#128058=CARTESIAN_POINT('Ctrl Pts',(80.5251595237089,-7.41890539737718,
139.166248831528));
#128059=CARTESIAN_POINT('Ctrl Pts',(80.5468327157855,-7.42624642897226,
139.164736927369));
#128060=CARTESIAN_POINT('Ctrl Pts',(80.559144276443,-7.43057844554725,139.163879422684));
#128061=CARTESIAN_POINT('Ctrl Pts',(80.5990935705138,-7.44516501676963,
139.161100159304));
#128062=CARTESIAN_POINT('Ctrl Pts',(80.6265112179921,-7.45600880997235,
139.159197893095));
#128063=CARTESIAN_POINT('Ctrl Pts',(80.6916105920269,-7.48377576698143,
139.154680964787));
#128064=CARTESIAN_POINT('Ctrl Pts',(80.7289794051964,-7.50138379780424,
139.152088145992));
#128065=CARTESIAN_POINT('Ctrl Pts',(80.8623561745392,-7.57040135230035,
139.142761079237));
#128066=CARTESIAN_POINT('Ctrl Pts',(80.9539129070601,-7.62979577890478,
139.136233145291));
#128067=CARTESIAN_POINT('Ctrl Pts',(81.0837382271023,-7.73337446686093,
139.125942516964));
#128068=CARTESIAN_POINT('Ctrl Pts',(81.1265853934548,-7.77132890007261,
139.122340462722));
#128069=CARTESIAN_POINT('Ctrl Pts',(81.1754549745402,-7.81932673492763,
139.117856955963));
#128070=CARTESIAN_POINT('Ctrl Pts',(81.1834378663579,-7.8273284537776,139.117111704332));
#128071=CARTESIAN_POINT('Ctrl Pts',(81.1957887035048,-7.83996297203915,
139.115937137606));
#128072=CARTESIAN_POINT('Ctrl Pts',(81.2002127297484,-7.84454081437404,
139.115511994429));
#128073=CARTESIAN_POINT('Ctrl Pts',(81.2080252573827,-7.85271824908043,
139.114753077978));
#128074=CARTESIAN_POINT('Ctrl Pts',(81.2114241279721,-7.8563077256886,139.114420111112));
#128075=CARTESIAN_POINT('Ctrl Pts',(81.219597008072,-7.86501624100604,139.113612707633));
#128076=CARTESIAN_POINT('Ctrl Pts',(81.224354739907,-7.87015024817455,139.113137074994));
#128077=CARTESIAN_POINT('Ctrl Pts',(81.2390495351768,-7.88620902058621,
139.111650882181));
#128078=CARTESIAN_POINT('Ctrl Pts',(81.2488734714249,-7.89723569545139,
139.110632602807));
#128079=CARTESIAN_POINT('Ctrl Pts',(81.2990284598913,-7.95506090269255,
139.105310447461));
#128080=CARTESIAN_POINT('Ctrl Pts',(81.3368766919029,-8.00394184402509,
139.100872666353));
#128081=CARTESIAN_POINT('Ctrl Pts',(81.4570882857847,-8.17842517040699,
139.085508070088));
#128082=CARTESIAN_POINT('Ctrl Pts',(81.5251785484698,-8.31302113873978,
139.074524324563));
#128083=CARTESIAN_POINT('Ctrl Pts',(81.5811030584779,-8.47454789597075,
139.062769785278));
#128084=CARTESIAN_POINT('Ctrl Pts',(81.587526807376,-8.49428713845587,139.061354270288));
#128085=CARTESIAN_POINT('Ctrl Pts',(81.5972254986323,-8.52609817184272,
139.059105574938));
#128086=CARTESIAN_POINT('Ctrl Pts',(81.6007361444671,-8.53809519726469,
139.058264818814));
#128087=CARTESIAN_POINT('Ctrl Pts',(81.6067534547674,-8.55955129749134,
139.056773805271));
#128088=CARTESIAN_POINT('Ctrl Pts',(81.6093123974102,-8.56899496695653,
139.056121879899));
#128089=CARTESIAN_POINT('Ctrl Pts',(81.614512959671,-8.58887972317174,139.054758002613));
#128090=CARTESIAN_POINT('Ctrl Pts',(81.6171368357983,-8.59932501643513,
139.054046649405));
#128091=CARTESIAN_POINT('Ctrl Pts',(81.6238244612891,-8.62708396658456,
139.052169138659));
#128092=CARTESIAN_POINT('Ctrl Pts',(81.6277126660476,-8.64443880207056,
139.051008621214));
#128093=CARTESIAN_POINT('Ctrl Pts',(81.646684389425,-8.73596411027016,139.044952676544));
#128094=CARTESIAN_POINT('Ctrl Pts',(81.6569794717248,-8.81104083498744,
139.040211539027));
#128095=CARTESIAN_POINT('Ctrl Pts',(81.6692157845001,-8.99033709402061,
139.029131904));
#128096=CARTESIAN_POINT('Ctrl Pts',(81.6665639372429,-9.09453784548305,
139.022889697919));
#128097=CARTESIAN_POINT('Ctrl Pts',(81.6485596052606,-9.24510491714907,
139.013428296461));
#128098=CARTESIAN_POINT('Ctrl Pts',(81.6408782397394,-9.29213504358959,
139.010406203584));
#128099=CARTESIAN_POINT('Ctrl Pts',(81.6289718448549,-9.34946549794788,
139.006569086307));
#128100=CARTESIAN_POINT('Ctrl Pts',(81.6266447414103,-9.36014202085136,
139.005847883685));
#128101=CARTESIAN_POINT('Ctrl Pts',(81.622828921443,-9.37685667925658,139.004707275751));
#128102=CARTESIAN_POINT('Ctrl Pts',(81.6214110816232,-9.38291091157659,
139.004291750468));
#128103=CARTESIAN_POINT('Ctrl Pts',(81.6186685003208,-9.39433343660984,
139.003503021156));
#128104=CARTESIAN_POINT('Ctrl Pts',(81.6173508844832,-9.39970324732988,
139.003130217162));
#128105=CARTESIAN_POINT('Ctrl Pts',(81.6141616867702,-9.41242650897211,
139.002242202601));
#128106=CARTESIAN_POINT('Ctrl Pts',(81.6122665676593,-9.4197738504856,139.001725684514));
#128107=CARTESIAN_POINT('Ctrl Pts',(81.6056823884638,-9.44459813193324,
138.99996853776));
#128108=CARTESIAN_POINT('Ctrl Pts',(81.6007589903592,-9.46201084391851,
138.998715814736));
#128109=CARTESIAN_POINT('Ctrl Pts',(81.5879289415297,-9.50471762477543,
138.995599043641));
#128110=CARTESIAN_POINT('Ctrl Pts',(81.5797006411595,-9.52990936294555,
138.993721808239));
#128111=CARTESIAN_POINT('Ctrl Pts',(81.5407094005852,-9.64029176324238,
138.985353711912));
#128112=CARTESIAN_POINT('Ctrl Pts',(81.5036303681489,-9.72308662970838,
138.978706454975));
#128113=CARTESIAN_POINT('Ctrl Pts',(81.4133986209474,-9.887256275759,138.965137209152));
#128114=CARTESIAN_POINT('Ctrl Pts',(81.3594846578721,-9.96784638168643,
138.958256394555));
#128115=CARTESIAN_POINT('Ctrl Pts',(81.2871068676301,-10.0579530477069,
138.950352436821));
#128116=CARTESIAN_POINT('Ctrl Pts',(81.2750981212901,-10.0723961819373,
138.949077814952));
#128117=CARTESIAN_POINT('Ctrl Pts',(81.255614451474,-10.0950394144237,138.947066337866));
#128118=CARTESIAN_POINT('Ctrl Pts',(81.2482977415181,-10.1033728874261,
138.946323108888));
#128119=CARTESIAN_POINT('Ctrl Pts',(81.234469922968,-10.1188086629687,138.944940642752));
#128120=CARTESIAN_POINT('Ctrl Pts',(81.2279793960653,-10.1259286942567,
138.944300586777));
#128121=CARTESIAN_POINT('Ctrl Pts',(81.213184158602,-10.1418787674245,138.94286109795));
#128122=CARTESIAN_POINT('Ctrl Pts',(81.2048440499005,-10.1506753454214,
138.942063215308));
#128123=CARTESIAN_POINT('Ctrl Pts',(81.1794611121129,-10.1768689610236,
138.939674376835));
#128124=CARTESIAN_POINT('Ctrl Pts',(81.1621316509018,-10.1939845856308,
138.938095900388));
#128125=CARTESIAN_POINT('Ctrl Pts',(81.1211872542965,-10.23268741861,138.934478500816));
#128126=CARTESIAN_POINT('Ctrl Pts',(81.097313156499,-10.2539869040337,138.93245113995));
#128127=CARTESIAN_POINT('Ctrl Pts',(81.0072187051488,-10.329820797807,138.925062898522));
#128128=CARTESIAN_POINT('Ctrl Pts',(80.9374294033046,-10.3799058304871,
138.919846998417));
#128129=CARTESIAN_POINT('Ctrl Pts',(80.7867978735428,-10.4712843910356,
138.909083028692));
#128130=CARTESIAN_POINT('Ctrl Pts',(80.7058266837974,-10.5117979899266,
138.903548120027));
#128131=CARTESIAN_POINT('Ctrl Pts',(80.6073565927027,-10.5514259613815,
138.896661246888));
#128132=CARTESIAN_POINT('Ctrl Pts',(80.5926490493154,-10.5571035946484,
138.89562856959));
#128133=CARTESIAN_POINT('Ctrl Pts',(80.5711965936094,-10.5650370547405,
138.894113377604));
#128134=CARTESIAN_POINT('Ctrl Pts',(80.5645138102336,-10.5674599467685,
138.893640126414));
#128135=CARTESIAN_POINT('Ctrl Pts',(80.5526467059649,-10.5716767200934,
138.892797194074));
#128136=CARTESIAN_POINT('Ctrl Pts',(80.5474687308649,-10.5734878714346,
138.892428530702));
#128137=CARTESIAN_POINT('Ctrl Pts',(80.5362057212862,-10.5773651187782,
138.891624647997));
#128138=CARTESIAN_POINT('Ctrl Pts',(80.5301177430218,-10.5794215613716,
138.891188912372));
#128139=CARTESIAN_POINT('Ctrl Pts',(80.5127235205137,-10.5851852152572,
138.889940802131));
#128140=CARTESIAN_POINT('Ctrl Pts',(80.5013895207989,-10.5888065028011,
138.889123758127));
#128141=CARTESIAN_POINT('Ctrl Pts',(80.4754563525984,-10.5967872066983,
138.887247212396));
#128142=CARTESIAN_POINT('Ctrl Pts',(80.4608343613467,-10.6010683250892,
138.886184082174));
#128143=CARTESIAN_POINT('Ctrl Pts',(80.3060670505471,-10.6440864178984,
138.874892248395));
#128144=CARTESIAN_POINT('Ctrl Pts',(80.1614840342172,-10.664519051482,138.864075581864));
#128145=CARTESIAN_POINT('Ctrl Pts',(79.9507120684992,-10.666553286255,138.849022903426));
#128146=CARTESIAN_POINT('Ctrl Pts',(79.8853587767227,-10.6633365494475,
138.844443159493));
#128147=CARTESIAN_POINT('Ctrl Pts',(79.8028201934209,-10.6543842482472,
138.838777170037));
#128148=CARTESIAN_POINT('Ctrl Pts',(79.7853152806429,-10.6522038705261,
138.837582081662));
#128149=CARTESIAN_POINT('Ctrl Pts',(79.7572137075095,-10.6482494159339,
138.835673439323));
#128150=CARTESIAN_POINT('Ctrl Pts',(79.746594227845,-10.6466501889977,138.834954450985));
#128151=CARTESIAN_POINT('Ctrl Pts',(79.7263216489237,-10.6433965010427,
138.833586008472));
#128152=CARTESIAN_POINT('Ctrl Pts',(79.7166662623906,-10.6417593915083,
138.832936037184));
#128153=CARTESIAN_POINT('Ctrl Pts',(79.6944492618709,-10.6377905728283,
138.831444293622));
#128154=CARTESIAN_POINT('Ctrl Pts',(79.6818988072796,-10.6353992969059,
138.830604443108));
#128155=CARTESIAN_POINT('Ctrl Pts',(79.6420374199767,-10.6273281405852,
138.827945004566));
#128156=CARTESIAN_POINT('Ctrl Pts',(79.614840198836,-10.6211064611918,138.82614258319));
#128157=CARTESIAN_POINT('Ctrl Pts',(79.5156892451251,-10.5957881311155,
138.819599937934));
#128158=CARTESIAN_POINT('Ctrl Pts',(79.4448791678645,-10.5725581631489,
138.814987170475));
#128159=CARTESIAN_POINT('Ctrl Pts',(79.2563727472063,-10.496389367791,138.802521098322));
#128160=CARTESIAN_POINT('Ctrl Pts',(79.1429144477376,-10.4344187789382,
138.794823601157));
#128161=CARTESIAN_POINT('Ctrl Pts',(79.0263614493235,-10.3519535891143,
138.785554713314));
#128162=CARTESIAN_POINT('Ctrl Pts',(79.0150776629315,-10.3437553698324,
138.784641540473));
#128163=CARTESIAN_POINT('Ctrl Pts',(78.9983272179701,-10.3312610367618,
138.783259831104));
#128164=CARTESIAN_POINT('Ctrl Pts',(78.9927820373413,-10.3270705639592,
138.782798048324));
#128165=CARTESIAN_POINT('Ctrl Pts',(78.9828227851343,-10.3194460161396,
138.781960421194));
#128166=CARTESIAN_POINT('Ctrl Pts',(78.9783994072971,-10.3160241273241,
138.781585413341));
#128167=CARTESIAN_POINT('Ctrl Pts',(78.9694186609889,-10.3090041325214,
138.780817760678));
#128168=CARTESIAN_POINT('Ctrl Pts',(78.9648627588378,-10.3054043835621,
138.780425014286));
#128169=CARTESIAN_POINT('Ctrl Pts',(78.9535305410094,-10.2963538487905,
138.779439982242));
#128170=CARTESIAN_POINT('Ctrl Pts',(78.9467780071182,-10.2908737565632,
138.778845701987));
#128171=CARTESIAN_POINT('Ctrl Pts',(78.9317431800531,-10.2784755846167,
138.777506569767));
#128172=CARTESIAN_POINT('Ctrl Pts',(78.9234846425289,-10.2715294431498,
138.776759968635));
#128173=CARTESIAN_POINT('Ctrl Pts',(78.8991134467303,-10.2506235570128,
138.774525111573));
#128174=CARTESIAN_POINT('Ctrl Pts',(78.8832011607647,-10.2364346921585,
138.773024144763));
#128175=CARTESIAN_POINT('Ctrl Pts',(78.8231402598813,-10.1807734479365,
138.767209270554));
#128176=CARTESIAN_POINT('Ctrl Pts',(78.7809950559529,-10.1372118943443,
138.762810883504));
#128177=CARTESIAN_POINT('Ctrl Pts',(78.6562619125777,-9.99336781705434,
138.748954119857));
#128178=CARTESIAN_POINT('Ctrl Pts',(78.5829465834908,-9.88565436811021,
138.739549489168));
#128179=CARTESIAN_POINT('Ctrl Pts',(78.5134952003582,-9.7525099803891,138.729229690625));
#128180=CARTESIAN_POINT('Ctrl Pts',(78.5044393173238,-9.73434739552867,
138.72784644108));
#128181=CARTESIAN_POINT('Ctrl Pts',(78.4903442080147,-9.70473518234833,
138.725629613013));
#128182=CARTESIAN_POINT('Ctrl Pts',(78.4850983435307,-9.69338681378128,
138.724788985808));
#128183=CARTESIAN_POINT('Ctrl Pts',(78.4759856550359,-9.67307616041793,
138.723299962849));
#128184=CARTESIAN_POINT('Ctrl Pts',(78.4720689647162,-9.66413703387003,
138.722649884185));
#128185=CARTESIAN_POINT('Ctrl Pts',(78.46395169687,-9.64515891166399,138.721280601481));
#128186=CARTESIAN_POINT('Ctrl Pts',(78.4597704593522,-9.63511210225471,
138.720562078149));
#128187=CARTESIAN_POINT('Ctrl Pts',(78.448820388865,-9.60805665503589,138.718643617584));
#128188=CARTESIAN_POINT('Ctrl Pts',(78.4422328186799,-9.59097591628757,
138.717449777295));
#128189=CARTESIAN_POINT('Ctrl Pts',(78.4060847467122,-9.49244119123581,
138.710655162977));
#128190=CARTESIAN_POINT('Ctrl Pts',(78.3826313546794,-9.40888344053641,
138.705261407724));
#128191=CARTESIAN_POINT('Ctrl Pts',(78.3445816311609,-9.21688870063967,
138.693247528272));
#128192=CARTESIAN_POINT('Ctrl Pts',(78.3339388140977,-9.10809724434987,
138.686703611574));
#128193=CARTESIAN_POINT('Ctrl Pts',(78.3340002645784,-8.99906107773531,
138.679802703723));
#128194=CARTESIAN_POINT('Ctrl Pts',(78.3340002659352,-8.9990586732761,138.679802551545));
#128195=CARTESIAN_POINT('Ctrl Pts',(78.3340122908892,-8.97777640250722,
138.678455593874));
#128196=CARTESIAN_POINT('Ctrl Pts',(78.3344321193602,-8.95649709999227,
138.677095246544));
#128197=CARTESIAN_POINT('Ctrl Pts',(78.3358009540242,-8.92131348367504,
138.67481502874));
#128198=CARTESIAN_POINT('Ctrl Pts',(78.3365170051759,-8.90740232859391,
138.673905425437));
#128199=CARTESIAN_POINT('Ctrl Pts',(78.3378248684508,-8.88698456957304,
138.672556420238));
#128200=CARTESIAN_POINT('Ctrl Pts',(78.3382806792744,-8.88046945513672,
138.672123874439));
#128201=CARTESIAN_POINT('Ctrl Pts',(78.3391689393945,-8.86876230860699,
138.671342591399));
#128202=CARTESIAN_POINT('Ctrl Pts',(78.3395874622305,-8.86356926269507,
138.67099460244));
#128203=CARTESIAN_POINT('Ctrl Pts',(78.3404626590702,-8.85331094236375,
138.6703042116));
#128204=CARTESIAN_POINT('Ctrl Pts',(78.3409181710623,-8.84824576329396,
138.669961869966));
#128205=CARTESIAN_POINT('Ctrl Pts',(78.3420395514555,-8.83638530291543,
138.669156852411));
#128206=CARTESIAN_POINT('Ctrl Pts',(78.3427239995179,-8.82959204207361,
138.668693172819));
#128207=CARTESIAN_POINT('Ctrl Pts',(78.3449257623353,-8.80900852954848,
138.667280747579));
#128208=CARTESIAN_POINT('Ctrl Pts',(78.3465735514021,-8.79523325050894,
138.666325306197));
#128209=CARTESIAN_POINT('Ctrl Pts',(78.3545977592447,-8.73458488322595,
138.66207839854));
#128210=CARTESIAN_POINT('Ctrl Pts',(78.3627964138434,-8.68797865093281,
138.658708642598));
#128211=CARTESIAN_POINT('Ctrl Pts',(78.3892162346329,-8.56797690308466,
138.649852340649));
#128212=CARTESIAN_POINT('Ctrl Pts',(78.4104657701459,-8.49537864982559,
138.644319845945));
#128213=CARTESIAN_POINT('Ctrl Pts',(78.436559345854,-8.42449211911253,138.638847691527));
#128214=CARTESIAN_POINT('Ctrl Pts',(78.4365593750041,-8.42449203992252,
138.833737849951));
#128215=CARTESIAN_POINT('Ctrl Pts',(78.4357654627803,-8.42664880352886,
138.833891290677));
#128216=CARTESIAN_POINT('Ctrl Pts',(78.4349760076973,-8.42880722551953,
138.834044583115));
#128217=CARTESIAN_POINT('Ctrl Pts',(78.4308396898992,-8.44018914343849,
138.834851539479));
#128218=CARTESIAN_POINT('Ctrl Pts',(78.4275698389047,-8.44944058502104,
138.835502628057));
#128219=CARTESIAN_POINT('Ctrl Pts',(78.4201791056846,-8.47095437667124,
138.83700585588));
#128220=CARTESIAN_POINT('Ctrl Pts',(78.4161188918261,-8.48323701707355,
138.837855968269));
#128221=CARTESIAN_POINT('Ctrl Pts',(78.4034747020729,-8.52303690839969,
138.840585659804));
#128222=CARTESIAN_POINT('Ctrl Pts',(78.3954613590095,-8.55073089736053,
138.842446720717));
#128223=CARTESIAN_POINT('Ctrl Pts',(78.3649421910079,-8.66747049985526,
138.850153225424));
#128224=CARTESIAN_POINT('Ctrl Pts',(78.3490992446991,-8.75809293572287,
138.855791524017));
#128225=CARTESIAN_POINT('Ctrl Pts',(78.3307435608108,-8.96054648702028,
138.868210307207));
#128226=CARTESIAN_POINT('Ctrl Pts',(78.3318429385482,-9.07223950797057,
138.874946240725));
#128227=CARTESIAN_POINT('Ctrl Pts',(78.345676015335,-9.19743340964611,138.883137059902));
#128228=CARTESIAN_POINT('Ctrl Pts',(78.3474637306941,-9.21187647540124,
138.884091970012));
#128229=CARTESIAN_POINT('Ctrl Pts',(78.3503854186024,-9.23318692748227,
138.885518151753));
#128230=CARTESIAN_POINT('Ctrl Pts',(78.3513736460147,-9.24007405299294,
138.885981735949));
#128231=CARTESIAN_POINT('Ctrl Pts',(78.3532149466878,-9.25235856789412,
138.886813725034));
#128232=CARTESIAN_POINT('Ctrl Pts',(78.3540514732453,-9.25775822795488,
138.887181205429));
#128233=CARTESIAN_POINT('Ctrl Pts',(78.3559612207556,-9.2696968667602,138.887997699576));
#128234=CARTESIAN_POINT('Ctrl Pts',(78.3570468824366,-9.27623351948151,
138.888447373386));
#128235=CARTESIAN_POINT('Ctrl Pts',(78.3603559833217,-9.29544738024032,
138.889776537574));
#128236=CARTESIAN_POINT('Ctrl Pts',(78.362687311603,-9.30810516225522,138.890661655817));
#128237=CARTESIAN_POINT('Ctrl Pts',(78.3684118462298,-9.33728406070953,
138.89272206758));
#128238=CARTESIAN_POINT('Ctrl Pts',(78.3719097151171,-9.35378300890375,
138.893902022913));
#128239=CARTESIAN_POINT('Ctrl Pts',(78.3848745738333,-9.4106655989781,138.898015580042));
#128240=CARTESIAN_POINT('Ctrl Pts',(78.3955983074982,-9.45074510014426,
138.900993480983));
#128241=CARTESIAN_POINT('Ctrl Pts',(78.4451145988264,-9.61151751358259,
138.913166572));
#128242=CARTESIAN_POINT('Ctrl Pts',(78.4961331980123,-9.72802109726034,
138.922476660456));
#128243=CARTESIAN_POINT('Ctrl Pts',(78.5817385502336,-9.875203573505,138.93444442158));
#128244=CARTESIAN_POINT('Ctrl Pts',(78.6050656555788,-9.91192412359391,
138.93745427323));
#128245=CARTESIAN_POINT('Ctrl Pts',(78.6386422790772,-9.96046994167867,
138.941468598723));
#128246=CARTESIAN_POINT('Ctrl Pts',(78.6476581072446,-9.97312321248951,
138.942518391084));
#128247=CARTESIAN_POINT('Ctrl Pts',(78.6623297722622,-9.9931163850955,138.944183255617));
#128248=CARTESIAN_POINT('Ctrl Pts',(78.6678719369064,-10.0005381662012,
138.944802656392));
#128249=CARTESIAN_POINT('Ctrl Pts',(78.6794382270635,-10.0157606670721,
138.946076128631));
#128250=CARTESIAN_POINT('Ctrl Pts',(78.6854702666044,-10.0235549404123,
138.94672985669));
#128251=CARTESIAN_POINT('Ctrl Pts',(78.699755812662,-10.0416793497508,138.948254268952));
#128252=CARTESIAN_POINT('Ctrl Pts',(78.7080639106748,-10.0519657657019,
138.949122740492));
#128253=CARTESIAN_POINT('Ctrl Pts',(78.7359439856612,-10.085656079992,138.951979430824));
#128254=CARTESIAN_POINT('Ctrl Pts',(78.7560370060276,-10.1086221124858,
138.953946565433));
#128255=CARTESIAN_POINT('Ctrl Pts',(78.8777093875024,-10.2402157882939,
138.965372180505));
#128256=CARTESIAN_POINT('Ctrl Pts',(78.9928255613813,-10.3353914340398,
138.974203251278));
#128257=CARTESIAN_POINT('Ctrl Pts',(79.1676650222503,-10.4443185494194,
138.986966430809));
#128258=CARTESIAN_POINT('Ctrl Pts',(79.2178108548987,-10.472078889972,138.990573127886));
#128259=CARTESIAN_POINT('Ctrl Pts',(79.2794407214493,-10.5021578317847,
138.995061827805));
#128260=CARTESIAN_POINT('Ctrl Pts',(79.2896510534084,-10.5070130000715,
138.995807276204));
#128261=CARTESIAN_POINT('Ctrl Pts',(79.3056866175785,-10.5144389909557,
138.996982042738));
#128262=CARTESIAN_POINT('Ctrl Pts',(79.311478740144,-10.5170810794716,138.997407186286));
#128263=CARTESIAN_POINT('Ctrl Pts',(79.3217950848453,-10.5217156538283,
138.998166097348));
#128264=CARTESIAN_POINT('Ctrl Pts',(79.3263132329559,-10.523721291979,138.998499058561));
#128265=CARTESIAN_POINT('Ctrl Pts',(79.3372499262112,-10.5285180166273,
138.999306413092));
#128266=CARTESIAN_POINT('Ctrl Pts',(79.343677146171,-10.5312887691616,138.999782001796));
#128267=CARTESIAN_POINT('Ctrl Pts',(79.363714522277,-10.5397774914202,139.001267754765));
#128268=CARTESIAN_POINT('Ctrl Pts',(79.3773829243795,-10.5453549339939,
139.002285627907));
#128269=CARTESIAN_POINT('Ctrl Pts',(79.4485795306223,-10.5733091368075,
139.007603595204));
#128270=CARTESIAN_POINT('Ctrl Pts',(79.5072399477876,-10.5926557040071,
139.012037311236));
#128271=CARTESIAN_POINT('Ctrl Pts',(79.7118081413373,-10.6477389056236,
139.027398716744));
#128272=CARTESIAN_POINT('Ctrl Pts',(79.8614335449113,-10.6670079403707,
139.038383640353));
#128273=CARTESIAN_POINT('Ctrl Pts',(80.0323665402619,-10.6658146426545,
139.050137982387));
#128274=CARTESIAN_POINT('Ctrl Pts',(80.0530991329156,-10.6652827284884,
139.051552181808));
#128275=CARTESIAN_POINT('Ctrl Pts',(80.0862990603242,-10.6638102580642,
139.053799212641));
#128276=CARTESIAN_POINT('Ctrl Pts',(80.0987745577488,-10.6631162629689,
139.054639599674));
#128277=CARTESIAN_POINT('Ctrl Pts',(80.1210027308491,-10.6616287341169,
139.056130199461));
#128278=CARTESIAN_POINT('Ctrl Pts',(80.1307583240794,-10.660889514271,139.056782076316));
#128279=CARTESIAN_POINT('Ctrl Pts',(80.1512408935126,-10.6591558798163,
139.058146094951));
#128280=CARTESIAN_POINT('Ctrl Pts',(80.1619659080164,-10.658143267402,139.058857636047));
#128281=CARTESIAN_POINT('Ctrl Pts',(80.190381465752,-10.6551820510527,139.06073620679));
#128282=CARTESIAN_POINT('Ctrl Pts',(80.2080522030789,-10.653053854273,139.06189758614));
#128283=CARTESIAN_POINT('Ctrl Pts',(80.3009130684846,-10.640357347065,139.067969907922));
#128284=CARTESIAN_POINT('Ctrl Pts',(80.3753541586966,-10.6249406998734,
139.072725524982));
#128285=CARTESIAN_POINT('Ctrl Pts',(80.5500972025953,-10.5760962469182,
139.083910609427));
#128286=CARTESIAN_POINT('Ctrl Pts',(80.648769083236,-10.5381101484378,139.090239133787));
#128287=CARTESIAN_POINT('Ctrl Pts',(80.7844210682072,-10.4704974628363,
139.099708393852));
#128288=CARTESIAN_POINT('Ctrl Pts',(80.8247861040395,-10.4482424687139,
139.102635401686));
#128289=CARTESIAN_POINT('Ctrl Pts',(80.8734287501862,-10.4187302157357,
139.106364745582));
#128290=CARTESIAN_POINT('Ctrl Pts',(80.8826293490558,-10.4130246366018,
139.10707941089));
#128291=CARTESIAN_POINT('Ctrl Pts',(80.8970066692135,-10.4039136087939,
139.108211930331));
#128292=CARTESIAN_POINT('Ctrl Pts',(80.9022213035857,-10.4005681353655,
139.108625994407));
#128293=CARTESIAN_POINT('Ctrl Pts',(80.9120557258954,-10.3941811023156,
139.109413403265));
#128294=CARTESIAN_POINT('Ctrl Pts',(80.9166791767232,-10.3911455266973,
139.109786363018));
#128295=CARTESIAN_POINT('Ctrl Pts',(80.9276385213664,-10.3838716993669,
139.110676941632));
#128296=CARTESIAN_POINT('Ctrl Pts',(80.9339605435542,-10.3796129181916,
139.111195893278));
#128297=CARTESIAN_POINT('Ctrl Pts',(80.955388482954,-10.3649633710228,139.112972057691));
#128298=CARTESIAN_POINT('Ctrl Pts',(80.9703513945365,-10.3543671067065,
139.114241727563));
#128299=CARTESIAN_POINT('Ctrl Pts',(81.0068974031942,-10.32756989012,139.117410391055));
#128300=CARTESIAN_POINT('Ctrl Pts',(81.0282671182901,-10.3110876264722,
139.119323123501));
#128301=CARTESIAN_POINT('Ctrl Pts',(81.1223055716679,-10.2348431425141,
139.127982044712));
#128302=CARTESIAN_POINT('Ctrl Pts',(81.1902335271836,-10.1695090043202,
139.134893419425));
#128303=CARTESIAN_POINT('Ctrl Pts',(81.3135590047839,-10.0289559907336,
139.148420685002));
#128304=CARTESIAN_POINT('Ctrl Pts',(81.3688940057096,-9.9541080016211,139.155014791111));
#128305=CARTESIAN_POINT('Ctrl Pts',(81.4275744848557,-9.8590344266445,139.162653017737));
#128306=CARTESIAN_POINT('Ctrl Pts',(81.4371724637305,-9.84287864824879,
139.163927794711));
#128307=CARTESIAN_POINT('Ctrl Pts',(81.451942601725,-9.81703073625185,139.165931753165));
#128308=CARTESIAN_POINT('Ctrl Pts',(81.4572955243766,-9.80744430601168,
139.166667391658));
#128309=CARTESIAN_POINT('Ctrl Pts',(81.4667474109426,-9.79011691281913,
139.167983746783));
#128310=CARTESIAN_POINT('Ctrl Pts',(81.4708807948246,-9.7823952938621,139.168565672047));
#128311=CARTESIAN_POINT('Ctrl Pts',(81.480454589229,-9.76416634305832,139.169928705837));
#128312=CARTESIAN_POINT('Ctrl Pts',(81.4858443843175,-9.75363284715538,
139.170708010123));
#128313=CARTESIAN_POINT('Ctrl Pts',(81.5013392258646,-9.72253813808178,
139.172984966399));
#128314=CARTESIAN_POINT('Ctrl Pts',(81.511133180982,-9.701824354067,139.174471836469));
#128315=CARTESIAN_POINT('Ctrl Pts',(81.5545678892191,-9.60483365950251,
139.181307329184));
#128316=CARTESIAN_POINT('Ctrl Pts',(81.5828824965542,-9.52629880540434,
139.186476374112));
#128317=CARTESIAN_POINT('Ctrl Pts',(81.6283618491473,-9.36260144581922,
139.196889616307));
#128318=CARTESIAN_POINT('Ctrl Pts',(81.6449922152124,-9.27756328726469,
139.202114256777));
#128319=CARTESIAN_POINT('Ctrl Pts',(81.6605055395375,-9.14358313068467,
139.210524640583));
#128320=CARTESIAN_POINT('Ctrl Pts',(81.6639730348982,-9.09532865618125,
139.21359091935));
#128321=CARTESIAN_POINT('Ctrl Pts',(81.6656425916159,-9.0361679198286,139.217469048152));
#128322=CARTESIAN_POINT('Ctrl Pts',(81.6658425518073,-9.02533651086294,
139.218183950568));
#128323=CARTESIAN_POINT('Ctrl Pts',(81.6659913384069,-9.00824713174338,
139.21932067823));
#128324=CARTESIAN_POINT('Ctrl Pts',(81.6660105618148,-9.00198985817584,
139.219738748212));
#128325=CARTESIAN_POINT('Ctrl Pts',(81.6659804065235,-8.99021679746421,
139.220529091812));
#128326=CARTESIAN_POINT('Ctrl Pts',(81.665938884974,-8.98470118065836,139.220900933308));
#128327=CARTESIAN_POINT('Ctrl Pts',(81.665776247815,-8.97168436904526,139.221782089728));
#128328=CARTESIAN_POINT('Ctrl Pts',(81.6656318524333,-8.96418367016243,
139.222292656523));
#128329=CARTESIAN_POINT('Ctrl Pts',(81.6649796485914,-8.93910716416467,
139.224008449677));
#128330=CARTESIAN_POINT('Ctrl Pts',(81.6642442727935,-8.92153913792775,
139.225225038674));
#128331=CARTESIAN_POINT('Ctrl Pts',(81.6617623174051,-8.87854430881846,
139.228232910677));
#128332=CARTESIAN_POINT('Ctrl Pts',(81.6597100664976,-8.85314007145961,
139.230036297735));
#128333=CARTESIAN_POINT('Ctrl Pts',(81.6484208755317,-8.74450804695441,
139.237834262732));
#128334=CARTESIAN_POINT('Ctrl Pts',(81.6334992484543,-8.66199558686887,
139.243968580014));
#128335=CARTESIAN_POINT('Ctrl Pts',(81.5880354831232,-8.48705516877,139.257090678194));
#128336=CARTESIAN_POINT('Ctrl Pts',(81.5554728734917,-8.39545161228709,
139.264029326413));
#128337=CARTESIAN_POINT('Ctrl Pts',(81.5052710113702,-8.28566429093416,
139.272340679899));
#128338=CARTESIAN_POINT('Ctrl Pts',(81.4949692404908,-8.26434832108724,
139.273955102075));
#128339=CARTESIAN_POINT('Ctrl Pts',(81.478699577489,-8.23243823474725,139.276374176812));
#128340=CARTESIAN_POINT('Ctrl Pts',(81.4730646652475,-8.2216787234766,139.277190258056));
#128341=CARTESIAN_POINT('Ctrl Pts',(81.4627059432925,-8.20241493857962,
139.278652437866));
#128342=CARTESIAN_POINT('Ctrl Pts',(81.4580244058265,-8.19388868905047,
139.279299990825));
#128343=CARTESIAN_POINT('Ctrl Pts',(81.4478369629443,-8.17571393194336,
139.280681405892));
#128344=CARTESIAN_POINT('Ctrl Pts',(81.442308662733,-8.16607846609383,139.281414429577));
#128345=CARTESIAN_POINT('Ctrl Pts',(81.4268821689816,-8.13980345713761,
139.283415691732));
#128346=CARTESIAN_POINT('Ctrl Pts',(81.4167894605229,-8.12327969583428,
139.284676868815));
#128347=CARTESIAN_POINT('Ctrl Pts',(81.3465725830168,-8.0127012163698,139.293143772132));
#128348=CARTESIAN_POINT('Ctrl Pts',(81.2774132635477,-7.92471572678365,
139.299989343676));
#128349=CARTESIAN_POINT('Ctrl Pts',(81.1262955392844,-7.76780996550157,
139.313294437602));
#128350=CARTESIAN_POINT('Ctrl Pts',(81.0454917251394,-7.69854900069521,
139.319734685963));
#128351=CARTESIAN_POINT('Ctrl Pts',(80.9465992895673,-7.62896997803671,
139.327592255134));
#128352=CARTESIAN_POINT('Ctrl Pts',(80.9344250221196,-7.62064385393388,
139.328559383554));
#128353=CARTESIAN_POINT('Ctrl Pts',(80.9162291843967,-7.60855093843947,
139.330007170816));
#128354=CARTESIAN_POINT('Ctrl Pts',(80.9102911040183,-7.60465899844532,
139.330480003006));
#128355=CARTESIAN_POINT('Ctrl Pts',(80.8997246339761,-7.59782967077172,
139.331322355417));
#128356=CARTESIAN_POINT('Ctrl Pts',(80.8951063650861,-7.59487700086125,
139.331690863198));
#128357=CARTESIAN_POINT('Ctrl Pts',(80.8849473958799,-7.58845231815264,
139.332502299767));
#128358=CARTESIAN_POINT('Ctrl Pts',(80.8794008690894,-7.58499015572465,
139.332945819337));
#128359=CARTESIAN_POINT('Ctrl Pts',(80.8632818028448,-7.57505995086257,
139.334235864697));
#128360=CARTESIAN_POINT('Ctrl Pts',(80.8526575485988,-7.56867729113766,
139.335087517461));
#128361=CARTESIAN_POINT('Ctrl Pts',(80.8281114789083,-7.55430118142076,
139.337056565091));
#128362=CARTESIAN_POINT('Ctrl Pts',(80.814143503225,-7.54638931972059,139.338178072111));
#128363=CARTESIAN_POINT('Ctrl Pts',(80.766367502663,-7.52023222950363,139.342012187541));
#128364=CARTESIAN_POINT('Ctrl Pts',(80.7320450405205,-7.50295574849416,
139.344763249164));
#128365=CARTESIAN_POINT('Ctrl Pts',(80.6328625112713,-7.45725809061481,
139.35264864543));
#128366=CARTESIAN_POINT('Ctrl Pts',(80.5667439989889,-7.431762503023,139.357826474518));
#128367=CARTESIAN_POINT('Ctrl Pts',(80.4070366551528,-7.3816026603498,139.369947844441));
#128368=CARTESIAN_POINT('Ctrl Pts',(80.3125131974446,-7.36072270970312,
139.376816046572));
#128369=CARTESIAN_POINT('Ctrl Pts',(80.1980779205702,-7.34571048063891,
139.384708637636));
#128370=CARTESIAN_POINT('Ctrl Pts',(80.1794171779391,-7.34358272082952,
139.385983097254));
#128371=CARTESIAN_POINT('Ctrl Pts',(80.1496787973133,-7.34070032995489,
139.387994920842));
#128372=CARTESIAN_POINT('Ctrl Pts',(80.1386231842156,-7.33974015272477,
139.388738641321));
#128373=CARTESIAN_POINT('Ctrl Pts',(80.1179405065252,-7.33815190540202,
139.390122410837));
#128374=CARTESIAN_POINT('Ctrl Pts',(80.1083160440931,-7.33749685898879,
139.390763275428));
#128375=CARTESIAN_POINT('Ctrl Pts',(80.0865629160185,-7.33620603602546,
139.39220511338));
#128376=CARTESIAN_POINT('Ctrl Pts',(80.0744318096969,-7.33561921072226,
139.393004528911));
#128377=CARTESIAN_POINT('Ctrl Pts',(80.0378816720721,-7.33425157098279,
139.395399930388));
#128378=CARTESIAN_POINT('Ctrl Pts',(80.0134501600528,-7.33387514206634,
139.39698335957));
#128379=CARTESIAN_POINT('Ctrl Pts',(79.9569122344079,-7.33424783383181,
139.400613212122));
#128380=CARTESIAN_POINT('Ctrl Pts',(79.9248178057395,-7.33538753403498,
139.402647977563));
#128381=CARTESIAN_POINT('Ctrl Pts',(79.8066594070181,-7.3430081095544,139.41007559726));
#128382=CARTESIAN_POINT('Ctrl Pts',(79.7211041821049,-7.35524441251809,
139.415321710573));
#128383=CARTESIAN_POINT('Ctrl Pts',(79.549169724019,-7.39364246086482,139.426085428576));
#128384=CARTESIAN_POINT('Ctrl Pts',(79.4632007283571,-7.42029278227903,
139.431589757663));
#128385=CARTESIAN_POINT('Ctrl Pts',(79.3652150567596,-7.45959374814087,
139.438440030539));
#128386=CARTESIAN_POINT('Ctrl Pts',(79.3507024823065,-7.46565452569573,
139.439470267458));
#128387=CARTESIAN_POINT('Ctrl Pts',(79.3297659706607,-7.47474829581623,
139.440982438017));
#128388=CARTESIAN_POINT('Ctrl Pts',(79.3232717054569,-7.47761856751154,
139.441455156496));
#128389=CARTESIAN_POINT('Ctrl Pts',(79.31180577059,-7.48277403096381,139.442296607062));
#128390=CARTESIAN_POINT('Ctrl Pts',(79.3068267075362,-7.48504233585205,
139.44266431683));
#128391=CARTESIAN_POINT('Ctrl Pts',(79.2960636870118,-7.49000980008923,
139.443464321018));
#128392=CARTESIAN_POINT('Ctrl Pts',(79.2902841397156,-7.49271763402121,
139.443897114828));
#128393=CARTESIAN_POINT('Ctrl Pts',(79.2738498905341,-7.50053288548231,
139.445136638163));
#128394=CARTESIAN_POINT('Ctrl Pts',(79.2632340257019,-7.5057204116621,139.445948006113));
#128395=CARTESIAN_POINT('Ctrl Pts',(79.1670791002145,-7.55398098386478,
139.453388948551));
#128396=CARTESIAN_POINT('Ctrl Pts',(79.0853565530412,-7.60423795889812,
139.46036873848));
#128397=CARTESIAN_POINT('Ctrl Pts',(78.9109705802748,-7.73340036811098,
139.47617715688));
#128398=CARTESIAN_POINT('Ctrl Pts',(78.8216819984057,-7.81600815811391,
139.484937470301));
#128399=CARTESIAN_POINT('Ctrl Pts',(78.7283665603689,-7.92345651350948,
139.494728244193));
#128400=CARTESIAN_POINT('Ctrl Pts',(78.7148900055743,-7.93958033989662,
139.496161656021));
#128401=CARTESIAN_POINT('Ctrl Pts',(78.6938650444635,-7.96572506198106,
139.498430543781));
#128402=CARTESIAN_POINT('Ctrl Pts',(78.6861189059643,-7.97558326096429,
139.499273907597));
#128403=CARTESIAN_POINT('Ctrl Pts',(78.6725513831199,-7.99325717798711,
139.500764844494));
#128404=CARTESIAN_POINT('Ctrl Pts',(78.6666859840328,-8.00103819796508,
139.501414142837));
#128405=CARTESIAN_POINT('Ctrl Pts',(78.6545511924222,-8.01743346206989,
139.502767757607));
#128406=CARTESIAN_POINT('Ctrl Pts',(78.6482954684241,-8.02605730993669,
139.503471521148));
#128407=CARTESIAN_POINT('Ctrl Pts',(78.6320287865222,-8.04894044397087,
139.50531786036));
#128408=CARTESIAN_POINT('Ctrl Pts',(78.6221578606527,-8.06329802149247,
139.506455058233));
#128409=CARTESIAN_POINT('Ctrl Pts',(78.5734443906988,-8.13659001803001,
139.512158771233));
#128410=CARTESIAN_POINT('Ctrl Pts',(78.5381473041907,-8.19779915812948,
139.516592024258));
#128411=CARTESIAN_POINT('Ctrl Pts',(78.4805144020893,-8.31425847162602,
139.524620536356));
#128412=CARTESIAN_POINT('Ctrl Pts',(78.457055835973,-8.36881079569985,139.528231549375));
#128413=CARTESIAN_POINT('Ctrl Pts',(78.4365593777415,-8.42449203248626,
139.531855306428));
#128414=CARTESIAN_POINT('Origin',(80.,-9.,141.545925280538));
#128415=CARTESIAN_POINT('',(77.9452506264311,-9.00160446819347,139.095925280496));
#128416=CARTESIAN_POINT('Ctrl Pts',(81.2520391107129,-7.37076839346111,
139.547882946156));
#128417=CARTESIAN_POINT('Ctrl Pts',(81.308376492207,-7.41406279355911,139.544018177529));
#128418=CARTESIAN_POINT('Ctrl Pts',(81.3625557941979,-7.46035206945108,
139.540153408901));
#128419=CARTESIAN_POINT('Ctrl Pts',(81.4142433388808,-7.50939162053498,
139.536288640274));
#128420=CARTESIAN_POINT('Ctrl Pts',(81.4658662946457,-7.55836989164198,
139.532428701074));
#128421=CARTESIAN_POINT('Ctrl Pts',(81.515003327894,-7.61009127859361,139.528568761873));
#128422=CARTESIAN_POINT('Ctrl Pts',(81.5613536305889,-7.66427083480709,
139.524708822673));
#128423=CARTESIAN_POINT('Ctrl Pts',(81.6076723958972,-7.71841352650165,
139.520851509828));
#128424=CARTESIAN_POINT('Ctrl Pts',(81.6512078775579,-7.7750107012777,139.516994196984));
#128425=CARTESIAN_POINT('Ctrl Pts',(81.6916969813358,-7.83374150127879,
139.51313688414));
#128426=CARTESIAN_POINT('Ctrl Pts',(81.7321720676574,-7.89245196849052,
139.509280906709));
#128427=CARTESIAN_POINT('Ctrl Pts',(81.7696025941656,-7.95329419518399,
139.505424929279));
#128428=CARTESIAN_POINT('Ctrl Pts',(81.8037675969863,-8.01591666076381,
139.501568951848));
#128429=CARTESIAN_POINT('Ctrl Pts',(81.8379321897393,-8.07853837471322,
139.497713020699));
#128430=CARTESIAN_POINT('Ctrl Pts',(81.8688311057131,-8.14293985793319,
139.493857089551));
#128431=CARTESIAN_POINT('Ctrl Pts',(81.896289179377,-8.20874472470788,139.490001158402));
#128432=CARTESIAN_POINT('Ctrl Pts',(81.9237751180498,-8.27461637159319,
139.486141314176));
#128433=CARTESIAN_POINT('Ctrl Pts',(81.9478130540654,-8.34189379684482,
139.48228146995));
#128434=CARTESIAN_POINT('Ctrl Pts',(81.9682762259155,-8.41018116256268,
139.478421625724));
#128435=CARTESIAN_POINT('Ctrl Pts',(81.9887500346486,-8.47850402447474,
139.474559775128));
#128436=CARTESIAN_POINT('Ctrl Pts',(82.0056452636483,-8.54783740001086,
139.470697924531));
#128437=CARTESIAN_POINT('Ctrl Pts',(82.0188859519888,-8.61777352870029,
139.466836073934));
#128438=CARTESIAN_POINT('Ctrl Pts',(82.0321504672958,-8.68783550929022,
139.462967273836));
#128439=CARTESIAN_POINT('Ctrl Pts',(82.0417472410663,-8.7585019275549,139.459098473738));
#128440=CARTESIAN_POINT('Ctrl Pts',(82.0476520986989,-8.82935872365122,
139.45522967364));
#128441=CARTESIAN_POINT('Ctrl Pts',(82.052086736227,-8.88257325084868,139.452324146162));
#128442=CARTESIAN_POINT('Ctrl Pts',(82.0544401302615,-8.93589502683532,
139.449418618684));
#128443=CARTESIAN_POINT('Ctrl Pts',(82.0547213515201,-8.98914964943005,
139.446513091206));
#128444=CARTESIAN_POINT('Ctrl Pts',(82.0550957922083,-9.06005715348447,
139.442644437343));
#128445=CARTESIAN_POINT('Ctrl Pts',(82.0517961792383,-9.1311232476299,139.438775783481));
#128446=CARTESIAN_POINT('Ctrl Pts',(82.0448030571631,-9.20193568262351,
139.434907129618));
#128447=CARTESIAN_POINT('Ctrl Pts',(82.0378203675282,-9.27264247860433,
139.431044247069));
#128448=CARTESIAN_POINT('Ctrl Pts',(82.0271551533183,-9.34309588696136,
139.427181364519));
#128449=CARTESIAN_POINT('Ctrl Pts',(82.0128399703195,-9.41288353852396,
139.42331848197));
#128450=CARTESIAN_POINT('Ctrl Pts',(81.998541609247,-9.48258918186285,139.419460138736));
#128451=CARTESIAN_POINT('Ctrl Pts',(81.9806018961423,-9.55163014870729,
139.415601795502));
#128452=CARTESIAN_POINT('Ctrl Pts',(81.9591049949775,-9.61960082404249,
139.411743452268));
#128453=CARTESIAN_POINT('Ctrl Pts',(81.9376216617892,-9.68752859903064,
139.407887544264));
#128454=CARTESIAN_POINT('Ctrl Pts',(81.9125857410267,-9.75438696053742,
139.404031636261));
#128455=CARTESIAN_POINT('Ctrl Pts',(81.8841317678587,-9.81978353474901,
139.400175728257));
#128456=CARTESIAN_POINT('Ctrl Pts',(81.8556862293651,-9.8851607233089,139.396320963269));
#128457=CARTESIAN_POINT('Ctrl Pts',(81.8238248437278,-9.9490765395105,139.392466198281));
#128458=CARTESIAN_POINT('Ctrl Pts',(81.7887303644301,-10.0111583683408,
139.388611433293));
#128459=CARTESIAN_POINT('Ctrl Pts',(81.7536345415136,-10.0732425740212,
139.384756520722));
#128460=CARTESIAN_POINT('Ctrl Pts',(81.7153056202243,-10.133492231011,139.380901608151));
#128461=CARTESIAN_POINT('Ctrl Pts',(81.6739715583618,-10.1915606506997,
139.37704669558));
#128462=CARTESIAN_POINT('Ctrl Pts',(81.6325942438482,-10.2496898341503,
139.373187749165));
#128463=CARTESIAN_POINT('Ctrl Pts',(81.5882057937322,-10.3056328272753,
139.369328802749));
#128464=CARTESIAN_POINT('Ctrl Pts',(81.5410761084176,-10.3590739459516,
139.365469856334));
#128465=CARTESIAN_POINT('Ctrl Pts',(81.4939197547027,-10.4125453043619,
139.361608726328));
#128466=CARTESIAN_POINT('Ctrl Pts',(81.444019418087,-10.4635116227775,139.357747596322));
#128467=CARTESIAN_POINT('Ctrl Pts',(81.3916817944375,-10.5116941970952,
139.353886466316));
#128468=CARTESIAN_POINT('Ctrl Pts',(81.339252561045,-10.559961108319,139.350018577938));
#128469=CARTESIAN_POINT('Ctrl Pts',(81.2843778974373,-10.6054342371213,
139.34615068956));
#128470=CARTESIAN_POINT('Ctrl Pts',(81.2273969197782,-10.6478757124914,
139.342282801182));
#128471=CARTESIAN_POINT('Ctrl Pts',(81.1934998810702,-10.6731234423926,
139.339981858526));
#128472=CARTESIAN_POINT('Ctrl Pts',(81.1588580068394,-10.6972991413891,
139.337680915871));
#128473=CARTESIAN_POINT('Ctrl Pts',(81.1235469328426,-10.7203603843962,
139.335379973215));
#128474=CARTESIAN_POINT('Ctrl Pts',(81.064169403796,-10.7591391433384,139.331510810544));
#128475=CARTESIAN_POINT('Ctrl Pts',(81.0026656025668,-10.7949161392637,
139.327641647873));
#128476=CARTESIAN_POINT('Ctrl Pts',(80.9393714614606,-10.8274514548664,
139.323772485202));
#128477=CARTESIAN_POINT('Ctrl Pts',(80.8761716184376,-10.8599382980854,
139.319909086961));
#128478=CARTESIAN_POINT('Ctrl Pts',(80.8111871586046,-10.8891928273149,
139.31604568872));
#128479=CARTESIAN_POINT('Ctrl Pts',(80.7447823129528,-10.9150187646111,
139.312182290478));
#128480=CARTESIAN_POINT('Ctrl Pts',(80.6784553574967,-10.9408144091283,
139.308323423847));
#128481=CARTESIAN_POINT('Ctrl Pts',(80.610711776106,-10.9631892747637,139.304464557215));
#128482=CARTESIAN_POINT('Ctrl Pts',(80.5419381060237,-10.9819941099154,
139.300605690584));
#128483=CARTESIAN_POINT('Ctrl Pts',(80.4732077575516,-11.0007870996075,
139.296749254713));
#128484=CARTESIAN_POINT('Ctrl Pts',(80.4034490751883,-11.016014392627,139.292892818841));
#128485=CARTESIAN_POINT('Ctrl Pts',(80.3330647821262,-11.0275762410837,
139.28903638297));
#128486=CARTESIAN_POINT('Ctrl Pts',(80.2627012832298,-11.0391346737358,
139.285181086435));
#128487=CARTESIAN_POINT('Ctrl Pts',(80.1917130196465,-11.0470297330092,
139.2813257899));
#128488=CARTESIAN_POINT('Ctrl Pts',(80.1205122587922,-11.0512128992332,
139.277470493365));
#128489=CARTESIAN_POINT('Ctrl Pts',(80.0493087189167,-11.0553962287295,
139.273615046355));
#128490=CARTESIAN_POINT('Ctrl Pts',(79.9778931503567,-11.0558673512484,
139.269759599345));
#128491=CARTESIAN_POINT('Ctrl Pts',(79.9066805502896,-11.0526297870794,
139.265904152335));
#128492=CARTESIAN_POINT('Ctrl Pts',(79.8353934290479,-11.0493888349274,
139.262044670751));
#128493=CARTESIAN_POINT('Ctrl Pts',(79.764310186547,-11.0424314708572,139.258185189168));
#128494=CARTESIAN_POINT('Ctrl Pts',(79.6938425160225,-11.0318132683651,
139.254325707585));
#128495=CARTESIAN_POINT('Ctrl Pts',(79.6233349545345,-11.0211890550269,
139.250464041192));
#128496=CARTESIAN_POINT('Ctrl Pts',(79.5534441348589,-11.0068999751735,
139.246602374799));
#128497=CARTESIAN_POINT('Ctrl Pts',(79.4845706367511,-10.989052571955,139.242740708406));
#128498=CARTESIAN_POINT('Ctrl Pts',(79.4155766714858,-10.9711739517083,
139.238872287543));
#128499=CARTESIAN_POINT('Ctrl Pts',(79.3476040438129,-10.949724728142,139.23500386668));
#128500=CARTESIAN_POINT('Ctrl Pts',(79.2810366107104,-10.92486082805,139.231135445818));
#128501=CARTESIAN_POINT('Ctrl Pts',(79.2415238646542,-10.9101022452939,
139.228839248953));
#128502=CARTESIAN_POINT('Ctrl Pts',(79.2025058194015,-10.8941414848041,
139.226543052088));
#128503=CARTESIAN_POINT('Ctrl Pts',(79.1640586576305,-10.8770188157335,
139.224246855223));
#128504=CARTESIAN_POINT('Ctrl Pts',(79.0992743299609,-10.8481667353053,
139.220377712139));
#128505=CARTESIAN_POINT('Ctrl Pts',(79.035858637873,-10.8159002327603,139.216508569054));
#128506=CARTESIAN_POINT('Ctrl Pts',(78.9741953427939,-10.7803714128671,
139.21263942597));
#128507=CARTESIAN_POINT('Ctrl Pts',(78.912623899062,-10.7448955153804,139.208776046217));
#128508=CARTESIAN_POINT('Ctrl Pts',(78.8528000884208,-10.7061671869215,
139.204912666463));
#128509=CARTESIAN_POINT('Ctrl Pts',(78.7950863573877,-10.664385975772,139.20104928671));
#128510=CARTESIAN_POINT('Ctrl Pts',(78.7374402965986,-10.6226537537402,
139.19719043683));
#128511=CARTESIAN_POINT('Ctrl Pts',(78.6818997925833,-10.5778760426978,
139.193331586949));
#128512=CARTESIAN_POINT('Ctrl Pts',(78.6287998814073,-10.5302966370189,
139.189472737069));
#128513=CARTESIAN_POINT('Ctrl Pts',(78.5757334039231,-10.4827471891149,
139.185616316865));
#128514=CARTESIAN_POINT('Ctrl Pts',(78.5251048314328,-10.4323998698312,
139.181759896661));
#128515=CARTESIAN_POINT('Ctrl Pts',(78.4772163885171,-10.3795389211976,
139.177903476456));
#128516=CARTESIAN_POINT('Ctrl Pts',(78.4293420799125,-10.3266935745141,
139.174048194478));
#128517=CARTESIAN_POINT('Ctrl Pts',(78.3842066212449,-10.2713364311666,
139.170192912499));
#128518=CARTESIAN_POINT('Ctrl Pts',(78.342074374492,-10.2137875360968,139.16633763052));
#128519=CARTESIAN_POINT('Ctrl Pts',(78.2999404708373,-10.1562363778468,
139.162482196928));
#128520=CARTESIAN_POINT('Ctrl Pts',(78.2608102987546,-10.0964936900018,
139.158626763336));
#128521=CARTESIAN_POINT('Ctrl Pts',(78.2249059796854,-10.0349100354831,
139.154771329743));
#128522=CARTESIAN_POINT('Ctrl Pts',(78.1889640708374,-9.97326190638249,
139.150911859731));
#128523=CARTESIAN_POINT('Ctrl Pts',(78.1562550019824,-9.90976938362367,
139.147052389719));
#128524=CARTESIAN_POINT('Ctrl Pts',(78.1269553705043,-9.84480848623664,
139.143192919707));
#128525=CARTESIAN_POINT('Ctrl Pts',(78.0976391450011,-9.77981079784868,
139.139331263861));
#128526=CARTESIAN_POINT('Ctrl Pts',(78.0717363772824,-9.71334353215134,
139.135469608015));
#128527=CARTESIAN_POINT('Ctrl Pts',(78.0493748152645,-9.64580101515523,
139.131607952168));
#128528=CARTESIAN_POINT('Ctrl Pts',(78.026974130229,-9.57814032810112,139.127739540102));
#128529=CARTESIAN_POINT('Ctrl Pts',(78.0081271490154,-9.50940110245736,
139.123871128036));
#128530=CARTESIAN_POINT('Ctrl Pts',(77.9929110603408,-9.4399903985291,139.12000271597));
#128531=CARTESIAN_POINT('Ctrl Pts',(77.9838786451825,-9.39878754359592,
139.117706389724));
#128532=CARTESIAN_POINT('Ctrl Pts',(77.9761246711039,-9.35734824655245,
139.115410063478));
#128533=CARTESIAN_POINT('Ctrl Pts',(77.9696566259696,-9.31575836652541,
139.113113737232));
#128534=CARTESIAN_POINT('Ctrl Pts',(77.9535184264028,-9.21198887050296,
139.107384251667));
#128535=CARTESIAN_POINT('Ctrl Pts',(77.9453328874797,-9.10695137253559,
139.101654766102));
#128536=CARTESIAN_POINT('Ctrl Pts',(77.9452506264317,-9.00160446896122,
139.095925280538));
#128537=CARTESIAN_POINT('Ctrl Pts',(77.9452506264311,-9.00160446819347,
139.095925280496));
#128538=CARTESIAN_POINT('Ctrl Pts',(77.9451944260495,-8.9296318985583,139.092010919611));
#128539=CARTESIAN_POINT('Ctrl Pts',(77.9489244684886,-8.85751959834465,
139.088096558725));
#128540=CARTESIAN_POINT('Ctrl Pts',(77.9564551529281,-8.78570576184602,
139.084182197839));
#128541=CARTESIAN_POINT('Ctrl Pts',(77.9637702774153,-8.71594754025189,
139.080379882473));
#128542=CARTESIAN_POINT('Ctrl Pts',(77.9746713407522,-8.64647146490485,
139.076577567106));
#128543=CARTESIAN_POINT('Ctrl Pts',(77.989118824301,-8.57767967167147,139.072775251739));
#128544=CARTESIAN_POINT('Ctrl Pts',(78.0035569312041,-8.50893252540201,
139.068975404136));
#128545=CARTESIAN_POINT('Ctrl Pts',(78.0215367933465,-8.44086927047645,
139.065175556532));
#128546=CARTESIAN_POINT('Ctrl Pts',(78.04296740632,-8.37388420418094,139.061375708928));
#128547=CARTESIAN_POINT('Ctrl Pts',(78.0643917757445,-8.3069186531715,139.057576968364));
#128548=CARTESIAN_POINT('Ctrl Pts',(78.0892647486508,-8.24103114499242,
139.053778227799));
#128549=CARTESIAN_POINT('Ctrl Pts',(78.1174453485376,-8.17660122251894,
139.049979487235));
#128550=CARTESIAN_POINT('Ctrl Pts',(78.1456278173538,-8.11216702707126,
139.046180494739));
#128551=CARTESIAN_POINT('Ctrl Pts',(78.1771181441239,-8.04919106713867,
139.042381502244));
#128552=CARTESIAN_POINT('Ctrl Pts',(78.2117278439726,-7.98803149333731,
139.038582509748));
#128553=CARTESIAN_POINT('Ctrl Pts',(78.2463733781589,-7.92680859587732,
139.034779583835));
#128554=CARTESIAN_POINT('Ctrl Pts',(78.284144478339,-7.86740627170997,139.030976657923));
#128555=CARTESIAN_POINT('Ctrl Pts',(78.3248080762865,-7.81015564831994,
139.02717373201));
#128556=CARTESIAN_POINT('Ctrl Pts',(78.3654974020029,-7.75286880258645,
139.023368399995));
#128557=CARTESIAN_POINT('Ctrl Pts',(78.4090825513877,-7.69773675553732,
139.019563067979));
#128558=CARTESIAN_POINT('Ctrl Pts',(78.4552905398303,-7.64505710594054,
139.015757735964));
#128559=CARTESIAN_POINT('Ctrl Pts',(78.5015729500498,-7.59229261142271,
139.011946275147));
#128560=CARTESIAN_POINT('Ctrl Pts',(78.5504862702189,-7.5419887443633,139.00813481433));
#128561=CARTESIAN_POINT('Ctrl Pts',(78.6017220132516,-7.49440502316367,
139.004323353514));
#128562=CARTESIAN_POINT('Ctrl Pts',(78.6122194521588,-7.48465582901318,
139.003542442089));
#128563=CARTESIAN_POINT('Ctrl Pts',(78.622814278579,-7.47502067954326,139.002761530665));
#128564=CARTESIAN_POINT('Ctrl Pts',(78.6335036862727,-7.46550158453334,
139.001980619241));
#128565=CARTESIAN_POINT('Ctrl Pts',(78.6864653129501,-7.41833837674232,
138.99811152373));
#128566=CARTESIAN_POINT('Ctrl Pts',(78.741975216377,-7.37382789140775,138.994242428218));
#128567=CARTESIAN_POINT('Ctrl Pts',(78.7997368192305,-7.33225725623249,
138.990373332707));
#128568=CARTESIAN_POINT('Ctrl Pts',(78.8574123619349,-7.29074855796495,
138.986510001838));
#128569=CARTESIAN_POINT('Ctrl Pts',(78.9173325537051,-7.25217129684877,
138.982646670968));
#128570=CARTESIAN_POINT('Ctrl Pts',(78.9791663526586,-7.21677364674147,
138.978783340098));
#128571=CARTESIAN_POINT('Ctrl Pts',(79.0409276221684,-7.18141751716047,
138.974924540816));
#128572=CARTESIAN_POINT('Ctrl Pts',(79.1045976207614,-7.14923383050781,
138.971065741533));
#128573=CARTESIAN_POINT('Ctrl Pts',(79.1698162652816,-7.12042756747473,
138.967206942251));
#128574=CARTESIAN_POINT('Ctrl Pts',(79.234993827726,-7.09163944988286,138.963350573676));
#128575=CARTESIAN_POINT('Ctrl Pts',(79.3017176573821,-7.06622473082228,
138.959494205102));
#128576=CARTESIAN_POINT('Ctrl Pts',(79.3696043147107,-7.04434183905555,
138.955637836527));
#128577=CARTESIAN_POINT('Ctrl Pts',(79.437470918147,-7.02246541155104,138.951782607134));
#128578=CARTESIAN_POINT('Ctrl Pts',(79.5064992052078,-7.00411888903381,
138.94792737774));
#128579=CARTESIAN_POINT('Ctrl Pts',(79.5762886922953,-6.98941145675622,
138.944072148347));
#128580=CARTESIAN_POINT('Ctrl Pts',(79.6460809080327,-6.9747034494431,138.940216768221));
#128581=CARTESIAN_POINT('Ctrl Pts',(79.7166339070914,-6.9636349128697,138.936361388094));
#128582=CARTESIAN_POINT('Ctrl Pts',(79.7875367805005,-6.95626397427165,
138.932506007968));
#128583=CARTESIAN_POINT('Ctrl Pts',(79.8585138681322,-6.94888532049294,
138.928646592405));
#128584=CARTESIAN_POINT('Ctrl Pts',(79.929841076995,-6.94521204097988,138.924787176843));
#128585=CARTESIAN_POINT('Ctrl Pts',(80.0011030377304,-6.94525029606821,
138.92092776128));
#128586=CARTESIAN_POINT('Ctrl Pts',(80.0724053469192,-6.94528857281654,
138.91706616052));
#128587=CARTESIAN_POINT('Ctrl Pts',(80.1436418491016,-6.94904254196509,
138.91320455976));
#128588=CARTESIAN_POINT('Ctrl Pts',(80.2144005988324,-6.95646630913011,
138.909342959));
#128589=CARTESIAN_POINT('Ctrl Pts',(80.2852831397793,-6.96390306404816,
138.905474602435));
#128590=CARTESIAN_POINT('Ctrl Pts',(80.3556857795533,-6.97502235938342,
138.901606245871));
#128591=CARTESIAN_POINT('Ctrl Pts',(80.425205779222,-6.98972698177183,138.897737889307));
#128592=CARTESIAN_POINT('Ctrl Pts',(80.4664825477539,-6.99845769663903,
138.895441093288));
#128593=CARTESIAN_POINT('Ctrl Pts',(80.5074484142674,-7.00845136765168,
138.893144297268));
#128594=CARTESIAN_POINT('Ctrl Pts',(80.5480219975304,-7.01967945707702,
138.890847501249));
#128595=CARTESIAN_POINT('Ctrl Pts',(80.6163512059742,-7.03858847129437,
138.886979510272));
#128596=CARTESIAN_POINT('Ctrl Pts',(80.6838343956939,-7.06107511666485,
138.883111519295));
#128597=CARTESIAN_POINT('Ctrl Pts',(80.7500698253181,-7.08704604873845,
138.879243528319));
#128598=CARTESIAN_POINT('Ctrl Pts',(80.8162190584746,-7.11298318315084,
138.87538057101));
#128599=CARTESIAN_POINT('Ctrl Pts',(80.8811233032238,-7.1423954376098,138.871517613701));
#128600=CARTESIAN_POINT('Ctrl Pts',(80.9443946161016,-7.17513935557307,
138.867654656392));
#128601=CARTESIAN_POINT('Ctrl Pts',(81.0075967034356,-7.20784744820844,
138.86379592557));
#128602=CARTESIAN_POINT('Ctrl Pts',(81.0691689767197,-7.24387974524783,
138.859937194747));
#128603=CARTESIAN_POINT('Ctrl Pts',(81.1287439327008,-7.28304493451599,
138.856078463924));
#128604=CARTESIAN_POINT('Ctrl Pts',(81.1708819766027,-7.31074691830482,
138.853349139728));
#128605=CARTESIAN_POINT('Ctrl Pts',(81.21202117558,-7.34001523367997,138.850619815533));
#128606=CARTESIAN_POINT('Ctrl Pts',(81.2520391107129,-7.37076839346111,
138.847890491337));
#128607=CARTESIAN_POINT('',(77.9452503313529,-8.99883308321583,139.154074719413));
#128608=CARTESIAN_POINT('Ctrl Pts',(77.9452503313529,-8.99883308321583,
139.154074719413));
#128609=CARTESIAN_POINT('Ctrl Pts',(77.9452955388054,-8.91923015076267,
139.149777319356));
#128610=CARTESIAN_POINT('Ctrl Pts',(77.9499707048544,-8.83979433416053,
139.145479919299));
#128611=CARTESIAN_POINT('Ctrl Pts',(77.9591932155917,-8.761032991371,139.141182519242));
#128612=CARTESIAN_POINT('Ctrl Pts',(77.9684534931109,-8.68194911575514,
139.136867521052));
#128613=CARTESIAN_POINT('Ctrl Pts',(77.9822982979791,-8.60354550943924,
139.132552522862));
#128614=CARTESIAN_POINT('Ctrl Pts',(78.0005942479508,-8.52631846017337,
139.128237524672));
#128615=CARTESIAN_POINT('Ctrl Pts',(78.0189841118794,-8.44869500089355,
139.123900377397));
#128616=CARTESIAN_POINT('Ctrl Pts',(78.0418707971446,-8.37226046029615,
139.119563230122));
#128617=CARTESIAN_POINT('Ctrl Pts',(78.069070752716,-8.29749747012325,139.115226082847));
#128618=CARTESIAN_POINT('Ctrl Pts',(78.0780409913188,-8.2728414790961,139.113795740587));
#128619=CARTESIAN_POINT('Ctrl Pts',(78.0874799658388,-8.2483670990492,139.112365398327));
#128620=CARTESIAN_POINT('Ctrl Pts',(78.0973799938381,-8.22409106549,139.110935056068));
#128621=CARTESIAN_POINT('Ctrl Pts',(78.1241601719728,-8.15842291756506,
139.107065893222));
#128622=CARTESIAN_POINT('Ctrl Pts',(78.1543965425552,-8.09401427390062,
139.103196730376));
#128623=CARTESIAN_POINT('Ctrl Pts',(78.1879492686742,-8.03125353698621,
139.09932756753));
#128624=CARTESIAN_POINT('Ctrl Pts',(78.2214520066495,-7.96858630343507,
139.095464169112));
#128625=CARTESIAN_POINT('Ctrl Pts',(78.2582610655738,-7.90756252818727,
139.091600770694));
#128626=CARTESIAN_POINT('Ctrl Pts',(78.2981885117691,-7.84855081700258,
139.087737372276));
#128627=CARTESIAN_POINT('Ctrl Pts',(78.3380691247073,-7.78960832413534,
139.083878505466));
#128628=CARTESIAN_POINT('Ctrl Pts',(78.3810605885034,-7.73267360779941,
139.080019638656));
#128629=CARTESIAN_POINT('Ctrl Pts',(78.4269298749198,-7.67808928286357,
139.076160771846));
#128630=CARTESIAN_POINT('Ctrl Pts',(78.4727702675689,-7.62353934143152,
139.072304335796));
#128631=CARTESIAN_POINT('Ctrl Pts',(78.5214845745239,-7.57133722501943,
139.068447899745));
#128632=CARTESIAN_POINT('Ctrl Pts',(78.5727982977411,-7.52179403885339,
139.064591463694));
#128633=CARTESIAN_POINT('Ctrl Pts',(78.6240968609664,-7.47226548959643,
139.060736166979));
#128634=CARTESIAN_POINT('Ctrl Pts',(78.6779929665586,-7.42539464827194,
139.056880870264));
#128635=CARTESIAN_POINT('Ctrl Pts',(78.7341751285011,-7.3814559143493,139.053025573549));
#128636=CARTESIAN_POINT('Ctrl Pts',(78.7903594832843,-7.33751546545815,
139.049170126358));
#128637=CARTESIAN_POINT('Ctrl Pts',(78.8488296875721,-7.29650764869656,
139.045314679167));
#128638=CARTESIAN_POINT('Ctrl Pts',(78.9092424104538,-7.25866561414891,
139.041459231976));
#128639=CARTESIAN_POINT('Ctrl Pts',(78.969718352854,-7.22078397941294,139.037599750212));
#128640=CARTESIAN_POINT('Ctrl Pts',(79.0321404592024,-7.18607499850772,
139.033740268449));
#128641=CARTESIAN_POINT('Ctrl Pts',(79.0961385087842,-7.15472712933909,
139.029880786685));
#128642=CARTESIAN_POINT('Ctrl Pts',(79.1601727869471,-7.12336151449182,
139.026019120112));
#128643=CARTESIAN_POINT('Ctrl Pts',(79.2257843373035,-7.09536098981289,
139.022157453539));
#128644=CARTESIAN_POINT('Ctrl Pts',(79.2925830888667,-7.0708657702631,139.018295786966));
#128645=CARTESIAN_POINT('Ctrl Pts',(79.3594986785926,-7.04632770595379,
139.014427365925));
#128646=CARTESIAN_POINT('Ctrl Pts',(79.4276051510998,-7.02530733110495,
139.010558944884));
#128647=CARTESIAN_POINT('Ctrl Pts',(79.4964981007915,-7.0078947316988,139.006690523843));
#128648=CARTESIAN_POINT('Ctrl Pts',(79.5373911841844,-6.99755906044666,
139.004394328587));
#128649=CARTESIAN_POINT('Ctrl Pts',(79.5785611680086,-6.98849353941898,
139.002098133332));
#128650=CARTESIAN_POINT('Ctrl Pts',(79.6199224887927,-6.98070837966023,
138.999801938076));
#128651=CARTESIAN_POINT('Ctrl Pts',(79.6902200529322,-6.96747674785778,
138.995899332206));
#128652=CARTESIAN_POINT('Ctrl Pts',(79.7613482220587,-6.95789427115864,
138.991996726337));
#128653=CARTESIAN_POINT('Ctrl Pts',(79.8328942558139,-6.95205634043317,
138.988094120467));
#128654=CARTESIAN_POINT('Ctrl Pts',(79.9037074294676,-6.94627820878081,
138.984231489758));
#128655=CARTESIAN_POINT('Ctrl Pts',(79.9749294567065,-6.94416834348739,
138.980368859048));
#128656=CARTESIAN_POINT('Ctrl Pts',(80.0461489039904,-6.94576830879268,
138.976506228338));
#128657=CARTESIAN_POINT('Ctrl Pts',(80.1172967808345,-6.94736666624752,
138.972647479296));
#128658=CARTESIAN_POINT('Ctrl Pts',(80.1884415998422,-6.95266744653637,
138.968788730253));
#128659=CARTESIAN_POINT('Ctrl Pts',(80.2591691608483,-6.9616602568352,138.964929981211));
#128660=CARTESIAN_POINT('Ctrl Pts',(80.3298493056808,-6.97064703830099,
138.961073819096));
#128661=CARTESIAN_POINT('Ctrl Pts',(80.4001122671532,-6.98332087521417,
138.957217656981));
#128662=CARTESIAN_POINT('Ctrl Pts',(80.4695479369975,-6.99961946186196,
138.953361494867));
#128663=CARTESIAN_POINT('Ctrl Pts',(80.5404063424309,-7.01625200624832,
138.949426320062));
#128664=CARTESIAN_POINT('Ctrl Pts',(80.6104026566569,-7.0366594470523,138.945491145257));
#128665=CARTESIAN_POINT('Ctrl Pts',(80.6791123432621,-7.06072075560815,
138.941555970452));
#128666=CARTESIAN_POINT('Ctrl Pts',(80.7464442673682,-7.08429958825344,
138.937699703536));
#128667=CARTESIAN_POINT('Ctrl Pts',(80.8125402343916,-7.11138688392842,
138.933843436619));
#128668=CARTESIAN_POINT('Ctrl Pts',(80.877018521144,-7.1418191487182,138.929987169702));
#128669=CARTESIAN_POINT('Ctrl Pts',(80.9434758638943,-7.17318548231151,
138.926012540953));
#128670=CARTESIAN_POINT('Ctrl Pts',(81.0082140902805,-7.20810526770631,
138.922037912204));
#128671=CARTESIAN_POINT('Ctrl Pts',(81.0708422988144,-7.24634828612698,
138.918063283455));
#128672=CARTESIAN_POINT('Ctrl Pts',(81.1334705073483,-7.28459130454764,
138.914088654706));
#128673=CARTESIAN_POINT('Ctrl Pts',(81.1939882517061,-7.32615721258586,
138.910114025957));
#128674=CARTESIAN_POINT('Ctrl Pts',(81.2520391107129,-7.37076839346111,
138.906139397208));
#128675=CARTESIAN_POINT('Ctrl Pts',(81.2520391107129,-7.37076839346111,
139.606097362913));
#128676=CARTESIAN_POINT('Ctrl Pts',(81.3086788835608,-7.4142951766041,139.60223519659));
#128677=CARTESIAN_POINT('Ctrl Pts',(81.3630354864183,-7.46077074580535,
139.598373030266));
#128678=CARTESIAN_POINT('Ctrl Pts',(81.4147982803809,-7.50991832830168,
139.594510863943));
#128679=CARTESIAN_POINT('Ctrl Pts',(81.466618276899,-7.55912022330893,139.590644429577));
#128680=CARTESIAN_POINT('Ctrl Pts',(81.5158383936151,-7.61099968960752,
139.586777995211));
#128681=CARTESIAN_POINT('Ctrl Pts',(81.5621848353351,-7.66524305480394,
139.582911560846));
#128682=CARTESIAN_POINT('Ctrl Pts',(81.6085610024906,-7.71952121032284,
139.579042646647));
#128683=CARTESIAN_POINT('Ctrl Pts',(81.652059532174,-7.7761658982234,139.575173732448));
#128684=CARTESIAN_POINT('Ctrl Pts',(81.6924485874334,-7.83483248354808,
139.571304818249));
#128685=CARTESIAN_POINT('Ctrl Pts',(81.7329055584333,-7.89359771897892,
139.567429398323));
#128686=CARTESIAN_POINT('Ctrl Pts',(81.7702423687397,-7.95439122419767,
139.563553978397));
#128687=CARTESIAN_POINT('Ctrl Pts',(81.8042723619686,-8.0168424305656,139.559678558471));
#128688=CARTESIAN_POINT('Ctrl Pts',(81.8165980230159,-8.03946225292367,
139.558274881659));
#128689=CARTESIAN_POINT('Ctrl Pts',(81.8284903220569,-8.06229934988405,
139.556871204846));
#128690=CARTESIAN_POINT('Ctrl Pts',(81.8399419628445,-8.0853355063938,139.555467528034));
#128691=CARTESIAN_POINT('Ctrl Pts',(81.8714784322706,-8.14877436715937,
139.551601967482));
#128692=CARTESIAN_POINT('Ctrl Pts',(81.8997929599867,-8.21397258847203,
139.547736406931));
#128693=CARTESIAN_POINT('Ctrl Pts',(81.9246862746981,-8.28056945680009,
139.543870846379));
#128694=CARTESIAN_POINT('Ctrl Pts',(81.949542139255,-8.34706613505579,139.540011101278));
#128695=CARTESIAN_POINT('Ctrl Pts',(81.9709868376719,-8.41495683172817,
139.536151356177));
#128696=CARTESIAN_POINT('Ctrl Pts',(81.9888677006433,-8.48385774069773,
139.532291611075));
#128697=CARTESIAN_POINT('Ctrl Pts',(82.0067273008979,-8.55267671735107,
139.528436455723));
#128698=CARTESIAN_POINT('Ctrl Pts',(82.0210313614891,-8.62250305142058,
139.524581300371));
#128699=CARTESIAN_POINT('Ctrl Pts',(82.0316764967262,-8.69293620345219,
139.520726145018));
#128700=CARTESIAN_POINT('Ctrl Pts',(82.0423148262782,-8.76332432591449,
139.516873454357));
#128701=CARTESIAN_POINT('Ctrl Pts',(82.0492987985764,-8.8343180165325,139.513020763696));
#128702=CARTESIAN_POINT('Ctrl Pts',(82.0525760686228,-8.90550637578659,
139.509168073035));
#128703=CARTESIAN_POINT('Ctrl Pts',(82.0558523453396,-8.97667315808627,
139.505316550112));
#128704=CARTESIAN_POINT('Ctrl Pts',(82.0554241276904,-9.04803400587314,
139.501465027188));
#128705=CARTESIAN_POINT('Ctrl Pts',(82.0512910588627,-9.11917447012652,
139.497613504265));
#128706=CARTESIAN_POINT('Ctrl Pts',(82.0471578531392,-9.19031729069972,
139.493761853771));
#128707=CARTESIAN_POINT('Ctrl Pts',(82.0393195830591,-9.2612392273806,139.489910203277));
#128708=CARTESIAN_POINT('Ctrl Pts',(82.0278278969249,-9.33152915852604,
139.486058552784));
#128709=CARTESIAN_POINT('Ctrl Pts',(82.0163242000214,-9.4018925546219,139.482202876659));
#128710=CARTESIAN_POINT('Ctrl Pts',(82.0011595432771,-9.47162214513738,
139.478347200534));
#128711=CARTESIAN_POINT('Ctrl Pts',(81.9824368915262,-9.54031614228697,
139.47449152441));
#128712=CARTESIAN_POINT('Ctrl Pts',(81.9637036833706,-9.60904887121698,
139.470633674337));
#128713=CARTESIAN_POINT('Ctrl Pts',(81.9414086392753,-9.67674438189115,
139.466775824264));
#128714=CARTESIAN_POINT('Ctrl Pts',(81.9157040514693,-9.74301786632893,
139.462917974191));
#128715=CARTESIAN_POINT('Ctrl Pts',(81.8899542975128,-9.80940780150311,
139.459053345397));
#128716=CARTESIAN_POINT('Ctrl Pts',(81.8607832382982,-9.87437027759518,
139.455188716602));
#128717=CARTESIAN_POINT('Ctrl Pts',(81.8283902625532,-9.93754285784748,
139.451324087808));
#128718=CARTESIAN_POINT('Ctrl Pts',(81.808861309546,-9.97562810079643,139.448994195219));
#128719=CARTESIAN_POINT('Ctrl Pts',(81.7881621998911,-10.0130632909878,
139.446664302631));
#128720=CARTESIAN_POINT('Ctrl Pts',(81.7663441333031,-10.0497742448953,
139.444334410042));
#128721=CARTESIAN_POINT('Ctrl Pts',(81.7301084811426,-10.1107441457301,
139.440464902308));
#128722=CARTESIAN_POINT('Ctrl Pts',(81.6906414186229,-10.169955001328,139.436595394573));
#128723=CARTESIAN_POINT('Ctrl Pts',(81.6481389450854,-10.2270434304428,
139.432725886839));
#128724=CARTESIAN_POINT('Ctrl Pts',(81.605699812798,-10.2840467809218,139.428862145815));
#128725=CARTESIAN_POINT('Ctrl Pts',(81.5602345365568,-10.3389335971282,
139.424998404791));
#128726=CARTESIAN_POINT('Ctrl Pts',(81.5119837389329,-10.3913672181356,
139.421134663766));
#128727=CARTESIAN_POINT('Ctrl Pts',(81.4637895967741,-10.4437392722606,
139.417275459497));
#128728=CARTESIAN_POINT('Ctrl Pts',(81.4128167573264,-10.4936634972701,
139.413416255228));
#128729=CARTESIAN_POINT('Ctrl Pts',(81.3593465778319,-10.5408356316742,
139.409557050959));
#128730=CARTESIAN_POINT('Ctrl Pts',(81.3059101238675,-10.5879780129475,
139.405700280826));
#128731=CARTESIAN_POINT('Ctrl Pts',(81.249979818307,-10.6323714269904,139.401843510694));
#128732=CARTESIAN_POINT('Ctrl Pts',(81.1918733503977,-10.6737489295327,
139.397986740561));
#128733=CARTESIAN_POINT('Ctrl Pts',(81.1337841065074,-10.7151141668846,
139.394131113659));
#128734=CARTESIAN_POINT('Ctrl Pts',(81.0735203762951,-10.7534649859936,
139.390275486756));
#128735=CARTESIAN_POINT('Ctrl Pts',(81.0114309784969,-10.7885762321569,
139.386419859854));
#128736=CARTESIAN_POINT('Ctrl Pts',(80.949339228629,-10.8236888084041,139.382564086893));
#128737=CARTESIAN_POINT('Ctrl Pts',(80.885422097698,-10.8555613309118,139.378708313932));
#128738=CARTESIAN_POINT('Ctrl Pts',(80.8200537745665,-10.8840141637788,
139.374852540971));
#128739=CARTESIAN_POINT('Ctrl Pts',(80.7546172056999,-10.9124967019282,
139.370992742511));
#128740=CARTESIAN_POINT('Ctrl Pts',(80.6877268664157,-10.9375522292262,
139.367132944052));
#128741=CARTESIAN_POINT('Ctrl Pts',(80.6197769045767,-10.9590492977598,
139.363273145593));
#128742=CARTESIAN_POINT('Ctrl Pts',(80.5517885619752,-10.9805585086679,
139.35941116697));
#128743=CARTESIAN_POINT('Ctrl Pts',(80.4827398756082,-10.9985051373091,
139.355549188348));
#128744=CARTESIAN_POINT('Ctrl Pts',(80.4130374665832,-11.0128083897129,
139.351687209725));
#128745=CARTESIAN_POINT('Ctrl Pts',(80.3432133455862,-11.0271366179687,
139.347818487448));
#128746=CARTESIAN_POINT('Ctrl Pts',(80.2727337032124,-11.0378086954034,
139.34394976517));
#128747=CARTESIAN_POINT('Ctrl Pts',(80.2020118990309,-11.0447955289344,
139.340081042892));
#128748=CARTESIAN_POINT('Ctrl Pts',(80.1600903586339,-11.0489370921694,
139.337787792611));
#128749=CARTESIAN_POINT('Ctrl Pts',(80.1180837809894,-11.0517847582771,
139.335494542331));
#128750=CARTESIAN_POINT('Ctrl Pts',(80.0760779610836,-11.0533411081302,
139.333201292051));
#128751=CARTESIAN_POINT('Ctrl Pts',(80.0051960423676,-11.055967340972,139.329331590654));
#128752=CARTESIAN_POINT('Ctrl Pts',(79.9340396619645,-11.054924095133,139.325461889257));
#128753=CARTESIAN_POINT('Ctrl Pts',(79.8630204738569,-11.0501790585014,
139.32159218786));
#128754=CARTESIAN_POINT('Ctrl Pts',(79.7921068390491,-11.0454410742493,
139.317728237864));
#128755=CARTESIAN_POINT('Ctrl Pts',(79.7213304723844,-11.0370122524541,
139.313864287867));
#128756=CARTESIAN_POINT('Ctrl Pts',(79.6511047644822,-11.0249122640581,
139.31000033787));
#128757=CARTESIAN_POINT('Ctrl Pts',(79.5809611129923,-11.0128264140976,
139.30614090277));
#128758=CARTESIAN_POINT('Ctrl Pts',(79.5113673184356,-10.997078000316,139.302281467671));
#128759=CARTESIAN_POINT('Ctrl Pts',(79.4427316308838,-10.9777384880925,
139.298422032572));
#128760=CARTESIAN_POINT('Ctrl Pts',(79.374138993588,-10.9584111061614,139.29456501822));
#128761=CARTESIAN_POINT('Ctrl Pts',(79.3065037373071,-10.9354972260411,
139.290708003868));
#128762=CARTESIAN_POINT('Ctrl Pts',(79.2402224506115,-10.9091190737995,
139.286850989516));
#128763=CARTESIAN_POINT('Ctrl Pts',(79.1739605856351,-10.8827486508749,
139.282995105345));
#128764=CARTESIAN_POINT('Ctrl Pts',(79.1090523535346,-10.8529161505769,
139.279139221174));
#128765=CARTESIAN_POINT('Ctrl Pts',(79.0458761036871,-10.8197926126305,
139.275283337003));
#128766=CARTESIAN_POINT('Ctrl Pts',(78.9826972522886,-10.7866677106816,
139.27142729405));
#128767=CARTESIAN_POINT('Ctrl Pts',(78.9212509537941,-10.7502517294585,
139.267571251097));
#128768=CARTESIAN_POINT('Ctrl Pts',(78.8618910631971,-10.7107617047588,
139.263715208144));
#128769=CARTESIAN_POINT('Ctrl Pts',(78.802468931596,-10.6712302733322,139.259855121989));
#128770=CARTESIAN_POINT('Ctrl Pts',(78.7451379801005,-10.6286186336461,
139.255995035834));
#128771=CARTESIAN_POINT('Ctrl Pts',(78.6902223949398,-10.5831867191783,
139.25213494968));
#128772=CARTESIAN_POINT('Ctrl Pts',(78.6352756453157,-10.5377290222076,
139.248272672935));
#128773=CARTESIAN_POINT('Ctrl Pts',(78.5827473484004,-10.4894481931033,
139.244410396191));
#128774=CARTESIAN_POINT('Ctrl Pts',(78.5329258898893,-10.4386421090539,
139.240548119447));
#128775=CARTESIAN_POINT('Ctrl Pts',(78.4830172689758,-10.3877471400044,
139.236679085668));
#128776=CARTESIAN_POINT('Ctrl Pts',(78.4358252628058,-10.334318459567,139.232810051889));
#128777=CARTESIAN_POINT('Ctrl Pts',(78.3915984689724,-10.2786876387484,
139.22894101811));
#128778=CARTESIAN_POINT('Ctrl Pts',(78.3654107199297,-10.2457472908652,
139.226650070093));
#128779=CARTESIAN_POINT('Ctrl Pts',(78.3402617982504,-10.2120354314329,
139.224359122076));
#128780=CARTESIAN_POINT('Ctrl Pts',(78.3161959180139,-10.1776253122225,
139.222068174059));
#128781=CARTESIAN_POINT('Ctrl Pts',(78.2750915169463,-10.1188530035883,
139.218155246495));
#128782=CARTESIAN_POINT('Ctrl Pts',(78.2369898127519,-10.0578146704116,
139.214242318932));
#128783=CARTESIAN_POINT('Ctrl Pts',(78.2021456985161,-9.99484545188481,
139.210329391368));
#128784=CARTESIAN_POINT('Ctrl Pts',(78.1673565385612,-9.93197554505502,
139.206422635065));
#128785=CARTESIAN_POINT('Ctrl Pts',(78.1358149939178,-9.86718120799267,
139.202515878762));
#128786=CARTESIAN_POINT('Ctrl Pts',(78.1077333167647,-9.80082729849671,
139.198609122459));
#128787=CARTESIAN_POINT('Ctrl Pts',(78.0796926665112,-9.73457033104502,
139.194708073868));
#128788=CARTESIAN_POINT('Ctrl Pts',(78.0551020175886,-9.66675875233996,
139.190807025276));
#128789=CARTESIAN_POINT('Ctrl Pts',(78.0341273801337,-9.59778123503494,
139.186905976684));
#128790=CARTESIAN_POINT('Ctrl Pts',(78.0131709343877,-9.52886354326538,
139.183008311547));
#128791=CARTESIAN_POINT('Ctrl Pts',(77.9958244089983,-9.45878237028468,
139.17911064641));
#128792=CARTESIAN_POINT('Ctrl Pts',(77.9822049975602,-9.38794444270915,
139.175212981273));
#128793=CARTESIAN_POINT('Ctrl Pts',(77.9685917193691,-9.31713841566859,
139.171317071377));
#128794=CARTESIAN_POINT('Ctrl Pts',(77.9587023155159,-9.24557677214363,
139.167421161481));
#128795=CARTESIAN_POINT('Ctrl Pts',(77.9526032387532,-9.17367804851513,
139.163525251585));
#128796=CARTESIAN_POINT('Ctrl Pts',(77.9476716119619,-9.11554176240162,
139.16037507421));
#128797=CARTESIAN_POINT('Ctrl Pts',(77.9452171923888,-9.05718542585664,
139.157224896836));
#128798=CARTESIAN_POINT('Ctrl Pts',(77.9452503313524,-8.99883308411473,
139.154074719462));
#128799=CARTESIAN_POINT('Origin',(80.,9.,134.));
#128800=CARTESIAN_POINT('',(78.3340002645793,9.00093892397456,138.679802731044));
#128801=CARTESIAN_POINT('Ctrl Pts',(78.4365593737638,9.57550795670799,139.340802412607));
#128802=CARTESIAN_POINT('Ctrl Pts',(78.4404068226713,9.58596004144325,139.340073158341));
#128803=CARTESIAN_POINT('Ctrl Pts',(78.4443588589399,9.59637293080484,139.339338614757));
#128804=CARTESIAN_POINT('Ctrl Pts',(78.4507209975141,9.61264236620036,139.338177131073));
#128805=CARTESIAN_POINT('Ctrl Pts',(78.4530606839165,9.61852634983335,139.337754213156));
#128806=CARTESIAN_POINT('Ctrl Pts',(78.4572880712981,9.62898361092206,139.336997239269));
#128807=CARTESIAN_POINT('Ctrl Pts',(78.4591626815642,9.63356202021996,139.336663966555));
#128808=CARTESIAN_POINT('Ctrl Pts',(78.4637554368413,9.64463807647073,139.335853258296));
#128809=CARTESIAN_POINT('Ctrl Pts',(78.466494402472,9.65112685806699,139.335374597762));
#128810=CARTESIAN_POINT('Ctrl Pts',(78.4751941310678,9.67137767851389,139.333869525295));
#128811=CARTESIAN_POINT('Ctrl Pts',(78.4812994425996,9.68507627530903,139.332835122305));
#128812=CARTESIAN_POINT('Ctrl Pts',(78.5143715333345,9.75666540579144,139.327350024636));
#128813=CARTESIAN_POINT('Ctrl Pts',(78.5444633730473,9.81304734265798,139.322756861721));
#128814=CARTESIAN_POINT('Ctrl Pts',(78.6346526201113,9.96090503443917,139.310189598706));
#128815=CARTESIAN_POINT('Ctrl Pts',(78.7006510636092,10.0484316740427,139.302185198289));
#128816=CARTESIAN_POINT('Ctrl Pts',(78.8088869487155,10.165908680851,139.290894928653));
#128817=CARTESIAN_POINT('Ctrl Pts',(78.8446838450898,10.2013903821324,139.287394207462));
#128818=CARTESIAN_POINT('Ctrl Pts',(78.8941311229802,10.2461444950879,139.282852433657));
#128819=CARTESIAN_POINT('Ctrl Pts',(78.9063854330165,10.2569126013951,139.281749049446));
#128820=CARTESIAN_POINT('Ctrl Pts',(78.9267517724024,10.2742855189152,139.27995060464));
#128821=CARTESIAN_POINT('Ctrl Pts',(78.934771107336,10.2809967824331,139.279251195608));
#128822=CARTESIAN_POINT('Ctrl Pts',(78.9505044712475,10.2939138824925,139.277895627228));
#128823=CARTESIAN_POINT('Ctrl Pts',(78.9582116578861,10.3001273236168,139.277239177777));
#128824=CARTESIAN_POINT('Ctrl Pts',(78.9765385304608,10.3146346138431,139.275695697084));
#128825=CARTESIAN_POINT('Ctrl Pts',(78.9872044584987,10.3228691380142,139.274811042446));
#128826=CARTESIAN_POINT('Ctrl Pts',(79.0235626270761,10.3502415812307,139.271839660943));
#128827=CARTESIAN_POINT('Ctrl Pts',(79.0497075258949,10.3687683147958,139.269776481048));
#128828=CARTESIAN_POINT('Ctrl Pts',(79.114924104198,10.4122119044117,139.264788925647));
#128829=CARTESIAN_POINT('Ctrl Pts',(79.1545324549174,10.4362753585315,139.261893365329));
#128830=CARTESIAN_POINT('Ctrl Pts',(79.2558435354716,10.4921800527771,139.254738013854));
#128831=CARTESIAN_POINT('Ctrl Pts',(79.3186283502537,10.5218748548831,139.250525413001));
#128832=CARTESIAN_POINT('Ctrl Pts',(79.4047577048759,10.5562092149828,139.244851480178));
#128833=CARTESIAN_POINT('Ctrl Pts',(79.4266124587449,10.5643935576172,139.243420075882));
#128834=CARTESIAN_POINT('Ctrl Pts',(79.5093044828733,10.593395091149,139.238012128862));
#128835=CARTESIAN_POINT('Ctrl Pts',(79.5711514267309,10.6111414986151,139.23398452943));
#128836=CARTESIAN_POINT('Ctrl Pts',(79.6450208759008,10.6277827533342,139.229029823763));
#128837=CARTESIAN_POINT('Ctrl Pts',(79.6562062772238,10.6301818085748,139.228275723817));
#128838=CARTESIAN_POINT('Ctrl Pts',(79.6736845772325,10.6337426916433,139.227090107031));
#128839=CARTESIAN_POINT('Ctrl Pts',(79.6799612155504,10.6349838258107,139.226662886039));
#128840=CARTESIAN_POINT('Ctrl Pts',(79.6910966237643,10.6371191498506,139.225902126262));
#128841=CARTESIAN_POINT('Ctrl Pts',(79.695952441036,10.6380279259856,139.225569415596));
#128842=CARTESIAN_POINT('Ctrl Pts',(79.7076584566262,10.6401648865566,139.224765045173));
#128843=CARTESIAN_POINT('Ctrl Pts',(79.7145123126687,10.6413717461578,139.22429221607));
#128844=CARTESIAN_POINT('Ctrl Pts',(79.7357208331176,10.6449693902631,139.222823736774));
#128845=CARTESIAN_POINT('Ctrl Pts',(79.750098967077,10.6472149862114,139.221820621464));
#128846=CARTESIAN_POINT('Ctrl Pts',(79.8237557947681,10.6577322849405,139.21664935566));
#128847=CARTESIAN_POINT('Ctrl Pts',(79.883414819369,10.6629927313519,139.212355054702));
#128848=CARTESIAN_POINT('Ctrl Pts',(80.0495460003891,10.6686579526859,139.20030963045));
#128849=CARTESIAN_POINT('Ctrl Pts',(80.1559852038318,10.662090991782,139.1925102786));
#128850=CARTESIAN_POINT('Ctrl Pts',(80.3168558794727,10.6365659837214,139.180943711137));
#128851=CARTESIAN_POINT('Ctrl Pts',(80.3721557607356,10.6248837582514,139.177004373364));
#128852=CARTESIAN_POINT('Ctrl Pts',(80.4432517991695,10.6060432381723,139.171989457209));
#128853=CARTESIAN_POINT('Ctrl Pts',(80.4596749057441,10.6014200132898,139.17083437767));
#128854=CARTESIAN_POINT('Ctrl Pts',(80.4861970543714,10.593512190503,139.168973842607));
#128855=CARTESIAN_POINT('Ctrl Pts',(80.4963404409305,10.5903819832587,139.168263436977));
#128856=CARTESIAN_POINT('Ctrl Pts',(80.5158197563398,10.5841662285839,139.166901152849));
#128857=CARTESIAN_POINT('Ctrl Pts',(80.5251596155036,10.5810945721632,139.16624885287));
#128858=CARTESIAN_POINT('Ctrl Pts',(80.5468328269296,10.5737535325418,139.164736947359));
#128859=CARTESIAN_POINT('Ctrl Pts',(80.5591444024363,10.5694215096984,139.163879441639));
#128860=CARTESIAN_POINT('Ctrl Pts',(80.5990937860606,10.5548349017069,139.161100172025));
#128861=CARTESIAN_POINT('Ctrl Pts',(80.6265115068149,10.543991074371,139.159197900738));
#128862=CARTESIAN_POINT('Ctrl Pts',(80.6916110878453,10.5162240109812,139.154680958014));
#128863=CARTESIAN_POINT('Ctrl Pts',(80.7289800316512,10.4986159016409,139.152088130076));
#128864=CARTESIAN_POINT('Ctrl Pts',(80.8623365761505,10.4296087269023,139.142762476515));
#128865=CARTESIAN_POINT('Ctrl Pts',(80.9538751682516,10.3702286761206,139.136235854507));
#128866=CARTESIAN_POINT('Ctrl Pts',(81.0837028540863,10.2666567248658,139.12594551084));
#128867=CARTESIAN_POINT('Ctrl Pts',(81.1265662505306,10.2286896072184,139.122342222886));
#128868=CARTESIAN_POINT('Ctrl Pts',(81.1754514646162,10.180676770483,139.117857309997));
#128869=CARTESIAN_POINT('Ctrl Pts',(81.1834351897454,10.1726742584859,139.117111984074));
#128870=CARTESIAN_POINT('Ctrl Pts',(81.1957870321312,10.1600387522657,139.115937325167));
#128871=CARTESIAN_POINT('Ctrl Pts',(81.2002112447982,10.155460729518,139.115512165151));
#128872=CARTESIAN_POINT('Ctrl Pts',(81.208023934129,10.1472831440658,139.114753234609));
#128873=CARTESIAN_POINT('Ctrl Pts',(81.2114227823699,10.1436936994349,139.114420270673));
#128874=CARTESIAN_POINT('Ctrl Pts',(81.2195953961233,10.1349854888543,139.113612895331));
#128875=CARTESIAN_POINT('Ctrl Pts',(81.2243528870579,10.1298517573838,139.113137288134));
#128876=CARTESIAN_POINT('Ctrl Pts',(81.2390461532584,10.1137947158913,139.111651255061));
#128877=CARTESIAN_POINT('Ctrl Pts',(81.2488688365197,10.1027695275106,139.110633112279));
#128878=CARTESIAN_POINT('Ctrl Pts',(81.2990113950014,10.0449592768906,139.105312326445));
#128879=CARTESIAN_POINT('Ctrl Pts',(81.3368499205332,9.99609300183868,139.100875849382));
#128880=CARTESIAN_POINT('Ctrl Pts',(81.4570768493695,9.82160117787799,139.08551020595));
#128881=CARTESIAN_POINT('Ctrl Pts',(81.5251832678669,9.68697564742368,139.074523934561));
#128882=CARTESIAN_POINT('Ctrl Pts',(81.5811126946868,9.52542283135678,139.062767708023));
#128883=CARTESIAN_POINT('Ctrl Pts',(81.5875339559354,9.50569013338958,139.061352680344));
#128884=CARTESIAN_POINT('Ctrl Pts',(81.5972297090175,9.47388758510644,139.059104602231));
#128885=CARTESIAN_POINT('Ctrl Pts',(81.6007396985286,9.46189243229859,139.058263982643));
#128886=CARTESIAN_POINT('Ctrl Pts',(81.6067562634227,9.44043845065898,139.056773123634));
#128887=CARTESIAN_POINT('Ctrl Pts',(81.6093150786288,9.43099501572934,139.056121217502));
#128888=CARTESIAN_POINT('Ctrl Pts',(81.6145157169252,9.41110947581618,139.054757292526));
#128889=CARTESIAN_POINT('Ctrl Pts',(81.6171397726104,9.40066315819406,139.054045873163));
#128890=CARTESIAN_POINT('Ctrl Pts',(81.6238285502723,9.37289845794113,139.052167984069));
#128891=CARTESIAN_POINT('Ctrl Pts',(81.6277175965278,9.35553886739058,139.051007158595));
#128892=CARTESIAN_POINT('Ctrl Pts',(81.6467065083611,9.26392297529577,139.044945286787));
#128893=CARTESIAN_POINT('Ctrl Pts',(81.657006347636,9.18875841022886,139.040198916405));
#128894=CARTESIAN_POINT('Ctrl Pts',(81.6692599293877,9.00874863605022,139.029075772722));
#128895=CARTESIAN_POINT('Ctrl Pts',(81.6665149103011,8.90392049647273,139.022797288656));
#128896=CARTESIAN_POINT('Ctrl Pts',(81.6483191537308,8.75340945376733,139.013332909244));
#128897=CARTESIAN_POINT('Ctrl Pts',(81.6407112838855,8.70703492592829,139.010351004561));
#128898=CARTESIAN_POINT('Ctrl Pts',(81.62893935155,8.65038416620291,139.006558974952));
#128899=CARTESIAN_POINT('Ctrl Pts',(81.6266188276171,8.63974201409532,139.005840034976));
#128900=CARTESIAN_POINT('Ctrl Pts',(81.6228116393935,8.62306903299932,139.004702212132));
#128901=CARTESIAN_POINT('Ctrl Pts',(81.621395263543,8.61702223687432,139.004287178101));
#128902=CARTESIAN_POINT('Ctrl Pts',(81.618653519927,8.60560504589117,139.003498785897));
#128903=CARTESIAN_POINT('Ctrl Pts',(81.6173351739051,8.60023315677666,139.003125821843));
#128904=CARTESIAN_POINT('Ctrl Pts',(81.6141412395193,8.58749319333404,139.002236603353));
#128905=CARTESIAN_POINT('Ctrl Pts',(81.6122419339988,8.58013127374146,139.001719031333));
#128906=CARTESIAN_POINT('Ctrl Pts',(81.60562856751,8.55520378179635,138.999954458945));
#128907=CARTESIAN_POINT('Ctrl Pts',(81.6006774725734,8.53770319712688,138.998695230358));
#128908=CARTESIAN_POINT('Ctrl Pts',(81.5877579298106,8.49473497060424,138.995558735837));
#128909=CARTESIAN_POINT('Ctrl Pts',(81.5794623250883,8.46937150563186,138.993668081348));
#128910=CARTESIAN_POINT('Ctrl Pts',(81.5399122156118,8.35760812529544,138.985191840629));
#128911=CARTESIAN_POINT('Ctrl Pts',(81.5021515070241,8.2736822746639,138.978446679774));
#128912=CARTESIAN_POINT('Ctrl Pts',(81.411496417037,8.1098735246819,138.964892067466));
#128913=CARTESIAN_POINT('Ctrl Pts',(81.358244601958,8.03055456833383,138.958116998613));
#128914=CARTESIAN_POINT('Ctrl Pts',(81.2866515207404,7.94149122292979,138.950303546905));
#128915=CARTESIAN_POINT('Ctrl Pts',(81.2745642685879,7.92696740813512,138.949021584936));
#128916=CARTESIAN_POINT('Ctrl Pts',(81.2550477401424,7.90431193354309,138.947008570631));
#128917=CARTESIAN_POINT('Ctrl Pts',(81.2477807341328,7.89604328952335,138.946270974457));
#128918=CARTESIAN_POINT('Ctrl Pts',(81.2345818487011,7.8813220025922,138.944952264514));
#128919=CARTESIAN_POINT('Ctrl Pts',(81.2286800528808,7.87484306174711,138.944369928145));
#128920=CARTESIAN_POINT('Ctrl Pts',(81.2147005736506,7.85973767516507,138.943007385054));
#128921=CARTESIAN_POINT('Ctrl Pts',(81.2065816141077,7.85114993423826,138.94222896933));
#128922=CARTESIAN_POINT('Ctrl Pts',(81.1825296049206,7.8262454305747,138.939959626976));
#128923=CARTESIAN_POINT('Ctrl Pts',(81.1663517042526,7.81016814669137,138.938479352931));
#128924=CARTESIAN_POINT('Ctrl Pts',(81.0901643650076,7.73750236615975,138.931706266261));
#128925=CARTESIAN_POINT('Ctrl Pts',(81.0263323756214,7.68508449802901,138.926588875406));
#128926=CARTESIAN_POINT('Ctrl Pts',(80.9119012339443,7.60454613930618,138.918009272305));
#128927=CARTESIAN_POINT('Ctrl Pts',(80.8632511251667,7.5739380242485,138.914520117631));
#128928=CARTESIAN_POINT('Ctrl Pts',(80.7458212019398,7.50827224107048,138.906263423895));
#128929=CARTESIAN_POINT('Ctrl Pts',(80.67600185028,7.47536255512107,138.901477853062));
#128930=CARTESIAN_POINT('Ctrl Pts',(80.5933465041269,7.44319856504702,138.895676617026));
#128931=CARTESIAN_POINT('Ctrl Pts',(80.5824838966771,7.43910177352648,138.894911563568));
#128932=CARTESIAN_POINT('Ctrl Pts',(80.5655353298124,7.43291123424384,138.893712449777));
#128933=CARTESIAN_POINT('Ctrl Pts',(80.5594783073788,7.43073857209131,138.893282845821));
#128934=CARTESIAN_POINT('Ctrl Pts',(80.5482850922439,7.42679659036717,138.892486715536));
#128935=CARTESIAN_POINT('Ctrl Pts',(80.5431526463564,7.42501723497488,138.892120780624));
#128936=CARTESIAN_POINT('Ctrl Pts',(80.5312107586048,7.42094244348017,138.891267338891));
#128937=CARTESIAN_POINT('Ctrl Pts',(80.524395107462,7.41866594188989,138.890778764549));
#128938=CARTESIAN_POINT('Ctrl Pts',(80.5025736348129,7.41153391817042,138.889210249206));
#128939=CARTESIAN_POINT('Ctrl Pts',(80.4875140137342,7.40684752994001,138.888121364217));
#128940=CARTESIAN_POINT('Ctrl Pts',(80.4039927024236,7.38215167014042,138.882055582529));
#128941=CARTESIAN_POINT('Ctrl Pts',(80.3343728683518,7.36634272133175,138.876903749626));
#128942=CARTESIAN_POINT('Ctrl Pts',(80.1347254798889,7.3343057734282,138.862204453047));
#128943=CARTESIAN_POINT('Ctrl Pts',(80.0034697195409,7.32886632828541,138.852669560682));
#128944=CARTESIAN_POINT('Ctrl Pts',(79.8447127407914,7.34101175452654,138.841651452545));
#128945=CARTESIAN_POINT('Ctrl Pts',(79.8165667005079,7.34388752631555,138.839715470578));
#128946=CARTESIAN_POINT('Ctrl Pts',(79.7759022594195,7.34909186850973,138.836942130089));
#128947=CARTESIAN_POINT('Ctrl Pts',(79.7633171035397,7.3508491039305,138.836087104017));
#128948=CARTESIAN_POINT('Ctrl Pts',(79.7410500895531,7.35421834822134,138.83457978855));
#128949=CARTESIAN_POINT('Ctrl Pts',(79.7313601919956,7.35577222925397,138.833925701665));
#128950=CARTESIAN_POINT('Ctrl Pts',(79.7111656646915,7.35919393370254,138.832566155215));
#128951=CARTESIAN_POINT('Ctrl Pts',(79.7006640824533,7.36107723249207,138.83186121731));
#128952=CARTESIAN_POINT('Ctrl Pts',(79.6731713115377,7.36628071382591,138.830020649792));
#128953=CARTESIAN_POINT('Ctrl Pts',(79.6562122350053,7.36976513750182,138.82889025843));
#128954=CARTESIAN_POINT('Ctrl Pts',(79.5729583094963,7.38822754385139,138.823361087912));
#128955=CARTESIAN_POINT('Ctrl Pts',(79.5075645725196,7.40698900395815,138.819084530675));
#128956=CARTESIAN_POINT('Ctrl Pts',(79.3768020250966,7.45333046446893,138.81049777654));
#128957=CARTESIAN_POINT('Ctrl Pts',(79.3116826741024,7.48119062532437,138.806202147965));
#128958=CARTESIAN_POINT('Ctrl Pts',(79.175671963896,7.54992972835588,138.796878436688));
#128959=CARTESIAN_POINT('Ctrl Pts',(79.1056257332216,7.5920540089126,138.791851628775));
#128960=CARTESIAN_POINT('Ctrl Pts',(79.0260641671065,7.64824035246158,138.785532306932));
#128961=CARTESIAN_POINT('Ctrl Pts',(79.0133012696898,7.65752812970628,138.784498397428));
#128962=CARTESIAN_POINT('Ctrl Pts',(78.9949825298433,7.6712613265876,138.782981736006));
#128963=CARTESIAN_POINT('Ctrl Pts',(78.9893197284526,7.67556353053581,138.782508273499));
#128964=CARTESIAN_POINT('Ctrl Pts',(78.9795158616251,7.68311131662061,138.78168015851));
#128965=CARTESIAN_POINT('Ctrl Pts',(78.975362355064,7.68634046394217,138.781326647072));
#128966=CARTESIAN_POINT('Ctrl Pts',(78.9664098434199,7.69336889268544,138.780558786581));
#128967=CARTESIAN_POINT('Ctrl Pts',(78.9616165386678,7.69717489792751,138.780143986943));
#128968=CARTESIAN_POINT('Ctrl Pts',(78.9487827224328,7.70748108793751,138.779023702781));
#128969=CARTESIAN_POINT('Ctrl Pts',(78.9407817255431,7.71402972962652,138.778314965539));
#128970=CARTESIAN_POINT('Ctrl Pts',(78.9226228123415,7.72917683922673,138.77668365365));
#128971=CARTESIAN_POINT('Ctrl Pts',(78.9125060396484,7.73782332005442,138.775758184024));
#128972=CARTESIAN_POINT('Ctrl Pts',(78.8806777361102,7.76569268247144,138.772796060345));
#128973=CARTESIAN_POINT('Ctrl Pts',(78.8593648579604,7.78536089185063,138.770736390998));
#128974=CARTESIAN_POINT('Ctrl Pts',(78.7593527734994,7.88260952872156,138.760738120544));
#128975=CARTESIAN_POINT('Ctrl Pts',(78.687988437749,7.96733632513103,138.752595624068));
#128976=CARTESIAN_POINT('Ctrl Pts',(78.5836293190767,8.11968798760006,138.739342731608));
#128977=CARTESIAN_POINT('Ctrl Pts',(78.5458489314751,8.18360391158375,138.734124780613));
#128978=CARTESIAN_POINT('Ctrl Pts',(78.5042636115694,8.26606597521267,138.727816668625));
#128979=CARTESIAN_POINT('Ctrl Pts',(78.4963436930611,8.28243170883749,138.726584144183));
#128980=CARTESIAN_POINT('Ctrl Pts',(78.484125129964,8.30877123608531,138.724630503009));
#128981=CARTESIAN_POINT('Ctrl Pts',(78.4796535544265,8.31866269678607,138.723903483568));
#128982=CARTESIAN_POINT('Ctrl Pts',(78.4713436667529,8.3375340274822,138.722528747547));
#128983=CARTESIAN_POINT('Ctrl Pts',(78.4674870295011,8.34650527767667,138.721880428125));
#128984=CARTESIAN_POINT('Ctrl Pts',(78.4588544455196,8.36708303553032,138.720404943349));
#128985=CARTESIAN_POINT('Ctrl Pts',(78.4541302886478,8.37871073252396,138.719579554884));
#128986=CARTESIAN_POINT('Ctrl Pts',(78.4397898314646,8.41518384045414,138.717015504033));
#128987=CARTESIAN_POINT('Ctrl Pts',(78.4306374736656,8.44020798626491,138.715292267821));
#128988=CARTESIAN_POINT('Ctrl Pts',(78.3843189260331,8.57693133839935,138.70604944903));
#128989=CARTESIAN_POINT('Ctrl Pts',(78.358470220905,8.69211092607303,138.698908399452));
#128990=CARTESIAN_POINT('Ctrl Pts',(78.3376286856976,8.87276265300322,138.687793230822));
#128991=CARTESIAN_POINT('Ctrl Pts',(78.3339641330686,8.93682820906066,138.683860303415));
#128992=CARTESIAN_POINT('Ctrl Pts',(78.3340002645793,9.00093892397456,138.679802731044));
#128993=CARTESIAN_POINT('Ctrl Pts',(78.3340002659362,9.00094132848483,138.679802578862));
#128994=CARTESIAN_POINT('Ctrl Pts',(78.3340122909079,9.02222359066603,138.678455621731));
#128995=CARTESIAN_POINT('Ctrl Pts',(78.3344321190674,9.04350288459769,138.677095274952));
#128996=CARTESIAN_POINT('Ctrl Pts',(78.335800952913,9.07868649292419,138.674815057685));
#128997=CARTESIAN_POINT('Ctrl Pts',(78.3365170039007,9.09259764858293,138.673905454353));
#128998=CARTESIAN_POINT('Ctrl Pts',(78.3378248671248,9.11301541109249,138.672556448937));
#128999=CARTESIAN_POINT('Ctrl Pts',(78.3382806780811,9.11953052843225,138.672123902949));
#129000=CARTESIAN_POINT('Ctrl Pts',(78.3391689384659,9.13123767971605,138.671342619596));
#129001=CARTESIAN_POINT('Ctrl Pts',(78.3395874614174,9.13643072747922,138.670994630515));
#129002=CARTESIAN_POINT('Ctrl Pts',(78.3404626584501,9.14668905065455,138.670304239487));
#129003=CARTESIAN_POINT('Ctrl Pts',(78.3409181705115,9.15175423071767,138.669961897786));
#129004=CARTESIAN_POINT('Ctrl Pts',(78.3420395510613,9.16361469313387,138.669156880096));
#129005=CARTESIAN_POINT('Ctrl Pts',(78.3427239992148,9.17040795502056,138.668693200433));
#129006=CARTESIAN_POINT('Ctrl Pts',(78.3449257620241,9.19099146768943,138.667280775185));
#129007=CARTESIAN_POINT('Ctrl Pts',(78.346573550956,9.20476674582777,138.666325333866));
#129008=CARTESIAN_POINT('Ctrl Pts',(78.3545977611215,9.26541513195532,138.662078424901));
#129009=CARTESIAN_POINT('Ctrl Pts',(78.3627964198778,9.31202138374526,138.658708667515));
#129010=CARTESIAN_POINT('Ctrl Pts',(78.3852576384601,9.41404270652216,138.651179346744));
#129011=CARTESIAN_POINT('Ctrl Pts',(78.4004150068948,9.4692034413495,138.647007138059));
#129012=CARTESIAN_POINT('Ctrl Pts',(78.4241525990979,9.54092402435479,138.641512903841));
#129013=CARTESIAN_POINT('Ctrl Pts',(78.4302142694855,9.55827066911257,138.640178362243));
#129014=CARTESIAN_POINT('Ctrl Pts',(78.4365593294404,9.57550783629781,138.638847722432));
#129015=CARTESIAN_POINT('Ctrl Pts',(78.4365593737687,9.57550795672114,138.833737829798));
#129016=CARTESIAN_POINT('Ctrl Pts',(78.4357692491731,9.57336148267508,138.833890538484));
#129017=CARTESIAN_POINT('Ctrl Pts',(78.434983539282,9.57121336600505,138.834043100294));
#129018=CARTESIAN_POINT('Ctrl Pts',(78.4308510841927,9.55984277640087,138.834849266783));
#129019=CARTESIAN_POINT('Ctrl Pts',(78.4275813760033,9.55059234665785,138.835500295248));
#129020=CARTESIAN_POINT('Ctrl Pts',(78.4201928105344,9.52908637313912,138.837003003153));
#129021=CARTESIAN_POINT('Ctrl Pts',(78.4161344814598,9.51681058518315,138.837852660339));
#129022=CARTESIAN_POINT('Ctrl Pts',(78.4035034946116,9.47705698110891,138.840579250395));
#129023=CARTESIAN_POINT('Ctrl Pts',(78.3954995880927,9.44940298378392,138.842437725573));
#129024=CARTESIAN_POINT('Ctrl Pts',(78.3648350198884,9.332159038107,138.850178097835));
#129025=CARTESIAN_POINT('Ctrl Pts',(78.3489306474362,9.24097008691327,138.855849713538));
#129026=CARTESIAN_POINT('Ctrl Pts',(78.3307615371578,9.03852853225636,138.868266132359));
#129027=CARTESIAN_POINT('Ctrl Pts',(78.3318966575602,8.92743470978668,138.874968455501));
#129028=CARTESIAN_POINT('Ctrl Pts',(78.3456509678574,8.80277234630258,138.883123457903));
#129029=CARTESIAN_POINT('Ctrl Pts',(78.3474441632568,8.78827225429018,138.884082046146));
#129030=CARTESIAN_POINT('Ctrl Pts',(78.3503739193868,8.7668941091527,138.885512684605));
#129031=CARTESIAN_POINT('Ctrl Pts',(78.3513633794776,8.7599961431404,138.88597697809));
#129032=CARTESIAN_POINT('Ctrl Pts',(78.3532059284696,8.74770027724662,138.886809706563));
#129033=CARTESIAN_POINT('Ctrl Pts',(78.3540423403343,8.74230008741915,138.887177209765));
#129034=CARTESIAN_POINT('Ctrl Pts',(78.3559503006038,8.73036993477362,138.88799309534));
#129035=CARTESIAN_POINT('Ctrl Pts',(78.3570341766908,8.72384228091856,138.888442131348));
#129036=CARTESIAN_POINT('Ctrl Pts',(78.36033309306,8.70468164012298,138.889767550045));
#129037=CARTESIAN_POINT('Ctrl Pts',(78.362655106246,8.6920679081068,138.890649514557));
#129038=CARTESIAN_POINT('Ctrl Pts',(78.3683523979806,8.66300746293163,138.892701332986));
#129039=CARTESIAN_POINT('Ctrl Pts',(78.3718310932534,8.64658263923721,138.893875797502));
#129040=CARTESIAN_POINT('Ctrl Pts',(78.3846990049891,8.59005486258268,138.897962887116));
#129041=CARTESIAN_POINT('Ctrl Pts',(78.395326260614,8.55025109615191,138.9009192615));
#129042=CARTESIAN_POINT('Ctrl Pts',(78.4439959631655,8.39178014556828,138.912913224673));
#129043=CARTESIAN_POINT('Ctrl Pts',(78.4938274719577,8.27713667223757,138.922065989366));
#129044=CARTESIAN_POINT('Ctrl Pts',(78.5786993296101,8.12963487475271,138.93404814134));
#129045=CARTESIAN_POINT('Ctrl Pts',(78.6030292165121,8.09109716641648,138.937205119208));
#129046=CARTESIAN_POINT('Ctrl Pts',(78.6378754586152,8.0406138443944,138.941378731347));
#129047=CARTESIAN_POINT('Ctrl Pts',(78.6470248568391,8.02775345021318,138.942445514144));
#129048=CARTESIAN_POINT('Ctrl Pts',(78.6624702455775,8.0066837810718,138.944199786827));
#129049=CARTESIAN_POINT('Ctrl Pts',(78.6686622455977,7.99839990675778,138.944891219221));
#129050=CARTESIAN_POINT('Ctrl Pts',(78.6809650325927,7.98225649055595,138.946242297613));
#129051=CARTESIAN_POINT('Ctrl Pts',(78.6870699120153,7.97439301501973,138.946902135934));
#129052=CARTESIAN_POINT('Ctrl Pts',(78.7018142601135,7.95574876994713,138.948471082713));
#129053=CARTESIAN_POINT('Ctrl Pts',(78.7105181515312,7.94501970247346,138.949377584196));
#129054=CARTESIAN_POINT('Ctrl Pts',(78.7412614358887,7.9080722199774,138.95251355375));
#129055=CARTESIAN_POINT('Ctrl Pts',(78.7639759108039,7.88242505387744,138.954715645285));
#129056=CARTESIAN_POINT('Ctrl Pts',(78.822383092881,7.82043786565147,138.960124168288));
#129057=CARTESIAN_POINT('Ctrl Pts',(78.8589819740554,7.78499923645947,138.963294508447));
#129058=CARTESIAN_POINT('Ctrl Pts',(78.9772810613102,7.68051834483437,138.97302113719));
#129059=CARTESIAN_POINT('Ctrl Pts',(79.0640340870432,7.61762839794364,138.979431576538));
#129060=CARTESIAN_POINT('Ctrl Pts',(79.1942384289264,7.54114785047247,138.988881566925));
#129061=CARTESIAN_POINT('Ctrl Pts',(79.2331371563621,7.52033046286871,138.99168777954));
#129062=CARTESIAN_POINT('Ctrl Pts',(79.2824431925521,7.49641002125102,138.995280964287));
#129063=CARTESIAN_POINT('Ctrl Pts',(79.2921190555448,7.49183053013492,138.995987785118));
#129064=CARTESIAN_POINT('Ctrl Pts',(79.3074397010656,7.4847593276703,138.997110660218));
#129065=CARTESIAN_POINT('Ctrl Pts',(79.3130555430832,7.48220509528942,138.997523031445));
#129066=CARTESIAN_POINT('Ctrl Pts',(79.3237446737536,7.47741487222536,138.998309647952));
#129067=CARTESIAN_POINT('Ctrl Pts',(79.3288151011754,7.47517293917561,138.998683531523));
#129068=CARTESIAN_POINT('Ctrl Pts',(79.3409428793794,7.46988274621522,138.999579483106));
#129069=CARTESIAN_POINT('Ctrl Pts',(79.3480102592148,7.46685797439554,139.000102924389));
#129070=CARTESIAN_POINT('Ctrl Pts',(79.3723453572463,7.45664147219591,139.001909224417));
#129071=CARTESIAN_POINT('Ctrl Pts',(79.3897124140637,7.44969200302547,139.003205072442));
#129072=CARTESIAN_POINT('Ctrl Pts',(79.4331066815716,7.43316979192352,139.006453323264));
#129073=CARTESIAN_POINT('Ctrl Pts',(79.4592623958316,7.42395190272819,139.008420277806));
#129074=CARTESIAN_POINT('Ctrl Pts',(79.5681683902661,7.38860089929623,139.016615754553));
#129075=CARTESIAN_POINT('Ctrl Pts',(79.6526673643786,7.3682998958565,139.022979473595));
#129076=CARTESIAN_POINT('Ctrl Pts',(79.8357847192328,7.33918073794056,139.036415851139));
#129077=CARTESIAN_POINT('Ctrl Pts',(79.9344052656145,7.33236972653376,139.043434880908));
#129078=CARTESIAN_POINT('Ctrl Pts',(80.0519278264193,7.33470258459134,139.051471897582));
#129079=CARTESIAN_POINT('Ctrl Pts',(80.0707844850185,7.33539746834601,139.052752046667));
#129080=CARTESIAN_POINT('Ctrl Pts',(80.1006114830504,7.33700440126782,139.054762843428));
#129081=CARTESIAN_POINT('Ctrl Pts',(80.1115910922268,7.33770505923055,139.055500010075));
#129082=CARTESIAN_POINT('Ctrl Pts',(80.1313030568346,7.33915915625824,139.056818279471));
#129083=CARTESIAN_POINT('Ctrl Pts',(80.1400378425088,7.3398728335882,139.057400600822));
#129084=CARTESIAN_POINT('Ctrl Pts',(80.1605431207748,7.34171121201776,139.058763525863));
#129085=CARTESIAN_POINT('Ctrl Pts',(80.1723081792958,7.34289236880078,139.059542334698));
#129086=CARTESIAN_POINT('Ctrl Pts',(80.2067588999614,7.34672193281049,139.061814275838));
#129087=CARTESIAN_POINT('Ctrl Pts',(80.2294044232828,7.34971175169727,139.063296717616));
#129088=CARTESIAN_POINT('Ctrl Pts',(80.3337770024127,7.36568181396698,139.070089013551));
#129089=CARTESIAN_POINT('Ctrl Pts',(80.4145305097773,7.38427422003881,139.075222228073));
#129090=CARTESIAN_POINT('Ctrl Pts',(80.5482693859694,7.42575862916321,139.083806765298));
#129091=CARTESIAN_POINT('Ctrl Pts',(80.6020514041023,7.44553248866636,139.08728534675));
#129092=CARTESIAN_POINT('Ctrl Pts',(80.7254998019522,7.49829003881839,139.095524342095));
#129093=CARTESIAN_POINT('Ctrl Pts',(80.7941004190273,7.53341070020239,139.100302985286));
#129094=CARTESIAN_POINT('Ctrl Pts',(80.8699589936861,7.57913333599058,139.106096369263));
#129095=CARTESIAN_POINT('Ctrl Pts',(80.8798368561949,7.58522870556923,139.106861271032));
#129096=CARTESIAN_POINT('Ctrl Pts',(80.8950892173173,7.59486204170529,139.108060126745));
#129097=CARTESIAN_POINT('Ctrl Pts',(80.9005084941648,7.59832891259672,139.108489625891));
#129098=CARTESIAN_POINT('Ctrl Pts',(80.9105067571738,7.60480701003788,139.109288869155));
#129099=CARTESIAN_POINT('Ctrl Pts',(80.9150911278067,7.60780954652006,139.109658049459));
#129100=CARTESIAN_POINT('Ctrl Pts',(80.9256711350002,7.61481376335306,139.110516319469));
#129101=CARTESIAN_POINT('Ctrl Pts',(80.9316556693983,7.61883177374747,139.111006466169));
#129102=CARTESIAN_POINT('Ctrl Pts',(80.9507727503427,7.63184774057316,139.112586764383));
#129103=CARTESIAN_POINT('Ctrl Pts',(80.9638020164294,7.64099482908725,139.113686056936));
#129104=CARTESIAN_POINT('Ctrl Pts',(81.0357393633405,7.69305264070969,139.119871973738));
#129105=CARTESIAN_POINT('Ctrl Pts',(81.0919083323157,7.73960262617889,139.125140816355));
#129106=CARTESIAN_POINT('Ctrl Pts',(81.2435074045345,7.88299978946355,139.140315999192));
#129107=CARTESIAN_POINT('Ctrl Pts',(81.330409862682,7.98805958431232,139.150195079913));
#129108=CARTESIAN_POINT('Ctrl Pts',(81.4163593328022,8.12247881739747,139.161179912788));
#129109=CARTESIAN_POINT('Ctrl Pts',(81.4286942594245,8.14270775185891,139.162795588655));
#129110=CARTESIAN_POINT('Ctrl Pts',(81.4466923350692,8.17369213335468,139.165215588268));
#129111=CARTESIAN_POINT('Ctrl Pts',(81.4526757449046,8.1842570278951,139.166031378889));
#129112=CARTESIAN_POINT('Ctrl Pts',(81.4632388376915,8.20339312542098,139.167492574988));
#129113=CARTESIAN_POINT('Ctrl Pts',(81.4678599824138,8.2119406826567,139.168139439171));
#129114=CARTESIAN_POINT('Ctrl Pts',(81.4775943503616,8.23032870636824,139.169518874926));
#129115=CARTESIAN_POINT('Ctrl Pts',(81.4826846575776,8.24018082371478,139.170250613835));
#129116=CARTESIAN_POINT('Ctrl Pts',(81.496366277121,8.2673222644671,139.172246988692));
#129117=CARTESIAN_POINT('Ctrl Pts',(81.504756206573,8.28471159065525,139.173504602973));
#129118=CARTESIAN_POINT('Ctrl Pts',(81.560933364796,8.40651220572631,139.182174775952));
#129119=CARTESIAN_POINT('Ctrl Pts',(81.5981184416421,8.51547690452788,139.189202974856));
#129120=CARTESIAN_POINT('Ctrl Pts',(81.6467966474662,8.72762500633572,139.202493444823));
#129121=CARTESIAN_POINT('Ctrl Pts',(81.6604614833694,8.82973781925677,139.208740482576));
#129122=CARTESIAN_POINT('Ctrl Pts',(81.6651844740251,8.94611256066371,139.216305709975));
#129123=CARTESIAN_POINT('Ctrl Pts',(81.6655708385299,8.95978878752331,139.217201853024));
#129124=CARTESIAN_POINT('Ctrl Pts',(81.6658983279396,8.98034968508746,139.218561852008));
#129125=CARTESIAN_POINT('Ctrl Pts',(81.6659652912678,8.98723214651758,139.219019235916));
#129126=CARTESIAN_POINT('Ctrl Pts',(81.6660092905257,8.99968724595585,139.219851157759));
#129127=CARTESIAN_POINT('Ctrl Pts',(81.6660010165673,9.00525981466055,139.220224893772));
#129128=CARTESIAN_POINT('Ctrl Pts',(81.6659260856385,9.01678399480822,139.221001118786));
#129129=CARTESIAN_POINT('Ctrl Pts',(81.6658554929286,9.02273541648955,139.221403804207));
#129130=CARTESIAN_POINT('Ctrl Pts',(81.6655858267819,9.03839440896083,139.222467890329));
#129131=CARTESIAN_POINT('Ctrl Pts',(81.6653337777657,9.04810066860475,139.223132085162));
#129132=CARTESIAN_POINT('Ctrl Pts',(81.6637555761683,9.09355957250443,139.226262758297));
#129133=CARTESIAN_POINT('Ctrl Pts',(81.6613628834445,9.12926309794042,139.228779261488));
#129134=CARTESIAN_POINT('Ctrl Pts',(81.6503915938091,9.23959063454353,139.236681672161));
#129135=CARTESIAN_POINT('Ctrl Pts',(81.6379157083485,9.31373126292154,139.242168142917));
#129136=CARTESIAN_POINT('Ctrl Pts',(81.5953222533608,9.49218671842658,139.255513048377));
#129137=CARTESIAN_POINT('Ctrl Pts',(81.5599330956303,9.5949092957262,139.263299512595));
#129138=CARTESIAN_POINT('Ctrl Pts',(81.5050176944035,9.71486425501044,139.272380687931));
#129139=CARTESIAN_POINT('Ctrl Pts',(81.4947754805915,9.73604043644773,139.2739845395));
#129140=CARTESIAN_POINT('Ctrl Pts',(81.4785835593894,9.76778473759124,139.276391065084));
#129141=CARTESIAN_POINT('Ctrl Pts',(81.4729616380445,9.77851574914366,139.277204991305));
#129142=CARTESIAN_POINT('Ctrl Pts',(81.4626167011207,9.79774867279879,139.278664839818));
#129143=CARTESIAN_POINT('Ctrl Pts',(81.4579353892392,9.80627226606789,139.27931219662));
#129144=CARTESIAN_POINT('Ctrl Pts',(81.4477364844404,9.82446282526617,139.280694826209));
#129145=CARTESIAN_POINT('Ctrl Pts',(81.4421960800286,9.83411651193372,139.281429245587));
#129146=CARTESIAN_POINT('Ctrl Pts',(81.4267025032489,9.86049682182268,139.283438563704));
#129147=CARTESIAN_POINT('Ctrl Pts',(81.4165521173167,9.87710601612858,139.284706303334));
#129148=CARTESIAN_POINT('Ctrl Pts',(81.3469557760927,9.98662650915673,139.293092718759));
#129149=CARTESIAN_POINT('Ctrl Pts',(81.2786983865789,10.0736183654656,139.299861126766));
#129150=CARTESIAN_POINT('Ctrl Pts',(81.1279686121786,10.2307657788421,139.313161309424));
#129151=CARTESIAN_POINT('Ctrl Pts',(81.0462876306508,10.3009124991158,139.319671439941));
#129152=CARTESIAN_POINT('Ctrl Pts',(80.9474605814812,10.3704213160674,139.327523795779));
#129153=CARTESIAN_POINT('Ctrl Pts',(80.9363900032069,10.3780093873317,139.32840326883));
#129154=CARTESIAN_POINT('Ctrl Pts',(80.919554744259,10.3892521854819,139.329742461064));
#129155=CARTESIAN_POINT('Ctrl Pts',(80.9138569989904,10.3930067996752,139.330195998075));
#129156=CARTESIAN_POINT('Ctrl Pts',(80.9034714638576,10.3997593636885,139.331023534536));
#129157=CARTESIAN_POINT('Ctrl Pts',(80.8987913456885,10.4027690751538,139.331396768845));
#129158=CARTESIAN_POINT('Ctrl Pts',(80.8890336025733,10.4089752489483,139.332175763998));
#129159=CARTESIAN_POINT('Ctrl Pts',(80.8839536958779,10.4121677872447,139.332581750743));
#129160=CARTESIAN_POINT('Ctrl Pts',(80.8704576236274,10.4205482294225,139.333661289074));
#129161=CARTESIAN_POINT('Ctrl Pts',(80.862012483487,10.4256886802755,139.334337758768));
#129162=CARTESIAN_POINT('Ctrl Pts',(80.8211143979894,10.4500866147024,139.337616475561));
#129163=CARTESIAN_POINT('Ctrl Pts',(80.7880616347628,10.4683114143862,139.340274218421));
#129164=CARTESIAN_POINT('Ctrl Pts',(80.6803365676113,10.5230241602307,139.348897684124));
#129165=CARTESIAN_POINT('Ctrl Pts',(80.6035426474527,10.5550549722217,139.354981446099));
#129166=CARTESIAN_POINT('Ctrl Pts',(80.4244444872526,10.6144834426629,139.368676281499));
#129167=CARTESIAN_POINT('Ctrl Pts',(80.3212556839463,10.6381428675606,139.376213547164));
#129168=CARTESIAN_POINT('Ctrl Pts',(80.1976987827919,10.6543370055795,139.384734680179));
#129169=CARTESIAN_POINT('Ctrl Pts',(80.1788515345371,10.6564805814864,139.3860216645));
#129170=CARTESIAN_POINT('Ctrl Pts',(80.1489907367143,10.6593611573852,139.388041254577));
#129171=CARTESIAN_POINT('Ctrl Pts',(80.1379999067815,10.6603113340909,139.388780455287));
#129172=CARTESIAN_POINT('Ctrl Pts',(80.1182528024387,10.6618210611349,139.390101387859));
#129173=CARTESIAN_POINT('Ctrl Pts',(80.1095001019975,10.6624207341126,139.390684350556));
#129174=CARTESIAN_POINT('Ctrl Pts',(80.0889468035803,10.6636658695073,139.39204755524));
#129175=CARTESIAN_POINT('Ctrl Pts',(80.077143163462,10.664254969525,139.392826012649));
#129176=CARTESIAN_POINT('Ctrl Pts',(80.042587680798,10.6656111434507,139.39509277293));
#129177=CARTESIAN_POINT('Ctrl Pts',(80.0198246263635,10.6660375916688,139.396570485389));
#129178=CARTESIAN_POINT('Ctrl Pts',(79.9150083711597,10.6658525623273,139.403314013684));
#129179=CARTESIAN_POINT('Ctrl Pts',(79.8330756485913,10.6596466130065,139.408406458951));
#129180=CARTESIAN_POINT('Ctrl Pts',(79.623794575424,10.6281324774774,139.421384618289));
#129181=CARTESIAN_POINT('Ctrl Pts',(79.4983715315212,10.5939588600333,139.429121433734));
#129182=CARTESIAN_POINT('Ctrl Pts',(79.3639637242141,10.5398860845557,139.438528689698));
#129183=CARTESIAN_POINT('Ctrl Pts',(79.3498131381566,10.5339648957099,139.439534061743));
#129184=CARTESIAN_POINT('Ctrl Pts',(79.3292996749242,10.5250463921841,139.441016304928));
#129185=CARTESIAN_POINT('Ctrl Pts',(79.3228703531876,10.5222026347784,139.441484463366));
#129186=CARTESIAN_POINT('Ctrl Pts',(79.3114761846957,10.5170764035241,139.442320883757));
#129187=CARTESIAN_POINT('Ctrl Pts',(79.3065042822255,10.514810069531,139.442688168378));
#129188=CARTESIAN_POINT('Ctrl Pts',(79.2957037759191,10.5098225733702,139.443491175486));
#129189=CARTESIAN_POINT('Ctrl Pts',(79.289879855386,10.5070921508022,139.443927432893));
#129190=CARTESIAN_POINT('Ctrl Pts',(79.2731889810486,10.4991487614854,139.445186779839));
#129191=CARTESIAN_POINT('Ctrl Pts',(79.2623628622817,10.4938516319351,139.446014734336));
#129192=CARTESIAN_POINT('Ctrl Pts',(79.2377359605263,10.4814689287182,139.447922095803));
#129193=CARTESIAN_POINT('Ctrl Pts',(79.2239749092783,10.4743071839206,139.44900534099));
#129194=CARTESIAN_POINT('Ctrl Pts',(79.1781252738224,10.4496256410324,139.452668738487));
#129195=CARTESIAN_POINT('Ctrl Pts',(79.1465151992474,10.4312427889872,139.45528456391));
#129196=CARTESIAN_POINT('Ctrl Pts',(79.0542519521836,10.3734433281636,139.463142569012));
#129197=CARTESIAN_POINT('Ctrl Pts',(78.9955318730438,10.3311009278282,139.4684391669));
#129198=CARTESIAN_POINT('Ctrl Pts',(78.8627301698412,10.2215330967392,139.480926723629));
#129199=CARTESIAN_POINT('Ctrl Pts',(78.7915685120538,10.1511843896484,139.488036808255));
#129200=CARTESIAN_POINT('Ctrl Pts',(78.7151245231262,10.0606588081365,139.49613812222));
#129201=CARTESIAN_POINT('Ctrl Pts',(78.7033602644596,10.0462444951057,139.49740047211));
#129202=CARTESIAN_POINT('Ctrl Pts',(78.685021072553,10.0229895724865,139.499394449581));
#129203=CARTESIAN_POINT('Ctrl Pts',(78.6782884051204,10.0142759561069,139.500132349261));
#129204=CARTESIAN_POINT('Ctrl Pts',(78.6658601359839,9.99785701058727,139.501505879796));
#129205=CARTESIAN_POINT('Ctrl Pts',(78.6601436945794,9.9901681058014,139.502142314505));
#129206=CARTESIAN_POINT('Ctrl Pts',(78.6473754008669,9.9726810427655,139.503574805987));
#129207=CARTESIAN_POINT('Ctrl Pts',(78.6403630241468,9.96285462240757,139.504369310828));
#129208=CARTESIAN_POINT('Ctrl Pts',(78.6195548004498,9.93301545462512,139.506751514334));
#129209=CARTESIAN_POINT('Ctrl Pts',(78.606089124474,9.91277563334462,139.508326707875));
#129210=CARTESIAN_POINT('Ctrl Pts',(78.5759582657796,9.86526416330425,139.511938231557));
#129211=CARTESIAN_POINT('Ctrl Pts',(78.5596250305868,9.8377929747174,139.513962951576));
#129212=CARTESIAN_POINT('Ctrl Pts',(78.5023852446224,9.73489233014485,139.521348469257));
#129213=CARTESIAN_POINT('Ctrl Pts',(78.4665321901734,9.65680612437858,139.526563553791));
#129214=CARTESIAN_POINT('Ctrl Pts',(78.4367543527153,9.57603743440659,139.531820828887));
#129215=CARTESIAN_POINT('Ctrl Pts',(78.4366568293464,9.57577270720414,139.531838058773));
#129216=CARTESIAN_POINT('Ctrl Pts',(78.4365593737676,9.57550795671827,139.531855288841));
#129217=CARTESIAN_POINT('Origin',(80.,9.,141.545925280538));
#129218=CARTESIAN_POINT('',(77.9452506264307,8.99839553228233,139.095925280496));
#129219=CARTESIAN_POINT('Ctrl Pts',(81.252039109102,10.6292316077768,139.54788294617));
#129220=CARTESIAN_POINT('Ctrl Pts',(81.308376489574,10.585937208553,139.54401817761));
#129221=CARTESIAN_POINT('Ctrl Pts',(81.3625557906715,10.539647933612,139.54015340905));
#129222=CARTESIAN_POINT('Ctrl Pts',(81.4142433345909,10.4906083835351,139.53628864049));
#129223=CARTESIAN_POINT('Ctrl Pts',(81.4658662895611,10.4416301134644,139.532428701359));
#129224=CARTESIAN_POINT('Ctrl Pts',(81.5150033221473,10.3899087276083,139.528568762228));
#129225=CARTESIAN_POINT('Ctrl Pts',(81.5613536243118,10.3357291725303,139.524708823097));
#129226=CARTESIAN_POINT('Ctrl Pts',(81.6076723890728,10.2815864819905,139.520851510324));
#129227=CARTESIAN_POINT('Ctrl Pts',(81.6512078703199,10.2249893084108,139.51699419755));
#129228=CARTESIAN_POINT('Ctrl Pts',(81.6916969738153,10.1662585096298,139.513136884777));
#129229=CARTESIAN_POINT('Ctrl Pts',(81.7321720598409,10.1075480436577,139.509280907419));
#129230=CARTESIAN_POINT('Ctrl Pts',(81.7696025861863,10.0467058182288,139.505424930061));
#129231=CARTESIAN_POINT('Ctrl Pts',(81.803767588974,9.98408335392235,139.501568952702));
#129232=CARTESIAN_POINT('Ctrl Pts',(81.8379321816834,9.92146164126539,139.497713021627));
#129233=CARTESIAN_POINT('Ctrl Pts',(81.8688310977455,9.85706015934763,139.493857090552));
#129234=CARTESIAN_POINT('Ctrl Pts',(81.8962891716252,9.79125529386987,139.490001159476));
#129235=CARTESIAN_POINT('Ctrl Pts',(81.9237751105049,9.72538364830441,139.486141315325));
#129236=CARTESIAN_POINT('Ctrl Pts',(81.9478130468575,9.65810622436826,139.482281471174));
#129237=CARTESIAN_POINT('Ctrl Pts',(81.96827621917,9.58981885994765,139.478421627023));
#129238=CARTESIAN_POINT('Ctrl Pts',(81.9887500283614,9.52149599934791,139.474559776502));
#129239=CARTESIAN_POINT('Ctrl Pts',(82.0056452579464,9.45216262510631,139.470697925981));
#129240=CARTESIAN_POINT('Ctrl Pts',(82.0188859469942,9.38222649768085,139.46683607546));
#129241=CARTESIAN_POINT('Ctrl Pts',(82.0321504630082,9.31216451836531,139.462967275438));
#129242=CARTESIAN_POINT('Ctrl Pts',(82.0417472376092,9.2414981013445,139.459098475416));
#129243=CARTESIAN_POINT('Ctrl Pts',(82.0476520961904,9.17064130644974,139.455229675394));
#129244=CARTESIAN_POINT('Ctrl Pts',(82.0520867354107,9.11742676839861,139.452324147332));
#129245=CARTESIAN_POINT('Ctrl Pts',(82.0544401302839,9.06410498148714,139.449418619269));
#129246=CARTESIAN_POINT('Ctrl Pts',(82.0547213515336,9.0108503480071,139.446513091207));
#129247=CARTESIAN_POINT('Ctrl Pts',(82.055095792145,8.93994284176746,139.442644437237));
#129248=CARTESIAN_POINT('Ctrl Pts',(82.0517961788713,8.86887674551251,139.438775783267));
#129249=CARTESIAN_POINT('Ctrl Pts',(82.0448030562872,8.7980643085072,139.434907129298));
#129250=CARTESIAN_POINT('Ctrl Pts',(82.0378203661409,8.72735751048363,139.43104424664));
#129251=CARTESIAN_POINT('Ctrl Pts',(82.0271551512116,8.65690410018162,139.427181363982));
#129252=CARTESIAN_POINT('Ctrl Pts',(82.0128399673072,8.58711644679066,139.423318481324));
#129253=CARTESIAN_POINT('Ctrl Pts',(81.9985416053222,8.517410801587,139.41946013798));
#129254=CARTESIAN_POINT('Ctrl Pts',(81.9806018911152,8.44836983299485,139.415601794635));
#129255=CARTESIAN_POINT('Ctrl Pts',(81.9591049886799,8.3803991560452,139.41174345129));
#129256=CARTESIAN_POINT('Ctrl Pts',(81.9376216542149,8.31247137942159,139.407887543175));
#129257=CARTESIAN_POINT('Ctrl Pts',(81.9125857320053,8.24561301641311,139.404031635059));
#129258=CARTESIAN_POINT('Ctrl Pts',(81.8841317572407,8.18021644084738,139.400175726944));
#129259=CARTESIAN_POINT('Ctrl Pts',(81.8556862171433,8.11483925091596,139.396320961843));
#129260=CARTESIAN_POINT('Ctrl Pts',(81.8238248297509,8.05092343349106,139.392466196742));
#129261=CARTESIAN_POINT('Ctrl Pts',(81.7887303485671,7.98884160359757,139.388611431641));
#129262=CARTESIAN_POINT('Ctrl Pts',(81.7536345237565,7.9267573968403,139.384756518956));
#129263=CARTESIAN_POINT('Ctrl Pts',(81.7153056004407,7.86650773893452,139.380901606272));
#129264=CARTESIAN_POINT('Ctrl Pts',(81.6739715364385,7.80843931850121,139.377046693587));
#129265=CARTESIAN_POINT('Ctrl Pts',(81.6325942197785,7.750310134299,139.373187747058));
#129266=CARTESIAN_POINT('Ctrl Pts',(81.588205767402,7.69436714059467,139.369328800528));
#129267=CARTESIAN_POINT('Ctrl Pts',(81.5410760797314,7.64092602152064,139.365469853998));
#129268=CARTESIAN_POINT('Ctrl Pts',(81.4939197236542,7.58745466270674,139.361608723878));
#129269=CARTESIAN_POINT('Ctrl Pts',(81.4440193845799,7.53648834406992,139.357747593757));
#129270=CARTESIAN_POINT('Ctrl Pts',(81.3916817583935,7.48830576972232,139.353886463636));
#129271=CARTESIAN_POINT('Ctrl Pts',(81.3392525224691,7.44003885847724,139.350018575144));
#129272=CARTESIAN_POINT('Ctrl Pts',(81.2843778562518,7.39456572984455,139.346150686652));
#129273=CARTESIAN_POINT('Ctrl Pts',(81.2273968759229,7.35212425484364,139.34228279816));
#129274=CARTESIAN_POINT('Ctrl Pts',(81.1934998514691,7.32687653696197,139.339981856512));
#129275=CARTESIAN_POINT('Ctrl Pts',(81.1588579921675,7.3027008490532,139.337680914863));
#129276=CARTESIAN_POINT('Ctrl Pts',(81.1235469336721,7.27963961614549,139.335379973215));
#129277=CARTESIAN_POINT('Ctrl Pts',(81.0641694052924,7.24086085759806,139.331510810583));
#129278=CARTESIAN_POINT('Ctrl Pts',(81.0026656047539,7.20508386198724,139.327641647951));
#129279=CARTESIAN_POINT('Ctrl Pts',(80.9393714643523,7.17254854662003,139.323772485319));
#129280=CARTESIAN_POINT('Ctrl Pts',(80.8761716220403,7.14006170364008,139.319909087117));
#129281=CARTESIAN_POINT('Ctrl Pts',(80.8111871629325,7.11080717457016,139.316045688916));
#129282=CARTESIAN_POINT('Ctrl Pts',(80.7447823180106,7.08498123735595,139.312182290714));
#129283=CARTESIAN_POINT('Ctrl Pts',(80.6784553632913,7.05918559292363,139.308323424122));
#129284=CARTESIAN_POINT('Ctrl Pts',(80.6107117826425,7.03681072729491,139.30446455753));
#129285=CARTESIAN_POINT('Ctrl Pts',(80.5419381132986,7.01800589207375,139.300605690939));
#129286=CARTESIAN_POINT('Ctrl Pts',(80.4732077655688,6.99921290231356,139.296749255107));
#129287=CARTESIAN_POINT('Ctrl Pts',(80.4034490839446,6.98398560914946,139.292892819276));
#129288=CARTESIAN_POINT('Ctrl Pts',(80.3330647916101,6.97242376047416,139.289036383445));
#129289=CARTESIAN_POINT('Ctrl Pts',(80.2627012934443,6.96086532760408,139.285181086951));
#129290=CARTESIAN_POINT('Ctrl Pts',(80.1917130305803,6.95297026803838,139.281325790456));
#129291=CARTESIAN_POINT('Ctrl Pts',(80.1205122704267,6.94878710145032,139.277470493961));
#129292=CARTESIAN_POINT('Ctrl Pts',(80.0493087312538,6.94460377159011,139.273615046991));
#129293=CARTESIAN_POINT('Ctrl Pts',(79.9778931633775,6.94413264863522,139.269759600021));
#129294=CARTESIAN_POINT('Ctrl Pts',(79.9066805639685,6.94737021229868,139.265904153051));
#129295=CARTESIAN_POINT('Ctrl Pts',(79.8353934433826,6.95061116394483,139.262044671508));
#129296=CARTESIAN_POINT('Ctrl Pts',(79.7643102015117,6.95756852743989,139.258185189965));
#129297=CARTESIAN_POINT('Ctrl Pts',(79.6938425315846,6.96818672928996,139.254325708422));
#129298=CARTESIAN_POINT('Ctrl Pts',(79.6233349706938,6.9788109419859,139.250464042069));
#129299=CARTESIAN_POINT('Ctrl Pts',(79.5534441515828,6.99310002113018,139.246602375717));
#129300=CARTESIAN_POINT('Ctrl Pts',(79.4845706540003,7.01094742357516,139.242740709364));
#129301=CARTESIAN_POINT('Ctrl Pts',(79.415576689252,7.02882604304938,139.238872288541));
#129302=CARTESIAN_POINT('Ctrl Pts',(79.347604062057,7.05027526577957,139.235003867718));
#129303=CARTESIAN_POINT('Ctrl Pts',(79.2810366293864,7.07513916497426,139.231135446895));
#129304=CARTESIAN_POINT('Ctrl Pts',(79.2415238770009,7.08989774965758,139.228839249671));
#129305=CARTESIAN_POINT('Ctrl Pts',(79.2025058255676,7.105858512454,139.226543052447));
#129306=CARTESIAN_POINT('Ctrl Pts',(79.1640586578012,7.1229811841905,139.224246855223));
#129307=CARTESIAN_POINT('Ctrl Pts',(79.099274330323,7.15183326452633,139.220377712148));
#129308=CARTESIAN_POINT('Ctrl Pts',(79.035858638409,7.18409976696277,139.216508569073));
#129309=CARTESIAN_POINT('Ctrl Pts',(78.9741953434853,7.21962858673456,139.212639425999));
#129310=CARTESIAN_POINT('Ctrl Pts',(78.9126238999133,7.25510448409725,139.208776046255));
#129311=CARTESIAN_POINT('Ctrl Pts',(78.8528000894136,7.29383281241874,139.204912666512));
#129312=CARTESIAN_POINT('Ctrl Pts',(78.7950863585028,7.33561402342066,139.201049286769));
#129313=CARTESIAN_POINT('Ctrl Pts',(78.7374402978417,7.37734624530099,139.197190436899));
#129314=CARTESIAN_POINT('Ctrl Pts',(78.6818997939348,7.42212395618128,139.193331587029));
#129315=CARTESIAN_POINT('Ctrl Pts',(78.6287998828478,7.46970336169033,139.189472737159));
#129316=CARTESIAN_POINT('Ctrl Pts',(78.5757334054558,7.51725280942168,139.185616316965));
#129317=CARTESIAN_POINT('Ctrl Pts',(78.5251048330378,7.56760012852479,139.181759896771));
#129318=CARTESIAN_POINT('Ctrl Pts',(78.4772163901747,7.62046107697261,139.177903476578));
#129319=CARTESIAN_POINT('Ctrl Pts',(78.4293420816255,7.67330642346745,139.17404819461));
#129320=CARTESIAN_POINT('Ctrl Pts',(78.3842066229932,7.72866356662089,139.170192912642));
#129321=CARTESIAN_POINT('Ctrl Pts',(78.342074376256,7.78621246149379,139.166337630674));
#129322=CARTESIAN_POINT('Ctrl Pts',(78.2999404726191,7.84376361954402,139.162482197093));
#129323=CARTESIAN_POINT('Ctrl Pts',(78.2608103005342,7.90350630718624,139.158626763511));
#129324=CARTESIAN_POINT('Ctrl Pts',(78.2249059814435,7.96508996150155,139.15477132993));
#129325=CARTESIAN_POINT('Ctrl Pts',(78.1889640725758,8.02673809039502,139.150911859929));
#129326=CARTESIAN_POINT('Ctrl Pts',(78.1562550036814,8.0902306129459,139.147052389928));
#129327=CARTESIAN_POINT('Ctrl Pts',(78.1269553721447,8.15519151012636,139.143192919928));
#129328=CARTESIAN_POINT('Ctrl Pts',(78.0976391465839,8.22018919830535,139.139331264092));
#129329=CARTESIAN_POINT('Ctrl Pts',(78.0717363787881,8.28665646379498,139.135469608257));
#129330=CARTESIAN_POINT('Ctrl Pts',(78.0493748166742,8.35419898058668,139.131607952422));
#129331=CARTESIAN_POINT('Ctrl Pts',(78.0269741315431,8.42185966743443,139.127739540368));
#129332=CARTESIAN_POINT('Ctrl Pts',(78.0081271502149,8.49059889287508,139.123871128313));
#129333=CARTESIAN_POINT('Ctrl Pts',(77.9929110614074,8.56000959660532,139.120002716258));
#129334=CARTESIAN_POINT('Ctrl Pts',(77.9838786457656,8.60121245326676,139.117706389916));
#129335=CARTESIAN_POINT('Ctrl Pts',(77.9761246713115,8.64265175206147,139.115410063574));
#129336=CARTESIAN_POINT('Ctrl Pts',(77.969656625911,8.68424163385155,139.113113737232));
#129337=CARTESIAN_POINT('Ctrl Pts',(77.9535184263551,8.78801112993064,139.107384251667));
#129338=CARTESIAN_POINT('Ctrl Pts',(77.945332887455,8.89304862793086,139.101654766102));
#129339=CARTESIAN_POINT('Ctrl Pts',(77.9452506264313,8.99839553151457,139.095925280538));
#129340=CARTESIAN_POINT('Ctrl Pts',(77.9452506264307,8.99839553228234,139.095925280496));
#129341=CARTESIAN_POINT('Ctrl Pts',(77.9451944260658,9.07036810192396,139.092010919611));
#129342=CARTESIAN_POINT('Ctrl Pts',(77.9489244685222,9.14248040213294,139.088096558725));
#129343=CARTESIAN_POINT('Ctrl Pts',(77.9564551529768,9.21429423861822,139.084182197839));
#129344=CARTESIAN_POINT('Ctrl Pts',(77.9637702775113,9.28405246051092,139.080379882456));
#129345=CARTESIAN_POINT('Ctrl Pts',(77.9746713409255,9.35352853614584,139.076577567072));
#129346=CARTESIAN_POINT('Ctrl Pts',(77.9891188245793,9.42232032965372,139.072775251688));
#129347=CARTESIAN_POINT('Ctrl Pts',(78.0035569315878,9.49106747619983,139.068975404067));
#129348=CARTESIAN_POINT('Ctrl Pts',(78.0215367938635,9.55913073138864,139.065175556447));
#129349=CARTESIAN_POINT('Ctrl Pts',(78.0429674069959,9.62611579793157,139.061375708826));
#129350=CARTESIAN_POINT('Ctrl Pts',(78.0643917765798,9.69308134919031,139.057576968244));
#129351=CARTESIAN_POINT('Ctrl Pts',(78.0892647496713,9.7589688576028,139.053778227663));
#129352=CARTESIAN_POINT('Ctrl Pts',(78.1174453497669,9.82339878029161,139.049979487081));
#129353=CARTESIAN_POINT('Ctrl Pts',(78.1456278187924,9.88783297595597,139.046180494568));
#129354=CARTESIAN_POINT('Ctrl Pts',(78.1771181457956,9.95080893608708,139.042381502055));
#129355=CARTESIAN_POINT('Ctrl Pts',(78.2117278458989,10.0119685100668,139.038582509542));
#129356=CARTESIAN_POINT('Ctrl Pts',(78.2463733803406,10.0731914077059,139.034779583612));
#129357=CARTESIAN_POINT('Ctrl Pts',(78.2841444807975,10.1325937320322,139.030976657682));
#129358=CARTESIAN_POINT('Ctrl Pts',(78.3248080790415,10.1898443555589,139.027173731752));
#129359=CARTESIAN_POINT('Ctrl Pts',(78.3654974050552,10.2471312014299,139.023368399719));
#129360=CARTESIAN_POINT('Ctrl Pts',(78.4090825547568,10.3022632485942,139.019563067687));
#129361=CARTESIAN_POINT('Ctrl Pts',(78.4552905435339,10.3549428982818,139.015757735654));
#129362=CARTESIAN_POINT('Ctrl Pts',(78.5015729540876,10.4077073928896,139.01194627482));
#129363=CARTESIAN_POINT('Ctrl Pts',(78.5504862746083,10.4580112600147,139.008134813986));
#129364=CARTESIAN_POINT('Ctrl Pts',(78.6017220180081,10.5055949812539,139.004323353152));
#129365=CARTESIAN_POINT('Ctrl Pts',(78.6122194553207,10.5153441738616,139.003542441848));
#129366=CARTESIAN_POINT('Ctrl Pts',(78.6228142801158,10.5249793218239,139.002761530544));
#129367=CARTESIAN_POINT('Ctrl Pts',(78.6335036861555,10.5344984153623,139.001980619241));
#129368=CARTESIAN_POINT('Ctrl Pts',(78.6864653127342,10.5816616230727,138.998111523736));
#129369=CARTESIAN_POINT('Ctrl Pts',(78.7419752160566,10.6261721083391,138.994242428231));
#129370=CARTESIAN_POINT('Ctrl Pts',(78.7997368188016,10.6677427434588,138.990373332726));
#129371=CARTESIAN_POINT('Ctrl Pts',(78.8574123613961,10.7092514416698,138.986510001863));
#129372=CARTESIAN_POINT('Ctrl Pts',(78.9173325530523,10.7478287027422,138.982646671));
#129373=CARTESIAN_POINT('Ctrl Pts',(78.9791663518893,10.7832263528181,138.978783340137));
#129374=CARTESIAN_POINT('Ctrl Pts',(79.0409276212815,10.8185824823672,138.974924540861));
#129375=CARTESIAN_POINT('Ctrl Pts',(79.1045976197542,10.8507661690005,138.971065741585));
#129376=CARTESIAN_POINT('Ctrl Pts',(79.1698162641529,10.8795724320267,138.967206942309));
#129377=CARTESIAN_POINT('Ctrl Pts',(79.2349938264751,10.9083605496114,138.963350573741));
#129378=CARTESIAN_POINT('Ctrl Pts',(79.3017176560076,10.9337752686773,138.959494205173));
#129379=CARTESIAN_POINT('Ctrl Pts',(79.3696043132128,10.9556581604616,138.955637836605));
#129380=CARTESIAN_POINT('Ctrl Pts',(79.4374709165253,10.9775345879836,138.951782607218));
#129381=CARTESIAN_POINT('Ctrl Pts',(79.5064992034623,10.9958811105306,138.947927377831));
#129382=CARTESIAN_POINT('Ctrl Pts',(79.5762886904272,11.0105885428501,138.944072148445));
#129383=CARTESIAN_POINT('Ctrl Pts',(79.6460809060418,11.0252965502051,138.940216768325));
#129384=CARTESIAN_POINT('Ctrl Pts',(79.7166339049791,11.0363650868325,138.936361388205));
#129385=CARTESIAN_POINT('Ctrl Pts',(79.7875367782694,11.0437360254964,138.932506008086));
#129386=CARTESIAN_POINT('Ctrl Pts',(79.8585138657824,11.0511146793411,138.92864659253));
#129387=CARTESIAN_POINT('Ctrl Pts',(79.9298410745291,11.054787958932,138.924787176974));
#129388=CARTESIAN_POINT('Ctrl Pts',(80.0011030351522,11.0547497039332,138.920927761417));
#129389=CARTESIAN_POINT('Ctrl Pts',(80.0724053442286,11.0547114272744,138.917066160664));
#129390=CARTESIAN_POINT('Ctrl Pts',(80.1436418463023,11.050957458227,138.91320455991));
#129391=CARTESIAN_POINT('Ctrl Pts',(80.2144005959293,11.0435336911745,138.909342959157));
#129392=CARTESIAN_POINT('Ctrl Pts',(80.2852831367737,11.036096936369,138.905474602599));
#129393=CARTESIAN_POINT('Ctrl Pts',(80.35568577645,11.0249776411575,138.901606246042));
#129394=CARTESIAN_POINT('Ctrl Pts',(80.4252057760271,11.010273018904,138.897737889484));
#129395=CARTESIAN_POINT('Ctrl Pts',(80.4664825456352,11.0015423038777,138.895441093406));
#129396=CARTESIAN_POINT('Ctrl Pts',(80.5074484132099,10.9915486326406,138.893144297327));
#129397=CARTESIAN_POINT('Ctrl Pts',(80.5480219975128,10.9803205429278,138.890847501249));
#129398=CARTESIAN_POINT('Ctrl Pts',(80.6163512059331,10.9614115287177,138.886979510273));
#129399=CARTESIAN_POINT('Ctrl Pts',(80.683834395631,10.9389248833565,138.883111519298));
#129400=CARTESIAN_POINT('Ctrl Pts',(80.7500698252355,10.912953951294,138.879243528322));
#129401=CARTESIAN_POINT('Ctrl Pts',(80.8162190583714,10.8870168168929,138.875380571014));
#129402=CARTESIAN_POINT('Ctrl Pts',(80.8811233031021,10.8576045624471,138.871517613707));
#129403=CARTESIAN_POINT('Ctrl Pts',(80.9443946159635,10.8248606444984,138.867654656399));
#129404=CARTESIAN_POINT('Ctrl Pts',(81.0075967032803,10.792152551878,138.863795925577));
#129405=CARTESIAN_POINT('Ctrl Pts',(81.0691689765495,10.756120254855,138.859937194756));
#129406=CARTESIAN_POINT('Ctrl Pts',(81.1287439325178,10.7169550656043,138.856078463934));
#129407=CARTESIAN_POINT('Ctrl Pts',(81.1708819759179,10.6892530821518,138.853349139771));
#129408=CARTESIAN_POINT('Ctrl Pts',(81.2120211744178,10.6599847671502,138.850619815608));
#129409=CARTESIAN_POINT('Ctrl Pts',(81.252039109102,10.6292316077768,138.847890491445));
#129410=CARTESIAN_POINT('',(77.9452503313537,9.00116691815225,139.154074719413));
#129411=CARTESIAN_POINT('Ctrl Pts',(77.9452503313537,9.00116691815225,139.154074719413));
#129412=CARTESIAN_POINT('Ctrl Pts',(77.9452955388611,9.08076985405426,139.14977731915));
#129413=CARTESIAN_POINT('Ctrl Pts',(77.9499707053658,9.16020567409785,139.145479918886));
#129414=CARTESIAN_POINT('Ctrl Pts',(77.9591932169553,9.23896702027448,139.141182518622));
#129415=CARTESIAN_POINT('Ctrl Pts',(77.9684534953407,9.31805089938046,139.13686752022));
#129416=CARTESIAN_POINT('Ctrl Pts',(77.9822983014852,9.39645450913027,139.132552521817));
#129417=CARTESIAN_POINT('Ctrl Pts',(78.0005942531386,9.47368156172441,139.128237523415));
#129418=CARTESIAN_POINT('Ctrl Pts',(78.0189841187588,9.55130502435452,139.123900375926));
#129419=CARTESIAN_POINT('Ctrl Pts',(78.0418708061259,9.62773956819543,139.119563228437));
#129420=CARTESIAN_POINT('Ctrl Pts',(78.0690707642039,9.70250256145301,139.115226080948));
#129421=CARTESIAN_POINT('Ctrl Pts',(78.0780409992218,9.72715854137151,139.113795739321));
#129422=CARTESIAN_POINT('Ctrl Pts',(78.0874799697398,9.75163291047114,139.112365397694));
#129423=CARTESIAN_POINT('Ctrl Pts',(78.0973799933312,9.7759089332671,139.110935056068));
#129424=CARTESIAN_POINT('Ctrl Pts',(78.124160171027,9.84157708023847,139.107065893275));
#129425=CARTESIAN_POINT('Ctrl Pts',(78.1543965410821,9.90598572302029,139.103196730482));
#129426=CARTESIAN_POINT('Ctrl Pts',(78.1879492665976,9.96874645912945,139.099327567689));
#129427=CARTESIAN_POINT('Ctrl Pts',(78.2214520039649,10.0314136918665,139.095464169324));
#129428=CARTESIAN_POINT('Ctrl Pts',(78.2582610622044,10.0924374663779,139.09160077096));
#129429=CARTESIAN_POINT('Ctrl Pts',(78.2981885076497,10.151449176909,139.087737372595));
#129430=CARTESIAN_POINT('Ctrl Pts',(78.3380691198323,10.2103916691139,139.083878505839));
#129431=CARTESIAN_POINT('Ctrl Pts',(78.381060582807,10.2673263848709,139.080019639083));
#129432=CARTESIAN_POINT('Ctrl Pts',(78.4269298683473,10.3219107093152,139.076160772327));
#129433=CARTESIAN_POINT('Ctrl Pts',(78.4727702601167,10.3764606502512,139.072304336331));
#129434=CARTESIAN_POINT('Ctrl Pts',(78.5214845661371,10.428662766255,139.068447900334));
#129435=CARTESIAN_POINT('Ctrl Pts',(78.5727982883753,10.4782059521039,139.064591464338));
#129436=CARTESIAN_POINT('Ctrl Pts',(78.6240968506186,10.5277345010408,139.060736167677));
#129437=CARTESIAN_POINT('Ctrl Pts',(78.6779929551842,10.5746053421367,139.056880871016));
#129438=CARTESIAN_POINT('Ctrl Pts',(78.7341751160657,10.6185440759253,139.053025574356));
#129439=CARTESIAN_POINT('Ctrl Pts',(78.7903594697857,10.6624845246806,139.049170127219));
#129440=CARTESIAN_POINT('Ctrl Pts',(78.8488296729757,10.703492341401,139.045314680083));
#129441=CARTESIAN_POINT('Ctrl Pts',(78.9092423947348,10.7413343760048,139.041459232947));
#129442=CARTESIAN_POINT('Ctrl Pts',(78.9697183360146,10.7792160107991,139.037599751238));
#129443=CARTESIAN_POINT('Ctrl Pts',(79.0321404412179,10.8139249918597,139.033740269529));
#129444=CARTESIAN_POINT('Ctrl Pts',(79.0961384896395,10.8452728612833,139.029880787819));
#129445=CARTESIAN_POINT('Ctrl Pts',(79.1601727666421,10.876638476386,139.026019121301));
#129446=CARTESIAN_POINT('Ctrl Pts',(79.225784315823,10.90463900142,139.022157454782));
#129447=CARTESIAN_POINT('Ctrl Pts',(79.292583066205,10.9291342214268,139.018295788264));
#129448=CARTESIAN_POINT('Ctrl Pts',(79.3594986547597,10.9536722861984,139.014427367277));
#129449=CARTESIAN_POINT('Ctrl Pts',(79.4276051260904,10.9746926616106,139.010558946289));
#129450=CARTESIAN_POINT('Ctrl Pts',(79.4964980746094,10.9921052616837,139.006690525302));
#129451=CARTESIAN_POINT('Ctrl Pts',(79.537391166539,11.0024409356653,139.00439432956));
#129452=CARTESIAN_POINT('Ctrl Pts',(79.5785611590264,11.0115064588851,139.002098133818));
#129453=CARTESIAN_POINT('Ctrl Pts',(79.6199224885441,11.019291620293,138.999801938076));
#129454=CARTESIAN_POINT('Ctrl Pts',(79.6902200525406,11.0325232520775,138.995899332212));
#129455=CARTESIAN_POINT('Ctrl Pts',(79.7613482215346,11.0421057287759,138.991996726347));
#129456=CARTESIAN_POINT('Ctrl Pts',(79.8328942551689,11.0479436595142,138.988094120483));
#129457=CARTESIAN_POINT('Ctrl Pts',(79.9037074285486,11.0537217911667,138.984231489787));
#129458=CARTESIAN_POINT('Ctrl Pts',(79.9749294555231,11.0558316564894,138.980368859091));
#129459=CARTESIAN_POINT('Ctrl Pts',(80.0461489025551,11.0542316912396,138.976506228395));
#129460=CARTESIAN_POINT('Ctrl Pts',(80.1172967791412,11.0526333338403,138.972647479366));
#129461=CARTESIAN_POINT('Ctrl Pts',(80.1884415979034,11.0473325536336,138.968788730337));
#129462=CARTESIAN_POINT('Ctrl Pts',(80.2591691586792,11.0383397434406,138.964929981309));
#129463=CARTESIAN_POINT('Ctrl Pts',(80.3298493032757,11.0293529620813,138.961073819208));
#129464=CARTESIAN_POINT('Ctrl Pts',(80.4001122645271,11.0166791252986,138.957217657108));
#129465=CARTESIAN_POINT('Ctrl Pts',(80.4695479341675,11.0003805388023,138.953361495008));
#129466=CARTESIAN_POINT('Ctrl Pts',(80.5404063396775,10.9837479945037,138.949426320201));
#129467=CARTESIAN_POINT('Ctrl Pts',(80.610402653991,10.963340553779,138.945491145395));
#129468=CARTESIAN_POINT('Ctrl Pts',(80.6791123406911,10.9392792452922,138.941555970589));
#129469=CARTESIAN_POINT('Ctrl Pts',(80.7464442646084,10.9157004128132,138.937699703687));
#129470=CARTESIAN_POINT('Ctrl Pts',(80.8125402314606,10.8886131173241,138.933843436786));
#129471=CARTESIAN_POINT('Ctrl Pts',(80.8770185180608,10.858180852737,138.929987169884));
#129472=CARTESIAN_POINT('Ctrl Pts',(80.9434758610669,10.8268145191578,138.926012541126));
#129473=CARTESIAN_POINT('Ctrl Pts',(81.0082140877077,10.7918947337507,138.922037912367));
#129474=CARTESIAN_POINT('Ctrl Pts',(81.0708422964889,10.7536517152931,138.918063283609));
#129475=CARTESIAN_POINT('Ctrl Pts',(81.1334705052701,10.7154086968354,138.91408865485));
#129476=CARTESIAN_POINT('Ctrl Pts',(81.1939882498678,10.6738427887355,138.910114026092));
#129477=CARTESIAN_POINT('Ctrl Pts',(81.252039109102,10.6292316077768,138.906139397334));
#129478=CARTESIAN_POINT('Ctrl Pts',(81.252039109102,10.6292316077768,139.606097362941));
#129479=CARTESIAN_POINT('Ctrl Pts',(81.3086788770668,10.5857048284755,139.602235197034));
#129480=CARTESIAN_POINT('Ctrl Pts',(81.3630354755369,10.5392292635521,139.598373031127));
#129481=CARTESIAN_POINT('Ctrl Pts',(81.4147982656329,10.4900816857012,139.59451086522));
#129482=CARTESIAN_POINT('Ctrl Pts',(81.4666182581804,10.4408797954392,139.590644431278));
#129483=CARTESIAN_POINT('Ctrl Pts',(81.5158383714577,10.3890003342646,139.586777997337));
#129484=CARTESIAN_POINT('Ctrl Pts',(81.5621848102927,10.3347569745054,139.582911563396));
#129485=CARTESIAN_POINT('Ctrl Pts',(81.6085609745073,10.2804788244905,139.579042649626));
#129486=CARTESIAN_POINT('Ctrl Pts',(81.6520595018109,10.2238341424132,139.575173735856));
#129487=CARTESIAN_POINT('Ctrl Pts',(81.6924485552715,10.1651675631683,139.571304822086));
#129488=CARTESIAN_POINT('Ctrl Pts',(81.7329055244302,10.1064023338847,139.567429402594));
#129489=CARTESIAN_POINT('Ctrl Pts',(81.7702423334845,10.0456088350746,139.563553983102));
#129490=CARTESIAN_POINT('Ctrl Pts',(81.8042723260695,9.98315763531587,139.559678563609));
#129491=CARTESIAN_POINT('Ctrl Pts',(81.8165980033016,9.96053778522156,139.558274885084));
#129492=CARTESIAN_POINT('Ctrl Pts',(81.8284903174524,9.93770065997237,139.556871206559));
#129493=CARTESIAN_POINT('Ctrl Pts',(81.8399419722473,9.91466447469142,139.555467528034));
#129494=CARTESIAN_POINT('Ctrl Pts',(81.8714784485882,9.85122559838008,139.551601966646));
#129495=CARTESIAN_POINT('Ctrl Pts',(81.8997929813764,9.78602736127449,139.547736405259));
#129496=CARTESIAN_POINT('Ctrl Pts',(81.9246862993926,9.71943047713488,139.543870843871));
#129497=CARTESIAN_POINT('Ctrl Pts',(81.9495421673408,9.65293378284705,139.540011097921));
#129498=CARTESIAN_POINT('Ctrl Pts',(81.9709868673624,9.58504307011365,139.536151351971));
#129499=CARTESIAN_POINT('Ctrl Pts',(81.988867730239,9.51614214526027,139.532291606022));
#129500=CARTESIAN_POINT('Ctrl Pts',(82.0067273304742,9.44732315245196,139.528436449805));
#129501=CARTESIAN_POINT('Ctrl Pts',(82.021031389321,9.37749680239563,139.524581293589));
#129502=CARTESIAN_POINT('Ctrl Pts',(82.0316765211828,9.30706363473175,139.520726137372));
#129503=CARTESIAN_POINT('Ctrl Pts',(82.0423148473879,9.23667549647311,139.516873445838));
#129504=CARTESIAN_POINT('Ctrl Pts',(82.0492988146928,9.16568179040966,139.513020754304));
#129505=CARTESIAN_POINT('Ctrl Pts',(82.0525760781977,9.0944934162287,139.50916806277));
#129506=CARTESIAN_POINT('Ctrl Pts',(82.0558523483818,9.02332661885882,139.505316538966));
#129507=CARTESIAN_POINT('Ctrl Pts',(82.0554241226374,8.95196575651897,139.501465015162));
#129508=CARTESIAN_POINT('Ctrl Pts',(82.0512910442517,8.88082527838157,139.497613491358));
#129509=CARTESIAN_POINT('Ctrl Pts',(82.0471578289629,8.80968244380407,139.493761839977));
#129510=CARTESIAN_POINT('Ctrl Pts',(82.0393195478422,8.73876049378837,139.489910188596));
#129511=CARTESIAN_POINT('Ctrl Pts',(82.027827849291,8.66847055011675,139.486058537215));
#129512=CARTESIAN_POINT('Ctrl Pts',(82.0163241399483,8.59810714142592,139.482202860199));
#129513=CARTESIAN_POINT('Ctrl Pts',(82.0011594693797,8.5283775391265,139.478347183183));
#129514=CARTESIAN_POINT('Ctrl Pts',(81.9824368025165,8.45968353113359,139.474491506167));
#129515=CARTESIAN_POINT('Ctrl Pts',(81.9637035792248,8.3909507912984,139.470633655199));
#129516=CARTESIAN_POINT('Ctrl Pts',(81.9414085186979,8.32325527066213,139.466775804232));
#129517=CARTESIAN_POINT('Ctrl Pts',(81.9157039132598,8.25698177732901,139.462917953264));
#129518=CARTESIAN_POINT('Ctrl Pts',(81.8899541416765,8.19059183333773,139.459053323579));
#129519=CARTESIAN_POINT('Ctrl Pts',(81.8607830636398,8.12562934949478,139.455188693893));
#129520=CARTESIAN_POINT('Ctrl Pts',(81.8283900679697,8.06245676267714,139.451324064208));
#129521=CARTESIAN_POINT('Ctrl Pts',(81.8088611733903,8.02437165314194,139.448994179486));
#129522=CARTESIAN_POINT('Ctrl Pts',(81.7881621302068,7.98693659210319,139.446664294764));
#129523=CARTESIAN_POINT('Ctrl Pts',(81.7663441375903,7.95022576231819,139.444334410042));
#129524=CARTESIAN_POINT('Ctrl Pts',(81.7301084889346,7.88925586681367,139.440464902628));
#129525=CARTESIAN_POINT('Ctrl Pts',(81.6906414303863,7.83004501603826,139.436595395214));
#129526=CARTESIAN_POINT('Ctrl Pts',(81.6481389612067,7.77295659121104,139.432725887799));
#129527=CARTESIAN_POINT('Ctrl Pts',(81.6056998333134,7.71595324507047,139.428862147099));
#129528=CARTESIAN_POINT('Ctrl Pts',(81.5602345618575,7.66106643266508,139.424998406399));
#129529=CARTESIAN_POINT('Ctrl Pts',(81.5119837693341,7.60863281490103,139.421134665698));
#129530=CARTESIAN_POINT('Ctrl Pts',(81.4637896323175,7.55626076406748,139.417275461756));
#129531=CARTESIAN_POINT('Ctrl Pts',(81.4128167983318,7.50633654178831,139.413416257814));
#129532=CARTESIAN_POINT('Ctrl Pts',(81.3593466245471,7.45916440953868,139.409557053872));
#129533=CARTESIAN_POINT('Ctrl Pts',(81.3059101763189,7.41202203044485,139.405700284068));
#129534=CARTESIAN_POINT('Ctrl Pts',(81.2499798767448,7.36762861800326,139.401843514265));
#129535=CARTESIAN_POINT('Ctrl Pts',(81.1918734150042,7.32625111647348,139.397986744461));
#129536=CARTESIAN_POINT('Ctrl Pts',(81.133784177304,7.2848858801503,139.394131117889));
#129537=CARTESIAN_POINT('Ctrl Pts',(81.0735204534658,7.24653506147924,139.390275491317));
#129538=CARTESIAN_POINT('Ctrl Pts',(81.0114310621613,7.21142381515487,139.386419864745));
#129539=CARTESIAN_POINT('Ctrl Pts',(80.9493393188025,7.17631123875524,139.382564092116));
#129540=CARTESIAN_POINT('Ctrl Pts',(80.8854221945011,7.14443871549472,139.378708319486));
#129541=CARTESIAN_POINT('Ctrl Pts',(80.8200538780584,7.11598588126802,139.374852546856));
#129542=CARTESIAN_POINT('Ctrl Pts',(80.7546173158675,7.08750334174889,139.370992748728));
#129543=CARTESIAN_POINT('Ctrl Pts',(80.6877269833174,7.06244781247504,139.367132950599));
#129544=CARTESIAN_POINT('Ctrl Pts',(80.6197770282117,7.04095074135409,139.363273152471));
#129545=CARTESIAN_POINT('Ctrl Pts',(80.5517886923445,7.01944152785635,139.359411174179));
#129546=CARTESIAN_POINT('Ctrl Pts',(80.482740012711,7.00149489601355,139.355549195887));
#129547=CARTESIAN_POINT('Ctrl Pts',(80.41303761036,6.98719163979078,139.351687217595));
#129548=CARTESIAN_POINT('Ctrl Pts',(80.3432134959739,6.97286340769394,139.347818495644));
#129549=CARTESIAN_POINT('Ctrl Pts',(80.2727338601499,6.96219132580645,139.343949773694));
#129550=CARTESIAN_POINT('Ctrl Pts',(80.2020120623991,6.95520448720532,139.340081051743));
#129551=CARTESIAN_POINT('Ctrl Pts',(80.1600904683361,6.9510629152864,139.337787798512));
#129552=CARTESIAN_POINT('Ctrl Pts',(80.1180838367506,6.94821524382756,139.335494545281));
#129553=CARTESIAN_POINT('Ctrl Pts',(80.0760779629691,6.94665889193966,139.333201292051));
#129554=CARTESIAN_POINT('Ctrl Pts',(80.0051960461625,6.94403265910342,139.329331590743));
#129555=CARTESIAN_POINT('Ctrl Pts',(79.934039667594,6.94507590474726,139.325461889435));
#129556=CARTESIAN_POINT('Ctrl Pts',(79.8630204812265,6.94982094100623,139.321592188127));
#129557=CARTESIAN_POINT('Ctrl Pts',(79.7921068482023,6.95455892488306,139.317728238222));
#129558=CARTESIAN_POINT('Ctrl Pts',(79.7213304832265,6.96298774612134,139.313864288316));
#129559=CARTESIAN_POINT('Ctrl Pts',(79.6511047769023,6.97508773380188,139.310000338411));
#129560=CARTESIAN_POINT('Ctrl Pts',(79.5809611270469,6.98717358303777,139.306140903406));
#129561=CARTESIAN_POINT('Ctrl Pts',(79.5113673340132,7.00292199593063,139.302281468401));
#129562=CARTESIAN_POINT('Ctrl Pts',(79.4427316478592,7.02226150712429,139.298422033396));
#129563=CARTESIAN_POINT('Ctrl Pts',(79.3741390119948,7.04158888801658,139.29456501914));
#129564=CARTESIAN_POINT('Ctrl Pts',(79.3065037570193,7.06450276695379,139.290708004885));
#129565=CARTESIAN_POINT('Ctrl Pts',(79.2402224714927,7.09088091789029,139.286850990629));
#129566=CARTESIAN_POINT('Ctrl Pts',(79.1739606077154,7.11725133949825,139.282995106556));
#129567=CARTESIAN_POINT('Ctrl Pts',(79.1090523766764,7.14708383835458,139.279139222483));
#129568=CARTESIAN_POINT('Ctrl Pts',(79.0458761277446,7.18020737475601,139.275283338411));
#129569=CARTESIAN_POINT('Ctrl Pts',(78.9826972772882,7.21333227514625,139.271427295557));
#129570=CARTESIAN_POINT('Ctrl Pts',(78.9212509795886,7.24974825470462,139.267571252703));
#129571=CARTESIAN_POINT('Ctrl Pts',(78.8618910896333,7.28923827765412,139.26371520985));
#129572=CARTESIAN_POINT('Ctrl Pts',(78.8024689587002,7.32876970731177,139.259855123796));
#129573=CARTESIAN_POINT('Ctrl Pts',(78.7451380077172,7.37138134514055,139.255995037743));
#129574=CARTESIAN_POINT('Ctrl Pts',(78.6902224229091,7.41681325768247,139.25213495169));
#129575=CARTESIAN_POINT('Ctrl Pts',(78.6352756736537,7.46227095271314,139.248272675048));
#129576=CARTESIAN_POINT('Ctrl Pts',(78.5827473769454,7.51055177980714,139.244410398407));
#129577=CARTESIAN_POINT('Ctrl Pts',(78.5329259184762,7.5613578617943,139.240548121765));
#129578=CARTESIAN_POINT('Ctrl Pts',(78.4830172976119,7.61225282877056,139.23667908809));
#129579=CARTESIAN_POINT('Ctrl Pts',(78.4358252913247,7.665681507082,139.232810054414));
#129580=CARTESIAN_POINT('Ctrl Pts',(78.391598497205,7.72131232573913,139.228941020738));
#129581=CARTESIAN_POINT('Ctrl Pts',(78.3654107372799,7.75425268581786,139.226650071845));
#129582=CARTESIAN_POINT('Ctrl Pts',(78.3402618055092,7.78796455806452,139.224359122952));
#129583=CARTESIAN_POINT('Ctrl Pts',(78.3161959160251,7.82237469062124,139.222068174059));
#129584=CARTESIAN_POINT('Ctrl Pts',(78.2750915133202,7.88114700180774,139.218155246347));
#129585=CARTESIAN_POINT('Ctrl Pts',(78.2369898078095,7.94218533763197,139.214242318635));
#129586=CARTESIAN_POINT('Ctrl Pts',(78.2021456925714,8.0051545588583,139.210329390922));
#129587=CARTESIAN_POINT('Ctrl Pts',(78.1673565315928,8.06802446842476,139.206422634469));
#129588=CARTESIAN_POINT('Ctrl Pts',(78.1358149862431,8.1328188082781,139.202515878015));
#129589=CARTESIAN_POINT('Ctrl Pts',(78.1077333086913,8.19917272057976,139.198609121561));
#129590=CARTESIAN_POINT('Ctrl Pts',(78.0796926580191,8.26542969088187,139.194708072816));
#129591=CARTESIAN_POINT('Ctrl Pts',(78.0551020089896,8.33324127245433,139.190807024071));
#129592=CARTESIAN_POINT('Ctrl Pts',(78.0341273717282,8.40221879260742,139.186905975326));
#129593=CARTESIAN_POINT('Ctrl Pts',(78.0131709261672,8.47113648725012,139.183008310034));
#129594=CARTESIAN_POINT('Ctrl Pts',(77.9958244012656,8.54121766308561,139.179110644742));
#129595=CARTESIAN_POINT('Ctrl Pts',(77.9822049906054,8.61205559346455,139.17521297945));
#129596=CARTESIAN_POINT('Ctrl Pts',(77.9685917131875,8.6828616233298,139.171317069398));
#129597=CARTESIAN_POINT('Ctrl Pts',(77.9587023103997,8.75442326962861,139.167421159346));
#129598=CARTESIAN_POINT('Ctrl Pts',(77.9526032349813,8.82632199594982,139.163525249293));
#129599=CARTESIAN_POINT('Ctrl Pts',(77.9476716106702,8.88445826781668,139.160375072683));
#129600=CARTESIAN_POINT('Ctrl Pts',(77.9452171923589,8.94281458993765,139.157224896072));
#129601=CARTESIAN_POINT('Ctrl Pts',(77.9452503313532,9.00116691725337,139.154074719462));
#129602=CARTESIAN_POINT('Origin',(80.,9.,129.));
#129603=CARTESIAN_POINT('Ctrl Pts',(79.2300979593294,7.52256748114465,129.));
#129604=CARTESIAN_POINT('Ctrl Pts',(79.281830748178,7.48750058327585,129.));
#129605=CARTESIAN_POINT('Ctrl Pts',(79.3355405243692,7.45568942276443,129.));
#129606=CARTESIAN_POINT('Ctrl Pts',(79.3908959010939,7.42706960794827,129.));
#129607=CARTESIAN_POINT('Ctrl Pts',(79.4259930678064,7.40892368480008,129.));
#129608=CARTESIAN_POINT('Ctrl Pts',(79.4617526563836,7.39206132563758,129.));
#129609=CARTESIAN_POINT('Ctrl Pts',(79.4980977986663,7.37647332647928,129.));
#129610=CARTESIAN_POINT('Ctrl Pts',(79.5226963251973,7.36592331107759,129.));
#129611=CARTESIAN_POINT('Ctrl Pts',(79.5475631896663,7.35595715019795,129.));
#129612=CARTESIAN_POINT('Ctrl Pts',(79.5726757725026,7.34657353461922,129.));
#129613=CARTESIAN_POINT('Ctrl Pts',(79.5862857126981,7.34148801841897,129.));
#129614=CARTESIAN_POINT('Ctrl Pts',(79.599968045098,7.33657368647343,129.));
#129615=CARTESIAN_POINT('Ctrl Pts',(79.6137049524654,7.33183503949085,129.));
#129616=CARTESIAN_POINT('Ctrl Pts',(79.6760826347754,7.31031740031977,129.));
#129617=CARTESIAN_POINT('Ctrl Pts',(79.7396533189192,7.29239195390877,129.));
#129618=CARTESIAN_POINT('Ctrl Pts',(79.8040665846156,7.2780116608573,129.));
#129619=CARTESIAN_POINT('Ctrl Pts',(79.850512417162,7.26764260603894,129.));
#129620=CARTESIAN_POINT('Ctrl Pts',(79.8973972321369,7.25911760209265,129.));
#129621=CARTESIAN_POINT('Ctrl Pts',(79.9445987750863,7.25243304107414,129.));
#129622=CARTESIAN_POINT('Ctrl Pts',(79.9573802290497,7.25062296446254,129.));
#129623=CARTESIAN_POINT('Ctrl Pts',(79.9701849395111,7.24894790625536,129.));
#129624=CARTESIAN_POINT('Ctrl Pts',(79.9830105439016,7.24740795082224,129.));
#129625=CARTESIAN_POINT('Ctrl Pts',(79.9965305707581,7.2457846168896,129.));
#129626=CARTESIAN_POINT('Ctrl Pts',(80.010066274218,7.24431236541112,129.));
#129627=CARTESIAN_POINT('Ctrl Pts',(80.0236082610051,7.24299136914067,129.));
#129628=CARTESIAN_POINT('Ctrl Pts',(80.0912918487103,7.23638895781539,129.));
#129629=CARTESIAN_POINT('Ctrl Pts',(80.1591802213322,7.23355533205344,129.));
#129630=CARTESIAN_POINT('Ctrl Pts',(80.2269161369356,7.23444184514064,129.));
#129631=CARTESIAN_POINT('Ctrl Pts',(80.2955027350948,7.23533949177806,129.));
#129632=CARTESIAN_POINT('Ctrl Pts',(80.3639340445116,7.24005098621149,129.));
#129633=CARTESIAN_POINT('Ctrl Pts',(80.4318607174046,7.24857423381045,129.));
#129634=CARTESIAN_POINT('Ctrl Pts',(80.4737684724859,7.25383270088474,129.));
#129635=CARTESIAN_POINT('Ctrl Pts',(80.515484509682,7.26054302178907,129.));
#129636=CARTESIAN_POINT('Ctrl Pts',(80.5569281451476,7.26871452189268,129.));
#129637=CARTESIAN_POINT('Ctrl Pts',(80.59098326124,7.27542921720238,129.));
#129638=CARTESIAN_POINT('Ctrl Pts',(80.6248544845506,7.28313067078347,129.));
#129639=CARTESIAN_POINT('Ctrl Pts',(80.6584967044525,7.29182802522507,129.));
#129640=CARTESIAN_POINT('Ctrl Pts',(80.6723040435688,7.29539756738195,129.));
#129641=CARTESIAN_POINT('Ctrl Pts',(80.6860753217099,7.29913575892529,129.));
#129642=CARTESIAN_POINT('Ctrl Pts',(80.6997840581602,7.30303636166769,129.));
#129643=CARTESIAN_POINT('Ctrl Pts',(80.7675838280963,7.32232770697194,129.));
#129644=CARTESIAN_POINT('Ctrl Pts',(80.8339731467169,7.34561685223654,129.));
#129645=CARTESIAN_POINT('Ctrl Pts',(80.898588998481,7.37288464964485,129.));
#129646=CARTESIAN_POINT('Ctrl Pts',(80.9057659256999,7.37591330270869,129.));
#129647=CARTESIAN_POINT('Ctrl Pts',(80.9129209821764,7.37899109153126,129.));
#129648=CARTESIAN_POINT('Ctrl Pts',(80.9200536746534,7.3821180294085,129.));
#129649=CARTESIAN_POINT('Ctrl Pts',(80.984149627247,7.41021738495922,129.));
#129650=CARTESIAN_POINT('Ctrl Pts',(81.0464406059207,7.44228062654433,129.));
#129651=CARTESIAN_POINT('Ctrl Pts',(81.1067678836995,7.477962347096,129.));
#129652=CARTESIAN_POINT('Ctrl Pts',(81.1670951614783,7.51364406764767,129.));
#129653=CARTESIAN_POINT('Ctrl Pts',(81.2254594571749,7.55294494292302,129.));
#129654=CARTESIAN_POINT('Ctrl Pts',(81.2816840111194,7.59557425376097,129.));
#129655=CARTESIAN_POINT('Ctrl Pts',(81.2922356478337,7.60357447732499,129.));
#129656=CARTESIAN_POINT('Ctrl Pts',(81.3027118541411,7.61169206594889,129.));
#129657=CARTESIAN_POINT('Ctrl Pts',(81.313111358469,7.61992528231288,129.));
#129658=CARTESIAN_POINT('Ctrl Pts',(81.3222610024349,7.62716899278696,129.));
#129659=CARTESIAN_POINT('Ctrl Pts',(81.3313442109961,7.63449663645984,129.));
#129660=CARTESIAN_POINT('Ctrl Pts',(81.340358501486,7.64190506046335,129.));
#129661=CARTESIAN_POINT('Ctrl Pts',(81.3958400493656,7.68750275132147,129.));
#129662=CARTESIAN_POINT('Ctrl Pts',(81.4487348274871,7.73617414202039,129.));
#129663=CARTESIAN_POINT('Ctrl Pts',(81.4988881430576,7.78755864017411,129.));
#129664=CARTESIAN_POINT('Ctrl Pts',(81.5490414586282,7.83894313832784,129.));
#129665=CARTESIAN_POINT('Ctrl Pts',(81.596453992352,7.89304144632724,129.));
#129666=CARTESIAN_POINT('Ctrl Pts',(81.6409514014518,7.94954263372726,129.));
#129667=CARTESIAN_POINT('Ctrl Pts',(81.6861833091593,8.00697646067449,129.));
#129668=CARTESIAN_POINT('Ctrl Pts',(81.7284038904358,8.06689379464521,129.));
#129669=CARTESIAN_POINT('Ctrl Pts',(81.7673981934856,8.12900933410927,129.));
#129670=CARTESIAN_POINT('Ctrl Pts',(81.7770296357955,8.14435163255051,129.));
#129671=CARTESIAN_POINT('Ctrl Pts',(81.786464068092,8.15982820433461,129.));
#129672=CARTESIAN_POINT('Ctrl Pts',(81.7956978659394,8.17543505634213,129.));
#129673=CARTESIAN_POINT('Ctrl Pts',(81.8029371409721,8.18767079032106,129.));
#129674=CARTESIAN_POINT('Ctrl Pts',(81.8100538149155,8.19998811837099,129.));
#129675=CARTESIAN_POINT('Ctrl Pts',(81.8170357172675,8.21236610903634,129.));
#129676=CARTESIAN_POINT('Ctrl Pts',(81.854021820935,8.27793758552841,129.));
#129677=CARTESIAN_POINT('Ctrl Pts',(81.8872984696483,8.34532395025826,129.));
#129678=CARTESIAN_POINT('Ctrl Pts',(81.9166855007576,8.41417988544907,129.));
#129679=CARTESIAN_POINT('Ctrl Pts',(81.9459284893018,8.48269831851237,129.));
#129680=CARTESIAN_POINT('Ctrl Pts',(81.9713206084984,8.55267279654377,129.));
#129681=CARTESIAN_POINT('Ctrl Pts',(81.9926494449667,8.62379991350796,129.));
#129682=CARTESIAN_POINT('Ctrl Pts',(82.0137867709559,8.69428838390283,129.));
#129683=CARTESIAN_POINT('Ctrl Pts',(82.0309341246297,8.76590972191823,129.));
#129684=CARTESIAN_POINT('Ctrl Pts',(82.0438402050009,8.83839240103824,129.));
#129685=CARTESIAN_POINT('Ctrl Pts',(82.0465861966793,8.85381434387207,129.));
#129686=CARTESIAN_POINT('Ctrl Pts',(82.0491400035047,8.8692753399892,129.));
#129687=CARTESIAN_POINT('Ctrl Pts',(82.0514988962123,8.88477285886849,129.));
#129688=CARTESIAN_POINT('Ctrl Pts',(82.053488432599,8.89784377032416,129.));
#129689=CARTESIAN_POINT('Ctrl Pts',(82.0553393131761,8.9109406630385,129.));
#129690=CARTESIAN_POINT('Ctrl Pts',(82.0570523367261,8.92406189548185,129.));
#129691=CARTESIAN_POINT('Ctrl Pts',(81.8174278887596,9.95862058795901,129.));
#129692=CARTESIAN_POINT('Ctrl Pts',(81.7762160018567,10.0216592895785,129.));
#129693=CARTESIAN_POINT('Ctrl Pts',(81.7313405655059,10.0821005916704,129.));
#129694=CARTESIAN_POINT('Ctrl Pts',(81.6831396740662,10.1397906903828,129.));
#129695=CARTESIAN_POINT('Ctrl Pts',(81.6370503035558,10.1949535775186,129.));
#129696=CARTESIAN_POINT('Ctrl Pts',(81.5879193937338,10.2476011126225,129.));
#129697=CARTESIAN_POINT('Ctrl Pts',(81.5360172152856,10.2975621775029,129.));
#129698=CARTESIAN_POINT('Ctrl Pts',(81.5243247634357,10.3088173379403,129.));
#129699=CARTESIAN_POINT('Ctrl Pts',(81.5124900085598,10.3199374555242,129.));
#129700=CARTESIAN_POINT('Ctrl Pts',(81.5005210105629,10.3309156511376,129.));
#129701=CARTESIAN_POINT('Ctrl Pts',(81.4455937863517,10.381295959669,129.));
#129702=CARTESIAN_POINT('Ctrl Pts',(81.3879517403589,10.4285914676262,129.));
#129703=CARTESIAN_POINT('Ctrl Pts',(81.32791149294,10.4726299004967,129.));
#129704=CARTESIAN_POINT('Ctrl Pts',(81.2857591326134,10.5035478925167,129.));
#129705=CARTESIAN_POINT('Ctrl Pts',(81.2424240158456,10.5328595775406,129.));
#129706=CARTESIAN_POINT('Ctrl Pts',(81.198010382721,10.5604909361764,129.));
#129707=CARTESIAN_POINT('Ctrl Pts',(81.1811383966962,10.5709876207291,129.));
#129708=CARTESIAN_POINT('Ctrl Pts',(81.1641107403089,10.5812416863955,129.));
#129709=CARTESIAN_POINT('Ctrl Pts',(81.1469330529734,10.5912485887382,129.));
#129710=CARTESIAN_POINT('Ctrl Pts',(81.1305340848948,10.6008018463378,129.));
#129711=CARTESIAN_POINT('Ctrl Pts',(81.1139930505993,10.6101325847749,129.));
#129712=CARTESIAN_POINT('Ctrl Pts',(81.0973444947477,10.6192209212688,129.));
#129713=CARTESIAN_POINT('Ctrl Pts',(81.0336769966004,10.6539765872885,129.));
#129714=CARTESIAN_POINT('Ctrl Pts',(80.968373580833,10.6852316531886,129.));
#129715=CARTESIAN_POINT('Ctrl Pts',(80.9017255995023,10.7128251457784,129.));
#129716=CARTESIAN_POINT('Ctrl Pts',(80.8366062693887,10.7397857485914,129.));
#129717=CARTESIAN_POINT('Ctrl Pts',(80.7702024261762,10.7632509566609,129.));
#129718=CARTESIAN_POINT('Ctrl Pts',(80.7027772959504,10.783022803573,129.));
#129719=CARTESIAN_POINT('Ctrl Pts',(80.6364369119638,10.8024765578613,129.));
#129720=CARTESIAN_POINT('Ctrl Pts',(80.5691070645839,10.8183549948411,129.));
#129721=CARTESIAN_POINT('Ctrl Pts',(80.501042459281,10.8304204386017,129.));
#129722=CARTESIAN_POINT('Ctrl Pts',(80.4789907160657,10.8343294316298,129.));
#129723=CARTESIAN_POINT('Ctrl Pts',(80.4568619287533,10.8378377953482,129.));
#129724=CARTESIAN_POINT('Ctrl Pts',(80.4346650539684,10.8409362728209,129.));
#129725=CARTESIAN_POINT('Ctrl Pts',(80.4221749866782,10.8426797701603,129.));
#129726=CARTESIAN_POINT('Ctrl Pts',(80.4096620712929,10.8442935310645,129.));
#129727=CARTESIAN_POINT('Ctrl Pts',(80.3971456250734,10.8457740253543,129.));
#129728=CARTESIAN_POINT('Ctrl Pts',(80.3293080731436,10.8537981167383,129.));
#129729=CARTESIAN_POINT('Ctrl Pts',(80.2612484637432,10.8579293246703,129.));
#129730=CARTESIAN_POINT('Ctrl Pts',(80.1932129649845,10.8579897571609,129.));
#129731=CARTESIAN_POINT('Ctrl Pts',(80.183419062696,10.8579984565887,129.));
#129732=CARTESIAN_POINT('Ctrl Pts',(80.173625666279,10.8579227116332,129.));
#129733=CARTESIAN_POINT('Ctrl Pts',(80.1638335195185,10.8577619017594,129.));
#129734=CARTESIAN_POINT('Ctrl Pts',(80.094125774739,10.8566171381119,129.));
#129735=CARTESIAN_POINT('Ctrl Pts',(80.0244798679339,10.8511657002129,129.));
#129736=CARTESIAN_POINT('Ctrl Pts',(79.9552253060309,10.8415831053598,129.));
#129737=CARTESIAN_POINT('Ctrl Pts',(79.8912776929718,10.8327348208435,129.));
#129738=CARTESIAN_POINT('Ctrl Pts',(79.8276632746924,10.8203632855842,129.));
#129739=CARTESIAN_POINT('Ctrl Pts',(79.7646616788188,10.8045727994338,129.));
#129740=CARTESIAN_POINT('Ctrl Pts',(79.7507943070261,10.8010971328383,129.));
#129741=CARTESIAN_POINT('Ctrl Pts',(79.7369567233517,10.7974557117189,129.));
#129742=CARTESIAN_POINT('Ctrl Pts',(79.7231520870758,10.7936494709069,129.));
#129743=CARTESIAN_POINT('Ctrl Pts',(79.7120934934718,10.7906003742514,129.));
#129744=CARTESIAN_POINT('Ctrl Pts',(79.7010565962289,10.7874455711953,129.));
#129745=CARTESIAN_POINT('Ctrl Pts',(79.6900560633263,10.7841896646439,129.));
#129746=CARTESIAN_POINT('Ctrl Pts',(79.6245012361557,10.7647869326896,129.));
#129747=CARTESIAN_POINT('Ctrl Pts',(79.5601138344761,10.7417646897258,129.));
#129748=CARTESIAN_POINT('Ctrl Pts',(79.4971959262021,10.715304780306,129.));
#129749=CARTESIAN_POINT('Ctrl Pts',(79.4345683059016,10.6889669504927,129.));
#129750=CARTESIAN_POINT('Ctrl Pts',(79.3733957590305,10.6592224003991,129.));
#129751=CARTESIAN_POINT('Ctrl Pts',(79.3140059902934,10.6262089191606,129.));
#129752=CARTESIAN_POINT('Ctrl Pts',(79.2558864207415,10.5939015140336,129.));
#129753=CARTESIAN_POINT('Ctrl Pts',(79.1994735144971,10.558462809005,129.));
#129754=CARTESIAN_POINT('Ctrl Pts',(79.1451143324441,10.5199925315035,129.));
#129755=CARTESIAN_POINT('Ctrl Pts',(79.1336097299013,10.5118506641014,129.));
#129756=CARTESIAN_POINT('Ctrl Pts',(79.1221972825761,10.5035729216371,129.));
#129757=CARTESIAN_POINT('Ctrl Pts',(79.1108805595173,10.4951601203912,129.));
#129758=CARTESIAN_POINT('Ctrl Pts',(79.1002618280376,10.4872662029598,129.));
#129759=CARTESIAN_POINT('Ctrl Pts',(79.0897261684286,10.479252279507,129.));
#129760=CARTESIAN_POINT('Ctrl Pts',(79.0792930565818,10.4711322469418,129.));
#129761=CARTESIAN_POINT('Ctrl Pts',(79.0277338571515,10.4310040105575,129.));
#129762=CARTESIAN_POINT('Ctrl Pts',(78.978581104871,10.3882180036356,129.));
#129763=CARTESIAN_POINT('Ctrl Pts',(78.9321255592781,10.3429060921625,129.));
#129764=CARTESIAN_POINT('Ctrl Pts',(78.8871753821825,10.2990624903005,129.));
#129765=CARTESIAN_POINT('Ctrl Pts',(78.8447499809854,10.2528533437791,129.));
#129766=CARTESIAN_POINT('Ctrl Pts',(78.8051532326766,10.2043735161521,129.));
#129767=CARTESIAN_POINT('Ctrl Pts',(78.7657598821795,10.1561427163183,129.));
#129768=CARTESIAN_POINT('Ctrl Pts',(78.7291656220547,10.1056639886396,129.));
#129769=CARTESIAN_POINT('Ctrl Pts',(78.6957182918309,10.0530146622108,129.));
#129770=CARTESIAN_POINT('Ctrl Pts',(78.6902769744426,10.0444495033935,129.));
#129771=CARTESIAN_POINT('Ctrl Pts',(78.6849190588097,10.0358268728766,129.));
#129772=CARTESIAN_POINT('Ctrl Pts',(78.6796461810995,10.0271470773945,129.));
#129773=CARTESIAN_POINT('Ctrl Pts',(78.6739912646832,10.017838399921,129.));
#129774=CARTESIAN_POINT('Ctrl Pts',(78.6684341558143,10.0084639727813,129.));
#129775=CARTESIAN_POINT('Ctrl Pts',(78.6629752590626,9.99902545690085,129.));
#129776=CARTESIAN_POINT('Ctrl Pts',(81.2663555529872,10.0778216258784,139.998270369527));
#129777=CARTESIAN_POINT('Ctrl Pts',(81.624882726317,9.65660459345759,139.961212857736));
#129778=CARTESIAN_POINT('Ctrl Pts',(81.8817055576156,8.43521511269861,139.887110973282));
#129779=CARTESIAN_POINT('Ctrl Pts',(80.5443606420769,7.1101993889356,139.775964716164));
#129780=CARTESIAN_POINT('Ctrl Pts',(78.7083082983556,7.51894549756411,139.664831598172));
#129781=CARTESIAN_POINT('Ctrl Pts',(78.0547700623159,9.28127667726292,139.553698480181));
#129782=CARTESIAN_POINT('Ctrl Pts',(79.181430819152,10.7871147142069,139.442565362189));
#129783=CARTESIAN_POINT('Ctrl Pts',(81.0573526210883,10.6568543838274,139.331432244198));
#129784=CARTESIAN_POINT('Ctrl Pts',(81.9655073494158,9.01040090821446,139.220299126206));
#129785=CARTESIAN_POINT('Ctrl Pts',(81.0747701558528,7.35431801012218,139.109166008215));
#129786=CARTESIAN_POINT('Ctrl Pts',(79.2003523271827,7.20448187233449,138.998032890223));
#129787=CARTESIAN_POINT('Ctrl Pts',(78.0578077691287,8.69794827804849,138.886899772231));
#129788=CARTESIAN_POINT('Ctrl Pts',(78.6928319084955,10.4678771753584,138.77576665424));
#129789=CARTESIAN_POINT('Ctrl Pts',(80.5242287499213,10.8943408158948,138.664633536248));
#129790=CARTESIAN_POINT('Ctrl Pts',(81.8758303096953,9.58703225682554,138.553500418257));
#129791=CARTESIAN_POINT('Ctrl Pts',(81.5105983807109,7.74244716724272,138.442367300265));
#129792=CARTESIAN_POINT('Ctrl Pts',(79.7628072385,7.04882466216988,138.331234182274));
#129793=CARTESIAN_POINT('Ctrl Pts',(78.2321043054277,8.14099426435935,138.220101064282));
#129794=CARTESIAN_POINT('Ctrl Pts',(78.3194490673689,10.0193599016733,138.108967946291));
#129795=CARTESIAN_POINT('Ctrl Pts',(79.9449002025574,10.9647671494451,137.997834828299));
#129796=CARTESIAN_POINT('Ctrl Pts',(81.6207808342945,10.1119422115685,137.886701710307));
#129797=CARTESIAN_POINT('Ctrl Pts',(81.8132590564869,8.24142397550868,137.775568592316));
#129798=CARTESIAN_POINT('Ctrl Pts',(80.3461712193815,7.06518438436528,137.664435474324));
#129799=CARTESIAN_POINT('Ctrl Pts',(78.5622538579237,7.65976419334241,137.553302356333));
#129800=CARTESIAN_POINT('Ctrl Pts',(78.0942183544438,9.48098056613988,137.442169238341));
#129801=CARTESIAN_POINT('Ctrl Pts',(79.3704292240006,10.8619845924221,137.33103612035));
#129802=CARTESIAN_POINT('Ctrl Pts',(81.222848047324,10.5388270332939,137.219903002358));
#129803=CARTESIAN_POINT('Ctrl Pts',(81.9560682069516,8.80727440537282,137.108769884366));
#129804=CARTESIAN_POINT('Ctrl Pts',(80.8990177534605,7.25211182739711,136.997636766375));
#129805=CARTESIAN_POINT('Ctrl Pts',(79.0191508670193,7.2966853011286,136.886503648383));
#129806=CARTESIAN_POINT('Ctrl Pts',(78.0369957129224,8.90019942911323,136.775370530392));
#129807=CARTESIAN_POINT('Ctrl Pts',(78.8514593454574,10.5950549676696,136.6642374124));
#129808=CARTESIAN_POINT('Ctrl Pts',(80.7171125911482,10.8300534190709,136.553104294409));
#129809=CARTESIAN_POINT('Ctrl Pts',(81.9264361681442,9.39011495113394,136.441971176417));
#129810=CARTESIAN_POINT('Ctrl Pts',(81.3726095402657,7.59312792514629,136.330838058426));
#129811=CARTESIAN_POINT('Ctrl Pts',(79.562516635751,7.08376559600911,136.219704940434));
#129812=CARTESIAN_POINT('Ctrl Pts',(78.1528257253745,8.32821641565602,136.108571822443));
#129813=CARTESIAN_POINT('Ctrl Pts',(78.4337414152061,10.1875100128385,135.997438704451));
#129814=CARTESIAN_POINT('Ctrl Pts',(80.1481586091783,10.9599477063327,135.886305586459));
#129815=CARTESIAN_POINT('Ctrl Pts',(81.7269752125645,9.93856411620112,135.775172468468));
#129816=CARTESIAN_POINT('Ctrl Pts',(81.7251961283297,8.05816970539868,135.664039350476));
#129817=CARTESIAN_POINT('Ctrl Pts',(80.1444496443897,7.0397754502945,135.552906232485));
#129818=CARTESIAN_POINT('Ctrl Pts',(78.4314971604217,7.81545585676727,135.441773114493));
#129819=CARTESIAN_POINT('Ctrl Pts',(78.1541002109059,9.67527768632976,135.330639996501));
#129820=CARTESIAN_POINT('Ctrl Pts',(79.5661434022768,10.9170587986925,135.21950687851));
#129821=CARTESIAN_POINT('Ctrl Pts',(81.3752692283133,10.4042722437928,135.108373760518));
#129822=CARTESIAN_POINT('Ctrl Pts',(81.9256945265281,8.60624045975704,134.997240642527));
#129823=CARTESIAN_POINT('Ctrl Pts',(80.7136483994663,7.16859290517607,134.886107524535));
#129824=CARTESIAN_POINT('Ctrl Pts',(78.8484431682858,7.40712120725877,134.774974406544));
#129825=CARTESIAN_POINT('Ctrl Pts',(78.0371880743253,9.10351487555662,134.663841288552));
#129826=CARTESIAN_POINT('Ctrl Pts',(79.0223757102669,10.7051676554393,134.552708170561));
#129827=CARTESIAN_POINT('Ctrl Pts',(80.9023235750891,10.7461838823189,134.441575052569));
#129828=CARTESIAN_POINT('Ctrl Pts',(81.9564293888803,9.18902389097254,134.330441934578));
#129829=CARTESIAN_POINT('Ctrl Pts',(81.2199340216575,7.45886179470017,134.219308816586));
#129830=CARTESIAN_POINT('Ctrl Pts',(79.3669070216788,7.13921004252689,134.108175698594));
#129831=CARTESIAN_POINT('Ctrl Pts',(78.0933116337564,8.52262649941205,133.997042580603));
#129832=CARTESIAN_POINT('Ctrl Pts',(78.5647924851429,10.3429539732731,133.885909462611));
#129833=CARTESIAN_POINT('Ctrl Pts',(80.3498317433441,10.9341571126414,133.77477634462));
#129834=CARTESIAN_POINT('Ctrl Pts',(81.8146912207933,9.75514353483809,133.663643226628));
#129835=CARTESIAN_POINT('Ctrl Pts',(81.6186738674224,7.88499287179108,133.552510108637));
#129836=CARTESIAN_POINT('Ctrl Pts',(79.9411824802037,7.03534061873377,133.441376990645));
#129837=CARTESIAN_POINT('Ctrl Pts',(78.3175232021377,7.98382195965104,133.330243872653));
#129838=CARTESIAN_POINT('Ctrl Pts',(78.2337329111168,9.86234943947361,133.219110754662));
#129839=CARTESIAN_POINT('Ctrl Pts',(79.766499779437,10.9516207705468,133.10797763667));
#129840=CARTESIAN_POINT('Ctrl Pts',(81.5129752400956,10.2546919573705,132.996844518679));
#129841=CARTESIAN_POINT('Ctrl Pts',(81.8747162108936,8.40941968061457,132.885711400687));
#129842=CARTESIAN_POINT('Ctrl Pts',(80.5206431173708,7.10466975717507,132.774578282696));
#129843=CARTESIAN_POINT('Ctrl Pts',(78.6900569505169,7.53460067144032,132.663445164704));
#129844=CARTESIAN_POINT('Ctrl Pts',(78.0583822214058,9.30572272875902,132.552312046712));
#129845=CARTESIAN_POINT('Ctrl Pts',(79.2037525045956,10.7970353115879,132.441178928721));
#129846=CARTESIAN_POINT('Ctrl Pts',(81.0778798355747,10.6436304466314,132.330045810729));
#129847=CARTESIAN_POINT('Ctrl Pts',(81.9654891161006,8.98591030425289,132.218912692738));
#129848=CARTESIAN_POINT('Ctrl Pts',(81.0542053966701,7.34108560598915,132.107779574746));
#129849=CARTESIAN_POINT('Ctrl Pts',(79.1780714050938,7.21456465535435,131.996646456755));
#129850=CARTESIAN_POINT('Ctrl Pts',(78.0541988143562,8.72214440619798,131.885513338763));
#129851=CARTESIAN_POINT('Ctrl Pts',(78.7112000547364,10.4840285327618,131.774380220772));
#129852=CARTESIAN_POINT('Ctrl Pts',(80.5477617316354,10.887671335383,131.66324710278));
#129853=CARTESIAN_POINT('Ctrl Pts',(81.8829903121689,9.56364303377056,131.552113984788));
#129854=CARTESIAN_POINT('Ctrl Pts',(81.4948320449856,7.72374644302386,131.440980866797));
#129855=CARTESIAN_POINT('Ctrl Pts',(79.7385446547136,7.05192734017315,131.329847748805));
#129856=CARTESIAN_POINT('Ctrl Pts',(78.2215514862109,8.16306101160042,131.218714630814));
#129857=CARTESIAN_POINT('Ctrl Pts',(78.3322643986637,10.0401941855574,131.107581512822));
#129858=CARTESIAN_POINT('Ctrl Pts',(79.9693545706299,10.9653007018072,130.996448394831));
#129859=CARTESIAN_POINT('Ctrl Pts',(81.634492654468,10.0916866570469,130.885315276839));
#129860=CARTESIAN_POINT('Ctrl Pts',(81.8036787100972,8.2189180260953,130.774182158847));
#129861=CARTESIAN_POINT('Ctrl Pts',(80.3220670546241,7.06102633885022,130.663049040856));
#129862=CARTESIAN_POINT('Ctrl Pts',(78.5456868797065,7.67775970833857,130.551915922864));
#129863=CARTESIAN_POINT('Ctrl Pts',(78.1003514663068,9.50465934401503,130.440782804873));
#129864=CARTESIAN_POINT('Ctrl Pts',(79.3936488482192,10.8696750722296,130.329649686881));
#129865=CARTESIAN_POINT('Ctrl Pts',(81.2419033084764,10.5234902013865,130.21851656889));
#129866=CARTESIAN_POINT('Ctrl Pts',(81.9535176740369,8.78294791815207,130.107383450898));
#129867=CARTESIAN_POINT('Ctrl Pts',(80.8771984457467,7.24105863992984,129.996250332907));
#129868=CARTESIAN_POINT('Ctrl Pts',(78.9980272102543,7.30902500521152,129.885117214915));
#129869=CARTESIAN_POINT('Ctrl Pts',(78.0359120840056,8.92463153403525,129.773984096924));
#129870=CARTESIAN_POINT('Ctrl Pts',(78.8713846676021,10.6092319693557,129.662850978932));
#129871=CARTESIAN_POINT('Ctrl Pts',(80.7398571755473,10.8209719051349,129.551717860941));
#129872=CARTESIAN_POINT('Ctrl Pts',(81.9310876541967,9.36614407866247,129.440584742949));
#129873=CARTESIAN_POINT('Ctrl Pts',(81.3551062875205,7.57608937952851,129.329451624957));
#129874=CARTESIAN_POINT('Ctrl Pts',(79.5384782449276,7.08949384998904,129.218318506966));
#129875=CARTESIAN_POINT('Ctrl Pts',(78.1450715048774,8.35097752792031,129.107185388974));
#129876=CARTESIAN_POINT('Ctrl Pts',(78.4476865286044,10.2074757739787,128.996052270983));
#129877=CARTESIAN_POINT('Ctrl Pts',(80.1745002968193,10.9567650420694,128.884919152991));
#129878=CARTESIAN_POINT('Ctrl Pts',(81.2128991468495,10.264901734376,128.810830407663));
#129879=CARTESIAN_POINT('Ctrl Pts',(81.4708680456716,9.7758241190599,128.773786035));
#129880=CARTESIAN_POINT('Ctrl Pts',(81.3664711693111,10.1630321152291,140.074173738579));
#129881=CARTESIAN_POINT('Ctrl Pts',(81.7533428062807,9.70851448037676,140.037116226789));
#129882=CARTESIAN_POINT('Ctrl Pts',(82.0304695530007,8.39056431383793,139.963014342335));
#129883=CARTESIAN_POINT('Ctrl Pts',(80.5873967396842,6.96079541430976,139.851868085216));
#129884=CARTESIAN_POINT('Ctrl Pts',(78.6061896552104,7.40185619829842,139.740734967225));
#129885=CARTESIAN_POINT('Ctrl Pts',(77.9009839525276,9.30351386636456,139.629601849233));
#129886=CARTESIAN_POINT('Ctrl Pts',(79.116716325777,10.9284005407918,139.518468731242));
#129887=CARTESIAN_POINT('Ctrl Pts',(81.140944870581,10.7878420810855,139.40733561325));
#129888=CARTESIAN_POINT('Ctrl Pts',(82.1208965520861,9.01122318386506,139.296202495259));
#129889=CARTESIAN_POINT('Ctrl Pts',(81.1597394018957,7.22421358068219,139.185069377267));
#129890=CARTESIAN_POINT('Ctrl Pts',(79.1371337315701,7.06253168816407,139.073936259276));
#129891=CARTESIAN_POINT('Ctrl Pts',(77.9042618145551,8.67406865416758,138.962803141284));
#129892=CARTESIAN_POINT('Ctrl Pts',(78.5894897319551,10.5839247006777,138.851670023292));
#129893=CARTESIAN_POINT('Ctrl Pts',(80.5656732591424,11.0441037303175,138.740536905301));
#129894=CARTESIAN_POINT('Ctrl Pts',(82.0241298193638,9.63344188961423,138.629403787309));
#129895=CARTESIAN_POINT('Ctrl Pts',(81.6300233617486,7.64302747692412,138.518270669318));
#129896=CARTESIAN_POINT('Ctrl Pts',(79.7440552383615,6.89456852056587,138.407137551326));
#129897=CARTESIAN_POINT('Ctrl Pts',(78.0923378972964,8.0730829353124,138.296004433335));
#129898=CARTESIAN_POINT('Ctrl Pts',(78.186587966877,10.0999485203839,138.184871315343));
#129899=CARTESIAN_POINT('Ctrl Pts',(79.9405441193332,11.1200978333399,138.073738197351));
#129900=CARTESIAN_POINT('Ctrl Pts',(81.7489166266227,10.1998502083116,137.96260507936));
#129901=CARTESIAN_POINT('Ctrl Pts',(81.9566118041151,8.18145242483221,137.851471961368));
#129902=CARTESIAN_POINT('Ctrl Pts',(80.3735388452432,6.91222161069935,137.740338843377));
#129903=CARTESIAN_POINT('Ctrl Pts',(78.4485884337135,7.5538077473141,137.629205725385));
#129904=CARTESIAN_POINT('Ctrl Pts',(77.9435509501959,9.5190059577491,137.518072607394));
#129905=CARTESIAN_POINT('Ctrl Pts',(79.3206565783088,11.0091894865106,137.406939489402));
#129906=CARTESIAN_POINT('Ctrl Pts',(81.3195240445505,10.660483716909,137.295806371411));
#129907=CARTESIAN_POINT('Ctrl Pts',(82.1107111693078,8.79203789328744,137.184673253419));
#129908=CARTESIAN_POINT('Ctrl Pts',(80.9700923551089,7.11392717518595,137.073540135427));
#129909=CARTESIAN_POINT('Ctrl Pts',(78.9416068350628,7.16202454138493,136.962407017436));
#129910=CARTESIAN_POINT('Ctrl Pts',(77.8818043975107,8.89230938935288,136.851273899444));
#129911=CARTESIAN_POINT('Ctrl Pts',(78.760657946726,10.7211569228289,136.740140781453));
#129912=CARTESIAN_POINT('Ctrl Pts',(80.7738061231242,10.974733896464,136.629007663461));
#129913=CARTESIAN_POINT('Ctrl Pts',(82.0787364789275,9.42095668328237,136.51787454547));
#129914=CARTESIAN_POINT('Ctrl Pts',(81.4811253909457,7.48190334486909,136.406741427478));
#129915=CARTESIAN_POINT('Ctrl Pts',(79.5279300486431,6.93227181693272,136.295608309486));
#129916=CARTESIAN_POINT('Ctrl Pts',(78.0067917063145,8.27510650712824,136.184475191495));
#129917=CARTESIAN_POINT('Ctrl Pts',(78.3099160462811,10.2813922535296,136.073342073503));
#129918=CARTESIAN_POINT('Ctrl Pts',(80.1598717417471,11.1148973743932,135.962208955512));
#129919=CARTESIAN_POINT('Ctrl Pts',(81.863506526676,10.0127651766626,135.85107583752));
#129920=CARTESIAN_POINT('Ctrl Pts',(81.8615867914887,7.98371042720149,135.739942719529));
#129921=CARTESIAN_POINT('Ctrl Pts',(80.155869553389,6.8848038955334,135.628809601537));
#129922=CARTESIAN_POINT('Ctrl Pts',(78.3074943650616,7.72180809198056,135.517676483546));
#129923=CARTESIAN_POINT('Ctrl Pts',(78.0081669502028,9.72866383179037,135.406543365554));
#129924=CARTESIAN_POINT('Ctrl Pts',(79.531843540303,11.0686177528167,135.295410247562));
#129925=CARTESIAN_POINT('Ctrl Pts',(81.4839953487769,10.5152912864638,135.184277129571));
#129926=CARTESIAN_POINT('Ctrl Pts',(82.0779362045621,8.57511059345543,135.073144011579));
#129927=CARTESIAN_POINT('Ctrl Pts',(80.7700680591604,7.0238054088007,134.962010893588));
#129928=CARTESIAN_POINT('Ctrl Pts',(78.7574033164313,7.28119129627272,134.850877775596));
#129929=CARTESIAN_POINT('Ctrl Pts',(77.8820119666334,9.11169856104729,134.739744657605));
#129930=CARTESIAN_POINT('Ctrl Pts',(78.9450866281691,10.8399749063389,134.628611539613));
#129931=CARTESIAN_POINT('Ctrl Pts',(80.9736595285902,10.8842337966425,134.517478421622));
#129932=CARTESIAN_POINT('Ctrl Pts',(82.1111009055799,9.2039677535394,134.40634530363));
#129933=CARTESIAN_POINT('Ctrl Pts',(81.316379641661,7.33702239430447,134.295212185638));
#129934=CARTESIAN_POINT('Ctrl Pts',(79.3168559174961,6.99209959396283,134.184079067647));
#129935=CARTESIAN_POINT('Ctrl Pts',(77.9425725459279,8.4848862754163,134.072945949655));
#129936=CARTESIAN_POINT('Ctrl Pts',(78.4513277598819,10.4491253122873,133.961812831664));
#129937=CARTESIAN_POINT('Ctrl Pts',(80.3774887631374,11.0870678263366,133.850679713672));
#129938=CARTESIAN_POINT('Ctrl Pts',(81.9581571925566,9.81484371953338,133.739546595681));
#129939=CARTESIAN_POINT('Ctrl Pts',(81.746643087032,7.79684256867697,133.628413477689));
#129940=CARTESIAN_POINT('Ctrl Pts',(79.9365324810536,6.88001845478242,133.517280359698));
#129941=CARTESIAN_POINT('Ctrl Pts',(78.1845098464722,7.90348489273153,133.406147241706));
#129942=CARTESIAN_POINT('Ctrl Pts',(78.0940952573956,9.93052511526679,133.295014123714));
#129943=CARTESIAN_POINT('Ctrl Pts',(79.7480397044302,11.1059121271983,133.183881005723));
#129944=CARTESIAN_POINT('Ctrl Pts',(81.6325881310308,10.3538854724243,133.072747887731));
#129945=CARTESIAN_POINT('Ctrl Pts',(82.0229276420695,8.36272954487466,132.96161476974));
#129946=CARTESIAN_POINT('Ctrl Pts',(80.5618041534298,6.95482862057646,132.850481651748));
#129947=CARTESIAN_POINT('Ctrl Pts',(78.5864953911754,7.41874903988775,132.739348533757));
#129948=CARTESIAN_POINT('Ctrl Pts',(77.9048816819162,9.32989257532517,132.628215415765));
#129949=CARTESIAN_POINT('Ctrl Pts',(79.1408027204212,10.9391054413796,132.517082297773));
#129950=CARTESIAN_POINT('Ctrl Pts',(81.163094926871,10.7735726850374,132.405949179782));
#129951=CARTESIAN_POINT('Ctrl Pts',(82.1208768772803,8.98479640020736,132.29481606179));
#129952=CARTESIAN_POINT('Ctrl Pts',(81.1375488326983,7.20993504831756,132.183682943799));
#129953=CARTESIAN_POINT('Ctrl Pts',(79.1130913229525,7.07341159647303,132.072549825807));
#129954=CARTESIAN_POINT('Ctrl Pts',(77.9003675428109,8.70017768132606,131.961416707816));
#129955=CARTESIAN_POINT('Ctrl Pts',(78.6093100282476,10.6013529531025,131.850283589824));
#129956=CARTESIAN_POINT('Ctrl Pts',(80.5910667127933,11.0369069735992,131.739150471833));
#129957=CARTESIAN_POINT('Ctrl Pts',(82.0318558777597,9.60820355990355,131.628017353841));
#129958=CARTESIAN_POINT('Ctrl Pts',(81.6130105700699,7.62284830968311,131.51688423585));
#129959=CARTESIAN_POINT('Ctrl Pts',(79.7178745017121,6.8979164902803,131.405751117858));
#129960=CARTESIAN_POINT('Ctrl Pts',(78.0809507926393,8.09689423683374,131.294617999866));
#129961=CARTESIAN_POINT('Ctrl Pts',(78.200416453433,10.1224299223834,131.183484881875));
#129962=CARTESIAN_POINT('Ctrl Pts',(79.9669318023625,11.1206735673178,131.072351763883));
#129963=CARTESIAN_POINT('Ctrl Pts',(81.763712476731,10.1779932888968,130.961218645892));
#129964=CARTESIAN_POINT('Ctrl Pts',(81.9462740541028,8.15716719866583,130.8500855279));
#129965=CARTESIAN_POINT('Ctrl Pts',(80.3475290519243,6.90773483816252,130.738952409908));
#129966=CARTESIAN_POINT('Ctrl Pts',(78.4307117022989,7.57322595285769,130.627819291917));
#129967=CARTESIAN_POINT('Ctrl Pts',(77.9501689339994,9.54455673392297,130.516686173925));
#129968=CARTESIAN_POINT('Ctrl Pts',(79.3457119010278,11.0174879607505,130.405553055934));
#129969=CARTESIAN_POINT('Ctrl Pts',(81.3400857777279,10.6439343847877,130.294419937942));
#129970=CARTESIAN_POINT('Ctrl Pts',(82.107958996203,8.76578820112213,130.183286819951));
#129971=CARTESIAN_POINT('Ctrl Pts',(80.9465480552043,7.1020001441342,130.072153701959));
#129972=CARTESIAN_POINT('Ctrl Pts',(78.9188131829234,7.17533979856319,129.961020583968));
#129973=CARTESIAN_POINT('Ctrl Pts',(77.8806350989911,8.91867304915029,129.849887465976));
#129974=CARTESIAN_POINT('Ctrl Pts',(78.7821585262321,10.7364547307989,129.738754347984));
#129975=CARTESIAN_POINT('Ctrl Pts',(80.7983488502959,10.9649344156327,129.627621229993));
#129976=CARTESIAN_POINT('Ctrl Pts',(82.0837557024546,9.39509072007935,129.516488112001));
#129977=CARTESIAN_POINT('Ctrl Pts',(81.4622383649526,7.46351776484872,129.40535499401));
#129978=CARTESIAN_POINT('Ctrl Pts',(79.501991229218,6.93845293557322,129.294221876018));
#129979=CARTESIAN_POINT('Ctrl Pts',(77.9984244521695,8.29966706882612,129.183088758027));
#129980=CARTESIAN_POINT('Ctrl Pts',(78.3249636333244,10.3029364690596,129.071955640035));
#129981=CARTESIAN_POINT('Ctrl Pts',(80.1882959521733,11.11146309486,128.960822522044));
#129982=CARTESIAN_POINT('Ctrl Pts',(81.3087886032814,10.3649024146173,128.886733776716));
#129983=CARTESIAN_POINT('Ctrl Pts',(81.5871520234028,9.83715927067298,128.849689404052));
#129984=CARTESIAN_POINT('Ctrl Pts',(81.4665867856348,10.2482426045797,140.150077107631));
#129985=CARTESIAN_POINT('Ctrl Pts',(81.8818028862442,9.76042436729594,140.113019595841));
#129986=CARTESIAN_POINT('Ctrl Pts',(82.1792335483859,8.34591351497726,140.038917711386));
#129987=CARTESIAN_POINT('Ctrl Pts',(80.6304328372915,6.81139143968391,139.927771454269));
#129988=CARTESIAN_POINT('Ctrl Pts',(78.5040710120652,7.28476689903274,139.816638336277));
#129989=CARTESIAN_POINT('Ctrl Pts',(77.7471978427393,9.32575105546619,139.705505218286));
#129990=CARTESIAN_POINT('Ctrl Pts',(79.052001832402,11.0696863673767,139.594372100294));
#129991=CARTESIAN_POINT('Ctrl Pts',(81.2245371200737,10.9188297783435,139.483238982303));
#129992=CARTESIAN_POINT('Ctrl Pts',(82.2762857547564,9.01204545951565,139.372105864311));
#129993=CARTESIAN_POINT('Ctrl Pts',(81.2447086479385,7.09410915124218,139.260972746319));
#129994=CARTESIAN_POINT('Ctrl Pts',(79.0739151359574,6.92058150399365,139.149839628328));
#129995=CARTESIAN_POINT('Ctrl Pts',(77.7507158599816,8.65018903028666,139.038706510336));
#129996=CARTESIAN_POINT('Ctrl Pts',(78.4861475554145,10.6999722259972,138.927573392345));
#129997=CARTESIAN_POINT('Ctrl Pts',(80.6071177683635,11.1938666447401,138.816440274353));
#129998=CARTESIAN_POINT('Ctrl Pts',(82.1724293290323,9.67985152240289,138.705307156362));
#129999=CARTESIAN_POINT('Ctrl Pts',(81.7494483427865,7.54360778660553,138.59417403837));
#130000=CARTESIAN_POINT('Ctrl Pts',(79.7253032382228,6.74031237896183,138.483040920378));
#130001=CARTESIAN_POINT('Ctrl Pts',(77.952571489165,8.00517160626547,138.371907802387));
#130002=CARTESIAN_POINT('Ctrl Pts',(78.0537268663851,10.1805371390946,138.260774684395));
#130003=CARTESIAN_POINT('Ctrl Pts',(79.936188036109,11.2754285172347,138.149641566404));
#130004=CARTESIAN_POINT('Ctrl Pts',(81.8770524189507,10.2877582050546,138.038508448412));
#130005=CARTESIAN_POINT('Ctrl Pts',(82.0999645517432,8.12148087415575,137.927375330421));
#130006=CARTESIAN_POINT('Ctrl Pts',(80.4009064711046,6.75925883703344,137.816242212429));
#130007=CARTESIAN_POINT('Ctrl Pts',(78.3349230095036,7.44785130128577,137.705109094438));
#130008=CARTESIAN_POINT('Ctrl Pts',(77.792883545948,9.55703134935834,137.593975976446));
#130009=CARTESIAN_POINT('Ctrl Pts',(79.2708839326172,11.1563943805989,137.482842858454));
#130010=CARTESIAN_POINT('Ctrl Pts',(81.4162000417767,10.782140400524,137.371709740463));
#130011=CARTESIAN_POINT('Ctrl Pts',(82.265354131664,8.77680138120206,137.260576622471));
#130012=CARTESIAN_POINT('Ctrl Pts',(81.0411669567573,6.9757425229748,137.14944350448));
#130013=CARTESIAN_POINT('Ctrl Pts',(78.8640628031065,7.02736378164124,137.038310386488));
#130014=CARTESIAN_POINT('Ctrl Pts',(77.7266130820991,8.88441934959255,136.927177268497));
#130015=CARTESIAN_POINT('Ctrl Pts',(78.6698565479946,10.8472588779883,136.816044150505));
#130016=CARTESIAN_POINT('Ctrl Pts',(80.8304996551003,11.1194143738573,136.704911032514));
#130017=CARTESIAN_POINT('Ctrl Pts',(82.2310367897109,9.45179841543078,136.593777914522));
#130018=CARTESIAN_POINT('Ctrl Pts',(81.5896412416254,7.37067876459188,136.482644796531));
#130019=CARTESIAN_POINT('Ctrl Pts',(79.493343461535,6.78077803785633,136.371511678539));
#130020=CARTESIAN_POINT('Ctrl Pts',(77.8607576872547,8.22199659860045,136.260378560547));
#130021=CARTESIAN_POINT('Ctrl Pts',(78.1860906773558,10.3752744942207,136.149245442556));
#130022=CARTESIAN_POINT('Ctrl Pts',(80.1715848743162,11.2698470424537,136.038112324564));
#130023=CARTESIAN_POINT('Ctrl Pts',(82.0000378407876,10.086966237124,135.926979206573));
#130024=CARTESIAN_POINT('Ctrl Pts',(81.9979774546478,7.90925114900429,135.815846088581));
#130025=CARTESIAN_POINT('Ctrl Pts',(80.1672894623882,6.7298323407723,135.70471297059));
#130026=CARTESIAN_POINT('Ctrl Pts',(78.1834915697017,7.62816032719385,135.593579852598));
#130027=CARTESIAN_POINT('Ctrl Pts',(77.8622336894994,9.78204997725095,135.482446734607));
#130028=CARTESIAN_POINT('Ctrl Pts',(79.4975436783292,11.2201767069408,135.371313616615));
#130029=CARTESIAN_POINT('Ctrl Pts',(81.5927214692403,10.6263103291348,135.260180498623));
#130030=CARTESIAN_POINT('Ctrl Pts',(82.2301778825965,8.54398072715382,135.149047380632));
#130031=CARTESIAN_POINT('Ctrl Pts',(80.8264877188542,6.87901791242533,135.03791426264));
#130032=CARTESIAN_POINT('Ctrl Pts',(78.666363464577,7.15526138528666,134.926781144649));
#130033=CARTESIAN_POINT('Ctrl Pts',(77.7268358589415,9.11988224653797,134.815648026657));
#130034=CARTESIAN_POINT('Ctrl Pts',(78.8677975460713,10.9747821572384,134.704514908666));
#130035=CARTESIAN_POINT('Ctrl Pts',(81.0449954820912,11.022283710966,134.593381790674));
#130036=CARTESIAN_POINT('Ctrl Pts',(82.2657724222796,9.21891161610627,134.482248672683));
#130037=CARTESIAN_POINT('Ctrl Pts',(81.4128252616645,7.21518299390877,134.371115554691));
#130038=CARTESIAN_POINT('Ctrl Pts',(79.2668048133133,6.84498914539877,134.259982436699));
#130039=CARTESIAN_POINT('Ctrl Pts',(77.7918334580994,8.44714605142053,134.148849318708));
#130040=CARTESIAN_POINT('Ctrl Pts',(78.3378630346208,10.5552966513015,134.037716200716));
#130041=CARTESIAN_POINT('Ctrl Pts',(80.405145782931,11.2399785400318,133.926583082725));
#130042=CARTESIAN_POINT('Ctrl Pts',(82.1016231643198,9.87454390422866,133.815449964733));
#130043=CARTESIAN_POINT('Ctrl Pts',(81.8746123066417,7.70869226556286,133.704316846742));
#130044=CARTESIAN_POINT('Ctrl Pts',(79.9318824819036,6.72469629083107,133.59318372875));
#130045=CARTESIAN_POINT('Ctrl Pts',(78.0514964908067,7.82314782581201,133.482050610758));
#130046=CARTESIAN_POINT('Ctrl Pts',(77.9544576036744,9.99870079106,133.370917492767));
#130047=CARTESIAN_POINT('Ctrl Pts',(79.7295796294233,11.2602034838498,133.259784374775));
#130048=CARTESIAN_POINT('Ctrl Pts',(81.7522010219662,10.453078987478,133.148651256784));
#130049=CARTESIAN_POINT('Ctrl Pts',(82.1711390732453,8.31603940913473,133.037518138792));
#130050=CARTESIAN_POINT('Ctrl Pts',(80.6029651894892,6.80498748397788,132.926385020801));
#130051=CARTESIAN_POINT('Ctrl Pts',(78.482933831834,7.30289740833519,132.815251902809));
#130052=CARTESIAN_POINT('Ctrl Pts',(77.7513811424265,9.35406242189131,132.704118784817));
#130053=CARTESIAN_POINT('Ctrl Pts',(79.0778529362468,11.0811755711711,132.592985666826));
#130054=CARTESIAN_POINT('Ctrl Pts',(81.2483100181675,10.9035149234434,132.481852548834));
#130055=CARTESIAN_POINT('Ctrl Pts',(82.2762646384599,8.98368249616185,132.370719430843));
#130056=CARTESIAN_POINT('Ctrl Pts',(81.2208922687267,7.07878449064595,132.259586312851));
#130057=CARTESIAN_POINT('Ctrl Pts',(79.0481112408112,6.93225853759174,132.14845319486));
#130058=CARTESIAN_POINT('Ctrl Pts',(77.7465362712657,8.67821095645413,132.037320076868));
#130059=CARTESIAN_POINT('Ctrl Pts',(78.5074200017588,10.7186773734432,131.926186958876));
#130060=CARTESIAN_POINT('Ctrl Pts',(80.634371693951,11.1861426118154,131.815053840885));
#130061=CARTESIAN_POINT('Ctrl Pts',(82.1807214433505,9.65276408603656,131.703920722893));
#130062=CARTESIAN_POINT('Ctrl Pts',(81.7311890951541,7.52195017634236,131.592787604902));
#130063=CARTESIAN_POINT('Ctrl Pts',(79.6972043487107,6.74390564038746,131.48165448691));
#130064=CARTESIAN_POINT('Ctrl Pts',(77.9403500990677,8.03072746206706,131.370521368919));
#130065=CARTESIAN_POINT('Ctrl Pts',(78.0685685082022,10.2046656592093,131.259388250927));
#130066=CARTESIAN_POINT('Ctrl Pts',(79.9645090340951,11.2760464328285,131.148255132935));
#130067=CARTESIAN_POINT('Ctrl Pts',(81.892932298994,10.2642999207466,131.037122014944));
#130068=CARTESIAN_POINT('Ctrl Pts',(82.0888693981082,8.09541637123634,130.925988896952));
#130069=CARTESIAN_POINT('Ctrl Pts',(80.3729910492246,6.75444333747484,130.814855778961));
#130070=CARTESIAN_POINT('Ctrl Pts',(78.3157365248911,7.46869219737679,130.703722660969));
#130071=CARTESIAN_POINT('Ctrl Pts',(77.7999864016918,9.58445412383093,130.592589542978));
#130072=CARTESIAN_POINT('Ctrl Pts',(79.2977749538362,11.1653008492713,130.481456424986));
#130073=CARTESIAN_POINT('Ctrl Pts',(81.4382682469794,10.7643785681889,130.370323306995));
#130074=CARTESIAN_POINT('Ctrl Pts',(82.2624003183689,8.74862848409216,130.259190189003));
#130075=CARTESIAN_POINT('Ctrl Pts',(81.0158976646619,6.96294164833859,130.148057071012));
#130076=CARTESIAN_POINT('Ctrl Pts',(78.8395991555924,7.04165459191484,130.03692395302));
#130077=CARTESIAN_POINT('Ctrl Pts',(77.725358113977,8.91271456426536,129.925790835029));
#130078=CARTESIAN_POINT('Ctrl Pts',(78.6929323848621,10.8636774922421,129.814657717037));
#130079=CARTESIAN_POINT('Ctrl Pts',(80.8568405250446,11.1088969261305,129.703524599046));
#130080=CARTESIAN_POINT('Ctrl Pts',(82.2364237507125,9.42403736149622,129.592391481054));
#130081=CARTESIAN_POINT('Ctrl Pts',(81.5693704423849,7.35094615016893,129.481258363063));
#130082=CARTESIAN_POINT('Ctrl Pts',(79.4655042135082,6.7874120211574,129.370125245071));
#130083=CARTESIAN_POINT('Ctrl Pts',(77.8517773994617,8.24835660973194,129.258992127079));
#130084=CARTESIAN_POINT('Ctrl Pts',(78.2022407380443,10.3983971641407,129.147859009088));
#130085=CARTESIAN_POINT('Ctrl Pts',(80.2020916075274,11.2661611476506,129.036725891096));
#130086=CARTESIAN_POINT('Ctrl Pts',(81.4046780597132,10.4649030948587,128.962637145768));
#130087=CARTESIAN_POINT('Ctrl Pts',(81.7034360011341,9.89849442228607,128.925592773105));
#130088=CARTESIAN_POINT('Ctrl Pts',(81.5667024019587,10.3334530939303,140.225980476683));
#130089=CARTESIAN_POINT('Ctrl Pts',(82.0102629662079,9.81233425421511,140.188922964893));
#130090=CARTESIAN_POINT('Ctrl Pts',(82.327997543771,8.30126271611657,140.114821080439));
#130091=CARTESIAN_POINT('Ctrl Pts',(80.6734689348986,6.66198746505808,140.00367482332));
#130092=CARTESIAN_POINT('Ctrl Pts',(78.4019523689201,7.16767759976703,139.892541705329));
#130093=CARTESIAN_POINT('Ctrl Pts',(77.5934117329509,9.34798824456784,139.781408587337));
#130094=CARTESIAN_POINT('Ctrl Pts',(78.9872873390269,11.2109721939615,139.670275469346));
#130095=CARTESIAN_POINT('Ctrl Pts',(81.3081293695664,11.0498174756014,139.559142351354));
#130096=CARTESIAN_POINT('Ctrl Pts',(82.4316749574265,9.01286773516624,139.448009233363));
#130097=CARTESIAN_POINT('Ctrl Pts',(81.3296778939815,6.96400472180219,139.336876115371));
#130098=CARTESIAN_POINT('Ctrl Pts',(79.010696540345,6.77863131982322,139.225742997379));
#130099=CARTESIAN_POINT('Ctrl Pts',(77.5971699054081,8.62630940640575,139.114609879388));
#130100=CARTESIAN_POINT('Ctrl Pts',(78.3828053788741,10.8160197513165,139.003476761396));
#130101=CARTESIAN_POINT('Ctrl Pts',(80.6485622775848,11.3436295591627,138.892343643405));
#130102=CARTESIAN_POINT('Ctrl Pts',(82.3207288387009,9.72626115519157,138.781210525413));
#130103=CARTESIAN_POINT('Ctrl Pts',(81.8688733238243,7.44418809628693,138.670077407422));
#130104=CARTESIAN_POINT('Ctrl Pts',(79.7065512380843,6.58605623735781,138.55894428943));
#130105=CARTESIAN_POINT('Ctrl Pts',(77.8128050810336,7.93726027721854,138.447811171439));
#130106=CARTESIAN_POINT('Ctrl Pts',(77.9208657658932,10.2611257578052,138.336678053447));
#130107=CARTESIAN_POINT('Ctrl Pts',(79.9318319528847,11.4307592011295,138.225544935455));
#130108=CARTESIAN_POINT('Ctrl Pts',(82.0051882112789,10.3756662017978,138.114411817464));
#130109=CARTESIAN_POINT('Ctrl Pts',(82.2433172993713,8.06150932347929,138.003278699472));
#130110=CARTESIAN_POINT('Ctrl Pts',(80.4282740969664,6.60629606336752,137.892145581481));
#130111=CARTESIAN_POINT('Ctrl Pts',(78.2212575852933,7.34189485525748,137.781012463489));
#130112=CARTESIAN_POINT('Ctrl Pts',(77.6422161417002,9.59505674096755,137.669879345498));
#130113=CARTESIAN_POINT('Ctrl Pts',(79.2211112869253,11.3035992746874,137.558746227506));
#130114=CARTESIAN_POINT('Ctrl Pts',(81.5128760390032,10.9037970841391,137.447613109514));
#130115=CARTESIAN_POINT('Ctrl Pts',(82.4199970940205,8.7615648691167,137.336479991523));
#130116=CARTESIAN_POINT('Ctrl Pts',(81.1122415584055,6.83755787076364,137.225346873531));
#130117=CARTESIAN_POINT('Ctrl Pts',(78.78651877115,6.89270302189758,137.11421375554));
#130118=CARTESIAN_POINT('Ctrl Pts',(77.5714217666873,8.87652930983221,137.003080637548));
#130119=CARTESIAN_POINT('Ctrl Pts',(78.5790551492632,10.9733608331476,136.891947519557));
#130120=CARTESIAN_POINT('Ctrl Pts',(80.8871931870763,11.2640948512505,136.780814401565));
#130121=CARTESIAN_POINT('Ctrl Pts',(82.3833371004942,9.48264014757921,136.669681283574));
#130122=CARTESIAN_POINT('Ctrl Pts',(81.6981570923054,7.25945418431468,136.558548165582));
#130123=CARTESIAN_POINT('Ctrl Pts',(79.4587568744269,6.62928425877995,136.44741504759));
#130124=CARTESIAN_POINT('Ctrl Pts',(77.7147236681948,8.16888669007266,136.336281929599));
#130125=CARTESIAN_POINT('Ctrl Pts',(78.0622653084306,10.4691567349117,136.225148811607));
#130126=CARTESIAN_POINT('Ctrl Pts',(80.1832980068851,11.4247967105141,136.114015693616));
#130127=CARTESIAN_POINT('Ctrl Pts',(82.136569154899,10.1611672975854,136.002882575624));
#130128=CARTESIAN_POINT('Ctrl Pts',(82.134368117807,7.83479187080711,135.891749457633));
#130129=CARTESIAN_POINT('Ctrl Pts',(80.1787093713873,6.57486078601119,135.780616339641));
#130130=CARTESIAN_POINT('Ctrl Pts',(78.0594887743418,7.53451256240715,135.66948322165));
#130131=CARTESIAN_POINT('Ctrl Pts',(77.7163004287961,9.83543612271155,135.558350103658));
#130132=CARTESIAN_POINT('Ctrl Pts',(79.4632438163555,11.371735661065,135.447216985666));
#130133=CARTESIAN_POINT('Ctrl Pts',(81.7014475897037,10.7373293718058,135.336083867675));
#130134=CARTESIAN_POINT('Ctrl Pts',(82.3824195606306,8.51285086085221,135.224950749683));
#130135=CARTESIAN_POINT('Ctrl Pts',(80.8829073785483,6.73423041604996,135.113817631692));
#130136=CARTESIAN_POINT('Ctrl Pts',(78.5753236127225,7.0293314743006,135.0026845137));
#130137=CARTESIAN_POINT('Ctrl Pts',(77.5716597512496,9.12806593202865,134.891551395709));
#130138=CARTESIAN_POINT('Ctrl Pts',(78.7905084639736,11.1095894081381,134.780418277717));
#130139=CARTESIAN_POINT('Ctrl Pts',(81.1163314355921,11.1603336252896,134.669285159726));
#130140=CARTESIAN_POINT('Ctrl Pts',(82.4204439389795,9.23385547867315,134.558152041734));
#130141=CARTESIAN_POINT('Ctrl Pts',(81.5092708816678,7.09334359351305,134.447018923742));
#130142=CARTESIAN_POINT('Ctrl Pts',(79.2167537091307,6.69787869683471,134.335885805751));
#130143=CARTESIAN_POINT('Ctrl Pts',(77.6410943702708,8.40940582742477,134.224752687759));
#130144=CARTESIAN_POINT('Ctrl Pts',(78.2243983093599,10.6614679903157,134.113619569768));
#130145=CARTESIAN_POINT('Ctrl Pts',(80.4328028027243,11.3928892537269,134.002486451776));
#130146=CARTESIAN_POINT('Ctrl Pts',(82.2450891360831,9.93424408892397,133.891353333785));
#130147=CARTESIAN_POINT('Ctrl Pts',(82.0025815262513,7.62054196244875,133.780220215793));
#130148=CARTESIAN_POINT('Ctrl Pts',(79.9272324827536,6.56937412687972,133.669087097802));
#130149=CARTESIAN_POINT('Ctrl Pts',(77.9184831351412,7.74281075889249,133.55795397981));
#130150=CARTESIAN_POINT('Ctrl Pts',(77.8148199499532,10.0668764668532,133.446820861818));
#130151=CARTESIAN_POINT('Ctrl Pts',(79.7111195544165,11.4144948405014,133.335687743827));
#130152=CARTESIAN_POINT('Ctrl Pts',(81.8718139129015,10.5522725025318,133.224554625835));
#130153=CARTESIAN_POINT('Ctrl Pts',(82.3193505044213,8.26934927339481,133.113421507844));
#130154=CARTESIAN_POINT('Ctrl Pts',(80.6441262255484,6.65514634737931,133.002288389852));
#130155=CARTESIAN_POINT('Ctrl Pts',(78.3793722724926,7.18704577678262,132.891155271861));
#130156=CARTESIAN_POINT('Ctrl Pts',(77.597880602937,9.37823226845748,132.780022153869));
#130157=CARTESIAN_POINT('Ctrl Pts',(79.0149031520722,11.2232457009628,132.668889035877));
#130158=CARTESIAN_POINT('Ctrl Pts',(81.333525109464,11.0334571618495,132.557755917886));
#130159=CARTESIAN_POINT('Ctrl Pts',(82.4316523996396,8.98256859211635,132.446622799894));
#130160=CARTESIAN_POINT('Ctrl Pts',(81.3042357047549,6.94763393297434,132.335489681903));
#130161=CARTESIAN_POINT('Ctrl Pts',(78.98313115867,6.79110547871043,132.224356563911));
#130162=CARTESIAN_POINT('Ctrl Pts',(77.5927049997205,8.65624423158219,132.11322344592));
#130163=CARTESIAN_POINT('Ctrl Pts',(78.40552997527,10.836001793784,132.002090327928));
#130164=CARTESIAN_POINT('Ctrl Pts',(80.6776766751088,11.3353782500316,131.890957209937));
#130165=CARTESIAN_POINT('Ctrl Pts',(82.3295870089414,9.69732461216955,131.779824091945));
#130166=CARTESIAN_POINT('Ctrl Pts',(81.8493676202382,7.42105204300162,131.668690973954));
#130167=CARTESIAN_POINT('Ctrl Pts',(79.6765341957092,6.58989479049461,131.557557855962));
#130168=CARTESIAN_POINT('Ctrl Pts',(77.7997494054962,7.96456068730038,131.44642473797));
#130169=CARTESIAN_POINT('Ctrl Pts',(77.9367205629714,10.2869013960352,131.335291619979));
#130170=CARTESIAN_POINT('Ctrl Pts',(79.9620862658279,11.4314192983393,131.224158501987));
#130171=CARTESIAN_POINT('Ctrl Pts',(82.022152121257,10.3506065525964,131.113025383996));
#130172=CARTESIAN_POINT('Ctrl Pts',(82.2314647421138,8.03366554380687,131.001892266004));
#130173=CARTESIAN_POINT('Ctrl Pts',(80.3984530465246,6.60115183678714,130.890759148013));
#130174=CARTESIAN_POINT('Ctrl Pts',(78.2007613474834,7.36415844189591,130.779626030021));
#130175=CARTESIAN_POINT('Ctrl Pts',(77.6498038693843,9.62435151373887,130.668492912029));
#130176=CARTESIAN_POINT('Ctrl Pts',(79.2498380066448,11.3131137377922,130.557359794038));
#130177=CARTESIAN_POINT('Ctrl Pts',(81.5364507162309,10.8848227515901,130.446226676046));
#130178=CARTESIAN_POINT('Ctrl Pts',(82.416841640535,8.73146876706222,130.335093558055));
#130179=CARTESIAN_POINT('Ctrl Pts',(81.0852472741196,6.82388315254297,130.223960440063));
#130180=CARTESIAN_POINT('Ctrl Pts',(78.7603851282614,6.90796938526652,130.112827322072));
#130181=CARTESIAN_POINT('Ctrl Pts',(77.5700811289627,8.90675607938041,130.00169420408));
#130182=CARTESIAN_POINT('Ctrl Pts',(78.6037062434921,10.9909002536853,129.890561086088));
#130183=CARTESIAN_POINT('Ctrl Pts',(80.9153321997933,11.2528594366284,129.779427968097));
#130184=CARTESIAN_POINT('Ctrl Pts',(82.3890917989704,9.45298400291311,129.668294850105));
#130185=CARTESIAN_POINT('Ctrl Pts',(81.6765025198171,7.23837453548914,129.557161732114));
#130186=CARTESIAN_POINT('Ctrl Pts',(79.4290171977985,6.63637110674158,129.446028614122));
#130187=CARTESIAN_POINT('Ctrl Pts',(77.7051303467539,8.19704615063774,129.334895496131));
#130188=CARTESIAN_POINT('Ctrl Pts',(78.0795178427644,10.4938578592218,129.223762378139));
#130189=CARTESIAN_POINT('Ctrl Pts',(80.2158872628815,11.4208592004411,129.112629260147));
#130190=CARTESIAN_POINT('Ctrl Pts',(81.5005675161451,10.5649037751,129.03854051482));
#130191=CARTESIAN_POINT('Ctrl Pts',(81.8197199788653,9.95982957389915,129.001496142156));
#130192=CARTESIAN_POINT('Ctrl Pts',(81.2690708798525,10.0793586530483,140.));
#130193=CARTESIAN_POINT('Ctrl Pts',(81.3143922493461,10.037078625412,140.));
#130194=CARTESIAN_POINT('Ctrl Pts',(81.3569831621752,9.99222888973338,140.));
#130195=CARTESIAN_POINT('Ctrl Pts',(81.3968454123345,9.94515461985499,140.));
#130196=CARTESIAN_POINT('Ctrl Pts',(81.4393469149689,9.89496359458048,140.));
#130197=CARTESIAN_POINT('Ctrl Pts',(81.4787471926403,9.84224348169698,140.));
#130198=CARTESIAN_POINT('Ctrl Pts',(81.5150195594611,9.78735790922335,140.));
#130199=CARTESIAN_POINT('Ctrl Pts',(81.5467578804294,9.73933303330892,140.));
#130200=CARTESIAN_POINT('Ctrl Pts',(81.5761011504664,9.68964900085175,140.));
#130201=CARTESIAN_POINT('Ctrl Pts',(81.6030085858433,9.63852184375101,140.));
#130202=CARTESIAN_POINT('Ctrl Pts',(81.6165037566978,9.61287949951723,140.));
#130203=CARTESIAN_POINT('Ctrl Pts',(81.6293858497916,9.58687379163623,140.));
#130204=CARTESIAN_POINT('Ctrl Pts',(81.6416473796641,9.56053013392403,140.));
#130205=CARTESIAN_POINT('Ctrl Pts',(81.6472597696334,9.54847202357099,140.));
#130206=CARTESIAN_POINT('Ctrl Pts',(81.6527427313326,9.53634140530439,140.));
#130207=CARTESIAN_POINT('Ctrl Pts',(81.6580870166726,9.5241607216166,140.));
#130208=CARTESIAN_POINT('Ctrl Pts',(81.6852360971005,9.46228259571773,140.));
#130209=CARTESIAN_POINT('Ctrl Pts',(81.7088626185403,9.39900435672435,140.));
#130210=CARTESIAN_POINT('Ctrl Pts',(81.7289426467891,9.33469347024794,140.));
#130211=CARTESIAN_POINT('Ctrl Pts',(81.7490226750378,9.27038258377154,140.));
#130212=CARTESIAN_POINT('Ctrl Pts',(81.7655566446948,9.20503811827903,140.));
#130213=CARTESIAN_POINT('Ctrl Pts',(81.7784823019253,9.13899201824649,140.));
#130214=CARTESIAN_POINT('Ctrl Pts',(81.7914980138043,9.07248576688647,140.));
#130215=CARTESIAN_POINT('Ctrl Pts',(81.800855473018,9.00526711378445,140.));
#130216=CARTESIAN_POINT('Ctrl Pts',(81.8064450545183,8.93765313125535,140.));
#130217=CARTESIAN_POINT('Ctrl Pts',(81.8076966254415,8.92251359092883,140.));
#130218=CARTESIAN_POINT('Ctrl Pts',(81.8087590894417,8.90735417722168,140.));
#130219=CARTESIAN_POINT('Ctrl Pts',(81.8096308609416,8.8921783781706,140.));
#130220=CARTESIAN_POINT('Ctrl Pts',(81.8102881062911,8.8807370505378,140.));
#130221=CARTESIAN_POINT('Ctrl Pts',(81.8108368598249,8.86928658800379,140.));
#130222=CARTESIAN_POINT('Ctrl Pts',(81.8112761266604,8.85784267362559,140.));
#130223=CARTESIAN_POINT('Ctrl Pts',(81.8139681483841,8.78770929767787,140.));
#130224=CARTESIAN_POINT('Ctrl Pts',(81.8125602359496,8.71769045278861,140.));
#130225=CARTESIAN_POINT('Ctrl Pts',(81.8069981196216,8.64814732532177,140.));
#130226=CARTESIAN_POINT('Ctrl Pts',(81.8020258450083,8.58597898743637,140.));
#130227=CARTESIAN_POINT('Ctrl Pts',(81.793733374456,8.52418985638038,140.));
#130228=CARTESIAN_POINT('Ctrl Pts',(81.7820488148449,8.46302583141971,140.));
#130229=CARTESIAN_POINT('Ctrl Pts',(81.769316661712,8.39637807078986,140.));
#130230=CARTESIAN_POINT('Ctrl Pts',(81.7525579964158,8.33047169570494,140.));
#130231=CARTESIAN_POINT('Ctrl Pts',(81.7320178331077,8.26552006538765,140.));
#130232=CARTESIAN_POINT('Ctrl Pts',(81.7240897912002,8.2404501942579,140.));
#130233=CARTESIAN_POINT('Ctrl Pts',(81.7155978327267,8.2155226071289,140.));
#130234=CARTESIAN_POINT('Ctrl Pts',(81.7065540378326,8.19074989375515,140.));
#130235=CARTESIAN_POINT('Ctrl Pts',(81.7025873788784,8.17988444330244,140.));
#130236=CARTESIAN_POINT('Ctrl Pts',(81.6985146637445,8.16904935856075,140.));
#130237=CARTESIAN_POINT('Ctrl Pts',(81.6943419939996,8.15825823120868,140.));
#130238=CARTESIAN_POINT('Ctrl Pts',(81.6688285338256,8.09227673380644,140.));
#130239=CARTESIAN_POINT('Ctrl Pts',(81.6395390164229,8.0278166187107,140.));
#130240=CARTESIAN_POINT('Ctrl Pts',(81.6067965122877,7.96510411531983,140.));
#130241=CARTESIAN_POINT('Ctrl Pts',(81.5740540081525,7.90239161192896,140.));
#130242=CARTESIAN_POINT('Ctrl Pts',(81.5378580152312,7.84142593331998,140.));
#130243=CARTESIAN_POINT('Ctrl Pts',(81.4984773919093,7.78243697400106,140.));
#130244=CARTESIAN_POINT('Ctrl Pts',(81.4582451906682,7.72217242046859,140.));
#130245=CARTESIAN_POINT('Ctrl Pts',(81.4146887664041,7.66397006974518,140.));
#130246=CARTESIAN_POINT('Ctrl Pts',(81.3680445980429,7.60809196964191,140.));
#130247=CARTESIAN_POINT('Ctrl Pts',(81.3573469119398,7.59527651176268,140.));
#130248=CARTESIAN_POINT('Ctrl Pts',(81.3464866201888,7.58258341222455,140.));
#130249=CARTESIAN_POINT('Ctrl Pts',(81.3354662478833,7.57001603639548,140.));
#130250=CARTESIAN_POINT('Ctrl Pts',(81.3227850921236,7.55555474180744,140.));
#130251=CARTESIAN_POINT('Ctrl Pts',(81.3098875424283,7.54125535227706,140.));
#130252=CARTESIAN_POINT('Ctrl Pts',(81.2968012384801,7.52714834847591,140.));
#130253=CARTESIAN_POINT('Ctrl Pts',(81.2459376695597,7.47231754499339,140.));
#130254=CARTESIAN_POINT('Ctrl Pts',(81.1921776208598,7.42033184651139,140.));
#130255=CARTESIAN_POINT('Ctrl Pts',(81.1358057253517,7.37145486543547,140.));
#130256=CARTESIAN_POINT('Ctrl Pts',(81.0936523414515,7.33490597651479,140.));
#130257=CARTESIAN_POINT('Ctrl Pts',(81.050037349269,7.30009557097858,140.));
#130258=CARTESIAN_POINT('Ctrl Pts',(81.005063375939,7.26714361886256,140.));
#130259=CARTESIAN_POINT('Ctrl Pts',(80.9910000906874,7.25683959927322,140.));
#130260=CARTESIAN_POINT('Ctrl Pts',(80.9768038313551,7.24671737660939,140.));
#130261=CARTESIAN_POINT('Ctrl Pts',(80.9624774943437,7.23678084594061,140.));
#130262=CARTESIAN_POINT('Ctrl Pts',(80.9486909780282,7.22721872674186,140.));
#130263=CARTESIAN_POINT('Ctrl Pts',(80.9347910474626,7.21783351877335,140.));
#130264=CARTESIAN_POINT('Ctrl Pts',(80.9207856469263,7.20863142672219,140.));
#130265=CARTESIAN_POINT('Ctrl Pts',(80.8578389195166,7.16727298228203,140.));
#130266=CARTESIAN_POINT('Ctrl Pts',(80.7927341061665,7.12958962170196,140.));
#130267=CARTESIAN_POINT('Ctrl Pts',(80.7257321762408,7.09586020443097,140.));
#130268=CARTESIAN_POINT('Ctrl Pts',(80.6745101548169,7.07007454518227,140.));
#130269=CARTESIAN_POINT('Ctrl Pts',(80.6221784116493,7.04660013039904,140.));
#130270=CARTESIAN_POINT('Ctrl Pts',(80.5688396787843,7.02557680443979,140.));
#130271=CARTESIAN_POINT('Ctrl Pts',(80.5565366069901,7.02072757996939,140.));
#130272=CARTESIAN_POINT('Ctrl Pts',(80.5441799163443,7.0160088282093,140.));
#130273=CARTESIAN_POINT('Ctrl Pts',(80.5317714801634,7.01141998135025,140.));
#130274=CARTESIAN_POINT('Ctrl Pts',(79.4691328668544,7.01221613569387,139.998440578768));
#130275=CARTESIAN_POINT('Ctrl Pts',(78.8081758252084,7.18873450679631,139.961396206104));
#130276=CARTESIAN_POINT('Ctrl Pts',(77.687752744404,8.25079161293192,139.887307460776));
#130277=CARTESIAN_POINT('Ctrl Pts',(78.116148705963,10.5399996648632,139.776174342785));
#130278=CARTESIAN_POINT('Ctrl Pts',(80.2721800561424,11.416134581678,139.665041224793));
#130279=CARTESIAN_POINT('Ctrl Pts',(82.177427932532,10.0826818014991,139.553908106802));
#130280=CARTESIAN_POINT('Ctrl Pts',(82.090625956823,7.75746322787376,139.44277498881));
#130281=CARTESIAN_POINT('Ctrl Pts',(80.0900009572206,6.56988012499553,139.331641870819));
#130282=CARTESIAN_POINT('Ctrl Pts',(78.00719905694,7.60623453967738,139.220508752827));
#130283=CARTESIAN_POINT('Ctrl Pts',(77.7481914138751,9.91831763289069,139.109375634835));
#130284=CARTESIAN_POINT('Ctrl Pts',(79.5501743653611,11.3898715478751,138.998242516844));
#130285=CARTESIAN_POINT('Ctrl Pts',(81.7638325852258,10.6741447881572,138.887109398852));
#130286=CARTESIAN_POINT('Ctrl Pts',(82.3631729758628,8.426163172343,138.775976280861));
#130287=CARTESIAN_POINT('Ctrl Pts',(80.7996389804333,6.70338530479118,138.664843162869));
#130288=CARTESIAN_POINT('Ctrl Pts',(78.5042465888265,7.08255681422626,138.553710044878));
#130289=CARTESIAN_POINT('Ctrl Pts',(77.5778252847861,9.21664915934671,138.442576926886));
#130290=CARTESIAN_POINT('Ctrl Pts',(78.8682742548729,11.1524550005147,138.331443808895));
#130291=CARTESIAN_POINT('Ctrl Pts',(81.1945228587917,11.1182496311054,138.220310690903));
#130292=CARTESIAN_POINT('Ctrl Pts',(82.4274972791361,9.14533866655995,138.109177572911));
#130293=CARTESIAN_POINT('Ctrl Pts',(81.4387305695618,7.03940811177544,137.99804445492));
#130294=CARTESIAN_POINT('Ctrl Pts',(79.1331810513629,6.72788838316243,137.886911336928));
#130295=CARTESIAN_POINT('Ctrl Pts',(77.62097833476,8.49589465433908,137.775778218937));
#130296=CARTESIAN_POINT('Ctrl Pts',(78.2861498922971,10.7252779701539,137.664645100945));
#130297=CARTESIAN_POINT('Ctrl Pts',(80.519904520617,11.3756189858562,137.553511982953));
#130298=CARTESIAN_POINT('Ctrl Pts',(82.2778220705136,9.85170000007408,137.442378864962));
#130299=CARTESIAN_POINT('Ctrl Pts',(81.9509872062522,7.54827165270313,137.331245746971));
#130300=CARTESIAN_POINT('Ctrl Pts',(79.8385320612198,6.5735222277288,137.220112628979));
#130301=CARTESIAN_POINT('Ctrl Pts',(77.8738587288312,7.81958076542601,137.108979510988));
#130302=CARTESIAN_POINT('Ctrl Pts',(77.8551135720406,10.1460054473293,136.997846392996));
#130303=CARTESIAN_POINT('Ctrl Pts',(79.7994528959673,11.4235608375628,136.886713275004));
#130304=CARTESIAN_POINT('Ctrl Pts',(81.9273408229903,10.4829779588041,136.775580157013));
#130305=CARTESIAN_POINT('Ctrl Pts',(82.2912505694032,8.18511528271877,136.664447039021));
#130306=CARTESIAN_POINT('Ctrl Pts',(80.5581176119615,6.63306717343212,136.55331392103));
#130307=CARTESIAN_POINT('Ctrl Pts',(78.3141734487542,7.24732914859208,136.442180803038));
#130308=CARTESIAN_POINT('Ctrl Pts',(77.6131640987352,9.46570447141138,136.331047685047));
#130309=CARTESIAN_POINT('Ctrl Pts',(79.0966809104985,11.2578487320464,136.219914567055));
#130310=CARTESIAN_POINT('Ctrl Pts',(81.406950907267,10.9835209650521,136.108781449063));
#130311=CARTESIAN_POINT('Ctrl Pts',(82.4295240566564,8.89379674021785,135.997648331072));
#130312=CARTESIAN_POINT('Ctrl Pts',(81.228501164259,6.90127391885572,135.88651521308));
#130313=CARTESIAN_POINT('Ctrl Pts',(78.903105652997,6.82958781201049,135.775382095089));
#130314=CARTESIAN_POINT('Ctrl Pts',(77.5816310214531,8.74434836620449,135.664248977097));
#130315=CARTESIAN_POINT('Ctrl Pts',(78.4735428651507,10.8930913579985,135.553115859106));
#130316=CARTESIAN_POINT('Ctrl Pts',(80.7625283594298,11.3092026276025,135.441982741114));
#130317=CARTESIAN_POINT('Ctrl Pts',(82.3536178863351,9.61184076309495,135.330849623122));
#130318=CARTESIAN_POINT('Ctrl Pts',(81.7905836861691,7.35449815038521,135.219716505131));
#130319=CARTESIAN_POINT('Ctrl Pts',(79.5887368197341,6.60318359676461,135.108583387139));
#130320=CARTESIAN_POINT('Ctrl Pts',(77.7632942030395,8.04552975315939,134.997450269148));
#130321=CARTESIAN_POINT('Ctrl Pts',(77.9849727676055,10.3614446470455,134.886317151156));
#130322=CARTESIAN_POINT('Ctrl Pts',(80.050883565958,11.4313118140165,134.775184033165));
#130323=CARTESIAN_POINT('Ctrl Pts',(82.070223721988,10.2759467132991,134.664050915173));
#130324=CARTESIAN_POINT('Ctrl Pts',(82.1948136444431,7.95278495979708,134.552917797182));
#130325=CARTESIAN_POINT('Ctrl Pts',(80.3106237324807,6.58807562907116,134.44178467919));
#130326=CARTESIAN_POINT('Ctrl Pts',(78.1421387545208,7.43085441503748,134.330651561199));
#130327=CARTESIAN_POINT('Ctrl Pts',(77.6740415131297,9.70977700132987,134.219518443207));
#130328=CARTESIAN_POINT('Ctrl Pts',(79.3347530277562,11.3390837394547,134.108385325215));
#130329=CARTESIAN_POINT('Ctrl Pts',(81.6043247552459,10.8275689737917,133.997252207224));
#130330=CARTESIAN_POINT('Ctrl Pts',(82.4055553211276,8.64339115090071,133.886119089232));
#130331=CARTESIAN_POINT('Ctrl Pts',(81.0051269753784,6.78559578269294,133.774985971241));
#130332=CARTESIAN_POINT('Ctrl Pts',(78.6847668603508,6.95451031226528,133.663852853249));
#130333=CARTESIAN_POINT('Ctrl Pts',(77.5681598818021,8.995537513742,133.552719735258));
#130334=CARTESIAN_POINT('Ctrl Pts',(78.6772686957224,11.0406489582838,133.441586617266));
#130335=CARTESIAN_POINT('Ctrl Pts',(80.9969932615145,11.218078157044,133.330453499275));
#130336=CARTESIAN_POINT('Ctrl Pts',(82.4042303530961,9.36543492377197,133.219320381283));
#130337=CARTESIAN_POINT('Ctrl Pts',(81.6110211959397,7.17833126488543,133.108187263291));
#130338=CARTESIAN_POINT('Ctrl Pts',(79.3433420310828,6.65849053255848,132.9970541453));
#130339=CARTESIAN_POINT('Ctrl Pts',(77.6766620851849,8.2816914257486,132.885921027308));
#130340=CARTESIAN_POINT('Ctrl Pts',(78.1363924446149,10.5623165984436,132.774787909317));
#130341=CARTESIAN_POINT('Ctrl Pts',(80.3017697896119,11.4130481280609,132.663654791325));
#130342=CARTESIAN_POINT('Ctrl Pts',(82.1909555456132,10.0552630342281,132.552521673334));
#130343=CARTESIAN_POINT('Ctrl Pts',(82.0748925510988,7.73165967672142,132.441388555342));
#130344=CARTESIAN_POINT('Ctrl Pts',(80.0598062268449,6.56889130446804,132.33025543735));
#130345=CARTESIAN_POINT('Ctrl Pts',(77.9899828898302,7.63116929787119,132.219122319359));
#130346=CARTESIAN_POINT('Ctrl Pts',(77.7598063255501,9.94625502651435,132.107989201367));
#130347=CARTESIAN_POINT('Ctrl Pts',(79.5799431852807,11.3952909106561,131.996856083376));
#130348=CARTESIAN_POINT('Ctrl Pts',(81.7845325751376,10.6520622756351,131.885722965384));
#130349=CARTESIAN_POINT('Ctrl Pts',(82.3558475136698,8.39680122141269,131.774589847393));
#130350=CARTESIAN_POINT('Ctrl Pts',(80.7709980825209,6.69361143103145,131.663456729401));
#130351=CARTESIAN_POINT('Ctrl Pts',(78.4805008598881,7.10131923752851,131.55232361141));
#130352=CARTESIAN_POINT('Ctrl Pts',(77.580709057541,9.24677440920892,131.441190493418));
#130353=CARTESIAN_POINT('Ctrl Pts',(78.8951475473763,11.1663719285885,131.330057375426));
#130354=CARTESIAN_POINT('Ctrl Pts',(81.2207904898933,11.1032205914513,131.218924257435));
#130355=CARTESIAN_POINT('Ctrl Pts',(82.429117923205,9.11511898686653,131.107791139443));
#130356=CARTESIAN_POINT('Ctrl Pts',(81.4142210302046,7.02165595486222,130.996658021452));
#130357=CARTESIAN_POINT('Ctrl Pts',(79.104973374576,6.73885125901313,130.88552490346));
#130358=CARTESIAN_POINT('Ctrl Pts',(77.6148893401839,8.52553889053475,130.774391785469));
#130359=CARTESIAN_POINT('Ctrl Pts',(78.307752406047,10.7464720006261,130.663258667477));
#130360=CARTESIAN_POINT('Ctrl Pts',(80.5494271837866,11.3689652022709,130.552125549485));
#130361=CARTESIAN_POINT('Ctrl Pts',(82.288244357474,9.82328819493091,130.440992431494));
#130362=CARTESIAN_POINT('Ctrl Pts',(81.9327706811323,7.52410545653742,130.329859313502));
#130363=CARTESIAN_POINT('Ctrl Pts',(79.8083482832819,6.57571943513415,130.218726195511));
#130364=CARTESIAN_POINT('Ctrl Pts',(77.8593349635166,7.84613052780885,130.107593077519));
#130365=CARTESIAN_POINT('Ctrl Pts',(77.8695386886888,10.1726081270525,129.996459959528));
#130366=CARTESIAN_POINT('Ctrl Pts',(79.8296323383495,11.4258691267836,129.885326841536));
#130367=CARTESIAN_POINT('Ctrl Pts',(81.9456370655975,10.4588781737672,129.774193723544));
#130368=CARTESIAN_POINT('Ctrl Pts',(82.280951121822,8.15666663573472,129.663060605553));
#130369=CARTESIAN_POINT('Ctrl Pts',(80.5285815452698,6.62630260836619,129.551927487561));
#130370=CARTESIAN_POINT('Ctrl Pts',(78.2925711520252,7.2684488144164,129.44079436957));
#130371=CARTESIAN_POINT('Ctrl Pts',(77.6189849879312,9.49536050885278,129.329661251578));
#130372=CARTESIAN_POINT('Ctrl Pts',(79.1251739340349,11.2689362351057,129.218528133587));
#130373=CARTESIAN_POINT('Ctrl Pts',(81.4308590042111,10.9658155584414,129.107395015595));
#130374=CARTESIAN_POINT('Ctrl Pts',(82.429384248427,8.86366644097112,128.996261897604));
#130375=CARTESIAN_POINT('Ctrl Pts',(81.1993093722144,6.88573951185316,128.885115641378));
#130376=CARTESIAN_POINT('Ctrl Pts',(79.6553399314687,6.85926310844778,128.811013757815));
#130377=CARTESIAN_POINT('Ctrl Pts',(79.0485528000777,7.17575966835091,128.773956246917));
#130378=CARTESIAN_POINT('Ctrl Pts',(79.5030640075578,7.13926821666982,140.074365000815));
#130379=CARTESIAN_POINT('Ctrl Pts',(78.8843529912895,7.30450416075302,140.037320628152));
#130380=CARTESIAN_POINT('Ctrl Pts',(77.835543372364,8.29867835070604,139.963231882824));
#130381=CARTESIAN_POINT('Ctrl Pts',(78.2365577863739,10.4415683587053,139.852098764832));
#130382=CARTESIAN_POINT('Ctrl Pts',(80.2547832741512,11.2617038450006,139.740965646841));
#130383=CARTESIAN_POINT('Ctrl Pts',(82.0382544766191,10.0134806280791,139.629832528849));
#130384=CARTESIAN_POINT('Ctrl Pts',(81.9570005747449,7.83688176296831,139.518699410858));
#130385=CARTESIAN_POINT('Ctrl Pts',(80.0842484158553,6.7252047519253,139.407566292866));
#130386=CARTESIAN_POINT('Ctrl Pts',(78.1345718117616,7.69531907512722,139.296433174875));
#130387=CARTESIAN_POINT('Ctrl Pts',(77.8921190168525,9.85962203305674,139.185300056883));
#130388=CARTESIAN_POINT('Ctrl Pts',(79.5789256214626,11.2371194509922,139.074166938891));
#130389=CARTESIAN_POINT('Ctrl Pts',(81.6510946741933,10.5671394024057,138.9630338209));
#130390=CARTESIAN_POINT('Ctrl Pts',(82.212127356829,8.46284078322597,138.851900702908));
#130391=CARTESIAN_POINT('Ctrl Pts',(80.7485288983373,6.85017675504178,138.740767584917));
#130392=CARTESIAN_POINT('Ctrl Pts',(78.5998498316785,7.20511296898747,138.629634466925));
#130393=CARTESIAN_POINT('Ctrl Pts',(77.7326420853354,9.20280171494848,138.518501348934));
#130394=CARTESIAN_POINT('Ctrl Pts',(78.9406101428909,11.0148777256745,138.407368230942));
#130395=CARTESIAN_POINT('Ctrl Pts',(81.118173202419,10.9828586419285,138.296235112951));
#130396=CARTESIAN_POINT('Ctrl Pts',(82.2723402792148,9.13604913545734,138.185101994959));
#130397=CARTESIAN_POINT('Ctrl Pts',(81.3467720241138,7.16472217826751,138.073968876967));
#130398=CARTESIAN_POINT('Ctrl Pts',(79.188585038301,6.87311368371572,137.962835758976));
#130399=CARTESIAN_POINT('Ctrl Pts',(77.7730369457001,8.52811527668511,137.851702640984));
#130400=CARTESIAN_POINT('Ctrl Pts',(78.3956931009801,10.6150043331122,137.740569522993));
#130401=CARTESIAN_POINT('Ctrl Pts',(80.4866740711505,11.2237778620907,137.629436405001));
#130402=CARTESIAN_POINT('Ctrl Pts',(82.1322317780535,9.79726236260266,137.51830328701));
#130403=CARTESIAN_POINT('Ctrl Pts',(81.8262870369014,7.64106096991607,137.407170169018));
#130404=CARTESIAN_POINT('Ctrl Pts',(79.848852518087,6.72861406439414,137.296037051027));
#130405=CARTESIAN_POINT('Ctrl Pts',(78.0097541235979,7.89502896825616,137.184903933035));
#130406=CARTESIAN_POINT('Ctrl Pts',(77.9922070906181,10.0727568514897,137.073770815043));
#130407=CARTESIAN_POINT('Ctrl Pts',(79.8122711542087,11.2686554409985,136.962637697052));
#130408=CARTESIAN_POINT('Ctrl Pts',(81.8041520464296,10.3881912774696,136.85150457906));
#130409=CARTESIAN_POINT('Ctrl Pts',(82.1448019750125,8.23719981813793,136.740371461069));
#130410=CARTESIAN_POINT('Ctrl Pts',(80.5224447174872,6.78435310876227,136.629238343077));
#130411=CARTESIAN_POINT('Ctrl Pts',(78.4219254912908,7.35935364126247,136.518105225086));
#130412=CARTESIAN_POINT('Ctrl Pts',(77.7657221678739,9.43593829648909,136.406972107094));
#130413=CARTESIAN_POINT('Ctrl Pts',(79.1544178567368,11.1135350644055,136.295838989103));
#130414=CARTESIAN_POINT('Ctrl Pts',(81.3170236049032,10.8567413534482,136.184705871111));
#130415=CARTESIAN_POINT('Ctrl Pts',(82.2742375123182,8.90058487518767,136.073572753119));
#130416=CARTESIAN_POINT('Ctrl Pts',(81.1499797353433,7.03541703209655,135.962439635128));
#130417=CARTESIAN_POINT('Ctrl Pts',(78.9732152418211,6.9683128464628,135.851306517136));
#130418=CARTESIAN_POINT('Ctrl Pts',(77.7362045728382,8.76068871017342,135.740173399145));
#130419=CARTESIAN_POINT('Ctrl Pts',(78.5711085809138,10.7720916855339,135.629040281153));
#130420=CARTESIAN_POINT('Ctrl Pts',(80.7137902563551,11.1616066014447,135.517907163162));
#130421=CARTESIAN_POINT('Ctrl Pts',(82.2031829946697,9.57273407570653,135.40677404517));
#130422=CARTESIAN_POINT('Ctrl Pts',(81.6761359398247,7.45967278128821,135.295640927178));
#130423=CARTESIAN_POINT('Ctrl Pts',(79.6150233007846,6.75637958412346,135.184507809187));
#130424=CARTESIAN_POINT('Ctrl Pts',(77.9062564894017,8.10653609960796,135.073374691195));
#130425=CARTESIAN_POINT('Ctrl Pts',(78.1137661478597,10.2744259431277,134.962241573204));
#130426=CARTESIAN_POINT('Ctrl Pts',(80.0476312692378,11.2759110025806,134.851108455212));
#130427=CARTESIAN_POINT('Ctrl Pts',(81.9379023782607,10.1943927334876,134.739975337221));
#130428=CARTESIAN_POINT('Ctrl Pts',(82.0545289556053,8.01971922386687,134.628842219229));
#130429=CARTESIAN_POINT('Ctrl Pts',(80.2907697673081,6.7422372640385,134.517709101238));
#130430=CARTESIAN_POINT('Ctrl Pts',(78.2608866433841,7.53114862483747,134.406575983246));
#130431=CARTESIAN_POINT('Ctrl Pts',(77.8227085142696,9.66441057761191,134.295442865254));
#130432=CARTESIAN_POINT('Ctrl Pts',(79.3772732502533,11.1895778188105,134.184309747263));
#130433=CARTESIAN_POINT('Ctrl Pts',(81.5017820178913,10.7107572592905,134.073176629271));
#130434=CARTESIAN_POINT('Ctrl Pts',(82.2518007731909,8.66618432131833,133.96204351128));
#130435=CARTESIAN_POINT('Ctrl Pts',(80.9408828308515,6.92713263133267,133.850910393288));
#130436=CARTESIAN_POINT('Ctrl Pts',(78.7688318889294,7.08525074441597,133.739777275297));
#130437=CARTESIAN_POINT('Ctrl Pts',(77.7235944605638,8.99582274000608,133.628644157305));
#130438=CARTESIAN_POINT('Ctrl Pts',(78.7618129803392,10.910217928358,133.517511039313));
#130439=CARTESIAN_POINT('Ctrl Pts',(80.9332689950743,11.0763064832317,133.406377921322));
#130440=CARTESIAN_POINT('Ctrl Pts',(82.2505604924078,9.34207762202491,133.29524480333));
#130441=CARTESIAN_POINT('Ctrl Pts',(81.5080504458918,7.29476585709696,133.184111685339));
#130442=CARTESIAN_POINT('Ctrl Pts',(79.3853132750087,6.80815149711572,133.072978567347));
#130443=CARTESIAN_POINT('Ctrl Pts',(77.8251615886712,8.32760315729057,132.961845449356));
#130444=CARTESIAN_POINT('Ctrl Pts',(78.2555076171877,10.462458873195,132.850712331364));
#130445=CARTESIAN_POINT('Ctrl Pts',(80.2824817370051,11.2588146665309,132.739579213373));
#130446=CARTESIAN_POINT('Ctrl Pts',(82.0509174527428,9.98781437097895,132.628446095381));
#130447=CARTESIAN_POINT('Ctrl Pts',(81.9422727924055,7.81272748311218,132.51731297739));
#130448=CARTESIAN_POINT('Ctrl Pts',(80.0559836253476,6.72427913329213,132.406179859398));
#130449=CARTESIAN_POINT('Ctrl Pts',(78.1184560408754,7.71866009218345,132.295046741406));
#130450=CARTESIAN_POINT('Ctrl Pts',(77.902991544647,9.88577376775608,132.183913623415));
#130451=CARTESIAN_POINT('Ctrl Pts',(79.6067917241972,11.242192427362,132.072780505423));
#130452=CARTESIAN_POINT('Ctrl Pts',(81.6704715943076,10.5464683256135,131.961647387432));
#130453=CARTESIAN_POINT('Ctrl Pts',(82.2052701121483,8.43535554386083,131.85051426944));
#130454=CARTESIAN_POINT('Ctrl Pts',(80.7217186248435,6.84102759256112,131.739381151449));
#130455=CARTESIAN_POINT('Ctrl Pts',(78.577621845353,7.22267616486489,131.628248033457));
#130456=CARTESIAN_POINT('Ctrl Pts',(77.7353415375832,9.2310014658902,131.517114915466));
#130457=CARTESIAN_POINT('Ctrl Pts',(78.9657657900324,11.0279051331599,131.405981797474));
#130458=CARTESIAN_POINT('Ctrl Pts',(81.1427618998832,10.968790205083,131.294848679482));
#130459=CARTESIAN_POINT('Ctrl Pts',(82.2738573374737,9.10776099030368,131.183715561491));
#130460=CARTESIAN_POINT('Ctrl Pts',(81.3238290474173,7.14810467614153,131.072582443499));
#130461=CARTESIAN_POINT('Ctrl Pts',(79.1621802959776,6.88337585149887,130.961449325508));
#130462=CARTESIAN_POINT('Ctrl Pts',(77.76733713802,8.55586475864455,130.850316207516));
#130463=CARTESIAN_POINT('Ctrl Pts',(78.4159148588162,10.63484371647,130.739183089525));
#130464=CARTESIAN_POINT('Ctrl Pts',(80.5143097505996,11.217549364708,130.628049971533));
#130465=CARTESIAN_POINT('Ctrl Pts',(82.1419879094673,9.7706665390823,130.516916853541));
#130466=CARTESIAN_POINT('Ctrl Pts',(81.8092348473344,7.6184393911342,130.40578373555));
#130467=CARTESIAN_POINT('Ctrl Pts',(79.8205979799762,6.73067083410996,130.294650617558));
#130468=CARTESIAN_POINT('Ctrl Pts',(77.9961586657518,7.91988176417262,130.183517499567));
#130469=CARTESIAN_POINT('Ctrl Pts',(78.00571020507,10.0976591824581,130.072384381575));
#130470=CARTESIAN_POINT('Ctrl Pts',(79.8405216338773,11.270816192575,129.961251263584));
#130471=CARTESIAN_POINT('Ctrl Pts',(81.8212788582255,10.3656318650533,129.850118145592));
#130472=CARTESIAN_POINT('Ctrl Pts',(82.1351608315215,8.21056950757627,129.738985027601));
#130473=CARTESIAN_POINT('Ctrl Pts',(80.4947964912215,6.77802091065733,129.627851909609));
#130474=CARTESIAN_POINT('Ctrl Pts',(78.4017039366046,7.37912341309647,129.516718791617));
#130475=CARTESIAN_POINT('Ctrl Pts',(77.7711710065171,9.46369882540057,129.405585673626));
#130476=CARTESIAN_POINT('Ctrl Pts',(79.1810897074592,11.1239138936689,129.294452555634));
#130477=CARTESIAN_POINT('Ctrl Pts',(81.3394035812484,10.8401676135116,129.183319437643));
#130478=CARTESIAN_POINT('Ctrl Pts',(82.2741066401341,8.87238039760016,129.072186319651));
#130479=CARTESIAN_POINT('Ctrl Pts',(81.1226537789126,7.02087552918776,128.961040063426));
#130480=CARTESIAN_POINT('Ctrl Pts',(79.6773693782926,6.99609140340361,128.886938179863));
#130481=CARTESIAN_POINT('Ctrl Pts',(79.1093659241097,7.2923586278747,128.849880668964));
#130482=CARTESIAN_POINT('Ctrl Pts',(79.5369951482613,7.26632029764578,140.150289422863));
#130483=CARTESIAN_POINT('Ctrl Pts',(78.9605301573707,7.42027381470975,140.113245050199));
#130484=CARTESIAN_POINT('Ctrl Pts',(77.9833340003239,8.34656508848017,140.039156304871));
#130485=CARTESIAN_POINT('Ctrl Pts',(78.3569668667848,10.3431370525474,139.92802318688));
#130486=CARTESIAN_POINT('Ctrl Pts',(80.2373864921598,11.1072731083233,139.816890068888));
#130487=CARTESIAN_POINT('Ctrl Pts',(81.8990810207062,9.94427945465913,139.705756950897));
#130488=CARTESIAN_POINT('Ctrl Pts',(81.8233751926667,7.91630029806288,139.594623832905));
#130489=CARTESIAN_POINT('Ctrl Pts',(80.07849587449,6.88052937885506,139.483490714914));
#130490=CARTESIAN_POINT('Ctrl Pts',(78.2619445665833,7.78440361057707,139.372357596922));
#130491=CARTESIAN_POINT('Ctrl Pts',(78.0360466198298,9.80092643322281,139.26122447893));
#130492=CARTESIAN_POINT('Ctrl Pts',(79.6076768775642,11.0843673541092,139.150091360939));
#130493=CARTESIAN_POINT('Ctrl Pts',(81.5383567631607,10.4601340166544,139.038958242947));
#130494=CARTESIAN_POINT('Ctrl Pts',(82.0610817377952,8.49951839410893,138.927825124956));
#130495=CARTESIAN_POINT('Ctrl Pts',(80.6974188162415,6.99696820529239,138.816692006964));
#130496=CARTESIAN_POINT('Ctrl Pts',(78.6954530745305,7.32766912374867,138.705558888973));
#130497=CARTESIAN_POINT('Ctrl Pts',(77.8874588858846,9.18895427055025,138.594425770981));
#130498=CARTESIAN_POINT('Ctrl Pts',(79.012946030909,10.8773004508344,138.48329265299));
#130499=CARTESIAN_POINT('Ctrl Pts',(81.0418235460464,10.8474676527515,138.372159534998));
#130500=CARTESIAN_POINT('Ctrl Pts',(82.1171832792935,9.12675960435475,138.261026417006));
#130501=CARTESIAN_POINT('Ctrl Pts',(81.254813478666,7.29003624475958,138.149893299015));
#130502=CARTESIAN_POINT('Ctrl Pts',(79.243989025239,7.01833898426903,138.038760181023));
#130503=CARTESIAN_POINT('Ctrl Pts',(77.9250955566404,8.56033589903112,137.927627063032));
#130504=CARTESIAN_POINT('Ctrl Pts',(78.5052363096632,10.5047306960704,137.81649394504));
#130505=CARTESIAN_POINT('Ctrl Pts',(80.4534436216841,11.0719367383254,137.705360827049));
#130506=CARTESIAN_POINT('Ctrl Pts',(81.9866414855934,9.74282472513125,137.594227709057));
#130507=CARTESIAN_POINT('Ctrl Pts',(81.7015868675506,7.73385028712899,137.483094591066));
#130508=CARTESIAN_POINT('Ctrl Pts',(79.8591729749542,6.88370590105949,137.371961473074));
#130509=CARTESIAN_POINT('Ctrl Pts',(78.1456495183648,7.97047717108632,137.260828355082));
#130510=CARTESIAN_POINT('Ctrl Pts',(78.1293006091955,9.99950825565009,137.149695237091));
#130511=CARTESIAN_POINT('Ctrl Pts',(79.8250894124504,11.1137500444344,137.038562119099));
#130512=CARTESIAN_POINT('Ctrl Pts',(81.680963269869,10.2934045961353,136.927429001108));
#130513=CARTESIAN_POINT('Ctrl Pts',(81.9983533806219,8.28928435355709,136.816295883116));
#130514=CARTESIAN_POINT('Ctrl Pts',(80.486771823013,6.93563904409244,136.705162765125));
#130515=CARTESIAN_POINT('Ctrl Pts',(78.5296775338274,7.47137813393286,136.594029647133));
#130516=CARTESIAN_POINT('Ctrl Pts',(77.9182802370128,9.40617212156682,136.482896529142));
#130517=CARTESIAN_POINT('Ctrl Pts',(79.2121548029749,10.9692213967646,136.37176341115));
#130518=CARTESIAN_POINT('Ctrl Pts',(81.2270963025394,10.7299617418442,136.260630293158));
#130519=CARTESIAN_POINT('Ctrl Pts',(82.11895096798,8.9073730101575,136.149497175167));
#130520=CARTESIAN_POINT('Ctrl Pts',(81.0714583064278,7.16956014533737,136.038364057175));
#130521=CARTESIAN_POINT('Ctrl Pts',(79.0433248306451,7.10703788091514,135.927230939184));
#130522=CARTESIAN_POINT('Ctrl Pts',(77.8907781242235,8.77702905414233,135.816097821192));
#130523=CARTESIAN_POINT('Ctrl Pts',(78.6686742966767,10.6510920130694,135.704964703201));
#130524=CARTESIAN_POINT('Ctrl Pts',(80.6650521532805,11.0140105752869,135.593831585209));
#130525=CARTESIAN_POINT('Ctrl Pts',(82.0527481030041,9.53362738831814,135.482698467217));
#130526=CARTESIAN_POINT('Ctrl Pts',(81.5616881934805,7.56484741219121,135.371565349226));
#130527=CARTESIAN_POINT('Ctrl Pts',(79.6413097818351,6.90957557148231,135.260432231234));
#130528=CARTESIAN_POINT('Ctrl Pts',(78.0492187757636,8.16754244605654,135.149299113243));
#130529=CARTESIAN_POINT('Ctrl Pts',(78.2425595281141,10.1874072392099,135.038165995251));
#130530=CARTESIAN_POINT('Ctrl Pts',(80.0443789725174,11.1205101911448,134.92703287726));
#130531=CARTESIAN_POINT('Ctrl Pts',(81.8055810345334,10.1128387536762,134.815899759268));
#130532=CARTESIAN_POINT('Ctrl Pts',(81.9142442667676,8.08665348793663,134.704766641277));
#130533=CARTESIAN_POINT('Ctrl Pts',(80.2709158021357,6.89639889900585,134.593633523285));
#130534=CARTESIAN_POINT('Ctrl Pts',(78.3796345322474,7.63144283463743,134.482500405293));
#130535=CARTESIAN_POINT('Ctrl Pts',(77.9713755154094,9.61904415389396,134.371367287302));
#130536=CARTESIAN_POINT('Ctrl Pts',(79.4197934727505,11.0400718981662,134.26023416931));
#130537=CARTESIAN_POINT('Ctrl Pts',(81.3992392805367,10.5939455447894,134.149101051319));
#130538=CARTESIAN_POINT('Ctrl Pts',(82.0980462252544,8.68897749173593,134.037967933327));
#130539=CARTESIAN_POINT('Ctrl Pts',(80.8766386863244,7.06866947997241,133.926834815336));
#130540=CARTESIAN_POINT('Ctrl Pts',(78.852896917508,7.21599117656667,133.815701697344));
#130541=CARTESIAN_POINT('Ctrl Pts',(77.8790290393256,8.99610796627015,133.704568579353));
#130542=CARTESIAN_POINT('Ctrl Pts',(78.8463572649559,10.7797868984321,133.593435461361));
#130543=CARTESIAN_POINT('Ctrl Pts',(80.8695447286342,10.9345348094194,133.482302343369));
#130544=CARTESIAN_POINT('Ctrl Pts',(82.0968906317194,9.31872032027786,133.371169225378));
#130545=CARTESIAN_POINT('Ctrl Pts',(81.4050796958441,7.41120044930849,133.260036107386));
#130546=CARTESIAN_POINT('Ctrl Pts',(79.4272845189342,6.95781246167295,133.148902989395));
#130547=CARTESIAN_POINT('Ctrl Pts',(77.9736610921575,8.37351488883257,133.037769871403));
#130548=CARTESIAN_POINT('Ctrl Pts',(78.3746227897605,10.3626011479463,132.926636753412));
#130549=CARTESIAN_POINT('Ctrl Pts',(80.2631936843982,11.104581205001,132.81550363542));
#130550=CARTESIAN_POINT('Ctrl Pts',(81.9108793598724,9.92036570772979,132.704370517429));
#130551=CARTESIAN_POINT('Ctrl Pts',(81.8096530337122,7.89379528950295,132.593237399437));
#130552=CARTESIAN_POINT('Ctrl Pts',(80.0521610238504,6.87966696211622,132.482104281445));
#130553=CARTESIAN_POINT('Ctrl Pts',(78.2469291919207,7.80615088649572,132.370971163454));
#130554=CARTESIAN_POINT('Ctrl Pts',(78.0461767637439,9.8252925089978,132.259838045462));
#130555=CARTESIAN_POINT('Ctrl Pts',(79.6336402631136,11.089093944068,132.148704927471));
#130556=CARTESIAN_POINT('Ctrl Pts',(81.5564106134778,10.4408743755918,132.037571809479));
#130557=CARTESIAN_POINT('Ctrl Pts',(82.0546927106265,8.47390986630898,131.926438691488));
#130558=CARTESIAN_POINT('Ctrl Pts',(80.6724391671662,6.98844375409079,131.815305573496));
#130559=CARTESIAN_POINT('Ctrl Pts',(78.6747428308176,7.34403309220127,131.704172455504));
#130560=CARTESIAN_POINT('Ctrl Pts',(77.8899740176255,9.21522852257146,131.593039337513));
#130561=CARTESIAN_POINT('Ctrl Pts',(79.0363840326883,10.8894383377314,131.481906219521));
#130562=CARTESIAN_POINT('Ctrl Pts',(81.0647333098732,10.8343598187147,131.37077310153));
#130563=CARTESIAN_POINT('Ctrl Pts',(82.1185967517424,9.10040299374085,131.259639983538));
#130564=CARTESIAN_POINT('Ctrl Pts',(81.2334370646298,7.27455339742084,131.148506865547));
#130565=CARTESIAN_POINT('Ctrl Pts',(79.2193872173793,7.0279004439846,131.037373747555));
#130566=CARTESIAN_POINT('Ctrl Pts',(77.9197849358561,8.58619062675434,130.926240629564));
#130567=CARTESIAN_POINT('Ctrl Pts',(78.5240773115852,10.5232154323138,130.815107511572));
#130568=CARTESIAN_POINT('Ctrl Pts',(80.4791923174128,11.0661335271449,130.70397439358));
#130569=CARTESIAN_POINT('Ctrl Pts',(81.9957314614605,9.71804488323371,130.592841275589));
#130570=CARTESIAN_POINT('Ctrl Pts',(81.6856990135364,7.71277332573098,130.481708157597));
#130571=CARTESIAN_POINT('Ctrl Pts',(79.8328476766705,6.88562223308578,130.370575039606));
#130572=CARTESIAN_POINT('Ctrl Pts',(78.132982367987,7.99363300053637,130.259441921614));
#130573=CARTESIAN_POINT('Ctrl Pts',(78.1418817214514,10.0227102378639,130.148308803623));
#130574=CARTESIAN_POINT('Ctrl Pts',(79.8514109294049,11.1157632583664,130.037175685631));
#130575=CARTESIAN_POINT('Ctrl Pts',(81.6969206508535,10.2723855563395,129.926042567639));
#130576=CARTESIAN_POINT('Ctrl Pts',(81.9893705412209,8.26447237941779,129.814909449648));
#130577=CARTESIAN_POINT('Ctrl Pts',(80.4610114371731,6.9297392129485,129.703776331656));
#130578=CARTESIAN_POINT('Ctrl Pts',(78.5108367211839,7.48979801177652,129.592643213665));
#130579=CARTESIAN_POINT('Ctrl Pts',(77.9233570251033,9.43203714194838,129.481510095673));
#130580=CARTESIAN_POINT('Ctrl Pts',(79.2370054808835,10.9788915522322,129.370376977682));
#130581=CARTESIAN_POINT('Ctrl Pts',(81.247948158286,10.7145196685817,129.25924385969));
#130582=CARTESIAN_POINT('Ctrl Pts',(82.1188290318412,8.88109435422919,129.148110741698));
#130583=CARTESIAN_POINT('Ctrl Pts',(81.045998185611,7.15601154652237,129.036964485473));
#130584=CARTESIAN_POINT('Ctrl Pts',(79.6993988251165,7.13291969835944,128.96286260191));
#130585=CARTESIAN_POINT('Ctrl Pts',(79.1701790481417,7.4089575873985,128.925805091013));
#130586=CARTESIAN_POINT('Ctrl Pts',(79.5709262889649,7.39337237862174,140.22621384491));
#130587=CARTESIAN_POINT('Ctrl Pts',(79.0367073234519,7.53604346866648,140.189169472247));
#130588=CARTESIAN_POINT('Ctrl Pts',(78.1311246282838,8.39445182625427,140.115080726919));
#130589=CARTESIAN_POINT('Ctrl Pts',(78.4773759471957,10.2447057463896,140.003947608927));
#130590=CARTESIAN_POINT('Ctrl Pts',(80.2199897101685,10.9528423716459,139.892814490936));
#130591=CARTESIAN_POINT('Ctrl Pts',(81.7599075647934,9.87507828123918,139.781681372944));
#130592=CARTESIAN_POINT('Ctrl Pts',(81.6897498105885,7.99571883315742,139.670548254953));
#130593=CARTESIAN_POINT('Ctrl Pts',(80.0727433331246,7.03585400578483,139.559415136961));
#130594=CARTESIAN_POINT('Ctrl Pts',(78.3893173214049,7.87348814602691,139.44828201897));
#130595=CARTESIAN_POINT('Ctrl Pts',(78.1799742228073,9.74223083338886,139.337148900978));
#130596=CARTESIAN_POINT('Ctrl Pts',(79.6364281336657,10.9316152572264,139.226015782987));
#130597=CARTESIAN_POINT('Ctrl Pts',(81.4256188521281,10.353128630903,139.114882664995));
#130598=CARTESIAN_POINT('Ctrl Pts',(81.9100361187613,8.53619600499189,139.003749547003));
#130599=CARTESIAN_POINT('Ctrl Pts',(80.6463087341457,7.143759655543,138.892616429012));
#130600=CARTESIAN_POINT('Ctrl Pts',(78.7910563173825,7.45022527850987,138.78148331102));
#130601=CARTESIAN_POINT('Ctrl Pts',(78.0422756864338,9.17510682615201,138.670350193029));
#130602=CARTESIAN_POINT('Ctrl Pts',(79.085281918927,10.7397231759942,138.559217075037));
#130603=CARTESIAN_POINT('Ctrl Pts',(80.9654738896738,10.7120766635745,138.448083957046));
#130604=CARTESIAN_POINT('Ctrl Pts',(81.9620262793723,9.11747007325214,138.336950839054));
#130605=CARTESIAN_POINT('Ctrl Pts',(81.1628549332179,7.41535031125165,138.225817721063));
#130606=CARTESIAN_POINT('Ctrl Pts',(79.2993930121772,7.16356428482233,138.114684603071));
#130607=CARTESIAN_POINT('Ctrl Pts',(78.0771541675805,8.59255652137716,138.003551485079));
#130608=CARTESIAN_POINT('Ctrl Pts',(78.6147795183462,10.3944570590286,137.892418367088));
#130609=CARTESIAN_POINT('Ctrl Pts',(80.4202131722175,10.92009561456,137.781285249096));
#130610=CARTESIAN_POINT('Ctrl Pts',(81.8410511931334,9.68838708765981,137.670152131105));
#130611=CARTESIAN_POINT('Ctrl Pts',(81.5768866981997,7.82663960434193,137.559019013113));
#130612=CARTESIAN_POINT('Ctrl Pts',(79.8694934318215,7.03879773772482,137.447885895122));
#130613=CARTESIAN_POINT('Ctrl Pts',(78.2815449131314,8.04592537391647,137.33675277713));
#130614=CARTESIAN_POINT('Ctrl Pts',(78.2663941277731,9.92625965981055,137.225619659138));
#130615=CARTESIAN_POINT('Ctrl Pts',(79.837907670692,10.9588446478703,137.114486541147));
#130616=CARTESIAN_POINT('Ctrl Pts',(81.5577744933084,10.198617914801,137.003353423155));
#130617=CARTESIAN_POINT('Ctrl Pts',(81.8519047862312,8.34136888897625,136.892220305164));
#130618=CARTESIAN_POINT('Ctrl Pts',(80.4510989285387,7.0869249794226,136.781087187172));
#130619=CARTESIAN_POINT('Ctrl Pts',(78.6374295763639,7.58340262660325,136.66995406918));
#130620=CARTESIAN_POINT('Ctrl Pts',(78.0708383061516,9.37640594664453,136.558820951189));
#130621=CARTESIAN_POINT('Ctrl Pts',(79.269891749213,10.8249077291237,136.447687833197));
#130622=CARTESIAN_POINT('Ctrl Pts',(81.1371690001757,10.6031821302402,136.336554715206));
#130623=CARTESIAN_POINT('Ctrl Pts',(81.9636644236418,8.91416114512732,136.225421597214));
#130624=CARTESIAN_POINT('Ctrl Pts',(80.9929368775125,7.30370325857819,136.114288479223));
#130625=CARTESIAN_POINT('Ctrl Pts',(79.113434419469,7.24576291536748,136.003155361231));
#130626=CARTESIAN_POINT('Ctrl Pts',(78.0453516756087,8.79336939811123,135.89202224324));
#130627=CARTESIAN_POINT('Ctrl Pts',(78.7662400124398,10.5300923406048,135.780889125248));
#130628=CARTESIAN_POINT('Ctrl Pts',(80.6163140502057,10.8664145491293,135.669756007257));
#130629=CARTESIAN_POINT('Ctrl Pts',(81.9023132113388,9.49452070092974,135.558622889265));
#130630=CARTESIAN_POINT('Ctrl Pts',(81.4472404471363,7.67002204309423,135.447489771273));
#130631=CARTESIAN_POINT('Ctrl Pts',(79.6675962628857,7.06277155884116,135.336356653282));
#130632=CARTESIAN_POINT('Ctrl Pts',(78.1921810621257,8.2285487925051,135.22522353529));
#130633=CARTESIAN_POINT('Ctrl Pts',(78.3713529083684,10.100388535292,135.114090417299));
#130634=CARTESIAN_POINT('Ctrl Pts',(80.0411266757971,10.965109379709,135.002957299307));
#130635=CARTESIAN_POINT('Ctrl Pts',(81.6732596908063,10.0312847738648,134.891824181316));
#130636=CARTESIAN_POINT('Ctrl Pts',(81.7739595779298,8.15358775200641,134.780691063324));
#130637=CARTESIAN_POINT('Ctrl Pts',(80.2510618369633,7.05056053397319,134.669557945332));
#130638=CARTESIAN_POINT('Ctrl Pts',(78.4983824211106,7.73173704443741,134.558424827341));
#130639=CARTESIAN_POINT('Ctrl Pts',(78.1200425165492,9.573677730176,134.447291709349));
#130640=CARTESIAN_POINT('Ctrl Pts',(79.4623136952477,10.890565977522,134.336158591358));
#130641=CARTESIAN_POINT('Ctrl Pts',(81.2966965431822,10.4771338302882,134.225025473366));
#130642=CARTESIAN_POINT('Ctrl Pts',(81.9442916773176,8.71177066215355,134.113892355375));
#130643=CARTESIAN_POINT('Ctrl Pts',(80.8123945417976,7.21020632861215,134.002759237383));
#130644=CARTESIAN_POINT('Ctrl Pts',(78.9369619460865,7.34673160871737,133.891626119392));
#130645=CARTESIAN_POINT('Ctrl Pts',(78.0344636180874,8.99639319253423,133.7804930014));
#130646=CARTESIAN_POINT('Ctrl Pts',(78.9309015495727,10.6493558685063,133.669359883408));
#130647=CARTESIAN_POINT('Ctrl Pts',(80.8058204621942,10.7927631356071,133.558226765417));
#130648=CARTESIAN_POINT('Ctrl Pts',(81.9432207710311,9.29536301853081,133.447093647425));
#130649=CARTESIAN_POINT('Ctrl Pts',(81.3021089457963,7.52763504152003,133.335960529434));
#130650=CARTESIAN_POINT('Ctrl Pts',(79.4692557628599,7.10747342623018,133.224827411442));
#130651=CARTESIAN_POINT('Ctrl Pts',(78.1221605956438,8.41942662037456,133.113694293451));
#130652=CARTESIAN_POINT('Ctrl Pts',(78.4937379623332,10.2627434226976,133.002561175459));
#130653=CARTESIAN_POINT('Ctrl Pts',(80.2439056317912,10.9503477434711,132.891428057468));
#130654=CARTESIAN_POINT('Ctrl Pts',(81.770841267002,9.85291704448063,132.780294939476));
#130655=CARTESIAN_POINT('Ctrl Pts',(81.6770332750191,7.97486309589373,132.669161821485));
#130656=CARTESIAN_POINT('Ctrl Pts',(80.048338422353,7.0350547909403,132.558028703493));
#130657=CARTESIAN_POINT('Ctrl Pts',(78.375402342966,7.89364168080799,132.446895585501));
#130658=CARTESIAN_POINT('Ctrl Pts',(78.1893619828409,9.76481125023954,132.33576246751));
#130659=CARTESIAN_POINT('Ctrl Pts',(79.66048880203,10.935995460774,132.224629349518));
#130660=CARTESIAN_POINT('Ctrl Pts',(81.4423496326477,10.3352804255702,132.113496231527));
#130661=CARTESIAN_POINT('Ctrl Pts',(81.904115309105,8.51246418875713,132.002363113535));
#130662=CARTESIAN_POINT('Ctrl Pts',(80.6231597094889,7.13585991562045,131.891229995544));
#130663=CARTESIAN_POINT('Ctrl Pts',(78.7718638162824,7.46539001953766,131.780096877552));
#130664=CARTESIAN_POINT('Ctrl Pts',(78.0446064976679,9.1994555792527,131.668963759561));
#130665=CARTESIAN_POINT('Ctrl Pts',(79.1070022753443,10.7509715423028,131.557830641569));
#130666=CARTESIAN_POINT('Ctrl Pts',(80.9867047198631,10.6999294323463,131.446697523577));
#130667=CARTESIAN_POINT('Ctrl Pts',(81.9633361660112,9.093044997178,131.335564405586));
#130668=CARTESIAN_POINT('Ctrl Pts',(81.1430450818425,7.40100211870016,131.224431287594));
#130669=CARTESIAN_POINT('Ctrl Pts',(79.2765941387811,7.17242503647032,131.113298169603));
#130670=CARTESIAN_POINT('Ctrl Pts',(78.0722327336921,8.61651649486414,131.002165051611));
#130671=CARTESIAN_POINT('Ctrl Pts',(78.6322397643545,10.4115871481576,130.89103193362));
#130672=CARTESIAN_POINT('Ctrl Pts',(80.4440748842258,10.9147176895819,130.779898815628));
#130673=CARTESIAN_POINT('Ctrl Pts',(81.8494750134538,9.66542322738512,130.668765697637));
#130674=CARTESIAN_POINT('Ctrl Pts',(81.5621631797384,7.80710726032776,130.557632579645));
#130675=CARTESIAN_POINT('Ctrl Pts',(79.8450973733649,7.04057363206159,130.446499461653));
#130676=CARTESIAN_POINT('Ctrl Pts',(78.269806070222,8.06738423690015,130.335366343662));
#130677=CARTESIAN_POINT('Ctrl Pts',(78.2780532378328,9.94776129326954,130.22423322567));
#130678=CARTESIAN_POINT('Ctrl Pts',(79.8623002249327,10.9607103241578,130.113100107679));
#130679=CARTESIAN_POINT('Ctrl Pts',(81.5725624434815,10.1791392476256,130.001966989687));
#130680=CARTESIAN_POINT('Ctrl Pts',(81.8435802509203,8.31837525125933,129.890833871696));
#130681=CARTESIAN_POINT('Ctrl Pts',(80.4272263831248,7.08145751523965,129.779700753704));
#130682=CARTESIAN_POINT('Ctrl Pts',(78.6199695057632,7.60047261045659,129.668567635712));
#130683=CARTESIAN_POINT('Ctrl Pts',(78.0755430436893,9.40037545849617,129.557434517721));
#130684=CARTESIAN_POINT('Ctrl Pts',(79.2929212543077,10.8338692107953,129.446301399729));
#130685=CARTESIAN_POINT('Ctrl Pts',(81.1564927353234,10.5888717236517,129.335168281738));
#130686=CARTESIAN_POINT('Ctrl Pts',(81.9635514235481,8.88980831085824,129.224035163746));
#130687=CARTESIAN_POINT('Ctrl Pts',(80.9693425923095,7.29114756385696,129.112888907521));
#130688=CARTESIAN_POINT('Ctrl Pts',(79.7214282719405,7.26974799331527,129.038787023958));
#130689=CARTESIAN_POINT('Ctrl Pts',(79.2309921721737,7.5255565469223,129.00172951306));
#130690=CARTESIAN_POINT('',(78.7297156500765,10.0802549060841,140.000878868843));
#130691=CARTESIAN_POINT('Ctrl Pts',(78.7308621553943,10.0792799133634,140.000878868843));
#130692=CARTESIAN_POINT('Ctrl Pts',(78.736370574171,10.0857573272824,140.000585912562));
#130693=CARTESIAN_POINT('Ctrl Pts',(78.7419285829586,10.092192569647,140.000292956281));
#130694=CARTESIAN_POINT('Ctrl Pts',(78.7475355302757,10.0985848861505,140.));
#130695=CARTESIAN_POINT('Ctrl Pts',(79.4698297828112,7.01482567432834,140.));
#130696=CARTESIAN_POINT('Ctrl Pts',(79.4008201088926,7.04037739808265,140.));
#130697=CARTESIAN_POINT('Ctrl Pts',(79.333531264625,7.06986024816562,140.));
#130698=CARTESIAN_POINT('Ctrl Pts',(79.2681550277024,7.10297535276265,140.));
#130699=CARTESIAN_POINT('Ctrl Pts',(79.2013067432528,7.13683609537928,140.));
#130700=CARTESIAN_POINT('Ctrl Pts',(79.1364574168441,7.17449523887906,140.));
#130701=CARTESIAN_POINT('Ctrl Pts',(79.0738433838076,7.21567796853842,140.));
#130702=CARTESIAN_POINT('Ctrl Pts',(79.0212317769186,7.25028186607351,140.));
#130703=CARTESIAN_POINT('Ctrl Pts',(78.9701986946478,7.28737455147851,140.));
#130704=CARTESIAN_POINT('Ctrl Pts',(78.9209066494717,7.32681062951119,140.));
#130705=CARTESIAN_POINT('Ctrl Pts',(78.8988725699372,7.34443898469096,140.));
#130706=CARTESIAN_POINT('Ctrl Pts',(78.8771866812342,7.36253576994061,140.));
#130707=CARTESIAN_POINT('Ctrl Pts',(78.8558650479428,7.38108871910383,140.));
#130708=CARTESIAN_POINT('Ctrl Pts',(78.8441549123335,7.39127825513441,140.));
#130709=CARTESIAN_POINT('Ctrl Pts',(78.8325546668865,7.40160539314329,140.));
#130710=CARTESIAN_POINT('Ctrl Pts',(78.8210671070671,7.41206814268509,140.));
#130711=CARTESIAN_POINT('Ctrl Pts',(78.8104708100333,7.42171913938738,140.));
#130712=CARTESIAN_POINT('Ctrl Pts',(78.7999689523207,7.43148704191031,140.));
#130713=CARTESIAN_POINT('Ctrl Pts',(78.7895796274579,7.44135481790265,140.));
#130714=CARTESIAN_POINT('Ctrl Pts',(78.7364949706948,7.4917746005629,140.));
#130715=CARTESIAN_POINT('Ctrl Pts',(78.6862504774249,7.54488334682044,140.));
#130716=CARTESIAN_POINT('Ctrl Pts',(78.6390647471674,7.60042107429915,140.));
#130717=CARTESIAN_POINT('Ctrl Pts',(78.592610468946,7.65509788082504,140.));
#130718=CARTESIAN_POINT('Ctrl Pts',(78.5491204205517,7.71212983833611,140.));
#130719=CARTESIAN_POINT('Ctrl Pts',(78.5088467574884,7.77129247852492,140.));
#130720=CARTESIAN_POINT('Ctrl Pts',(78.474800950115,7.82130630141469,140.));
#130721=CARTESIAN_POINT('Ctrl Pts',(78.4430542558921,7.87284343154723,140.));
#130722=CARTESIAN_POINT('Ctrl Pts',(78.4137873790238,7.92577492972471,140.));
#130723=CARTESIAN_POINT('Ctrl Pts',(78.4016823401401,7.94766786508959,140.));
#130724=CARTESIAN_POINT('Ctrl Pts',(78.3900018581821,7.96979937807893,140.));
#130725=CARTESIAN_POINT('Ctrl Pts',(78.3787601693597,7.992160428703,140.));
#130726=CARTESIAN_POINT('Ctrl Pts',(78.3735606798431,8.00250282922102,140.));
#130727=CARTESIAN_POINT('Ctrl Pts',(78.3684550708377,8.01289433315706,140.));
#130728=CARTESIAN_POINT('Ctrl Pts',(78.3634448160861,8.02333404404232,140.));
#130729=CARTESIAN_POINT('Ctrl Pts',(78.3582119146326,8.03423767688612,140.));
#130730=CARTESIAN_POINT('Ctrl Pts',(78.3530866368273,8.04518644941609,140.));
#130731=CARTESIAN_POINT('Ctrl Pts',(78.3480720486465,8.05617503558337,140.));
#130732=CARTESIAN_POINT('Ctrl Pts',(78.3195311610532,8.11871736035694,140.));
#130733=CARTESIAN_POINT('Ctrl Pts',(78.2945512775789,8.18259159922865,140.));
#130734=CARTESIAN_POINT('Ctrl Pts',(78.2733558100535,8.24759283259564,140.));
#130735=CARTESIAN_POINT('Ctrl Pts',(78.2541541352166,8.30647959909913,140.));
#130736=CARTESIAN_POINT('Ctrl Pts',(78.2380587088044,8.36629190489806,140.));
#130737=CARTESIAN_POINT('Ctrl Pts',(78.2252723327201,8.42688219532759,140.));
#130738=CARTESIAN_POINT('Ctrl Pts',(78.2101393236097,8.49859238209378,140.));
#130739=CARTESIAN_POINT('Ctrl Pts',(78.1996408096421,8.5713938352022,140.));
#130740=CARTESIAN_POINT('Ctrl Pts',(78.1937017441597,8.64486393524295,140.));
#130741=CARTESIAN_POINT('Ctrl Pts',(78.1923945903257,8.66103427773769,140.));
#130742=CARTESIAN_POINT('Ctrl Pts',(78.1913085266392,8.67723692864844,140.));
#130743=CARTESIAN_POINT('Ctrl Pts',(78.1904431222916,8.69346721770384,140.));
#130744=CARTESIAN_POINT('Ctrl Pts',(78.1895475165414,8.71026392117007,140.));
#130745=CARTESIAN_POINT('Ctrl Pts',(78.1888882301811,8.72709641868181,140.));
#130746=CARTESIAN_POINT('Ctrl Pts',(78.1884653473802,8.74392526443646,140.));
#130747=CARTESIAN_POINT('Ctrl Pts',(78.1867426630314,8.81248040340845,140.));
#130748=CARTESIAN_POINT('Ctrl Pts',(78.1889312907711,8.88106164831567,140.));
#130749=CARTESIAN_POINT('Ctrl Pts',(78.1949107281129,8.94933109926134,140.));
#130750=CARTESIAN_POINT('Ctrl Pts',(78.2008889807299,9.01758702376556,140.));
#130751=CARTESIAN_POINT('Ctrl Pts',(78.2106569943201,9.08553234841923,140.));
#130752=CARTESIAN_POINT('Ctrl Pts',(78.2241439421755,9.15281433200293,140.));
#130753=CARTESIAN_POINT('Ctrl Pts',(78.2339020360718,9.20149427948872,140.));
#130754=CARTESIAN_POINT('Ctrl Pts',(78.2456079790146,9.24982671336545,140.));
#130755=CARTESIAN_POINT('Ctrl Pts',(78.2592491471692,9.29766838566998,140.));
#130756=CARTESIAN_POINT('Ctrl Pts',(78.2670120870047,9.32489420823299,140.));
#130757=CARTESIAN_POINT('Ctrl Pts',(78.2754019651411,9.3519609244368,140.));
#130758=CARTESIAN_POINT('Ctrl Pts',(78.284417996475,9.37884052478954,140.));
#130759=CARTESIAN_POINT('Ctrl Pts',(78.2903710440095,9.39658841548341,140.));
#130760=CARTESIAN_POINT('Ctrl Pts',(78.2965990797181,9.41425955524979,140.));
#130761=CARTESIAN_POINT('Ctrl Pts',(78.3030899812727,9.4318142879203,140.));
#130762=CARTESIAN_POINT('Ctrl Pts',(78.3040429931651,9.43439172171164,140.));
#130763=CARTESIAN_POINT('Ctrl Pts',(78.3050017082472,9.43696676507744,140.));
#130764=CARTESIAN_POINT('Ctrl Pts',(78.3059661198725,9.43953939093159,140.));
#130765=CARTESIAN_POINT('Ctrl Pts',(78.329146503839,9.50137445547726,140.));
#130766=CARTESIAN_POINT('Ctrl Pts',(78.3556159827812,9.56181902474221,140.));
#130767=CARTESIAN_POINT('Ctrl Pts',(78.38532430616,9.62053681691923,140.));
#130768=CARTESIAN_POINT('Ctrl Pts',(78.4060956394296,9.66159086142438,140.));
#130769=CARTESIAN_POINT('Ctrl Pts',(78.4284511313581,9.70180023814684,140.));
#130770=CARTESIAN_POINT('Ctrl Pts',(78.4523839013391,9.74103877789827,140.));
#130771=CARTESIAN_POINT('Ctrl Pts',(78.4600963609368,9.75368360140783,140.));
#130772=CARTESIAN_POINT('Ctrl Pts',(78.4679737809338,9.76622922088728,140.));
#130773=CARTESIAN_POINT('Ctrl Pts',(78.4760125858817,9.77866574969129,140.));
#130774=CARTESIAN_POINT('Ctrl Pts',(78.5102589136736,9.8316469384092,140.));
#130775=CARTESIAN_POINT('Ctrl Pts',(78.5473615905134,9.88254471555941,140.));
#130776=CARTESIAN_POINT('Ctrl Pts',(78.5872864455964,9.93104413524139,140.));
#130777=CARTESIAN_POINT('Ctrl Pts',(78.6240638497462,9.97572013356295,140.));
#130778=CARTESIAN_POINT('Ctrl Pts',(78.6632365895196,10.018361106523,140.));
#130779=CARTESIAN_POINT('Ctrl Pts',(78.7047993791355,10.0586880242349,140.));
#130780=CARTESIAN_POINT('Ctrl Pts',(78.7126175960375,10.0662737660143,140.));
#130781=CARTESIAN_POINT('Ctrl Pts',(78.7205204353165,10.0737775242579,140.));
#130782=CARTESIAN_POINT('Ctrl Pts',(78.7285063046483,10.0811986317636,140.));
#130783=CARTESIAN_POINT('Origin',(80.,-9.,129.));
#130784=CARTESIAN_POINT('Ctrl Pts',(79.2300979593296,-10.4774325188555,
129.));
#130785=CARTESIAN_POINT('Ctrl Pts',(79.2818307626562,-10.5124994265382,
129.));
#130786=CARTESIAN_POINT('Ctrl Pts',(79.3355405524417,-10.5443105979769,
129.));
#130787=CARTESIAN_POINT('Ctrl Pts',(79.3908959420258,-10.5729304242413,
129.));
#130788=CARTESIAN_POINT('Ctrl Pts',(79.4259931310383,-10.5910763619622,
129.));
#130789=CARTESIAN_POINT('Ctrl Pts',(79.4617527421542,-10.607938734873,129.));
#130790=CARTESIAN_POINT('Ctrl Pts',(79.4980979071617,-10.6235267468153,
129.));
#130791=CARTESIAN_POINT('Ctrl Pts',(79.5226967495725,-10.63407689975,129.));
#130792=CARTESIAN_POINT('Ctrl Pts',(79.5475639365611,-10.6440431834583,
129.));
#130793=CARTESIAN_POINT('Ctrl Pts',(79.572676847719,-10.6534269071554,129.));
#130794=CARTESIAN_POINT('Ctrl Pts',(79.5862865628442,-10.6585123313631,
129.));
#130795=CARTESIAN_POINT('Ctrl Pts',(79.5999686671651,-10.6634265769751,
129.));
#130796=CARTESIAN_POINT('Ctrl Pts',(79.6137053445211,-10.6681651435862,
129.));
#130797=CARTESIAN_POINT('Ctrl Pts',(79.6760830398119,-10.6896827825697,
129.));
#130798=CARTESIAN_POINT('Ctrl Pts',(79.7396537355289,-10.7076082288804,
129.));
#130799=CARTESIAN_POINT('Ctrl Pts',(79.8040670116738,-10.7219885211612,
129.));
#130800=CARTESIAN_POINT('Ctrl Pts',(79.850512820343,-10.7323575684114,129.));
#130801=CARTESIAN_POINT('Ctrl Pts',(79.8973976102623,-10.7408825669339,
129.));
#130802=CARTESIAN_POINT('Ctrl Pts',(79.9445991273204,-10.7475671243797,
129.));
#130803=CARTESIAN_POINT('Ctrl Pts',(79.9573807540249,-10.7493772254798,
129.));
#130804=CARTESIAN_POINT('Ctrl Pts',(79.97018563782,-10.7510523045138,129.));
#130805=CARTESIAN_POINT('Ctrl Pts',(79.9830114160439,-10.7525922771026,
129.));
#130806=CARTESIAN_POINT('Ctrl Pts',(79.996531159052,-10.7542155730365,129.));
#130807=CARTESIAN_POINT('Ctrl Pts',(80.0100665770587,-10.7556877927573,
129.));
#130808=CARTESIAN_POINT('Ctrl Pts',(80.0236082784729,-10.7570087636515,
129.));
#130809=CARTESIAN_POINT('Ctrl Pts',(80.091484178783,-10.7636299470602,129.));
#130810=CARTESIAN_POINT('Ctrl Pts',(80.1595660163247,-10.7664609181679,
129.));
#130811=CARTESIAN_POINT('Ctrl Pts',(80.2274935340178,-10.7655506742358,
129.));
#130812=CARTESIAN_POINT('Ctrl Pts',(80.296076466387,-10.7646316476003,129.));
#130813=CARTESIAN_POINT('Ctrl Pts',(80.3645031228694,-10.7598991585355,
129.));
#130814=CARTESIAN_POINT('Ctrl Pts',(80.4324242364423,-10.7513551603384,
129.));
#130815=CARTESIAN_POINT('Ctrl Pts',(80.4996588750007,-10.7428975158681,
129.));
#130816=CARTESIAN_POINT('Ctrl Pts',(80.5663992262361,-10.730705158574,129.));
#130817=CARTESIAN_POINT('Ctrl Pts',(80.6323115272082,-10.7147296965981,
129.));
#130818=CARTESIAN_POINT('Ctrl Pts',(80.6410547490952,-10.7126105624344,
129.));
#130819=CARTESIAN_POINT('Ctrl Pts',(80.6497833941471,-10.7104247863846,
129.));
#130820=CARTESIAN_POINT('Ctrl Pts',(80.6584966740677,-10.7081721860126,
129.));
#130821=CARTESIAN_POINT('Ctrl Pts',(80.6723039786817,-10.7046026530936,
129.));
#130822=CARTESIAN_POINT('Ctrl Pts',(80.6860752224786,-10.7008644715111,
129.));
#130823=CARTESIAN_POINT('Ctrl Pts',(80.6997839249182,-10.6969638794083,
129.));
#130824=CARTESIAN_POINT('Ctrl Pts',(80.767583687095,-10.6776725410715,129.));
#130825=CARTESIAN_POINT('Ctrl Pts',(80.8339729993893,-10.654383400419,129.));
#130826=CARTESIAN_POINT('Ctrl Pts',(80.8985888467434,-10.6271156045297,
129.));
#130827=CARTESIAN_POINT('Ctrl Pts',(80.9057657592136,-10.6240869576517,
129.));
#130828=CARTESIAN_POINT('Ctrl Pts',(80.9129208010519,-10.6210091751721,
129.));
#130829=CARTESIAN_POINT('Ctrl Pts',(80.9200534790049,-10.617882243794,129.));
#130830=CARTESIAN_POINT('Ctrl Pts',(80.9841494242166,-10.5897828926648,
129.));
#130831=CARTESIAN_POINT('Ctrl Pts',(81.0464403977837,-10.5577196528645,
129.));
#130832=CARTESIAN_POINT('Ctrl Pts',(81.1067676723926,-10.5220379319953,
129.));
#130833=CARTESIAN_POINT('Ctrl Pts',(81.1670949470016,-10.4863562111261,
129.));
#130834=CARTESIAN_POINT('Ctrl Pts',(81.2254592414653,-10.4470553334301,
129.));
#130835=CARTESIAN_POINT('Ctrl Pts',(81.2816837958061,-10.4044260185767,
129.));
#130836=CARTESIAN_POINT('Ctrl Pts',(81.2922353885737,-10.3964258276358,
129.));
#130837=CARTESIAN_POINT('Ctrl Pts',(81.3027115516211,-10.3883082725581,
129.));
#130838=CARTESIAN_POINT('Ctrl Pts',(81.31311101339,-10.380075090645,129.));
#130839=CARTESIAN_POINT('Ctrl Pts',(81.3222607011055,-10.3728313462008,
129.));
#130840=CARTESIAN_POINT('Ctrl Pts',(81.3313439530095,-10.3655036675837,
129.));
#130841=CARTESIAN_POINT('Ctrl Pts',(81.3403582861554,-10.3580952079013,
129.));
#130842=CARTESIAN_POINT('Ctrl Pts',(81.3951033706617,-10.3131027780881,
129.));
#130843=CARTESIAN_POINT('Ctrl Pts',(81.4473298717614,-10.2651175909719,
129.));
#130844=CARTESIAN_POINT('Ctrl Pts',(81.496889274164,-10.2144864134273,129.));
#130845=CARTESIAN_POINT('Ctrl Pts',(81.5478632629694,-10.1624100575344,
129.));
#130846=CARTESIAN_POINT('Ctrl Pts',(81.5960165224352,-10.1075340205125,
129.));
#130847=CARTESIAN_POINT('Ctrl Pts',(81.641166947533,-10.0501836096891,129.));
#130848=CARTESIAN_POINT('Ctrl Pts',(81.6863173726308,-9.99283319886575,
129.));
#130849=CARTESIAN_POINT('Ctrl Pts',(81.7284657192251,-9.93300764353711,
129.));
#130850=CARTESIAN_POINT('Ctrl Pts',(81.7673980299202,-9.87099085777822,
129.));
#130851=CARTESIAN_POINT('Ctrl Pts',(81.7770294648137,-9.85564857206042,
129.));
#130852=CARTESIAN_POINT('Ctrl Pts',(81.7864638901199,-9.84017201327144,
129.));
#130853=CARTESIAN_POINT('Ctrl Pts',(81.7956976814099,-9.82456517452716,
129.));
#130854=CARTESIAN_POINT('Ctrl Pts',(81.8029369736993,-9.81232941309025,
129.));
#130855=CARTESIAN_POINT('Ctrl Pts',(81.8100536644344,-9.80001205719501,
129.));
#130856=CARTESIAN_POINT('Ctrl Pts',(81.8170355830307,-9.78763403843294,
129.));
#130857=CARTESIAN_POINT('Ctrl Pts',(81.8540216960544,-9.72206254907344,
129.));
#130858=CARTESIAN_POINT('Ctrl Pts',(81.8872983542923,-9.6546761717898,129.));
#130859=CARTESIAN_POINT('Ctrl Pts',(81.9166853947369,-9.58582022495588,
129.));
#130860=CARTESIAN_POINT('Ctrl Pts',(81.9459283936586,-9.51730177775739,
129.));
#130861=CARTESIAN_POINT('Ctrl Pts',(81.9713205227596,-9.4473272863831,129.));
#130862=CARTESIAN_POINT('Ctrl Pts',(81.9926493682963,-9.37620015748104,
129.));
#130863=CARTESIAN_POINT('Ctrl Pts',(82.0137867027778,-9.30571167690551,
129.));
#130864=CARTESIAN_POINT('Ctrl Pts',(82.0309340643105,-9.23409033014075,
129.));
#130865=CARTESIAN_POINT('Ctrl Pts',(82.0438401515687,-9.1616076442864,129.));
#130866=CARTESIAN_POINT('Ctrl Pts',(82.0465861480475,-9.14618568128984,
129.));
#130867=CARTESIAN_POINT('Ctrl Pts',(82.0491399591624,-9.13072466500652,
129.));
#130868=CARTESIAN_POINT('Ctrl Pts',(82.0514988556353,-9.11522712597233,
129.));
#130869=CARTESIAN_POINT('Ctrl Pts',(82.0534883930455,-9.10215621165814,
129.));
#130870=CARTESIAN_POINT('Ctrl Pts',(82.0553392745732,-9.08905931614965,
129.));
#130871=CARTESIAN_POINT('Ctrl Pts',(82.0570522990024,-9.07593808097501,
129.));
#130872=CARTESIAN_POINT('Ctrl Pts',(81.8174278887595,-8.04137941204075,
129.));
#130873=CARTESIAN_POINT('Ctrl Pts',(81.7762159990727,-7.97834070616292,
129.));
#130874=CARTESIAN_POINT('Ctrl Pts',(81.7313405623381,-7.91789939904031,
129.));
#130875=CARTESIAN_POINT('Ctrl Pts',(81.6831396723547,-7.86020929481065,
129.));
#130876=CARTESIAN_POINT('Ctrl Pts',(81.6370503049079,-7.80504640439929,
129.));
#130877=CARTESIAN_POINT('Ctrl Pts',(81.5879194000536,-7.75239886539245,
129.));
#130878=CARTESIAN_POINT('Ctrl Pts',(81.5360172279659,-7.70243779621757,
129.));
#130879=CARTESIAN_POINT('Ctrl Pts',(81.5243247771145,-7.69118263439461,
129.));
#130880=CARTESIAN_POINT('Ctrl Pts',(81.5124900232915,-7.68006251540966,
129.));
#130881=CARTESIAN_POINT('Ctrl Pts',(81.5005210264171,-7.66908431840279,
129.));
#130882=CARTESIAN_POINT('Ctrl Pts',(81.4455928567033,-7.61870313151859,
129.));
#130883=CARTESIAN_POINT('Ctrl Pts',(81.3879497724495,-7.57140685173894,
129.));
#130884=CARTESIAN_POINT('Ctrl Pts',(81.3279084097019,-7.52736776321866,
129.));
#130885=CARTESIAN_POINT('Ctrl Pts',(81.2857570428461,-7.49645061391918,
129.));
#130886=CARTESIAN_POINT('Ctrl Pts',(81.2424229811911,-7.46713969363308,
129.));
#130887=CARTESIAN_POINT('Ctrl Pts',(81.1980104568253,-7.43950901649432,
129.));
#130888=CARTESIAN_POINT('Ctrl Pts',(81.1811384663816,-7.42901232603832,
129.));
#130889=CARTESIAN_POINT('Ctrl Pts',(81.1641108054664,-7.41875825468291,
129.));
#130890=CARTESIAN_POINT('Ctrl Pts',(81.14693311349,-7.40875134687659,129.));
#130891=CARTESIAN_POINT('Ctrl Pts',(81.1305341636591,-7.39919809727218,
129.));
#130892=CARTESIAN_POINT('Ctrl Pts',(81.1139931479043,-7.38986736642136,
129.));
#130893=CARTESIAN_POINT('Ctrl Pts',(81.0973446108032,-7.38077903707112,
129.));
#130894=CARTESIAN_POINT('Ctrl Pts',(81.0336771270485,-7.34602336708333,
129.));
#130895=CARTESIAN_POINT('Ctrl Pts',(80.9683737258037,-7.31476829705795,
129.));
#130896=CARTESIAN_POINT('Ctrl Pts',(80.9017257585264,-7.28717480040604,
129.));
#130897=CARTESIAN_POINT('Ctrl Pts',(80.8366064434856,-7.2602141941796,129.));
#130898=CARTESIAN_POINT('Ctrl Pts',(80.770202614952,-7.2367489826126,129.));
#130899=CARTESIAN_POINT('Ctrl Pts',(80.7027774984244,-7.2169771323118,129.));
#130900=CARTESIAN_POINT('Ctrl Pts',(80.6364371264415,-7.19752337425697,
129.));
#130901=CARTESIAN_POINT('Ctrl Pts',(80.5691072900731,-7.18164493377435,
129.));
#130902=CARTESIAN_POINT('Ctrl Pts',(80.5010426942184,-7.16957948697683,
129.));
#130903=CARTESIAN_POINT('Ctrl Pts',(80.4789909407811,-7.16567049061024,
129.));
#130904=CARTESIAN_POINT('Ctrl Pts',(80.4568621429895,-7.1621621240849,129.));
#130905=CARTESIAN_POINT('Ctrl Pts',(80.434665257464,-7.15906364436086,129.));
#130906=CARTESIAN_POINT('Ctrl Pts',(80.4221751971582,-7.15732014757321,
129.));
#130907=CARTESIAN_POINT('Ctrl Pts',(80.4096622887256,-7.15570638712659,
129.));
#130908=CARTESIAN_POINT('Ctrl Pts',(80.3971458493996,-7.15422589319744,
129.));
#130909=CARTESIAN_POINT('Ctrl Pts',(80.3293083065445,-7.14620180042234,
129.));
#130910=CARTESIAN_POINT('Ctrl Pts',(80.2612487043902,-7.14207059151351,
129.));
#130911=CARTESIAN_POINT('Ctrl Pts',(80.1932132104911,-7.14201015864512,
129.));
#130912=CARTESIAN_POINT('Ctrl Pts',(80.1834193046227,-7.14200145915915,
129.));
#130913=CARTESIAN_POINT('Ctrl Pts',(80.1736259045768,-7.14207720414265,
129.));
#130914=CARTESIAN_POINT('Ctrl Pts',(80.1638337541376,-7.14223801413209,
129.));
#130915=CARTESIAN_POINT('Ctrl Pts',(80.0941260097053,-7.14338277816691,
129.));
#130916=CARTESIAN_POINT('Ctrl Pts',(80.0244801006768,-7.14883421760917,
129.));
#130917=CARTESIAN_POINT('Ctrl Pts',(79.9552255344744,-7.15841681494381,
129.));
#130918=CARTESIAN_POINT('Ctrl Pts',(79.8912779185903,-7.16726510159306,
129.));
#130919=CARTESIAN_POINT('Ctrl Pts',(79.8276634957026,-7.17963663965979,
129.));
#130920=CARTESIAN_POINT('Ctrl Pts',(79.7646618938049,-7.19542712913009,
129.));
#130921=CARTESIAN_POINT('Ctrl Pts',(79.7507945251221,-7.19890279534443,
129.));
#130922=CARTESIAN_POINT('Ctrl Pts',(79.73695694447,-7.20254421600149,129.));
#130923=CARTESIAN_POINT('Ctrl Pts',(79.7231523111297,-7.20635045626908,
129.));
#130924=CARTESIAN_POINT('Ctrl Pts',(79.7120937153582,-7.20939955373447,
129.));
#130925=CARTESIAN_POINT('Ctrl Pts',(79.7010568159009,-7.21255435763673,
129.));
#130926=CARTESIAN_POINT('Ctrl Pts',(79.6900562807526,-7.21581026506554,
129.));
#130927=CARTESIAN_POINT('Ctrl Pts',(79.6245241542564,-7.2352062794056,129.));
#130928=CARTESIAN_POINT('Ctrl Pts',(79.5601586446492,-7.25821930074134,
129.));
#130929=CARTESIAN_POINT('Ctrl Pts',(79.497261502229,-7.28466766521021,129.));
#130930=CARTESIAN_POINT('Ctrl Pts',(79.4350282189579,-7.31083687568166,
129.));
#130931=CARTESIAN_POINT('Ctrl Pts',(79.3742316278236,-7.34037002111481,
129.));
#130932=CARTESIAN_POINT('Ctrl Pts',(79.3151931372451,-7.37313178272857,
129.));
#130933=CARTESIAN_POINT('Ctrl Pts',(79.2566545492536,-7.40561613736218,
129.));
#130934=CARTESIAN_POINT('Ctrl Pts',(79.1998436436882,-7.44127530985043,
129.));
#130935=CARTESIAN_POINT('Ctrl Pts',(79.1451144630058,-7.48000743341435,
129.));
#130936=CARTESIAN_POINT('Ctrl Pts',(79.1336098695569,-7.48814929356024,
129.));
#130937=CARTESIAN_POINT('Ctrl Pts',(79.1221974311397,-7.49642702849065,
129.));
#130938=CARTESIAN_POINT('Ctrl Pts',(79.1108807167964,-7.50483982192541,
129.));
#130939=CARTESIAN_POINT('Ctrl Pts',(79.1002619712711,-7.51273374854853,
129.));
#130940=CARTESIAN_POINT('Ctrl Pts',(79.0897262977731,-7.52074768146701,
129.));
#130941=CARTESIAN_POINT('Ctrl Pts',(79.0792931722657,-7.52886772372503,
129.));
#130942=CARTESIAN_POINT('Ctrl Pts',(79.0276936912682,-7.56902730638227,
129.));
#130943=CARTESIAN_POINT('Ctrl Pts',(78.9785044128779,-7.61184880861672,
129.));
#130944=CARTESIAN_POINT('Ctrl Pts',(78.9320167948803,-7.65720006725642,
129.));
#130945=CARTESIAN_POINT('Ctrl Pts',(78.8870712692266,-7.70104692898903,
129.));
#130946=CARTESIAN_POINT('Ctrl Pts',(78.8446506824178,-7.74725918924175,
129.));
#130947=CARTESIAN_POINT('Ctrl Pts',(78.8050589359191,-7.7957420041302,129.));
#130948=CARTESIAN_POINT('Ctrl Pts',(78.7657015104581,-7.84393787680228,
129.));
#130949=CARTESIAN_POINT('Ctrl Pts',(78.7291389707237,-7.8943780226341,129.));
#130950=CARTESIAN_POINT('Ctrl Pts',(78.6957183447143,-7.94698530266433,
129.));
#130951=CARTESIAN_POINT('Ctrl Pts',(78.6902770143314,-7.95555048008235,
129.));
#130952=CARTESIAN_POINT('Ctrl Pts',(78.6849190860989,-7.9641731294301,129.));
#130953=CARTESIAN_POINT('Ctrl Pts',(78.6796461961968,-7.97285294397019,
129.));
#130954=CARTESIAN_POINT('Ctrl Pts',(78.6739912788964,-7.98216162181429,
129.));
#130955=CARTESIAN_POINT('Ctrl Pts',(78.6684341691904,-7.99153604930243,
129.));
#130956=CARTESIAN_POINT('Ctrl Pts',(78.6629752716474,-8.00097456550985,
129.));
#130957=CARTESIAN_POINT('Ctrl Pts',(81.2663555976867,-7.92217834879833,
139.998270398006));
#130958=CARTESIAN_POINT('Ctrl Pts',(81.6248827770132,-8.34339539386142,
139.961212886432));
#130959=CARTESIAN_POINT('Ctrl Pts',(81.8817058969813,-9.56478460164107,
139.887111002195));
#130960=CARTESIAN_POINT('Ctrl Pts',(80.5443605470635,-10.8898007373938,
139.775964745293));
#130961=CARTESIAN_POINT('Ctrl Pts',(78.7083083354406,-10.4810544455385,
139.664831627301));
#130962=CARTESIAN_POINT('Ctrl Pts',(78.0547700220628,-8.71872336189441,
139.55369850931));
#130963=CARTESIAN_POINT('Ctrl Pts',(79.1814308219956,-7.21288524523363,
139.442565391318));
#130964=CARTESIAN_POINT('Ctrl Pts',(81.0573526260259,-7.34314561460427,
139.331432273327));
#130965=CARTESIAN_POINT('Ctrl Pts',(81.9655073696431,-8.98959908412584,
139.220299155335));
#130966=CARTESIAN_POINT('Ctrl Pts',(81.0747701647197,-10.6456820091187,
139.109166037344));
#130967=CARTESIAN_POINT('Ctrl Pts',(79.2003523202965,-10.7955181419101,
138.998032919352));
#130968=CARTESIAN_POINT('Ctrl Pts',(78.0578077510972,-9.30205172592216,
138.886899801361));
#130969=CARTESIAN_POINT('Ctrl Pts',(78.6928318965889,-7.53212281053173,
138.775766683369));
#130970=CARTESIAN_POINT('Ctrl Pts',(80.524228754692,-7.10565916705379,138.664633565377));
#130971=CARTESIAN_POINT('Ctrl Pts',(81.8758303269309,-8.41296773760928,
138.553500447386));
#130972=CARTESIAN_POINT('Ctrl Pts',(81.5105983945688,-10.2575528443921,
138.442367329394));
#130973=CARTESIAN_POINT('Ctrl Pts',(79.7628072363265,-10.9511753556914,
138.331234211403));
#130974=CARTESIAN_POINT('Ctrl Pts',(78.2321042891996,-9.85900574355044,
138.220101093411));
#130975=CARTESIAN_POINT('Ctrl Pts',(78.3194490519439,-7.98064008895766,
138.10896797542));
#130976=CARTESIAN_POINT('Ctrl Pts',(79.9449002020512,-7.0352328325274,137.997834857428));
#130977=CARTESIAN_POINT('Ctrl Pts',(81.6207808491711,-7.88805777822167,
137.886701739436));
#130978=CARTESIAN_POINT('Ctrl Pts',(81.8132590731305,-9.75857603145555,
137.775568621445));
#130979=CARTESIAN_POINT('Ctrl Pts',(80.3461712225592,-10.9348156333929,
137.664435503453));
#130980=CARTESIAN_POINT('Ctrl Pts',(78.5622538447273,-10.3402358189599,
137.553302385462));
#130981=CARTESIAN_POINT('Ctrl Pts',(78.094218336951,-8.51901942944539,137.44216926747));
#130982=CARTESIAN_POINT('Ctrl Pts',(79.3704292182216,-7.13801539048741,
137.331036149478));
#130983=CARTESIAN_POINT('Ctrl Pts',(81.222848058548,-7.46117295258134,137.219903031487));
#130984=CARTESIAN_POINT('Ctrl Pts',(81.9560682249059,-9.1927255963959,137.108769913495));
#130985=CARTESIAN_POINT('Ctrl Pts',(80.8990177617125,-10.7478881886462,
136.997636795504));
#130986=CARTESIAN_POINT('Ctrl Pts',(79.0191508580167,-10.7033147145058,
136.886503677512));
#130987=CARTESIAN_POINT('Ctrl Pts',(78.0369956949045,-9.0998005718031,136.775370559521));
#130988=CARTESIAN_POINT('Ctrl Pts',(78.8514593349149,-7.40494501768999,
136.664237441529));
#130989=CARTESIAN_POINT('Ctrl Pts',(80.7171125977301,-7.16994656413151,
136.553104323538));
#130990=CARTESIAN_POINT('Ctrl Pts',(81.9264361858263,-8.60988504528501,
136.441971205546));
#130991=CARTESIAN_POINT('Ctrl Pts',(81.3726095528648,-10.4068720877668,
136.330838087554));
#130992=CARTESIAN_POINT('Ctrl Pts',(79.5625166317358,-10.9162344215796,
136.219704969563));
#130993=CARTESIAN_POINT('Ctrl Pts',(78.15282570842,-9.67178359051037,136.108571851571));
#130994=CARTESIAN_POINT('Ctrl Pts',(78.4337414008296,-7.81248997626183,
135.99743873358));
#130995=CARTESIAN_POINT('Ctrl Pts',(80.148158610538,-7.04005227567747,135.886305615588));
#130996=CARTESIAN_POINT('Ctrl Pts',(81.7269752284157,-8.06143587518381,
135.775172497597));
#130997=CARTESIAN_POINT('Ctrl Pts',(81.7251961441649,-9.9418303032459,135.664039379605));
#130998=CARTESIAN_POINT('Ctrl Pts',(80.1444496457157,-10.9602245676979,
135.552906261614));
#130999=CARTESIAN_POINT('Ctrl Pts',(78.4314971460249,-10.1845441541056,
135.441773143622));
#131000=CARTESIAN_POINT('Ctrl Pts',(78.1541001939629,-8.32472230747231,
135.330640025631));
#131001=CARTESIAN_POINT('Ctrl Pts',(79.5661433982943,-7.08294118371136,
135.219506907639));
#131002=CARTESIAN_POINT('Ctrl Pts',(81.3752692409363,-7.59572774331752,
135.108373789647));
#131003=CARTESIAN_POINT('Ctrl Pts',(81.9256945442036,-9.39375954385691,
134.997240671656));
#131004=CARTESIAN_POINT('Ctrl Pts',(80.713648406017,-10.8314071116339,134.886107553664));
#131005=CARTESIAN_POINT('Ctrl Pts',(78.8484431577161,-10.592878807362,134.774974435673));
#131006=CARTESIAN_POINT('Ctrl Pts',(78.0371880563092,-8.89648512349353,
134.663841317681));
#131007=CARTESIAN_POINT('Ctrl Pts',(79.0223757012933,-7.29483232890963,
134.55270819969));
#131008=CARTESIAN_POINT('Ctrl Pts',(80.9023235833712,-7.25381610165316,
134.441575081698));
#131009=CARTESIAN_POINT('Ctrl Pts',(81.9564294068378,-8.81097610729224,
134.330441963706));
#131010=CARTESIAN_POINT('Ctrl Pts',(81.2199340328551,-10.5411382194453,
134.219308845715));
#131011=CARTESIAN_POINT('Ctrl Pts',(79.3669070158681,-10.8607899745529,
134.108175727723));
#131012=CARTESIAN_POINT('Ctrl Pts',(78.0933116162554,-9.4773735049699,133.997042609732));
#131013=CARTESIAN_POINT('Ctrl Pts',(78.5647924719695,-7.6570460144004,133.88590949174));
#131014=CARTESIAN_POINT('Ctrl Pts',(80.3498317465547,-7.06584286960547,
133.774776373749));
#131015=CARTESIAN_POINT('Ctrl Pts',(81.8146912374499,-8.24485645823041,
133.663643255757));
#131016=CARTESIAN_POINT('Ctrl Pts',(81.6186738822797,-10.1150071384431,
133.552510137766));
#131017=CARTESIAN_POINT('Ctrl Pts',(79.9411824796641,-10.9646593992994,
133.441377019774));
#131018=CARTESIAN_POINT('Ctrl Pts',(78.3175231866948,-10.0161780496764,
133.330243901783));
#131019=CARTESIAN_POINT('Ctrl Pts',(78.2337328949045,-8.13765055261137,
133.219110783791));
#131020=CARTESIAN_POINT('Ctrl Pts',(79.7664997772935,-7.04837921153991,
133.107977665799));
#131021=CARTESIAN_POINT('Ctrl Pts',(81.5129752539825,-7.74530803111284,
132.996844547808));
#131022=CARTESIAN_POINT('Ctrl Pts',(81.8747162281011,-9.59058032480595,
132.885711429816));
#131023=CARTESIAN_POINT('Ctrl Pts',(80.5206431221497,-10.8953302602216,
132.774578311825));
#131024=CARTESIAN_POINT('Ctrl Pts',(78.6900569384936,-10.4653993420104,
132.663445193833));
#131025=CARTESIAN_POINT('Ctrl Pts',(78.0583822035841,-8.69427726843509,
132.552312075842));
#131026=CARTESIAN_POINT('Ctrl Pts',(79.2037524972869,-7.20296467191772,
132.44117895785));
#131027=CARTESIAN_POINT('Ctrl Pts',(81.077879845468,-7.35636953828203,132.330045839859));
#131028=CARTESIAN_POINT('Ctrl Pts',(81.9654891341413,-9.01408969587618,
132.218912721867));
#131029=CARTESIAN_POINT('Ctrl Pts',(81.0542054063466,-10.6589144092374,
132.107779603875));
#131030=CARTESIAN_POINT('Ctrl Pts',(79.1780713975498,-10.7854353610338,
131.996646485884));
#131031=CARTESIAN_POINT('Ctrl Pts',(78.0541987964962,-9.27785559635263,
131.885513367892));
#131032=CARTESIAN_POINT('Ctrl Pts',(78.7112000429067,-7.51597145361696,
131.774380249901));
#131033=CARTESIAN_POINT('Ctrl Pts',(80.5477617366628,-7.11232864729046,
131.663247131909));
#131034=CARTESIAN_POINT('Ctrl Pts',(81.8829903294524,-8.43635696105569,
131.552114013917));
#131035=CARTESIAN_POINT('Ctrl Pts',(81.4948320587062,-10.2762535686903,
131.440980895926));
#131036=CARTESIAN_POINT('Ctrl Pts',(79.7385446523142,-10.9480726777078,
131.329847777934));
#131037=CARTESIAN_POINT('Ctrl Pts',(78.2215514698866,-9.83693899608168,
131.218714659943));
#131038=CARTESIAN_POINT('Ctrl Pts',(78.3322643833567,-7.95980580489549,
131.107581541951));
#131039=CARTESIAN_POINT('Ctrl Pts',(79.9693545703466,-7.03469928015326,
130.99644842396));
#131040=CARTESIAN_POINT('Ctrl Pts',(81.6344926694737,-7.90831333293382,
130.885315305968));
#131041=CARTESIAN_POINT('Ctrl Pts',(81.8036787266466,-9.78108198107158,
130.774182187977));
#131042=CARTESIAN_POINT('Ctrl Pts',(80.3220670575926,-10.9389736789513,
130.663049069985));
#131043=CARTESIAN_POINT('Ctrl Pts',(78.5456868663343,-10.3222403037902,
130.551915951993));
#131044=CARTESIAN_POINT('Ctrl Pts',(78.1003514489162,-8.49534065136783,
130.440782834002));
#131045=CARTESIAN_POINT('Ctrl Pts',(79.3936488425649,-7.13032491058225,
130.32964971601));
#131046=CARTESIAN_POINT('Ctrl Pts',(81.2419033200459,-7.47650978467848,
130.218516598019));
#131047=CARTESIAN_POINT('Ctrl Pts',(81.9535176916404,-9.21705208375298,
130.107383480027));
#131048=CARTESIAN_POINT('Ctrl Pts',(80.8771984544237,-10.7589413763661,
129.996250362036));
#131049=CARTESIAN_POINT('Ctrl Pts',(78.9980271998695,-10.6909750100548,
129.885117244044));
#131050=CARTESIAN_POINT('Ctrl Pts',(78.035912068222,-9.0753684670664,129.773984126053));
#131051=CARTESIAN_POINT('Ctrl Pts',(78.8713846530321,-7.39076801526417,
129.662851008061));
#131052=CARTESIAN_POINT('Ctrl Pts',(80.7398571901727,-7.17902807893094,
129.551717890069));
#131053=CARTESIAN_POINT('Ctrl Pts',(81.9310876574871,-8.63385591733535,
129.440584772078));
#131054=CARTESIAN_POINT('Ctrl Pts',(81.3551063262338,-10.4239106328993,
129.329451654086));
#131055=CARTESIAN_POINT('Ctrl Pts',(79.538478193619,-10.910506172836,129.218318536095));
#131056=CARTESIAN_POINT('Ctrl Pts',(78.1450715714801,-9.64902245878714,
129.107185418103));
#131057=CARTESIAN_POINT('Ctrl Pts',(78.4476863760178,-7.79252426730275,
128.996052300112));
#131058=CARTESIAN_POINT('Ctrl Pts',(80.1745006914082,-7.04323474754915,
128.88491918212));
#131059=CARTESIAN_POINT('Ctrl Pts',(81.2128991836478,-7.73509822724767,
128.810830436792));
#131060=CARTESIAN_POINT('Ctrl Pts',(81.4708680902966,-8.22417585740202,
128.773786064129));
#131061=CARTESIAN_POINT('Ctrl Pts',(81.3664711939768,-7.83696787750457,
140.074173751493));
#131062=CARTESIAN_POINT('Ctrl Pts',(81.7533428307448,-8.29148551815949,
140.03711623992));
#131063=CARTESIAN_POINT('Ctrl Pts',(82.0304698841766,-9.60943536740704,
139.963014355682));
#131064=CARTESIAN_POINT('Ctrl Pts',(80.5873966270283,-11.0392046868368,
139.85186809878));
#131065=CARTESIAN_POINT('Ctrl Pts',(78.6061897192665,-10.5981437127428,
139.740734980789));
#131066=CARTESIAN_POINT('Ctrl Pts',(77.900983945294,-8.69648618112318,139.629601862797));
#131067=CARTESIAN_POINT('Ctrl Pts',(79.1167163440794,-7.07159944870142,
139.518468744806));
#131068=CARTESIAN_POINT('Ctrl Pts',(81.1409448562311,-7.21215794805729,
139.407335626814));
#131069=CARTESIAN_POINT('Ctrl Pts',(82.1208965373333,-8.98877680806325,
139.296202508823));
#131070=CARTESIAN_POINT('Ctrl Pts',(81.1597393914615,-10.7757864094529,
139.185069390831));
#131071=CARTESIAN_POINT('Ctrl Pts',(79.1371337390217,-10.9374682937912,
139.073936272839));
#131072=CARTESIAN_POINT('Ctrl Pts',(77.9042618312433,-9.32593134449562,
138.962803154848));
#131073=CARTESIAN_POINT('Ctrl Pts',(78.5894897434344,-7.41607531141488,
138.851670036856));
#131074=CARTESIAN_POINT('Ctrl Pts',(80.565673254534,-6.95589628653788,138.740536918865));
#131075=CARTESIAN_POINT('Ctrl Pts',(82.0241298030518,-8.36655811530563,
138.629403800873));
#131076=CARTESIAN_POINT('Ctrl Pts',(81.630023348589,-10.3569725122268,138.518270682882));
#131077=CARTESIAN_POINT('Ctrl Pts',(79.7440552404305,-11.105431462395,138.40713756489));
#131078=CARTESIAN_POINT('Ctrl Pts',(78.0923379126866,-9.92691705723613,
138.296004446898));
#131079=CARTESIAN_POINT('Ctrl Pts',(78.1865879815086,-7.90005148847718,
138.184871328907));
#131080=CARTESIAN_POINT('Ctrl Pts',(79.9405441198124,-6.87990218377285,
138.073738210915));
#131081=CARTESIAN_POINT('Ctrl Pts',(81.7489166125117,-7.80014980136526,
137.962605092924));
#131082=CARTESIAN_POINT('Ctrl Pts',(81.9566117883287,-9.81854756856506,
137.851471974932));
#131083=CARTESIAN_POINT('Ctrl Pts',(80.3735388422295,-11.0877783724548,
137.740338856941));
#131084=CARTESIAN_POINT('Ctrl Pts',(78.4485884462312,-10.4461922410183,
137.629205738949));
#131085=CARTESIAN_POINT('Ctrl Pts',(77.9435509667878,-8.48099404643846,
137.518072620958));
#131086=CARTESIAN_POINT('Ctrl Pts',(79.3206565837898,-6.99081052970044,
137.406939502966));
#131087=CARTESIAN_POINT('Ctrl Pts',(81.3195240339037,-7.33951629648805,
137.295806384974));
#131088=CARTESIAN_POINT('Ctrl Pts',(82.1107111522781,-9.20796210503437,
137.184673266983));
#131089=CARTESIAN_POINT('Ctrl Pts',(80.970092347282,-10.8860728095965,137.073540148991));
#131090=CARTESIAN_POINT('Ctrl Pts',(78.9416068436026,-10.8379754437858,
136.962407031));
#131091=CARTESIAN_POINT('Ctrl Pts',(77.8818044146011,-9.10769060977854,
136.851273913008));
#131092=CARTESIAN_POINT('Ctrl Pts',(78.7606579567252,-7.2788430910581,136.740140795017));
#131093=CARTESIAN_POINT('Ctrl Pts',(80.7738061168806,-7.02526611946862,
136.629007677025));
#131094=CARTESIAN_POINT('Ctrl Pts',(82.0787364621556,-8.57904332011374,
136.517874559034));
#131095=CARTESIAN_POINT('Ctrl Pts',(81.4811253789957,-10.5180966428822,
136.406741441042));
#131096=CARTESIAN_POINT('Ctrl Pts',(79.5279300524522,-11.0677281663842,
136.29560832305));
#131097=CARTESIAN_POINT('Ctrl Pts',(78.0067917223965,-9.72489348702338,
136.184475205059));
#131098=CARTESIAN_POINT('Ctrl Pts',(78.309916059917,-7.71860775680932,136.073342087067));
#131099=CARTESIAN_POINT('Ctrl Pts',(80.159871740457,-6.88510264267047,135.962208969076));
#131100=CARTESIAN_POINT('Ctrl Pts',(81.8635065116406,-7.98723483150851,
135.851075851084));
#131101=CARTESIAN_POINT('Ctrl Pts',(81.861586776469,-10.0162895645985,135.739942733093));
#131102=CARTESIAN_POINT('Ctrl Pts',(80.1558695521316,-11.1151960874005,
135.628809615101));
#131103=CARTESIAN_POINT('Ctrl Pts',(78.3074943787175,-10.2781918977068,
135.51767649711));
#131104=CARTESIAN_POINT('Ctrl Pts',(78.0081669662734,-8.27133617408902,
135.406543379118));
#131105=CARTESIAN_POINT('Ctrl Pts',(79.5318435440799,-6.93138226387365,
135.295410261126));
#131106=CARTESIAN_POINT('Ctrl Pts',(81.4839953368033,-7.48470872576181,
135.184277143135));
#131107=CARTESIAN_POINT('Ctrl Pts',(82.0779361877968,-9.42488940311613,
135.073144025143));
#131108=CARTESIAN_POINT('Ctrl Pts',(80.7700680529474,-10.9761945752546,
134.962010907152));
#131109=CARTESIAN_POINT('Ctrl Pts',(78.7574033264573,-10.7188086898595,
134.85087778916));
#131110=CARTESIAN_POINT('Ctrl Pts',(77.8820119837219,-8.88830143985422,
134.739744671169));
#131111=CARTESIAN_POINT('Ctrl Pts',(78.9450866366803,-7.1600251085068,134.628611553177));
#131112=CARTESIAN_POINT('Ctrl Pts',(80.9736595207341,-7.11576621855994,
134.517478435185));
#131113=CARTESIAN_POINT('Ctrl Pts',(82.1111008885469,-8.79603224810603,
134.406345317194));
#131114=CARTESIAN_POINT('Ctrl Pts',(81.3163796310402,-10.6629775922779,
134.295212199202));
#131115=CARTESIAN_POINT('Ctrl Pts',(79.3168559230081,-11.0079003898369,
134.184079081211));
#131116=CARTESIAN_POINT('Ctrl Pts',(77.942572562528,-9.5151137204279,134.072945963219));
#131117=CARTESIAN_POINT('Ctrl Pts',(78.4513277723769,-7.55087469940482,
133.961812845228));
#131118=CARTESIAN_POINT('Ctrl Pts',(80.3774887600915,-6.9129321905025,133.850679727236));
#131119=CARTESIAN_POINT('Ctrl Pts',(81.9581571767575,-8.18515628704078,
133.739546609245));
#131120=CARTESIAN_POINT('Ctrl Pts',(81.7466430729396,-10.2031574216154,
133.628413491253));
#131121=CARTESIAN_POINT('Ctrl Pts',(79.9365324815659,-11.1199815281129,
133.517280373261));
#131122=CARTESIAN_POINT('Ctrl Pts',(78.1845098611203,-10.0965150984217,
133.40614725527));
#131123=CARTESIAN_POINT('Ctrl Pts',(78.0940952727729,-8.06947489224123,
133.295014137278));
#131124=CARTESIAN_POINT('Ctrl Pts',(79.7480397064628,-6.89408788979295,
133.183881019287));
#131125=CARTESIAN_POINT('Ctrl Pts',(81.6325881178585,-7.6461145384991,133.072747901295));
#131126=CARTESIAN_POINT('Ctrl Pts',(82.0229276257478,-9.63727044998339,
132.961614783304));
#131127=CARTESIAN_POINT('Ctrl Pts',(80.5618041488974,-11.0451713629224,
132.850481665312));
#131128=CARTESIAN_POINT('Ctrl Pts',(78.5864954025802,-10.5812509473544,
132.739348547321));
#131129=CARTESIAN_POINT('Ctrl Pts',(77.9048816988202,-8.67010742733677,
132.628215429329));
#131130=CARTESIAN_POINT('Ctrl Pts',(79.1408027273532,-7.06089457426592,
132.517082311337));
#131131=CARTESIAN_POINT('Ctrl Pts',(81.1630949174867,-7.22642732927219,
132.405949193346));
#131132=CARTESIAN_POINT('Ctrl Pts',(82.1208768601684,-9.01520359966968,
132.294816075354));
#131133=CARTESIAN_POINT('Ctrl Pts',(81.1375488235206,-10.7900649372395,
132.183682957363));
#131134=CARTESIAN_POINT('Ctrl Pts',(79.1130913301086,-10.9265883879828,
132.072549839371));
#131135=CARTESIAN_POINT('Ctrl Pts',(77.9003675597515,-9.29982231625516,
131.96141672138));
#131136=CARTESIAN_POINT('Ctrl Pts',(78.609310039468,-7.39864705981793,131.850283603388));
#131137=CARTESIAN_POINT('Ctrl Pts',(80.591066708024,-6.96309304283512,131.739150485397));
#131138=CARTESIAN_POINT('Ctrl Pts',(82.0318558613661,-8.39179644500338,
131.628017367405));
#131139=CARTESIAN_POINT('Ctrl Pts',(81.6130105570556,-10.3771516792053,
131.516884249414));
#131140=CARTESIAN_POINT('Ctrl Pts',(79.7178745039888,-11.1020834927595,
131.405751131422));
#131141=CARTESIAN_POINT('Ctrl Pts',(78.0809508081225,-9.90310575587979,
131.29461801343));
#131142=CARTESIAN_POINT('Ctrl Pts',(78.2004164679532,-7.87757008667339,
131.183484895439));
#131143=CARTESIAN_POINT('Ctrl Pts',(79.9669318026273,-6.87932644979174,
131.072351777447));
#131144=CARTESIAN_POINT('Ctrl Pts',(81.7637124625041,-7.82200672060876,
130.961218659456));
#131145=CARTESIAN_POINT('Ctrl Pts',(81.946274038393,-9.84283279453126,130.850085541464));
#131146=CARTESIAN_POINT('Ctrl Pts',(80.3475290491337,-11.092265144961,130.738952423472));
#131147=CARTESIAN_POINT('Ctrl Pts',(78.430711714935,-10.4267740356223,130.627819305481));
#131148=CARTESIAN_POINT('Ctrl Pts',(77.9501689505874,-8.45544327048684,
130.516686187489));
#131149=CARTESIAN_POINT('Ctrl Pts',(79.3457119062108,-6.98251205549822,
130.405553069498));
#131150=CARTESIAN_POINT('Ctrl Pts',(81.3400857670997,-7.35606562852865,
130.294419951506));
#131151=CARTESIAN_POINT('Ctrl Pts',(82.1079589788419,-9.23421179689408,
130.183286833515));
#131152=CARTESIAN_POINT('Ctrl Pts',(80.9465480482423,-10.8979998407152,
130.072153715523));
#131153=CARTESIAN_POINT('Ctrl Pts',(78.9188131903647,-10.8246601864401,
129.961020597532));
#131154=CARTESIAN_POINT('Ctrl Pts',(77.8806351185129,-9.08132695063578,
129.84988747954));
#131155=CARTESIAN_POINT('Ctrl Pts',(78.7821585315143,-7.26354528255374,
129.738754361548));
#131156=CARTESIAN_POINT('Ctrl Pts',(80.7983488523086,-7.03506560106271,
129.627621243557));
#131157=CARTESIAN_POINT('Ctrl Pts',(82.0837556700664,-8.6049092824162,129.516488125565));
#131158=CARTESIAN_POINT('Ctrl Pts',(81.4622383815074,-10.5364822220618,
129.405355007574));
#131159=CARTESIAN_POINT('Ctrl Pts',(79.5019911824421,-11.0615470535008,
129.294221889582));
#131160=CARTESIAN_POINT('Ctrl Pts',(77.9984245585591,-9.70033290475177,
129.183088771591));
#131161=CARTESIAN_POINT('Ctrl Pts',(78.3249634975641,-7.69706359795712,
129.071955653599));
#131162=CARTESIAN_POINT('Ctrl Pts',(80.1882963747102,-6.88853671454275,
128.960822535608));
#131163=CARTESIAN_POINT('Ctrl Pts',(81.3087886204161,-7.63509756751294,
128.88673379028));
#131164=CARTESIAN_POINT('Ctrl Pts',(81.5871520441821,-8.16284071836659,
128.849689417616));
#131165=CARTESIAN_POINT('Ctrl Pts',(81.4665867902668,-7.7517574062108,140.150077104981));
#131166=CARTESIAN_POINT('Ctrl Pts',(81.8818028844763,-8.23957564245756,
140.113019593406));
#131167=CARTESIAN_POINT('Ctrl Pts',(82.1792338713718,-9.65408613317302,
140.038917709168));
#131168=CARTESIAN_POINT('Ctrl Pts',(80.6304327069932,-11.1886086362797,
139.927771452267));
#131169=CARTESIAN_POINT('Ctrl Pts',(78.5040711030923,-10.715232979947,139.816638334275));
#131170=CARTESIAN_POINT('Ctrl Pts',(77.7471978685252,-8.67424900035197,
139.705505216284));
#131171=CARTESIAN_POINT('Ctrl Pts',(79.0520018661632,-6.93031365216921,
139.594372098292));
#131172=CARTESIAN_POINT('Ctrl Pts',(81.2245370864363,-7.0811702815103,139.483238980301));
#131173=CARTESIAN_POINT('Ctrl Pts',(82.2762857050234,-8.98795453200066,
139.372105862309));
#131174=CARTESIAN_POINT('Ctrl Pts',(81.2447086182033,-10.9058908097869,
139.260972744318));
#131175=CARTESIAN_POINT('Ctrl Pts',(79.0739151577466,-11.0794184456721,
139.149839626326));
#131176=CARTESIAN_POINT('Ctrl Pts',(77.7507159113895,-9.3498109630691,139.038706508334));
#131177=CARTESIAN_POINT('Ctrl Pts',(78.4861475902798,-7.30002781229801,
138.927573390343));
#131178=CARTESIAN_POINT('Ctrl Pts',(80.607117754376,-6.80613340602198,138.816440272351));
#131179=CARTESIAN_POINT('Ctrl Pts',(82.1724292791728,-8.32014849300197,
138.70530715436));
#131180=CARTESIAN_POINT('Ctrl Pts',(81.7494483026092,-10.4563921800615,
138.594174036368));
#131181=CARTESIAN_POINT('Ctrl Pts',(79.7253032445344,-11.2596875690987,
138.483040918377));
#131182=CARTESIAN_POINT('Ctrl Pts',(77.9525715361738,-9.99482837092183,
138.371907800385));
#131183=CARTESIAN_POINT('Ctrl Pts',(78.0537269110733,-7.81946288799671,
138.260774682393));
#131184=CARTESIAN_POINT('Ctrl Pts',(79.9361880375736,-6.72457153501829,
138.149641564402));
#131185=CARTESIAN_POINT('Ctrl Pts',(81.8770523758524,-7.71224182450884,
138.03850844641));
#131186=CARTESIAN_POINT('Ctrl Pts',(82.0999645035268,-9.8785191056746,137.927375328419));
#131187=CARTESIAN_POINT('Ctrl Pts',(80.4009064619,-11.2407411115166,137.816242210427));
#131188=CARTESIAN_POINT('Ctrl Pts',(78.3349230477351,-10.5521486630767,
137.705109092436));
#131189=CARTESIAN_POINT('Ctrl Pts',(77.7928835966247,-8.44296866343152,
137.593975974444));
#131190=CARTESIAN_POINT('Ctrl Pts',(79.2708839493578,-6.8436056689135,137.482842856453));
#131191=CARTESIAN_POINT('Ctrl Pts',(81.4162000092596,-7.21785964039476,
137.371709738461));
#131192=CARTESIAN_POINT('Ctrl Pts',(82.2653540796503,-9.22319861367285,
137.260576620469));
#131193=CARTESIAN_POINT('Ctrl Pts',(81.0411669328516,-11.0242574305468,
137.149443502478));
#131194=CARTESIAN_POINT('Ctrl Pts',(78.8640628291885,-10.9726361730659,
137.038310384486));
#131195=CARTESIAN_POINT('Ctrl Pts',(77.7266131342975,-9.11558064775398,
136.927177266495));
#131196=CARTESIAN_POINT('Ctrl Pts',(78.6698565785353,-7.15274116442619,
136.816044148503));
#131197=CARTESIAN_POINT('Ctrl Pts',(80.8304996360312,-6.88058567480575,
136.704911030512));
#131198=CARTESIAN_POINT('Ctrl Pts',(82.2310367384848,-8.54820159494246,
136.59377791252));
#131199=CARTESIAN_POINT('Ctrl Pts',(81.5896412051266,-10.6293211979976,
136.482644794529));
#131200=CARTESIAN_POINT('Ctrl Pts',(79.4933434731685,-11.219221911189,136.371511676537));
#131201=CARTESIAN_POINT('Ctrl Pts',(77.8607577363731,-9.77800338353641,
136.260378558545));
#131202=CARTESIAN_POINT('Ctrl Pts',(78.1860907190042,-7.62472553735678,
136.149245440554));
#131203=CARTESIAN_POINT('Ctrl Pts',(80.1715848703761,-6.73015300966351,
136.038112322562));
#131204=CARTESIAN_POINT('Ctrl Pts',(82.0000377948652,-7.91303378783318,
135.926979204571));
#131205=CARTESIAN_POINT('Ctrl Pts',(81.9979774087732,-10.0907488259511,
135.815846086579));
#131206=CARTESIAN_POINT('Ctrl Pts',(80.1672894585474,-11.2701676071032,
135.704712968588));
#131207=CARTESIAN_POINT('Ctrl Pts',(78.1834916114102,-10.3718396413081,
135.593579850596));
#131208=CARTESIAN_POINT('Ctrl Pts',(77.8622337385839,-8.21795004070572,
135.482446732605));
#131209=CARTESIAN_POINT('Ctrl Pts',(79.4975436898657,-6.77982334403592,
135.371313614613));
#131210=CARTESIAN_POINT('Ctrl Pts',(81.5927214326702,-7.37368970820611,
135.260180496621));
#131211=CARTESIAN_POINT('Ctrl Pts',(82.2301778313902,-9.45601926237537,
135.14904737863));
#131212=CARTESIAN_POINT('Ctrl Pts',(80.8264876998778,-11.1209820388755,
135.037914260638));
#131213=CARTESIAN_POINT('Ctrl Pts',(78.6663634951985,-10.8447385723571,
134.926781142647));
#131214=CARTESIAN_POINT('Ctrl Pts',(77.7268359111347,-8.88011775621491,
134.815648024655));
#131215=CARTESIAN_POINT('Ctrl Pts',(78.8677975720673,-7.02521788810393,
134.704514906664));
#131216=CARTESIAN_POINT('Ctrl Pts',(81.044995458097,-6.97771633546675,134.593381788672));
#131217=CARTESIAN_POINT('Ctrl Pts',(82.2657723702561,-8.7810883889198,134.482248670681));
#131218=CARTESIAN_POINT('Ctrl Pts',(81.4128252292252,-10.7848169651105,
134.371115552689));
#131219=CARTESIAN_POINT('Ctrl Pts',(79.2668048301483,-11.1550108051209,
134.259982434697));
#131220=CARTESIAN_POINT('Ctrl Pts',(77.7918335088003,-9.5528539358859,134.148849316706));
#131221=CARTESIAN_POINT('Ctrl Pts',(78.3378630727844,-7.44470338440925,
134.037716198714));
#131222=CARTESIAN_POINT('Ctrl Pts',(80.4051457736282,-6.76002151139955,
133.926583080723));
#131223=CARTESIAN_POINT('Ctrl Pts',(82.1016231160651,-8.12545611585114,
133.815449962731));
#131224=CARTESIAN_POINT('Ctrl Pts',(81.8746122635996,-10.2913077047877,
133.70431684474));
#131225=CARTESIAN_POINT('Ctrl Pts',(79.9318824834679,-11.2753036569265,
133.593183726748));
#131226=CARTESIAN_POINT('Ctrl Pts',(78.0514965355458,-10.176852147167,133.482050608757));
#131227=CARTESIAN_POINT('Ctrl Pts',(77.9544576506411,-8.00129923187109,
133.370917490765));
#131228=CARTESIAN_POINT('Ctrl Pts',(79.7295796356322,-6.73979656804598,
133.259784372773));
#131229=CARTESIAN_POINT('Ctrl Pts',(81.7522009817343,-7.54692104588537,
133.148651254782));
#131230=CARTESIAN_POINT('Ctrl Pts',(82.1711390233947,-9.6839605751608,133.03751813679));
#131231=CARTESIAN_POINT('Ctrl Pts',(80.6029651756449,-11.1950124656231,
132.926385018798));
#131232=CARTESIAN_POINT('Ctrl Pts',(78.482933866667,-10.6971025526985,132.815251900807));
#131233=CARTESIAN_POINT('Ctrl Pts',(77.7513811940564,-8.64593758623847,
132.704118782815));
#131234=CARTESIAN_POINT('Ctrl Pts',(79.0778529574195,-6.91882447661411,
132.592985664824));
#131235=CARTESIAN_POINT('Ctrl Pts',(81.2483099895054,-7.09648512026235,
132.481852546832));
#131236=CARTESIAN_POINT('Ctrl Pts',(82.2762645861953,-9.01631750346318,
132.370719428841));
#131237=CARTESIAN_POINT('Ctrl Pts',(81.2208922406947,-10.9212154652415,
132.259586310849));
#131238=CARTESIAN_POINT('Ctrl Pts',(79.0481112626675,-11.0677414149317,
132.148453192858));
#131239=CARTESIAN_POINT('Ctrl Pts',(77.7465363230069,-9.32178903615767,
132.037320074866));
#131240=CARTESIAN_POINT('Ctrl Pts',(78.5074200360291,-7.2813226660189,131.926186956875));
#131241=CARTESIAN_POINT('Ctrl Pts',(80.6343716793853,-6.81385743837979,
131.815053838883));
#131242=CARTESIAN_POINT('Ctrl Pts',(82.1807213932797,-8.34723592895108,
131.703920720891));
#131243=CARTESIAN_POINT('Ctrl Pts',(81.7311890554049,-10.4780497897204,
131.5927876029));
#131244=CARTESIAN_POINT('Ctrl Pts',(79.6972043556635,-11.2560943078113,
131.481654484908));
#131245=CARTESIAN_POINT('Ctrl Pts',(77.9403501463584,-9.96927251567788,
131.370521366917));
#131246=CARTESIAN_POINT('Ctrl Pts',(78.0685685525499,-7.79533436845129,
131.259388248925));
#131247=CARTESIAN_POINT('Ctrl Pts',(79.9645090349079,-6.72395361943023,
131.148255130934));
#131248=CARTESIAN_POINT('Ctrl Pts',(81.8929322555346,-7.73570010828368,
131.037122012942));
#131249=CARTESIAN_POINT('Ctrl Pts',(82.0888693501395,-9.90458360799097,
130.92598889495));
#131250=CARTESIAN_POINT('Ctrl Pts',(80.3729910406748,-11.2455566109706,
130.814855776959));
#131251=CARTESIAN_POINT('Ctrl Pts',(78.3157365635357,-10.5313077674544,
130.703722658967));
#131252=CARTESIAN_POINT('Ctrl Pts',(77.7999864522586,-8.41554588960587,
130.592589540976));
#131253=CARTESIAN_POINT('Ctrl Pts',(79.2977749698569,-6.8346992004142,130.481456422984));
#131254=CARTESIAN_POINT('Ctrl Pts',(81.4382682141534,-7.23562147237883,
130.370323304993));
#131255=CARTESIAN_POINT('Ctrl Pts',(82.2624002660436,-9.25137151003518,
130.259190187001));
#131256=CARTESIAN_POINT('Ctrl Pts',(81.0158976420608,-11.0370583050643,
130.14805706901));
#131257=CARTESIAN_POINT('Ctrl Pts',(78.8395991808601,-10.9583453628253,
130.036923951018));
#131258=CARTESIAN_POINT('Ctrl Pts',(77.7253581688036,-9.08728543420517,
129.925790833026));
#131259=CARTESIAN_POINT('Ctrl Pts',(78.6929324099967,-7.13632254984329,
129.814657715035));
#131260=CARTESIAN_POINT('Ctrl Pts',(80.8568405144443,-6.89110312319448,
129.703524597043));
#131261=CARTESIAN_POINT('Ctrl Pts',(82.2364236826459,-8.57596264749706,
129.592391479052));
#131262=CARTESIAN_POINT('Ctrl Pts',(81.5693704367807,-10.6490538112244,
129.48125836106));
#131263=CARTESIAN_POINT('Ctrl Pts',(79.4655041712653,-11.2125879341655,
129.370125243069));
#131264=CARTESIAN_POINT('Ctrl Pts',(77.8517775456378,-9.75164335071642,
129.258992125077));
#131265=CARTESIAN_POINT('Ctrl Pts',(78.2022406191104,-7.60160292861149,
129.147859007086));
#131266=CARTESIAN_POINT('Ctrl Pts',(80.2020920580122,-6.73383868153635,
129.036725889094));
#131267=CARTESIAN_POINT('Ctrl Pts',(81.4046780571844,-7.5350969077782,128.962637143766));
#131268=CARTESIAN_POINT('Ctrl Pts',(81.7034359980675,-8.10150557933116,
128.925592771103));
#131269=CARTESIAN_POINT('Ctrl Pts',(81.566702386557,-7.66654693491703,140.225980458467));
#131270=CARTESIAN_POINT('Ctrl Pts',(82.010262938208,-8.18766576675564,140.188922946894));
#131271=CARTESIAN_POINT('Ctrl Pts',(82.327997858567,-9.69873689893897,140.114821062656));
#131272=CARTESIAN_POINT('Ctrl Pts',(80.6734687869581,-11.3380125857227,
140.003674805754));
#131273=CARTESIAN_POINT('Ctrl Pts',(78.401952486918,-10.8323222471513,139.892541687763));
#131274=CARTESIAN_POINT('Ctrl Pts',(77.5934117917565,-8.65201181958074,
139.781408569771));
#131275=CARTESIAN_POINT('Ctrl Pts',(78.9872873882469,-6.78902785563699,
139.67027545178));
#131276=CARTESIAN_POINT('Ctrl Pts',(81.3081293166415,-6.95018261496333,
139.559142333788));
#131277=CARTESIAN_POINT('Ctrl Pts',(82.4316748727135,-8.98713225593806,
139.448009215796));
#131278=CARTESIAN_POINT('Ctrl Pts',(81.3296778449453,-11.035995210121,139.336876097805));
#131279=CARTESIAN_POINT('Ctrl Pts',(79.0106965764716,-11.2213685975531,
139.225742979813));
#131280=CARTESIAN_POINT('Ctrl Pts',(77.5971699915357,-9.37369058164258,
139.114609861822));
#131281=CARTESIAN_POINT('Ctrl Pts',(78.3828054371252,-7.18398031318115,
139.00347674383));
#131282=CARTESIAN_POINT('Ctrl Pts',(80.6485622542183,-6.65637052550606,
138.892343625839));
#131283=CARTESIAN_POINT('Ctrl Pts',(82.3207287552936,-8.27373887069834,
138.781210507847));
#131284=CARTESIAN_POINT('Ctrl Pts',(81.8688732566295,-10.5558118478961,
138.670077389856));
#131285=CARTESIAN_POINT('Ctrl Pts',(79.7065512486383,-11.4139436758023,
138.558944271864));
#131286=CARTESIAN_POINT('Ctrl Pts',(77.8128051596609,-10.0627396846075,
138.447811153873));
#131287=CARTESIAN_POINT('Ctrl Pts',(77.9208658406379,-7.73887428751625,
138.336678035881));
#131288=CARTESIAN_POINT('Ctrl Pts',(79.9318319553347,-6.56924088626373,
138.225544917889));
#131289=CARTESIAN_POINT('Ctrl Pts',(82.0051881391931,-7.62433384765245,
138.114411799898));
#131290=CARTESIAN_POINT('Ctrl Pts',(82.243317218725,-9.93849064278411,138.003278681906));
#131291=CARTESIAN_POINT('Ctrl Pts',(80.4282740815705,-11.3937038505785,
137.892145563915));
#131292=CARTESIAN_POINT('Ctrl Pts',(78.221257649239,-10.658105085135,137.781012445923));
#131293=CARTESIAN_POINT('Ctrl Pts',(77.6422162264616,-8.40494328042461,
137.669879327932));
#131294=CARTESIAN_POINT('Ctrl Pts',(79.2211113149259,-6.69640080812653,
137.55874620994));
#131295=CARTESIAN_POINT('Ctrl Pts',(81.5128759846153,-7.09620298430149,
137.447613091949));
#131296=CARTESIAN_POINT('Ctrl Pts',(82.4199970070225,-9.23843512231133,
137.336479973957));
#131297=CARTESIAN_POINT('Ctrl Pts',(81.1122415184211,-11.162442051497,137.225346855965));
#131298=CARTESIAN_POINT('Ctrl Pts',(78.7865188147747,-11.107296902346,137.114213737974));
#131299=CARTESIAN_POINT('Ctrl Pts',(77.5714218539939,-9.12347068572941,
137.003080619982));
#131300=CARTESIAN_POINT('Ctrl Pts',(78.5790552003455,-7.02663923779428,
136.891947501991));
#131301=CARTESIAN_POINT('Ctrl Pts',(80.8871931551817,-6.73590523014286,
136.780814383999));
#131302=CARTESIAN_POINT('Ctrl Pts',(82.3833370148139,-8.51735986977119,
136.669681266007));
#131303=CARTESIAN_POINT('Ctrl Pts',(81.6981570312575,-10.740545753113,136.558548148016));
#131304=CARTESIAN_POINT('Ctrl Pts',(79.4587568938848,-11.3707156559936,
136.447415030024));
#131305=CARTESIAN_POINT('Ctrl Pts',(77.7147237503498,-9.83111328004943,
136.336281912033));
#131306=CARTESIAN_POINT('Ctrl Pts',(78.0622653780914,-7.53084331790425,
136.225148794041));
#131307=CARTESIAN_POINT('Ctrl Pts',(80.1832980002954,-6.57520337665653,
136.11401567605));
#131308=CARTESIAN_POINT('Ctrl Pts',(82.13656907809,-7.83883274415787,136.002882558058));
#131309=CARTESIAN_POINT('Ctrl Pts',(82.1343680410774,-10.1652080873037,
135.891749440067));
#131310=CARTESIAN_POINT('Ctrl Pts',(80.1787093649632,-11.4251391268058,
135.780616322075));
#131311=CARTESIAN_POINT('Ctrl Pts',(78.0594888441027,-10.4654873849093,
135.669483204083));
#131312=CARTESIAN_POINT('Ctrl Pts',(77.7163005108943,-8.16456390732242,
135.558350086092));
#131313=CARTESIAN_POINT('Ctrl Pts',(79.4632438356514,-6.62826442419822,
135.4472169681));
#131314=CARTESIAN_POINT('Ctrl Pts',(81.7014475285372,-7.2626706906504,135.336083850109));
#131315=CARTESIAN_POINT('Ctrl Pts',(82.3824194749835,-9.48714912163461,
135.224950732117));
#131316=CARTESIAN_POINT('Ctrl Pts',(80.8829073468083,-11.2657695024962,
135.113817614126));
#131317=CARTESIAN_POINT('Ctrl Pts',(78.5753236639396,-10.9706684548548,
135.002684496134));
#131318=CARTESIAN_POINT('Ctrl Pts',(77.5716598385475,-8.8719340725756,134.891551378143));
#131319=CARTESIAN_POINT('Ctrl Pts',(78.7905085074542,-6.89041066770108,
134.780418260151));
#131320=CARTESIAN_POINT('Ctrl Pts',(81.11633139546,-6.83966645237353,134.66928514216));
#131321=CARTESIAN_POINT('Ctrl Pts',(82.4204438519653,-8.76614452973359,
134.558152024168));
#131322=CARTESIAN_POINT('Ctrl Pts',(81.5092708274104,-10.906656337943,134.447018906177));
#131323=CARTESIAN_POINT('Ctrl Pts',(79.2167537372884,-11.3021212204049,
134.335885788185));
#131324=CARTESIAN_POINT('Ctrl Pts',(77.6410944550728,-9.59059415134389,
134.224752670193));
#131325=CARTESIAN_POINT('Ctrl Pts',(78.224398373192,-7.33853206941367,134.113619552202));
#131326=CARTESIAN_POINT('Ctrl Pts',(80.432802787165,-6.60711083229659,134.00248643421));
#131327=CARTESIAN_POINT('Ctrl Pts',(82.2450890553728,-8.06575594466151,
133.891353316218));
#131328=CARTESIAN_POINT('Ctrl Pts',(82.0025814542595,-10.37945798796,133.780220198227));
#131329=CARTESIAN_POINT('Ctrl Pts',(79.9272324853697,-11.4306257857401,
133.669087080235));
#131330=CARTESIAN_POINT('Ctrl Pts',(77.9184832099714,-10.2571891959123,
133.557953962244));
#131331=CARTESIAN_POINT('Ctrl Pts',(77.8148200285094,-7.93312357150095,
133.446820844252));
#131332=CARTESIAN_POINT('Ctrl Pts',(79.7111195648015,-6.58550524629902,
133.335687726261));
#131333=CARTESIAN_POINT('Ctrl Pts',(81.8718138456102,-7.44772755327165,
133.224554608269));
#131334=CARTESIAN_POINT('Ctrl Pts',(82.3193504210416,-9.73065070033822,
133.113421490278));
#131335=CARTESIAN_POINT('Ctrl Pts',(80.6441262023926,-11.3448535683239,
133.002288372286));
#131336=CARTESIAN_POINT('Ctrl Pts',(78.3793723307539,-10.8129541580425,
132.891155254295));
#131337=CARTESIAN_POINT('Ctrl Pts',(77.5978806892923,-8.62176774514015,
132.780022136303));
#131338=CARTESIAN_POINT('Ctrl Pts',(79.014903187486,-6.77675437896232,132.668889018312));
#131339=CARTESIAN_POINT('Ctrl Pts',(81.3335250615239,-6.9665429112525,132.55775590032));
#131340=CARTESIAN_POINT('Ctrl Pts',(82.4316523122226,-9.01743140725671,
132.446622782328));
#131341=CARTESIAN_POINT('Ctrl Pts',(81.3042356578685,-11.0523659932435,
132.335489664337));
#131342=CARTESIAN_POINT('Ctrl Pts',(78.9831311952265,-11.2088944418807,
132.224356546345));
#131343=CARTESIAN_POINT('Ctrl Pts',(77.5927050862621,-9.34375575606019,
132.113223428354));
#131344=CARTESIAN_POINT('Ctrl Pts',(78.4055300325905,-7.16399827221987,
132.002090310362));
#131345=CARTESIAN_POINT('Ctrl Pts',(80.6776766507465,-6.66462183392446,
131.890957192371));
#131346=CARTESIAN_POINT('Ctrl Pts',(82.3295869251935,-8.30267541289877,
131.779824074379));
#131347=CARTESIAN_POINT('Ctrl Pts',(81.8493675537542,-10.5789479002354,
131.668690956388));
#131348=CARTESIAN_POINT('Ctrl Pts',(79.6765342073382,-11.4101051228631,
131.557557838396));
#131349=CARTESIAN_POINT('Ctrl Pts',(77.7997494845942,-10.035439275476,131.446424720404));
#131350=CARTESIAN_POINT('Ctrl Pts',(77.9367206371466,-7.71309865022921,
131.335291602413));
#131351=CARTESIAN_POINT('Ctrl Pts',(79.9620862671886,-6.56858078906871,
131.224158484421));
#131352=CARTESIAN_POINT('Ctrl Pts',(82.0221520485652,-7.6493934959586,131.11302536643));
#131353=CARTESIAN_POINT('Ctrl Pts',(82.2314646618857,-9.96633442145068,
131.001892248438));
#131354=CARTESIAN_POINT('Ctrl Pts',(80.3984530322158,-11.3988480769803,
130.890759130447));
#131355=CARTESIAN_POINT('Ctrl Pts',(78.2007614121363,-10.6358414992865,
130.779626012455));
#131356=CARTESIAN_POINT('Ctrl Pts',(77.6498039539297,-8.3756485087249,130.668492894463));
#131357=CARTESIAN_POINT('Ctrl Pts',(79.249838033503,-6.68688634533016,130.557359776472));
#131358=CARTESIAN_POINT('Ctrl Pts',(81.536450661207,-7.11517731622901,130.44622665848));
#131359=CARTESIAN_POINT('Ctrl Pts',(82.4168415532452,-9.26853122317627,
130.335093540489));
#131360=CARTESIAN_POINT('Ctrl Pts',(81.0852472358793,-11.1761167694134,
130.223960422497));
#131361=CARTESIAN_POINT('Ctrl Pts',(78.7603851713554,-11.0920305392106,
130.112827304506));
#131362=CARTESIAN_POINT('Ctrl Pts',(77.5700812190944,-9.09324391777456,
130.001694186514));
#131363=CARTESIAN_POINT('Ctrl Pts',(78.6037062884789,-7.00909981713288,
129.890561068523));
#131364=CARTESIAN_POINT('Ctrl Pts',(80.9153321765801,-6.74714064532625,
129.779427950531));
#131365=CARTESIAN_POINT('Ctrl Pts',(82.3890916952254,-8.54701601257792,
129.668294832539));
#131366=CARTESIAN_POINT('Ctrl Pts',(81.6765024920544,-10.7616254003869,
129.557161714548));
#131367=CARTESIAN_POINT('Ctrl Pts',(79.4290171600884,-11.3636288148302,
129.446028596556));
#131368=CARTESIAN_POINT('Ctrl Pts',(77.7051305327169,-9.80295379668104,
129.334895478565));
#131369=CARTESIAN_POINT('Ctrl Pts',(78.0795177406565,-7.50614225926586,
129.223762360573));
#131370=CARTESIAN_POINT('Ctrl Pts',(80.2158877413142,-6.57914064852994,
129.112629242582));
#131371=CARTESIAN_POINT('Ctrl Pts',(81.5005674939528,-7.43509624804347,
129.038540497254));
#131372=CARTESIAN_POINT('Ctrl Pts',(81.8197199519531,-8.04017044029572,
129.00149612459));
#131373=CARTESIAN_POINT('Ctrl Pts',(81.2690708798523,-7.92064134695145,
140.));
#131374=CARTESIAN_POINT('Ctrl Pts',(81.3143922592526,-7.96292138382976,
140.));
#131375=CARTESIAN_POINT('Ctrl Pts',(81.3569831825551,-8.00777112798572,
140.));
#131376=CARTESIAN_POINT('Ctrl Pts',(81.3968454433617,-8.05484540576437,
140.));
#131377=CARTESIAN_POINT('Ctrl Pts',(81.4393469469686,-8.10503642720478,
140.));
#131378=CARTESIAN_POINT('Ctrl Pts',(81.4787472273247,-8.15775653436478,
140.));
#131379=CARTESIAN_POINT('Ctrl Pts',(81.5150195980997,-8.21264209971973,
140.));
#131380=CARTESIAN_POINT('Ctrl Pts',(81.5467579225278,-8.26066696940532,
140.));
#131381=CARTESIAN_POINT('Ctrl Pts',(81.5761011969975,-8.31035099456426,
140.));
#131382=CARTESIAN_POINT('Ctrl Pts',(81.6030086375,-8.36147814360778,140.));
#131383=CARTESIAN_POINT('Ctrl Pts',(81.6165038148102,-8.38712049118233,
140.));
#131384=CARTESIAN_POINT('Ctrl Pts',(81.6293859141812,-8.41312620242211,
140.));
#131385=CARTESIAN_POINT('Ctrl Pts',(81.6416474501114,-8.4394698635273,140.));
#131386=CARTESIAN_POINT('Ctrl Pts',(81.6472598357352,-8.45152796013997,
140.));
#131387=CARTESIAN_POINT('Ctrl Pts',(81.6527427933622,-8.46365856446902,
140.));
#131388=CARTESIAN_POINT('Ctrl Pts',(81.6580870749244,-8.47583923409168,
140.));
#131389=CARTESIAN_POINT('Ctrl Pts',(81.6849965902534,-8.53717131626459,
140.));
#131390=CARTESIAN_POINT('Ctrl Pts',(81.7084453900242,-8.59987896898128,
140.));
#131391=CARTESIAN_POINT('Ctrl Pts',(81.7284103210218,-8.66360419268533,
140.));
#131392=CARTESIAN_POINT('Ctrl Pts',(81.7487859790682,-8.72864039878482,
140.));
#131393=CARTESIAN_POINT('Ctrl Pts',(81.7655335305298,-8.79473730760459,
140.));
#131394=CARTESIAN_POINT('Ctrl Pts',(81.7785886627868,-8.86155122472489,
140.));
#131395=CARTESIAN_POINT('Ctrl Pts',(81.7894440925633,-8.91710744362078,
140.));
#131396=CARTESIAN_POINT('Ctrl Pts',(81.7977459929751,-8.97316035289416,
140.));
#131397=CARTESIAN_POINT('Ctrl Pts',(81.8034327980193,-9.02952452320688,
140.));
#131398=CARTESIAN_POINT('Ctrl Pts',(81.806059918276,-9.05556294942861,140.));
#131399=CARTESIAN_POINT('Ctrl Pts',(81.8081286078971,-9.08166791525863,
140.));
#131400=CARTESIAN_POINT('Ctrl Pts',(81.8096310008458,-9.10782153849097,
140.));
#131401=CARTESIAN_POINT('Ctrl Pts',(81.8102882463636,-9.11926285393143,
140.));
#131402=CARTESIAN_POINT('Ctrl Pts',(81.8108370002414,-9.13071330424245,
140.));
#131403=CARTESIAN_POINT('Ctrl Pts',(81.8112762675986,-9.14215720643866,
140.));
#131404=CARTESIAN_POINT('Ctrl Pts',(81.813968295031,-9.21229057315298,140.));
#131405=CARTESIAN_POINT('Ctrl Pts',(81.8125603873038,-9.28230940983736,
140.));
#131406=CARTESIAN_POINT('Ctrl Pts',(81.8069982742316,-9.35185253060966,
140.));
#131407=CARTESIAN_POINT('Ctrl Pts',(81.8020260032913,-9.41402085297565,
140.));
#131408=CARTESIAN_POINT('Ctrl Pts',(81.7937335362703,-9.47580996983483,
140.));
#131409=CARTESIAN_POINT('Ctrl Pts',(81.7820489797618,-9.53697398237741,
140.));
#131410=CARTESIAN_POINT('Ctrl Pts',(81.7693168290942,-9.6036217342678,140.));
#131411=CARTESIAN_POINT('Ctrl Pts',(81.7525581651765,-9.6695281026167,140.));
#131412=CARTESIAN_POINT('Ctrl Pts',(81.7320180024232,-9.73447972793787,
140.));
#131413=CARTESIAN_POINT('Ctrl Pts',(81.7240899589877,-9.75954960264804,
140.));
#131414=CARTESIAN_POINT('Ctrl Pts',(81.7155979986156,-9.78447719355442,
140.));
#131415=CARTESIAN_POINT('Ctrl Pts',(81.7065542014754,-9.80924991088,140.));
#131416=CARTESIAN_POINT('Ctrl Pts',(81.702587541701,-9.82011536261413,140.));
#131417=CARTESIAN_POINT('Ctrl Pts',(81.6985148256868,-9.83095044867854,
140.));
#131418=CARTESIAN_POINT('Ctrl Pts',(81.6943421550071,-9.84174157738441,
140.));
#131419=CARTESIAN_POINT('Ctrl Pts',(81.6692401550965,-9.90665897264566,
140.));
#131420=CARTESIAN_POINT('Ctrl Pts',(81.6404827620673,-9.97010366580973,
140.));
#131421=CARTESIAN_POINT('Ctrl Pts',(81.6083781064462,-10.0318601884806,
140.));
#131422=CARTESIAN_POINT('Ctrl Pts',(81.575580286364,-10.0949500824628,140.));
#131423=CARTESIAN_POINT('Ctrl Pts',(81.5392887976022,-10.1562789155961,
140.));
#131424=CARTESIAN_POINT('Ctrl Pts',(81.499777343564,-10.21561337491,140.));
#131425=CARTESIAN_POINT('Ctrl Pts',(81.4596177776799,-10.2759211055673,
140.));
#131426=CARTESIAN_POINT('Ctrl Pts',(81.416131326886,-10.3341694205845,140.));
#131427=CARTESIAN_POINT('Ctrl Pts',(81.3695549575856,-10.3900965447165,
140.));
#131428=CARTESIAN_POINT('Ctrl Pts',(81.3583695251126,-10.4035275845288,
140.));
#131429=CARTESIAN_POINT('Ctrl Pts',(81.3470056786722,-10.4168246423396,
140.));
#131430=CARTESIAN_POINT('Ctrl Pts',(81.3354663202672,-10.4299838569706,
140.));
#131431=CARTESIAN_POINT('Ctrl Pts',(81.3227851686387,-10.444445145908,140.));
#131432=CARTESIAN_POINT('Ctrl Pts',(81.3098876232902,-10.4587445299804,
140.));
#131433=CARTESIAN_POINT('Ctrl Pts',(81.2968013238845,-10.4728515285403,
140.));
#131434=CARTESIAN_POINT('Ctrl Pts',(81.2459377457121,-10.527682340658,140.));
#131435=CARTESIAN_POINT('Ctrl Pts',(81.1921776876492,-10.5796680480248,
140.));
#131436=CARTESIAN_POINT('Ctrl Pts',(81.1358057830487,-10.6285450378629,
140.));
#131437=CARTESIAN_POINT('Ctrl Pts',(81.0936523916007,-10.6650939339847,
140.));
#131438=CARTESIAN_POINT('Ctrl Pts',(81.0500373919693,-10.6999043465923,
140.));
#131439=CARTESIAN_POINT('Ctrl Pts',(81.0050634114518,-10.7328563054907,
140.));
#131440=CARTESIAN_POINT('Ctrl Pts',(80.9910001257159,-10.7431603259091,
140.));
#131441=CARTESIAN_POINT('Ctrl Pts',(80.9768038659581,-10.7532825494193,
140.));
#131442=CARTESIAN_POINT('Ctrl Pts',(80.9624775285841,-10.7632190809483,
140.));
#131443=CARTESIAN_POINT('Ctrl Pts',(80.948691008792,-10.7727812031442,140.));
#131444=CARTESIAN_POINT('Ctrl Pts',(80.9347910747477,-10.782166414048,140.));
#131445=CARTESIAN_POINT('Ctrl Pts',(80.9207856707492,-10.7913685089582,
140.));
#131446=CARTESIAN_POINT('Ctrl Pts',(80.8578389347226,-10.8327269616862,
140.));
#131447=CARTESIAN_POINT('Ctrl Pts',(80.7927341134844,-10.8704103298825,
140.));
#131448=CARTESIAN_POINT('Ctrl Pts',(80.7257321767826,-10.9041397537238,
140.));
#131449=CARTESIAN_POINT('Ctrl Pts',(80.6745101487068,-10.9299254187363,
140.));
#131450=CARTESIAN_POINT('Ctrl Pts',(80.6221783994731,-10.9533998385397,
140.));
#131451=CARTESIAN_POINT('Ctrl Pts',(80.56883966131,-10.9744231685942,140.));
#131452=CARTESIAN_POINT('Ctrl Pts',(80.5565365876157,-10.9792723942765,
140.));
#131453=CARTESIAN_POINT('Ctrl Pts',(80.5441798951046,-10.9839911471849,
140.));
#131454=CARTESIAN_POINT('Ctrl Pts',(80.5317714570928,-10.98857999513,140.));
#131455=CARTESIAN_POINT('Ctrl Pts',(79.4691328777287,-10.9877838235895,
139.9984406031));
#131456=CARTESIAN_POINT('Ctrl Pts',(78.8081758496214,-10.811265456103,139.961396230436));
#131457=CARTESIAN_POINT('Ctrl Pts',(77.6877526904063,-9.74920906242341,
139.887307485108));
#131458=CARTESIAN_POINT('Ctrl Pts',(78.1161488323421,-7.46000016524759,
139.776174367117));
#131459=CARTESIAN_POINT('Ctrl Pts',(80.2721800425073,-6.58386568048153,
139.665041249125));
#131460=CARTESIAN_POINT('Ctrl Pts',(82.1774278168464,-7.91731817278388,
139.553908131134));
#131461=CARTESIAN_POINT('Ctrl Pts',(82.0906258630199,-10.2425367543248,
139.442775013142));
#131462=CARTESIAN_POINT('Ctrl Pts',(80.0900009463851,-11.4301197324817,
139.331641895151));
#131463=CARTESIAN_POINT('Ctrl Pts',(78.0071991588717,-10.3937654044698,
139.220508777159));
#131464=CARTESIAN_POINT('Ctrl Pts',(77.7481915217547,-8.0816824054986,139.109375659168));
#131465=CARTESIAN_POINT('Ctrl Pts',(79.550174388928,-6.61012857285443,138.998242541176));
#131466=CARTESIAN_POINT('Ctrl Pts',(81.763832497857,-7.32585529210686,138.887109423184));
#131467=CARTESIAN_POINT('Ctrl Pts',(82.3631728604374,-9.57383680047761,
138.775976305193));
#131468=CARTESIAN_POINT('Ctrl Pts',(80.7996389409501,-11.2966145820648,
138.664843187201));
#131469=CARTESIAN_POINT('Ctrl Pts',(78.5042466623318,-10.9174430919909,
138.55371006921));
#131470=CARTESIAN_POINT('Ctrl Pts',(77.5778254035081,-8.78335085114467,
138.442576951218));
#131471=CARTESIAN_POINT('Ctrl Pts',(78.8682743104211,-6.84754510512543,
138.331443833227));
#131472=CARTESIAN_POINT('Ctrl Pts',(81.1945228001823,-6.88175047275135,
138.220310715235));
#131473=CARTESIAN_POINT('Ctrl Pts',(82.4274971600873,-8.85466134058638,
138.109177597244));
#131474=CARTESIAN_POINT('Ctrl Pts',(81.4387304989914,-10.9605917920548,
137.998044479252));
#131475=CARTESIAN_POINT('Ctrl Pts',(79.1331810938808,-11.2721115054034,
137.88691136126));
#131476=CARTESIAN_POINT('Ctrl Pts',(77.6209784514413,-9.50410532093426,
137.775778243269));
#131477=CARTESIAN_POINT('Ctrl Pts',(78.286149976356,-7.27472211446641,137.664645125277));
#131478=CARTESIAN_POINT('Ctrl Pts',(80.5199044951167,-6.62438113065896,
137.553512007286));
#131479=CARTESIAN_POINT('Ctrl Pts',(82.2778219587944,-8.1483000416988,137.442378889294));
#131480=CARTESIAN_POINT('Ctrl Pts',(81.9509871105632,-10.4517282760942,
137.331245771303));
#131481=CARTESIAN_POINT('Ctrl Pts',(79.8385320691397,-11.4264776532609,
137.220112653311));
#131482=CARTESIAN_POINT('Ctrl Pts',(77.8738588331112,-10.1804191766788,
137.10897953532));
#131483=CARTESIAN_POINT('Ctrl Pts',(77.8551136772396,-7.85399460887872,
136.997846417328));
#131484=CARTESIAN_POINT('Ctrl Pts',(79.799452905803,-6.57643928130455,136.886713299336));
#131485=CARTESIAN_POINT('Ctrl Pts',(81.9273407284608,-7.51702211393059,
136.775580181345));
#131486=CARTESIAN_POINT('Ctrl Pts',(82.2912504570253,-9.81488467731359,
136.664447063353));
#131487=CARTESIAN_POINT('Ctrl Pts',(80.5581175845882,-11.366932710478,136.553313945362));
#131488=CARTESIAN_POINT('Ctrl Pts',(78.3141735314383,-10.7526707654457,
136.44218082737));
#131489=CARTESIAN_POINT('Ctrl Pts',(77.6131642158011,-8.5342955514302,136.331047709378));
#131490=CARTESIAN_POINT('Ctrl Pts',(79.0966809548029,-6.74215137869336,
136.219914591387));
#131491=CARTESIAN_POINT('Ctrl Pts',(81.4069508382607,-7.01647913223252,
136.108781473395));
#131492=CARTESIAN_POINT('Ctrl Pts',(82.4295239374967,-9.10620325457287,
135.997648355404));
#131493=CARTESIAN_POINT('Ctrl Pts',(81.2285011040056,-11.0987259782088,
135.886515237412));
#131494=CARTESIAN_POINT('Ctrl Pts',(78.9031057067962,-11.1704120815385,
135.775382119421));
#131495=CARTESIAN_POINT('Ctrl Pts',(77.5816311400657,-9.25565162125707,
135.664249001429));
#131496=CARTESIAN_POINT('Ctrl Pts',(78.4735429400179,-7.10690873485139,
135.553115883438));
#131497=CARTESIAN_POINT('Ctrl Pts',(80.76252832203,-6.69079748565583,135.441982765446));
#131498=CARTESIAN_POINT('Ctrl Pts',(82.3536177708982,-8.38815926691335,
135.330849647455));
#131499=CARTESIAN_POINT('Ctrl Pts',(81.7905835983475,-10.6455017689083,
135.219716529463));
#131500=CARTESIAN_POINT('Ctrl Pts',(79.5887368399055,-11.3968162856799,
135.108583411471));
#131501=CARTESIAN_POINT('Ctrl Pts',(77.7632943127424,-9.95447020002752,
134.99745029348));
#131502=CARTESIAN_POINT('Ctrl Pts',(77.9849728664353,-7.63855541972894,
134.886317175488));
#131503=CARTESIAN_POINT('Ctrl Pts',(80.0508835634619,-6.56868830523093,
134.775184057497));
#131504=CARTESIAN_POINT('Ctrl Pts',(82.0702236204505,-7.72405334928139,
134.664050939505));
#131505=CARTESIAN_POINT('Ctrl Pts',(82.1948135367953,-10.0472149888403,
134.552917821514));
#131506=CARTESIAN_POINT('Ctrl Pts',(80.3106237172459,-11.4119242526323,
134.441784703522));
#131507=CARTESIAN_POINT('Ctrl Pts',(78.1421388456428,-10.5691455080017,
134.33065158553));
#131508=CARTESIAN_POINT('Ctrl Pts',(77.6740416272099,-8.2902230334826,134.219518467539));
#131509=CARTESIAN_POINT('Ctrl Pts',(79.3347530603838,-6.6609163752694,134.108385349547));
#131510=CARTESIAN_POINT('Ctrl Pts',(81.6043246765592,-7.17243111584399,
133.997252231556));
#131511=CARTESIAN_POINT('Ctrl Pts',(82.4055552031433,-9.35660883160848,
133.886119113564));
#131512=CARTESIAN_POINT('Ctrl Pts',(81.0051269260808,-11.2144041086981,
133.774985995573));
#131513=CARTESIAN_POINT('Ctrl Pts',(78.6847669248588,-11.0454895874108,
133.663852877581));
#131514=CARTESIAN_POINT('Ctrl Pts',(77.5681600010754,-9.00446248603955,
133.55271975959));
#131515=CARTESIAN_POINT('Ctrl Pts',(78.6772687605974,-6.95935114180318,
133.441586641598));
#131516=CARTESIAN_POINT('Ctrl Pts',(80.996993212615,-6.78192195174491,133.330453523606));
#131517=CARTESIAN_POINT('Ctrl Pts',(82.4042302351769,-8.63456509415099,
133.219320405615));
#131518=CARTESIAN_POINT('Ctrl Pts',(81.611021116925,-10.8216686457678,133.108187287623));
#131519=CARTESIAN_POINT('Ctrl Pts',(79.3433420632901,-11.3415093525987,
132.997054169632));
#131520=CARTESIAN_POINT('Ctrl Pts',(77.6766621991367,-9.71830853902125,
132.88592105164));
#131521=CARTESIAN_POINT('Ctrl Pts',(78.1363925360183,-7.43768347818297,
132.774787933649));
#131522=CARTESIAN_POINT('Ctrl Pts',(80.3017697748106,-6.58695199029069,
132.663654815657));
#131523=CARTESIAN_POINT('Ctrl Pts',(82.1909554381543,-7.94473701752852,
132.552521697666));
#131524=CARTESIAN_POINT('Ctrl Pts',(82.0748924493326,-10.2683402610705,
132.441388579674));
#131525=CARTESIAN_POINT('Ctrl Pts',(80.0598062239121,-11.4311085762945,
132.330255461682));
#131526=CARTESIAN_POINT('Ctrl Pts',(77.9899829884147,-10.3688306349928,
132.219122343691));
#131527=CARTESIAN_POINT('Ctrl Pts',(77.7598064354237,-8.05374501989655,
132.107989225699));
#131528=CARTESIAN_POINT('Ctrl Pts',(79.5799432058827,-6.60470920682474,
131.996856107708));
#131529=CARTESIAN_POINT('Ctrl Pts',(81.7845324876121,-7.34793780539253,
131.885722989716));
#131530=CARTESIAN_POINT('Ctrl Pts',(82.3558473981236,-9.6031987490021,131.774589871725));
#131531=CARTESIAN_POINT('Ctrl Pts',(80.7709980447065,-11.3063884558481,
131.663456753733));
#131532=CARTESIAN_POINT('Ctrl Pts',(78.4805009344145,-10.8986806693481,
131.552323635741));
#131533=CARTESIAN_POINT('Ctrl Pts',(77.580709176199,-8.75322560289489,131.44119051775));
#131534=CARTESIAN_POINT('Ctrl Pts',(78.8951476015647,-6.83362817766481,
131.330057399758));
#131535=CARTESIAN_POINT('Ctrl Pts',(81.2207904300182,-6.89677951170404,
131.218924281767));
#131536=CARTESIAN_POINT('Ctrl Pts',(82.4291178040635,-8.8848810187796,131.107791163775));
#131537=CARTESIAN_POINT('Ctrl Pts',(81.4142209608452,-10.9783439481059,
130.996658045784));
#131538=CARTESIAN_POINT('Ctrl Pts',(79.1049734184687,-11.2611486300869,
130.885524927792));
#131539=CARTESIAN_POINT('Ctrl Pts',(77.6148894571761,-9.47446108619213,
130.774391809801));
#131540=CARTESIAN_POINT('Ctrl Pts',(78.3077524890248,-7.25352808503831,
130.663258691809));
#131541=CARTESIAN_POINT('Ctrl Pts',(80.5494271568789,-6.63103491390683,
130.552125573817));
#131542=CARTESIAN_POINT('Ctrl Pts',(82.2882442451662,-8.17671184547162,
130.440992455826));
#131543=CARTESIAN_POINT('Ctrl Pts',(81.9327705864848,-10.4758944710274,
130.329859337834));
#131544=CARTESIAN_POINT('Ctrl Pts',(79.8083482924002,-11.4242804460588,
130.218726219843));
#131545=CARTESIAN_POINT('Ctrl Pts',(77.8593350690433,-10.1538694154057,
130.107593101851));
#131546=CARTESIAN_POINT('Ctrl Pts',(77.8695387921742,-7.82739193084829,
129.99645998386));
#131547=CARTESIAN_POINT('Ctrl Pts',(79.8296323485855,-6.57413099141478,
129.885326865868));
#131548=CARTESIAN_POINT('Ctrl Pts',(81.9456369666873,-7.54112189936117,
129.774193747877));
#131549=CARTESIAN_POINT('Ctrl Pts',(82.2809510163317,-9.84333331972787,
129.663060629885));
#131550=CARTESIAN_POINT('Ctrl Pts',(80.5285815078084,-11.3736972816056,
129.551927511894));
#131551=CARTESIAN_POINT('Ctrl Pts',(78.2925712562624,-10.731551087784,129.440794393902));
#131552=CARTESIAN_POINT('Ctrl Pts',(77.6189850691365,-8.50463954136352,
129.32966127591));
#131553=CARTESIAN_POINT('Ctrl Pts',(79.1251740367243,-6.73106382404891,
129.218528157919));
#131554=CARTESIAN_POINT('Ctrl Pts',(81.4308588372317,-7.03418464412087,
129.107395039927));
#131555=CARTESIAN_POINT('Ctrl Pts',(82.4293842699421,-9.13633334838347,
128.996261921936));
#131556=CARTESIAN_POINT('Ctrl Pts',(81.1993089591602,-11.1142610176031,
128.885115666002));
#131557=CARTESIAN_POINT('Ctrl Pts',(79.65533995085,-11.1407368472887,128.811013782731));
#131558=CARTESIAN_POINT('Ctrl Pts',(79.0485528339274,-10.8242403017729,
128.773956272126));
#131559=CARTESIAN_POINT('Ctrl Pts',(79.5030640089439,-10.8607317781412,
140.074365003916));
#131560=CARTESIAN_POINT('Ctrl Pts',(78.884352994401,-10.6954958345189,140.037320631253));
#131561=CARTESIAN_POINT('Ctrl Pts',(77.835543283518,-9.70132229389272,139.963231885925));
#131562=CARTESIAN_POINT('Ctrl Pts',(78.2365578734717,-7.55843145675596,
139.852098767933));
#131563=CARTESIAN_POINT('Ctrl Pts',(80.2547832658959,-6.73829636038229,
139.740965649942));
#131564=CARTESIAN_POINT('Ctrl Pts',(82.0382544043942,-7.9865193299143,139.62983253195));
#131565=CARTESIAN_POINT('Ctrl Pts',(81.9570005215658,-10.1631182409492,
139.518699413959));
#131566=CARTESIAN_POINT('Ctrl Pts',(80.0842484072031,-11.2747951549134,
139.407566295967));
#131567=CARTESIAN_POINT('Ctrl Pts',(78.1345718741699,-10.3046808956759,
139.296433177976));
#131568=CARTESIAN_POINT('Ctrl Pts',(77.8921190805384,-8.14037798766803,
139.185300059984));
#131569=CARTESIAN_POINT('Ctrl Pts',(79.5789256360724,-6.76288062243545,
139.074166941992));
#131570=CARTESIAN_POINT('Ctrl Pts',(81.6510946216244,-7.4328606449979,138.963033824001));
#131571=CARTESIAN_POINT('Ctrl Pts',(82.2121272879242,-9.53715920083675,
138.851900706009));
#131572=CARTESIAN_POINT('Ctrl Pts',(80.7485288746228,-11.1498231770866,
138.740767588018));
#131573=CARTESIAN_POINT('Ctrl Pts',(78.5998498757103,-10.794886974984,138.629634470026));
#131574=CARTESIAN_POINT('Ctrl Pts',(77.7326421563487,-8.79719829128381,
138.518501352035));
#131575=CARTESIAN_POINT('Ctrl Pts',(78.9406101761429,-6.98512233756069,
138.407368234043));
#131576=CARTESIAN_POINT('Ctrl Pts',(81.1181731673415,-7.01714142020401,
138.296235116052));
#131577=CARTESIAN_POINT('Ctrl Pts',(82.2723402079837,-8.86395086882484,
138.18510199806));
#131578=CARTESIAN_POINT('Ctrl Pts',(81.3467719818848,-10.8352777641842,
138.073968880068));
#131579=CARTESIAN_POINT('Ctrl Pts',(79.1885850637436,-11.1268862496072,
137.962835762077));
#131580=CARTESIAN_POINT('Ctrl Pts',(77.7730370155179,-9.47188470851856,
137.851702644085));
#131581=CARTESIAN_POINT('Ctrl Pts',(78.3956931512785,-7.38499571752248,
137.740569526094));
#131582=CARTESIAN_POINT('Ctrl Pts',(80.4866740558917,-6.77622220762796,
137.629436408102));
#131583=CARTESIAN_POINT('Ctrl Pts',(82.1322317112042,-8.20273766239288,
137.518303290111));
#131584=CARTESIAN_POINT('Ctrl Pts',(81.8262869796441,-10.3589389874783,
137.407170172119));
#131585=CARTESIAN_POINT('Ctrl Pts',(79.8488525228262,-11.271385864394,137.296037054127));
#131586=CARTESIAN_POINT('Ctrl Pts',(78.0097541859958,-10.1049709971013,
137.184903936136));
#131587=CARTESIAN_POINT('Ctrl Pts',(77.9922071535657,-7.9272431821435,137.073770818144));
#131588=CARTESIAN_POINT('Ctrl Pts',(79.812271160094,-6.73134463012783,136.962637700153));
#131589=CARTESIAN_POINT('Ctrl Pts',(81.8041519898661,-7.61180876605229,
136.851504582161));
#131590=CARTESIAN_POINT('Ctrl Pts',(82.1448019077693,-9.76280015794658,
136.74037146417));
#131591=CARTESIAN_POINT('Ctrl Pts',(80.522444701108,-11.2156468217732,136.629238346178));
#131592=CARTESIAN_POINT('Ctrl Pts',(78.4219255407664,-10.6406463073006,
136.518105228187));
#131593=CARTESIAN_POINT('Ctrl Pts',(77.7657222379225,-8.56406171717871,
136.406972110195));
#131594=CARTESIAN_POINT('Ctrl Pts',(79.1544178832468,-6.88646500185769,
136.295838992204));
#131595=CARTESIAN_POINT('Ctrl Pts',(81.317023563612,-7.14325870476379,136.184705874212));
#131596=CARTESIAN_POINT('Ctrl Pts',(82.2742374410167,-9.09941512169513,
136.07357275622));
#131597=CARTESIAN_POINT('Ctrl Pts',(81.1499796992898,-10.9645829063101,
135.962439638229));
#131598=CARTESIAN_POINT('Ctrl Pts',(78.9732152740129,-11.0316870898403,
135.851306520237));
#131599=CARTESIAN_POINT('Ctrl Pts',(77.7362046438123,-9.23931128232413,
135.740173402246));
#131600=CARTESIAN_POINT('Ctrl Pts',(78.5711086257117,-7.22790837002455,
135.629040284254));
#131601=CARTESIAN_POINT('Ctrl Pts',(80.7137902339762,-6.8383934663254,135.517907166263));
#131602=CARTESIAN_POINT('Ctrl Pts',(82.2031829255959,-8.42726594224934,
135.406774048271));
#131603=CARTESIAN_POINT('Ctrl Pts',(81.6761358872752,-10.5403271704196,
135.29564093028));
#131604=CARTESIAN_POINT('Ctrl Pts',(79.6150233128547,-11.2436203455352,
135.184507812288));
#131605=CARTESIAN_POINT('Ctrl Pts',(77.9062565550443,-9.89346387238071,
135.073374694296));
#131606=CARTESIAN_POINT('Ctrl Pts',(78.1137662069962,-7.72557409682812,
134.962241576305));
#131607=CARTESIAN_POINT('Ctrl Pts',(80.0476312677441,-6.72408906877321,
134.851108458313));
#131608=CARTESIAN_POINT('Ctrl Pts',(81.9379023175039,-7.80560730395839,
134.739975340322));
#131609=CARTESIAN_POINT('Ctrl Pts',(82.0545288911924,-9.98028074539927,
134.62884222233));
#131610=CARTESIAN_POINT('Ctrl Pts',(80.2907697581922,-11.2577626651766,
134.517709104338));
#131611=CARTESIAN_POINT('Ctrl Pts',(78.2608866979087,-10.4688513291117,
134.406575986347));
#131612=CARTESIAN_POINT('Ctrl Pts',(77.8227085825314,-8.33558944321889,
134.295442868355));
#131613=CARTESIAN_POINT('Ctrl Pts',(79.3772732697765,-6.81042224983678,
134.184309750364));
#131614=CARTESIAN_POINT('Ctrl Pts',(81.5017819708075,-7.28924279434453,
134.073176632372));
#131615=CARTESIAN_POINT('Ctrl Pts',(82.251800702593,-9.3338156682156,133.962043514381));
#131616=CARTESIAN_POINT('Ctrl Pts',(80.9408828013534,-11.0728673036791,
133.850910396389));
#131617=CARTESIAN_POINT('Ctrl Pts',(78.768831927529,-10.9147491955534,133.739777278398));
#131618=CARTESIAN_POINT('Ctrl Pts',(77.7235945319332,-9.00417725986336,
133.628644160406));
#131619=CARTESIAN_POINT('Ctrl Pts',(78.7618130191583,-7.08978213153095,
133.517511042414));
#131620=CARTESIAN_POINT('Ctrl Pts',(80.9332689658142,-6.92369358186409,
133.406377924423));
#131621=CARTESIAN_POINT('Ctrl Pts',(82.2505604218487,-8.65792238869949,
133.295244806431));
#131622=CARTESIAN_POINT('Ctrl Pts',(81.508050398612,-10.7052340894407,133.18411168844));
#131623=CARTESIAN_POINT('Ctrl Pts',(79.3853132942805,-11.1918484341661,
133.072978570448));
#131624=CARTESIAN_POINT('Ctrl Pts',(77.8251616568562,-9.67239682162895,
132.961845452457));
#131625=CARTESIAN_POINT('Ctrl Pts',(78.2555076718805,-7.53754117265604,
132.850712334465));
#131626=CARTESIAN_POINT('Ctrl Pts',(80.2824817281482,-6.74118540428684,
132.739579216473));
#131627=CARTESIAN_POINT('Ctrl Pts',(82.0509173884428,-8.01218565999045,
132.628446098482));
#131628=CARTESIAN_POINT('Ctrl Pts',(81.9422727315119,-10.1872724796644,
132.51731298049));
#131629=CARTESIAN_POINT('Ctrl Pts',(80.0559836235928,-11.27572079536,132.406179862499));
#131630=CARTESIAN_POINT('Ctrl Pts',(78.1184560998653,-10.2813398676446,
132.295046744507));
#131631=CARTESIAN_POINT('Ctrl Pts',(77.9029916103919,-8.11422626001485,
132.183913626516));
#131632=CARTESIAN_POINT('Ctrl Pts',(79.6067917365245,-6.75780764293479,
132.072780508524));
#131633=CARTESIAN_POINT('Ctrl Pts',(81.6704715419352,-7.45353172287077,
131.961647390533));
#131634=CARTESIAN_POINT('Ctrl Pts',(82.2052700430089,-9.56464443843619,
131.850514272541));
#131635=CARTESIAN_POINT('Ctrl Pts',(80.7217186022169,-11.1589723397512,
131.73938115455));
#131636=CARTESIAN_POINT('Ctrl Pts',(78.5776218899472,-10.7773237794131,
131.628248036558));
#131637=CARTESIAN_POINT('Ctrl Pts',(77.7353416085845,-8.76899854135246,
131.517114918566));
#131638=CARTESIAN_POINT('Ctrl Pts',(78.9657658224566,-6.97209493041876,
131.405981800575));
#131639=CARTESIAN_POINT('Ctrl Pts',(81.142761864056,-7.03120985664177,131.294848682583));
#131640=CARTESIAN_POINT('Ctrl Pts',(82.2738572661827,-8.89223901307474,
131.183715564592));
#131641=CARTESIAN_POINT('Ctrl Pts',(81.3238290059157,-10.8518952657974,
131.0725824466));
#131642=CARTESIAN_POINT('Ctrl Pts',(79.16218032224,-11.1166240821426,130.961449328609));
#131643=CARTESIAN_POINT('Ctrl Pts',(77.767337208028,-9.44413522742874,130.850316210617));
#131644=CARTESIAN_POINT('Ctrl Pts',(78.4159149084603,-7.36515633479095,
130.739183092626));
#131645=CARTESIAN_POINT('Ctrl Pts',(80.5143097345124,-6.78245070480519,
130.628049974634));
#131646=CARTESIAN_POINT('Ctrl Pts',(82.1419878422397,-8.22933348510106,
130.516916856643));
#131647=CARTESIAN_POINT('Ctrl Pts',(81.8092347907504,-10.3815605655068,
130.405783738651));
#131648=CARTESIAN_POINT('Ctrl Pts',(79.8205979853371,-11.269329094832,130.294650620659));
#131649=CARTESIAN_POINT('Ctrl Pts',(77.9961587290761,-10.0801182017839,
130.183517502668));
#131650=CARTESIAN_POINT('Ctrl Pts',(78.0057102666526,-7.90234085231897,
130.072384384676));
#131651=CARTESIAN_POINT('Ctrl Pts',(79.840521640637,-6.72918387788704,129.961251266685));
#131652=CARTESIAN_POINT('Ctrl Pts',(81.8212787978642,-7.63436817923641,
129.850118148693));
#131653=CARTESIAN_POINT('Ctrl Pts',(82.1351607705549,-9.78943046470178,
129.738985030701));
#131654=CARTESIAN_POINT('Ctrl Pts',(80.4947964649098,-11.2219790256644,
129.62785191271));
#131655=CARTESIAN_POINT('Ctrl Pts',(78.4017040058978,-10.6208765240359,
129.516718794718));
#131656=CARTESIAN_POINT('Ctrl Pts',(77.7711710430936,-8.53630121340103,
129.405585676727));
#131657=CARTESIAN_POINT('Ctrl Pts',(79.1810897890947,-6.87608612412261,
129.294452558735));
#131658=CARTESIAN_POINT('Ctrl Pts',(81.3394034486423,-7.15983254354241,
129.183319440744));
#131659=CARTESIAN_POINT('Ctrl Pts',(82.2741067005136,-9.12761940747632,
129.072186322752));
#131660=CARTESIAN_POINT('Ctrl Pts',(81.1226534121246,-10.9791250014477,
128.961040066819));
#131661=CARTESIAN_POINT('Ctrl Pts',(79.6773693907263,-11.0039085906207,
128.886938183549));
#131662=CARTESIAN_POINT('Ctrl Pts',(79.1093659400363,-10.7076413743751,
128.849880672942));
#131663=CARTESIAN_POINT('Ctrl Pts',(79.5369951401592,-10.7336797326929,
140.150289404733));
#131664=CARTESIAN_POINT('Ctrl Pts',(78.9605301391807,-10.5797262129349,
140.113245032069));
#131665=CARTESIAN_POINT('Ctrl Pts',(77.9833338766298,-9.653435525362,140.039156286741));
#131666=CARTESIAN_POINT('Ctrl Pts',(78.3569669146011,-7.65686274826432,
139.92802316875));
#131667=CARTESIAN_POINT('Ctrl Pts',(80.2373864892844,-6.89272704028306,
139.816890050758));
#131668=CARTESIAN_POINT('Ctrl Pts',(81.8990809919417,-8.05572048704471,
139.705756932767));
#131669=CARTESIAN_POINT('Ctrl Pts',(81.8233751801121,-10.0836997275735,
139.594623814775));
#131670=CARTESIAN_POINT('Ctrl Pts',(80.0784958680211,-11.1194705773451,
139.483490696784));
#131671=CARTESIAN_POINT('Ctrl Pts',(78.2619445894682,-10.2155963868819,
139.372357578792));
#131672=CARTESIAN_POINT('Ctrl Pts',(78.036046639322,-8.19907356983747,139.261224460801));
#131673=CARTESIAN_POINT('Ctrl Pts',(79.6076768832169,-6.91563267201647,
139.150091342809));
#131674=CARTESIAN_POINT('Ctrl Pts',(81.5383567453918,-7.53986599788894,
139.038958224817));
#131675=CARTESIAN_POINT('Ctrl Pts',(82.061081715411,-9.50048160119588,138.927825106826));
#131676=CARTESIAN_POINT('Ctrl Pts',(80.6974188082955,-11.0030317721083,
138.816691988834));
#131677=CARTESIAN_POINT('Ctrl Pts',(78.6954530890887,-10.6723308579772,
138.705558870843));
#131678=CARTESIAN_POINT('Ctrl Pts',(77.8874589091894,-8.81104573142295,
138.594425752851));
#131679=CARTESIAN_POINT('Ctrl Pts',(79.0129460418649,-7.12269956999594,
138.48329263486));
#131680=CARTESIAN_POINT('Ctrl Pts',(81.0418235345008,-7.15253236765667,
138.372159516868));
#131681=CARTESIAN_POINT('Ctrl Pts',(82.11718325588,-8.87324039706331,138.261026398876));
#131682=CARTESIAN_POINT('Ctrl Pts',(81.2548134647783,-10.7099637363138,
138.149893280885));
#131683=CARTESIAN_POINT('Ctrl Pts',(79.2439890336062,-10.9816609938111,
138.038760162893));
#131684=CARTESIAN_POINT('Ctrl Pts',(77.9250955795947,-9.43966409610286,
137.927627044902));
#131685=CARTESIAN_POINT('Ctrl Pts',(78.505236326201,-7.49526932057854,137.81649392691));
#131686=CARTESIAN_POINT('Ctrl Pts',(80.4534436166667,-6.92806328459693,
137.705360808919));
#131687=CARTESIAN_POINT('Ctrl Pts',(81.9866414636141,-8.25717528308697,
137.594227690927));
#131688=CARTESIAN_POINT('Ctrl Pts',(81.7015868487251,-10.2661496988625,
137.483094572936));
#131689=CARTESIAN_POINT('Ctrl Pts',(79.8591729765127,-11.116294075527,137.371961454944));
#131690=CARTESIAN_POINT('Ctrl Pts',(78.1456495388805,-10.0295228175239,
137.260828336952));
#131691=CARTESIAN_POINT('Ctrl Pts',(78.1293006298919,-8.00049175540828,
137.149695218961));
#131692=CARTESIAN_POINT('Ctrl Pts',(79.8250894143851,-6.88624997895113,
137.038562100969));
#131693=CARTESIAN_POINT('Ctrl Pts',(81.6809632512715,-7.70659541817398,
136.927428982978));
#131694=CARTESIAN_POINT('Ctrl Pts',(81.9983533585131,-9.71071563857958,
136.816295864986));
#131695=CARTESIAN_POINT('Ctrl Pts',(80.4867718176279,-11.0643609330684,
136.705162746995));
#131696=CARTESIAN_POINT('Ctrl Pts',(78.5296775500945,-10.5286218491554,
136.594029629003));
#131697=CARTESIAN_POINT('Ctrl Pts',(77.9182802600438,-8.59382788292722,
136.482896511012));
#131698=CARTESIAN_POINT('Ctrl Pts',(79.2121548116908,-7.03077862502201,
136.37176339302));
#131699=CARTESIAN_POINT('Ctrl Pts',(81.2270962889633,-7.27003827729506,
136.260630275028));
#131700=CARTESIAN_POINT('Ctrl Pts',(82.1189509445369,-9.09262698881739,
136.149497157037));
#131701=CARTESIAN_POINT('Ctrl Pts',(81.071458294574,-10.8304398344114,136.038364039045));
#131702=CARTESIAN_POINT('Ctrl Pts',(79.0433248412296,-10.8929620981422,
135.927230921054));
#131703=CARTESIAN_POINT('Ctrl Pts',(77.8907781475588,-9.22297094339117,
135.816097803062));
#131704=CARTESIAN_POINT('Ctrl Pts',(78.6686743114057,-7.34890800519772,
135.704964685071));
#131705=CARTESIAN_POINT('Ctrl Pts',(80.6650521459222,-6.98598944699497,
135.593831567079));
#131706=CARTESIAN_POINT('Ctrl Pts',(82.0527480802936,-8.46637261758534,
135.482698449088));
#131707=CARTESIAN_POINT('Ctrl Pts',(81.5616881762029,-10.4351525719307,
135.371565331096));
#131708=CARTESIAN_POINT('Ctrl Pts',(79.6413097858039,-11.0904244053903,
135.260432213105));
#131709=CARTESIAN_POINT('Ctrl Pts',(78.0492187973462,-9.83245754473388,
135.149299095113));
#131710=CARTESIAN_POINT('Ctrl Pts',(78.2425595475572,-7.81259277392733,
135.038165977121));
#131711=CARTESIAN_POINT('Ctrl Pts',(80.0443789720261,-6.87948983231548,
134.92703285913));
#131712=CARTESIAN_POINT('Ctrl Pts',(81.8055810145572,-7.8871612586354,134.815899741138));
#131713=CARTESIAN_POINT('Ctrl Pts',(81.9142442455895,-9.91334650195824,
134.704766623147));
#131714=CARTESIAN_POINT('Ctrl Pts',(80.2709157991388,-11.1036010777208,
134.593633505155));
#131715=CARTESIAN_POINT('Ctrl Pts',(78.3796345501745,-10.3685571502218,
134.482500387163));
#131716=CARTESIAN_POINT('Ctrl Pts',(77.971375537853,-8.38095585295519,134.371367269172));
#131717=CARTESIAN_POINT('Ctrl Pts',(79.4197934791693,-6.95992812440418,
134.26023415118));
#131718=CARTESIAN_POINT('Ctrl Pts',(81.3992392650559,-7.40605447284507,
134.149101033189));
#131719=CARTESIAN_POINT('Ctrl Pts',(82.0980462020426,-9.31102250482272,
134.037967915197));
#131720=CARTESIAN_POINT('Ctrl Pts',(80.876638676626,-10.9313304986601,133.926834797206));
#131721=CARTESIAN_POINT('Ctrl Pts',(78.8528969301993,-10.7840088036961,
133.815701679214));
#131722=CARTESIAN_POINT('Ctrl Pts',(77.879029062791,-9.00389203368715,133.704568561223));
#131723=CARTESIAN_POINT('Ctrl Pts',(78.846357277719,-7.22021312125874,133.593435443231));
#131724=CARTESIAN_POINT('Ctrl Pts',(80.8695447190136,-7.06546521198324,
133.482302325239));
#131725=CARTESIAN_POINT('Ctrl Pts',(82.0968906085204,-8.68127968324799,
133.371169207248));
#131726=CARTESIAN_POINT('Ctrl Pts',(81.4050796802991,-10.5887995331135,
133.260036089256));
#131727=CARTESIAN_POINT('Ctrl Pts',(79.4272845252708,-11.0421875157334,
133.148902971265));
#131728=CARTESIAN_POINT('Ctrl Pts',(77.973661114576,-9.62648510423664,133.037769853273));
#131729=CARTESIAN_POINT('Ctrl Pts',(78.3746228077427,-7.63739886712913,
132.926636735282));
#131730=CARTESIAN_POINT('Ctrl Pts',(80.2631936814858,-6.89541881828299,
132.81550361729));
#131731=CARTESIAN_POINT('Ctrl Pts',(81.9108793387313,-8.07963430245237,
132.704370499299));
#131732=CARTESIAN_POINT('Ctrl Pts',(81.8096530136912,-10.1062046982582,
132.593237381307));
#131733=CARTESIAN_POINT('Ctrl Pts',(80.0521610232735,-11.1203330144254,
132.482104263315));
#131734=CARTESIAN_POINT('Ctrl Pts',(78.246929211316,-10.1938491002965,132.370971145324));
#131735=CARTESIAN_POINT('Ctrl Pts',(78.04617678536,-8.17470750013315,132.259838027332));
#131736=CARTESIAN_POINT('Ctrl Pts',(79.6336402671663,-6.91090607904484,
132.148704909341));
#131737=CARTESIAN_POINT('Ctrl Pts',(81.5564105962581,-7.55912564034901,
132.037571791349));
#131738=CARTESIAN_POINT('Ctrl Pts',(82.0546926878945,-9.52609012787027,
131.926438673358));
#131739=CARTESIAN_POINT('Ctrl Pts',(80.6724391597271,-11.0115562236542,
131.815305555366));
#131740=CARTESIAN_POINT('Ctrl Pts',(78.6747428454798,-10.6559668894782,
131.704172437375));
#131741=CARTESIAN_POINT('Ctrl Pts',(77.8899740409698,-8.78477147981007,
131.593039319383));
#131742=CARTESIAN_POINT('Ctrl Pts',(79.0363840433487,-7.1105616831727,131.481906201391));
#131743=CARTESIAN_POINT('Ctrl Pts',(81.0647332980937,-7.16564020157951,
131.3707730834));
#131744=CARTESIAN_POINT('Ctrl Pts',(82.118596728302,-8.8995970073699,131.259639965408));
#131745=CARTESIAN_POINT('Ctrl Pts',(81.2334370509863,-10.7254465834888,
131.148506847417));
#131746=CARTESIAN_POINT('Ctrl Pts',(79.2193872260113,-10.9720995341984,
131.037373729425));
#131747=CARTESIAN_POINT('Ctrl Pts',(77.9197849588799,-9.41380936866533,
130.926240611434));
#131748=CARTESIAN_POINT('Ctrl Pts',(78.5240773278958,-7.47678458454359,
130.815107493442));
#131749=CARTESIAN_POINT('Ctrl Pts',(80.4791923121458,-6.93386649570354,
130.70397437545));
#131750=CARTESIAN_POINT('Ctrl Pts',(81.9957314393132,-8.28195512473053,
130.592841257459));
#131751=CARTESIAN_POINT('Ctrl Pts',(81.6856989950159,-10.2872266599862,
130.481708139467));
#131752=CARTESIAN_POINT('Ctrl Pts',(79.8328476782742,-11.1143777436051,
130.370575021476));
#131753=CARTESIAN_POINT('Ctrl Pts',(78.1329823891089,-10.0063669881622,
130.259441903484));
#131754=CARTESIAN_POINT('Ctrl Pts',(78.141881741131,-7.97728977378966,130.148308785492));
#131755=CARTESIAN_POINT('Ctrl Pts',(79.8514109326885,-6.88423676435929,
130.037175667501));
#131756=CARTESIAN_POINT('Ctrl Pts',(81.6969206290413,-7.72761445911164,
129.926042549509));
#131757=CARTESIAN_POINT('Ctrl Pts',(81.9893705247781,-9.7355276096757,129.814909431518));
#131758=CARTESIAN_POINT('Ctrl Pts',(80.4610114220111,-11.0702607697232,
129.703776313526));
#131759=CARTESIAN_POINT('Ctrl Pts',(78.5108367555332,-10.5102019602878,
129.592643195535));
#131760=CARTESIAN_POINT('Ctrl Pts',(77.9233570170507,-8.56796288543854,
129.481510077543));
#131761=CARTESIAN_POINT('Ctrl Pts',(79.2370055414648,-7.02110842419632,
129.370376959552));
#131762=CARTESIAN_POINT('Ctrl Pts',(81.247948060053,-7.28548044296393,129.25924384156));
#131763=CARTESIAN_POINT('Ctrl Pts',(82.1188291310851,-9.11890546656919,
129.148110723569));
#131764=CARTESIAN_POINT('Ctrl Pts',(81.045997865089,-10.8439889852923,129.036964467635));
#131765=CARTESIAN_POINT('Ctrl Pts',(79.6993988306026,-10.8670803339528,
128.962862584365));
#131766=CARTESIAN_POINT('Ctrl Pts',(79.1701790461452,-10.5910424469771,
128.92580507376));
#131767=CARTESIAN_POINT('Ctrl Pts',(79.5709262713745,-10.6066276872446,
140.22621380555));
#131768=CARTESIAN_POINT('Ctrl Pts',(79.0367072839604,-10.4639565913509,
140.189169432887));
#131769=CARTESIAN_POINT('Ctrl Pts',(78.1311244697415,-9.6055487568313,140.115080687559));
#131770=CARTESIAN_POINT('Ctrl Pts',(78.4773759557306,-7.75529403977268,
140.003947569567));
#131771=CARTESIAN_POINT('Ctrl Pts',(80.2199897126731,-7.04715772018383,
139.892814451576));
#131772=CARTESIAN_POINT('Ctrl Pts',(81.7599075794896,-8.12492164417513,
139.781681333584));
#131773=CARTESIAN_POINT('Ctrl Pts',(81.689749838658,-10.0042812141978,139.670548215593));
#131774=CARTESIAN_POINT('Ctrl Pts',(80.0727433288392,-10.9641459997769,
139.559415097601));
#131775=CARTESIAN_POINT('Ctrl Pts',(78.3893173047664,-10.126511878088,139.44828197961));
#131776=CARTESIAN_POINT('Ctrl Pts',(78.1799741981056,-8.25776915200689,
139.337148861618));
#131777=CARTESIAN_POINT('Ctrl Pts',(79.6364281303614,-7.0683847215975,139.226015743626));
#131778=CARTESIAN_POINT('Ctrl Pts',(81.4256188691593,-7.64687135077996,
139.114882625635));
#131779=CARTESIAN_POINT('Ctrl Pts',(81.9100361428979,-9.46380400155503,
139.003749507643));
#131780=CARTESIAN_POINT('Ctrl Pts',(80.6463087419684,-10.8562403671301,
138.892616389652));
#131781=CARTESIAN_POINT('Ctrl Pts',(78.7910563024672,-10.5497747409704,
138.78148327166));
#131782=CARTESIAN_POINT('Ctrl Pts',(78.04227566203,-8.82489317156209,138.670350153669));
#131783=CARTESIAN_POINT('Ctrl Pts',(79.0852819075869,-7.26027680243122,
138.559217035677));
#131784=CARTESIAN_POINT('Ctrl Pts',(80.9654739016601,-7.28792331510932,
138.448083917685));
#131785=CARTESIAN_POINT('Ctrl Pts',(81.9620263037764,-8.88252992530179,
138.336950799694));
#131786=CARTESIAN_POINT('Ctrl Pts',(81.1628549476717,-10.5846497084434,
138.225817681702));
#131787=CARTESIAN_POINT('Ctrl Pts',(79.2993930034689,-10.836435738015,138.114684563711));
#131788=CARTESIAN_POINT('Ctrl Pts',(78.0771541436715,-9.40744348368716,
138.003551445719));
#131789=CARTESIAN_POINT('Ctrl Pts',(78.6147795011235,-7.6055429236346,137.892418327728));
#131790=CARTESIAN_POINT('Ctrl Pts',(80.4202131774415,-7.07990436156593,
137.781285209736));
#131791=CARTESIAN_POINT('Ctrl Pts',(81.8410512160243,-8.31161290378106,
137.670152091745));
#131792=CARTESIAN_POINT('Ctrl Pts',(81.5768867178061,-10.1733604102468,
137.559018973753));
#131793=CARTESIAN_POINT('Ctrl Pts',(79.8694934301991,-10.9612022866599,
137.447885855761));
#131794=CARTESIAN_POINT('Ctrl Pts',(78.281544891765,-9.9540746379463,137.33675273777));
#131795=CARTESIAN_POINT('Ctrl Pts',(78.266394106218,-8.07374032867307,137.225619619778));
#131796=CARTESIAN_POINT('Ctrl Pts',(79.8379076686761,-7.04115532777441,
137.114486501787));
#131797=CARTESIAN_POINT('Ctrl Pts',(81.5577745126769,-7.80138207029568,
137.003353383795));
#131798=CARTESIAN_POINT('Ctrl Pts',(81.851904809257,-9.65863111921257,136.892220265804));
#131799=CARTESIAN_POINT('Ctrl Pts',(80.4510989341479,-10.9130750443636,
136.781087147812));
#131800=CARTESIAN_POINT('Ctrl Pts',(78.6374295594225,-10.4165973910102,
136.669954029821));
#131801=CARTESIAN_POINT('Ctrl Pts',(78.0708382821652,-8.62359404867573,
136.558820911829));
#131802=CARTESIAN_POINT('Ctrl Pts',(79.2698917401348,-7.17509224818634,
136.447687793838));
#131803=CARTESIAN_POINT('Ctrl Pts',(81.1371690143145,-7.39681784982634,
136.336554675846));
#131804=CARTESIAN_POINT('Ctrl Pts',(81.9636644480571,-9.08583885593964,
136.225421557854));
#131805=CARTESIAN_POINT('Ctrl Pts',(80.9929368898583,-10.6962967625126,
136.114288439863));
#131806=CARTESIAN_POINT('Ctrl Pts',(79.1134344084462,-10.7542371064441,
136.003155321871));
#131807=CARTESIAN_POINT('Ctrl Pts',(78.0453516513057,-9.20663060445822,
135.89202220388));
#131808=CARTESIAN_POINT('Ctrl Pts',(78.7662399970995,-7.46990764037088,
135.780889085888));
#131809=CARTESIAN_POINT('Ctrl Pts',(80.6163140578685,-7.13358542766454,
135.669755967897));
#131810=CARTESIAN_POINT('Ctrl Pts',(81.9023132349912,-8.50547929292133,
135.558622849905));
#131811=CARTESIAN_POINT('Ctrl Pts',(81.4472404651308,-10.3299779734419,
135.447489731913));
#131812=CARTESIAN_POINT('Ctrl Pts',(79.6675962587529,-10.9372284652455,
135.336356613922));
#131813=CARTESIAN_POINT('Ctrl Pts',(78.1921810396483,-9.77145121708706,
135.22522349593));
#131814=CARTESIAN_POINT('Ctrl Pts',(78.3713528881184,-7.89961145102653,
135.114090377939));
#131815=CARTESIAN_POINT('Ctrl Pts',(80.0411266763082,-7.03489059585776,
135.002957259947));
#131816=CARTESIAN_POINT('Ctrl Pts',(81.6732597116106,-7.96871521331242,
134.891824141956));
#131817=CARTESIAN_POINT('Ctrl Pts',(81.7739595999865,-9.8464122585172,134.780691023964));
#131818=CARTESIAN_POINT('Ctrl Pts',(80.2510618400852,-10.9494394902652,
134.669557905973));
#131819=CARTESIAN_POINT('Ctrl Pts',(78.4983824024403,-10.2682629713319,
134.558424787981));
#131820=CARTESIAN_POINT('Ctrl Pts',(78.1200424931747,-8.42632226269147,
134.44729166999));
#131821=CARTESIAN_POINT('Ctrl Pts',(79.462313688562,-7.10943399897156,134.336158551998));
#131822=CARTESIAN_POINT('Ctrl Pts',(81.2966965593045,-7.5228661513456,134.225025434006));
#131823=CARTESIAN_POINT('Ctrl Pts',(81.9442917014921,-9.28822934142986,
134.113892316015));
#131824=CARTESIAN_POINT('Ctrl Pts',(80.8123945518987,-10.7897936936412,
134.002759198023));
#131825=CARTESIAN_POINT('Ctrl Pts',(78.9369619328696,-10.6532684118388,
133.891626080032));
#131826=CARTESIAN_POINT('Ctrl Pts',(78.0344635936487,-9.00360680751095,
133.78049296204));
#131827=CARTESIAN_POINT('Ctrl Pts',(78.9309015362798,-7.35064411098652,
133.669359844049));
#131828=CARTESIAN_POINT('Ctrl Pts',(80.805820472213,-7.20723684210242,133.558226726057));
#131829=CARTESIAN_POINT('Ctrl Pts',(81.9432207951922,-8.70463697779649,
133.447093608065));
#131830=CARTESIAN_POINT('Ctrl Pts',(81.3021089619863,-10.4723649767864,
133.335960490074));
#131831=CARTESIAN_POINT('Ctrl Pts',(79.4692557562613,-10.8925265973008,
133.224827372082));
#131832=CARTESIAN_POINT('Ctrl Pts',(78.1221605722958,-9.58057338684435,
133.113694254091));
#131833=CARTESIAN_POINT('Ctrl Pts',(78.4937379436049,-7.73725656160221,
133.002561136099));
#131834=CARTESIAN_POINT('Ctrl Pts',(80.2439056348234,-7.04965223227914,
132.891428018108));
#131835=CARTESIAN_POINT('Ctrl Pts',(81.7708412890197,-8.14708294491428,
132.780294900116));
#131836=CARTESIAN_POINT('Ctrl Pts',(81.6770332958706,-10.0251369168521,
132.669161782124));
#131837=CARTESIAN_POINT('Ctrl Pts',(80.0483384229543,-10.9649452334909,
132.558028664133));
#131838=CARTESIAN_POINT('Ctrl Pts',(78.3754023227666,-10.1063583329482,
132.446895546141));
#131839=CARTESIAN_POINT('Ctrl Pts',(78.1893619603281,-8.23518874025145,
132.33576242815));
#131840=CARTESIAN_POINT('Ctrl Pts',(79.6604887978082,-7.0640045151549,132.224629310158));
#131841=CARTESIAN_POINT('Ctrl Pts',(81.4423496505812,-7.66471955782726,
132.113496192167));
#131842=CARTESIAN_POINT('Ctrl Pts',(81.9041153327798,-9.48753581730435,
132.002363074175));
#131843=CARTESIAN_POINT('Ctrl Pts',(80.6231597172374,-10.8641401075573,
131.891229956184));
#131844=CARTESIAN_POINT('Ctrl Pts',(78.7718638010126,-10.5346099995432,
131.780096838192));
#131845=CARTESIAN_POINT('Ctrl Pts',(78.0446064733555,-8.80054441826766,
131.668963720201));
#131846=CARTESIAN_POINT('Ctrl Pts',(79.1070022642405,-7.24902843592665,
131.557830602209));
#131847=CARTESIAN_POINT('Ctrl Pts',(80.9867047321316,-7.30007054651723,
131.446697484217));
#131848=CARTESIAN_POINT('Ctrl Pts',(81.9633361904213,-8.90695500166506,
131.335564366226));
#131849=CARTESIAN_POINT('Ctrl Pts',(81.1430450960569,-10.5989979011803,
131.224431248234));
#131850=CARTESIAN_POINT('Ctrl Pts',(79.2765941297824,-10.8275749862541,
131.113298130243));
#131851=CARTESIAN_POINT('Ctrl Pts',(78.0722327097319,-9.38348350990194,
131.002165012251));
#131852=CARTESIAN_POINT('Ctrl Pts',(78.6322397473312,-7.58841283429622,
130.89103189426));
#131853=CARTESIAN_POINT('Ctrl Pts',(80.4440748897793,-7.08528228660189,
130.779898776268));
#131854=CARTESIAN_POINT('Ctrl Pts',(81.8494750363867,-8.33457676435999,
130.668765658276));
#131855=CARTESIAN_POINT('Ctrl Pts',(81.5621631992815,-10.1928927544656,
130.557632540285));
#131856=CARTESIAN_POINT('Ctrl Pts',(79.8450973712113,-10.9594263923782,
130.446499422293));
#131857=CARTESIAN_POINT('Ctrl Pts',(78.2698060491417,-9.93261577454027,
130.335366304302));
#131858=CARTESIAN_POINT('Ctrl Pts',(78.2780532156094,-8.05223869526036,
130.22423318631));
#131859=CARTESIAN_POINT('Ctrl Pts',(79.8623002247402,-7.03928965083155,
130.113100068319));
#131860=CARTESIAN_POINT('Ctrl Pts',(81.5725624602183,-7.82086073898689,
130.001966950327));
#131861=CARTESIAN_POINT('Ctrl Pts',(81.8435802790012,-9.68162475464961,
129.890833832335));
#131862=CARTESIAN_POINT('Ctrl Pts',(80.4272263791125,-10.9185425137821,
129.779700714344));
#131863=CARTESIAN_POINT('Ctrl Pts',(78.6199695051686,-10.3995273965398,
129.668567596352));
#131864=CARTESIAN_POINT('Ctrl Pts',(78.0755429910078,-8.59962455747607,
129.557434478361));
#131865=CARTESIAN_POINT('Ctrl Pts',(79.2929212938352,-7.16613072427,129.446301360369));
#131866=CARTESIAN_POINT('Ctrl Pts',(81.1564926714636,-7.41112834238548,
129.335168242378));
#131867=CARTESIAN_POINT('Ctrl Pts',(81.9635515616568,-9.11019152566204,
129.224035124386));
#131868=CARTESIAN_POINT('Ctrl Pts',(80.9693423180533,-10.7088529691368,
129.112888868452));
#131869=CARTESIAN_POINT('Ctrl Pts',(79.7214282704788,-10.7302520772847,
129.038786985182));
#131870=CARTESIAN_POINT('Ctrl Pts',(79.230992152254,-10.4744435195791,129.001729474576));
#131871=CARTESIAN_POINT('',(78.7297156613008,-7.9197450866006,140.000878852949));
#131872=CARTESIAN_POINT('Ctrl Pts',(78.7308621637076,-7.92072007686099,
140.000878852949));
#131873=CARTESIAN_POINT('Ctrl Pts',(78.7363705291969,-7.91424272570425,
140.000585901966));
#131874=CARTESIAN_POINT('Ctrl Pts',(78.7419284837365,-7.9078075452857,140.000292950983));
#131875=CARTESIAN_POINT('Ctrl Pts',(78.7475353758638,-7.90141528989,140.));
#131876=CARTESIAN_POINT('Ctrl Pts',(79.4698297828115,-10.9851743256717,
140.));
#131877=CARTESIAN_POINT('Ctrl Pts',(79.4008200957994,-10.9596225970694,
140.));
#131878=CARTESIAN_POINT('Ctrl Pts',(79.333531238509,-10.9301397446099,140.));
#131879=CARTESIAN_POINT('Ctrl Pts',(79.2681549888845,-10.8970246394104,
140.));
#131880=CARTESIAN_POINT('Ctrl Pts',(79.2013067023064,-10.8631639016782,
140.));
#131881=CARTESIAN_POINT('Ctrl Pts',(79.1364573734554,-10.8255047661518,
140.));
#131882=CARTESIAN_POINT('Ctrl Pts',(79.0738433378323,-10.7843220466833,
140.));
#131883=CARTESIAN_POINT('Ctrl Pts',(79.0212317311646,-10.7497181592862,
140.));
#131884=CARTESIAN_POINT('Ctrl Pts',(78.9701986488695,-10.7126254858123,
140.));
#131885=CARTESIAN_POINT('Ctrl Pts',(78.9209066035052,-10.6731894209709,
140.));
#131886=CARTESIAN_POINT('Ctrl Pts',(78.8988725316228,-10.6555610778773,
140.));
#131887=CARTESIAN_POINT('Ctrl Pts',(78.8771866502947,-10.6374643052944,
140.));
#131888=CARTESIAN_POINT('Ctrl Pts',(78.8558650240912,-10.6189113693179,
140.));
#131889=CARTESIAN_POINT('Ctrl Pts',(78.8441548842812,-10.6087218334872,
140.));
#131890=CARTESIAN_POINT('Ctrl Pts',(78.8325546346987,-10.5983946956447,
140.));
#131891=CARTESIAN_POINT('Ctrl Pts',(78.8210670708132,-10.58793194623,140.));
#131892=CARTESIAN_POINT('Ctrl Pts',(78.8104707785347,-10.5782809573921,
140.));
#131893=CARTESIAN_POINT('Ctrl Pts',(78.7999689254918,-10.5685130628946,
140.));
#131894=CARTESIAN_POINT('Ctrl Pts',(78.7895796051904,-10.5586452950551,
140.));
#131895=CARTESIAN_POINT('Ctrl Pts',(78.7365483625556,-10.5082762646108,
140.));
#131896=CARTESIAN_POINT('Ctrl Pts',(78.6863515775254,-10.4552236751168,
140.));
#131897=CARTESIAN_POINT('Ctrl Pts',(78.6392071691807,-10.3997467391998,
140.));
#131898=CARTESIAN_POINT('Ctrl Pts',(78.5923344111128,-10.3445894663248,
140.));
#131899=CARTESIAN_POINT('Ctrl Pts',(78.5484784305652,-10.2870348269277,
140.));
#131900=CARTESIAN_POINT('Ctrl Pts',(78.5078983274109,-10.2273132639917,
140.));
#131901=CARTESIAN_POINT('Ctrl Pts',(78.4742112341867,-10.177736114065,140.));
#131902=CARTESIAN_POINT('Ctrl Pts',(78.4427822939888,-10.1266650192556,
140.));
#131903=CARTESIAN_POINT('Ctrl Pts',(78.4137873452838,-10.0742253403816,
140.));
#131904=CARTESIAN_POINT('Ctrl Pts',(78.4016823044879,-10.0523324079764,
140.));
#131905=CARTESIAN_POINT('Ctrl Pts',(78.3900018207447,-10.0302008977002,
140.));
#131906=CARTESIAN_POINT('Ctrl Pts',(78.3787601302745,-10.0078398495078,
140.));
#131907=CARTESIAN_POINT('Ctrl Pts',(78.3735606382605,-9.99749744666275,
140.));
#131908=CARTESIAN_POINT('Ctrl Pts',(78.3684550268498,-9.98710594030671,
140.));
#131909=CARTESIAN_POINT('Ctrl Pts',(78.3634447697875,-9.97666622690583,
140.));
#131910=CARTESIAN_POINT('Ctrl Pts',(78.3582118701569,-9.96576260026162,
140.));
#131911=CARTESIAN_POINT('Ctrl Pts',(78.3530865941153,-9.95481383392318,
140.));
#131912=CARTESIAN_POINT('Ctrl Pts',(78.3480720076244,-9.94382525390416,
140.));
#131913=CARTESIAN_POINT('Ctrl Pts',(78.3195311208759,-9.88128294489856,
140.));
#131914=CARTESIAN_POINT('Ctrl Pts',(78.2945512381878,-9.81740871987298,
140.));
#131915=CARTESIAN_POINT('Ctrl Pts',(78.2733557714692,-9.75240749763881,
140.));
#131916=CARTESIAN_POINT('Ctrl Pts',(78.2541540953671,-9.69352073509912,
140.));
#131917=CARTESIAN_POINT('Ctrl Pts',(78.2380586683517,-9.63370843084546,
140.));
#131918=CARTESIAN_POINT('Ctrl Pts',(78.2252722924462,-9.57311813897071,
140.));
#131919=CARTESIAN_POINT('Ctrl Pts',(78.2101392841633,-9.50140795341181,
140.));
#131920=CARTESIAN_POINT('Ctrl Pts',(78.1996407717424,-9.42860649740764,
140.));
#131921=CARTESIAN_POINT('Ctrl Pts',(78.1937017083734,-9.35513639115956,
140.));
#131922=CARTESIAN_POINT('Ctrl Pts',(78.1923945550754,-9.33896604817427,
140.));
#131923=CARTESIAN_POINT('Ctrl Pts',(78.1913084919283,-9.32276339661601,
140.));
#131924=CARTESIAN_POINT('Ctrl Pts',(78.1904430881221,-9.30653310676373,
140.));
#131925=CARTESIAN_POINT('Ctrl Pts',(78.1895474828392,-9.28973640072695,
140.));
#131926=CARTESIAN_POINT('Ctrl Pts',(78.1888881969976,-9.27290390047659,
140.));
#131927=CARTESIAN_POINT('Ctrl Pts',(78.1884653147637,-9.25607505183301,
140.));
#131928=CARTESIAN_POINT('Ctrl Pts',(78.1867405462831,-9.18743686990091,
140.));
#131929=CARTESIAN_POINT('Ctrl Pts',(78.1889365602746,-9.11877251451354,
140.));
#131930=CARTESIAN_POINT('Ctrl Pts',(78.194932447553,-9.05042112078302,140.));
#131931=CARTESIAN_POINT('Ctrl Pts',(78.2009126413601,-8.98224862812093,
140.));
#131932=CARTESIAN_POINT('Ctrl Pts',(78.2106733153825,-8.91438639908554,
140.));
#131933=CARTESIAN_POINT('Ctrl Pts',(78.2241439281836,-8.84718590809215,
140.));
#131934=CARTESIAN_POINT('Ctrl Pts',(78.233903850027,-8.79849684326436,140.));
#131935=CARTESIAN_POINT('Ctrl Pts',(78.2456123494515,-8.7501554211586,140.));
#131936=CARTESIAN_POINT('Ctrl Pts',(78.259256796517,-8.70230497136332,140.));
#131937=CARTESIAN_POINT('Ctrl Pts',(78.26949384472,-8.66640411303307,140.));
#131938=CARTESIAN_POINT('Ctrl Pts',(78.2808209031763,-8.63077978202661,
140.));
#131939=CARTESIAN_POINT('Ctrl Pts',(78.2932365554045,-8.59549668869302,
140.));
#131940=CARTESIAN_POINT('Ctrl Pts',(78.2973629100911,-8.58377031662187,
140.));
#131941=CARTESIAN_POINT('Ctrl Pts',(78.3016063044215,-8.57209085321481,
140.));
#131942=CARTESIAN_POINT('Ctrl Pts',(78.3059661153362,-8.56046079440967,
140.));
#131943=CARTESIAN_POINT('Ctrl Pts',(78.3291465008772,-8.49862571664103,
140.));
#131944=CARTESIAN_POINT('Ctrl Pts',(78.3556159809548,-8.43818113391062,
140.));
#131945=CARTESIAN_POINT('Ctrl Pts',(78.3853243049125,-8.37946332859205,
140.));
#131946=CARTESIAN_POINT('Ctrl Pts',(78.406095636309,-8.3384092794008,140.));
#131947=CARTESIAN_POINT('Ctrl Pts',(78.428451125745,-8.29819989796544,140.));
#131948=CARTESIAN_POINT('Ctrl Pts',(78.4523838925721,-8.25896135362974,
140.));
#131949=CARTESIAN_POINT('Ctrl Pts',(78.4600963530419,-8.24631652554664,
140.));
#131950=CARTESIAN_POINT('Ctrl Pts',(78.4679737739132,-8.23377090157036,
140.));
#131951=CARTESIAN_POINT('Ctrl Pts',(78.4760125797683,-8.22133436830632,
140.));
#131952=CARTESIAN_POINT('Ctrl Pts',(78.5102589047579,-8.16835317090255,
140.));
#131953=CARTESIAN_POINT('Ctrl Pts',(78.5473615778501,-8.11745538563355,
140.));
#131954=CARTESIAN_POINT('Ctrl Pts',(78.5872864281299,-8.06895595885705,
140.));
#131955=CARTESIAN_POINT('Ctrl Pts',(78.6240638473892,-8.02427993027098,
140.));
#131956=CARTESIAN_POINT('Ctrl Pts',(78.663236603919,-7.98163893007374,140.));
#131957=CARTESIAN_POINT('Ctrl Pts',(78.7047994118345,-7.9413119889715,140.));
#131958=CARTESIAN_POINT('Ctrl Pts',(78.7126176289588,-7.93372624591629,
140.));
#131959=CARTESIAN_POINT('Ctrl Pts',(78.7205204684454,-7.9262224864657,140.));
#131960=CARTESIAN_POINT('Ctrl Pts',(78.7285063379699,-7.91880137781994,
140.));
#131961=CARTESIAN_POINT('Origin',(80.,-9.,128.));
#131962=CARTESIAN_POINT('Origin',(80.,9.,128.));
#131963=CARTESIAN_POINT('Origin',(70.,4.,140.));
#131964=CARTESIAN_POINT('',(90.,4.,111.633307652784));
#131965=CARTESIAN_POINT('',(70.,4.,111.633307652784));
#131966=CARTESIAN_POINT('',(60.,4.,111.633307652784));
#131967=CARTESIAN_POINT('',(90.,4.,140.));
#131968=CARTESIAN_POINT('',(90.,4.,140.));
#131969=CARTESIAN_POINT('',(70.,4.,140.));
#131970=CARTESIAN_POINT('',(65.,4.,140.));
#131971=CARTESIAN_POINT('',(70.,4.,140.));
#131972=CARTESIAN_POINT('Origin',(70.,-4.,140.));
#131973=CARTESIAN_POINT('',(70.,-4.,111.633307652784));
#131974=CARTESIAN_POINT('Origin',(70.,0.,90.));
#131975=CARTESIAN_POINT('',(70.,-4.,140.));
#131976=CARTESIAN_POINT('',(70.,-2.,140.));
#131977=CARTESIAN_POINT('',(70.,-4.,140.));
#131978=CARTESIAN_POINT('Origin',(90.,-4.,140.));
#131979=CARTESIAN_POINT('',(90.,-4.,111.633307652784));
#131980=CARTESIAN_POINT('',(60.,-4.,111.633307652784));
#131981=CARTESIAN_POINT('',(90.,-4.,140.));
#131982=CARTESIAN_POINT('',(75.,-4.,140.));
#131983=CARTESIAN_POINT('',(90.,-4.,140.));
#131984=CARTESIAN_POINT('Origin',(90.,4.,140.));
#131985=CARTESIAN_POINT('Origin',(90.,0.,90.));
#131986=CARTESIAN_POINT('',(90.,2.,140.));
#131987=CARTESIAN_POINT('Origin',(130.,-35.,35.));
#131988=CARTESIAN_POINT('',(125.5,-35.,40.));
#131989=CARTESIAN_POINT('Origin',(130.,-35.,40.));
#131990=CARTESIAN_POINT('',(125.5,-35.,30.));
#131991=CARTESIAN_POINT('',(125.5,-35.,35.));
#131992=CARTESIAN_POINT('Origin',(130.,-35.,30.));
#131993=CARTESIAN_POINT('Origin',(-10.,-35.,35.));
#131994=CARTESIAN_POINT('',(-14.5,-35.,40.));
#131995=CARTESIAN_POINT('Origin',(-10.,-35.,40.));
#131996=CARTESIAN_POINT('',(-14.5,-35.,30.));
#131997=CARTESIAN_POINT('',(-14.5,-35.,35.));
#131998=CARTESIAN_POINT('Origin',(-10.,-35.,30.));
#131999=CARTESIAN_POINT('Origin',(-10.,35.,35.));
#132000=CARTESIAN_POINT('',(-14.5,35.,40.));
#132001=CARTESIAN_POINT('Origin',(-10.,35.,40.));
#132002=CARTESIAN_POINT('',(-14.5,35.,30.));
#132003=CARTESIAN_POINT('',(-14.5,35.,35.));
#132004=CARTESIAN_POINT('Origin',(-10.,35.,30.));
#132005=CARTESIAN_POINT('Origin',(130.,35.,35.));
#132006=CARTESIAN_POINT('',(125.5,35.,40.));
#132007=CARTESIAN_POINT('Origin',(130.,35.,40.));
#132008=CARTESIAN_POINT('',(125.5,35.,30.));
#132009=CARTESIAN_POINT('',(125.5,35.,35.));
#132010=CARTESIAN_POINT('Origin',(130.,35.,30.));
#132011=CARTESIAN_POINT('Ctrl Pts',(0.00170278829429053,-31.2663976828551,
56.0778454928015));
#132012=CARTESIAN_POINT('Ctrl Pts',(0.0387608137938565,-31.624937451848,
55.6566083896577));
#132013=CARTESIAN_POINT('Ctrl Pts',(0.112863929572942,-31.8820300337866,
54.4354445242093));
#132014=CARTESIAN_POINT('Ctrl Pts',(0.224012135631548,-30.544181885415,
53.1100227718196));
#132015=CARTESIAN_POINT('Ctrl Pts',(0.335147406470108,-28.7082554303748,
53.5190716991923));
#132016=CARTESIAN_POINT('Ctrl Pts',(0.446282677308667,-28.0547317584378,
55.2813852137159));
#132017=CARTESIAN_POINT('Ctrl Pts',(0.557417948147225,-29.1816019930474,
56.787252268337));
#132018=CARTESIAN_POINT('Ctrl Pts',(0.668553218985785,-31.0575569454888,
56.6567445709802));
#132019=CARTESIAN_POINT('Ctrl Pts',(0.779688489824345,-31.9655456415866,
55.0101441815013));
#132020=CARTESIAN_POINT('Ctrl Pts',(0.890823760662904,-31.074532934791,
53.3541184147092));
#132021=CARTESIAN_POINT('Ctrl Pts',(1.00195903150147,-29.2000268959159,
53.204592662045));
#132022=CARTESIAN_POINT('Ctrl Pts',(1.11309430234002,-28.0577155228313,
54.6983168732093));
#132023=CARTESIAN_POINT('Ctrl Pts',(1.22422957317858,-28.6931214980771,
56.4681812061873));
#132024=CARTESIAN_POINT('Ctrl Pts',(1.33536484401714,-30.5246770131522,
56.894251534457));
#132025=CARTESIAN_POINT('Ctrl Pts',(1.4465001148557,-31.8760102052004,55.5865713892929));
#132026=CARTESIAN_POINT('Ctrl Pts',(1.55763538569426,-31.5102842230428,
53.7420166588749));
#132027=CARTESIAN_POINT('Ctrl Pts',(1.66877065653282,-29.7622375781494,
53.0488598107174));
#132028=CARTESIAN_POINT('Ctrl Pts',(1.77990592737138,-28.2318082099653,
54.1415260230505));
#132029=CARTESIAN_POINT('Ctrl Pts',(1.89104119820994,-28.3197549605855,
56.019929579839));
#132030=CARTESIAN_POINT('Ctrl Pts',(2.0021764690485,-29.9455826694406,56.9648201745416));
#132031=CARTESIAN_POINT('Ctrl Pts',(2.11331173988706,-31.621217024128,56.1113662898202));
#132032=CARTESIAN_POINT('Ctrl Pts',(2.22444701072562,-31.8129971096645,
54.240710110029));
#132033=CARTESIAN_POINT('Ctrl Pts',(2.33558228156418,-30.3453920134525,
53.0650105959154));
#132034=CARTESIAN_POINT('Ctrl Pts',(2.44671755240274,-28.5616593378144,
53.6603523633191));
#132035=CARTESIAN_POINT('Ctrl Pts',(2.5578528232413,-28.0943993507182,55.4818358784335));
#132036=CARTESIAN_POINT('Ctrl Pts',(2.66898809407986,-29.3712819556072,
56.8623085852841));
#132037=CARTESIAN_POINT('Ctrl Pts',(2.78012336491841,-31.2236124749314,
56.5382627081225));
#132038=CARTESIAN_POINT('Ctrl Pts',(2.89125863575698,-31.9560049662107,
54.8062883077869));
#132039=CARTESIAN_POINT('Ctrl Pts',(3.00239390659553,-30.8981212142627,
53.2516127626239));
#132040=CARTESIAN_POINT('Ctrl Pts',(3.1135291774341,-29.0182124157641,53.297186802082));
#132041=CARTESIAN_POINT('Ctrl Pts',(3.22466444827265,-28.0369061353021,
54.901297791946));
#132042=CARTESIAN_POINT('Ctrl Pts',(3.33579971911122,-28.8523643671384,
56.5957481322741));
#132043=CARTESIAN_POINT('Ctrl Pts',(3.44693498994977,-30.7182211638377,
56.8296551607653));
#132044=CARTESIAN_POINT('Ctrl Pts',(3.55807026078833,-31.9267103621918,
55.3889303635752));
#132045=CARTESIAN_POINT('Ctrl Pts',(3.66920553162689,-31.3717358431385,
53.5922285611165));
#132046=CARTESIAN_POINT('Ctrl Pts',(3.78034080246546,-29.5612501498527,
53.0840202985193));
#132047=CARTESIAN_POINT('Ctrl Pts',(3.891476073304,-28.1523398344416,54.3294542818737));
#132048=CARTESIAN_POINT('Ctrl Pts',(4.00261134414257,-28.434540818372,56.1886198711722));
#132049=CARTESIAN_POINT('Ctrl Pts',(4.11374661498113,-30.1495624908996,
56.9598751768429));
#132050=CARTESIAN_POINT('Ctrl Pts',(4.22488188581969,-31.7276938288123,
55.9373119445377));
#132051=CARTESIAN_POINT('Ctrl Pts',(4.33601715665825,-31.724515675851,54.0568534942901));
#132052=CARTESIAN_POINT('Ctrl Pts',(4.44715242749681,-30.1429369058903,
53.0396304714612));
#132053=CARTESIAN_POINT('Ctrl Pts',(4.55828769833536,-28.430532012625,53.8166784527888));
#132054=CARTESIAN_POINT('Ctrl Pts',(4.66942296917392,-28.1546169549256,
55.6767873110815));
#132055=CARTESIAN_POINT('Ctrl Pts',(4.78055824001249,-29.5677290123371,
56.9174518092285));
#132056=CARTESIAN_POINT('Ctrl Pts',(4.89169351085105,-31.3764865273067,
56.4031266826741));
#132057=CARTESIAN_POINT('Ctrl Pts',(5.0028287816896,-31.9253847006554,54.6045592307673));
#132058=CARTESIAN_POINT('Ctrl Pts',(5.11396405252817,-30.7120324972562,
53.1679275750288));
#132059=CARTESIAN_POINT('Ctrl Pts',(5.22509932336672,-28.8469770076932,
53.4081401987923));
#132060=CARTESIAN_POINT('Ctrl Pts',(5.33623459420528,-28.037250981328,55.105337254526));
#132061=CARTESIAN_POINT('Ctrl Pts',(5.44736986504384,-29.023973839406,56.7061220886341));
#132062=CARTESIAN_POINT('Ctrl Pts',(5.5585051358824,-30.9040259467696,56.7453414379588));
#132063=CARTESIAN_POINT('Ctrl Pts',(5.66964040672096,-31.9566485722524,
55.1870989369065));
#132064=CARTESIAN_POINT('Ctrl Pts',(5.78077567755952,-31.2184058800449,
53.4576100496434));
#132065=CARTESIAN_POINT('Ctrl Pts',(5.89191094839808,-29.3649906093859,
53.1398272334751));
#132066=CARTESIAN_POINT('Ctrl Pts',(6.00304621923664,-28.0927815451889,
54.524608147822));
#132067=CARTESIAN_POINT('Ctrl Pts',(6.1141814900752,-28.5661958046776,56.3445018322654));
#132068=CARTESIAN_POINT('Ctrl Pts',(6.22531676091376,-30.3519306526335,
56.9338108654224));
#132069=CARTESIAN_POINT('Ctrl Pts',(6.33645203175232,-31.8155532884263,
55.7531572905929));
#132070=CARTESIAN_POINT('Ctrl Pts',(6.44758730259087,-31.6174511450385,
53.8831600647792));
#132071=CARTESIAN_POINT('Ctrl Pts',(6.55872257342944,-29.9389415336019,
53.0353749693217));
#132072=CARTESIAN_POINT('Ctrl Pts',(6.66985784426799,-28.3163170163911,
53.9857558192458));
#132073=CARTESIAN_POINT('Ctrl Pts',(6.78099311510656,-28.2347201032599,
55.8644457956774));
#132074=CARTESIAN_POINT('Ctrl Pts',(6.89212838594511,-29.7688341501512,
56.9519328875076));
#132075=CARTESIAN_POINT('Ctrl Pts',(7.00326365678368,-31.514527787253,56.2528707950653));
#132076=CARTESIAN_POINT('Ctrl Pts',(7.11439892762223,-31.8740168062734,
54.4070913583285));
#132077=CARTESIAN_POINT('Ctrl Pts',(7.22553419846079,-30.518271035144,53.1039844986238));
#132078=CARTESIAN_POINT('Ctrl Pts',(7.33666946929935,-28.6881663857952,
53.5362472147991));
#132079=CARTESIAN_POINT('Ctrl Pts',(7.44780474013791,-28.0587460878319,
55.3082416203242));
#132080=CARTESIAN_POINT('Ctrl Pts',(7.55894001097647,-29.2061008092653,
56.7981111537161));
#132081=CARTESIAN_POINT('Ctrl Pts',(7.67007528181502,-31.080089094353,56.6422202034286));
#132082=CARTESIAN_POINT('Ctrl Pts',(7.78121055265359,-31.9655022600037,
54.9832513618084));
#132083=CARTESIAN_POINT('Ctrl Pts',(7.89234582349214,-31.051946573859,53.3396120806803));
#132084=CARTESIAN_POINT('Ctrl Pts',(8.00348109433071,-29.1755738291021,
53.2156790800412));
#132085=CARTESIAN_POINT('Ctrl Pts',(8.11461636516927,-28.0537751214917,
54.7248847664219));
#132086=CARTESIAN_POINT('Ctrl Pts',(8.22575163600783,-28.7133012426661,
56.485895646412));
#132087=CARTESIAN_POINT('Ctrl Pts',(8.33688690684639,-30.5505064407611,
56.8869081585993));
#132088=CARTESIAN_POINT('Ctrl Pts',(8.44802217768495,-31.8838486975197,
55.5608866733121));
#132089=CARTESIAN_POINT('Ctrl Pts',(8.55915744852351,-31.4929571214681,
53.7215016460962));
#132090=CARTESIAN_POINT('Ctrl Pts',(8.67029271936206,-29.7356043259867,
53.0522896908207));
#132091=CARTESIAN_POINT('Ctrl Pts',(8.78142799020063,-28.2202446973277,
54.1657630148673));
#132092=CARTESIAN_POINT('Ctrl Pts',(8.89256326103917,-28.3338464376506,
56.0427881618974));
#132093=CARTESIAN_POINT('Ctrl Pts',(9.00369853187775,-29.9724286669489,
56.9653822260781));
#132094=CARTESIAN_POINT('Ctrl Pts',(9.11483380271629,-31.6362519689162,
56.0891102760781));
#132095=CARTESIAN_POINT('Ctrl Pts',(9.22596907355487,-31.8024484231335,
54.2160203074161));
#132096=CARTESIAN_POINT('Ctrl Pts',(9.33710434439342,-30.3189374419903,
53.0604572371698));
#132097=CARTESIAN_POINT('Ctrl Pts',(9.44823961523198,-28.5434667432019,
53.6801577952576));
#132098=CARTESIAN_POINT('Ctrl Pts',(9.55937488607055,-28.1012096376717,
55.5077641444152));
#132099=CARTESIAN_POINT('Ctrl Pts',(9.67051015690909,-29.3966839478976,
56.8708435823807));
#132100=CARTESIAN_POINT('Ctrl Pts',(9.78164542774768,-31.244709241904,56.5211656955268));
#132101=CARTESIAN_POINT('Ctrl Pts',(9.8927806985862,-31.9527868925014,54.7800545118344));
#132102=CARTESIAN_POINT('Ctrl Pts',(10.0039159694248,-30.874933117478,53.2385687957247));
#132103=CARTESIAN_POINT('Ctrl Pts',(10.1150512402633,-28.9933745151999,
53.3126786820222));
#132104=CARTESIAN_POINT('Ctrl Pts',(10.1891414208223,-28.358348784767,54.3865918892037));
#132105=CARTESIAN_POINT('Ctrl Pts',(10.2261865111019,-28.338128692637,54.9391906103726));
#132106=CARTESIAN_POINT('Ctrl Pts',(-0.074183729153435,-31.3664915399073,
56.1630365146595));
#132107=CARTESIAN_POINT('Ctrl Pts',(-0.0371257036538689,-31.7533696649088,
55.7085055679165));
#132108=CARTESIAN_POINT('Ctrl Pts',(0.0369774121252169,-32.0307823946921,
54.3908230471987));
#132109=CARTESIAN_POINT('Ctrl Pts',(0.148125618183823,-30.5871930694899,
52.9606422785743));
#132110=CARTESIAN_POINT('Ctrl Pts',(0.259260889022382,-28.6061581997412,
53.4020217174587));
#132111=CARTESIAN_POINT('Ctrl Pts',(0.370396159860942,-27.9009811602368,
55.3036254086718));
#132112=CARTESIAN_POINT('Ctrl Pts',(0.481531430699501,-29.1169172465188,
56.9285135604929));
#132113=CARTESIAN_POINT('Ctrl Pts',(0.592666701538061,-31.1411443960659,
56.7876907630847));
#132114=CARTESIAN_POINT('Ctrl Pts',(0.70380197237662,-32.1208989300063,
55.010945959858));
#132115=CARTESIAN_POINT('Ctrl Pts',(0.81493724321518,-31.1594621378598,
53.2240308139867));
#132116=CARTESIAN_POINT('Ctrl Pts',(0.926072514053739,-29.1367984214722,
53.0626868074554));
#132117=CARTESIAN_POINT('Ctrl Pts',(1.0372077848923,-27.9042007561473,54.674472366719));
#132118=CARTESIAN_POINT('Ctrl Pts',(1.14834305573085,-28.5898281079144,
56.5842236798656));
#132119=CARTESIAN_POINT('Ctrl Pts',(1.25947832656941,-30.5661465662507,
57.0439698613918));
#132120=CARTESIAN_POINT('Ctrl Pts',(1.37061359740797,-32.0242867693873,
55.6329329655858));
#132121=CARTESIAN_POINT('Ctrl Pts',(1.48174886824653,-31.6296544455062,
53.6425878566706));
#132122=CARTESIAN_POINT('Ctrl Pts',(1.59288413908509,-29.7434452523364,
52.8946451040428));
#132123=CARTESIAN_POINT('Ctrl Pts',(1.70401940992365,-28.0920534246646,
54.0736737419738));
#132124=CARTESIAN_POINT('Ctrl Pts',(1.81515468076221,-28.1869513325744,
56.1005430292712));
#132125=CARTESIAN_POINT('Ctrl Pts',(1.92628995160077,-29.9412816188465,
57.1201161233154));
#132126=CARTESIAN_POINT('Ctrl Pts',(2.03742522243933,-31.7493551810914,
56.1992067368236));
#132127=CARTESIAN_POINT('Ctrl Pts',(2.14856049327789,-31.9562932290335,
54.1806971656458));
#132128=CARTESIAN_POINT('Ctrl Pts',(2.25969576411645,-30.3726911938675,
52.912072419044));
#132129=CARTESIAN_POINT('Ctrl Pts',(2.37083103495501,-28.4479754085223,
53.5544689580811));
#132130=CARTESIAN_POINT('Ctrl Pts',(2.48196630579357,-27.9437840096051,
55.5199193432025));
#132131=CARTESIAN_POINT('Ctrl Pts',(2.59310157663213,-29.3215891814387,
57.0095021974063));
#132132=CARTESIAN_POINT('Ctrl Pts',(2.70423684747069,-31.3203246640101,
56.659844301093));
#132133=CARTESIAN_POINT('Ctrl Pts',(2.81537211830925,-32.1106041763419,
54.7909776745694));
#132134=CARTESIAN_POINT('Ctrl Pts',(2.92650738914781,-30.9691071436062,
53.1134232945136));
#132135=CARTESIAN_POINT('Ctrl Pts',(3.03764265998637,-28.9406136429279,
53.1625994263101));
#132136=CARTESIAN_POINT('Ctrl Pts',(3.14877793082492,-27.8817466310379,
54.8934965421195));
#132137=CARTESIAN_POINT('Ctrl Pts',(3.25991320166349,-28.7616572547211,
56.721873272588));
#132138=CARTESIAN_POINT('Ctrl Pts',(3.37104847250204,-30.7749881079645,
56.9742679033468));
#132139=CARTESIAN_POINT('Ctrl Pts',(3.4821837433406,-32.0789941780779,55.4196707390054));
#132140=CARTESIAN_POINT('Ctrl Pts',(3.59331901417916,-31.4801554440706,
53.4809607697478));
#132141=CARTESIAN_POINT('Ctrl Pts',(3.70445428501772,-29.5265721293723,
52.9325846152807));
#132142=CARTESIAN_POINT('Ctrl Pts',(3.81558955585628,-28.0063040077843,
54.2764555215586));
#132143=CARTESIAN_POINT('Ctrl Pts',(3.92672482669484,-28.310809663721,56.282566306076));
#132144=CARTESIAN_POINT('Ctrl Pts',(4.0378600975334,-30.1613836484926,57.1147802816508));
#132145=CARTESIAN_POINT('Ctrl Pts',(4.14899536837196,-31.8642477261168,
56.0113954406308));
#132146=CARTESIAN_POINT('Ctrl Pts',(4.26013063921052,-31.8608183775063,
53.9823088446907));
#132147=CARTESIAN_POINT('Ctrl Pts',(4.37126591004908,-30.1542343888369,
52.8846862939603));
#132148=CARTESIAN_POINT('Ctrl Pts',(4.48240118088764,-28.3064840089819,
53.7231507881405));
#132149=CARTESIAN_POINT('Ctrl Pts',(4.5935364517262,-28.0087611078872,55.730279395983));
#132150=CARTESIAN_POINT('Ctrl Pts',(4.70467172256476,-29.5335630698115,
57.0690038452879));
#132151=CARTESIAN_POINT('Ctrl Pts',(4.81580699340331,-31.4852816140033,
56.5140273606391));
#132152=CARTESIAN_POINT('Ctrl Pts',(4.92694226424188,-32.077563738573,54.5733042842651));
#132153=CARTESIAN_POINT('Ctrl Pts',(5.03807753508044,-30.7683103000047,
53.0231237761138));
#132154=CARTESIAN_POINT('Ctrl Pts',(5.149212805919,-28.7558440878116,53.2823223853626));
#132155=CARTESIAN_POINT('Ctrl Pts',(5.26034807675755,-27.8821187330902,
55.1136629268163));
#132156=CARTESIAN_POINT('Ctrl Pts',(5.37148334759611,-28.9468304394138,
56.8409709933388));
#132157=CARTESIAN_POINT('Ctrl Pts',(5.48261861843467,-30.9754785758391,
56.8832901714124));
#132158=CARTESIAN_POINT('Ctrl Pts',(5.59375388927323,-32.1112986518792,
55.2018869095149));
#132159=CARTESIAN_POINT('Ctrl Pts',(5.70488916011179,-31.3147065489737,
53.3357022466681));
#132160=CARTESIAN_POINT('Ctrl Pts',(5.81602443095035,-29.31480057822,52.9928024327307));
#132161=CARTESIAN_POINT('Ctrl Pts',(5.92715970178891,-27.9420383355576,
54.4870340076132));
#132162=CARTESIAN_POINT('Ctrl Pts',(6.03829497262747,-28.4528704297891,
56.4507689046292));
#132163=CARTESIAN_POINT('Ctrl Pts',(6.14943024346604,-30.3797466356488,
57.08665589266));
#132164=CARTESIAN_POINT('Ctrl Pts',(6.26056551430458,-31.9590514436921,
55.8126855250512));
#132165=CARTESIAN_POINT('Ctrl Pts',(6.37170078514316,-31.7452916535078,
53.7948869904205));
#132166=CARTESIAN_POINT('Ctrl Pts',(6.4828360559817,-29.9341155792511,52.8800944443774));
#132167=CARTESIAN_POINT('Ctrl Pts',(6.59397132682027,-28.1832416592862,
53.9055917338097));
#132168=CARTESIAN_POINT('Ctrl Pts',(6.70510659765882,-28.0951954689103,
55.9327700788575));
#132169=CARTESIAN_POINT('Ctrl Pts',(6.81624186849739,-29.7505632058472,
57.106210247663));
#132170=CARTESIAN_POINT('Ctrl Pts',(6.92737713933594,-31.6342334136067,
56.3518955105745));
#132171=CARTESIAN_POINT('Ctrl Pts',(7.03851241017451,-32.0221358156968,
54.3602288966959));
#132172=CARTESIAN_POINT('Ctrl Pts',(7.14964768101306,-30.5592342709492,
52.9541267508301));
#132173=CARTESIAN_POINT('Ctrl Pts',(7.26078295185163,-28.5844813522277,
53.4205547557672));
#132174=CARTESIAN_POINT('Ctrl Pts',(7.37191822269018,-27.9053127752024,
55.332604498668));
#132175=CARTESIAN_POINT('Ctrl Pts',(7.48305349352875,-29.1433524063054,
56.9402307131726));
#132176=CARTESIAN_POINT('Ctrl Pts',(7.59418876436729,-31.1654574465519,
56.7720184149349));
#132177=CARTESIAN_POINT('Ctrl Pts',(7.70532403520587,-32.1208521196191,
54.9819275787506));
#132178=CARTESIAN_POINT('Ctrl Pts',(7.81645930604441,-31.1350905904786,
53.2083779246979));
#132179=CARTESIAN_POINT('Ctrl Pts',(7.92759457688299,-29.1104126270428,
53.0746494765322));
#132180=CARTESIAN_POINT('Ctrl Pts',(8.03872984772154,-27.8999489123803,
54.7031401397257));
#132181=CARTESIAN_POINT('Ctrl Pts',(8.1498651185601,-28.6116028242076,56.6033382384509));
#132182=CARTESIAN_POINT('Ctrl Pts',(8.26100038939866,-30.5940175066244,
57.0360460779548));
#132183=CARTESIAN_POINT('Ctrl Pts',(8.37213566023721,-32.0327448024245,
55.6052181745942));
#132184=CARTESIAN_POINT('Ctrl Pts',(8.48327093107578,-31.6109578401403,
53.6204513731766));
#132185=CARTESIAN_POINT('Ctrl Pts',(8.59440620191433,-29.7147069545225,
52.8983460758682));
#132186=CARTESIAN_POINT('Ctrl Pts',(8.7055414727529,-28.0795759522207,54.0998263832167));
#132187=CARTESIAN_POINT('Ctrl Pts',(8.81667674359147,-28.2021565753311,
56.1252083136601));
#132188=CARTESIAN_POINT('Ctrl Pts',(8.92781201443001,-29.9702494770258,
57.120722598422));
#132189=CARTESIAN_POINT('Ctrl Pts',(9.03894728526858,-31.7655784616092,
56.1751916466963));
#132190=CARTESIAN_POINT('Ctrl Pts',(9.15008255610713,-31.944910792776,54.154055924234));
#132191=CARTESIAN_POINT('Ctrl Pts',(9.26121782694571,-30.3441456993643,
52.90715917079));
#132192=CARTESIAN_POINT('Ctrl Pts',(9.37235309778425,-28.428344903063,53.5758397767066));
#132193=CARTESIAN_POINT('Ctrl Pts',(9.48348836862282,-27.9511325697238,
55.547896933961));
#132194=CARTESIAN_POINT('Ctrl Pts',(9.59462363946135,-29.3489989027542,
57.0187117857399));
#132195=CARTESIAN_POINT('Ctrl Pts',(9.70575891029995,-31.3430888825314,
56.6413959705362));
#132196=CARTESIAN_POINT('Ctrl Pts',(9.81689418113849,-32.1071317517173,
54.7626704052856));
#132197=CARTESIAN_POINT('Ctrl Pts',(9.92802945197706,-30.9440863002237,
53.0993483552936));
#132198=CARTESIAN_POINT('Ctrl Pts',(10.0391647228156,-28.9138125981616,
53.1793157573348));
#132199=CARTESIAN_POINT('Ctrl Pts',(10.1132549033747,-28.2285955450921,
54.3381091853991));
#132200=CARTESIAN_POINT('Ctrl Pts',(10.1502999936542,-28.2067772922589,
54.9343843426139));
#132201=CARTESIAN_POINT('Ctrl Pts',(-0.15007024660116,-31.4665853969597,
56.2482275365175));
#132202=CARTESIAN_POINT('Ctrl Pts',(-0.113012221101594,-31.8818018779696,
55.7604027461753));
#132203=CARTESIAN_POINT('Ctrl Pts',(-0.0389091053225084,-32.1795347555977,
54.3462015701881));
#132204=CARTESIAN_POINT('Ctrl Pts',(0.072239100736097,-30.6302042535647,
52.8112617853291));
#132205=CARTESIAN_POINT('Ctrl Pts',(0.183374371574657,-28.5040609691078,
53.284971735725));
#132206=CARTESIAN_POINT('Ctrl Pts',(0.294509642413217,-27.7472305620358,
55.3258656036276));
#132207=CARTESIAN_POINT('Ctrl Pts',(0.405644913251776,-29.0522324999903,
57.0697748526486));
#132208=CARTESIAN_POINT('Ctrl Pts',(0.516780184090336,-31.2247318466428,
56.9186369551892));
#132209=CARTESIAN_POINT('Ctrl Pts',(0.627915454928895,-32.2762522184261,
55.0117477382148));
#132210=CARTESIAN_POINT('Ctrl Pts',(0.739050725767455,-31.2443913409285,
53.0939432132643));
#132211=CARTESIAN_POINT('Ctrl Pts',(0.850185996606014,-29.0735699470287,
52.9207809528658));
#132212=CARTESIAN_POINT('Ctrl Pts',(0.961321267444574,-27.7506859894634,
54.6506278602288));
#132213=CARTESIAN_POINT('Ctrl Pts',(1.07245653828313,-28.4865347177518,
56.7002661535439));
#132214=CARTESIAN_POINT('Ctrl Pts',(1.1835918091217,-30.6076161193494,57.1936881883264));
#132215=CARTESIAN_POINT('Ctrl Pts',(1.29472707996025,-32.1725633335742,
55.6792945418786));
#132216=CARTESIAN_POINT('Ctrl Pts',(1.40586235079882,-31.7490246679696,
53.5431590544662));
#132217=CARTESIAN_POINT('Ctrl Pts',(1.51699762163737,-29.7246529265234,
52.7404303973681));
#132218=CARTESIAN_POINT('Ctrl Pts',(1.62813289247593,-27.9522986393639,
54.0058214608971));
#132219=CARTESIAN_POINT('Ctrl Pts',(1.73926816331449,-28.0541477045633,
56.1811564787034));
#132220=CARTESIAN_POINT('Ctrl Pts',(1.85040343415305,-29.9369805682525,
57.2754120720893));
#132221=CARTESIAN_POINT('Ctrl Pts',(1.96153870499161,-31.8774933380549,
56.2870471838269));
#132222=CARTESIAN_POINT('Ctrl Pts',(2.07267397583017,-32.0995893484024,
54.1206842212628));
#132223=CARTESIAN_POINT('Ctrl Pts',(2.18380924666873,-30.3999903742827,
52.7591342421725));
#132224=CARTESIAN_POINT('Ctrl Pts',(2.29494451750729,-28.3342914792303,
53.448585552843));
#132225=CARTESIAN_POINT('Ctrl Pts',(2.40607978834585,-27.7931686684921,
55.5580028079716));
#132226=CARTESIAN_POINT('Ctrl Pts',(2.51721505918441,-29.2718964072702,
57.1566958095285));
#132227=CARTESIAN_POINT('Ctrl Pts',(2.62835033002297,-31.4170368530889,
56.7814258940635));
#132228=CARTESIAN_POINT('Ctrl Pts',(2.73948560086153,-32.2652033864732,
54.7756670413518));
#132229=CARTESIAN_POINT('Ctrl Pts',(2.85062087170008,-31.0400930729498,
52.9752338264031));
#132230=CARTESIAN_POINT('Ctrl Pts',(2.96175614253865,-28.8630148700916,
53.0280120505382));
#132231=CARTESIAN_POINT('Ctrl Pts',(3.0728914133772,-27.7265871267736,54.885695292293));
#132232=CARTESIAN_POINT('Ctrl Pts',(3.18402668421577,-28.6709501423038,
56.8479984129019));
#132233=CARTESIAN_POINT('Ctrl Pts',(3.29516195505432,-30.8317550520915,
57.1188806459284));
#132234=CARTESIAN_POINT('Ctrl Pts',(3.40629722589288,-32.2312779939638,
55.4504111144357));
#132235=CARTESIAN_POINT('Ctrl Pts',(3.51743249673144,-31.5885750450029,
53.3696929783789));
#132236=CARTESIAN_POINT('Ctrl Pts',(3.62856776757001,-29.4918941088918,
52.781148932042));
#132237=CARTESIAN_POINT('Ctrl Pts',(3.73970303840856,-27.860268181127,54.2234567612437));
#132238=CARTESIAN_POINT('Ctrl Pts',(3.85083830924712,-28.18707850907,56.3765127409798));
#132239=CARTESIAN_POINT('Ctrl Pts',(3.96197358008568,-30.1732048060856,
57.2696853864588));
#132240=CARTESIAN_POINT('Ctrl Pts',(4.07310885092424,-32.0008016234211,
56.0854789367237));
#132241=CARTESIAN_POINT('Ctrl Pts',(4.1842441217628,-31.9971210791615,53.9077641950914));
#132242=CARTESIAN_POINT('Ctrl Pts',(4.29537939260136,-30.1655318717835,
52.7297421164591));
#132243=CARTESIAN_POINT('Ctrl Pts',(4.40651466343992,-28.1824360053388,
53.6296231234923));
#132244=CARTESIAN_POINT('Ctrl Pts',(4.51764993427848,-27.8629052608487,
55.7837714808843));
#132245=CARTESIAN_POINT('Ctrl Pts',(4.62878520511703,-29.4993971272859,
57.2205558813473));
#132246=CARTESIAN_POINT('Ctrl Pts',(4.7399204759556,-31.5940767006999,56.624928038604));
#132247=CARTESIAN_POINT('Ctrl Pts',(4.85105574679415,-32.2297427764907,
54.5420493377628));
#132248=CARTESIAN_POINT('Ctrl Pts',(4.96219101763272,-30.8245881027533,
52.8783199771989));
#132249=CARTESIAN_POINT('Ctrl Pts',(5.07332628847127,-28.6647111679299,
53.1565045719328));
#132250=CARTESIAN_POINT('Ctrl Pts',(5.18446155930983,-27.7269864848525,
55.1219885991068));
#132251=CARTESIAN_POINT('Ctrl Pts',(5.2955968301484,-28.8696870394214,56.9758198980433));
#132252=CARTESIAN_POINT('Ctrl Pts',(5.40673210098694,-31.0469312049086,
57.0212389048661));
#132253=CARTESIAN_POINT('Ctrl Pts',(5.51786737182552,-32.2659487315058,
55.2166748821232));
#132254=CARTESIAN_POINT('Ctrl Pts',(5.62900264266406,-31.4110072179026,
53.2137944436928));
#132255=CARTESIAN_POINT('Ctrl Pts',(5.74013791350264,-29.264610547054,52.8457776319862));
#132256=CARTESIAN_POINT('Ctrl Pts',(5.85127318434119,-27.7912951259262,
54.4494598674044));
#132257=CARTESIAN_POINT('Ctrl Pts',(5.96240845517975,-28.3395450549005,
56.5570359769931));
#132258=CARTESIAN_POINT('Ctrl Pts',(6.07354372601831,-30.4075626186642,
57.2395009198977));
#132259=CARTESIAN_POINT('Ctrl Pts',(6.18467899685687,-32.1025495989578,
55.8722137595095));
#132260=CARTESIAN_POINT('Ctrl Pts',(6.29581426769543,-31.873132161977,53.7066139160619));
#132261=CARTESIAN_POINT('Ctrl Pts',(6.40694953853399,-29.9292896249002,
52.724813919433));
#132262=CARTESIAN_POINT('Ctrl Pts',(6.51808480937254,-28.0501663021814,
53.8254276483735));
#132263=CARTESIAN_POINT('Ctrl Pts',(6.62922008021111,-27.9556708345606,
56.0010943620377));
#132264=CARTESIAN_POINT('Ctrl Pts',(6.74035535104966,-29.7322922615432,
57.2604876078183));
#132265=CARTESIAN_POINT('Ctrl Pts',(6.85149062188823,-31.7539390399603,
56.4509202260838));
#132266=CARTESIAN_POINT('Ctrl Pts',(6.96262589272678,-32.1702548251203,
54.3133664350632));
#132267=CARTESIAN_POINT('Ctrl Pts',(7.07376116356534,-30.6001975067545,
52.8042690030366));
#132268=CARTESIAN_POINT('Ctrl Pts',(7.18489643440391,-28.4807963186602,
53.3048622967354));
#132269=CARTESIAN_POINT('Ctrl Pts',(7.29603170524246,-27.7518794625729,
55.3569673770119));
#132270=CARTESIAN_POINT('Ctrl Pts',(7.40716697608102,-29.0806040033454,
57.0823502726293));
#132271=CARTESIAN_POINT('Ctrl Pts',(7.51830224691958,-31.2508257987508,
56.9018166264413));
#132272=CARTESIAN_POINT('Ctrl Pts',(7.62943751775815,-32.2762019792346,
54.9806037956928));
#132273=CARTESIAN_POINT('Ctrl Pts',(7.7405727885967,-31.2182346070983,53.0771437687153));
#132274=CARTESIAN_POINT('Ctrl Pts',(7.85170805943526,-29.0452514249833,
52.9336198730232));
#132275=CARTESIAN_POINT('Ctrl Pts',(7.96284333027382,-27.746122703269,54.6813955130294));
#132276=CARTESIAN_POINT('Ctrl Pts',(8.07397860111238,-28.509904405749,56.7207808304898));
#132277=CARTESIAN_POINT('Ctrl Pts',(8.18511387195094,-30.6375285724877,
57.1851839973102));
#132278=CARTESIAN_POINT('Ctrl Pts',(8.29624914278949,-32.1816409073294,
55.6495496758762));
#132279=CARTESIAN_POINT('Ctrl Pts',(8.40738441362806,-31.7289585588121,
53.519401100257));
#132280=CARTESIAN_POINT('Ctrl Pts',(8.51851968446662,-29.6938095830584,
52.7444024609157));
#132281=CARTESIAN_POINT('Ctrl Pts',(8.62965495530518,-27.9389072071136,
54.0338897515661));
#132282=CARTESIAN_POINT('Ctrl Pts',(8.74079022614373,-28.0704667130116,
56.2076284654227));
#132283=CARTESIAN_POINT('Ctrl Pts',(8.85192549698231,-29.9680702871027,
57.2760629707658));
#132284=CARTESIAN_POINT('Ctrl Pts',(8.96306076782084,-31.8949049543022,
56.2612730173147));
#132285=CARTESIAN_POINT('Ctrl Pts',(9.07419603865942,-32.0873731624184,
54.0920915410519));
#132286=CARTESIAN_POINT('Ctrl Pts',(9.18533130949797,-30.3693539567383,
52.7538611044103));
#132287=CARTESIAN_POINT('Ctrl Pts',(9.29646658033654,-28.3132230629242,
53.4715217581555));
#132288=CARTESIAN_POINT('Ctrl Pts',(9.40760185117508,-27.8010555017756,
55.5880297235069));
#132289=CARTESIAN_POINT('Ctrl Pts',(9.51873712201365,-29.3013138576107,
57.1665799890989));
#132290=CARTESIAN_POINT('Ctrl Pts',(9.62987239285222,-31.441468523159,56.7616262455456));
#132291=CARTESIAN_POINT('Ctrl Pts',(9.74100766369077,-32.2614766109332,
54.7452862987369));
#132292=CARTESIAN_POINT('Ctrl Pts',(9.85214293452933,-31.0132394829693,
52.9601279148623));
#132293=CARTESIAN_POINT('Ctrl Pts',(9.96327820536789,-28.8342506811234,
53.0459528326475));
#132294=CARTESIAN_POINT('Ctrl Pts',(10.037368385927,-28.0988423054172,54.2896264815944));
#132295=CARTESIAN_POINT('Ctrl Pts',(10.0744134762065,-28.075425891881,54.9295780748552));
#132296=CARTESIAN_POINT('Ctrl Pts',(-0.225956764048886,-31.5666792540119,
56.3334185583754));
#132297=CARTESIAN_POINT('Ctrl Pts',(-0.188898738549319,-32.0102340910304,
55.8122999244342));
#132298=CARTESIAN_POINT('Ctrl Pts',(-0.114795622770234,-32.3282871165031,
54.3015800931774));
#132299=CARTESIAN_POINT('Ctrl Pts',(-0.00364741671162839,-30.6732154376395,
52.6618812920838));
#132300=CARTESIAN_POINT('Ctrl Pts',(0.107487854126931,-28.4019637384743,
53.1679217539914));
#132301=CARTESIAN_POINT('Ctrl Pts',(0.218623124965491,-27.5934799638349,
55.3481057985834));
#132302=CARTESIAN_POINT('Ctrl Pts',(0.32975839580405,-28.9875477534618,
57.2110361448045));
#132303=CARTESIAN_POINT('Ctrl Pts',(0.44089366664261,-31.3083192972198,
57.0495831472937));
#132304=CARTESIAN_POINT('Ctrl Pts',(0.552028937481168,-32.4316055068458,
55.0125495165716));
#132305=CARTESIAN_POINT('Ctrl Pts',(0.66316420831973,-31.3293205439973,
52.9638556125418));
#132306=CARTESIAN_POINT('Ctrl Pts',(0.774299479158287,-29.010341472585,
52.7788750982762));
#132307=CARTESIAN_POINT('Ctrl Pts',(0.885434749996847,-27.5971712227794,
54.6267833537386));
#132308=CARTESIAN_POINT('Ctrl Pts',(0.996570020835408,-28.3832413275893,
56.8163086272222));
#132309=CARTESIAN_POINT('Ctrl Pts',(1.10770529167397,-30.649085672448,57.3434065152611));
#132310=CARTESIAN_POINT('Ctrl Pts',(1.21884056251252,-32.320839897761,55.7256561181716));
#132311=CARTESIAN_POINT('Ctrl Pts',(1.32997583335109,-31.868394890433,53.4437302522617));
#132312=CARTESIAN_POINT('Ctrl Pts',(1.44111110418964,-29.7058606007103,
52.5862156906935));
#132313=CARTESIAN_POINT('Ctrl Pts',(1.5522463750282,-27.8125438540631,53.9379691798205));
#132314=CARTESIAN_POINT('Ctrl Pts',(1.66338164586676,-27.9213440765523,
56.2617699281355));
#132315=CARTESIAN_POINT('Ctrl Pts',(1.77451691670532,-29.9326795176583,
57.4307080208631));
#132316=CARTESIAN_POINT('Ctrl Pts',(1.88565218754388,-32.0056314950183,
56.3748876308303));
#132317=CARTESIAN_POINT('Ctrl Pts',(1.99678745838244,-32.2428854677713,
54.0606712768798));
#132318=CARTESIAN_POINT('Ctrl Pts',(2.107922729221,-30.4272895546977,52.606196065301));
#132319=CARTESIAN_POINT('Ctrl Pts',(2.21905800005956,-28.2206075499382,
53.3427021476049));
#132320=CARTESIAN_POINT('Ctrl Pts',(2.33019327089812,-27.6425533273791,
55.5960862727407));
#132321=CARTESIAN_POINT('Ctrl Pts',(2.44132854173668,-29.2222036331016,
57.3038894216507));
#132322=CARTESIAN_POINT('Ctrl Pts',(2.55246381257524,-31.5137490421676,
56.903007487034));
#132323=CARTESIAN_POINT('Ctrl Pts',(2.6635990834138,-32.4198025966044,54.7603564081343));
#132324=CARTESIAN_POINT('Ctrl Pts',(2.77473435425236,-31.1110790022934,
52.8370443582928));
#132325=CARTESIAN_POINT('Ctrl Pts',(2.88586962509092,-28.7854160972553,
52.8934246747662));
#132326=CARTESIAN_POINT('Ctrl Pts',(2.99700489592947,-27.5714276225093,
54.8778940424664));
#132327=CARTESIAN_POINT('Ctrl Pts',(3.10814016676804,-28.5802430298865,
56.9741235532158));
#132328=CARTESIAN_POINT('Ctrl Pts',(3.2192754376066,-30.8885219962184,57.2634933885099));
#132329=CARTESIAN_POINT('Ctrl Pts',(3.33041070844515,-32.3835618098499,
55.481151489866));
#132330=CARTESIAN_POINT('Ctrl Pts',(3.44154597928371,-31.6969946459351,
53.2584251870102));
#132331=CARTESIAN_POINT('Ctrl Pts',(3.55268125012228,-29.4572160884115,
52.6297132488032));
#132332=CARTESIAN_POINT('Ctrl Pts',(3.66381652096083,-27.7142323544697,
54.1704580009286));
#132333=CARTESIAN_POINT('Ctrl Pts',(3.7749517917994,-28.063347354419,56.4704591758836));
#132334=CARTESIAN_POINT('Ctrl Pts',(3.88608706263795,-30.1850259636787,
57.4245904912667));
#132335=CARTESIAN_POINT('Ctrl Pts',(3.99722233347652,-32.1373555207256,
56.1595624328168));
#132336=CARTESIAN_POINT('Ctrl Pts',(4.10835760431506,-32.1334237808167,
53.833219545492));
#132337=CARTESIAN_POINT('Ctrl Pts',(4.21949287515364,-30.1768293547301,
52.5747979389581));
#132338=CARTESIAN_POINT('Ctrl Pts',(4.33062814599218,-28.0583880016956,
53.536095458844));
#132339=CARTESIAN_POINT('Ctrl Pts',(4.44176341683075,-27.7170494138102,
55.8372635657857));
#132340=CARTESIAN_POINT('Ctrl Pts',(4.5528986876693,-29.4652311847602,57.3721079174066));
#132341=CARTESIAN_POINT('Ctrl Pts',(4.66403395850787,-31.7028717873966,
56.735828716569));
#132342=CARTESIAN_POINT('Ctrl Pts',(4.77516922934643,-32.3819218144083,
54.5107943912606));
#132343=CARTESIAN_POINT('Ctrl Pts',(4.88630450018498,-30.8808659055018,
52.7335161782839));
#132344=CARTESIAN_POINT('Ctrl Pts',(4.99743977102355,-28.5735782480482,
53.0306867585031));
#132345=CARTESIAN_POINT('Ctrl Pts',(5.1085750418621,-27.5718542366147,55.1303142713972));
#132346=CARTESIAN_POINT('Ctrl Pts',(5.21971031270067,-28.7925436394291,
57.110668802748));
#132347=CARTESIAN_POINT('Ctrl Pts',(5.33084558353922,-31.1183838339782,
57.1591876383197));
#132348=CARTESIAN_POINT('Ctrl Pts',(5.44198085437779,-32.4205988111325,
55.2314628547315));
#132349=CARTESIAN_POINT('Ctrl Pts',(5.55311612521634,-31.5073078868314,
53.0918866407176));
#132350=CARTESIAN_POINT('Ctrl Pts',(5.66425139605491,-29.214420515888,52.6987528312416));
#132351=CARTESIAN_POINT('Ctrl Pts',(5.77538666689346,-27.6405519162949,
54.4118857271955));
#132352=CARTESIAN_POINT('Ctrl Pts',(5.88652193773202,-28.2262196800119,
56.6633030493568));
#132353=CARTESIAN_POINT('Ctrl Pts',(5.99765720857058,-30.4353786016796,
57.3923459471355));
#132354=CARTESIAN_POINT('Ctrl Pts',(6.10879247940914,-32.2460477542236,
55.9317419939679));
#132355=CARTESIAN_POINT('Ctrl Pts',(6.2199277502477,-32.0009726704464,53.6183408417034));
#132356=CARTESIAN_POINT('Ctrl Pts',(6.33106302108626,-29.9244636705494,
52.5695333944887));
#132357=CARTESIAN_POINT('Ctrl Pts',(6.44219829192482,-27.9170909450764,
53.7452635629374));
#132358=CARTESIAN_POINT('Ctrl Pts',(6.55333356276338,-27.816146200211,56.0694186452177));
#132359=CARTESIAN_POINT('Ctrl Pts',(6.66446883360194,-29.7140213172392,
57.4147649679738));
#132360=CARTESIAN_POINT('Ctrl Pts',(6.77560410444049,-31.873644666314,56.549944941593));
#132361=CARTESIAN_POINT('Ctrl Pts',(6.88673937527906,-32.3183738345439,
54.2665039734305));
#132362=CARTESIAN_POINT('Ctrl Pts',(6.99787464611762,-30.6411607425598,
52.6544112552431));
#132363=CARTESIAN_POINT('Ctrl Pts',(7.10900991695617,-28.3771112850928,
53.1891698377035));
#132364=CARTESIAN_POINT('Ctrl Pts',(7.22014518779474,-27.5984461499434,
55.3813302553558));
#132365=CARTESIAN_POINT('Ctrl Pts',(7.33128045863329,-29.0178556003855,
57.2244698320859));
#132366=CARTESIAN_POINT('Ctrl Pts',(7.44241572947186,-31.3361941509497,
57.0316148379476));
#132367=CARTESIAN_POINT('Ctrl Pts',(7.55355100031041,-32.4315518388499,
54.979280012635));
#132368=CARTESIAN_POINT('Ctrl Pts',(7.66468627114897,-31.3013786237181,
52.9459096127328));
#132369=CARTESIAN_POINT('Ctrl Pts',(7.77582154198753,-28.980090222924,52.7925902695143));
#132370=CARTESIAN_POINT('Ctrl Pts',(7.88695681282609,-27.5922964941576,
54.6596508863331));
#132371=CARTESIAN_POINT('Ctrl Pts',(7.99809208366465,-28.4082059872904,
56.8382234225286));
#132372=CARTESIAN_POINT('Ctrl Pts',(8.1092273545032,-30.6810396383511,57.3343219166659));
#132373=CARTESIAN_POINT('Ctrl Pts',(8.22036262534177,-32.3305370122343,
55.6938811771581));
#132374=CARTESIAN_POINT('Ctrl Pts',(8.33149789618033,-31.8469592774841,
53.4183508273375));
#132375=CARTESIAN_POINT('Ctrl Pts',(8.44263316701889,-29.6729122115943,
52.5904588459632));
#132376=CARTESIAN_POINT('Ctrl Pts',(8.55376843785744,-27.7982384620065,
53.9679531199155));
#132377=CARTESIAN_POINT('Ctrl Pts',(8.66490370869601,-27.938776850692,56.2900486171853));
#132378=CARTESIAN_POINT('Ctrl Pts',(8.77603897953457,-29.9658910971795,
57.4314033431097));
#132379=CARTESIAN_POINT('Ctrl Pts',(8.88717425037312,-32.0242314469952,
56.3473543879329));
#132380=CARTESIAN_POINT('Ctrl Pts',(8.99830952121169,-32.2298355320608,
54.0301271578697));
#132381=CARTESIAN_POINT('Ctrl Pts',(9.10944479205024,-30.3945622141122,
52.6005630380306));
#132382=CARTESIAN_POINT('Ctrl Pts',(9.22058006288882,-28.1981012227853,
53.3672037396045));
#132383=CARTESIAN_POINT('Ctrl Pts',(9.33171533372735,-27.6509784338276,
55.6281625130527));
#132384=CARTESIAN_POINT('Ctrl Pts',(9.44285060456594,-29.2536288124672,
57.3144481924582));
#132385=CARTESIAN_POINT('Ctrl Pts',(9.55398587540448,-31.5398481637865,
56.8818565205549));
#132386=CARTESIAN_POINT('Ctrl Pts',(9.66512114624305,-32.415821470149,54.7279021921883));
#132387=CARTESIAN_POINT('Ctrl Pts',(9.7762564170816,-31.082392665715,52.8209074744312));
#132388=CARTESIAN_POINT('Ctrl Pts',(9.88739168792017,-28.7546887640851,
52.9125899079599));
#132389=CARTESIAN_POINT('Ctrl Pts',(9.9614818684792,-27.9690890657423,54.2411437777897));
#132390=CARTESIAN_POINT('Ctrl Pts',(9.99852695875872,-27.944074491503,54.9247718070965));
#132391=CARTESIAN_POINT('',(10.0008699698353,-30.7705894968619,53.5212323702993));
#132392=CARTESIAN_POINT('Ctrl Pts',(10.,-27.9466241674713,54.9248651020699));
#132393=CARTESIAN_POINT('Ctrl Pts',(9.99999999999999,-27.9564039519262,
54.8501832546246));
#132394=CARTESIAN_POINT('Ctrl Pts',(9.99999999999998,-27.9706090922962,
54.7762523429086));
#132395=CARTESIAN_POINT('Ctrl Pts',(9.99999999999999,-27.9890023094346,
54.7033576472274));
#132396=CARTESIAN_POINT('Ctrl Pts',(10.,-28.0065895417162,54.633657173656));
#132397=CARTESIAN_POINT('Ctrl Pts',(10.,-28.0280067648394,54.5649035539299));
#132398=CARTESIAN_POINT('Ctrl Pts',(9.99999999999999,-28.0530852461662,
54.4973682348888));
#132399=CARTESIAN_POINT('Ctrl Pts',(9.99999999999999,-28.0587349917983,
54.4821537022067));
#132400=CARTESIAN_POINT('Ctrl Pts',(9.99999999999999,-28.0645714906859,
54.4669991037866));
#132401=CARTESIAN_POINT('Ctrl Pts',(10.,-28.0705904602987,54.451914165365));
#132402=CARTESIAN_POINT('Ctrl Pts',(10.,-28.0982103307347,54.3826923431025));
#132403=CARTESIAN_POINT('Ctrl Pts',(10.,-28.1296130964609,54.3150720673866));
#132404=CARTESIAN_POINT('Ctrl Pts',(10.,-28.1645888762895,54.249345890764));
#132405=CARTESIAN_POINT('Ctrl Pts',(10.,-28.1891445313107,54.2032011206712));
#132406=CARTESIAN_POINT('Ctrl Pts',(10.,-28.2154623661137,54.1579904820105));
#132407=CARTESIAN_POINT('Ctrl Pts',(10.,-28.2434807977927,54.113825883058));
#132408=CARTESIAN_POINT('Ctrl Pts',(10.,-28.2541311786634,54.0970380126577));
#132409=CARTESIAN_POINT('Ctrl Pts',(10.,-28.2650273632795,54.0804013902968));
#132410=CARTESIAN_POINT('Ctrl Pts',(10.,-28.2761662488052,54.0639225691025));
#132411=CARTESIAN_POINT('Ctrl Pts',(10.,-28.2867799276645,54.0482207364789));
#132412=CARTESIAN_POINT('Ctrl Pts',(10.,-28.2976175556647,54.032657412247));
#132413=CARTESIAN_POINT('Ctrl Pts',(10.,-28.3086567111279,54.0172654083652));
#132414=CARTESIAN_POINT('Ctrl Pts',(9.99999999999999,-28.3509657809783,
53.9582734529077));
#132415=CARTESIAN_POINT('Ctrl Pts',(10.,-28.3962731815781,53.9017302005496));
#132416=CARTESIAN_POINT('Ctrl Pts',(10.,-28.444386329927,53.8479078339097));
#132417=CARTESIAN_POINT('Ctrl Pts',(10.,-28.4913495953192,53.7953717980173));
#132418=CARTESIAN_POINT('Ctrl Pts',(10.,-28.5409868702555,53.74542762759));
#132419=CARTESIAN_POINT('Ctrl Pts',(10.,-28.5931475035754,53.6983678482907));
#132420=CARTESIAN_POINT('Ctrl Pts',(10.,-28.644420195856,53.6521091771583));
#132421=CARTESIAN_POINT('Ctrl Pts',(10.,-28.6981316928852,53.6086370584655));
#132422=CARTESIAN_POINT('Ctrl Pts',(10.,-28.7541565899177,53.5682751474532));
#132423=CARTESIAN_POINT('Ctrl Pts',(10.,-28.7723276241148,53.5551842235227));
#132424=CARTESIAN_POINT('Ctrl Pts',(10.,-28.7907421194074,53.5424208732304));
#132425=CARTESIAN_POINT('Ctrl Pts',(9.99999999999999,-28.8093960417122,
53.5299973248125));
#132426=CARTESIAN_POINT('Ctrl Pts',(9.99999999999998,-28.8198979217188,
53.5230030523689));
#132427=CARTESIAN_POINT('Ctrl Pts',(9.99999999999998,-28.8304768374501,
53.5161158780251));
#132428=CARTESIAN_POINT('Ctrl Pts',(9.99999999999999,-28.8411168980571,
53.5093473810421));
#132429=CARTESIAN_POINT('Ctrl Pts',(10.,-28.8987469337441,53.4726869956283));
#132430=CARTESIAN_POINT('Ctrl Pts',(10.,-28.9582678505386,53.439437211614));
#132431=CARTESIAN_POINT('Ctrl Pts',(10.,-29.0195356012334,53.4098650402476));
#132432=CARTESIAN_POINT('Ctrl Pts',(10.,-29.0283680962592,53.4056018503388));
#132433=CARTESIAN_POINT('Ctrl Pts',(9.99999999999997,-29.037236928022,53.4014151736005));
#132434=CARTESIAN_POINT('Ctrl Pts',(9.99999999999997,-29.0461416956092,
53.3973058954662));
#132435=CARTESIAN_POINT('Ctrl Pts',(9.99999999999997,-29.1094439341424,
53.3680938467391));
#132436=CARTESIAN_POINT('Ctrl Pts',(9.99999999999997,-29.1745617485033,
53.3427887894062));
#132437=CARTESIAN_POINT('Ctrl Pts',(9.99999999999996,-29.2411215698538,
53.3213755702336));
#132438=CARTESIAN_POINT('Ctrl Pts',(9.99999999999996,-29.3025810355913,
53.3016032063154));
#132439=CARTESIAN_POINT('Ctrl Pts',(9.99999999999997,-29.3652708265432,
53.2851497565554));
#132440=CARTESIAN_POINT('Ctrl Pts',(9.99999999999996,-29.4288933318821,
53.2720425880717));
#132441=CARTESIAN_POINT('Ctrl Pts',(9.99999999999995,-29.4429446720262,
53.2691478060805));
#132442=CARTESIAN_POINT('Ctrl Pts',(9.99999999999999,-29.4570414665537,
53.266416387187));
#132443=CARTESIAN_POINT('Ctrl Pts',(9.99999999999999,-29.4711804257353,
53.2638488655497));
#132444=CARTESIAN_POINT('Ctrl Pts',(9.99999999999998,-29.4823151499984,
53.2618268888891));
#132445=CARTESIAN_POINT('Ctrl Pts',(9.99999999999999,-29.4934754862078,
53.2599067415914));
#132446=CARTESIAN_POINT('Ctrl Pts',(9.99999999999998,-29.5046466791603,
53.2580905770623));
#132447=CARTESIAN_POINT('Ctrl Pts',(9.99999999999998,-29.5721359464321,
53.2471184621026));
#132448=CARTESIAN_POINT('Ctrl Pts',(9.99999999999995,-29.6401457101856,
53.2399139604603));
#132449=CARTESIAN_POINT('Ctrl Pts',(9.99999999999996,-29.7083244050125,
53.2364442314095));
#132450=CARTESIAN_POINT('Ctrl Pts',(9.99999999999996,-29.7757601728194,
53.2330123111708));
#132451=CARTESIAN_POINT('Ctrl Pts',(9.99999999999997,-29.8433622859179,
53.23323450567));
#132452=CARTESIAN_POINT('Ctrl Pts',(9.99999999999997,-29.91078197846,53.2371283063634));
#132453=CARTESIAN_POINT('Ctrl Pts',(9.99999999999997,-29.977606070675,53.2409877083688));
#132454=CARTESIAN_POINT('Ctrl Pts',(9.99999999999998,-30.044251924723,53.2484543816368));
#132455=CARTESIAN_POINT('Ctrl Pts',(9.99999999999999,-30.1103563112186,
53.2595900434352));
#132456=CARTESIAN_POINT('Ctrl Pts',(9.99999999999999,-30.1294385130765,
53.2628045494237));
#132457=CARTESIAN_POINT('Ctrl Pts',(9.99999999999997,-30.1484753926267,
53.26632506233));
#132458=CARTESIAN_POINT('Ctrl Pts',(9.99999999999998,-30.1674576666939,
53.2701537231559));
#132459=CARTESIAN_POINT('Ctrl Pts',(9.99999999999998,-30.1780436988077,
53.2722888902235));
#132460=CARTESIAN_POINT('Ctrl Pts',(9.99999999999996,-30.1886032905924,
53.2745179938254));
#132461=CARTESIAN_POINT('Ctrl Pts',(9.99999999999996,-30.1991346915138,
53.2768408806036));
#132462=CARTESIAN_POINT('Ctrl Pts',(9.99999999999999,-30.2629071303035,
53.2909070201399));
#132463=CARTESIAN_POINT('Ctrl Pts',(9.99999999999999,-30.3256519182632,
53.3084091752865));
#132464=CARTESIAN_POINT('Ctrl Pts',(9.99999999999999,-30.3870487756711,
53.3293566078869));
#132465=CARTESIAN_POINT('Ctrl Pts',(9.99999999999999,-30.4475549976041,
53.3500001727101));
#132466=CARTESIAN_POINT('Ctrl Pts',(9.99999999999998,-30.5067529547149,
53.3739900996769));
#132467=CARTESIAN_POINT('Ctrl Pts',(9.99999999999999,-30.5643079758142,
53.4013774025353));
#132468=CARTESIAN_POINT('Ctrl Pts',(10.,-30.6218629969135,53.4287647053938));
#132469=CARTESIAN_POINT('Ctrl Pts',(9.99999999999999,-30.6777759450102,
53.4595495876129));
#132470=CARTESIAN_POINT('Ctrl Pts',(10.,-30.7316710181693,53.4938218163979));
#132471=CARTESIAN_POINT('Ctrl Pts',(10.,-30.7357940686267,53.4964436910942));
#132472=CARTESIAN_POINT('Ctrl Pts',(10.,-30.7399052858608,53.4990859932845));
#132473=CARTESIAN_POINT('Ctrl Pts',(10.,-30.7440044894661,53.5017487719653));
#132474=CARTESIAN_POINT('Ctrl Pts',(10.,-30.753120839882,53.5076706109057));
#132475=CARTESIAN_POINT('Ctrl Pts',(9.99999999999998,-30.762177774796,53.5136937234875));
#132476=CARTESIAN_POINT('Ctrl Pts',(9.99999999999999,-30.7711742170104,
53.5198167964781));
#132477=CARTESIAN_POINT('Ctrl Pts',(-2.78423117894278E-16,-31.2690708798524,
56.0793586530485));
#132478=CARTESIAN_POINT('Ctrl Pts',(-2.57282377653238E-14,-31.3146241118499,
56.0368623223042));
#132479=CARTESIAN_POINT('Ctrl Pts',(-2.2197106541116E-14,-31.3574205812789,
55.9917717560589));
#132480=CARTESIAN_POINT('Ctrl Pts',(-2.5278390491934E-14,-31.3974616756518,
55.9444369337232));
#132481=CARTESIAN_POINT('Ctrl Pts',(-2.84724648645398E-14,-31.4389684745802,
55.8953694198661));
#132482=CARTESIAN_POINT('Ctrl Pts',(-7.29811795260109E-15,-31.4775150387688,
55.8438898979911));
#132483=CARTESIAN_POINT('Ctrl Pts',(-8.77076189453874E-15,-31.5130762861459,
55.7903375833125));
#132484=CARTESIAN_POINT('Ctrl Pts',(-1.01167848752535E-14,-31.5455799041824,
55.7413898070204));
#132485=CARTESIAN_POINT('Ctrl Pts',(-3.36001753813602E-15,-31.5755894343036,
55.6907093117701));
#132486=CARTESIAN_POINT('Ctrl Pts',(-6.01602101468757E-15,-31.6030614619887,
55.6385258325769));
#132487=CARTESIAN_POINT('Ctrl Pts',(-7.67020104658086E-15,-31.6165640542223,
55.6128774804074));
#132488=CARTESIAN_POINT('Ctrl Pts',(-1.92883565851348E-14,-31.6294532670974,
55.5868656683753));
#132489=CARTESIAN_POINT('Ctrl Pts',(-6.94583279781114E-15,-31.6417215732041,
55.5605158025313));
#132490=CARTESIAN_POINT('Ctrl Pts',(-1.26737980692756E-15,-31.6473278423374,
55.5484746586063));
#132491=CARTESIAN_POINT('Ctrl Pts',(-1.47443749393244E-14,-31.6528050246646,
55.5363612489351));
#132492=CARTESIAN_POINT('Ctrl Pts',(-1.35724764760425E-14,-31.6581439011687,
55.524197929143));
#132493=CARTESIAN_POINT('Ctrl Pts',(-6.89730998572226E-15,-31.6850933570533,
55.4628002081252));
#132494=CARTESIAN_POINT('Ctrl Pts',(-6.57763955012823E-15,-31.7085741592776,
55.4000241140312));
#132495=CARTESIAN_POINT('Ctrl Pts',(-5.54417622922188E-15,-31.7285626394371,
55.3362284938232));
#132496=CARTESIAN_POINT('Ctrl Pts',(-4.49070260999537E-15,-31.7489381439281,
55.2711976392667));
#132497=CARTESIAN_POINT('Ctrl Pts',(-3.16205974643209E-14,-31.7656853518822,
55.2051065542478));
#132498=CARTESIAN_POINT('Ctrl Pts',(-2.57155408078802E-14,-31.7787394756354,
55.1382984849778));
#132499=CARTESIAN_POINT('Ctrl Pts',(-2.08116559556361E-14,-31.7895803402464,
55.0828173781973));
#132500=CARTESIAN_POINT('Ctrl Pts',(-1.68020975472041E-14,-31.7978736664125,
55.0268408524174));
#132501=CARTESIAN_POINT('Ctrl Pts',(-1.25038868148408E-14,-31.8035578588702,
54.9705533929035));
#132502=CARTESIAN_POINT('Ctrl Pts',(-1.02026785998301E-14,-31.8061882803694,
54.9445057626131));
#132503=CARTESIAN_POINT('Ctrl Pts',(-9.94370814337888E-15,-31.808259630761,
54.9183914347958));
#132504=CARTESIAN_POINT('Ctrl Pts',(-2.18020046460765E-14,-31.8097640080344,
54.8922282921563));
#132505=CARTESIAN_POINT('Ctrl Pts',(-2.8149256454812E-14,-31.8105739898639,
54.8781416195417));
#132506=CARTESIAN_POINT('Ctrl Pts',(-2.39741397133629E-14,-31.8112192935178,
54.8640433553622));
#132507=CARTESIAN_POINT('Ctrl Pts',(-1.78329573330416E-14,-31.811698521278,
54.8499553064024));
#132508=CARTESIAN_POINT('Ctrl Pts',(1.15714359936816E-14,-31.8139930959514,
54.7825007826369));
#132509=CARTESIAN_POINT('Ctrl Pts',(-9.17816564628055E-15,-31.812490761091,
54.7151643158931));
#132510=CARTESIAN_POINT('Ctrl Pts',(-6.80011602582908E-16,-31.8071420452598,
54.6482666402681));
#132511=CARTESIAN_POINT('Ctrl Pts',(7.39918467707698E-15,-31.8021719907044,
54.5861049723127));
#132512=CARTESIAN_POINT('Ctrl Pts',(1.51061130160261E-14,-31.7938807595678,
54.5243213359004));
#132513=CARTESIAN_POINT('Ctrl Pts',(1.60982338570648E-14,-31.7821961531115,
54.4631612860264));
#132514=CARTESIAN_POINT('Ctrl Pts',(1.69344470150937E-14,-31.7694646642199,
54.3965216008566));
#132515=CARTESIAN_POINT('Ctrl Pts',(1.19364270054881E-14,-31.7527055889607,
54.3306214152988));
#132516=CARTESIAN_POINT('Ctrl Pts',(4.9960036108132E-16,-31.7321642059902,
54.2656743472661));
#132517=CARTESIAN_POINT('Ctrl Pts',(-4.13176169865794E-15,-31.7242361536314,
54.240607692472));
#132518=CARTESIAN_POINT('Ctrl Pts',(-1.3612586526406E-14,-31.7157441295239,
54.2156830625258));
#132519=CARTESIAN_POINT('Ctrl Pts',(-1.49880108324396E-15,-31.7067002269016,
54.1909130590085));
#132520=CARTESIAN_POINT('Ctrl Pts',(3.98752837147791E-15,-31.702733264022,
54.1800480941163));
#132521=CARTESIAN_POINT('Ctrl Pts',(-1.32089167663491E-14,-31.6986602242431,
54.1692134541154));
#132522=CARTESIAN_POINT('Ctrl Pts',(-1.05193631583234E-14,-31.6944872093316,
54.1584227272008));
#132523=CARTESIAN_POINT('Ctrl Pts',(4.54181674810102E-15,-31.6694832150762,
54.0937665302998));
#132524=CARTESIAN_POINT('Ctrl Pts',(-2.05732350039661E-14,-31.640852147275,
54.0305697527002));
#132525=CARTESIAN_POINT('Ctrl Pts',(-4.52415882534751E-15,-31.6088988590651,
53.9690455844801));
#132526=CARTESIAN_POINT('Ctrl Pts',(1.20570199622642E-14,-31.5758861685673,
53.9054815997583));
#132527=CARTESIAN_POINT('Ctrl Pts',(-1.76645667684946E-14,-31.5393271021827,
53.8437021556787));
#132528=CARTESIAN_POINT('Ctrl Pts',(-8.93729534823251E-15,-31.4995017172175,
53.7839459944069));
#132529=CARTESIAN_POINT('Ctrl Pts',(-2.19864240011066E-15,-31.4687510467178,
53.7378060254599));
#132530=CARTESIAN_POINT('Ctrl Pts',(-1.86107330608832E-14,-31.4360517893389,
53.6928722834116));
#132531=CARTESIAN_POINT('Ctrl Pts',(-1.52100554373646E-14,-31.4015126326392,
53.6492609538454));
#132532=CARTESIAN_POINT('Ctrl Pts',(-1.30940809355439E-14,-31.3802217602078,
53.6223777481425));
#132533=CARTESIAN_POINT('Ctrl Pts',(-5.96119017066866E-15,-31.3582314248551,
53.595997163054));
#132534=CARTESIAN_POINT('Ctrl Pts',(-1.52655665885959E-14,-31.3355641610242,
53.570148108709));
#132535=CARTESIAN_POINT('Ctrl Pts',(-2.03883579394625E-14,-31.3228721183306,
53.555674491435));
#132536=CARTESIAN_POINT('Ctrl Pts',(1.45111025983856E-14,-31.3099633641148,
53.5413629717455));
#132537=CARTESIAN_POINT('Ctrl Pts',(1.47937218031302E-14,-31.2968655882308,
53.5272440845563));
#132538=CARTESIAN_POINT('Ctrl Pts',(1.63603910997093E-14,-31.2460184014874,
53.4724328173702));
#132539=CARTESIAN_POINT('Ctrl Pts',(-5.80558094253327E-15,-31.1922776399754,
53.4204635517656));
#132540=CARTESIAN_POINT('Ctrl Pts',(-2.99760216648792E-15,-31.1359279003417,
53.3715998536437));
#132541=CARTESIAN_POINT('Ctrl Pts',(-8.95100641520165E-16,-31.0937354826062,
53.335012682582));
#132542=CARTESIAN_POINT('Ctrl Pts',(-2.28577618870274E-15,-31.0500792097546,
53.3001668168172));
#132543=CARTESIAN_POINT('Ctrl Pts',(-1.52655665885959E-15,-31.0050621224658,
53.2671826644093));
#132544=CARTESIAN_POINT('Ctrl Pts',(-1.22529459397018E-15,-30.9910114153834,
53.2568876699582));
#132545=CARTESIAN_POINT('Ctrl Pts',(5.50416399254457E-15,-30.9768280471771,
53.2467741178013));
#132546=CARTESIAN_POINT('Ctrl Pts',(1.66533453693773E-15,-30.962514910112,
53.2368458953558));
#132547=CARTESIAN_POINT('Ctrl Pts',(-2.32875220709882E-15,-30.9487200109087,
53.2272771455227));
#132548=CARTESIAN_POINT('Ctrl Pts',(2.32032892379646E-14,-30.9348115999123,
53.2178854875332));
#132549=CARTESIAN_POINT('Ctrl Pts',(1.97897254139434E-14,-30.9207976678547,
53.2086771606816));
#132550=CARTESIAN_POINT('Ctrl Pts',(4.17236467677409E-15,-30.8578426129519,
53.1673104179198));
#132551=CARTESIAN_POINT('Ctrl Pts',(1.73679733454129E-14,-30.7927302716737,
53.129619436727));
#132552=CARTESIAN_POINT('Ctrl Pts',(1.97064586870965E-15,-30.7257220056234,
53.0958834398336));
#132553=CARTESIAN_POINT('Ctrl Pts',(-9.63241745287261E-15,-30.6744687584743,
53.070079468346));
#132554=CARTESIAN_POINT('Ctrl Pts',(-1.67306283423615E-14,-30.622105344157,
53.0465897299349));
#132555=CARTESIAN_POINT('Ctrl Pts',(-1.8623991238087E-14,-30.5687348286521,
53.0255544534855));
#132556=CARTESIAN_POINT('Ctrl Pts',(-1.893565290737E-14,-30.556454937019,
53.0207144980752));
#132557=CARTESIAN_POINT('Ctrl Pts',(-1.99912525927446E-14,-30.5441216860115,
53.0160045481786));
#132558=CARTESIAN_POINT('Ctrl Pts',(5.27355936696949E-16,-30.5317369366261,
53.0114240379353));
#132559=CARTESIAN_POINT('Ctrl Pts',(10.,-30.7922981853442,53.5344558739157));
#132560=CARTESIAN_POINT('Ctrl Pts',(10.0002899899451,-30.7848609529314,
53.530435179049));
#132561=CARTESIAN_POINT('Ctrl Pts',(10.0005799798902,-30.777393114057,53.5264710981355));
#132562=CARTESIAN_POINT('Ctrl Pts',(10.0008699698353,-30.7698955341219,
53.5225640905477));
#132563=CARTESIAN_POINT('Ctrl Pts',(0.00154683520447944,-29.4691384916359,
53.0122371971775));
#132564=CARTESIAN_POINT('Ctrl Pts',(0.0385919254839992,-28.8081756493506,
53.1887571174265));
#132565=CARTESIAN_POINT('Ctrl Pts',(0.112682106043039,-27.6876746937628,
54.2503605089641));
#132566=CARTESIAN_POINT('Ctrl Pts',(0.223817376881599,-28.1162794172484,
56.540242738843));
#132567=CARTESIAN_POINT('Ctrl Pts',(0.334952647720158,-30.2723120807304,
57.4159505201799));
#132568=CARTESIAN_POINT('Ctrl Pts',(0.446087918558717,-32.1774584443673,
56.082555317456));
#132569=CARTESIAN_POINT('Ctrl Pts',(0.557223189397277,-32.0904669771016,
53.7572516909355));
#132570=CARTESIAN_POINT('Ctrl Pts',(0.668358460235836,-30.0897123148979,
52.5699426008396));
#132571=CARTESIAN_POINT('Ctrl Pts',(0.779493731074396,-28.0070571020679,
53.6065233138136));
#132572=CARTESIAN_POINT('Ctrl Pts',(0.890629001912955,-27.7483801793046,
55.9186517854682));
#132573=CARTESIAN_POINT('Ctrl Pts',(1.00176427275152,-29.5506010031038,
57.3898946665584));
#132574=CARTESIAN_POINT('Ctrl Pts',(1.11289954359007,-31.7641170624246,
56.673769327145));
#132575=CARTESIAN_POINT('Ctrl Pts',(1.22403481442863,-32.363000089887,54.4256724031027));
#132576=CARTESIAN_POINT('Ctrl Pts',(1.33517008526719,-30.7990888352776,
52.7032502602688));
#132577=CARTESIAN_POINT('Ctrl Pts',(1.44630535610575,-28.503797543915,53.082973959131));
#132578=CARTESIAN_POINT('Ctrl Pts',(1.55744062694431,-27.5779364648995,
55.2172998549449));
#132579=CARTESIAN_POINT('Ctrl Pts',(1.66857589778287,-28.8689227885836,
57.1527361723464));
#132580=CARTESIAN_POINT('Ctrl Pts',(1.77971116862143,-31.195151776353,57.1178342918897));
#132581=CARTESIAN_POINT('Ctrl Pts',(1.89084643945999,-32.4274922356383,
55.1445380547168));
#132582=CARTESIAN_POINT('Ctrl Pts',(2.00198171029855,-31.4380173232809,
53.0389503543588));
#132583=CARTESIAN_POINT('Ctrl Pts',(2.11311698113711,-29.1323657220718,
52.7282560762878));
#132584=CARTESIAN_POINT('Ctrl Pts',(2.22425225197567,-27.6208353047203,
54.4968250518511));
#132585=CARTESIAN_POINT('Ctrl Pts',(2.33538752281423,-28.2868873243009,
56.725935863788));
#132586=CARTESIAN_POINT('Ctrl Pts',(2.44652279365279,-30.5209031087717,
57.3753462101905));
#132587=CARTESIAN_POINT('Ctrl Pts',(2.55765806449135,-32.2781509557601,
55.850669081196));
#132588=CARTESIAN_POINT('Ctrl Pts',(2.66879333532991,-31.9502714085785,
53.5473985086807));
#132589=CARTESIAN_POINT('Ctrl Pts',(2.77992860616847,-29.8373633829036,
52.573653158907));
#132590=CARTESIAN_POINT('Ctrl Pts',(2.89106387700702,-27.8733120707697,
53.8206747210973));
#132591=CARTESIAN_POINT('Ctrl Pts',(3.00219914784558,-27.8557583098495,
56.1470994881393));
#132592=CARTESIAN_POINT('Ctrl Pts',(3.11333441868415,-29.8007685626502,
57.4236164086336));
#132593=CARTESIAN_POINT('Ctrl Pts',(3.2244696895227,-31.9281297375949,56.4818655056094));
#132594=CARTESIAN_POINT('Ctrl Pts',(3.33560496036126,-32.2907280807803,
54.1838048507812));
#132595=CARTESIAN_POINT('Ctrl Pts',(3.44674023119983,-30.5566875434458,
52.6327846230853));
#132596=CARTESIAN_POINT('Ctrl Pts',(3.55787550203837,-28.3131265799599,
53.2484099433732));
#132597=CARTESIAN_POINT('Ctrl Pts',(3.66901077287695,-27.613513337149,55.4672162986708));
#132598=CARTESIAN_POINT('Ctrl Pts',(3.7801460437155,-29.0981841074383,57.2583927376871));
#132599=CARTESIAN_POINT('Ctrl Pts',(3.89128131455406,-31.4082615592521,
56.9825259247851));
#132600=CARTESIAN_POINT('Ctrl Pts',(4.00241658539262,-32.4293968778352,
54.8921089824078));
#132601=CARTESIAN_POINT('Ctrl Pts',(4.11355185623118,-31.2269736723593,
52.9004416490485));
#132602=CARTESIAN_POINT('Ctrl Pts',(4.22468712706974,-28.9015360294886,
52.83044092793));
#132603=CARTESIAN_POINT('Ctrl Pts',(4.3358223979083,-27.5814915141413,54.7461765071108));
#132604=CARTESIAN_POINT('Ctrl Pts',(4.44695766874686,-28.4750396844126,
56.8942295789044));
#132605=CARTESIAN_POINT('Ctrl Pts',(4.55809293958541,-30.7643410720823,
57.3085476792218));
#132606=CARTESIAN_POINT('Ctrl Pts',(4.66922821042398,-32.3540626086281,
55.609917122544));
#132607=CARTESIAN_POINT('Ctrl Pts',(4.78036348126253,-31.789176955488,53.3530466054973));
#132608=CARTESIAN_POINT('Ctrl Pts',(4.8914987521011,-29.586708037661,52.6035861343293));
#132609=CARTESIAN_POINT('Ctrl Pts',(5.00263402293966,-27.7625136101689,
54.0474957653462));
#132610=CARTESIAN_POINT('Ctrl Pts',(5.11376929377821,-27.9862274433511,
56.363205689469));
#132611=CARTESIAN_POINT('Ctrl Pts',(5.22490456461678,-30.0530905679093,
57.4312118487108));
#132612=CARTESIAN_POINT('Ctrl Pts',(5.33603983545533,-32.0713613912677,
56.2739982921804));
#132613=CARTESIAN_POINT('Ctrl Pts',(5.44717510629389,-32.193773485251,53.9507299884574));
#132614=CARTESIAN_POINT('Ctrl Pts',(5.55831037713245,-30.3082865086915,
52.5878289674504));
#132615=CARTESIAN_POINT('Ctrl Pts',(5.66944564797101,-28.1406335754259,
53.4327201395797));
#132616=CARTESIAN_POINT('Ctrl Pts',(5.78058091880957,-27.6748063506032,
55.7120984163146));
#132617=CARTESIAN_POINT('Ctrl Pts',(5.89171618964813,-29.3371633703456,
57.3397130730287));
#132618=CARTESIAN_POINT('Ctrl Pts',(6.00285146048669,-31.6061960845262,
56.8258542657522));
#132619=CARTESIAN_POINT('Ctrl Pts',(6.11398673132524,-32.405122770481,54.6408424849358));
#132620=CARTESIAN_POINT('Ctrl Pts',(6.22512200216382,-31.002708339015,52.7845574598779));
#132621=CARTESIAN_POINT('Ctrl Pts',(6.33625727300236,-28.6825432120152,
52.9560045808502));
#132622=CARTESIAN_POINT('Ctrl Pts',(6.44739254384094,-27.5682091691533,
54.9982631278413));
#132623=CARTESIAN_POINT('Ctrl Pts',(6.55852781467948,-28.6796247681038,
57.0421113849897));
#132624=CARTESIAN_POINT('Ctrl Pts',(6.66966308551805,-30.9995426206869,
57.216872619512));
#132625=CARTESIAN_POINT('Ctrl Pts',(6.78079835635661,-32.4046072705466,
55.3625927966234));
#132626=CARTESIAN_POINT('Ctrl Pts',(6.89193362719516,-31.6088026255414,
53.1764420015434));
#132627=CARTESIAN_POINT('Ctrl Pts',(7.00306889803373,-29.3405062587718,
52.6593424712286));
#132628=CARTESIAN_POINT('Ctrl Pts',(7.11420416887228,-27.675825934788,54.2845808386533));
#132629=CARTESIAN_POINT('Ctrl Pts',(7.22533943971084,-28.1383966587829,
56.5646222104514));
#132630=CARTESIAN_POINT('Ctrl Pts',(7.3364747105494,-30.3048404778189,57.4126089498457));
#132631=CARTESIAN_POINT('Ctrl Pts',(7.44760998138796,-32.1922723955041,
56.0524026826328));
#132632=CARTESIAN_POINT('Ctrl Pts',(7.55874525222652,-32.0731791470605,
53.728961887316));
#132633=CARTESIAN_POINT('Ctrl Pts',(7.66988052306508,-30.0565634300485,
52.5688664698714));
#132634=CARTESIAN_POINT('Ctrl Pts',(7.78101579390364,-27.988176796027,53.6339190862362));
#132635=CARTESIAN_POINT('Ctrl Pts',(7.8921510647422,-27.7611552715967,55.9493070776374));
#132636=CARTESIAN_POINT('Ctrl Pts',(8.00328633558076,-29.5832852453598,
57.395821046943));
#132637=CARTESIAN_POINT('Ctrl Pts',(8.11442160641932,-31.7868225176538,
56.6495074978805));
#132638=CARTESIAN_POINT('Ctrl Pts',(8.22555687725788,-32.3549314306192,
54.3934462168881));
#132639=CARTESIAN_POINT('Ctrl Pts',(8.33669214809644,-30.7676380353678,
52.6925465010098));
#132640=CARTESIAN_POINT('Ctrl Pts',(8.447827418935,-28.4777469933738,53.1035940201946));
#132641=CARTESIAN_POINT('Ctrl Pts',(8.55896268977356,-27.581131598138,55.2503684093247));
#132642=CARTESIAN_POINT('Ctrl Pts',(8.67009796061211,-28.8984376095163,
57.1679878447293));
#132643=CARTESIAN_POINT('Ctrl Pts',(8.78123323145067,-31.2239740330287,
57.1013086868512));
#132644=CARTESIAN_POINT('Ctrl Pts',(8.89236850228924,-32.4292387518736,
55.1113616631365));
#132645=CARTESIAN_POINT('Ctrl Pts',(9.00350377312779,-31.4110951335146,
53.0194869004384));
#132646=CARTESIAN_POINT('Ctrl Pts',(9.11463904396635,-29.1014050665648,
52.740323050515));
#132647=CARTESIAN_POINT('Ctrl Pts',(9.22577431480492,-27.6141950937383,
54.5293717763318));
#132648=CARTESIAN_POINT('Ctrl Pts',(9.33690958564347,-28.3106025739419,
56.749185312287));
#132649=CARTESIAN_POINT('Ctrl Pts',(9.44804485648204,-30.5533523395227,
57.367994902382));
#132650=CARTESIAN_POINT('Ctrl Pts',(9.55918012732059,-32.2894669018336,
55.8194928724932));
#132651=CARTESIAN_POINT('Ctrl Pts',(9.67031539815916,-31.9304288651689,
53.5208380958941));
#132652=CARTESIAN_POINT('Ctrl Pts',(9.78145066899771,-29.8038652797079,
52.5762049459999));
#132653=CARTESIAN_POINT('Ctrl Pts',(9.89258593983627,-27.8581251142671,
53.8496336413402));
#132654=CARTESIAN_POINT('Ctrl Pts',(10.0037212106749,-27.8701762214051,
56.1766909537225));
#132655=CARTESIAN_POINT('Ctrl Pts',(10.1148694181389,-29.837170584603,57.4254741206559));
#132656=CARTESIAN_POINT('Ctrl Pts',(10.1889725353234,-31.2393300826299,
56.7791900932959));
#132657=CARTESIAN_POINT('Ctrl Pts',(10.2260305622284,-31.6487083722557,
56.2307621881824));
#132658=CARTESIAN_POINT('Ctrl Pts',(-0.0743643433070923,-29.503063713713,
53.1392671163936));
#132659=CARTESIAN_POINT('Ctrl Pts',(-0.0373192530275725,-28.8843403460478,
53.3045063591003));
#132660=CARTESIAN_POINT('Ctrl Pts',(0.0367709275314672,-27.8354460960829,
54.298266951248));
#132661=CARTESIAN_POINT('Ctrl Pts',(0.147906198370027,-28.23666041699,56.441812025475));
#132662=CARTESIAN_POINT('Ctrl Pts',(0.259041469208586,-30.2549097118121,
57.2615568475682));
#132663=CARTESIAN_POINT('Ctrl Pts',(0.370176740047145,-32.0383058402982,
56.0133735648203));
#132664=CARTESIAN_POINT('Ctrl Pts',(0.481312010885705,-31.9568736475312,
53.8366707328262));
#132665=CARTESIAN_POINT('Ctrl Pts',(0.592447281724263,-30.0839791619795,
52.7252377873014));
#132666=CARTESIAN_POINT('Ctrl Pts',(0.703582552562825,-28.1344180603106,
53.6955747995465));
#132667=CARTESIAN_POINT('Ctrl Pts',(0.814717823401383,-27.8922721384068,
55.8599444477868));
#132668=CARTESIAN_POINT('Ctrl Pts',(0.925853094239943,-29.579320283991,
57.2371661186667));
#132669=CARTESIAN_POINT('Ctrl Pts',(1.0369883650785,-31.6513794422169,56.5668054670145));
#132670=CARTESIAN_POINT('Ctrl Pts',(1.14812363591707,-32.2119902661294,
54.4623753679303));
#132671=CARTESIAN_POINT('Ctrl Pts',(1.25925890675562,-30.7480222844559,
52.8500262908311));
#132672=CARTESIAN_POINT('Ctrl Pts',(1.37039417759418,-28.5994138200912,
53.2054833766335));
#132673=CARTESIAN_POINT('Ctrl Pts',(1.48152944843274,-27.7327207956875,
55.2034130959311));
#132674=CARTESIAN_POINT('Ctrl Pts',(1.5926647192713,-28.941205380143,57.0151634691656));
#132675=CARTESIAN_POINT('Ctrl Pts',(1.70379999010986,-31.1187744372733,
56.9824920273952));
#132676=CARTESIAN_POINT('Ctrl Pts',(1.81493526094842,-32.2723609784515,
55.1353012094613));
#132677=CARTESIAN_POINT('Ctrl Pts',(1.92607053178698,-31.3461194247246,
53.1642731432303));
#132678=CARTESIAN_POINT('Ctrl Pts',(2.03720580262554,-29.1878127362114,
52.8734340858064));
#132679=CARTESIAN_POINT('Ctrl Pts',(2.1483410734641,-27.7728781433397,54.528980937314));
#132680=CARTESIAN_POINT('Ctrl Pts',(2.25947634430266,-28.3963654594653,
56.6156382502912));
#132681=CARTESIAN_POINT('Ctrl Pts',(2.37061161514122,-30.4876142879261,
57.2235473955822));
#132682=CARTESIAN_POINT('Ctrl Pts',(2.48174688597978,-32.1325634986141,
55.796306244488));
#132683=CARTESIAN_POINT('Ctrl Pts',(2.59288215681834,-31.8256374134512,
53.6402284227095));
#132684=CARTESIAN_POINT('Ctrl Pts',(2.7040174276569,-29.8477568344271,52.7287112185391));
#132685=CARTESIAN_POINT('Ctrl Pts',(2.81515269849545,-28.0092201355873,
53.8960406524328));
#132686=CARTESIAN_POINT('Ctrl Pts',(2.92628796933401,-27.9927881648669,
56.0737929773703));
#132687=CARTESIAN_POINT('Ctrl Pts',(3.03742324017257,-29.8135006418279,
57.2687328399489));
#132688=CARTESIAN_POINT('Ctrl Pts',(3.14855851101114,-31.8049107275313,
56.3871654462264));
#132689=CARTESIAN_POINT('Ctrl Pts',(3.25969378184969,-32.144336870202,54.2359645972673));
#132690=CARTESIAN_POINT('Ctrl Pts',(3.37082905268826,-30.5211118834263,
52.7840638288688));
#132691=CARTESIAN_POINT('Ctrl Pts',(3.48196432352681,-28.4209278699183,
53.3603470130664));
#132692=CARTESIAN_POINT('Ctrl Pts',(3.59309959436537,-27.7660240932422,
55.4373583857486));
#132693=CARTESIAN_POINT('Ctrl Pts',(3.70423486520393,-29.1558155309749,
57.1140679487238));
#132694=CARTESIAN_POINT('Ctrl Pts',(3.81537013604249,-31.3182652317965,
56.8558306733639));
#132695=CARTESIAN_POINT('Ctrl Pts',(3.92650540688105,-32.2741439026325,
54.8990038630393));
#132696=CARTESIAN_POINT('Ctrl Pts',(4.03764067771961,-31.1485627240013,
53.0346159717254));
#132697=CARTESIAN_POINT('Ctrl Pts',(4.14877594855817,-28.9717344401026,
52.9690887149137));
#132698=CARTESIAN_POINT('Ctrl Pts',(4.25991121939673,-27.7360486560428,
54.7623973448038));
#132699=CARTESIAN_POINT('Ctrl Pts',(4.37104649023528,-28.5724937596281,
56.7731769915215));
#132700=CARTESIAN_POINT('Ctrl Pts',(4.48218176107385,-30.7154951109333,
57.161017689838));
#132701=CARTESIAN_POINT('Ctrl Pts',(4.5933170319124,-32.2036239433209,55.5709397743939));
#132702=CARTESIAN_POINT('Ctrl Pts',(4.70445230275097,-31.6748378583903,
53.4582967673173));
#132703=CARTESIAN_POINT('Ctrl Pts',(4.81558757358953,-29.6131198633146,
52.7567312979939));
#132704=CARTESIAN_POINT('Ctrl Pts',(4.92672284442808,-27.905502358597,54.1083664767859));
#132705=CARTESIAN_POINT('Ctrl Pts',(5.03785811526665,-28.1149195412349,
56.2760887012839));
#132706=CARTESIAN_POINT('Ctrl Pts',(5.14899338610521,-30.0496977634243,
57.2758428860254));
#132707=CARTESIAN_POINT('Ctrl Pts',(5.26012865694376,-31.9389890227805,
56.1925821896618));
#132708=CARTESIAN_POINT('Ctrl Pts',(5.37126392778233,-32.0535782525933,
54.0177846111785));
#132709=CARTESIAN_POINT('Ctrl Pts',(5.48239919862088,-30.2885851588932,
52.7419811082214));
#132710=CARTESIAN_POINT('Ctrl Pts',(5.59353446945944,-28.2594581989532,
53.5328786865529));
#132711=CARTESIAN_POINT('Ctrl Pts',(5.704669740298,-27.8234001169346,55.6665910729988));
#132712=CARTESIAN_POINT('Ctrl Pts',(5.81580501113656,-29.3795225911736,
57.1901914287792));
#132713=CARTESIAN_POINT('Ctrl Pts',(5.92694028197513,-31.5035505583231,
56.709171269396));
#132714=CARTESIAN_POINT('Ctrl Pts',(6.03807555281367,-32.2514210557666,
54.6637947959758));
#132715=CARTESIAN_POINT('Ctrl Pts',(6.14921082365225,-30.9386292853566,
52.9261374746062));
#132716=CARTESIAN_POINT('Ctrl Pts',(6.26034609449079,-28.7667365720634,
53.0866281002179));
#132717=CARTESIAN_POINT('Ctrl Pts',(6.37148136532936,-27.7236151322564,
54.9983741243495));
#132718=CARTESIAN_POINT('Ctrl Pts',(6.48261663616792,-28.7640046341545,
56.9116082666613));
#132719=CARTESIAN_POINT('Ctrl Pts',(6.59375190700648,-30.9356658753436,
57.0752012141665));
#132720=CARTESIAN_POINT('Ctrl Pts',(6.70488717784504,-32.2509384993579,
55.3394209505671));
#132721=CARTESIAN_POINT('Ctrl Pts',(6.8160224486836,-31.5059905257943,53.2929782527002));
#132722=CARTESIAN_POINT('Ctrl Pts',(6.92715771952215,-29.382651849057,52.8089244718427));
#132723=CARTESIAN_POINT('Ctrl Pts',(7.03829299036072,-27.8243545435983,
54.3303003974168));
#132724=CARTESIAN_POINT('Ctrl Pts',(7.14942826119927,-28.2573642346483,
56.4646335031895));
#132725=CARTESIAN_POINT('Ctrl Pts',(7.26056353203784,-30.2853593499821,
57.258428823543));
#132726=CARTESIAN_POINT('Ctrl Pts',(7.37169880287639,-32.0521730914497,
55.9851478635125));
#132727=CARTESIAN_POINT('Ctrl Pts',(7.48283407371496,-31.9406906131178,
53.8101888166788));
#132728=CARTESIAN_POINT('Ctrl Pts',(7.59396934455351,-30.0529486889238,
52.7242304275315));
#132729=CARTESIAN_POINT('Ctrl Pts',(7.70510461539206,-28.1167443186283,
53.721219818432));
#132730=CARTESIAN_POINT('Ctrl Pts',(7.81623988623064,-27.9042308259751,
55.8886406836328));
#132731=CARTESIAN_POINT('Ctrl Pts',(7.92737515706918,-29.6099158078912,
57.2427137679369));
#132732=CARTESIAN_POINT('Ctrl Pts',(8.03851042790776,-31.6726338832006,
56.5440941135952));
#132733=CARTESIAN_POINT('Ctrl Pts',(8.1496456987463,-32.204437242396,54.4322086275537));
#132734=CARTESIAN_POINT('Ctrl Pts',(8.26078096958488,-30.7185813785667,
52.8400065657396));
#132735=CARTESIAN_POINT('Ctrl Pts',(8.37191624042342,-28.5750280553716,
53.2247856925982));
#132736=CARTESIAN_POINT('Ctrl Pts',(8.483051511262,-27.7357117408224,55.2343683721141));
#132737=CARTESIAN_POINT('Ctrl Pts',(8.59418678210054,-28.9688340276785,
57.0294404685603));
#132738=CARTESIAN_POINT('Ctrl Pts',(8.70532205293911,-31.1457547795456,
56.9670225072527));
#132739=CARTESIAN_POINT('Ctrl Pts',(8.81645732377767,-32.2739958818645,
55.1042449875192));
#132740=CARTESIAN_POINT('Ctrl Pts',(8.92759259461623,-31.3209177237342,
53.146053520302));
#132741=CARTESIAN_POINT('Ctrl Pts',(9.03872786545478,-29.1588306515692,
52.884729908285));
#132742=CARTESIAN_POINT('Ctrl Pts',(9.14986313629334,-27.7666622815123,
54.5594477316463));
#132743=CARTESIAN_POINT('Ctrl Pts',(9.26099840713191,-28.4185651629648,
56.6374019201245));
#132744=CARTESIAN_POINT('Ctrl Pts',(9.37213367797046,-30.5179898189604,
57.2166658802639));
#132745=CARTESIAN_POINT('Ctrl Pts',(9.48326894880902,-32.143156288125,55.7671223817873));
#132746=CARTESIAN_POINT('Ctrl Pts',(9.59440421964759,-31.8070629271169,
53.6153653789881));
#132747=CARTESIAN_POINT('Ctrl Pts',(9.70553949048613,-29.816399460164,52.7310999311908));
#132748=CARTESIAN_POINT('Ctrl Pts',(9.81667476132471,-27.9950037163415,
53.9231489246537));
#132749=CARTESIAN_POINT('Ctrl Pts',(9.92781003216325,-28.0062846857326,
56.1014933715052));
#132750=CARTESIAN_POINT('Ctrl Pts',(10.0389582396273,-29.8475763570898,
57.2704718330739));
#132751=CARTESIAN_POINT('Ctrl Pts',(10.1130613568119,-31.1601294858308,
56.66548921636));
#132752=CARTESIAN_POINT('Ctrl Pts',(10.1501193837169,-31.5433460568722,
56.1521091310284));
#132753=CARTESIAN_POINT('Ctrl Pts',(-0.150275521818664,-29.5369889357901,
53.2662970356098));
#132754=CARTESIAN_POINT('Ctrl Pts',(-0.113230431539144,-28.960505042745,
53.4202556007742));
#132755=CARTESIAN_POINT('Ctrl Pts',(-0.0391402509801043,-27.9832174984029,
54.3461733935319));
#132756=CARTESIAN_POINT('Ctrl Pts',(0.0719950198584549,-28.3570414167314,
56.3433813121067));
#132757=CARTESIAN_POINT('Ctrl Pts',(0.183130290697014,-30.2375073428938,
57.1071631749565));
#132758=CARTESIAN_POINT('Ctrl Pts',(0.294265561535574,-31.8991532362291,
55.9441918121845));
#132759=CARTESIAN_POINT('Ctrl Pts',(0.405400832374133,-31.8232803179608,
53.9160897747171));
#132760=CARTESIAN_POINT('Ctrl Pts',(0.516536103212693,-30.078246009061,
52.8805329737631));
#132761=CARTESIAN_POINT('Ctrl Pts',(0.627671374051251,-28.2617790185534,
53.7846262852794));
#132762=CARTESIAN_POINT('Ctrl Pts',(0.738806644889812,-28.0361640975088,
55.8012371101055));
#132763=CARTESIAN_POINT('Ctrl Pts',(0.84994191572837,-29.6080395648783,
57.0844375707751));
#132764=CARTESIAN_POINT('Ctrl Pts',(0.96107718656693,-31.5386418220091,
56.4598416068841));
#132765=CARTESIAN_POINT('Ctrl Pts',(1.07221245740549,-32.0609804423719,
54.4990783327577));
#132766=CARTESIAN_POINT('Ctrl Pts',(1.18334772824404,-30.6969557336342,
52.9968023213935));
#132767=CARTESIAN_POINT('Ctrl Pts',(1.29448299908261,-28.6950300962674,
53.3279927941359));
#132768=CARTESIAN_POINT('Ctrl Pts',(1.40561826992116,-27.8875051264756,
55.1895263369173));
#132769=CARTESIAN_POINT('Ctrl Pts',(1.51675354075972,-29.0134879717024,
56.8775907659846));
#132770=CARTESIAN_POINT('Ctrl Pts',(1.62788881159828,-31.0423970981937,
56.8471497629006));
#132771=CARTESIAN_POINT('Ctrl Pts',(1.73902408243684,-32.1172297212648,
55.1260643642059));
#132772=CARTESIAN_POINT('Ctrl Pts',(1.8501593532754,-31.2542215261682,53.2895959321017));
#132773=CARTESIAN_POINT('Ctrl Pts',(1.96129462411396,-29.2432597503511,
53.0186120953251));
#132774=CARTESIAN_POINT('Ctrl Pts',(2.07242989495252,-27.9249209819592,
54.5611368227768));
#132775=CARTESIAN_POINT('Ctrl Pts',(2.18356516579108,-28.5058435946297,
56.5053406367943));
#132776=CARTESIAN_POINT('Ctrl Pts',(2.29470043662964,-30.4543254670805,
57.0717485809739));
#132777=CARTESIAN_POINT('Ctrl Pts',(2.4058357074682,-31.9869760414681,55.7419434077801));
#132778=CARTESIAN_POINT('Ctrl Pts',(2.51697097830676,-31.7010034183238,
53.7330583367382));
#132779=CARTESIAN_POINT('Ctrl Pts',(2.62810624914532,-29.8581502859505,
52.8837692781711));
#132780=CARTESIAN_POINT('Ctrl Pts',(2.73924151998388,-28.145128200405,53.9714065837682));
#132781=CARTESIAN_POINT('Ctrl Pts',(2.85037679082244,-28.1298180198844,
56.0004864666014));
#132782=CARTESIAN_POINT('Ctrl Pts',(2.961512061661,-29.8262327210055,57.1138492712643));
#132783=CARTESIAN_POINT('Ctrl Pts',(3.07264733249956,-31.6816917174677,
56.2924653868433));
#132784=CARTESIAN_POINT('Ctrl Pts',(3.18378260333811,-31.9979456596237,
54.2881243437535));
#132785=CARTESIAN_POINT('Ctrl Pts',(3.29491787417668,-30.4855362234068,
52.9353430346521));
#132786=CARTESIAN_POINT('Ctrl Pts',(3.40605314501523,-28.5287291598767,
53.4722840827597));
#132787=CARTESIAN_POINT('Ctrl Pts',(3.5171884158538,-27.9185348493353,55.4075004728264));
#132788=CARTESIAN_POINT('Ctrl Pts',(3.62832368669235,-29.2134469545116,
56.9697431597603));
#132789=CARTESIAN_POINT('Ctrl Pts',(3.73945895753091,-31.2282689043408,
56.7291354219427));
#132790=CARTESIAN_POINT('Ctrl Pts',(3.85059422836948,-32.1188909274298,
54.9058987436705));
#132791=CARTESIAN_POINT('Ctrl Pts',(3.96172949920803,-31.0701517756433,
53.1687902944022));
#132792=CARTESIAN_POINT('Ctrl Pts',(4.07286477004659,-29.0419328507167,
53.1077365018973));
#132793=CARTESIAN_POINT('Ctrl Pts',(4.18400004088515,-27.8906057979442,
54.7786181824969));
#132794=CARTESIAN_POINT('Ctrl Pts',(4.2951353117237,-28.6699478348436,56.6521244041387));
#132795=CARTESIAN_POINT('Ctrl Pts',(4.40627058256227,-30.6666491497843,
57.013487700454));
#132796=CARTESIAN_POINT('Ctrl Pts',(4.51740585340082,-32.0531852780137,
55.5319624262439));
#132797=CARTESIAN_POINT('Ctrl Pts',(4.62854112423939,-31.5604987612927,
53.563546929137));
#132798=CARTESIAN_POINT('Ctrl Pts',(4.73967639507795,-29.6395316889681,
52.9098764616585));
#132799=CARTESIAN_POINT('Ctrl Pts',(4.85081166591652,-28.048491107025,54.1692371882256));
#132800=CARTESIAN_POINT('Ctrl Pts',(4.96194693675506,-28.2436116391189,
56.1889717130987));
#132801=CARTESIAN_POINT('Ctrl Pts',(5.07308220759364,-30.0463049589392,
57.1204739233401));
#132802=CARTESIAN_POINT('Ctrl Pts',(5.18421747843218,-31.8066166542933,
56.1111660871432));
#132803=CARTESIAN_POINT('Ctrl Pts',(5.29535274927075,-31.9133830199357,
54.0848392338995));
#132804=CARTESIAN_POINT('Ctrl Pts',(5.4064880201093,-30.2688838090949,52.8961332489926));
#132805=CARTESIAN_POINT('Ctrl Pts',(5.51762329094786,-28.3782828224804,
53.6330372335263));
#132806=CARTESIAN_POINT('Ctrl Pts',(5.62875856178643,-27.9719938832659,
55.621083729683));
#132807=CARTESIAN_POINT('Ctrl Pts',(5.73989383262498,-29.4218818120017,
57.0406697845298));
#132808=CARTESIAN_POINT('Ctrl Pts',(5.85102910346354,-31.40090503212,56.5924882730395));
#132809=CARTESIAN_POINT('Ctrl Pts',(5.9621643743021,-32.0977193410523,54.6867471070161));
#132810=CARTESIAN_POINT('Ctrl Pts',(6.07329964514066,-30.874550231698,53.0677174893343));
#132811=CARTESIAN_POINT('Ctrl Pts',(6.18443491597923,-28.8509299321116,
53.2172516195854));
#132812=CARTESIAN_POINT('Ctrl Pts',(6.29557018681779,-27.8790210953594,
54.9984851208576));
#132813=CARTESIAN_POINT('Ctrl Pts',(6.40670545765634,-28.8483845002052,
56.7811051483327));
#132814=CARTESIAN_POINT('Ctrl Pts',(6.51784072849489,-30.8717891300001,
56.9335298088213));
#132815=CARTESIAN_POINT('Ctrl Pts',(6.62897599933347,-32.0972697281694,
55.3162491045108));
#132816=CARTESIAN_POINT('Ctrl Pts',(6.74011127017202,-31.4031784260473,
53.409514503857));
#132817=CARTESIAN_POINT('Ctrl Pts',(6.85124654101057,-29.4247974393421,
52.9585064724569));
#132818=CARTESIAN_POINT('Ctrl Pts',(6.96238181184914,-27.9728831524087,
54.3760199561802));
#132819=CARTESIAN_POINT('Ctrl Pts',(7.07351708268769,-28.3763318105138,
56.3646447959276));
#132820=CARTESIAN_POINT('Ctrl Pts',(7.18465235352626,-30.2658782221452,
57.1042486972401));
#132821=CARTESIAN_POINT('Ctrl Pts',(7.29578762436481,-31.9120737873953,
55.9178930443925));
#132822=CARTESIAN_POINT('Ctrl Pts',(7.40692289520338,-31.8082020791752,
53.8914157460416));
#132823=CARTESIAN_POINT('Ctrl Pts',(7.51805816604193,-30.049333947799,52.8795943851916));
#132824=CARTESIAN_POINT('Ctrl Pts',(7.6291934368805,-28.2453118412296,53.8085205506278));
#132825=CARTESIAN_POINT('Ctrl Pts',(7.74032870771905,-28.0473063803536,
55.8279742896283));
#132826=CARTESIAN_POINT('Ctrl Pts',(7.85146397855761,-29.6365463704225,
57.0896064889309));
#132827=CARTESIAN_POINT('Ctrl Pts',(7.96259924939617,-31.5584452487474,
56.4386807293097));
#132828=CARTESIAN_POINT('Ctrl Pts',(8.07373452023473,-32.0539430541726,
54.4709710382194));
#132829=CARTESIAN_POINT('Ctrl Pts',(8.18486979107328,-30.6695247217656,
52.9874666304696));
#132830=CARTESIAN_POINT('Ctrl Pts',(8.29600506191187,-28.6723091173694,
53.3459773650017));
#132831=CARTESIAN_POINT('Ctrl Pts',(8.4071403327504,-27.8902918835068,55.2183683349037));
#132832=CARTESIAN_POINT('Ctrl Pts',(8.51827560358897,-29.0392304458407,
56.8908930923912));
#132833=CARTESIAN_POINT('Ctrl Pts',(8.62941087442753,-31.0675355260624,
56.8327363276544));
#132834=CARTESIAN_POINT('Ctrl Pts',(8.74054614526609,-32.1187530118556,
55.0971283119017));
#132835=CARTESIAN_POINT('Ctrl Pts',(8.85168141610465,-31.2307403139536,
53.2726201401656));
#132836=CARTESIAN_POINT('Ctrl Pts',(8.96281668694321,-29.2162562365738,
53.0291367660549));
#132837=CARTESIAN_POINT('Ctrl Pts',(9.07395195778177,-27.9191294692861,
54.5895236869607));
#132838=CARTESIAN_POINT('Ctrl Pts',(9.18508722862032,-28.5265277519878,
56.525618527962));
#132839=CARTESIAN_POINT('Ctrl Pts',(9.2962224994589,-30.4826272983983,57.0653368581459));
#132840=CARTESIAN_POINT('Ctrl Pts',(9.40735777029745,-31.9968456744164,
55.7147518910812));
#132841=CARTESIAN_POINT('Ctrl Pts',(9.518493041136,-31.6836969890651,53.7098926620822));
#132842=CARTESIAN_POINT('Ctrl Pts',(9.62962831197457,-29.8289336406198,
52.8859949163817));
#132843=CARTESIAN_POINT('Ctrl Pts',(9.74076358281312,-28.1318823184159,
53.9966642079673));
#132844=CARTESIAN_POINT('Ctrl Pts',(9.85189885365168,-28.1423931500601,
56.0262957892879));
#132845=CARTESIAN_POINT('Ctrl Pts',(9.96304706111574,-29.8579821295766,
57.115469545492));
#132846=CARTESIAN_POINT('Ctrl Pts',(10.0371501783003,-31.0809288890316,
56.551788339424));
#132847=CARTESIAN_POINT('Ctrl Pts',(10.0742082052053,-31.4379837414887,
56.0734560738743));
#132848=CARTESIAN_POINT('Ctrl Pts',(-0.226186700330235,-29.5709141578673,
53.3933269548259));
#132849=CARTESIAN_POINT('Ctrl Pts',(-0.189141610050715,-29.0366697394421,
53.536004842448));
#132850=CARTESIAN_POINT('Ctrl Pts',(-0.115051429491676,-28.130988900723,
54.3940798358158));
#132851=CARTESIAN_POINT('Ctrl Pts',(-0.00391615865311672,-28.477422416473,
56.2449505987386));
#132852=CARTESIAN_POINT('Ctrl Pts',(0.107219112185443,-30.2201049739755,
56.9527695023448));
#132853=CARTESIAN_POINT('Ctrl Pts',(0.218354383024002,-31.7600006321599,
55.8750100595487));
#132854=CARTESIAN_POINT('Ctrl Pts',(0.329489653862562,-31.6896869883905,
53.995508816608));
#132855=CARTESIAN_POINT('Ctrl Pts',(0.44062492470112,-30.0725128561426,
53.0358281602248));
#132856=CARTESIAN_POINT('Ctrl Pts',(0.55176019553968,-28.3891399767961,
53.8736777710121));
#132857=CARTESIAN_POINT('Ctrl Pts',(0.662895466378239,-28.1800560566109,
55.7425297724241));
#132858=CARTESIAN_POINT('Ctrl Pts',(0.774030737216799,-29.6367588457657,
56.9317090228835));
#132859=CARTESIAN_POINT('Ctrl Pts',(0.885166008055357,-31.4259042018014,
56.3528777467535));
#132860=CARTESIAN_POINT('Ctrl Pts',(0.996301278893918,-31.9099706186142,
54.5357812975853));
#132861=CARTESIAN_POINT('Ctrl Pts',(1.10743654973247,-30.6458891828125,
53.1435783519559));
#132862=CARTESIAN_POINT('Ctrl Pts',(1.21857182057104,-28.7906463724437,
53.4505022116384));
#132863=CARTESIAN_POINT('Ctrl Pts',(1.32970709140959,-28.0422894572636,
55.1756395779036));
#132864=CARTESIAN_POINT('Ctrl Pts',(1.44084236224816,-29.0857705632619,
56.7400180628036));
#132865=CARTESIAN_POINT('Ctrl Pts',(1.55197763308671,-30.966019759114,56.7118074984061));
#132866=CARTESIAN_POINT('Ctrl Pts',(1.66311290392527,-31.962098464078,55.1168275189504));
#132867=CARTESIAN_POINT('Ctrl Pts',(1.77424817476383,-31.162323627612,53.4149187209731));
#132868=CARTESIAN_POINT('Ctrl Pts',(1.88538344560239,-29.2987067644908,
53.1637901048438));
#132869=CARTESIAN_POINT('Ctrl Pts',(1.99651871644095,-28.0769638205787,
54.5932927082397));
#132870=CARTESIAN_POINT('Ctrl Pts',(2.10765398727951,-28.6153217297941,
56.3950430232974));
#132871=CARTESIAN_POINT('Ctrl Pts',(2.21878925811807,-30.4210366462349,
56.9199497663655));
#132872=CARTESIAN_POINT('Ctrl Pts',(2.32992452895663,-31.841388584322,55.6875805710721));
#132873=CARTESIAN_POINT('Ctrl Pts',(2.44105979979519,-31.5763694231964,
53.8258882507669));
#132874=CARTESIAN_POINT('Ctrl Pts',(2.55219507063375,-29.8685437374741,
53.0388273378032));
#132875=CARTESIAN_POINT('Ctrl Pts',(2.66333034147231,-28.2810362652226,
54.0467725151036));
#132876=CARTESIAN_POINT('Ctrl Pts',(2.77446561231087,-28.2668478749018,
55.9271799558324));
#132877=CARTESIAN_POINT('Ctrl Pts',(2.88560088314943,-29.8389648001831,
56.9589657025797));
#132878=CARTESIAN_POINT('Ctrl Pts',(2.99673615398798,-31.5584727074041,
56.1977653274602));
#132879=CARTESIAN_POINT('Ctrl Pts',(3.10787142482655,-31.8515544490454,
54.3402840902397));
#132880=CARTESIAN_POINT('Ctrl Pts',(3.21900669566511,-30.4499605633874,
53.0866222404354));
#132881=CARTESIAN_POINT('Ctrl Pts',(3.33014196650366,-28.6365304498351,
53.5842211524528));
#132882=CARTESIAN_POINT('Ctrl Pts',(3.44127723734223,-28.0710456054286,
55.3776425599043));
#132883=CARTESIAN_POINT('Ctrl Pts',(3.55241250818078,-29.2710783780484,
56.8254183707968));
#132884=CARTESIAN_POINT('Ctrl Pts',(3.66354777901934,-31.1382725768852,
56.6024401705214));
#132885=CARTESIAN_POINT('Ctrl Pts',(3.7746830498579,-31.9636379522272,54.9127936243018));
#132886=CARTESIAN_POINT('Ctrl Pts',(3.88581832069646,-30.9917408272851,
53.3029646170791));
#132887=CARTESIAN_POINT('Ctrl Pts',(3.99695359153502,-29.1121312613309,
53.2463842888809));
#132888=CARTESIAN_POINT('Ctrl Pts',(4.10808886237358,-28.0451629398456,
54.7948390201899));
#132889=CARTESIAN_POINT('Ctrl Pts',(4.21922413321213,-28.7674019100592,
56.5310718167557));
#132890=CARTESIAN_POINT('Ctrl Pts',(4.3303594040507,-30.6178031886351,56.8659577110701));
#132891=CARTESIAN_POINT('Ctrl Pts',(4.44149467488925,-31.9027466127066,
55.4929850780938));
#132892=CARTESIAN_POINT('Ctrl Pts',(4.55262994572782,-31.4461596641949,
53.6687970909568));
#132893=CARTESIAN_POINT('Ctrl Pts',(4.66376521656638,-29.6659435146215,
53.0630216253231));
#132894=CARTESIAN_POINT('Ctrl Pts',(4.77490048740493,-28.1914798554531,
54.2301078996653));
#132895=CARTESIAN_POINT('Ctrl Pts',(4.8860357582435,-28.3723037370028,56.1018547249136));
#132896=CARTESIAN_POINT('Ctrl Pts',(4.99717102908206,-30.042912154454,56.9651049606548));
#132897=CARTESIAN_POINT('Ctrl Pts',(5.10830629992061,-31.6742442858063,
56.0297499846246));
#132898=CARTESIAN_POINT('Ctrl Pts',(5.21944157075917,-31.773187787278,54.1518938566205));
#132899=CARTESIAN_POINT('Ctrl Pts',(5.33057684159773,-30.2491824592966,
53.0502853897639));
#132900=CARTESIAN_POINT('Ctrl Pts',(5.4417121124363,-28.4971074460077,53.7331957804995));
#132901=CARTESIAN_POINT('Ctrl Pts',(5.55284738327485,-28.1205876495973,
55.5755763863672));
#132902=CARTESIAN_POINT('Ctrl Pts',(5.66398265411341,-29.4642410328297,
56.8911481402805));
#132903=CARTESIAN_POINT('Ctrl Pts',(5.77511792495198,-31.2982595059169,
56.4758052766832));
#132904=CARTESIAN_POINT('Ctrl Pts',(5.88625319579053,-31.944017626338,54.7096994180563));
#132905=CARTESIAN_POINT('Ctrl Pts',(5.99738846662909,-30.8104711780395,
53.2092975040626));
#132906=CARTESIAN_POINT('Ctrl Pts',(6.10852373746765,-28.9351232921599,
53.3478751389531));
#132907=CARTESIAN_POINT('Ctrl Pts',(6.21965900830621,-28.0344270584624,
54.9985961173656));
#132908=CARTESIAN_POINT('Ctrl Pts',(6.33079427914477,-28.932764366256,56.6506020300043));
#132909=CARTESIAN_POINT('Ctrl Pts',(6.44192954998333,-30.8079123846567,
56.7918584034759));
#132910=CARTESIAN_POINT('Ctrl Pts',(6.55306482082189,-31.9436009569808,
55.2930772584545));
#132911=CARTESIAN_POINT('Ctrl Pts',(6.66420009166045,-31.3003663263002,
53.5260507550139));
#132912=CARTESIAN_POINT('Ctrl Pts',(6.775335362499,-29.4669430296272,53.1080884730709));
#132913=CARTESIAN_POINT('Ctrl Pts',(6.88647063333757,-28.121411761219,54.4217395149438));
#132914=CARTESIAN_POINT('Ctrl Pts',(6.99760590417612,-28.4952993863792,
56.2646560886658));
#132915=CARTESIAN_POINT('Ctrl Pts',(7.10874117501469,-30.2463970943083,
56.9500685709374));
#132916=CARTESIAN_POINT('Ctrl Pts',(7.21987644585324,-31.7719744833409,
55.8506382252722));
#132917=CARTESIAN_POINT('Ctrl Pts',(7.3310117166918,-31.6757135452325,53.9726426754045));
#132918=CARTESIAN_POINT('Ctrl Pts',(7.44214698753037,-30.0457192066742,
53.0349583428515));
#132919=CARTESIAN_POINT('Ctrl Pts',(7.55328225836892,-28.3738793638309,
53.8958212828239));
#132920=CARTESIAN_POINT('Ctrl Pts',(7.66441752920749,-28.1903819347319,
55.7673078956236));
#132921=CARTESIAN_POINT('Ctrl Pts',(7.77555280004603,-29.663176932954,56.936499209925));
#132922=CARTESIAN_POINT('Ctrl Pts',(7.88668807088461,-31.4442566142942,
56.3332673450242));
#132923=CARTESIAN_POINT('Ctrl Pts',(7.99782334172316,-31.9034488659494,
54.5097334488851));
#132924=CARTESIAN_POINT('Ctrl Pts',(8.10895861256172,-30.6204680649645,
53.1349266951994));
#132925=CARTESIAN_POINT('Ctrl Pts',(8.22009388340028,-28.7695901793672,
53.4671690374053));
#132926=CARTESIAN_POINT('Ctrl Pts',(8.33122915423884,-28.0448720261911,
55.2023682976932));
#132927=CARTESIAN_POINT('Ctrl Pts',(8.44236442507739,-29.1096268640029,
56.7523457162221));
#132928=CARTESIAN_POINT('Ctrl Pts',(8.55349969591596,-30.9893162725793,
56.698450148056));
#132929=CARTESIAN_POINT('Ctrl Pts',(8.66463496675452,-31.9635101418466,
55.0900116362843));
#132930=CARTESIAN_POINT('Ctrl Pts',(8.77577023759308,-31.140562904173,53.3991867600292));
#132931=CARTESIAN_POINT('Ctrl Pts',(8.88690550843164,-29.2736818215783,
53.173543623825));
#132932=CARTESIAN_POINT('Ctrl Pts',(8.99804077927019,-28.07159665706,54.6195996422751));
#132933=CARTESIAN_POINT('Ctrl Pts',(9.10917605010876,-28.6344903410107,
56.4138351357996));
#132934=CARTESIAN_POINT('Ctrl Pts',(9.22031132094731,-30.447264777836,56.9140078360277));
#132935=CARTESIAN_POINT('Ctrl Pts',(9.33144659178588,-31.8505350607078,
55.6623814003752));
#132936=CARTESIAN_POINT('Ctrl Pts',(9.44258186262443,-31.5603310510131,
53.8044199451762));
#132937=CARTESIAN_POINT('Ctrl Pts',(9.553717133463,-29.8414678210757,53.0408899015726));
#132938=CARTESIAN_POINT('Ctrl Pts',(9.66485240430155,-28.2687609204902,
54.0701794912807));
#132939=CARTESIAN_POINT('Ctrl Pts',(9.77598767514011,-28.2785016143876,
55.9510982070706));
#132940=CARTESIAN_POINT('Ctrl Pts',(9.88713588260416,-29.8683879020635,
56.96046725791));
#132941=CARTESIAN_POINT('Ctrl Pts',(9.96123899978869,-31.0017282922326,
56.4380874624881));
#132942=CARTESIAN_POINT('Ctrl Pts',(9.99829702669369,-31.3326214261051,
55.9948030167202));
#132943=CARTESIAN_POINT('Ctrl Pts',(10.,-31.3346917155535,55.997072727755));
#132944=CARTESIAN_POINT('Ctrl Pts',(10.,-31.3032909346448,56.0511234363458));
#132945=CARTESIAN_POINT('Ctrl Pts',(9.99999999999997,-31.2686972100049,
56.1030990415617));
#132946=CARTESIAN_POINT('Ctrl Pts',(9.99999999999999,-31.2312367751759,
56.1529134472441));
#132947=CARTESIAN_POINT('Ctrl Pts',(10.,-31.2074766111454,56.1845094085695));
#132948=CARTESIAN_POINT('Ctrl Pts',(9.99999999999998,-31.1825620753087,
56.2152357171833));
#132949=CARTESIAN_POINT('Ctrl Pts',(9.99999999999999,-31.1565664281997,
56.2450672023032));
#132950=CARTESIAN_POINT('Ctrl Pts',(10.,-31.1387986277207,56.2654567649627));
#132951=CARTESIAN_POINT('Ctrl Pts',(10.,-31.1205256172073,56.2854282470845));
#132952=CARTESIAN_POINT('Ctrl Pts',(9.99999999999999,-31.1017689652775,
56.3049727142744));
#132953=CARTESIAN_POINT('Ctrl Pts',(9.99999999999998,-31.0918278768739,
56.3153313474069));
#132954=CARTESIAN_POINT('Ctrl Pts',(9.99999999999998,-31.0817509756526,
56.3255697751785));
#132955=CARTESIAN_POINT('Ctrl Pts',(9.99999999999998,-31.0715517224076,
56.3356767875606));
#132956=CARTESIAN_POINT('Ctrl Pts',(9.99999999999998,-31.0246754291279,
56.382129137083));
#132957=CARTESIAN_POINT('Ctrl Pts',(9.99999999999999,-30.9751667282857,
56.4258621586488));
#132958=CARTESIAN_POINT('Ctrl Pts',(9.99999999999998,-30.9233613204925,
56.4667657821209));
#132959=CARTESIAN_POINT('Ctrl Pts',(9.99999999999997,-30.8860273825892,
56.4962432711278));
#132960=CARTESIAN_POINT('Ctrl Pts',(9.99999999999999,-30.8474994872535,
56.5242509659966));
#132961=CARTESIAN_POINT('Ctrl Pts',(10.,-30.8078890088004,56.5507389966442));
#132962=CARTESIAN_POINT('Ctrl Pts',(10.,-30.797015398732,56.5580103179711));
#132963=CARTESIAN_POINT('Ctrl Pts',(10.,-30.7860601469677,56.5651670716741));
#132964=CARTESIAN_POINT('Ctrl Pts',(10.,-30.7750254260934,56.5722081087175));
#132965=CARTESIAN_POINT('Ctrl Pts',(10.,-30.7637763630091,56.5793859132839));
#132966=CARTESIAN_POINT('Ctrl Pts',(10.,-30.7524515667651,56.5864390456066));
#132967=CARTESIAN_POINT('Ctrl Pts',(10.,-30.7410580144043,56.5933641088242));
#132968=CARTESIAN_POINT('Ctrl Pts',(10.,-30.6829437846755,56.6286862543647));
#132969=CARTESIAN_POINT('Ctrl Pts',(10.,-30.6230097365582,56.6607008904149));
#132970=CARTESIAN_POINT('Ctrl Pts',(10.,-30.5615984318091,56.6892964836472));
#132971=CARTESIAN_POINT('Ctrl Pts',(10.,-30.4994238831573,56.7182474741841));
#132972=CARTESIAN_POINT('Ctrl Pts',(10.,-30.4357343478421,56.7436946380252));
#132973=CARTESIAN_POINT('Ctrl Pts',(10.,-30.3708449452616,56.7654879565643));
#132974=CARTESIAN_POINT('Ctrl Pts',(10.,-30.3308185453291,56.7789309541727));
#132975=CARTESIAN_POINT('Ctrl Pts',(10.,-30.2903348574852,56.7909829777777));
#132976=CARTESIAN_POINT('Ctrl Pts',(10.,-30.249462365503,56.8016005644171));
#132977=CARTESIAN_POINT('Ctrl Pts',(10.,-30.2158480327199,56.8103326742871));
#132978=CARTESIAN_POINT('Ctrl Pts',(10.,-30.1819706297403,56.8180944670961));
#132979=CARTESIAN_POINT('Ctrl Pts',(9.99999999999999,-30.1478668356042,
56.8248580322968));
#132980=CARTESIAN_POINT('Ctrl Pts',(9.99999999999998,-30.1339192196307,
56.8276241647));
#132981=CARTESIAN_POINT('Ctrl Pts',(10.,-30.1199311692375,56.8302235991369));
#132982=CARTESIAN_POINT('Ctrl Pts',(10.,-30.1059290408562,56.8326505130612));
#132983=CARTESIAN_POINT('Ctrl Pts',(9.99999999999999,-30.036479877866,56.8446877645493));
#132984=CARTESIAN_POINT('Ctrl Pts',(10.,-29.9665653006914,56.8525100973381));
#132985=CARTESIAN_POINT('Ctrl Pts',(10.,-29.8965201495899,56.855976934255));
#132986=CARTESIAN_POINT('Ctrl Pts',(10.,-29.8887467804205,56.8563616718533));
#132987=CARTESIAN_POINT('Ctrl Pts',(9.99999999999999,-29.8809717732861,
56.8566927244466));
#132988=CARTESIAN_POINT('Ctrl Pts',(9.99999999999999,-29.8731955649853,
56.8569698661726));
#132989=CARTESIAN_POINT('Ctrl Pts',(10.,-29.8058138556625,56.8593713300357));
#132990=CARTESIAN_POINT('Ctrl Pts',(9.99999999999998,-29.7383430939132,
56.857729193759));
#132991=CARTESIAN_POINT('Ctrl Pts',(9.99999999999998,-29.6710457952579,
56.8522613874595));
#132992=CARTESIAN_POINT('Ctrl Pts',(9.99999999999998,-29.5986466816943,
56.8463790662203));
#132993=CARTESIAN_POINT('Ctrl Pts',(9.99999999999999,-29.5264474184432,
56.836069467537));
#132994=CARTESIAN_POINT('Ctrl Pts',(9.99999999999999,-29.4547662757674,
56.8215402711312));
#132995=CARTESIAN_POINT('Ctrl Pts',(9.99999999999999,-29.441748496888,56.8189016710888));
#132996=CARTESIAN_POINT('Ctrl Pts',(10.,-29.4287478079428,56.816123737079));
#132997=CARTESIAN_POINT('Ctrl Pts',(10.,-29.4157661281353,56.8132074934358));
#132998=CARTESIAN_POINT('Ctrl Pts',(10.,-29.4044168231439,56.8106579513869));
#132999=CARTESIAN_POINT('Ctrl Pts',(9.99999999999998,-29.3930909204653,
56.8080046750453));
#133000=CARTESIAN_POINT('Ctrl Pts',(9.99999999999998,-29.3817917769416,
56.8052493638686));
#133001=CARTESIAN_POINT('Ctrl Pts',(10.,-29.3127468519509,56.788412667076));
#133002=CARTESIAN_POINT('Ctrl Pts',(9.99999999999998,-29.2446768142312,
56.7677647231327));
#133003=CARTESIAN_POINT('Ctrl Pts',(9.99999999999998,-29.1778687398964,
56.7435558218946));
#133004=CARTESIAN_POINT('Ctrl Pts',(9.99999999999998,-29.1093809169293,
56.7187382387098));
#133005=CARTESIAN_POINT('Ctrl Pts',(10.,-29.042218379655,56.6901782595077));
#133006=CARTESIAN_POINT('Ctrl Pts',(10.,-28.9766863196167,56.6580897906909));
#133007=CARTESIAN_POINT('Ctrl Pts',(10.,-28.9112758404337,56.6260608552304));
#133008=CARTESIAN_POINT('Ctrl Pts',(10.,-28.8474887900981,56.5905161312587));
#133009=CARTESIAN_POINT('Ctrl Pts',(10.,-28.7856393264207,56.5516176578855));
#133010=CARTESIAN_POINT('Ctrl Pts',(10.,-28.7688957142038,56.5410872358694));
#133011=CARTESIAN_POINT('Ctrl Pts',(10.,-28.7522942908099,56.5303108130768));
#133012=CARTESIAN_POINT('Ctrl Pts',(10.,-28.7358413036534,56.5192908377815));
#133013=CARTESIAN_POINT('Ctrl Pts',(10.,-28.7254089766122,56.5123034144539));
#133014=CARTESIAN_POINT('Ctrl Pts',(10.,-28.7150370135204,56.5052184142791));
#133015=CARTESIAN_POINT('Ctrl Pts',(10.,-28.704739183828,56.4980452468686));
#133016=CARTESIAN_POINT('Ctrl Pts',(10.,-28.6429556743447,56.4550086585805));
#133017=CARTESIAN_POINT('Ctrl Pts',(10.,-28.5837268958653,56.4087277658481));
#133018=CARTESIAN_POINT('Ctrl Pts',(10.,-28.5273654175275,56.3594358051663));
#133019=CARTESIAN_POINT('Ctrl Pts',(10.,-28.4712788591607,56.3103842807682));
#133020=CARTESIAN_POINT('Ctrl Pts',(10.,-28.4180306882043,56.2583505378195));
#133021=CARTESIAN_POINT('Ctrl Pts',(10.,-28.3679443534525,56.2035160661832));
#133022=CARTESIAN_POINT('Ctrl Pts',(10.,-28.3183087377282,56.1491750413094));
#133023=CARTESIAN_POINT('Ctrl Pts',(10.,-28.2717773418937,56.0920830054598));
#133024=CARTESIAN_POINT('Ctrl Pts',(10.,-28.2286947931129,56.0323758423507));
#133025=CARTESIAN_POINT('Ctrl Pts',(10.,-28.2195095858647,56.0196462642993));
#133026=CARTESIAN_POINT('Ctrl Pts',(10.,-28.2104812826155,56.0067976831957));
#133027=CARTESIAN_POINT('Ctrl Pts',(10.,-28.2016134661306,55.9938312042311));
#133028=CARTESIAN_POINT('Ctrl Pts',(10.,-28.1941455433265,55.982911643129));
#133029=CARTESIAN_POINT('Ctrl Pts',(10.0000000000001,-28.1867914389921,
55.9719084678104));
#133030=CARTESIAN_POINT('Ctrl Pts',(10.,-28.1795511441573,55.9608235055809));
#133031=CARTESIAN_POINT('',(-0.000879000304030074,-28.729739644302,56.080266780513));
#133032=CARTESIAN_POINT('Ctrl Pts',(-0.000879000304030431,-28.7308780712584,
56.079298628734));
#133033=CARTESIAN_POINT('Ctrl Pts',(-0.000586000202687196,-28.7363705706892,
56.0857571299178));
#133034=CARTESIAN_POINT('Ctrl Pts',(-0.000293000101343235,-28.7419123715811,
56.0921737036785));
#133035=CARTESIAN_POINT('Ctrl Pts',(0.,-28.7475028281235,56.0985476022646));
#133036=CARTESIAN_POINT('Ctrl Pts',(-2.77989437025283E-16,-29.4698297828114,
53.0148256743283));
#133037=CARTESIAN_POINT('Ctrl Pts',(-1.0665791516157E-14,-29.4008110336088,
53.0403807583238));
#133038=CARTESIAN_POINT('Ctrl Pts',(-1.4405926639662E-14,-29.3335131533633,
53.0698652662575));
#133039=CARTESIAN_POINT('Ctrl Pts',(-1.08229397666193E-14,-29.2681280944835,
53.1029808141168));
#133040=CARTESIAN_POINT('Ctrl Pts',(-7.159689807959E-15,-29.2012783340112,
53.1368381888785));
#133041=CARTESIAN_POINT('Ctrl Pts',(8.43478140072747E-15,-29.1364273041799,
53.1744918375422));
#133042=CARTESIAN_POINT('Ctrl Pts',(-7.1505301679764E-15,-29.0738114589791,
53.2156675542709));
#133043=CARTESIAN_POINT('Ctrl Pts',(-2.02460281250629E-14,-29.0211987364619,
53.2502652915009));
#133044=CARTESIAN_POINT('Ctrl Pts',(-1.09741656434686E-14,-28.970164437306,
53.2873507054925));
#133045=CARTESIAN_POINT('Ctrl Pts',(3.01841884819964E-15,-28.9208711427474,
53.3267787632336));
#133046=CARTESIAN_POINT('Ctrl Pts',(9.13037560475156E-15,-28.8988436927425,
53.3443977838014));
#133047=CARTESIAN_POINT('Ctrl Pts',(-1.22852585041228E-14,-28.8771642000329,
53.3624847793734));
#133048=CARTESIAN_POINT('Ctrl Pts',(-1.06165076729781E-14,-28.8558487196368,
53.3810275283898));
#133049=CARTESIAN_POINT('Ctrl Pts',(-9.88881029091767E-15,-28.8441362670507,
53.3912164176212));
#133050=CARTESIAN_POINT('Ctrl Pts',(7.41477610914109E-15,-28.8325337381655,
53.4015429188335));
#133051=CARTESIAN_POINT('Ctrl Pts',(-6.03683769639929E-16,-28.8210439308083,
53.4120050460791));
#133052=CARTESIAN_POINT('Ctrl Pts',(-7.96620544898847E-15,-28.8104503093549,
53.421651144764));
#133053=CARTESIAN_POINT('Ctrl Pts',(-3.05068135553069E-14,-28.7999510772543,
53.4314140526976));
#133054=CARTESIAN_POINT('Ctrl Pts',(-2.68118860446975E-14,-28.7895643152319,
53.4412767583167));
#133055=CARTESIAN_POINT('Ctrl Pts',(-7.62295780683882E-15,-28.7365326250796,
53.4916327737262));
#133056=CARTESIAN_POINT('Ctrl Pts',(1.51656315868618E-14,-28.6863352196068,
53.5446717148978));
#133057=CARTESIAN_POINT('Ctrl Pts',(3.91353616180368E-15,-28.6391900995011,
53.6001349753071));
#133058=CARTESIAN_POINT('Ctrl Pts',(-7.27372162178762E-15,-28.5923166424305,
53.655278641289));
#133059=CARTESIAN_POINT('Ctrl Pts',(2.48947925224922E-14,-28.548459871344,
53.7128196446158));
#133060=CARTESIAN_POINT('Ctrl Pts',(1.70835567914196E-14,-28.5078789636859,
53.7725281427631));
#133061=CARTESIAN_POINT('Ctrl Pts',(1.05450601504418E-14,-28.4741885332485,
53.8220983746639));
#133062=CARTESIAN_POINT('Ctrl Pts',(-2.04280178585247E-15,-28.442756603648,
53.8731631816402));
#133063=CARTESIAN_POINT('Ctrl Pts',(-1.48492329543615E-15,-28.4137591004027,
53.9255975295555));
#133064=CARTESIAN_POINT('Ctrl Pts',(-1.22938169818173E-15,-28.4016536375506,
53.9474870710616));
#133065=CARTESIAN_POINT('Ctrl Pts',(-9.11589881619325E-15,-28.3899727624535,
53.9696153320029));
#133066=CARTESIAN_POINT('Ctrl Pts',(2.48412401759879E-15,-28.3787307158643,
53.9919732986115));
#133067=CARTESIAN_POINT('Ctrl Pts',(7.89954593962274E-15,-28.3735286790514,
54.0023190096382));
#133068=CARTESIAN_POINT('Ctrl Pts',(-2.36829711337499E-14,-28.3684206163503,
54.0127139050674));
#133069=CARTESIAN_POINT('Ctrl Pts',(-1.07414077632484E-14,-28.3634080039989,
54.0231570898446));
#133070=CARTESIAN_POINT('Ctrl Pts',(2.9082809691703E-15,-28.358177440751,
54.0340543495284));
#133071=CARTESIAN_POINT('Ctrl Pts',(-1.10461030585208E-15,-28.353054421572,
54.0449967292496));
#133072=CARTESIAN_POINT('Ctrl Pts',(9.99200722162641E-16,-28.3480419952893,
54.0559789414607));
#133073=CARTESIAN_POINT('Ctrl Pts',(1.25291893836216E-14,-28.3195017414189,
54.1185105592614));
#133074=CARTESIAN_POINT('Ctrl Pts',(-1.82419144324192E-14,-28.2945224341956,
54.1823754520524));
#133075=CARTESIAN_POINT('Ctrl Pts',(-9.99200722162641E-16,-28.2733275400369,
54.2473692544875));
#133076=CARTESIAN_POINT('Ctrl Pts',(1.45523611235135E-14,-28.2541213280901,
54.3062647948684));
#133077=CARTESIAN_POINT('Ctrl Pts',(-1.08023430877253E-14,-28.2380229966997,
54.36608793415));
#133078=CARTESIAN_POINT('Ctrl Pts',(-2.27595720048157E-15,-28.225235550378,
54.4266914343325));
#133079=CARTESIAN_POINT('Ctrl Pts',(7.749618433971E-15,-28.2101043131511,
54.4984028546557));
#133080=CARTESIAN_POINT('Ctrl Pts',(-1.67522331911175E-14,-28.1996082812463,
54.5712084333142));
#133081=CARTESIAN_POINT('Ctrl Pts',(8.04911692853238E-15,-28.1936722887569,
54.6446849507566));
#133082=CARTESIAN_POINT('Ctrl Pts',(1.33492669303424E-14,-28.1923656613117,
54.6608585618995));
#133083=CARTESIAN_POINT('Ctrl Pts',(9.42994019188542E-16,-28.191280203414,
54.6770645999387));
#133084=CARTESIAN_POINT('Ctrl Pts',(1.08801856413265E-14,-28.190415482858,
54.6932983865838));
#133085=CARTESIAN_POINT('Ctrl Pts',(2.12756282169907E-14,-28.1895217390097,
54.7100770405054));
#133086=CARTESIAN_POINT('Ctrl Pts',(1.01404829358878E-14,-28.1888637889881,
54.7268915103632));
#133087=CARTESIAN_POINT('Ctrl Pts',(5.19029264012261E-15,-28.188441715024,
54.7437024356232));
#133088=CARTESIAN_POINT('Ctrl Pts',(-1.44902179624514E-14,-28.1867182332684,
54.8123475676241));
#133089=CARTESIAN_POINT('Ctrl Pts',(-2.06499258425703E-14,-28.1889159285315,
54.8810206540149));
#133090=CARTESIAN_POINT('Ctrl Pts',(-2.19546603119625E-14,-28.1949137770878,
54.9493820494338));
#133091=CARTESIAN_POINT('Ctrl Pts',(-2.32559660595922E-14,-28.2008958638517,
55.017563797415));
#133092=CARTESIAN_POINT('Ctrl Pts',(-1.15115769682287E-14,-28.2106586298725,
55.0854365535916));
#133093=CARTESIAN_POINT('Ctrl Pts',(-7.88258347483861E-15,-28.2241314254406,
55.15264835974));
#133094=CARTESIAN_POINT('Ctrl Pts',(-5.00043810275242E-15,-28.233892766503,
55.201344813265));
#133095=CARTESIAN_POINT('Ctrl Pts',(-2.02964811291747E-14,-28.2456026680783,
55.2496940495499));
#133096=CARTESIAN_POINT('Ctrl Pts',(-1.63757896132211E-14,-28.2592484588431,
55.2975525606475));
#133097=CARTESIAN_POINT('Ctrl Pts',(-1.37739671341366E-14,-28.2694856535417,
55.3334564451883));
#133098=CARTESIAN_POINT('Ctrl Pts',(-2.0853126275729E-14,-28.2808126421487,
55.3690839879711));
#133099=CARTESIAN_POINT('Ctrl Pts',(-2.19269047363468E-15,-28.2932279901634,
55.4043704183004));
#133100=CARTESIAN_POINT('Ctrl Pts',(4.080860316094E-15,-28.297356610343,
55.4161046256824));
#133101=CARTESIAN_POINT('Ctrl Pts',(-5.64529113086221E-15,-28.3016023883907,
55.4277919105227));
#133102=CARTESIAN_POINT('Ctrl Pts',(-4.55191440096314E-15,-28.3059646859586,
55.4394297312791));
#133103=CARTESIAN_POINT('Ctrl Pts',(1.18430705547116E-15,-28.3291463512111,
55.5012742205299));
#133104=CARTESIAN_POINT('Ctrl Pts',(-2.93539877151333E-14,-28.3556167596801,
55.5617283395611));
#133105=CARTESIAN_POINT('Ctrl Pts',(-1.02418074021671E-14,-28.3853255649081,
55.6204553959407));
#133106=CARTESIAN_POINT('Ctrl Pts',(3.12256336159443E-15,-28.4060997247117,
55.6615208391538));
#133107=CARTESIAN_POINT('Ctrl Pts',(-2.86399248371055E-16,-28.428458203708,
55.7017412727147));
#133108=CARTESIAN_POINT('Ctrl Pts',(6.85562717706034E-15,-28.4523940833834,
55.7409903379818));
#133109=CARTESIAN_POINT('Ctrl Pts',(9.35284774839498E-15,-28.4601069023448,
55.7536374994363));
#133110=CARTESIAN_POINT('Ctrl Pts',(-7.98569581965833E-15,-28.4679846656324,
55.7661854163635));
#133111=CARTESIAN_POINT('Ctrl Pts',(-9.13158437754191E-15,-28.4760238017732,
55.7786242039287));
#133112=CARTESIAN_POINT('Ctrl Pts',(-1.32593519350506E-14,-28.5102686331161,
55.831610516739));
#133113=CARTESIAN_POINT('Ctrl Pts',(2.63092452167841E-14,-28.5473690403558,
55.8825129450324));
#133114=CARTESIAN_POINT('Ctrl Pts',(1.35447209004269E-14,-28.5872907667857,
55.9310162114176));
#133115=CARTESIAN_POINT('Ctrl Pts',(1.94148639868689E-15,-28.6240879045149,
55.9757232302042));
#133116=CARTESIAN_POINT('Ctrl Pts',(1.25238026008096E-14,-28.663282593062,
56.0183920404323));
#133117=CARTESIAN_POINT('Ctrl Pts',(1.53765888910584E-14,-28.7048694629046,
56.0587428197802));
#133118=CARTESIAN_POINT('Ctrl Pts',(1.59003142960975E-14,-28.7126726657512,
56.0663140872852));
#133119=CARTESIAN_POINT('Ctrl Pts',(1.71809312476446E-14,-28.7205601438141,
56.0738036401068));
#133120=CARTESIAN_POINT('Ctrl Pts',(1.67643676718399E-14,-28.728530314404,
56.0812108165541));
#133121=CARTESIAN_POINT('Ctrl Pts',(0.00170274486062548,28.7336022489738,
56.0778455314206));
#133122=CARTESIAN_POINT('Ctrl Pts',(0.0387607700302481,28.375062470833,
55.6566084090024));
#133123=CARTESIAN_POINT('Ctrl Pts',(0.11286388547939,28.1179694426535,54.4354449555209));
#133124=CARTESIAN_POINT('Ctrl Pts',(0.224012091208053,29.4558183203175,
53.1100225039009));
#133125=CARTESIAN_POINT('Ctrl Pts',(0.335147362046612,31.2917444909721,
53.519071810237));
#133126=CARTESIAN_POINT('Ctrl Pts',(0.446282632885172,31.9452683344491,
55.2813851316961));
#133127=CARTESIAN_POINT('Ctrl Pts',(0.557417903723731,30.8183979982367,
56.7872523586237));
#133128=CARTESIAN_POINT('Ctrl Pts',(0.668553174562291,28.9424430451878,
56.6567445746501));
#133129=CARTESIAN_POINT('Ctrl Pts',(0.779688445400849,28.034454310918,55.0101441995473));
#133130=CARTESIAN_POINT('Ctrl Pts',(0.89082371623941,28.9254670458642,53.3541183701554));
#133131=CARTESIAN_POINT('Ctrl Pts',(1.00195898707797,30.79997311927,53.2045926301162));
#133132=CARTESIAN_POINT('Ctrl Pts',(1.11309425791653,31.9422845185978,54.6983168637613));
#133133=CARTESIAN_POINT('Ctrl Pts',(1.22422952875509,31.3068785288967,56.4681812386422));
#133134=CARTESIAN_POINT('Ctrl Pts',(1.33536479959365,29.4753229760543,56.8942515731679));
#133135=CARTESIAN_POINT('Ctrl Pts',(1.44650007043221,28.1239897554366,55.5865714020816));
#133136=CARTESIAN_POINT('Ctrl Pts',(1.55763534127076,28.4897157453897,53.7420166322667));
#133137=CARTESIAN_POINT('Ctrl Pts',(1.66877061210933,30.2377624268046,53.0488597700237));
#133138=CARTESIAN_POINT('Ctrl Pts',(1.77990588294789,31.7681918270586,54.141526005001));
#133139=CARTESIAN_POINT('Ctrl Pts',(1.89104115378645,31.6802450745805,56.0199296012311));
#133140=CARTESIAN_POINT('Ctrl Pts',(2.00217642462501,30.0544173317013,56.9648202156473));
#133141=CARTESIAN_POINT('Ctrl Pts',(2.11331169546357,28.3787829419347,56.1113663130958));
#133142=CARTESIAN_POINT('Ctrl Pts',(2.22444696630212,28.1870028523858,54.2407100941288));
#133143=CARTESIAN_POINT('Ctrl Pts',(2.33558223714069,29.6546079793174,53.0650105554149));
#133144=CARTESIAN_POINT('Ctrl Pts',(2.44671750797925,31.4383406922937,53.6603523352754));
#133145=CARTESIAN_POINT('Ctrl Pts',(2.55785277881781,31.9056006891706,55.4818358885204));
#133146=CARTESIAN_POINT('Ctrl Pts',(2.66898804965636,30.6287180575535,56.8623086242662));
#133147=CARTESIAN_POINT('Ctrl Pts',(2.78012332049493,28.7763874994555,56.5382627403222));
#133148=CARTESIAN_POINT('Ctrl Pts',(2.89125859133347,28.0439949928455,54.806288303732));
#133149=CARTESIAN_POINT('Ctrl Pts',(3.00239386217205,29.1018787669375,53.251612726026));
#133150=CARTESIAN_POINT('Ctrl Pts',(3.1135291330106,30.9817876047871,53.297186766438));
#133151=CARTESIAN_POINT('Ctrl Pts',(3.22466440384917,31.9630939057901,54.9012977898799));
#133152=CARTESIAN_POINT('Ctrl Pts',(3.33579967468772,31.1476356568844,56.595748165677));
#133153=CARTESIAN_POINT('Ctrl Pts',(3.44693494552628,29.2817788211282,56.8296551990643));
#133154=CARTESIAN_POINT('Ctrl Pts',(3.55807021636484,28.0732895974775,55.3889303717164));
#133155=CARTESIAN_POINT('Ctrl Pts',(3.6692054872034,28.6282641281478,53.5922285316486));
#133156=CARTESIAN_POINT('Ctrl Pts',(3.78034075804196,30.4387498593314,53.0840202584133));
#133157=CARTESIAN_POINT('Ctrl Pts',(3.89147602888052,31.8476602042343,54.3294542678376));
#133158=CARTESIAN_POINT('Ctrl Pts',(4.00261129971908,31.5654592143968,56.1886198960528));
#133159=CARTESIAN_POINT('Ctrl Pts',(4.11374657055764,29.8504375059698,56.9598752178678));
#133160=CARTESIAN_POINT('Ctrl Pts',(4.2248818413962,28.272306135023,55.937311964158));
#133161=CARTESIAN_POINT('Ctrl Pts',(4.33601711223476,28.2754842880507,54.0568534745479));
#133162=CARTESIAN_POINT('Ctrl Pts',(4.44715238307332,29.8570630911178,53.0396304304259));
#133163=CARTESIAN_POINT('Ctrl Pts',(4.55828765391188,31.5694680202276,53.8166784280192));
#133164=CARTESIAN_POINT('Ctrl Pts',(4.66942292475044,31.8453830837027,55.6767873252483));
#133165=CARTESIAN_POINT('Ctrl Pts',(4.780558195589,30.4322709967113,56.9174518493654));
#133166=CARTESIAN_POINT('Ctrl Pts',(4.89169346642755,28.6235134438802,56.403126712045));
#133167=CARTESIAN_POINT('Ctrl Pts',(5.00282873726612,28.0746152590417,54.6045592224899));
#133168=CARTESIAN_POINT('Ctrl Pts',(5.11396400810467,29.2879674878394,53.1679275366791));
#133169=CARTESIAN_POINT('Ctrl Pts',(5.22509927894324,31.1530230164423,53.4081401654709));
#133170=CARTESIAN_POINT('Ctrl Pts',(5.33623454978178,31.9627490597571,55.1053372567309));
#133171=CARTESIAN_POINT('Ctrl Pts',(5.44736982062036,30.9760261810247,56.7061221243472));
#133172=CARTESIAN_POINT('Ctrl Pts',(5.55850509145891,29.0959740343069,56.7453414744931));
#133173=CARTESIAN_POINT('Ctrl Pts',(5.66964036229747,28.0433513867903,55.1870989408228));
#133174=CARTESIAN_POINT('Ctrl Pts',(5.78077563313603,28.781594094451,53.4576100173576));
#133175=CARTESIAN_POINT('Ctrl Pts',(5.89191090397459,30.6350094039064,53.1398271945372));
#133176=CARTESIAN_POINT('Ctrl Pts',(6.00304617481315,31.9072184947336,54.5246081378709));
#133177=CARTESIAN_POINT('Ctrl Pts',(6.11418144565171,31.4338042253354,56.3445018604091));
#133178=CARTESIAN_POINT('Ctrl Pts',(6.22531671649026,29.6480693399998,56.9338109059017));
#133179=CARTESIAN_POINT('Ctrl Pts',(6.33645198732883,28.1844466735699,55.7531573063582));
#133180=CARTESIAN_POINT('Ctrl Pts',(6.44758725816739,28.3825488211043,53.8831600414011));
#133181=CARTESIAN_POINT('Ctrl Pts',(6.55872252900594,30.0610584676762,53.0353749281974));
#133182=CARTESIAN_POINT('Ctrl Pts',(6.66985779984451,31.6836830188524,53.9857557980152));
#133183=CARTESIAN_POINT('Ctrl Pts',(6.78099307068307,31.7652799336917,55.8644458137724));
#133184=CARTESIAN_POINT('Ctrl Pts',(6.89212834152162,30.2311658546877,56.9519329283661));
#133185=CARTESIAN_POINT('Ctrl Pts',(7.00326361236018,28.4854721810444,56.252870821291));
#133186=CARTESIAN_POINT('Ctrl Pts',(7.11439888319874,28.125983154499,54.4070913459176));
#133187=CARTESIAN_POINT('Ctrl Pts',(7.2255341540373,29.4817289540074,53.1039844589357));
#133188=CARTESIAN_POINT('Ctrl Pts',(7.33666942487587,31.3118336416646,53.5362471841592));
#133189=CARTESIAN_POINT('Ctrl Pts',(7.44780469571442,31.9412539528034,55.3082416267767));
#133190=CARTESIAN_POINT('Ctrl Pts',(7.55893996655298,30.7938992073525,56.7981111913546));
#133191=CARTESIAN_POINT('Ctrl Pts',(7.67007523739155,28.9199108830388,56.6422202378048));
#133192=CARTESIAN_POINT('Ctrl Pts',(7.7812105082301,28.0344976988523,54.9832513614566));
#133193=CARTESIAN_POINT('Ctrl Pts',(7.89234577906866,28.9480534041238,53.3396120459267));
#133194=CARTESIAN_POINT('Ctrl Pts',(8.00348104990723,30.8244261881505,53.2156790426869));
#133195=CARTESIAN_POINT('Ctrl Pts',(8.11461632074577,31.9462249192566,54.724884760671));
#133196=CARTESIAN_POINT('Ctrl Pts',(8.22575159158435,31.2866987842503,56.4858956775006));
#133197=CARTESIAN_POINT('Ctrl Pts',(8.3368868624229,29.4494935477483,56.8869081981243));
#133198=CARTESIAN_POINT('Ctrl Pts',(8.44802213326146,28.1161512629849,55.560886685002));
#133199=CARTESIAN_POINT('Ctrl Pts',(8.55915740410001,28.5070428473976,53.721501619428));
#133200=CARTESIAN_POINT('Ctrl Pts',(8.67029267493858,30.2643956793274,53.0522896498785));
#133201=CARTESIAN_POINT('Ctrl Pts',(8.78142794577713,31.7797553403405,54.1657629977179));
#133202=CARTESIAN_POINT('Ctrl Pts',(8.8925632166157,31.6661535964514,56.0427881831597));
#133203=CARTESIAN_POINT('Ctrl Pts',(9.00369848745425,30.0275713350733,56.9653822682303));
#133204=CARTESIAN_POINT('Ctrl Pts',(9.11483375829281,28.3637479941479,56.0891102970866));
#133205=CARTESIAN_POINT('Ctrl Pts',(9.22596902913138,28.1975515441048,54.2160202941221));
#133206=CARTESIAN_POINT('Ctrl Pts',(9.33710429996993,29.6810625421903,53.0604571912458));
#133207=CARTESIAN_POINT('Ctrl Pts',(9.4482395708085,31.4565333040147,53.6801577764939));
#133208=CARTESIAN_POINT('Ctrl Pts',(9.55937484164705,31.8987903716828,55.507764140826));
#133209=CARTESIAN_POINT('Ctrl Pts',(9.67051011248561,30.6033161195011,56.8708436430855));
#133210=CARTESIAN_POINT('Ctrl Pts',(9.78164538332418,28.7552906341999,56.5211656977594));
#133211=CARTESIAN_POINT('Ctrl Pts',(9.89278065416272,28.047213240497,54.7800545406207));
#133212=CARTESIAN_POINT('Ctrl Pts',(10.0039159250013,29.1250665498602,53.2385687370523));
#133213=CARTESIAN_POINT('Ctrl Pts',(10.1150511958398,31.0066261676809,53.3126786467944));
#133214=CARTESIAN_POINT('Ctrl Pts',(10.1891413763989,31.6416512911897,54.3865918608222));
#133215=CARTESIAN_POINT('Ctrl Pts',(10.2261864666784,31.6618713842553,54.9391906075592));
#133216=CARTESIAN_POINT('Ctrl Pts',(-0.0741837504160435,28.6335084204081,
56.1630365274997));
#133217=CARTESIAN_POINT('Ctrl Pts',(-0.037125725246421,28.2466302951262,
55.7085055712267));
#133218=CARTESIAN_POINT('Ctrl Pts',(0.0369773902027212,27.9692170907089,
54.3908235277015));
#133219=CARTESIAN_POINT('Ctrl Pts',(0.148125595931384,29.4128071670596,
52.9606420400344));
#133220=CARTESIAN_POINT('Ctrl Pts',(0.259260866769943,31.3938416808363,
53.4020218768933));
#133221=CARTESIAN_POINT('Ctrl Pts',(0.370396137608503,32.0990188879581,
55.3036253126424));
#133222=CARTESIAN_POINT('Ctrl Pts',(0.481531408447062,30.883082722185,56.9285136101086));
#133223=CARTESIAN_POINT('Ctrl Pts',(0.592666679285622,28.8588556221624,
56.7876907227286));
#133224=CARTESIAN_POINT('Ctrl Pts',(0.70380195012418,27.8791010713203,55.0109459790591));
#133225=CARTESIAN_POINT('Ctrl Pts',(0.814937220962741,28.8405378700091,
53.2240308099369));
#133226=CARTESIAN_POINT('Ctrl Pts',(0.9260724918013,30.8632015735155,53.062686821028));
#133227=CARTESIAN_POINT('Ctrl Pts',(1.03720776263986,32.0957992366023,54.6744723645939));
#133228=CARTESIAN_POINT('Ctrl Pts',(1.14834303347842,31.4101718862337,56.5842236756135));
#133229=CARTESIAN_POINT('Ctrl Pts',(1.25947830431697,29.4338534361371,57.0439698524931));
#133230=CARTESIAN_POINT('Ctrl Pts',(1.37061357515554,27.9757132383196,55.6329329636953));
#133231=CARTESIAN_POINT('Ctrl Pts',(1.48174884599409,28.3703455608296,53.6425878616088));
#133232=CARTESIAN_POINT('Ctrl Pts',(1.59288411683265,30.2565547466493,52.8946451123234));
#133233=CARTESIAN_POINT('Ctrl Pts',(1.70401938767121,31.9079465679885,54.073673745461));
#133234=CARTESIAN_POINT('Ctrl Pts',(1.81515465850977,31.8130486604264,56.1005430250722));
#133235=CARTESIAN_POINT('Ctrl Pts',(1.92628992934833,30.0587183809301,57.1201161151134));
#133236=CARTESIAN_POINT('Ctrl Pts',(2.03742520018689,28.2506448256545,56.1992067322111));
#133237=CARTESIAN_POINT('Ctrl Pts',(2.14856047102545,28.043706778513,54.1806971687991));
#133238=CARTESIAN_POINT('Ctrl Pts',(2.25969574186401,29.6273088075695,52.912072427101));
#133239=CARTESIAN_POINT('Ctrl Pts',(2.37083101270257,31.5520245854915,53.5544689636547));
#133240=CARTESIAN_POINT('Ctrl Pts',(2.48196628354113,32.0562159824636,55.5199193411982));
#133241=CARTESIAN_POINT('Ctrl Pts',(2.59310155437969,30.6784108159447,57.0095021896548));
#133242=CARTESIAN_POINT('Ctrl Pts',(2.70423682521824,28.6796753410825,56.6598442946911));
#133243=CARTESIAN_POINT('Ctrl Pts',(2.81537209605682,27.889395831799,54.7909776753754));
#133244=CARTESIAN_POINT('Ctrl Pts',(2.92650736689538,29.0308928601318,53.1134233017903));
#133245=CARTESIAN_POINT('Ctrl Pts',(3.03764263773393,31.059386352986,53.1625994333971));
#133246=CARTESIAN_POINT('Ctrl Pts',(3.14877790857249,32.1182533607917,54.8934965425302));
#133247=CARTESIAN_POINT('Ctrl Pts',(3.25991317941105,31.2383427405024,56.7218732659465));
#133248=CARTESIAN_POINT('Ctrl Pts',(3.37104845024961,29.2250118950247,56.9742678957318));
#133249=CARTESIAN_POINT('Ctrl Pts',(3.48218372108817,27.9210058299411,55.4196707373867));
#133250=CARTESIAN_POINT('Ctrl Pts',(3.59331899192673,28.5198445616384,53.4809607756069));
#133251=CARTESIAN_POINT('Ctrl Pts',(3.70445426276529,30.4734278688017,52.9325846232549));
#133252=CARTESIAN_POINT('Ctrl Pts',(3.81558953360385,31.9936959845257,54.2764555243495));
#133253=CARTESIAN_POINT('Ctrl Pts',(3.92672480444241,31.6891903297635,56.282566301129));
#133254=CARTESIAN_POINT('Ctrl Pts',(4.03786007528097,29.8386163521299,57.1147802734938));
#133255=CARTESIAN_POINT('Ctrl Pts',(4.14899534611951,28.135752281074,56.0113954367296));
#133256=CARTESIAN_POINT('Ctrl Pts',(4.26013061695809,28.1391816296711,53.9823088486162));
#133257=CARTESIAN_POINT('Ctrl Pts',(4.37126588779665,29.845765611758,52.8846863021191));
#133258=CARTESIAN_POINT('Ctrl Pts',(4.4824011586352,31.693515984486,53.7231507930656));
#133259=CARTESIAN_POINT('Ctrl Pts',(4.59353642947377,31.9912388844324,55.7302793931661));
#133260=CARTESIAN_POINT('Ctrl Pts',(4.70467170031233,30.4664369283895,57.0690038373076));
#133261=CARTESIAN_POINT('Ctrl Pts',(4.81580697115087,28.5147183917256,56.5140273547993));
#133262=CARTESIAN_POINT('Ctrl Pts',(4.92694224198944,27.9224362694404,54.5733042859109));
#133263=CARTESIAN_POINT('Ctrl Pts',(5.03807751282801,29.2316897029588,53.0231237837388));
#133264=CARTESIAN_POINT('Ctrl Pts',(5.14921278366655,31.2441559073895,53.2823223919879));
#133265=CARTESIAN_POINT('Ctrl Pts',(5.26034805450513,32.1178812587409,55.1136629263779));
#133266=CARTESIAN_POINT('Ctrl Pts',(5.37148332534367,31.0531695565241,56.8409709862378));
#133267=CARTESIAN_POINT('Ctrl Pts',(5.48261859618223,29.0245214279234,56.8832901641483));
#133268=CARTESIAN_POINT('Ctrl Pts',(5.59375386702079,27.8887013562645,55.2018869087362));
#133269=CARTESIAN_POINT('Ctrl Pts',(5.70488913785936,28.6852934560972,53.3357022530876));
#133270=CARTESIAN_POINT('Ctrl Pts',(5.81602440869791,30.6851994191372,52.9928024404727));
#133271=CARTESIAN_POINT('Ctrl Pts',(5.92715967953647,32.0579616565045,54.4870340095917));
#133272=CARTESIAN_POINT('Ctrl Pts',(6.03829495037504,31.5471295642435,56.4507688990334));
#133273=CARTESIAN_POINT('Ctrl Pts',(6.1494302212136,29.6202533658159,57.0866558846116));
#133274=CARTESIAN_POINT('Ctrl Pts',(6.26056549205216,28.0409485638643,55.8126855219167));
#133275=CARTESIAN_POINT('Ctrl Pts',(6.37170076289071,28.2547083532241,53.7948869950688));
#133276=CARTESIAN_POINT('Ctrl Pts',(6.48283603372927,30.0658844204948,52.8800944525541));
#133277=CARTESIAN_POINT('Ctrl Pts',(6.59397130456782,31.8167583337063,53.9055917380309));
#133278=CARTESIAN_POINT('Ctrl Pts',(6.70510657540639,31.9048045237427,55.9327700752596));
#133279=CARTESIAN_POINT('Ctrl Pts',(6.81624184624495,30.2494367931908,57.106210239539));
#133280=CARTESIAN_POINT('Ctrl Pts',(6.92737711708351,28.3657665926968,56.3518955053601));
#133281=CARTESIAN_POINT('Ctrl Pts',(7.03851238792207,27.9778641921028,54.3602288991636));
#133282=CARTESIAN_POINT('Ctrl Pts',(7.14964765876062,29.4407657312078,52.9541267587214));
#133283=CARTESIAN_POINT('Ctrl Pts',(7.26078292959918,31.4155186423124,53.4205547618593));
#133284=CARTESIAN_POINT('Ctrl Pts',(7.37191820043774,32.0946872167183,55.3326044973854));
#133285=CARTESIAN_POINT('Ctrl Pts',(7.4830534712763,30.8566475903901,56.9402307056887));
#133286=CARTESIAN_POINT('Ctrl Pts',(7.59418874211486,28.8345425579441,56.7720184081006));
#133287=CARTESIAN_POINT('Ctrl Pts',(7.70532401295343,27.8791478885599,54.981927578819));
#133288=CARTESIAN_POINT('Ctrl Pts',(7.81645928379199,28.8649094139022,53.2083779316108));
#133289=CARTESIAN_POINT('Ctrl Pts',(7.92759455463055,30.889587369521,53.0746494839541));
#133290=CARTESIAN_POINT('Ctrl Pts',(8.0387298254691,32.1000510795293,54.7031401408792));
#133291=CARTESIAN_POINT('Ctrl Pts',(8.14986509630766,31.3883971704186,56.6033382322506));
#133292=CARTESIAN_POINT('Ctrl Pts',(8.26100036714621,29.4059824957022,57.0360460701312));
#133293=CARTESIAN_POINT('Ctrl Pts',(8.37213563798479,27.9672552053491,55.6052181722048));
#133294=CARTESIAN_POINT('Ctrl Pts',(8.48327090882334,28.3890421661998,53.620451378599));
#133295=CARTESIAN_POINT('Ctrl Pts',(8.5944061796619,30.2852930441393,52.8983460837889));
#133296=CARTESIAN_POINT('Ctrl Pts',(8.70554145050047,31.9204240408184,54.0998263870268));
#133297=CARTESIAN_POINT('Ctrl Pts',(8.81667672133901,31.7978434168986,56.1252083087096));
#133298=CARTESIAN_POINT('Ctrl Pts',(8.92781199217758,30.0297505244187,57.1207225913341));
#133299=CARTESIAN_POINT('Ctrl Pts',(9.03894726301614,28.2344215423033,56.1751916402329));
#133300=CARTESIAN_POINT('Ctrl Pts',(9.15008253385469,28.0550892200863,54.1540559308596));
#133301=CARTESIAN_POINT('Ctrl Pts',(9.26121780469326,29.6558542920972,52.9071591731169));
#133302=CARTESIAN_POINT('Ctrl Pts',(9.37235307553181,31.5716551089249,53.5758397917641));
#133303=CARTESIAN_POINT('Ctrl Pts',(9.48348834637038,32.0488673895799,55.5478969165061));
#133304=CARTESIAN_POINT('Ctrl Pts',(9.59462361720893,30.6510011538336,57.0187118011999));
#133305=CARTESIAN_POINT('Ctrl Pts',(9.70575888804748,28.6569110170744,56.6413959322557));
#133306=CARTESIAN_POINT('Ctrl Pts',(9.81689415888607,27.892868444028,54.7626704422307));
#133307=CARTESIAN_POINT('Ctrl Pts',(9.9280294297246,29.0559133642249,53.0993483390999));
#133308=CARTESIAN_POINT('Ctrl Pts',(10.0391647005632,31.0861881117667,53.1793157644567));
#133309=CARTESIAN_POINT('Ctrl Pts',(10.1132548811223,31.7714044929558,54.3381091711824));
#133310=CARTESIAN_POINT('Ctrl Pts',(10.1502999714018,31.7932227462577,54.9343843412047));
#133311=CARTESIAN_POINT('Ctrl Pts',(-0.150070245692712,28.5334145918423,
56.248227523579));
#133312=CARTESIAN_POINT('Ctrl Pts',(-0.11301222052309,28.1181981194195,
55.7604027334509));
#133313=CARTESIAN_POINT('Ctrl Pts',(-0.0389091050739475,27.8204647387642,
54.3462020998821));
#133314=CARTESIAN_POINT('Ctrl Pts',(0.0722391006547147,29.3697960138018,
52.8112615761681));
#133315=CARTESIAN_POINT('Ctrl Pts',(0.183374371493274,31.4959388707004,
53.2849719435495));
#133316=CARTESIAN_POINT('Ctrl Pts',(0.294509642331834,32.2527694414669,
55.3258654935888));
#133317=CARTESIAN_POINT('Ctrl Pts',(0.405644913170393,30.9477674461335,
57.0697748615937));
#133318=CARTESIAN_POINT('Ctrl Pts',(0.516780184008953,28.775268199137,56.9186368708072));
#133319=CARTESIAN_POINT('Ctrl Pts',(0.627915454847512,27.7237478317228,
55.0117477585708));
#133320=CARTESIAN_POINT('Ctrl Pts',(0.739050725686071,28.7556086941538,
53.0939432497185));
#133321=CARTESIAN_POINT('Ctrl Pts',(0.850185996524631,30.9264300277611,
52.9207810119399));
#133322=CARTESIAN_POINT('Ctrl Pts',(0.961321267363189,32.2493139546068,
54.6506278654266));
#133323=CARTESIAN_POINT('Ctrl Pts',(1.07245653820176,31.5134652435707,56.7002661125848));
#133324=CARTESIAN_POINT('Ctrl Pts',(1.1835918090403,29.39238389622,57.1936881318183));
#133325=CARTESIAN_POINT('Ctrl Pts',(1.29472707987888,27.8274367212027,55.679294525309));
#133326=CARTESIAN_POINT('Ctrl Pts',(1.40586235071743,28.2509753762695,53.5431590909509));
#133327=CARTESIAN_POINT('Ctrl Pts',(1.51699762155598,30.2753470664941,52.7404304546232));
#133328=CARTESIAN_POINT('Ctrl Pts',(1.62813289239454,32.0477013089184,54.005821485921));
#133329=CARTESIAN_POINT('Ctrl Pts',(1.73926816323311,31.9458522462723,56.1811564489131));
#133330=CARTESIAN_POINT('Ctrl Pts',(1.85040343407167,30.0630194301587,57.2754120145795));
#133331=CARTESIAN_POINT('Ctrl Pts',(1.96153870491023,28.1225067093746,56.2870471513263));
#133332=CARTESIAN_POINT('Ctrl Pts',(2.07267397574878,27.9004107046402,54.1206842434695));
#133333=CARTESIAN_POINT('Ctrl Pts',(2.18380924658734,29.6000096358219,52.7591342987872));
#133334=CARTESIAN_POINT('Ctrl Pts',(2.2949445174259,31.6657084786893,53.4485855920342));
#133335=CARTESIAN_POINT('Ctrl Pts',(2.40607978826446,32.2068312757568,55.5580027938758));
#133336=CARTESIAN_POINT('Ctrl Pts',(2.51721505910302,30.7281035743359,57.1566957550435));
#133337=CARTESIAN_POINT('Ctrl Pts',(2.62835032994158,28.5829631827096,56.7814258490598));
#133338=CARTESIAN_POINT('Ctrl Pts',(2.73948560078014,27.7347966707524,54.7756670470189));
#133339=CARTESIAN_POINT('Ctrl Pts',(2.8506208716187,28.959906953326,52.9752338775547));
#133340=CARTESIAN_POINT('Ctrl Pts',(2.96175614245727,31.1369851011849,53.0280121003562));
#133341=CARTESIAN_POINT('Ctrl Pts',(3.07289141329581,32.2734128157934,54.8856952951807));
#133342=CARTESIAN_POINT('Ctrl Pts',(3.18402668413438,31.3290498241205,56.847998366216));
#133343=CARTESIAN_POINT('Ctrl Pts',(3.29516195497293,29.1682449689211,57.1188805923993));
#133344=CARTESIAN_POINT('Ctrl Pts',(3.40629722581149,27.7687220624047,55.4504111030571));
#133345=CARTESIAN_POINT('Ctrl Pts',(3.51743249665005,28.4114249951292,53.3696930195652));
#133346=CARTESIAN_POINT('Ctrl Pts',(3.62856776748862,30.5081058782719,52.7811489880965));
#133347=CARTESIAN_POINT('Ctrl Pts',(3.73970303832718,32.1397317648171,54.2234567808614));
#133348=CARTESIAN_POINT('Ctrl Pts',(3.85083830916574,31.8129214451303,56.3765127062051));
#133349=CARTESIAN_POINT('Ctrl Pts',(3.96197358000429,29.82679519829,57.26968532912));
#133350=CARTESIAN_POINT('Ctrl Pts',(4.07310885084286,27.9991984271249,56.0854789093014));
#133351=CARTESIAN_POINT('Ctrl Pts',(4.18424412168142,28.0028789712916,53.9077642226845));
#133352=CARTESIAN_POINT('Ctrl Pts',(4.29537939251997,29.8344681323984,52.7297421738124));
#133353=CARTESIAN_POINT('Ctrl Pts',(4.40651466335854,31.8175639487442,53.6296231581121));
#133354=CARTESIAN_POINT('Ctrl Pts',(4.5176499341971,32.1370946851621,55.783771461084));
#133355=CARTESIAN_POINT('Ctrl Pts',(4.62878520503565,30.5006028600674,57.2205558252495));
#133356=CARTESIAN_POINT('Ctrl Pts',(4.73992047587422,28.4059233395712,56.6249279975537));
#133357=CARTESIAN_POINT('Ctrl Pts',(4.85105574671277,27.7702572798392,54.542049349332));
#133358=CARTESIAN_POINT('Ctrl Pts',(4.96219101755134,29.1754119180782,52.8783200307987));
#133359=CARTESIAN_POINT('Ctrl Pts',(5.07332628838988,31.3352887983368,53.1565046185048));
#133360=CARTESIAN_POINT('Ctrl Pts',(5.18446155922844,32.2730134577246,55.121988596025));
#133361=CARTESIAN_POINT('Ctrl Pts',(5.295596830067,31.1303129320237,56.9758198481282));
#133362=CARTESIAN_POINT('Ctrl Pts',(5.40673210090556,28.9530688215398,57.0212388538038));
#133363=CARTESIAN_POINT('Ctrl Pts',(5.51786737174412,27.7340513257388,55.2166748766493));
#133364=CARTESIAN_POINT('Ctrl Pts',(5.6290026425827,28.5889928177436,53.2137944888177));
#133365=CARTESIAN_POINT('Ctrl Pts',(5.74013791342125,30.735389434368,52.8457776864079));
#133366=CARTESIAN_POINT('Ctrl Pts',(5.85127318425982,32.2087048182755,54.4494598813127));
#133367=CARTESIAN_POINT('Ctrl Pts',(5.96240845509836,31.6604549031516,56.5570359376577));
#133368=CARTESIAN_POINT('Ctrl Pts',(6.07354372593693,29.592437391632,57.2395008633215));
#133369=CARTESIAN_POINT('Ctrl Pts',(6.18467899677548,27.8974504541587,55.8722137374748));
#133370=CARTESIAN_POINT('Ctrl Pts',(6.29581426761406,28.1268678853437,53.7066139487367));
#133371=CARTESIAN_POINT('Ctrl Pts',(6.4069495384526,30.0707103733134,52.7248139769108));
#133372=CARTESIAN_POINT('Ctrl Pts',(6.51808480929118,31.9498336485602,53.8254276780467));
#133373=CARTESIAN_POINT('Ctrl Pts',(6.62922008012973,32.0443291137937,56.001094336747));
#133374=CARTESIAN_POINT('Ctrl Pts',(6.74035535096829,30.2677077316937,57.2604875507119));
#133375=CARTESIAN_POINT('Ctrl Pts',(6.85149062180684,28.2460610043493,56.4509201894293));
#133376=CARTESIAN_POINT('Ctrl Pts',(6.9626258926454,27.8297452297067,54.3133664524095));
#133377=CARTESIAN_POINT('Ctrl Pts',(7.07376116348396,29.3998025084083,52.8042690585072));
#133378=CARTESIAN_POINT('Ctrl Pts',(7.18489643432252,31.5192036429601,53.3048623395593));
#133379=CARTESIAN_POINT('Ctrl Pts',(7.29603170516107,32.2481204806333,55.3569673679941));
#133380=CARTESIAN_POINT('Ctrl Pts',(7.40716697599964,30.9193959734275,57.0823502200226));
#133381=CARTESIAN_POINT('Ctrl Pts',(7.51830224683819,28.7491742328494,56.9018165783966));
#133382=CARTESIAN_POINT('Ctrl Pts',(7.62943751767676,27.7237980782675,54.9806037961815));
#133383=CARTESIAN_POINT('Ctrl Pts',(7.7405727885153,28.7817654236807,53.0771438172949));
#133384=CARTESIAN_POINT('Ctrl Pts',(7.85170805935387,30.9547485508914,52.9336199252212));
#133385=CARTESIAN_POINT('Ctrl Pts',(7.96284333019243,32.2538772398021,54.6813955210875));
#133386=CARTESIAN_POINT('Ctrl Pts',(8.07397860103099,31.4900955565868,56.7207807870007));
#133387=CARTESIAN_POINT('Ctrl Pts',(8.18511387186956,29.362471443656,57.185183942138));
#133388=CARTESIAN_POINT('Ctrl Pts',(8.29624914270812,27.8183591477134,55.6495496594077));
#133389=CARTESIAN_POINT('Ctrl Pts',(8.40738441354667,28.2710414850018,53.5194011377699));
#133390=CARTESIAN_POINT('Ctrl Pts',(8.51851968438524,30.3061904089512,52.7444025176994));
#133391=CARTESIAN_POINT('Ctrl Pts',(8.62965495522378,32.0610927412963,54.0338897763355));
#133392=CARTESIAN_POINT('Ctrl Pts',(8.74079022606235,31.9295332373459,56.2076284342593));
#133393=CARTESIAN_POINT('Ctrl Pts',(8.85192549690091,30.0319297137642,57.2760629144379));
#133394=CARTESIAN_POINT('Ctrl Pts',(8.96306076773945,28.1050950904588,56.2612729833792));
#133395=CARTESIAN_POINT('Ctrl Pts',(9.07419603857805,27.9126268960678,54.0920915675973));
#133396=CARTESIAN_POINT('Ctrl Pts',(9.18533130941658,29.6306460420042,52.753861154988));
#133397=CARTESIAN_POINT('Ctrl Pts',(9.29646658025515,31.686776913835,53.4715218070343));
#133398=CARTESIAN_POINT('Ctrl Pts',(9.40760185109372,32.1989444074769,55.5880296921861));
#133399=CARTESIAN_POINT('Ctrl Pts',(9.51873712193226,30.698686188166,57.1665799593141));
#133400=CARTESIAN_POINT('Ctrl Pts',(9.62987239277085,28.5585313999489,56.7616261667521));
#133401=CARTESIAN_POINT('Ctrl Pts',(9.74100766360938,27.7385236475588,54.7452863438404));
#133402=CARTESIAN_POINT('Ctrl Pts',(9.85214293444796,28.9867601785899,52.9601279411475));
#133403=CARTESIAN_POINT('Ctrl Pts',(9.9632782052865,31.1657500558526,53.0459528821187));
#133404=CARTESIAN_POINT('Ctrl Pts',(10.0373683858456,31.9011576947219,54.2896264815424));
#133405=CARTESIAN_POINT('Ctrl Pts',(10.0744134761251,31.9245741082599,54.9295780748502));
#133406=CARTESIAN_POINT('Ctrl Pts',(-0.225956740969381,28.4333207632767,
56.3334185196581));
#133407=CARTESIAN_POINT('Ctrl Pts',(-0.188898715799759,27.9897659437127,
55.8122998956753));
#133408=CARTESIAN_POINT('Ctrl Pts',(-0.114795600350617,27.6717123868196,
54.3015806720628));
#133409=CARTESIAN_POINT('Ctrl Pts',(-0.00364739462195415,29.326784860544,
52.6618811123017));
#133410=CARTESIAN_POINT('Ctrl Pts',(0.107487876216605,31.5980360605646,
53.1679220102057));
#133411=CARTESIAN_POINT('Ctrl Pts',(0.218623147055165,32.4065199949758,
55.3481056745352));
#133412=CARTESIAN_POINT('Ctrl Pts',(0.329758417893724,31.0124521700819,
57.2110361130788));
#133413=CARTESIAN_POINT('Ctrl Pts',(0.440893688732284,28.6916807761116,
57.0495830188858));
#133414=CARTESIAN_POINT('Ctrl Pts',(0.552028959570843,27.5683945921251,
55.0125495380824));
#133415=CARTESIAN_POINT('Ctrl Pts',(0.663164230409402,28.6706795182987,
52.9638556895));
#133416=CARTESIAN_POINT('Ctrl Pts',(0.774299501247962,30.9896584820065,
52.7788752028517));
#133417=CARTESIAN_POINT('Ctrl Pts',(0.885434772086521,32.4028286726114,
54.6267833662593));
#133418=CARTESIAN_POINT('Ctrl Pts',(0.996570042925081,31.6167586009078,
56.8163085495561));
#133419=CARTESIAN_POINT('Ctrl Pts',(1.10770531376365,29.3509143563028,57.3434064111436));
#133420=CARTESIAN_POINT('Ctrl Pts',(1.21884058460219,27.6791602040858,55.7256560869226));
#133421=CARTESIAN_POINT('Ctrl Pts',(1.32997585544075,28.1316051917093,53.4437303202929));
#133422=CARTESIAN_POINT('Ctrl Pts',(1.44111112627932,30.2941393863388,52.5862157969229));
#133423=CARTESIAN_POINT('Ctrl Pts',(1.55224639711788,32.1874560498483,53.937969226381));
#133424=CARTESIAN_POINT('Ctrl Pts',(1.66338166795644,32.0786558321182,56.261769872754));
#133425=CARTESIAN_POINT('Ctrl Pts',(1.77451693879499,30.0673204793875,57.4307079140457));
#133426=CARTESIAN_POINT('Ctrl Pts',(1.88565220963356,27.9943685930944,56.3748875704415));
#133427=CARTESIAN_POINT('Ctrl Pts',(1.99678748047212,27.7571146307674,54.06067131814));
#133428=CARTESIAN_POINT('Ctrl Pts',(2.10792275131068,29.5727104640742,52.6061961704733));
#133429=CARTESIAN_POINT('Ctrl Pts',(2.21905802214923,31.779392371887,53.3427022204136));
#133430=CARTESIAN_POINT('Ctrl Pts',(2.33019329298779,32.3574465690499,55.5960862465536));
#133431=CARTESIAN_POINT('Ctrl Pts',(2.44132856382636,30.7777963327271,57.3038893204322));
#133432=CARTESIAN_POINT('Ctrl Pts',(2.55246383466492,28.4862510243367,56.9030074034286));
#133433=CARTESIAN_POINT('Ctrl Pts',(2.66359910550347,27.5801975097059,54.7603564186625));
#133434=CARTESIAN_POINT('Ctrl Pts',(2.77473437634204,28.8889210465201,52.837044453319));
#133435=CARTESIAN_POINT('Ctrl Pts',(2.88586964718059,31.2145838493837,52.8934247673154));
#133436=CARTESIAN_POINT('Ctrl Pts',(2.99700491801916,32.428572270795,54.8778940478309));
#133437=CARTESIAN_POINT('Ctrl Pts',(3.10814018885771,31.4197569077386,56.9741234664856));
#133438=CARTESIAN_POINT('Ctrl Pts',(3.21927545969628,29.1114780428174,57.2634932890667));
#133439=CARTESIAN_POINT('Ctrl Pts',(3.33041073053483,27.6164382948684,55.4811514687273));
#133440=CARTESIAN_POINT('Ctrl Pts',(3.44154600137339,28.3030054286198,53.2584252635236));
#133441=CARTESIAN_POINT('Ctrl Pts',(3.55268127221196,30.5427838877422,52.6297133529383));
#133442=CARTESIAN_POINT('Ctrl Pts',(3.6638165430505,32.2857675451084,54.1704580373733));
#133443=CARTESIAN_POINT('Ctrl Pts',(3.77495181388906,31.9366525604971,56.4704591112811));
#133444=CARTESIAN_POINT('Ctrl Pts',(3.88608708472762,29.8149740444501,57.424590384746));
#133445=CARTESIAN_POINT('Ctrl Pts',(3.99722235556618,27.8626445731759,56.1595623818731));
#133446=CARTESIAN_POINT('Ctrl Pts',(4.10835762640474,27.866576312912,53.8332195967528));
#133447=CARTESIAN_POINT('Ctrl Pts',(4.21949289724331,29.8231706530387,52.5747980455056));
#133448=CARTESIAN_POINT('Ctrl Pts',(4.33062816808186,31.9416119130024,53.5360955231585));
#133449=CARTESIAN_POINT('Ctrl Pts',(4.44176343892042,32.2829504858917,55.8372635290018));
#133450=CARTESIAN_POINT('Ctrl Pts',(4.55289870975898,30.5347687917455,57.3721078131917));
#133451=CARTESIAN_POINT('Ctrl Pts',(4.66403398059754,28.2971282874166,56.7358286403078));
#133452=CARTESIAN_POINT('Ctrl Pts',(4.77516925143611,27.6180782902379,54.5107944127531));
#133453=CARTESIAN_POINT('Ctrl Pts',(4.88630452227465,29.1191341331977,52.7335162778585));
#133454=CARTESIAN_POINT('Ctrl Pts',(4.99743979311322,31.426421689284,53.0306868450219));
#133455=CARTESIAN_POINT('Ctrl Pts',(5.10857506395178,32.4281456567085,55.130314265672));
#133456=CARTESIAN_POINT('Ctrl Pts',(5.21971033479033,31.2074563075231,57.1106687100188));
#133457=CARTESIAN_POINT('Ctrl Pts',(5.3308456056289,28.8816162151564,57.1591875434591));
#133458=CARTESIAN_POINT('Ctrl Pts',(5.44198087646746,27.5794012952129,55.2314628445626));
#133459=CARTESIAN_POINT('Ctrl Pts',(5.55311614730602,28.4926921793899,53.0918867245477));
#133460=CARTESIAN_POINT('Ctrl Pts',(5.66425141814458,30.7855794495987,52.6987529323434));
#133461=CARTESIAN_POINT('Ctrl Pts',(5.77538668898315,32.3594479800464,54.4118857530334));
#133462=CARTESIAN_POINT('Ctrl Pts',(5.88652195982169,31.7737802420597,56.6633029762821));
#133463=CARTESIAN_POINT('Ctrl Pts',(5.99765723066025,29.5646214174482,57.3923458420313));
#133464=CARTESIAN_POINT('Ctrl Pts',(6.10879250149881,27.7539523444532,55.9317419530332));
#133465=CARTESIAN_POINT('Ctrl Pts',(6.21992777233738,27.9990274174633,53.6183409024045));
#133466=CARTESIAN_POINT('Ctrl Pts',(6.33106304317593,30.0755363261321,52.5695335012675));
#133467=CARTESIAN_POINT('Ctrl Pts',(6.44219831401451,32.082908963414,53.7452636180623));
#133468=CARTESIAN_POINT('Ctrl Pts',(6.55333358485306,32.1838537038447,56.0694185982343));
#133469=CARTESIAN_POINT('Ctrl Pts',(6.66446885569162,30.2859786701968,57.4147648618848));
#133470=CARTESIAN_POINT('Ctrl Pts',(6.77560412653018,28.1263554160018,56.5499448734984));
#133471=CARTESIAN_POINT('Ctrl Pts',(6.88673939736874,27.6816262673105,54.2665040056556));
#133472=CARTESIAN_POINT('Ctrl Pts',(6.9978746682073,29.3588392856087,52.6544113582929));
#133473=CARTESIAN_POINT('Ctrl Pts',(7.10900993904585,31.622888643608,53.1891699172596));
#133474=CARTESIAN_POINT('Ctrl Pts',(7.22014520988442,32.4015537445481,55.3813302386028));
#133475=CARTESIAN_POINT('Ctrl Pts',(7.33128048072298,30.982144356465,57.2244697343568));
#133476=CARTESIAN_POINT('Ctrl Pts',(7.44241575156153,28.6638059077547,57.0316147486923));
#133477=CARTESIAN_POINT('Ctrl Pts',(7.5535510224001,27.5684482679751,54.9792800135439));
#133478=CARTESIAN_POINT('Ctrl Pts',(7.66468629323865,28.6986214334592,52.9459097029788));
#133479=CARTESIAN_POINT('Ctrl Pts',(7.77582156407722,31.019909732262,52.7925903664883));
#133480=CARTESIAN_POINT('Ctrl Pts',(7.88695683491577,32.4077034000748,54.6596509012957));
#133481=CARTESIAN_POINT('Ctrl Pts',(7.99809210575433,31.591793942755,56.8382233417508));
#133482=CARTESIAN_POINT('Ctrl Pts',(8.10922737659289,29.3189603916098,57.3343218141449));
#133483=CARTESIAN_POINT('Ctrl Pts',(8.22036264743145,27.6694630900778,55.6938811466105));
#133484=CARTESIAN_POINT('Ctrl Pts',(8.33149791827,28.1530408038039,53.4183508969409));
#133485=CARTESIAN_POINT('Ctrl Pts',(8.44263318910856,30.3270877737631,52.5904589516098));
#133486=CARTESIAN_POINT('Ctrl Pts',(8.55376845994713,32.2017614417742,53.9679531656445));
#133487=CARTESIAN_POINT('Ctrl Pts',(8.66490373078569,32.061223057793,56.2900485598091));
#133488=CARTESIAN_POINT('Ctrl Pts',(8.77603900162424,30.0341089031096,57.4314032375418));
#133489=CARTESIAN_POINT('Ctrl Pts',(8.8871742724628,27.9757686386143,56.3473543265254));
#133490=CARTESIAN_POINT('Ctrl Pts',(8.99830954330136,27.7701645720494,54.0301272043351));
#133491=CARTESIAN_POINT('Ctrl Pts',(9.10944481413992,29.6054377919111,52.6005631368589));
#133492=CARTESIAN_POINT('Ctrl Pts',(9.22058008497849,31.8018987187452,53.3672038223045));
#133493=CARTESIAN_POINT('Ctrl Pts',(9.33171535581705,32.3490214253738,55.6281624678661));
#133494=CARTESIAN_POINT('Ctrl Pts',(9.44285062665559,30.7463712224987,57.3144481174284));
#133495=CARTESIAN_POINT('Ctrl Pts',(9.55398589749417,28.4601517828233,56.8818564012485));
#133496=CARTESIAN_POINT('Ctrl Pts',(9.66512116833272,27.5841788510897,54.7279022454503));
#133497=CARTESIAN_POINT('Ctrl Pts',(9.77625643917129,28.9176069929546,52.8209075431952));
#133498=CARTESIAN_POINT('Ctrl Pts',(9.88739171000984,31.2453119999385,52.9125899997809));
#133499=CARTESIAN_POINT('Ctrl Pts',(9.96148189056888,32.030910896488,54.2411437919026));
#133500=CARTESIAN_POINT('Ctrl Pts',(9.9985269808484,32.0559254702622,54.9247718084957));
#133501=CARTESIAN_POINT('',(10.0008693306327,29.2294100445698,53.5212313410887));
#133502=CARTESIAN_POINT('Ctrl Pts',(10.,32.0533758325287,54.9248651020699));
#133503=CARTESIAN_POINT('Ctrl Pts',(9.99999999999998,32.0436832069832,54.8508488304773));
#133504=CARTESIAN_POINT('Ctrl Pts',(10.,32.0296436856721,54.777570200097));
#133505=CARTESIAN_POINT('Ctrl Pts',(10.,32.011488473763,54.7053068406861));
#133506=CARTESIAN_POINT('Ctrl Pts',(10.,31.9938094546564,54.6349388759312));
#133507=CARTESIAN_POINT('Ctrl Pts',(9.99999999999998,31.9722270068482,54.5655330028697));
#133508=CARTESIAN_POINT('Ctrl Pts',(9.99999999999999,31.9469147886137,54.4973682067378));
#133509=CARTESIAN_POINT('Ctrl Pts',(9.99999999999999,31.9412650452606,54.4821536727806));
#133510=CARTESIAN_POINT('Ctrl Pts',(10.,31.9354285487349,54.4669990730982));
#133511=CARTESIAN_POINT('Ctrl Pts',(10.,31.9294095815725,54.4519141334687));
#133512=CARTESIAN_POINT('Ctrl Pts',(10.,31.9017891954822,54.3826909851324));
#133513=CARTESIAN_POINT('Ctrl Pts',(10.,31.8703857715094,54.3150694449083));
#133514=CARTESIAN_POINT('Ctrl Pts',(10.,31.8354092014842,54.2493420824359));
#133515=CARTESIAN_POINT('Ctrl Pts',(10.,31.8108541343843,54.2031986271272));
#133516=CARTESIAN_POINT('Ctrl Pts',(10.,31.7845369863314,54.1579892552018));
#133517=CARTESIAN_POINT('Ctrl Pts',(10.,31.7565193347055,54.1138258658698));
#133518=CARTESIAN_POINT('Ctrl Pts',(10.,31.7458689517922,54.0970379846649));
#133519=CARTESIAN_POINT('Ctrl Pts',(10.,31.7349727648439,54.080401351714));
#133520=CARTESIAN_POINT('Ctrl Pts',(10.,31.7238338766828,54.063922520157));
#133521=CARTESIAN_POINT('Ctrl Pts',(10.,31.7132202172074,54.0482207100508));
#133522=CARTESIAN_POINT('Ctrl Pts',(10.,31.702382609243,54.0326574079742));
#133523=CARTESIAN_POINT('Ctrl Pts',(10.,31.6913434743771,54.0172654257873));
#133524=CARTESIAN_POINT('Ctrl Pts',(9.99999999999999,31.6490748357409,53.9583298170775));
#133525=CARTESIAN_POINT('Ctrl Pts',(10.,31.6038135855978,53.9018382421701));
#133526=CARTESIAN_POINT('Ctrl Pts',(10.,31.5557517714265,53.8480620861241));
#133527=CARTESIAN_POINT('Ctrl Pts',(10.,31.5087931407094,53.7955202772746));
#133528=CARTESIAN_POINT('Ctrl Pts',(10.,31.4591602697449,53.7455701374524));
#133529=CARTESIAN_POINT('Ctrl Pts',(10.,31.4070038374311,53.6985041612426));
#133530=CARTESIAN_POINT('Ctrl Pts',(10.,31.3556856160202,53.6521945867392));
#133531=CARTESIAN_POINT('Ctrl Pts',(9.99999999999999,31.3019236685778,53.6086767368471));
#133532=CARTESIAN_POINT('Ctrl Pts',(9.99999999999999,31.2458437756219,53.5682751968982));
#133533=CARTESIAN_POINT('Ctrl Pts',(9.99999999999999,31.2276727281975,53.5551842607403));
#133534=CARTESIAN_POINT('Ctrl Pts',(10.,31.2092582189262,53.5424208988166));
#133535=CARTESIAN_POINT('Ctrl Pts',(10.,31.1906042818692,53.5299973393956));
#133536=CARTESIAN_POINT('Ctrl Pts',(10.,31.1801024108385,53.5230030722668));
#133537=CARTESIAN_POINT('Ctrl Pts',(10.,31.1695235040959,53.5161159030876));
#133538=CARTESIAN_POINT('Ctrl Pts',(10.,31.1588834524544,53.5093474110969));
#133539=CARTESIAN_POINT('Ctrl Pts',(10.,31.101253429008,53.4726870296196));
#133540=CARTESIAN_POINT('Ctrl Pts',(9.99999999999998,31.0417325215066,53.4394372488709));
#133541=CARTESIAN_POINT('Ctrl Pts',(9.99999999999999,30.9804647762413,53.409865079986));
#133542=CARTESIAN_POINT('Ctrl Pts',(9.99999999999999,30.9716322758967,53.4056018874899));
#133543=CARTESIAN_POINT('Ctrl Pts',(9.99999999999998,30.9627634386846,53.4014152082538));
#133544=CARTESIAN_POINT('Ctrl Pts',(9.99999999999999,30.9538586655155,53.3973059277124));
#133545=CARTESIAN_POINT('Ctrl Pts',(9.99999999999999,30.8905564254343,53.3680938794712));
#133546=CARTESIAN_POINT('Ctrl Pts',(9.99999999999997,30.8254386050166,53.3427888225031));
#133547=CARTESIAN_POINT('Ctrl Pts',(9.99999999999996,30.7588787740053,53.3213756036074));
#133548=CARTESIAN_POINT('Ctrl Pts',(9.99999999999995,30.697419300789,53.3016032404087));
#133549=CARTESIAN_POINT('Ctrl Pts',(9.99999999999996,30.6347294993411,53.2851497911376));
#133550=CARTESIAN_POINT('Ctrl Pts',(9.99999999999998,30.5711069811699,53.2720426229371));
#133551=CARTESIAN_POINT('Ctrl Pts',(9.99999999999999,30.557055646849,53.269147842792));
#133552=CARTESIAN_POINT('Ctrl Pts',(9.99999999999998,30.5429588580867,53.2664164255331));
#133553=CARTESIAN_POINT('Ctrl Pts',(9.99999999999997,30.5288199046136,53.2638489053184));
#133554=CARTESIAN_POINT('Ctrl Pts',(9.99999999999997,30.5176851752098,53.2618269280282));
#133555=CARTESIAN_POINT('Ctrl Pts',(9.99999999999999,30.5065248337635,53.2599067801427));
#133556=CARTESIAN_POINT('Ctrl Pts',(9.99999999999999,30.4953536355096,53.2580906150721));
#133557=CARTESIAN_POINT('Ctrl Pts',(9.99999999999998,30.4278879692109,53.247122338992));
#133558=CARTESIAN_POINT('Ctrl Pts',(9.99999999999995,30.3599021685379,53.2399190427721));
#133559=CARTESIAN_POINT('Ctrl Pts',(9.99999999999996,30.2917474304394,53.2364479110107));
#133560=CARTESIAN_POINT('Ctrl Pts',(9.99999999999997,30.2243114893283,53.2330133876953));
#133561=CARTESIAN_POINT('Ctrl Pts',(9.99999999999996,30.1567090796788,53.233233010574));
#133562=CARTESIAN_POINT('Ctrl Pts',(9.99999999999997,30.0892889665376,53.2371242546236));
#133563=CARTESIAN_POINT('Ctrl Pts',(9.99999999999998,30.0224411516751,53.2409824676953));
#133564=CARTESIAN_POINT('Ctrl Pts',(9.99999999999999,29.9557715754486,53.2484504808556));
#133565=CARTESIAN_POINT('Ctrl Pts',(9.99999999999998,29.8896438474063,53.2595900690709));
#133566=CARTESIAN_POINT('Ctrl Pts',(9.99999999999998,29.8705616649699,53.2628045701717));
#133567=CARTESIAN_POINT('Ctrl Pts',(9.99999999999998,29.851524804742,53.2663250773652));
#133568=CARTESIAN_POINT('Ctrl Pts',(9.99999999999999,29.8325425498808,53.2701537316448));
#133569=CARTESIAN_POINT('Ctrl Pts',(10.,29.8219564844318,53.2722889039455));
#133570=CARTESIAN_POINT('Ctrl Pts',(9.99999999999997,29.8113968593313,53.2745180133388));
#133571=CARTESIAN_POINT('Ctrl Pts',(9.99999999999996,29.8008654253447,53.2768409064225));
#133572=CARTESIAN_POINT('Ctrl Pts',(9.99999999999995,29.7370929698571,53.2909070436615));
#133573=CARTESIAN_POINT('Ctrl Pts',(9.99999999999996,29.6743481658389,53.3084091960948));
#133574=CARTESIAN_POINT('Ctrl Pts',(9.99999999999998,29.6129512937306,53.3293566255847));
#133575=CARTESIAN_POINT('Ctrl Pts',(9.99999999999999,29.5524450572685,53.350000187357));
#133576=CARTESIAN_POINT('Ctrl Pts',(10.,29.4932470869475,53.3739901108916));
#133577=CARTESIAN_POINT('Ctrl Pts',(9.99999999999999,29.4356920546672,53.4013774099463));
#133578=CARTESIAN_POINT('Ctrl Pts',(9.99999999999998,29.3781370223868,53.428764709001));
#133579=CARTESIAN_POINT('Ctrl Pts',(10.,29.3222240651368,53.4595495870449));
#133580=CARTESIAN_POINT('Ctrl Pts',(10.,29.2683289856055,53.4938218112857));
#133581=CARTESIAN_POINT('Ctrl Pts',(10.,29.2642059165283,53.4964436971648));
#133582=CARTESIAN_POINT('Ctrl Pts',(9.99999999999998,29.2600946807948,53.4990860107153));
#133583=CARTESIAN_POINT('Ctrl Pts',(9.99999999999999,29.2559954588133,53.5017488009346));
#133584=CARTESIAN_POINT('Ctrl Pts',(10.,29.2468791070862,53.5076706398406));
#133585=CARTESIAN_POINT('Ctrl Pts',(9.99999999999998,29.2378221709542,53.5136937523903));
#133586=CARTESIAN_POINT('Ctrl Pts',(9.99999999999999,29.2288257276126,53.5198168253508));
#133587=CARTESIAN_POINT('Ctrl Pts',(-1.11065670549415E-15,28.7309291201476,
56.0793586530485));
#133588=CARTESIAN_POINT('Ctrl Pts',(1.40820494214792E-14,28.6853758729853,
56.036862308157));
#133589=CARTESIAN_POINT('Ctrl Pts',(7.46374256104984E-15,28.6425793874778,
55.9917717289187));
#133590=CARTESIAN_POINT('Ctrl Pts',(3.6949610038306E-15,28.6025382767428,
55.9444368944416));
#133591=CARTESIAN_POINT('Ctrl Pts',(-2.11776492034417E-16,28.5610314644456,
55.8953693722451));
#133592=CARTESIAN_POINT('Ctrl Pts',(-1.42116051368288E-14,28.5224848860696,
55.8438898433626));
#133593=CARTESIAN_POINT('Ctrl Pts',(4.5102810375397E-16,28.4869236243661,
55.7903375225762));
#133594=CARTESIAN_POINT('Ctrl Pts',(1.38529299224628E-14,28.4544200126287,
55.7413897699068));
#133595=CARTESIAN_POINT('Ctrl Pts',(3.2556342786873E-15,28.4244104857153,
55.6907093010964));
#133596=CARTESIAN_POINT('Ctrl Pts',(4.71844785465692E-16,28.3969384585817,
55.6385258504283));
#133597=CARTESIAN_POINT('Ctrl Pts',(-9.03483966360219E-16,28.383435856458,
55.612877492978));
#133598=CARTESIAN_POINT('Ctrl Pts',(-2.82856510769481E-14,28.3705466339733,
55.5868656756228));
#133599=CARTESIAN_POINT('Ctrl Pts',(-1.21569421196455E-14,28.3582783186024,
55.5605158043874));
#133600=CARTESIAN_POINT('Ctrl Pts',(-4.6121945743922E-15,28.3526720561333,
55.5484746814046));
#133601=CARTESIAN_POINT('Ctrl Pts',(1.38947693528612E-14,28.3471948800546,
55.5363612929739));
#133602=CARTESIAN_POINT('Ctrl Pts',(9.5964902691037E-15,28.3418560093508,
55.524197994614));
#133603=CARTESIAN_POINT('Ctrl Pts',(-1.11574869560312E-14,28.3149353070124,
55.4628658229304));
#133604=CARTESIAN_POINT('Ctrl Pts',(-7.98462157858785E-15,28.2914758629066,
55.400158212843));
#133605=CARTESIAN_POINT('Ctrl Pts',(-9.95731275210687E-15,28.2715012520033,
55.3364328839772));
#133606=CARTESIAN_POINT('Ctrl Pts',(-1.19923092204882E-14,28.2511181538008,
55.2714043513795));
#133607=CARTESIAN_POINT('Ctrl Pts',(-3.07508960440585E-14,28.2343632979817,
55.2053152157044));
#133608=CARTESIAN_POINT('Ctrl Pts',(-2.47163400857175E-14,28.2213014270528,
55.1385087524746));
#133609=CARTESIAN_POINT('Ctrl Pts',(-1.96985779232646E-14,28.2104404188577,
55.0829588585445));
#133610=CARTESIAN_POINT('Ctrl Pts',(-3.14336743467927E-14,28.2021333189636,
55.0269120563622));
#133611=CARTESIAN_POINT('Ctrl Pts',(-2.94902990916057E-14,28.1964419417431,
54.9705535356952));
#133612=CARTESIAN_POINT('Ctrl Pts',(-2.86701166028188E-14,28.1938115155022,
54.9445058980301));
#133613=CARTESIAN_POINT('Ctrl Pts',(-1.27533407423501E-14,28.191740161086,
54.9183915626081));
#133614=CARTESIAN_POINT('Ctrl Pts',(-2.15660822533437E-14,28.1902357805568,
54.8922284121185));
#133615=CARTESIAN_POINT('Ctrl Pts',(-2.53088403276183E-14,28.1895788075958,
54.8808027906674));
#133616=CARTESIAN_POINT('Ctrl Pts',(2.03905128226202E-15,28.1890300817403,
54.8693680844173));
#133617=CARTESIAN_POINT('Ctrl Pts',(1.98452365651747E-15,28.1885905940451,
54.8579398818212));
#133618=CARTESIAN_POINT('Ctrl Pts',(1.7123297641234E-15,28.1858938459936,
54.7878150901245));
#133619=CARTESIAN_POINT('Ctrl Pts',(-2.75809254679551E-14,28.1872979880003,
54.7178038384048));
#133620=CARTESIAN_POINT('Ctrl Pts',(-6.75848266240564E-15,28.1928577234074,
54.6482668481114));
#133621=CARTESIAN_POINT('Ctrl Pts',(1.18107030287633E-14,28.1978277731874,
54.5861052022779));
#133622=CARTESIAN_POINT('Ctrl Pts',(2.36466186055739E-15,28.2061189999238,
54.5243215858547));
#133623=CARTESIAN_POINT('Ctrl Pts',(5.45397060847108E-15,28.2178036028124,
54.4631615531338));
#133624=CARTESIAN_POINT('Ctrl Pts',(8.86164441660497E-15,28.2305350890377,
54.3965218802625));
#133625=CARTESIAN_POINT('Ctrl Pts',(-2.00354280069877E-14,28.2472941633897,
54.3306217037811));
#133626=CARTESIAN_POINT('Ctrl Pts',(-6.66133814775094E-16,28.2678355467659,
54.2656746420521));
#133627=CARTESIAN_POINT('Ctrl Pts',(6.62424595565122E-15,28.2757636019639,
54.2406079812093));
#133628=CARTESIAN_POINT('Ctrl Pts',(-1.52339698000625E-14,28.2842556294877,
54.2156833448971));
#133629=CARTESIAN_POINT('Ctrl Pts',(-6.80011602582908E-15,28.293299536066,
54.1909133347334));
#133630=CARTESIAN_POINT('Ctrl Pts',(-3.37245178901788E-15,28.2972665004933,
54.1800483674392));
#133631=CARTESIAN_POINT('Ctrl Pts',(-2.17185403739263E-14,28.3013395419173,
54.1692137249702));
#133632=CARTESIAN_POINT('Ctrl Pts',(-1.84574577843932E-14,28.3055125585617,
54.1584229955393));
#133633=CARTESIAN_POINT('Ctrl Pts',(1.52368349615535E-15,28.3310282228841,
54.0924437164197));
#133634=CARTESIAN_POINT('Ctrl Pts',(1.85341033795595E-14,28.3603207357524,
54.0279841981644));
#133635=CARTESIAN_POINT('Ctrl Pts',(8.10462807976364E-15,28.3930667172485,
53.9652709772947));
#133636=CARTESIAN_POINT('Ctrl Pts',(-2.32484722003222E-15,28.4258126987446,
53.902557756425));
#133637=CARTESIAN_POINT('Ctrl Pts',(3.91496741470812E-15,28.4620126514484,
53.8415900456593));
#133638=CARTESIAN_POINT('Ctrl Pts',(8.29891710907305E-15,28.5013974153454,
53.7825980208192));
#133639=CARTESIAN_POINT('Ctrl Pts',(1.17608196074637E-14,28.5318861331045,
53.7369308384517));
#133640=CARTESIAN_POINT('Ctrl Pts',(1.13837602802617E-15,28.5642845662645,
53.6924475817031));
#133641=CARTESIAN_POINT('Ctrl Pts',(5.41233724504764E-15,28.5984872509066,
53.6492611078387));
#133642=CARTESIAN_POINT('Ctrl Pts',(7.69524181669997E-15,28.6197781352125,
53.6223778900957));
#133643=CARTESIAN_POINT('Ctrl Pts',(-1.25356090036905E-15,28.6417684828538,
53.5959972930288));
#133644=CARTESIAN_POINT('Ctrl Pts',(-2.83106871279415E-15,28.6644357593109,
53.5701482268476));
#133645=CARTESIAN_POINT('Ctrl Pts',(-3.72072440462852E-15,28.6771277964087,
53.5556746173897));
#133646=CARTESIAN_POINT('Ctrl Pts',(4.76010837754156E-15,28.6900365447023,
53.5413631052373));
#133647=CARTESIAN_POINT('Ctrl Pts',(7.04991620636974E-15,28.7031343143651,
53.5272442252728));
#133648=CARTESIAN_POINT('Ctrl Pts',(1.66473880124441E-14,28.7540075643444,
53.4724048649576));
#133649=CARTESIAN_POINT('Ctrl Pts',(-2.32322889134241E-14,28.8077773503859,
53.4204104165983));
#133650=CARTESIAN_POINT('Ctrl Pts',(-2.78110867668602E-14,28.8641586498734,
53.3715248576467));
#133651=CARTESIAN_POINT('Ctrl Pts',(-3.11620636517304E-14,28.9063242170955,
53.3349650879907));
#133652=CARTESIAN_POINT('Ctrl Pts',(1.24250061455589E-14,28.9499515635121,
53.3001443221104));
#133653=CARTESIAN_POINT('Ctrl Pts',(7.99360577730113E-15,28.9949378639353,
53.2671827247916));
#133654=CARTESIAN_POINT('Ctrl Pts',(6.58027310319314E-15,29.0089885716387,
53.2568877290927));
#133655=CARTESIAN_POINT('Ctrl Pts',(-7.25313467225921E-15,29.0231719403568,
53.2467741756668));
#133656=CARTESIAN_POINT('Ctrl Pts',(-1.13520304267922E-14,29.0374850778181,
53.2368459519368));
#133657=CARTESIAN_POINT('Ctrl Pts',(-1.54901283588251E-14,29.0512799828038,
53.2272771971196));
#133658=CARTESIAN_POINT('Ctrl Pts',(1.57215114802889E-14,29.0651883995786,
53.2178855342609));
#133659=CARTESIAN_POINT('Ctrl Pts',(1.40443212615082E-14,29.0792023373798,
53.2086772026791));
#133660=CARTESIAN_POINT('Ctrl Pts',(5.95643201164454E-15,29.1421574061881,
53.167310446485));
#133661=CARTESIAN_POINT('Ctrl Pts',(5.87521379537194E-15,29.2072697599874,
53.1296194531803));
#133662=CARTESIAN_POINT('Ctrl Pts',(6.55031584528842E-15,29.2742780365298,
53.0958834461281));
#133663=CARTESIAN_POINT('Ctrl Pts',(7.02525033480137E-15,29.3255312944275,
53.070079465499));
#133664=CARTESIAN_POINT('Ctrl Pts',(-8.85054505632768E-15,29.3778947184249,
53.0465897193344));
#133665=CARTESIAN_POINT('Ctrl Pts',(-1.17683640610267E-14,29.4312652422325,
53.0255544368292));
#133666=CARTESIAN_POINT('Ctrl Pts',(-1.23454027065879E-14,29.4435451349662,
53.0207144803446));
#133667=CARTESIAN_POINT('Ctrl Pts',(-2.95665940748309E-14,29.4558783869943,
53.0160045294466));
#133668=CARTESIAN_POINT('Ctrl Pts',(-2.77555756156289E-16,29.4682631373226,
53.0114240182723));
#133669=CARTESIAN_POINT('Ctrl Pts',(10.,29.207701741744,53.534455913333));
#133670=CARTESIAN_POINT('Ctrl Pts',(10.0002897768776,29.215139018462,53.530435194036));
#133671=CARTESIAN_POINT('Ctrl Pts',(10.0005795537551,29.2226069020107,53.5264710893684));
#133672=CARTESIAN_POINT('Ctrl Pts',(10.0008693306327,29.2301045269737,53.5225640587107));
#133673=CARTESIAN_POINT('Ctrl Pts',(0.00154681533403014,30.5308614994839,
53.0122372304288));
#133674=CARTESIAN_POINT('Ctrl Pts',(0.03859190561355,31.1918243307126,53.1887571477249));
#133675=CARTESIAN_POINT('Ctrl Pts',(0.11268208617259,32.3123254329236,54.2503594776237));
#133676=CARTESIAN_POINT('Ctrl Pts',(0.223817357011149,31.8837204066822,
56.5402431757408));
#133677=CARTESIAN_POINT('Ctrl Pts',(0.334952627849709,29.7276879431726,
57.4159501049812));
#133678=CARTESIAN_POINT('Ctrl Pts',(0.446087898688268,27.822541677856,56.08255543116));
#133679=CARTESIAN_POINT('Ctrl Pts',(0.557223169526827,27.9095331143253,
53.757251657784));
#133680=CARTESIAN_POINT('Ctrl Pts',(0.668358440365387,29.9102877014042,
52.5699427782862));
#133681=CARTESIAN_POINT('Ctrl Pts',(0.779493711203945,31.9929427887065,
53.6065233542934));
#133682=CARTESIAN_POINT('Ctrl Pts',(0.890628982042508,32.2516197117106,
55.9186517555512));
#133683=CARTESIAN_POINT('Ctrl Pts',(1.00176425288106,30.4493989709057,57.3898945361969));
#133684=CARTESIAN_POINT('Ctrl Pts',(1.11289952371963,28.2358830289503,56.6737692472272));
#133685=CARTESIAN_POINT('Ctrl Pts',(1.22403479455818,27.6370000288693,54.425672429537));
#133686=CARTESIAN_POINT('Ctrl Pts',(1.33517006539674,29.20091120588,52.7032503782176));
#133687=CARTESIAN_POINT('Ctrl Pts',(1.4463053362353,31.4962023798426,53.0829740555855));
#133688=CARTESIAN_POINT('Ctrl Pts',(1.55744060707386,32.4220634124452,55.2172998443405));
#133689=CARTESIAN_POINT('Ctrl Pts',(1.66857587791242,31.1310771539381,57.1527360629333));
#133690=CARTESIAN_POINT('Ctrl Pts',(1.77971114875098,28.8048482843264,57.1178341845877));
#133691=CARTESIAN_POINT('Ctrl Pts',(1.89084641958954,27.5725078874562,55.1445380473229));
#133692=CARTESIAN_POINT('Ctrl Pts',(2.0019816904281,28.5619827496753,53.0389504538599));
#133693=CARTESIAN_POINT('Ctrl Pts',(2.11311696126666,30.8676342339108,52.7282561914974));
#133694=CARTESIAN_POINT('Ctrl Pts',(2.22425223210522,32.3791645746092,54.4968250773821));
#133695=CARTESIAN_POINT('Ctrl Pts',(2.33538750294378,31.7131125888044,56.7259357762407));
#133696=CARTESIAN_POINT('Ctrl Pts',(2.44652277378234,29.4790969176509,57.3753460897111));
#133697=CARTESIAN_POINT('Ctrl Pts',(2.5576580446209,27.7218491597909,55.8506690380474));
#133698=CARTESIAN_POINT('Ctrl Pts',(2.66879331545945,28.0497286903431,53.5473985823599));
#133699=CARTESIAN_POINT('Ctrl Pts',(2.77992858629801,30.162636608847,52.5736532819753));
#133700=CARTESIAN_POINT('Ctrl Pts',(2.89106385713658,32.1266878213609,53.820674780915));
#133701=CARTESIAN_POINT('Ctrl Pts',(3.00219912797513,32.1442415813906,56.1470994299562));
#133702=CARTESIAN_POINT('Ctrl Pts',(3.1133343988137,30.1992314272445,57.4236162857034));
#133703=CARTESIAN_POINT('Ctrl Pts',(3.22446966965225,28.0718703602033,56.4818654304466));
#133704=CARTESIAN_POINT('Ctrl Pts',(3.33560494049081,27.7092720354094,54.1838048921801));
#133705=CARTESIAN_POINT('Ctrl Pts',(3.44674021132937,29.4433124847903,52.6327847431547));
#133706=CARTESIAN_POINT('Ctrl Pts',(3.55787548216793,31.6868733344789,53.2484100322169));
#133707=CARTESIAN_POINT('Ctrl Pts',(3.66901075300649,32.3864865418042,55.4672162749728));
#133708=CARTESIAN_POINT('Ctrl Pts',(3.78014602384505,30.90181584682,57.2583926231375));
#133709=CARTESIAN_POINT('Ctrl Pts',(3.89128129468361,28.5917385121774,56.9825258242279));
#133710=CARTESIAN_POINT('Ctrl Pts',(4.00241656552217,27.5706032453881,54.8921089878803));
#133711=CARTESIAN_POINT('Ctrl Pts',(4.11355183636073,28.7730263898749,52.9004417555418));
#133712=CARTESIAN_POINT('Ctrl Pts',(4.22468710719928,31.0984639147953,52.8304410379739));
#133713=CARTESIAN_POINT('Ctrl Pts',(4.33582237803785,32.4185083631876,54.7461765199851));
#133714=CARTESIAN_POINT('Ctrl Pts',(4.4469576488764,31.5249602382387,56.8942294828257));
#133715=CARTESIAN_POINT('Ctrl Pts',(4.55809291971497,29.2356589666865,57.3085475621284));
#133716=CARTESIAN_POINT('Ctrl Pts',(4.66922819055352,27.6459375107741,55.6099170916078));
#133717=CARTESIAN_POINT('Ctrl Pts',(4.78036346139209,28.2108231352622,53.3530466890339));
#133718=CARTESIAN_POINT('Ctrl Pts',(4.89149873223064,30.413291941376,52.6035862558796));
#133719=CARTESIAN_POINT('Ctrl Pts',(5.0026340030692,32.2374862763419,54.0474958136589));
#133720=CARTESIAN_POINT('Ctrl Pts',(5.11376927390777,32.0137724545067,56.3632056203247));
#133721=CARTESIAN_POINT('Ctrl Pts',(5.22490454474632,29.9469094347836,57.4312117253954));
#133722=CARTESIAN_POINT('Ctrl Pts',(5.33603981558489,27.9286387137954,56.2739982275609));
#133723=CARTESIAN_POINT('Ctrl Pts',(5.44717508642344,27.806226626021,53.9507300416783));
#133724=CARTESIAN_POINT('Ctrl Pts',(5.558310357262,29.6917135069452,52.5878290898));
#133725=CARTESIAN_POINT('Ctrl Pts',(5.66944562810056,31.8593663302637,53.4327202190748));
#133726=CARTESIAN_POINT('Ctrl Pts',(5.78058089893912,32.3251935314588,55.7120983801957));
#133727=CARTESIAN_POINT('Ctrl Pts',(5.89171616977768,30.6628365960341,57.3397129543542));
#133728=CARTESIAN_POINT('Ctrl Pts',(6.00285144061624,28.3938039969429,56.8258541731416));
#133729=CARTESIAN_POINT('Ctrl Pts',(6.1139867114548,27.5948773515111,54.6408425031529));
#133730=CARTESIAN_POINT('Ctrl Pts',(6.22512198229336,28.997291711844,52.7845575722491));
#133731=CARTESIAN_POINT('Ctrl Pts',(6.33625725313191,31.317456721161,52.9560046845253));
#133732=CARTESIAN_POINT('Ctrl Pts',(6.44739252397048,32.431790707502,54.9982631279294));
#133733=CARTESIAN_POINT('Ctrl Pts',(6.55852779480903,31.3203751649245,57.0421112814102));
#133734=CARTESIAN_POINT('Ctrl Pts',(6.66966306564759,29.0004574300117,57.2168725070682));
#133735=CARTESIAN_POINT('Ctrl Pts',(6.78079833648615,27.5953928514194,55.3625927782321));
#133736=CARTESIAN_POINT('Ctrl Pts',(6.89193360732472,28.3911974560599,53.1764420940374));
#133737=CARTESIAN_POINT('Ctrl Pts',(7.00306887816327,30.6594937077774,52.6593425899509));
#133738=CARTESIAN_POINT('Ctrl Pts',(7.11420414900184,32.3241739473258,54.2845808749405));
#133739=CARTESIAN_POINT('Ctrl Pts',(7.2253394198404,31.8616032467933,56.5646221310909));
#133740=CARTESIAN_POINT('Ctrl Pts',(7.33647469067895,29.6951595376434,57.4126088274738));
#133741=CARTESIAN_POINT('Ctrl Pts',(7.44760996151752,27.8077277156913,56.0524026292531));
#133742=CARTESIAN_POINT('Ctrl Pts',(7.55874523235607,27.9268209580955,53.7289619517855));
#133743=CARTESIAN_POINT('Ctrl Pts',(7.66988050319463,29.9434365728189,52.5688665931827));
#133744=CARTESIAN_POINT('Ctrl Pts',(7.78101577403319,32.0118231019326,53.6339191555266));
#133745=CARTESIAN_POINT('Ctrl Pts',(7.89215104487175,32.2388446148396,55.9493070294859));
#133746=CARTESIAN_POINT('Ctrl Pts',(8.00328631571031,30.4167147335142,57.3958209254241));
#133747=CARTESIAN_POINT('Ctrl Pts',(8.11442158654887,28.2131775729573,56.6495074142123));
#133748=CARTESIAN_POINT('Ctrl Pts',(8.22555685738743,27.6450686888643,54.3934462476575));
#133749=CARTESIAN_POINT('Ctrl Pts',(8.33669212822598,29.2323620034979,52.6925466180413));
#133750=CARTESIAN_POINT('Ctrl Pts',(8.44782739906455,31.5222529295465,53.1035941163948));
#133751=CARTESIAN_POINT('Ctrl Pts',(8.5589626699031,32.418868278926,55.2503683966076));
#133752=CARTESIAN_POINT('Ctrl Pts',(8.67009794074167,31.1015623350708,57.1679877347923));
#133753=CARTESIAN_POINT('Ctrl Pts',(8.78123321158022,28.7760260281981,57.1013085802318));
#133754=CARTESIAN_POINT('Ctrl Pts',(8.89236848241879,27.5707613729241,55.1113616575299));
#133755=CARTESIAN_POINT('Ctrl Pts',(9.00350375325735,28.5889049351466,53.0194870008748));
#133756=CARTESIAN_POINT('Ctrl Pts',(9.1146390240959,30.8985948931835,52.7403231650404));
#133757=CARTESIAN_POINT('Ctrl Pts',(9.22577429493447,32.3858047755745,54.5293718006317));
#133758=CARTESIAN_POINT('Ctrl Pts',(9.33690956577302,31.6893973577937,56.7491852222167));
#133759=CARTESIAN_POINT('Ctrl Pts',(9.44804483661158,29.4466476574818,57.3679947859353));
#133760=CARTESIAN_POINT('Ctrl Pts',(9.55918010745014,27.7105332689696,55.8194928217058));
#133761=CARTESIAN_POINT('Ctrl Pts',(9.67031537828869,28.0695711380181,53.5208381930937));
#133762=CARTESIAN_POINT('Ctrl Pts',(9.78145064912726,30.1961348712651,52.5762050172338));
#133763=CARTESIAN_POINT('Ctrl Pts',(9.89258591996582,32.1418745091302,53.8496338177819));
#133764=CARTESIAN_POINT('Ctrl Pts',(10.0037211908043,32.1298241188128,56.1766906279436));
#133765=CARTESIAN_POINT('Ctrl Pts',(10.1148693978264,30.1628285126107,57.4254746165565));
#133766=CARTESIAN_POINT('Ctrl Pts',(10.188972514569,28.7606699551445,56.7791900710538));
#133767=CARTESIAN_POINT('Ctrl Pts',(10.2260305410321,28.3512916699711,56.2307621872168));
#133768=CARTESIAN_POINT('Ctrl Pts',(-0.0743643367184447,30.4969362892315,
53.1392671053682));
#133769=CARTESIAN_POINT('Ctrl Pts',(-0.0373192464389249,31.1156596605629,
53.3045063490539));
#133770=CARTESIAN_POINT('Ctrl Pts',(0.0367709341201149,32.1645540715419,
54.2982659699198));
#133771=CARTESIAN_POINT('Ctrl Pts',(0.147906204958674,31.763339458138,56.4418124671141));
#133772=CARTESIAN_POINT('Ctrl Pts',(0.259041475797234,29.7450903047889,
57.2615565101349));
#133773=CARTESIAN_POINT('Ctrl Pts',(0.370176746635793,27.9616942279399,
56.0133736942143));
#133774=CARTESIAN_POINT('Ctrl Pts',(0.481312017474353,28.0431263937234,
53.8366706754401));
#133775=CARTESIAN_POINT('Ctrl Pts',(0.592447288312911,29.9160208513783,
52.7252379018771));
#133776=CARTESIAN_POINT('Ctrl Pts',(0.703582559151472,31.8655818797056,
53.6955748078898));
#133777=CARTESIAN_POINT('Ctrl Pts',(0.81471782999003,32.1077278073204,55.8599444392623));
#133778=CARTESIAN_POINT('Ctrl Pts',(0.92585310082859,30.4206797012092,57.2371660473154));
#133779=CARTESIAN_POINT('Ctrl Pts',(1.03698837166715,28.3486206059095,56.5668054276972));
#133780=CARTESIAN_POINT('Ctrl Pts',(1.14812364250571,27.7880097949288,54.4623753804963));
#133781=CARTESIAN_POINT('Ctrl Pts',(1.25925891334427,29.2519777371264,52.8500263525383));
#133782=CARTESIAN_POINT('Ctrl Pts',(1.37039418418283,31.4005861402667,53.2054834262723));
#133783=CARTESIAN_POINT('Ctrl Pts',(1.48152945502139,32.2672791408569,55.2034130906123));
#133784=CARTESIAN_POINT('Ctrl Pts',(1.59266472585995,31.058794590037,57.0151634123946));
#133785=CARTESIAN_POINT('Ctrl Pts',(1.70379999669851,28.8812255941844,56.9824919718604));
#133786=CARTESIAN_POINT('Ctrl Pts',(1.81493526753707,27.7276390853,55.135301205605));
#133787=CARTESIAN_POINT('Ctrl Pts',(1.92607053837562,28.6538806130752,53.1642731947873));
#133788=CARTESIAN_POINT('Ctrl Pts',(2.03720580921418,30.8121872409829,52.8734341454796));
#133789=CARTESIAN_POINT('Ctrl Pts',(2.14834108005275,32.227121794153,54.5289809505433));
#133790=CARTESIAN_POINT('Ctrl Pts',(2.2594763508913,31.6036344955207,56.6156382049381));
#133791=CARTESIAN_POINT('Ctrl Pts',(2.37061162172987,29.5123857257618,57.2235473331729));
#133792=CARTESIAN_POINT('Ctrl Pts',(2.48174689256842,27.867436561243,55.7963062221357));
#133793=CARTESIAN_POINT('Ctrl Pts',(2.59288216340698,28.1743626377921,53.6402284608768));
#133794=CARTESIAN_POINT('Ctrl Pts',(2.70401743424554,30.1522431612995,52.7287112822902));
#133795=CARTESIAN_POINT('Ctrl Pts',(2.8151527050841,31.9907798085346,53.8960406834195));
#133796=CARTESIAN_POINT('Ctrl Pts',(2.92628797592267,32.0072117787937,56.0737929472303));
#133797=CARTESIAN_POINT('Ctrl Pts',(3.03742324676122,30.1864993529374,57.2687327762693));
#133798=CARTESIAN_POINT('Ctrl Pts',(3.14855851759978,28.1950893231298,56.3871654072907));
#133799=CARTESIAN_POINT('Ctrl Pts',(3.25969378843834,27.8556631899861,54.2359646187127));
#133800=CARTESIAN_POINT('Ctrl Pts',(3.37082905927689,29.4788881312005,52.7840638910666));
#133801=CARTESIAN_POINT('Ctrl Pts',(3.48196433011546,31.5790720857596,53.360347059089));
#133802=CARTESIAN_POINT('Ctrl Pts',(3.59309960095402,32.2339758440535,55.4373583734727));
#133803=CARTESIAN_POINT('Ctrl Pts',(3.70423487179258,30.8441844453301,57.1140678893851));
#133804=CARTESIAN_POINT('Ctrl Pts',(3.81537014263114,28.6817348052052,56.8558306212735));
#133805=CARTESIAN_POINT('Ctrl Pts',(3.92650541346969,27.7258561611993,54.8990038658741));
#133806=CARTESIAN_POINT('Ctrl Pts',(4.03764068430826,28.8514373082371,53.0346160268907));
#133807=CARTESIAN_POINT('Ctrl Pts',(4.1487759551468,31.0282655310355,52.9690887719183));
#133808=CARTESIAN_POINT('Ctrl Pts',(4.25991122598538,32.2639512804115,54.7623973514728));
#133809=CARTESIAN_POINT('Ctrl Pts',(4.37104649682393,31.4275062003041,56.7731769417513));
#133810=CARTESIAN_POINT('Ctrl Pts',(4.4821817676625,29.2845049091495,57.1610176291815));
#133811=CARTESIAN_POINT('Ctrl Pts',(4.59331703850104,27.7963761185315,55.5709397583685));
#133812=CARTESIAN_POINT('Ctrl Pts',(4.70445230933962,28.3251621886198,53.4582968105905));
#133813=CARTESIAN_POINT('Ctrl Pts',(4.81558758017816,30.3868801258263,52.7567313609589));
#133814=CARTESIAN_POINT('Ctrl Pts',(4.92672285101673,32.0944975826136,54.1083665018127));
#133815=CARTESIAN_POINT('Ctrl Pts',(5.03785812185529,31.8850804058537,56.2760886654659));
#133816=CARTESIAN_POINT('Ctrl Pts',(5.14899339269384,29.9503022379707,57.275842822146));
#133817=CARTESIAN_POINT('Ctrl Pts',(5.2601286635324,28.061011031644,56.1925821561879));
#133818=CARTESIAN_POINT('Ctrl Pts',(5.37126393437097,27.9464218050474,54.0177846387478));
#133819=CARTESIAN_POINT('Ctrl Pts',(5.48239920520953,29.7114148492069,52.7419811716006));
#133820=CARTESIAN_POINT('Ctrl Pts',(5.59353447604809,31.7405417521925,53.5328787277328));
#133821=CARTESIAN_POINT('Ctrl Pts',(5.70466974688665,32.1765998219716,55.6665910542886));
#133822=CARTESIAN_POINT('Ctrl Pts',(5.81580501772522,30.6204773914105,57.190191367304));
#133823=CARTESIAN_POINT('Ctrl Pts',(5.92694028856376,28.4964494838793,56.7091712214221));
#133824=CARTESIAN_POINT('Ctrl Pts',(6.03807555940233,27.7485790074273,54.6637948054127));
#133825=CARTESIAN_POINT('Ctrl Pts',(6.14921083024089,29.0613707409894,52.9261375328163));
#133826=CARTESIAN_POINT('Ctrl Pts',(6.26034610107943,31.2332633933208,53.0866281539233));
#133827=CARTESIAN_POINT('Ctrl Pts',(6.37148137191802,32.276384803849,54.9983741243951));
#133828=CARTESIAN_POINT('Ctrl Pts',(6.48261664275655,31.235995331153,56.9116082130054));
#133829=CARTESIAN_POINT('Ctrl Pts',(6.59375191359513,29.0643341509192,57.0752011559189));
#133830=CARTESIAN_POINT('Ctrl Pts',(6.70488718443368,27.7490615638223,55.3394209410401));
#133831=CARTESIAN_POINT('Ctrl Pts',(6.81602245527225,28.4940095164765,53.2929783006137));
#133832=CARTESIAN_POINT('Ctrl Pts',(6.9271577261108,30.6173481336149,52.8089245333429));
#133833=CARTESIAN_POINT('Ctrl Pts',(7.03829299694936,32.1756453953347,54.3303004162143));
#133834=CARTESIAN_POINT('Ctrl Pts',(7.14942826778791,31.7426357164384,56.4646334620794));
#133835=CARTESIAN_POINT('Ctrl Pts',(7.26056353862649,29.7146406580278,57.2584287601524));
#133836=CARTESIAN_POINT('Ctrl Pts',(7.37169880946503,27.9478269661512,55.985147835861));
#133837=CARTESIAN_POINT('Ctrl Pts',(7.48283408030359,28.0593094413551,53.8101888500751));
#133838=CARTESIAN_POINT('Ctrl Pts',(7.59396935114215,29.947051312561,52.7242304914087));
#133839=CARTESIAN_POINT('Ctrl Pts',(7.70510462198073,31.8832556285142,53.7212198543257));
#133840=CARTESIAN_POINT('Ctrl Pts',(7.81623989281927,32.0957691151947,55.8886406586893));
#133841=CARTESIAN_POINT('Ctrl Pts',(7.92737516365785,30.3900841811695,57.2427137049886));
#133842=CARTESIAN_POINT('Ctrl Pts',(8.03851043449638,28.3273661637292,56.5440940702528));
#133843=CARTESIAN_POINT('Ctrl Pts',(8.14964570533495,27.7955628195141,54.4322086434944));
#133844=CARTESIAN_POINT('Ctrl Pts',(8.26078097617351,29.2814186415371,52.8400066263611));
#133845=CARTESIAN_POINT('Ctrl Pts',(8.37191624701208,31.424971904755,53.2247857424361));
#133846=CARTESIAN_POINT('Ctrl Pts',(8.48305151785062,32.2642881953915,55.2343683655191));
#133847=CARTESIAN_POINT('Ctrl Pts',(8.59418678868919,31.0311659438091,57.0294404116223));
#133848=CARTESIAN_POINT('Ctrl Pts',(8.70532205952775,28.8542452518133,56.9670224520066));
#133849=CARTESIAN_POINT('Ctrl Pts',(8.8164573303663,27.7260041834442,55.1042449846322));
#133850=CARTESIAN_POINT('Ctrl Pts',(8.92759260120488,28.6790823106162,53.146053572322));
#133851=CARTESIAN_POINT('Ctrl Pts',(9.03872787204343,30.8411693298065,52.8847299675736));
#133852=CARTESIAN_POINT('Ctrl Pts',(9.149863142882,32.2333376467449,54.5594477444133));
#133853=CARTESIAN_POINT('Ctrl Pts',(9.26099841372054,31.5814348089579,56.6374018729028));
#133854=CARTESIAN_POINT('Ctrl Pts',(9.3721336845591,29.4820101665014,57.2166658214737));
#133855=CARTESIAN_POINT('Ctrl Pts',(9.48326895539768,27.8568438232133,55.7671223516233));
#133856=CARTESIAN_POINT('Ctrl Pts',(9.59440422623621,28.1929370349304,53.6153654386096));
#133857=CARTESIAN_POINT('Ctrl Pts',(9.7055394970748,30.1836006853202,52.7310999464744));
#133858=CARTESIAN_POINT('Ctrl Pts',(9.81667476791335,32.0049959765427,53.9231490654255));
#133859=CARTESIAN_POINT('Ctrl Pts',(9.92781003875191,31.9937156779076,56.1014930914981));
#133860=CARTESIAN_POINT('Ctrl Pts',(10.038958245774,30.1524228012702,57.2704723487172));
#133861=CARTESIAN_POINT('Ctrl Pts',(10.1130613625166,28.8398705232488,56.6654892332682));
#133862=CARTESIAN_POINT('Ctrl Pts',(10.1501193889796,28.4566539476942,56.1521091562236));
#133863=CARTESIAN_POINT('Ctrl Pts',(-0.15027548877092,30.4630110789791,
53.2662969803077));
#133864=CARTESIAN_POINT('Ctrl Pts',(-0.1132303984914,31.0394949904132,53.4202555503831));
#133865=CARTESIAN_POINT('Ctrl Pts',(-0.0391402179323597,32.0167827101601,
54.346172462216));
#133866=CARTESIAN_POINT('Ctrl Pts',(0.0719950529061993,31.6429585095939,
56.3433817584873));
#133867=CARTESIAN_POINT('Ctrl Pts',(0.183130323744759,29.7624926664051,
57.1071629152887));
#133868=CARTESIAN_POINT('Ctrl Pts',(0.294265594583318,28.1008467780239,
55.9441919572683));
#133869=CARTESIAN_POINT('Ctrl Pts',(0.405400865421878,28.1767196731213,
53.9160896930964));
#133870=CARTESIAN_POINT('Ctrl Pts',(0.516536136260436,29.9217540013526,
52.8805330254681));
#133871=CARTESIAN_POINT('Ctrl Pts',(0.627671407098997,31.7382209707045,
53.7846262614862));
#133872=CARTESIAN_POINT('Ctrl Pts',(0.738806677937555,31.9638359029301,
55.8012371229733));
#133873=CARTESIAN_POINT('Ctrl Pts',(0.849941948776116,30.3919604315126,
57.084437558434));
#133874=CARTESIAN_POINT('Ctrl Pts',(0.961077219614675,28.4613581828686,
56.4598416081671));
#133875=CARTESIAN_POINT('Ctrl Pts',(1.07221249045323,27.9390195609882,54.4990783314556));
#133876=CARTESIAN_POINT('Ctrl Pts',(1.1833477612918,29.3030442683727,52.996802326859));
#133877=CARTESIAN_POINT('Ctrl Pts',(1.29448303213035,31.3049699006907,53.3279927969591));
#133878=CARTESIAN_POINT('Ctrl Pts',(1.40561830296891,32.1124948692687,55.1895263368842));
#133879=CARTESIAN_POINT('Ctrl Pts',(1.51675357380747,30.986512026136,56.877590761856));
#133880=CARTESIAN_POINT('Ctrl Pts',(1.62788884464603,28.9576029040423,56.8471497591331));
#133881=CARTESIAN_POINT('Ctrl Pts',(1.73902411548459,27.8827702831439,55.126064363887));
#133882=CARTESIAN_POINT('Ctrl Pts',(1.85015938632315,28.7457784764752,53.2895959357148));
#133883=CARTESIAN_POINT('Ctrl Pts',(1.96129465716171,30.7567402480549,53.0186120994619));
#133884=CARTESIAN_POINT('Ctrl Pts',(2.07242992800027,32.0750790136968,54.5611368237044));
#133885=CARTESIAN_POINT('Ctrl Pts',(2.18356519883883,31.4941564022369,56.5053406336356));
#133886=CARTESIAN_POINT('Ctrl Pts',(2.29470046967739,29.5456745338728,57.0717485766346));
#133887=CARTESIAN_POINT('Ctrl Pts',(2.40583574051595,28.013023962695,55.7419434062243));
#133888=CARTESIAN_POINT('Ctrl Pts',(2.5169710113545,28.298996585241,53.7330583393936));
#133889=CARTESIAN_POINT('Ctrl Pts',(2.62810628219307,30.1418497137519,52.8837692826054));
#133890=CARTESIAN_POINT('Ctrl Pts',(2.73924155303162,31.8548717957082,53.9714065859237));
#133891=CARTESIAN_POINT('Ctrl Pts',(2.85037682387019,31.8701819761967,56.0004864645048));
#133892=CARTESIAN_POINT('Ctrl Pts',(2.96151209470874,30.1737672786304,57.1138492668348));
#133893=CARTESIAN_POINT('Ctrl Pts',(3.07264736554731,28.3183082860562,56.2924653841349));
#133894=CARTESIAN_POINT('Ctrl Pts',(3.18378263638586,28.0020543445629,54.2881243452452));
#133895=CARTESIAN_POINT('Ctrl Pts',(3.29491790722442,29.5144637776106,52.9353430389786));
#133896=CARTESIAN_POINT('Ctrl Pts',(3.40605317806298,31.4712708370402,53.472284085961));
#133897=CARTESIAN_POINT('Ctrl Pts',(3.51718844890155,32.0814651463029,55.4075004719725));
#133898=CARTESIAN_POINT('Ctrl Pts',(3.6283237197401,30.7865530438401,56.9697431556326));
#133899=CARTESIAN_POINT('Ctrl Pts',(3.73945899057866,28.771731098233,56.7291354183192));
#133900=CARTESIAN_POINT('Ctrl Pts',(3.85059426141722,27.8811090770103,54.9058987438678));
#133901=CARTESIAN_POINT('Ctrl Pts',(3.96172953225578,28.9298482265992,53.1687902982395));
#133902=CARTESIAN_POINT('Ctrl Pts',(4.07286480309434,30.9580671472756,53.1077365058626));
#133903=CARTESIAN_POINT('Ctrl Pts',(4.1840000739329,32.1093941976355,54.7786181829607));
#133904=CARTESIAN_POINT('Ctrl Pts',(4.29513534477146,31.3300521623692,56.6521244006766));
#133905=CARTESIAN_POINT('Ctrl Pts',(4.40627061561002,29.3333508516128,57.0134876962348));
#133906=CARTESIAN_POINT('Ctrl Pts',(4.51740588644858,27.9468147262887,55.5319624251291));
#133907=CARTESIAN_POINT('Ctrl Pts',(4.62854115728713,28.4395012419773,53.5635469321471));
#133908=CARTESIAN_POINT('Ctrl Pts',(4.7396764281257,30.3604683102766,52.9098764660384));
#133909=CARTESIAN_POINT('Ctrl Pts',(4.85081169896425,31.9515088888855,54.1692371899665));
#133910=CARTESIAN_POINT('Ctrl Pts',(4.96194696980282,31.7563883572006,56.1889717106072));
#133911=CARTESIAN_POINT('Ctrl Pts',(5.07308224064137,29.9536950411579,57.1204739188966));
#133912=CARTESIAN_POINT('Ctrl Pts',(5.18421751147994,28.1933833494923,56.1111660848148));
#133913=CARTESIAN_POINT('Ctrl Pts',(5.29535278231849,28.0866169840739,54.0848392358172));
#133914=CARTESIAN_POINT('Ctrl Pts',(5.40648805315706,29.7311161914685,52.8961332534013));
#133915=CARTESIAN_POINT('Ctrl Pts',(5.51762332399561,31.6217171741212,53.6330372363906));
#133916=CARTESIAN_POINT('Ctrl Pts',(5.62875859483417,32.0280061124844,55.6210837283815));
#133917=CARTESIAN_POINT('Ctrl Pts',(5.73989386567274,30.5781181867869,57.0406697802536));
#133918=CARTESIAN_POINT('Ctrl Pts',(5.85102913651129,28.5990949708156,56.5924882697025));
#133919=CARTESIAN_POINT('Ctrl Pts',(5.96216440734985,27.9022806633435,54.6867471076725));
#133920=CARTESIAN_POINT('Ctrl Pts',(6.07329967818841,29.1254497701346,53.0677174933834));
#133921=CARTESIAN_POINT('Ctrl Pts',(6.18443494902697,31.1490700654805,53.2172516233213));
#133922=CARTESIAN_POINT('Ctrl Pts',(6.29557021986553,32.120978900196,54.9984851208607));
#133923=CARTESIAN_POINT('Ctrl Pts',(6.40670549070409,31.1516154973816,56.7811051446004));
#133924=CARTESIAN_POINT('Ctrl Pts',(6.51784076154265,29.1282108718268,56.9335298047696));
#133925=CARTESIAN_POINT('Ctrl Pts',(6.6289760323812,27.9027302762255,55.316249103848));
#133926=CARTESIAN_POINT('Ctrl Pts',(6.74011130321977,28.5968215768931,53.4095145071899));
#133927=CARTESIAN_POINT('Ctrl Pts',(6.85124657405832,30.5752025594525,52.9585064767349));
#133928=CARTESIAN_POINT('Ctrl Pts',(6.96238184489689,32.0271168433436,54.3760199574878));
#133929=CARTESIAN_POINT('Ctrl Pts',(7.07351711573544,31.6236681860837,56.3646447930679));
#133930=CARTESIAN_POINT('Ctrl Pts',(7.18465238657401,29.7341217784122,57.1042486928307));
#133931=CARTESIAN_POINT('Ctrl Pts',(7.29578765741256,28.0879262166111,55.9178930424689));
#133932=CARTESIAN_POINT('Ctrl Pts',(7.40692292825113,28.1917979246146,53.8914157483648));
#133933=CARTESIAN_POINT('Ctrl Pts',(7.51805819908967,29.9506660523031,52.8795943896346));
#133934=CARTESIAN_POINT('Ctrl Pts',(7.62919346992825,31.7546881550959,53.808520553125));
#133935=CARTESIAN_POINT('Ctrl Pts',(7.74032874076679,31.9526936155498,55.8279742878926));
#133936=CARTESIAN_POINT('Ctrl Pts',(7.85146401160537,30.3634536288249,57.0896064845533));
#133937=CARTESIAN_POINT('Ctrl Pts',(7.96259928244391,28.4415547545012,56.4386807262929));
#133938=CARTESIAN_POINT('Ctrl Pts',(8.07373455328248,27.9460569501639,54.4709710393315));
#133939=CARTESIAN_POINT('Ctrl Pts',(8.18486982412104,29.3304752795761,52.9874666346809));
#133940=CARTESIAN_POINT('Ctrl Pts',(8.29600509495959,31.3276908799634,53.3459773684774));
#133941=CARTESIAN_POINT('Ctrl Pts',(8.40714036579816,32.1097081118571,55.2183683344306));
#133942=CARTESIAN_POINT('Ctrl Pts',(8.51827563663671,30.9607695525475,56.8908930884524));
#133943=CARTESIAN_POINT('Ctrl Pts',(8.62941090747528,28.9324644754286,56.8327363237813));
#133944=CARTESIAN_POINT('Ctrl Pts',(8.74054617831384,27.8812469939644,55.0971283117347));
#133945=CARTESIAN_POINT('Ctrl Pts',(8.8516814491524,28.7692596860857,53.272620143769));
#133946=CARTESIAN_POINT('Ctrl Pts',(8.96281671999095,30.7837437664296,53.0291367701069));
#133947=CARTESIAN_POINT('Ctrl Pts',(9.07395199082952,32.0808705179151,54.5895236881948));
#133948=CARTESIAN_POINT('Ctrl Pts',(9.18508726166807,31.4734722601222,56.525618523589));
#133949=CARTESIAN_POINT('Ctrl Pts',(9.29622253250664,29.5173726755208,57.0653368570119));
#133950=CARTESIAN_POINT('Ctrl Pts',(9.40735780334519,28.0031543774569,55.7147518815408));
#133951=CARTESIAN_POINT('Ctrl Pts',(9.51849307418375,28.3163029318427,53.7098926841253));
#133952=CARTESIAN_POINT('Ctrl Pts',(9.62962834502232,30.1710664993754,52.8859948757149));
#133953=CARTESIAN_POINT('Ctrl Pts',(9.74076361586087,31.8681174439553,53.996664313069));
#133954=CARTESIAN_POINT('Ctrl Pts',(9.85189888669943,31.8576072370023,56.0262955550524));
#133955=CARTESIAN_POINT('Ctrl Pts',(9.9630470937215,30.1420170899297,57.1154700808779));
#133956=CARTESIAN_POINT('Ctrl Pts',(10.0371502104641,28.9190710913532,56.5517883954824));
#133957=CARTESIAN_POINT('Ctrl Pts',(10.0742082369271,28.5620162254173,56.0734561252304));
#133958=CARTESIAN_POINT('Ctrl Pts',(-0.226186640823395,30.4290858687267,
53.393326855247));
#133959=CARTESIAN_POINT('Ctrl Pts',(-0.189141550543875,30.9633303202635,
53.536004751712));
#133960=CARTESIAN_POINT('Ctrl Pts',(-0.115051369984835,31.8690113487782,
54.3940789545122));
#133961=CARTESIAN_POINT('Ctrl Pts',(-0.00391609914627541,31.5225775610498,
56.2449510498606));
#133962=CARTESIAN_POINT('Ctrl Pts',(0.107219171692284,29.7798950280212,
56.9527693204424));
#133963=CARTESIAN_POINT('Ctrl Pts',(0.218354442530843,28.2399993281078,
55.8750102203225));
#133964=CARTESIAN_POINT('Ctrl Pts',(0.329489713369402,28.3103129525194,
53.9955087107525));
#133965=CARTESIAN_POINT('Ctrl Pts',(0.440624984207962,29.9274871513269,
53.035828149059));
#133966=CARTESIAN_POINT('Ctrl Pts',(0.551760255046521,31.6108600617036,
53.8736777150826));
#133967=CARTESIAN_POINT('Ctrl Pts',(0.662895525885082,31.8199439985398,
55.7425298066844));
#133968=CARTESIAN_POINT('Ctrl Pts',(0.774030796723639,30.363241161816,56.9317090695523));
#133969=CARTESIAN_POINT('Ctrl Pts',(0.885166067562201,28.5740957598277,
56.3528777886373));
#133970=CARTESIAN_POINT('Ctrl Pts',(0.996301338400759,28.0900293270476,
54.5357812824147));
#133971=CARTESIAN_POINT('Ctrl Pts',(1.10743660923932,29.3541107996191,53.1435783011798));
#133972=CARTESIAN_POINT('Ctrl Pts',(1.21857188007787,31.2093536611147,53.4505021676458));
#133973=CARTESIAN_POINT('Ctrl Pts',(1.32970715091643,31.9577105976804,55.1756395831562));
#133974=CARTESIAN_POINT('Ctrl Pts',(1.440842421755,30.9142294622349,56.7400181113173));
#133975=CARTESIAN_POINT('Ctrl Pts',(1.55197769259355,29.0339802139003,56.7118075464059));
#133976=CARTESIAN_POINT('Ctrl Pts',(1.66311296343211,28.0379014809877,55.1168275221689));
#133977=CARTESIAN_POINT('Ctrl Pts',(1.77424823427067,28.837676339875,53.4149186766423));
#133978=CARTESIAN_POINT('Ctrl Pts',(1.88538350510923,30.701293255127,53.1637900534441));
#133979=CARTESIAN_POINT('Ctrl Pts',(1.99651877594779,31.9230362332406,54.5932926968657));
#133980=CARTESIAN_POINT('Ctrl Pts',(2.10765404678635,31.3846783089532,56.3950430623329));
#133981=CARTESIAN_POINT('Ctrl Pts',(2.21878931762491,29.5789633419837,56.9199498200965));
#133982=CARTESIAN_POINT('Ctrl Pts',(2.32992458846347,28.158611364147,55.6875805903127));
#133983=CARTESIAN_POINT('Ctrl Pts',(2.44105985930203,28.42363053269,53.8258882179105));
#133984=CARTESIAN_POINT('Ctrl Pts',(2.55219513014059,30.1314562662045,53.0388272829205));
#133985=CARTESIAN_POINT('Ctrl Pts',(2.66333040097915,31.7189637828817,54.046772488428));
#133986=CARTESIAN_POINT('Ctrl Pts',(2.77446567181771,31.7331521735996,55.927179981779));
#133987=CARTESIAN_POINT('Ctrl Pts',(2.88560094265627,30.1610352043235,56.9589657574004));
#133988=CARTESIAN_POINT('Ctrl Pts',(2.99673621349482,28.4415272489827,56.1977653609792));
#133989=CARTESIAN_POINT('Ctrl Pts',(3.10787148433339,28.1484454991397,54.3402840717779));
#133990=CARTESIAN_POINT('Ctrl Pts',(3.21900675517194,29.5500394240206,53.0866221868906));
#133991=CARTESIAN_POINT('Ctrl Pts',(3.33014202601051,31.3634695883209,53.584221112833));
#133992=CARTESIAN_POINT('Ctrl Pts',(3.44127729684907,31.9289544485523,55.3776425704724));
#133993=CARTESIAN_POINT('Ctrl Pts',(3.55241256768762,30.7289216423502,56.8254184218802));
#133994=CARTESIAN_POINT('Ctrl Pts',(3.66354783852618,28.8617273912608,56.6024402153649));
#133995=CARTESIAN_POINT('Ctrl Pts',(3.77468310936474,28.0363619928214,54.9127936218614));
#133996=CARTESIAN_POINT('Ctrl Pts',(3.88581838020331,29.0082591449614,53.3029645695884));
#133997=CARTESIAN_POINT('Ctrl Pts',(3.99695365104185,30.8878687635158,53.2463842398069));
#133998=CARTESIAN_POINT('Ctrl Pts',(4.10808892188042,31.9548371148595,54.7948390144485));
#133999=CARTESIAN_POINT('Ctrl Pts',(4.21922419271897,31.2325981244345,56.5310718596021));
#134000=CARTESIAN_POINT('Ctrl Pts',(4.33035946355754,29.382196794076,56.865957763288));
#134001=CARTESIAN_POINT('Ctrl Pts',(4.4414947343961,28.0972533340459,55.4929850918898));
#134002=CARTESIAN_POINT('Ctrl Pts',(4.55263000523466,28.553840295335,53.6687970537037));
#134003=CARTESIAN_POINT('Ctrl Pts',(4.66376527607322,30.334056494727,53.0630215711176));
#134004=CARTESIAN_POINT('Ctrl Pts',(4.77490054691178,31.8085201951574,54.2301078781202));
#134005=CARTESIAN_POINT('Ctrl Pts',(4.88603581775034,31.6276963085475,56.1018547557485));
#134006=CARTESIAN_POINT('Ctrl Pts',(4.99717108858889,29.957087844345,56.9651050156472));
#134007=CARTESIAN_POINT('Ctrl Pts',(5.10830635942746,28.3257556673408,56.0297500134417));
#134008=CARTESIAN_POINT('Ctrl Pts',(5.21944163026601,28.2268121631002,54.1518938328867));
#134009=CARTESIAN_POINT('Ctrl Pts',(5.33057690110458,29.7508175337302,53.050285335202));
#134010=CARTESIAN_POINT('Ctrl Pts',(5.44171217194313,31.50289259605,53.7331957450487));
#134011=CARTESIAN_POINT('Ctrl Pts',(5.55284744278169,31.8794124029971,55.5755764024744));
#134012=CARTESIAN_POINT('Ctrl Pts',(5.66398271362025,30.5357589821632,56.8911481932033));
#134013=CARTESIAN_POINT('Ctrl Pts',(5.77511798445881,28.701740457752,56.475805317983));
#134014=CARTESIAN_POINT('Ctrl Pts',(5.88625325529737,28.0559823192596,54.7096994099324));
#134015=CARTESIAN_POINT('Ctrl Pts',(5.99738852613593,29.1895287992798,53.2092974539506));
#134016=CARTESIAN_POINT('Ctrl Pts',(6.10852379697449,31.0648767376402,53.3478750927192));
#134017=CARTESIAN_POINT('Ctrl Pts',(6.21965906781306,31.9655729965431,54.9985961173263));
#134018=CARTESIAN_POINT('Ctrl Pts',(6.3307943386516,31.0672356636102,56.6506020761956));
#134019=CARTESIAN_POINT('Ctrl Pts',(6.44192960949018,29.1920875927343,56.7918584536201));
#134020=CARTESIAN_POINT('Ctrl Pts',(6.55306488032872,28.0563989886284,55.2930772666561));
#134021=CARTESIAN_POINT('Ctrl Pts',(6.66420015116729,28.6996336373097,53.5260507137662));
#134022=CARTESIAN_POINT('Ctrl Pts',(6.77533542200584,30.53305698529,53.1080884201267));
#134023=CARTESIAN_POINT('Ctrl Pts',(6.88647069284441,31.8785882913524,54.4217394987615));
#134024=CARTESIAN_POINT('Ctrl Pts',(6.99760596368297,31.5047006557289,56.2646561240565));
#134025=CARTESIAN_POINT('Ctrl Pts',(7.10874123452152,29.7536028987965,56.9500686255091));
#134026=CARTESIAN_POINT('Ctrl Pts',(7.21987650536009,28.228025467071,55.8506382490768));
#134027=CARTESIAN_POINT('Ctrl Pts',(7.33101177619865,28.3242864078741,53.9726426466545));
#134028=CARTESIAN_POINT('Ctrl Pts',(7.4421470470372,29.9542807920451,53.0349582878607));
#134029=CARTESIAN_POINT('Ctrl Pts',(7.55328231787577,31.6261206816776,53.8958212519243));
#134030=CARTESIAN_POINT('Ctrl Pts',(7.66441758871431,31.8096181159048,55.7673079170957));
#134031=CARTESIAN_POINT('Ctrl Pts',(7.77555285955289,30.3368230764804,56.9364992641179));
#134032=CARTESIAN_POINT('Ctrl Pts',(7.88668813039144,28.555743345273,56.3332673823333));
#134033=CARTESIAN_POINT('Ctrl Pts',(7.99782340123,28.0965510808136,54.5097334351684));
#134034=CARTESIAN_POINT('Ctrl Pts',(8.10895867206856,29.3795319176152,53.1349266430008));
#134035=CARTESIAN_POINT('Ctrl Pts',(8.22009394290712,31.2304098551717,53.4671689945188));
#134036=CARTESIAN_POINT('Ctrl Pts',(8.33122921374569,31.9551280283227,55.2023683033418));
#134037=CARTESIAN_POINT('Ctrl Pts',(8.44236448458424,30.8903731612859,56.7523457652825));
#134038=CARTESIAN_POINT('Ctrl Pts',(8.5534997554228,29.0106836990437,56.698450195556));
#134039=CARTESIAN_POINT('Ctrl Pts',(8.66463502626136,28.0364898044845,55.0900116388371));
#134040=CARTESIAN_POINT('Ctrl Pts',(8.77577029709992,28.8594370615552,53.3991867152161));
#134041=CARTESIAN_POINT('Ctrl Pts',(8.88690556793847,30.7263182030527,53.1735435726402));
#134042=CARTESIAN_POINT('Ctrl Pts',(8.99804083877704,31.9284033890853,54.6195996319764));
#134043=CARTESIAN_POINT('Ctrl Pts',(9.10917610961559,31.3655097112866,56.4138351742751));
#134044=CARTESIAN_POINT('Ctrl Pts',(9.22031138045416,29.5527351845403,56.9140078925503));
#134045=CARTESIAN_POINT('Ctrl Pts',(9.33144665129271,28.1494649317004,55.6623814114582));
#134046=CARTESIAN_POINT('Ctrl Pts',(9.44258192213128,28.4396688287551,53.8044199296412));
#134047=CARTESIAN_POINT('Ctrl Pts',(9.55371719296983,30.1585323134304,53.0408898049554));
#134048=CARTESIAN_POINT('Ctrl Pts',(9.66485246380839,31.7312389113679,54.0701795607126));
#134049=CARTESIAN_POINT('Ctrl Pts',(9.77598773464695,31.7214987960971,55.9510980186068));
#134050=CARTESIAN_POINT('Ctrl Pts',(9.88713594166903,30.1316113785892,56.9604678130387));
#134051=CARTESIAN_POINT('Ctrl Pts',(9.96123905841159,28.9982716594575,56.4380875576967));
#134052=CARTESIAN_POINT('Ctrl Pts',(9.99829708487463,28.6673785031403,55.994803094237));
#134053=CARTESIAN_POINT('Ctrl Pts',(10.,28.6653082844465,55.9970727277551));
#134054=CARTESIAN_POINT('Ctrl Pts',(10.,28.6967090787531,56.0511234594078));
#134055=CARTESIAN_POINT('Ctrl Pts',(10.,28.7313028149014,56.1030990886654));
#134056=CARTESIAN_POINT('Ctrl Pts',(10.,28.7687632599603,56.1529135186339));
#134057=CARTESIAN_POINT('Ctrl Pts',(10.,28.7925234449976,56.1845095146696));
#134058=CARTESIAN_POINT('Ctrl Pts',(10.,28.8174380027366,56.2152358570303));
#134059=CARTESIAN_POINT('Ctrl Pts',(10.,28.8434336726689,56.2450673747019));
#134060=CARTESIAN_POINT('Ctrl Pts',(10.,28.8612018283552,56.2654573493296));
#134061=CARTESIAN_POINT('Ctrl Pts',(10.,28.879475213815,56.2854292268814));
#134062=CARTESIAN_POINT('Ctrl Pts',(10.,28.8982322592198,56.3049740723664));
#134063=CARTESIAN_POINT('Ctrl Pts',(10.,28.9081731573242,56.3153324904029));
#134064=CARTESIAN_POINT('Ctrl Pts',(10.,28.9182498619851,56.3255707073213));
#134065=CARTESIAN_POINT('Ctrl Pts',(10.,28.9284489135861,56.3356775141706));
#134066=CARTESIAN_POINT('Ctrl Pts',(10.,28.9753089563359,56.3821137338849));
#134067=CARTESIAN_POINT('Ctrl Pts',(10.,29.0247995791763,56.4258325114299));
#134068=CARTESIAN_POINT('Ctrl Pts',(10.,29.0765854237513,56.4667238945408));
#134069=CARTESIAN_POINT('Ctrl Pts',(10.,29.1139361671967,56.4962169649394));
#134070=CARTESIAN_POINT('Ctrl Pts',(9.99999999999999,29.1524820705888,56.5242388499532));
#134071=CARTESIAN_POINT('Ctrl Pts',(10.,29.1921115967059,56.5507396091909));
#134072=CARTESIAN_POINT('Ctrl Pts',(10.,29.2029855373481,56.5580111491551));
#134073=CARTESIAN_POINT('Ctrl Pts',(10.,29.2139411245786,56.5651681145049));
#134074=CARTESIAN_POINT('Ctrl Pts',(10.,29.2249761856231,56.5722093560925));
#134075=CARTESIAN_POINT('Ctrl Pts',(9.99999999999999,29.2362247392384,56.5793868228231));
#134076=CARTESIAN_POINT('Ctrl Pts',(9.99999999999999,29.2475490172341,56.5864396275743));
#134077=CARTESIAN_POINT('Ctrl Pts',(10.,29.2589420457756,56.5933643753857));
#134078=CARTESIAN_POINT('Ctrl Pts',(10.,29.3169247868431,56.6286066165372));
#134079=CARTESIAN_POINT('Ctrl Pts',(10.,29.3767191373825,56.6605562853147));
#134080=CARTESIAN_POINT('Ctrl Pts',(10.,29.4379848073917,56.6891026354925));
#134081=CARTESIAN_POINT('Ctrl Pts',(10.,29.5001359672636,56.718061574053));
#134082=CARTESIAN_POINT('Ctrl Pts',(10.,29.5638020498636,56.7435188436963));
#134083=CARTESIAN_POINT('Ctrl Pts',(10.,29.6286681086957,56.7653246387053));
#134084=CARTESIAN_POINT('Ctrl Pts',(10.,29.6688530659824,56.778833474556));
#134085=CARTESIAN_POINT('Ctrl Pts',(9.99999999999999,29.709499312355,56.7909402012805));
#134086=CARTESIAN_POINT('Ctrl Pts',(9.99999999999999,29.7505375207727,56.8016008389451));
#134087=CARTESIAN_POINT('Ctrl Pts',(9.99999999999999,29.784151885417,56.8103329589771));
#134088=CARTESIAN_POINT('Ctrl Pts',(10.,29.8180293214886,56.8180947591621));
#134089=CARTESIAN_POINT('Ctrl Pts',(10.,29.8521331499728,56.8248583287514));
#134090=CARTESIAN_POINT('Ctrl Pts',(10.,29.8660806800435,56.827624443127));
#134091=CARTESIAN_POINT('Ctrl Pts',(9.99999999999999,29.8800686440204,56.8302238613979));
#134092=CARTESIAN_POINT('Ctrl Pts',(9.99999999999999,29.8940706859101,56.8326507611155));
#134093=CARTESIAN_POINT('Ctrl Pts',(9.99999999999999,29.9635198353059,56.8446880141378));
#134094=CARTESIAN_POINT('Ctrl Pts',(10.,30.0334344025252,56.8525103460855));
#134095=CARTESIAN_POINT('Ctrl Pts',(10.,30.1034795484966,56.8559771790632));
#134096=CARTESIAN_POINT('Ctrl Pts',(10.,30.1112528776822,56.8563619142735));
#134097=CARTESIAN_POINT('Ctrl Pts',(9.99999999999999,30.1190278448756,56.8566929649851));
#134098=CARTESIAN_POINT('Ctrl Pts',(9.99999999999999,30.1268040132865,56.8569701053381));
#134099=CARTESIAN_POINT('Ctrl Pts',(9.99999999999999,30.1941857015925,56.8593715688738));
#134100=CARTESIAN_POINT('Ctrl Pts',(10.,30.2616564470238,56.8577294314614));
#134101=CARTESIAN_POINT('Ctrl Pts',(10.,30.3289537333749,56.8522616236189));
#134102=CARTESIAN_POINT('Ctrl Pts',(10.,30.401352855462,56.8463792989518));
#134103=CARTESIAN_POINT('Ctrl Pts',(9.99999999999998,30.473552131762,56.8360696937098));
#134104=CARTESIAN_POINT('Ctrl Pts',(9.99999999999997,30.5452332909405,56.8215404883134));
#134105=CARTESIAN_POINT('Ctrl Pts',(9.99999999999997,30.5582509814866,56.8189019051501));
#134106=CARTESIAN_POINT('Ctrl Pts',(9.99999999999999,30.5712515824525,56.8161239898941));
#134107=CARTESIAN_POINT('Ctrl Pts',(9.99999999999999,30.5842331746687,56.8132077668621));
#134108=CARTESIAN_POINT('Ctrl Pts',(9.99999999999998,30.59558256849,56.8106582056751));
#134109=CARTESIAN_POINT('Ctrl Pts',(9.99999999999997,30.6069085600895,56.8080049084806));
#134110=CARTESIAN_POINT('Ctrl Pts',(9.99999999999998,30.6182077920376,56.8052495748911));
#134111=CARTESIAN_POINT('Ctrl Pts',(9.99999999999999,30.6870524499179,56.7884617083184));
#134112=CARTESIAN_POINT('Ctrl Pts',(10.,30.7549278753879,56.767884646354));
#134113=CARTESIAN_POINT('Ctrl Pts',(9.99999999999999,30.8215494692935,56.7437665839902));
#134114=CARTESIAN_POINT('Ctrl Pts',(9.99999999999999,30.8900781708933,56.7189581187164));
#134115=CARTESIAN_POINT('Ctrl Pts',(9.99999999999999,30.9572811586239,56.6904029319238));
#134116=CARTESIAN_POINT('Ctrl Pts',(9.99999999999998,31.0228528016449,56.6583153826992));
#134117=CARTESIAN_POINT('Ctrl Pts',(9.99999999999997,31.0884244446658,56.6262278334746));
#134118=CARTESIAN_POINT('Ctrl Pts',(9.99999999999999,31.1523657592502,56.5906075547783));
#134119=CARTESIAN_POINT('Ctrl Pts',(9.99999999999999,31.2143603894943,56.5516177870526));
#134120=CARTESIAN_POINT('Ctrl Pts',(9.99999999999999,31.2296939735553,56.541974163426));
#134121=CARTESIAN_POINT('Ctrl Pts',(9.99999999999998,31.2449083747354,56.5321241791562));
#134122=CARTESIAN_POINT('Ctrl Pts',(9.99999999999999,31.2599985921039,56.5220698622709));
#134123=CARTESIAN_POINT('Ctrl Pts',(10.,31.27183436846,56.5141839158221));
#134124=CARTESIAN_POINT('Ctrl Pts',(9.99999999999997,31.2835950627688,56.506171208362));
#134125=CARTESIAN_POINT('Ctrl Pts',(9.99999999999997,31.2952606081233,56.498045330906));
#134126=CARTESIAN_POINT('Ctrl Pts',(9.99999999999999,31.3571930817231,56.4549049824932));
#134127=CARTESIAN_POINT('Ctrl Pts',(10.,31.4165584957401,56.4085046904197));
#134128=CARTESIAN_POINT('Ctrl Pts',(10.,31.4730420025436,56.3590793199022));
#134129=CARTESIAN_POINT('Ctrl Pts',(10.,31.5293868312765,56.3097752983484));
#134130=CARTESIAN_POINT('Ctrl Pts',(10.,31.5828649228564,56.2574605914182));
#134131=CARTESIAN_POINT('Ctrl Pts',(9.99999999999997,31.6331479801363,56.2023191232462));
#134132=CARTESIAN_POINT('Ctrl Pts',(9.99999999999995,31.6823740195989,56.1483368032542));
#134133=CARTESIAN_POINT('Ctrl Pts',(10.,31.7285388297368,56.0916447820002));
#134134=CARTESIAN_POINT('Ctrl Pts',(9.99999999999997,31.7713051866725,56.0323758367667));
#134135=CARTESIAN_POINT('Ctrl Pts',(9.99999999999996,31.7804904155719,56.0196462318247));
#134136=CARTESIAN_POINT('Ctrl Pts',(9.99999999999997,31.7895187396851,56.0067976234562));
#134137=CARTESIAN_POINT('Ctrl Pts',(9.99999999999997,31.7983865762153,55.9938311168654));
#134138=CARTESIAN_POINT('Ctrl Pts',(9.99999999999996,31.8058544816558,55.9829115825703));
#134139=CARTESIAN_POINT('Ctrl Pts',(9.99999999999997,31.8132085690898,55.9719084345694));
#134140=CARTESIAN_POINT('Ctrl Pts',(9.99999999999996,31.8204488474911,55.9608235001519));
#134141=CARTESIAN_POINT('',(-0.000875592065448203,31.2702649910176,56.0802705037372));
#134142=CARTESIAN_POINT('Ctrl Pts',(-0.000875592065447961,31.2691220366182,
56.0792985018844));
#134143=CARTESIAN_POINT('Ctrl Pts',(-0.00058372804363219,31.2636294785081,
56.0857570733759));
#134144=CARTESIAN_POINT('Ctrl Pts',(-0.000291864021815771,31.2580876178677,
56.0921737165434));
#134145=CARTESIAN_POINT('Ctrl Pts',(0.,31.2524971005285,56.0985476836113));
#134146=CARTESIAN_POINT('Ctrl Pts',(-8.33100949337862E-16,30.5301702171886,
53.0148256743283));
#134147=CARTESIAN_POINT('Ctrl Pts',(1.52400929049043E-14,30.5991889862419,
53.0403807656738));
#134148=CARTESIAN_POINT('Ctrl Pts',(-6.40578742936595E-15,30.6664868862982,
53.0698652772264));
#134149=CARTESIAN_POINT('Ctrl Pts',(-3.05311331771918E-16,30.731871964553,
53.1029808260606));
#134150=CARTESIAN_POINT('Ctrl Pts',(5.93182098850016E-15,30.7987217281326,
53.13683819336));
#134151=CARTESIAN_POINT('Ctrl Pts',(-1.66504703272918E-14,30.8635727616145,
53.1744918299003));
#134152=CARTESIAN_POINT('Ctrl Pts',(-9.52363188311267E-15,30.9261886107377,
53.2156675311995));
#134153=CARTESIAN_POINT('Ctrl Pts',(-3.5353337505241E-15,30.9788013330987,
53.250265253195));
#134154=CARTESIAN_POINT('Ctrl Pts',(-1.39536846550042E-14,31.0298356324975,
53.28735064929));
#134155=CARTESIAN_POINT('Ctrl Pts',(-1.00613961606655E-14,31.0791289275649,
53.3267786872998));
#134156=CARTESIAN_POINT('Ctrl Pts',(-8.36857957455973E-15,31.1011563662468,
53.3443976898116));
#134157=CARTESIAN_POINT('Ctrl Pts',(-2.11056085633504E-14,31.1228358480513,
53.3624846664704));
#134158=CARTESIAN_POINT('Ctrl Pts',(-1.45300438347817E-14,31.144151317974,
53.3810273958102));
#134159=CARTESIAN_POINT('Ctrl Pts',(-1.08684591444371E-14,31.1558637768627,
53.3912162847189));
#134160=CARTESIAN_POINT('Ctrl Pts',(-2.68961571318634E-14,31.1674663119545,
53.4015427856613));
#134161=CARTESIAN_POINT('Ctrl Pts',(-2.51187959321442E-14,31.1789561254162,
53.4120049126992));
#134162=CARTESIAN_POINT('Ctrl Pts',(-2.36718143111391E-14,31.1895497398249,
53.421650999653));
#134163=CARTESIAN_POINT('Ctrl Pts',(1.14391065484607E-15,31.2000489650095,
53.4314138956186));
#134164=CARTESIAN_POINT('Ctrl Pts',(1.1518563880486E-15,31.2104357202779,
53.4412765890835));
#134165=CARTESIAN_POINT('Ctrl Pts',(8.1966554988569E-16,31.2635217526087,
53.4916841755357));
#134166=CARTESIAN_POINT('Ctrl Pts',(-3.26175822196583E-15,31.3137676963847,
53.5447801824368));
#134167=CARTESIAN_POINT('Ctrl Pts',(-9.28424004342787E-15,31.3609548581112,
53.6003052242583));
#134168=CARTESIAN_POINT('Ctrl Pts',(-1.52131118947695E-14,31.4074085699195,
53.6549672169815));
#134169=CARTESIAN_POINT('Ctrl Pts',(5.15834010684451E-15,31.450898285427,
53.7119842112287));
#134170=CARTESIAN_POINT('Ctrl Pts',(8.42381719934338E-15,31.491171791901,
53.7711323423525));
#134171=CARTESIAN_POINT('Ctrl Pts',(1.11846352470455E-14,31.5252212800365,
53.8211395000414));
#134172=CARTESIAN_POINT('Ctrl Pts',(9.24895866556134E-15,31.556971266667,
53.8726706304121));
#134173=CARTESIAN_POINT('Ctrl Pts',(-6.82787160144471E-15,31.5862409537777,
53.9255971284423));
#134174=CARTESIAN_POINT('Ctrl Pts',(-1.34890089303024E-14,31.5983464196043,
53.9474866659287));
#134175=CARTESIAN_POINT('Ctrl Pts',(-4.85517114680581E-15,31.6100272974802,
53.9696149232492));
#134176=CARTESIAN_POINT('Ctrl Pts',(-1.90125692967058E-14,31.6212693466356,
53.9919728866902));
#134177=CARTESIAN_POINT('Ctrl Pts',(-2.5771791364664E-14,31.6264713864379,
54.0023185998349));
#134178=CARTESIAN_POINT('Ctrl Pts',(-2.75258379892674E-14,31.6315794520179,
54.0127134975132));
#134179=CARTESIAN_POINT('Ctrl Pts',(-2.43693953905222E-14,31.6365920671342,
54.0231566846752));
#134180=CARTESIAN_POINT('Ctrl Pts',(-2.07974541930872E-14,31.6418226285869,
54.0340539370965));
#134181=CARTESIAN_POINT('Ctrl Pts',(-2.23959949028931E-14,31.646945646026,
54.0449963095968));
#134182=CARTESIAN_POINT('Ctrl Pts',(-2.29816166097407E-14,31.6519580706395,
54.0559785146692));
#134183=CARTESIAN_POINT('Ctrl Pts',(-2.63568282812162E-14,31.6804983232411,
54.1185101098663));
#134184=CARTESIAN_POINT('Ctrl Pts',(-1.07629757736254E-14,31.7054776292798,
54.1823749831571));
#134185=CARTESIAN_POINT('Ctrl Pts',(-4.12170297892089E-15,31.7266725222073,
54.247368770426));
#134186=CARTESIAN_POINT('Ctrl Pts',(1.92857175470246E-15,31.745878736449,
54.3062643075221));
#134187=CARTESIAN_POINT('Ctrl Pts',(-2.25561961424682E-14,31.7619770689939,
54.366087447406));
#134188=CARTESIAN_POINT('Ctrl Pts',(-2.02060590481778E-14,31.7747645151277,
54.426690952962));
#134189=CARTESIAN_POINT('Ctrl Pts',(-1.72961694481268E-14,31.7898957509816,
54.4984023741906));
#134190=CARTESIAN_POINT('Ctrl Pts',(-1.01685731942279E-14,31.8003917803375,
54.5712079602738));
#134191=CARTESIAN_POINT('Ctrl Pts',(-5.35682609381638E-15,31.806327769353,
54.6446844903357));
#134192=CARTESIAN_POINT('Ctrl Pts',(-4.30837113251911E-15,31.8076343958791,
54.6608581023443));
#134193=CARTESIAN_POINT('Ctrl Pts',(5.81263003671622E-15,31.8087198528652,
54.6770641414933));
#134194=CARTESIAN_POINT('Ctrl Pts',(8.74300631892311E-15,31.8095845725196,
54.6932979294799));
#134195=CARTESIAN_POINT('Ctrl Pts',(1.17064828251018E-14,31.8104783156427,
54.7100765886703));
#134196=CARTESIAN_POINT('Ctrl Pts',(-1.48807671551939E-15,31.8111362648404,
54.7268910640621));
#134197=CARTESIAN_POINT('Ctrl Pts',(1.80411241501588E-15,31.8115583378869,
54.7437019950884));
#134198=CARTESIAN_POINT('Ctrl Pts',(1.47366039221688E-14,31.8132818157269,
54.8123471439272));
#134199=CARTESIAN_POINT('Ctrl Pts',(-1.9678893150324E-14,31.8110841157504,
54.8810202510296));
#134200=CARTESIAN_POINT('Ctrl Pts',(-1.16850973341798E-14,31.805086261906,
54.9493816698622));
#134201=CARTESIAN_POINT('Ctrl Pts',(-3.71230872538842E-15,31.7991041700553,
55.0175634390598));
#134202=CARTESIAN_POINT('Ctrl Pts',(-2.16825510572882E-14,31.7893413986122,
55.085436219163));
#134203=CARTESIAN_POINT('Ctrl Pts',(-6.46704911844154E-15,31.7758685974957,
55.1526480508404));
#134204=CARTESIAN_POINT('Ctrl Pts',(4.77989727775678E-15,31.7661072564571,
55.2013445026887));
#134205=CARTESIAN_POINT('Ctrl Pts',(1.70591577400874E-14,31.7543973564531,
55.2496937384255));
#134206=CARTESIAN_POINT('Ctrl Pts',(1.11299858218672E-14,31.7407515688752,
55.2975522498582));
#134207=CARTESIAN_POINT('Ctrl Pts',(6.6694150280109E-15,31.730514376406,
55.333456135217));
#134208=CARTESIAN_POINT('Ctrl Pts',(-2.94485010351568E-14,31.7191873909037,
55.3690836793064));
#134209=CARTESIAN_POINT('Ctrl Pts',(2.41473507855972E-15,31.7067720469057,
55.4043701113268));
#134210=CARTESIAN_POINT('Ctrl Pts',(1.31535546200685E-14,31.7026434175627,
55.4161043491114));
#134211=CARTESIAN_POINT('Ctrl Pts',(1.33952048454485E-14,31.6983976298144,
55.4277916642713));
#134212=CARTESIAN_POINT('Ctrl Pts',(1.0547118733939E-14,31.694035322072,
55.4394295150765));
#134213=CARTESIAN_POINT('Ctrl Pts',(-4.75894157798451E-15,31.6709110098913,
55.5011210121069));
#134214=CARTESIAN_POINT('Ctrl Pts',(-6.26081247270993E-15,31.6445141936346,
55.5614289964144));
#134215=CARTESIAN_POINT('Ctrl Pts',(-3.13638004456607E-15,31.6148948930439,
55.6200193099657));
#134216=CARTESIAN_POINT('Ctrl Pts',(-4.45298702533462E-16,31.5940584883539,
55.6612360659228));
#134217=CARTESIAN_POINT('Ctrl Pts',(-1.57022272665468E-14,31.5716265001234,
55.7016022596676));
#134218=CARTESIAN_POINT('Ctrl Pts',(6.66133814775094E-15,31.5476059348169,
55.7409902049166));
#134219=CARTESIAN_POINT('Ctrl Pts',(1.38011075348573E-14,31.5398931143376,
55.7536373739935));
#134220=CARTESIAN_POINT('Ctrl Pts',(-2.65642106040399E-15,31.5320153495236,
55.7661852983957));
#134221=CARTESIAN_POINT('Ctrl Pts',(-2.3037127760972E-15,31.523976211793,
55.7786240933602));
#134222=CARTESIAN_POINT('Ctrl Pts',(2.60456430514903E-16,31.489731385867,
55.8316104188294));
#134223=CARTESIAN_POINT('Ctrl Pts',(1.23913251833813E-14,31.4526309856926,
55.8825128586331));
#134224=CARTESIAN_POINT('Ctrl Pts',(1.1296519275561E-14,31.4127092681578,
55.9310161346265));
#134225=CARTESIAN_POINT('Ctrl Pts',(9.71221749203167E-15,31.3759121039422,
55.9757232044103));
#134226=CARTESIAN_POINT('Ctrl Pts',(1.80240216455387E-14,31.3367173859466,
56.0183920601835));
#134227=CARTESIAN_POINT('Ctrl Pts',(1.6153745008296E-14,31.2951304838667,
56.0587428782121));
#134228=CARTESIAN_POINT('Ctrl Pts',(1.60754418658392E-14,31.2873272806742,
56.0663141474415));
#134229=CARTESIAN_POINT('Ctrl Pts',(-3.83560330923859E-15,31.2794398022902,
56.0738037018648));
#134230=CARTESIAN_POINT('Ctrl Pts',(-1.11022302462516E-15,31.2714696314036,
56.0812108797947));
#134231=CARTESIAN_POINT('Ctrl Pts',(0.00172041412894349,28.7336299816271,
126.077829820709));
#134232=CARTESIAN_POINT('Ctrl Pts',(0.0387785735230462,28.3750939246243,
125.656600540125));
#134233=CARTESIAN_POINT('Ctrl Pts',(0.112881823196669,28.1181816877044,
124.435269010958));
#134234=CARTESIAN_POINT('Ctrl Pts',(0.224030163149812,29.4557424409344,
123.110121783689));
#134235=CARTESIAN_POINT('Ctrl Pts',(0.335165433988371,31.2917730403109,
123.519030371424));
#134236=CARTESIAN_POINT('Ctrl Pts',(0.44630070482693,31.9452349105524,125.281415227633));
#134237=CARTESIAN_POINT('Ctrl Pts',(0.55743597566549,30.818400731034,126.787219544026));
#134238=CARTESIAN_POINT('Ctrl Pts',(0.668571246504049,28.9424467746888,
126.656743001303));
#134239=CARTESIAN_POINT('Ctrl Pts',(0.779706517342608,28.0344714474466,
125.010137817827));
#134240=CARTESIAN_POINT('Ctrl Pts',(0.890841788181168,28.9254742404942,
123.354134483461));
#134241=CARTESIAN_POINT('Ctrl Pts',(1.00197705901972,30.7999674965501,123.204604403169));
#134242=CARTESIAN_POINT('Ctrl Pts',(1.11311232985828,31.9422694308905,124.698320240969));
#134243=CARTESIAN_POINT('Ctrl Pts',(1.22424760069684,31.3068686523209,126.468169431628));
#134244=CARTESIAN_POINT('Ctrl Pts',(1.3353828715354,29.4753269319837,126.894237405488));
#134245=CARTESIAN_POINT('Ctrl Pts',(1.44651814237396,28.1240041248564,125.586566748605));
#134246=CARTESIAN_POINT('Ctrl Pts',(1.55765341321252,28.4897272792089,123.742026340277));
#134247=CARTESIAN_POINT('Ctrl Pts',(1.66878868405108,30.2377606151872,123.04887463911));
#134248=CARTESIAN_POINT('Ctrl Pts',(1.77992395488964,31.7681783056687,124.141532593809));
#134249=CARTESIAN_POINT('Ctrl Pts',(1.8910592257282,31.6802322299405,126.019921790054));
#134250=CARTESIAN_POINT('Ctrl Pts',(2.00219449656676,30.0544169149864,126.964805201012));
#134251=CARTESIAN_POINT('Ctrl Pts',(2.11332976740532,28.3787953370211,126.111357812589));
#134252=CARTESIAN_POINT('Ctrl Pts',(2.22446503824388,28.1870167132214,124.240715901116));
#134253=CARTESIAN_POINT('Ctrl Pts',(2.33560030908244,29.6546106200314,123.065025348056));
#134254=CARTESIAN_POINT('Ctrl Pts',(2.44673557992099,31.438329695648,123.660362577878));
#134255=CARTESIAN_POINT('Ctrl Pts',(2.55787085075956,31.9055861202118,125.481832204441));
#134256=CARTESIAN_POINT('Ctrl Pts',(2.66900612159811,30.6287132507792,126.862294386418));
#134257=CARTESIAN_POINT('Ctrl Pts',(2.78014139243668,28.7763968543991,126.538250979697));
#134258=CARTESIAN_POINT('Ctrl Pts',(2.89127666327523,28.0440099471773,124.806289784764));
#134259=CARTESIAN_POINT('Ctrl Pts',(3.0024119341138,29.1018856333851,123.251626093031));
#134260=CARTESIAN_POINT('Ctrl Pts',(3.11354720495235,30.9817800986816,123.297199785044));
#134261=CARTESIAN_POINT('Ctrl Pts',(3.22468247579091,31.9630788972596,124.901298544487));
#134262=CARTESIAN_POINT('Ctrl Pts',(3.33581774662947,31.1476268828135,126.595735965634));
#134263=CARTESIAN_POINT('Ctrl Pts',(3.44695301746803,29.2817843121772,126.829641210717));
#134264=CARTESIAN_POINT('Ctrl Pts',(3.55808828830659,28.0733043278437,125.38892739821));
#134265=CARTESIAN_POINT('Ctrl Pts',(3.66922355914515,28.6282746155421,123.592239294547));
#134266=CARTESIAN_POINT('Ctrl Pts',(3.78035882998371,30.4387465049373,123.08403490674));
#134267=CARTESIAN_POINT('Ctrl Pts',(3.89149410082227,31.8476460782342,124.329459394392));
#134268=CARTESIAN_POINT('Ctrl Pts',(4.00262937166083,31.5654472459206,126.188610808644));
#134269=CARTESIAN_POINT('Ctrl Pts',(4.11376464249939,29.8504386494267,126.959860233945));
#134270=CARTESIAN_POINT('Ctrl Pts',(4.22489991333795,28.2723193438391,125.937304798085));
#134271=CARTESIAN_POINT('Ctrl Pts',(4.3360351841765,28.2754974725687,124.056860685229));
#134272=CARTESIAN_POINT('Ctrl Pts',(4.44717045501507,29.8570641839197,123.039645418128));
#134273=CARTESIAN_POINT('Ctrl Pts',(4.55830572585362,31.5694560211028,123.816687474921));
#134274=CARTESIAN_POINT('Ctrl Pts',(4.66944099669219,31.8453689751119,125.676782150975));
#134275=CARTESIAN_POINT('Ctrl Pts',(4.78057626753074,30.4322676918504,126.917437189784));
#134276=CARTESIAN_POINT('Ctrl Pts',(4.89171153836931,28.6235239675951,126.403115984657));
#134277=CARTESIAN_POINT('Ctrl Pts',(5.00284680920786,28.0746299792728,124.604562245771));
#134278=CARTESIAN_POINT('Ctrl Pts',(5.11398208004642,29.2879729315736,123.167941543506));
#134279=CARTESIAN_POINT('Ctrl Pts',(5.22511735088498,31.1530142011832,123.408152335789));
#134280=CARTESIAN_POINT('Ctrl Pts',(5.33625262172354,31.9627340538628,125.105336451391));
#134281=CARTESIAN_POINT('Ctrl Pts',(5.4473878925621,30.9760187189675,126.706109080455));
#134282=CARTESIAN_POINT('Ctrl Pts',(5.55852316340066,29.0959809458976,126.745328130754));
#134283=CARTESIAN_POINT('Ctrl Pts',(5.66965843423922,28.0433663460444,125.187097510387));
#134284=CARTESIAN_POINT('Ctrl Pts',(5.78079370507778,28.7816034095847,123.457621809462));
#134285=CARTESIAN_POINT('Ctrl Pts',(5.89192897591634,30.6350045490403,123.139841416201));
#134286=CARTESIAN_POINT('Ctrl Pts',(6.0030642467549,31.9072039133898,124.524611772405));
#134287=CARTESIAN_POINT('Ctrl Pts',(6.11419951759346,31.433793263407,126.344491581228));
#134288=CARTESIAN_POINT('Ctrl Pts',(6.22533478843202,29.6480720306313,126.93379612125));
#134289=CARTESIAN_POINT('Ctrl Pts',(6.33647005927058,28.1844605541017,125.753151548211));
#134290=CARTESIAN_POINT('Ctrl Pts',(6.44760533010913,28.3825611870771,123.883168580029));
#134291=CARTESIAN_POINT('Ctrl Pts',(6.5587406009477,30.0610580008629,123.035389948434));
#134292=CARTESIAN_POINT('Ctrl Pts',(6.66987587178625,31.683670146515,123.985763552263));
#134293=CARTESIAN_POINT('Ctrl Pts',(6.78101114262482,31.7652664375161,125.864439204784));
#134294=CARTESIAN_POINT('Ctrl Pts',(6.89214641346337,30.231164087347,126.951918005167));
#134295=CARTESIAN_POINT('Ctrl Pts',(7.00328168430194,28.4854837601286,126.252861242657));
#134296=CARTESIAN_POINT('Ctrl Pts',(7.11441695514049,28.1259974820121,124.407095878917));
#134297=CARTESIAN_POINT('Ctrl Pts',(7.22555222597905,29.4817329163543,123.103998954614));
#134298=CARTESIAN_POINT('Ctrl Pts',(7.33668749681761,31.3118236122709,123.536258375082));
#134299=CARTESIAN_POINT('Ctrl Pts',(7.44782276765618,31.9412391111934,125.30823927011));
#134300=CARTESIAN_POINT('Ctrl Pts',(7.55895803849473,30.7938931378223,126.798097444275));
#134301=CARTESIAN_POINT('Ctrl Pts',(7.67009330933329,28.9199191404933,126.64220768227));
#134302=CARTESIAN_POINT('Ctrl Pts',(7.78122858017185,28.0345127261816,124.983251489876));
#134303=CARTESIAN_POINT('Ctrl Pts',(7.89236385101041,28.9480614458749,123.339624739461));
#134304=CARTESIAN_POINT('Ctrl Pts',(8.00349912184897,30.82441988656,123.215692685774));
#134305=CARTESIAN_POINT('Ctrl Pts',(8.11463439268753,31.9462100369406,124.724886861491));
#134306=CARTESIAN_POINT('Ctrl Pts',(8.22576966352609,31.2866889522822,126.48588432209));
#134307=CARTESIAN_POINT('Ctrl Pts',(8.33690493436464,29.4494977464259,126.886893763084));
#134308=CARTESIAN_POINT('Ctrl Pts',(8.44804020520321,28.1161656850418,125.560882413626));
#134309=CARTESIAN_POINT('Ctrl Pts',(8.55917547604176,28.507054224578,123.721511362706));
#134310=CARTESIAN_POINT('Ctrl Pts',(8.67031074688032,30.2643937283649,123.052304598731));
#134311=CARTESIAN_POINT('Ctrl Pts',(8.78144601771889,31.7797415997414,124.165769269162));
#134312=CARTESIAN_POINT('Ctrl Pts',(8.89258128855744,31.6661411113959,126.042780405246));
#134313=CARTESIAN_POINT('Ctrl Pts',(9.00371655939601,30.0275706462923,126.965366890392));
#134314=CARTESIAN_POINT('Ctrl Pts',(9.11485183023456,28.3637614026585,126.089102599277));
#134315=CARTESIAN_POINT('Ctrl Pts',(9.22598710107312,28.1975636414152,124.216025180308));
#134316=CARTESIAN_POINT('Ctrl Pts',(9.33712237191168,29.6810681170523,123.060473934073));
#134317=CARTESIAN_POINT('Ctrl Pts',(9.44825764275024,31.4565163554669,123.680164641892));
#134318=CARTESIAN_POINT('Ctrl Pts',(9.5593929135888,31.8987865585251,125.507765498923));
#134319=CARTESIAN_POINT('Ctrl Pts',(9.67052818442736,30.6032919443857,126.870821286213));
#134320=CARTESIAN_POINT('Ctrl Pts',(9.78166345526592,28.7553356095551,126.521165323933));
#134321=CARTESIAN_POINT('Ctrl Pts',(9.89279872610447,28.0471642005665,124.780043256774));
#134322=CARTESIAN_POINT('Ctrl Pts',(10.0039339969431,29.125189557685,123.238590719592));
#134323=CARTESIAN_POINT('Ctrl Pts',(10.1150692677816,31.0063485869877,123.312692118962));
#134324=CARTESIAN_POINT('Ctrl Pts',(10.1891594483406,31.641620391195,124.386603406702));
#134325=CARTESIAN_POINT('Ctrl Pts',(10.2262045386202,31.6618401036677,124.939191752144));
#134326=CARTESIAN_POINT('Ctrl Pts',(-0.0741753660804533,28.6335242142575,
126.163031601966));
#134327=CARTESIAN_POINT('Ctrl Pts',(-0.0371172066863504,28.2466461035143,
125.708504407061));
#134328=CARTESIAN_POINT('Ctrl Pts',(0.0369860429872722,27.9694251130308,
124.390627375262));
#134329=CARTESIAN_POINT('Ctrl Pts',(0.148134382940415,29.412719217227,122.960728078584));
#134330=CARTESIAN_POINT('Ctrl Pts',(0.259269653778974,31.3938869008663,
123.401960637484));
#134331=CARTESIAN_POINT('Ctrl Pts',(0.370404924617533,32.0990045281285,
125.303660927471));
#134332=CARTESIAN_POINT('Ctrl Pts',(0.481540195456093,30.8830948030726,
126.928498144528));
#134333=CARTESIAN_POINT('Ctrl Pts',(0.592675466294653,28.8588478457675,
126.787707511733));
#134334=CARTESIAN_POINT('Ctrl Pts',(0.703810737133211,27.8790976300112,
125.010939206061));
#134335=CARTESIAN_POINT('Ctrl Pts',(0.814946007971772,28.8405336432333,
123.22402983148));
#134336=CARTESIAN_POINT('Ctrl Pts',(0.92608127881033,30.8632044327939,123.062679490744));
#134337=CARTESIAN_POINT('Ctrl Pts',(1.03721654964889,32.0958046291319,124.674472642447));
#134338=CARTESIAN_POINT('Ctrl Pts',(1.14835182048745,31.4101758116771,126.584227317909));
#134339=CARTESIAN_POINT('Ctrl Pts',(1.259487091326,29.4338518501909,127.043975701803));
#134340=CARTESIAN_POINT('Ctrl Pts',(1.37062236216457,27.9757078102415,125.632934487599));
#134341=CARTESIAN_POINT('Ctrl Pts',(1.48175763300312,28.3703411539385,123.64258429987));
#134342=CARTESIAN_POINT('Ctrl Pts',(1.59289290384169,30.256555444888,122.894639385076));
#134343=CARTESIAN_POINT('Ctrl Pts',(1.70402817468025,31.907951708045,124.073671275859));
#134344=CARTESIAN_POINT('Ctrl Pts',(1.8151634455188,31.8130535493788,126.100545977274));
#134345=CARTESIAN_POINT('Ctrl Pts',(1.92629871635736,30.0587185384879,127.120121837955));
#134346=CARTESIAN_POINT('Ctrl Pts',(2.03743398719592,28.2506401102737,126.199209960885));
#134347=CARTESIAN_POINT('Ctrl Pts',(2.14856925803448,28.0437015047767,124.180694962316));
#134348=CARTESIAN_POINT('Ctrl Pts',(2.25970452887304,29.6273078029863,122.912066797581));
#134349=CARTESIAN_POINT('Ctrl Pts',(2.3708397997116,31.5520287692397,123.554465067519));
#134350=CARTESIAN_POINT('Ctrl Pts',(2.48197507055016,32.0562215254133,125.519920742442));
#134351=CARTESIAN_POINT('Ctrl Pts',(2.59311034138872,30.6784126447253,127.009507606816));
#134352=CARTESIAN_POINT('Ctrl Pts',(2.70424561222729,28.6796717818933,126.659848769045));
#134353=CARTESIAN_POINT('Ctrl Pts',(2.81538088306583,27.8893901422511,124.790977111957));
#134354=CARTESIAN_POINT('Ctrl Pts',(2.92651615390439,29.0308902477149,123.113418216132));
#134355=CARTESIAN_POINT('Ctrl Pts',(3.03765142474296,31.0593892087685,123.162594480336));
#134356=CARTESIAN_POINT('Ctrl Pts',(3.14878669558152,32.1182590709579,124.893496255424));
#134357=CARTESIAN_POINT('Ctrl Pts',(3.25992196642008,31.2383460786973,126.721877907595));
#134358=CARTESIAN_POINT('Ctrl Pts',(3.37105723725863,29.2250098058928,126.974273217756));
#134359=CARTESIAN_POINT('Ctrl Pts',(3.4821925080972,27.9210002256061,125.419671868692));
#134360=CARTESIAN_POINT('Ctrl Pts',(3.59332777893576,28.5198405715902,123.48095668074));
#134361=CARTESIAN_POINT('Ctrl Pts',(3.70446304977431,30.473429145019,122.932579050133));
#134362=CARTESIAN_POINT('Ctrl Pts',(3.81559832061288,31.9937013589228,124.276453573894));
#134363=CARTESIAN_POINT('Ctrl Pts',(3.92673359145143,31.6891948833062,126.282569758537));
#134364=CARTESIAN_POINT('Ctrl Pts',(4.03786886229,29.8386159170887,127.114785974297));
#134365=CARTESIAN_POINT('Ctrl Pts',(4.14900413312855,28.13574725563,126.011398163144));
#134366=CARTESIAN_POINT('Ctrl Pts',(4.2601394039671,28.1391766134716,123.98230610523));
#134367=CARTESIAN_POINT('Ctrl Pts',(4.37127467480567,29.8457651959891,122.884680599877));
#134368=CARTESIAN_POINT('Ctrl Pts',(4.48240994564422,31.6935205496892,123.723147351069));
#134369=CARTESIAN_POINT('Ctrl Pts',(4.5935452164828,31.9912442522059,125.730281361776));
#134370=CARTESIAN_POINT('Ctrl Pts',(4.70468048732134,30.4664381857613,127.069009414712));
#134371=CARTESIAN_POINT('Ctrl Pts',(4.81581575815992,28.5147143878589,126.514031436155));
#134372=CARTESIAN_POINT('Ctrl Pts',(4.92695102899846,27.9224306689614,124.573303135669));
#134373=CARTESIAN_POINT('Ctrl Pts',(5.03808629983704,29.2316876318282,123.023118454682));
#134374=CARTESIAN_POINT('Ctrl Pts',(5.14922157067558,31.2441592612549,123.282317761652));
#134375=CARTESIAN_POINT('Ctrl Pts',(5.26035684151415,32.1178869679037,125.113663232778));
#134376=CARTESIAN_POINT('Ctrl Pts',(5.3714921123527,31.0531723955484,126.840975948935));
#134377=CARTESIAN_POINT('Ctrl Pts',(5.48262738319128,29.0245187983303,126.883295240925));
#134378=CARTESIAN_POINT('Ctrl Pts',(5.59376265402982,27.8886956648464,125.201887452962));
#134379=CARTESIAN_POINT('Ctrl Pts',(5.7048979248684,28.6852899120488,123.335697766648));
#134380=CARTESIAN_POINT('Ctrl Pts',(5.81603319570694,30.6852012662261,122.992797029679));
#134381=CARTESIAN_POINT('Ctrl Pts',(5.92716846654552,32.0579672041423,124.487032626791));
#134382=CARTESIAN_POINT('Ctrl Pts',(6.03830373738406,31.5471337348335,126.450772809865));
#134383=CARTESIAN_POINT('Ctrl Pts',(6.14943900822263,29.6202523421347,127.0866615096));
#134384=CARTESIAN_POINT('Ctrl Pts',(6.26057427906118,28.0409432828582,125.812687712669));
#134385=CARTESIAN_POINT('Ctrl Pts',(6.37170954989974,28.2547036484494,123.794883746451));
#134386=CARTESIAN_POINT('Ctrl Pts',(6.4828448207383,30.0658845980988,122.880088737935));
#134387=CARTESIAN_POINT('Ctrl Pts',(6.59398009157685,31.816763231134,123.90558878784));
#134388=CARTESIAN_POINT('Ctrl Pts',(6.70511536241541,31.9048096585145,125.932772589723));
#134389=CARTESIAN_POINT('Ctrl Pts',(6.81625063325399,30.2494374655985,127.106215917242));
#134390=CARTESIAN_POINT('Ctrl Pts',(6.92738590409254,28.3657621872972,126.351899149654));
#134391=CARTESIAN_POINT('Ctrl Pts',(7.0385211749311,27.9778587410484,124.360227174544));
#134392=CARTESIAN_POINT('Ctrl Pts',(7.14965644576966,29.4407642236672,122.954121243655));
#134393=CARTESIAN_POINT('Ctrl Pts',(7.26079171660821,31.4155224581491,123.420550504186));
#134394=CARTESIAN_POINT('Ctrl Pts',(7.37192698744678,32.0946928632995,125.332605393929));
#134395=CARTESIAN_POINT('Ctrl Pts',(7.48306225828533,30.8566498997625,126.94023593607));
#134396=CARTESIAN_POINT('Ctrl Pts',(7.5941975291239,28.8345394160104,126.772023184714));
#134397=CARTESIAN_POINT('Ctrl Pts',(7.70533279996246,27.8791421718047,124.981927530501));
#134398=CARTESIAN_POINT('Ctrl Pts',(7.81646807080102,28.8649063532411,123.208373101183));
#134399=CARTESIAN_POINT('Ctrl Pts',(7.92760334163957,30.8895897691232,123.074644295238));
#134400=CARTESIAN_POINT('Ctrl Pts',(8.03873861247814,32.100056737655,124.703139337904));
#134401=CARTESIAN_POINT('Ctrl Pts',(8.14987388331669,31.3884009188208,126.603342559515));
#134402=CARTESIAN_POINT('Ctrl Pts',(8.26100915415525,29.4059808834766,127.036051549007));
#134403=CARTESIAN_POINT('Ctrl Pts',(8.37214442499382,27.9672497466033,125.605219821814));
#134404=CARTESIAN_POINT('Ctrl Pts',(8.48327969583238,28.3890377836314,123.620447626));
#134405=CARTESIAN_POINT('Ctrl Pts',(8.59441496667093,30.2852938892039,122.898340480884));
#134406=CARTESIAN_POINT('Ctrl Pts',(8.70555023750948,31.9204290733683,124.099823845421));
#134407=CARTESIAN_POINT('Ctrl Pts',(8.81668550834805,31.7978485366211,126.12521155187));
#134408=CARTESIAN_POINT('Ctrl Pts',(8.92782077918661,30.0297500888439,127.120727928533));
#134409=CARTESIAN_POINT('Ctrl Pts',(9.03895605002517,28.2344177526903,126.175195486713));
#134410=CARTESIAN_POINT('Ctrl Pts',(9.15009132086374,28.0550821611265,124.154052455286));
#134411=CARTESIAN_POINT('Ctrl Pts',(9.26122659170229,29.6558567487967,122.907155597137));
#134412=CARTESIAN_POINT('Ctrl Pts',(9.37236186254086,31.5716530732786,123.575832472457));
#134413=CARTESIAN_POINT('Ctrl Pts',(9.48349713337941,32.0488844625773,125.547904047827));
#134414=CARTESIAN_POINT('Ctrl Pts',(9.59463240421796,30.6509817997711,127.018708552771));
#134415=CARTESIAN_POINT('Ctrl Pts',(9.70576767505652,28.6569456586597,126.641412502749));
#134416=CARTESIAN_POINT('Ctrl Pts',(9.81690294589508,27.8927937374215,124.762655812148));
#134417=CARTESIAN_POINT('Ctrl Pts',(9.92803821673365,29.0560363328294,123.099352404481));
#134418=CARTESIAN_POINT('Ctrl Pts',(10.0391734875722,31.0858998208927,123.179311473677));
#134419=CARTESIAN_POINT('Ctrl Pts',(10.1132636681313,31.7713894686415,124.338114785064));
#134420=CARTESIAN_POINT('Ctrl Pts',(10.1503087584108,31.79320753689,124.934384897729));
#134421=CARTESIAN_POINT('Ctrl Pts',(-0.15007114628985,28.5334184468878,
126.248233383223));
#134422=CARTESIAN_POINT('Ctrl Pts',(-0.113012986895747,28.1181982824042,
125.760408273996));
#134423=CARTESIAN_POINT('Ctrl Pts',(-0.0389097372221243,27.8206685383571,
124.345985739566));
#134424=CARTESIAN_POINT('Ctrl Pts',(0.0722386027310179,29.3696959935194,
122.811334373478));
#134425=CARTESIAN_POINT('Ctrl Pts',(0.183373873569577,31.4960007614218,
123.284890903545));
#134426=CARTESIAN_POINT('Ctrl Pts',(0.294509144408137,32.2527741457047,
125.325906627308));
#134427=CARTESIAN_POINT('Ctrl Pts',(0.405644415246696,30.9477888751111,
127.06977674503));
#134428=CARTESIAN_POINT('Ctrl Pts',(0.516779686085255,28.7752489168462,
126.918672022163));
#134429=CARTESIAN_POINT('Ctrl Pts',(0.627914956923815,27.7237238125758,
125.011740594295));
#134430=CARTESIAN_POINT('Ctrl Pts',(0.739050227762374,28.7555930459725,
123.093925179498));
#134431=CARTESIAN_POINT('Ctrl Pts',(0.850185498600933,30.9264413690376,
122.920754578321));
#134432=CARTESIAN_POINT('Ctrl Pts',(0.961320769439493,32.2493398273734,
124.650625043926));
#134433=CARTESIAN_POINT('Ctrl Pts',(1.07245604027805,31.5134829710332,126.700285204189));
#134434=CARTESIAN_POINT('Ctrl Pts',(1.18359131111662,29.3923767683981,127.193713998118));
#134435=CARTESIAN_POINT('Ctrl Pts',(1.29472658195517,27.8274114956265,125.679302226594));
#134436=CARTESIAN_POINT('Ctrl Pts',(1.40586185279373,28.250955028668,123.543142259463));
#134437=CARTESIAN_POINT('Ctrl Pts',(1.51699712363229,30.2753502745888,122.74040413104));
#134438=CARTESIAN_POINT('Ctrl Pts',(1.62813239447085,32.0477251104213,124.00580995791));
#134439=CARTESIAN_POINT('Ctrl Pts',(1.73926766530941,31.9458748688171,126.181170164493));
#134440=CARTESIAN_POINT('Ctrl Pts',(1.85040293614797,30.0630201619894,127.275438474898));
#134441=CARTESIAN_POINT('Ctrl Pts',(1.96153820698653,28.1224848835262,126.287062109182));
#134442=CARTESIAN_POINT('Ctrl Pts',(2.07267347782509,27.9003862963319,124.120674023516));
#134443=CARTESIAN_POINT('Ctrl Pts',(2.18380874866365,29.6000049859411,122.759108247108));
#134444=CARTESIAN_POINT('Ctrl Pts',(2.29494401950221,31.6657278428315,123.44856755716));
#134445=CARTESIAN_POINT('Ctrl Pts',(2.40607929034077,32.2068569306149,125.558009280444));
#134446=CARTESIAN_POINT('Ctrl Pts',(2.51721456117933,30.7281120386715,127.156720827214));
#134447=CARTESIAN_POINT('Ctrl Pts',(2.62834983201789,28.5829467093875,126.781446558392));
#134448=CARTESIAN_POINT('Ctrl Pts',(2.73948510285645,27.7347703373249,124.77566443915));
#134449=CARTESIAN_POINT('Ctrl Pts',(2.85062037369501,28.9598948620446,122.975210339235));
#134450=CARTESIAN_POINT('Ctrl Pts',(2.96175564453356,31.1369983188555,123.027989175629));
#134451=CARTESIAN_POINT('Ctrl Pts',(3.07289091537213,32.273439244656,124.88569396636));
#134452=CARTESIAN_POINT('Ctrl Pts',(3.18402618621068,31.329065274581,126.848019849556));
#134453=CARTESIAN_POINT('Ctrl Pts',(3.29516145704925,29.1682352996085,127.118905224794));
#134454=CARTESIAN_POINT('Ctrl Pts',(3.4062967278878,27.7686961233683,125.450416339173));
#134455=CARTESIAN_POINT('Ctrl Pts',(3.51743199872636,28.4114065276384,123.369674066932));
#134456=CARTESIAN_POINT('Ctrl Pts',(3.62856726956492,30.5081117851007,122.781123193526));
#134457=CARTESIAN_POINT('Ctrl Pts',(3.73970254040348,32.1397566396115,124.223447753396));
#134458=CARTESIAN_POINT('Ctrl Pts',(3.85083781124204,31.8129425206918,126.37652870843));
#134459=CARTESIAN_POINT('Ctrl Pts',(3.9619730820806,29.8267931847508,127.269711714649));
#134460=CARTESIAN_POINT('Ctrl Pts',(4.07310835291916,27.9991751674208,126.085491528203));
#134461=CARTESIAN_POINT('Ctrl Pts',(4.18424362375772,28.0028557543744,123.907751525233));
#134462=CARTESIAN_POINT('Ctrl Pts',(4.29537889459628,29.8344662080584,122.729715781627));
#134463=CARTESIAN_POINT('Ctrl Pts',(4.40651416543484,31.8175850782756,123.629607227217));
#134464=CARTESIAN_POINT('Ctrl Pts',(4.5176494362734,32.1371195293,125.783780572579));
#134465=CARTESIAN_POINT('Ctrl Pts',(4.62878470711196,30.5006086796722,127.22058163964));
#134466=CARTESIAN_POINT('Ctrl Pts',(4.73991997795051,28.4059048081225,126.624946887655));
#134467=CARTESIAN_POINT('Ctrl Pts',(4.85105524878908,27.77023135865,124.542044025567));
#134468=CARTESIAN_POINT('Ctrl Pts',(4.96219051962763,29.1754023320827,122.87829536586));
#134469=CARTESIAN_POINT('Ctrl Pts',(5.07332579046619,31.3353043213265,123.156483187516));
#134470=CARTESIAN_POINT('Ctrl Pts',(5.18446106130475,32.2730398819445,125.121990014166));
#134471=CARTESIAN_POINT('Ctrl Pts',(5.29559633214331,31.1303260721294,126.975842817415));
#134472=CARTESIAN_POINT('Ctrl Pts',(5.40673160298187,28.9530566507631,127.021262351096));
#134473=CARTESIAN_POINT('Ctrl Pts',(5.51786687382043,27.7340249836483,125.216677395537));
#134474=CARTESIAN_POINT('Ctrl Pts',(5.62900214465898,28.5889764145129,123.213773723834));
#134475=CARTESIAN_POINT('Ctrl Pts',(5.74013741549755,30.7353979834119,122.845752643158));
#134476=CARTESIAN_POINT('Ctrl Pts',(5.85127268633611,32.2087304948949,124.449453481178));
#134477=CARTESIAN_POINT('Ctrl Pts',(5.96240795717467,31.6604742062601,126.557054038501));
#134478=CARTESIAN_POINT('Ctrl Pts',(6.07354322801323,29.5924326536382,127.239526897951));
#134479=CARTESIAN_POINT('Ctrl Pts',(6.18467849885179,27.8974260116147,125.872223877128));
#134480=CARTESIAN_POINT('Ctrl Pts',(6.29581376969034,28.1268461098218,123.706598912874));
#134481=CARTESIAN_POINT('Ctrl Pts',(6.40694904052891,30.0707111953348,122.724787527434));
#134482=CARTESIAN_POINT('Ctrl Pts',(6.51808431136746,31.949856315753,123.825414023417));
#134483=CARTESIAN_POINT('Ctrl Pts',(6.62921958220603,32.0443528795128,126.001105974661));
#134484=CARTESIAN_POINT('Ctrl Pts',(6.74035485304458,30.2677108438501,127.260513829318));
#134485=CARTESIAN_POINT('Ctrl Pts',(6.85149012388314,28.2460406144659,126.450937056652));
#134486=CARTESIAN_POINT('Ctrl Pts',(6.96262539472171,27.8297200000849,124.313358470171));
#134487=CARTESIAN_POINT('Ctrl Pts',(7.07376066556025,29.3997955309802,122.804243532695));
#134488=CARTESIAN_POINT('Ctrl Pts',(7.18489593639883,31.5192213040273,123.304842633289));
#134489=CARTESIAN_POINT('Ctrl Pts',(7.29603120723738,32.2481466154056,125.356971517748));
#134490=CARTESIAN_POINT('Ctrl Pts',(7.40716647807594,30.9194066617026,127.082374427863));
#134491=CARTESIAN_POINT('Ctrl Pts',(7.5183017489145,28.7491596915275,126.901838687156));
#134492=CARTESIAN_POINT('Ctrl Pts',(7.62943701975306,27.7237716174278,124.980603571126));
#134493=CARTESIAN_POINT('Ctrl Pts',(7.74057229059162,28.7817512606074,123.077121462905));
#134494=CARTESIAN_POINT('Ctrl Pts',(7.85170756143018,30.9547596516863,122.933595904703));
#134495=CARTESIAN_POINT('Ctrl Pts',(7.96284283226874,32.2539034383696,124.681391814318));
#134496=CARTESIAN_POINT('Ctrl Pts',(8.07397810310729,31.4901128853594,126.72080079694));
#134497=CARTESIAN_POINT('Ctrl Pts',(8.18511337394586,29.3624640205271,127.185209334929));
#134498=CARTESIAN_POINT('Ctrl Pts',(8.29624864478441,27.818333808165,125.649557230001));
#134499=CARTESIAN_POINT('Ctrl Pts',(8.40738391562298,28.2710213426847,123.519383889294));
#134500=CARTESIAN_POINT('Ctrl Pts',(8.51851918646153,30.3061940500428,122.744376363038));
#134501=CARTESIAN_POINT('Ctrl Pts',(8.62965445730009,32.0611165469952,124.033878421681));
#134502=CARTESIAN_POINT('Ctrl Pts',(8.74078972813866,31.9295559618465,126.207642698494));
#134503=CARTESIAN_POINT('Ctrl Pts',(8.85192499897721,30.0319295313953,127.276088966675));
#134504=CARTESIAN_POINT('Ctrl Pts',(8.96306026981578,28.105074102722,126.26128837415));
#134505=CARTESIAN_POINT('Ctrl Pts',(9.07419554065433,27.9126006808377,124.092079730265));
#134506=CARTESIAN_POINT('Ctrl Pts',(9.1853308114929,29.630645380541,122.7538372602));
#134507=CARTESIAN_POINT('Ctrl Pts',(9.29646608233145,31.6867897910901,123.471500303021));
#134508=CARTESIAN_POINT('Ctrl Pts',(9.40760135317001,32.1989823666295,125.588042596731));
#134509=CARTESIAN_POINT('Ctrl Pts',(9.51873662400857,30.6986716551566,127.166595819328));
#134510=CARTESIAN_POINT('Ctrl Pts',(9.62987189484713,28.5585557077642,126.761659681567));
#134511=CARTESIAN_POINT('Ctrl Pts',(9.74100716568569,27.7384232742764,124.745268367524));
#134512=CARTESIAN_POINT('Ctrl Pts',(9.85214243652425,28.9868831079738,122.960114089368));
#134513=CARTESIAN_POINT('Ctrl Pts',(9.96327770736281,31.1654510547976,123.045930828392));
#134514=CARTESIAN_POINT('Ctrl Pts',(10.0373678879219,31.9011585460881,124.289626163427));
#134515=CARTESIAN_POINT('Ctrl Pts',(10.0744129782014,31.9245749701123,124.929578043314));
#134516=CARTESIAN_POINT('Ctrl Pts',(-0.225966926499246,28.4333126795182,
126.33343516448));
#134517=CARTESIAN_POINT('Ctrl Pts',(-0.188908767105143,27.9897504612942,
125.812312140931));
#134518=CARTESIAN_POINT('Ctrl Pts',(-0.114805517431522,27.6719119636834,
124.301344103871));
#134519=CARTESIAN_POINT('Ctrl Pts',(-0.0036571774783789,29.3266727698119,
122.661940668373));
#134520=CARTESIAN_POINT('Ctrl Pts',(0.10747809336018,31.5981146219772,123.167821169605));
#134521=CARTESIAN_POINT('Ctrl Pts',(0.21861336419874,32.4065437632808,125.348152327146));
#134522=CARTESIAN_POINT('Ctrl Pts',(0.329748635037299,31.0124829471497,
127.211055345531));
#134523=CARTESIAN_POINT('Ctrl Pts',(0.440883905875859,28.6916499879248,
127.049636532593));
#134524=CARTESIAN_POINT('Ctrl Pts',(0.552019176714417,27.5683499951404,
125.01254198253));
#134525=CARTESIAN_POINT('Ctrl Pts',(0.663154447552977,28.6706524487117,
122.963820527516));
#134526=CARTESIAN_POINT('Ctrl Pts',(0.774289718391537,30.9896783052814,
122.778829665898));
#134527=CARTESIAN_POINT('Ctrl Pts',(0.885424989230096,32.4028750256148,
124.626777445404));
#134528=CARTESIAN_POINT('Ctrl Pts',(0.996560260068655,31.6167901303894,
126.81634309047));
#134529=CARTESIAN_POINT('Ctrl Pts',(1.10769553090722,29.3509016866054,127.343452294435));
#134530=CARTESIAN_POINT('Ctrl Pts',(1.21883080174578,27.6791151810116,125.725669965589));
#134531=CARTESIAN_POINT('Ctrl Pts',(1.32996607258433,28.1315689033976,123.443700219056));
#134532=CARTESIAN_POINT('Ctrl Pts',(1.44110134342289,30.2941451042897,122.586168877006));
#134533=CARTESIAN_POINT('Ctrl Pts',(1.55223661426145,32.1874985127976,123.93794863996));
#134534=CARTESIAN_POINT('Ctrl Pts',(1.66337188510001,32.0786961882554,126.261794351712));
#134535=CARTESIAN_POINT('Ctrl Pts',(1.77450715593857,30.0673217854909,127.430755111841));
#134536=CARTESIAN_POINT('Ctrl Pts',(1.88564242677713,27.9943296567787,126.374914257477));
#134537=CARTESIAN_POINT('Ctrl Pts',(1.99677769761569,27.7570710878872,124.060653084717));
#134538=CARTESIAN_POINT('Ctrl Pts',(2.10791296845425,29.572702168896,122.606149696634));
#134539=CARTESIAN_POINT('Ctrl Pts',(2.21904823929281,31.7794269164233,123.342670046801));
#134540=CARTESIAN_POINT('Ctrl Pts',(2.33018351013137,32.3574923358165,125.596097818445));
#134541=CARTESIAN_POINT('Ctrl Pts',(2.44131878096993,30.7778114326176,127.303934047614));
#134542=CARTESIAN_POINT('Ctrl Pts',(2.55245405180849,28.4862216368817,126.903044347739));
#134543=CARTESIAN_POINT('Ctrl Pts',(2.66358932264705,27.5801505323987,124.760351766343));
#134544=CARTESIAN_POINT('Ctrl Pts',(2.77472459348561,28.8888994763742,122.837002462337));
#134545=CARTESIAN_POINT('Ctrl Pts',(2.88585986432417,31.2146074289425,122.893383870921));
#134546=CARTESIAN_POINT('Ctrl Pts',(2.99699513516273,32.4286194183543,124.877891677296));
#134547=CARTESIAN_POINT('Ctrl Pts',(3.10813040600128,31.4197844704647,126.974161791518));
#134548=CARTESIAN_POINT('Ctrl Pts',(3.21926567683985,29.1114607933241,127.263537231831));
#134549=CARTESIAN_POINT('Ctrl Pts',(3.3304009476784,27.6163920211307,125.481160809656));
#134550=CARTESIAN_POINT('Ctrl Pts',(3.44153621851696,28.3029724836865,123.258391453124));
#134551=CARTESIAN_POINT('Ctrl Pts',(3.55267148935552,30.5427944251824,122.629667336919));
#134552=CARTESIAN_POINT('Ctrl Pts',(3.66380676019408,32.2858119203001,124.1704419329));
#134553=CARTESIAN_POINT('Ctrl Pts',(3.77494203103264,31.9366901580772,126.470487658325));
#134554=CARTESIAN_POINT('Ctrl Pts',(3.8860773018712,29.8149704524129,127.424637455002));
#134555=CARTESIAN_POINT('Ctrl Pts',(3.99721257270976,27.8626030792116,126.159584893262));
#134556=CARTESIAN_POINT('Ctrl Pts',(4.10834784354832,27.8665348952773,123.833196945235));
#134557=CARTESIAN_POINT('Ctrl Pts',(4.21948311438688,29.8231672201278,122.574750963377));
#134558=CARTESIAN_POINT('Ctrl Pts',(4.33061838522544,31.941649606862,123.536067103365));
#134559=CARTESIAN_POINT('Ctrl Pts',(4.441753656064,32.282994806394,125.83727978338));
#134560=CARTESIAN_POINT('Ctrl Pts',(4.55288892690256,30.5347791735832,127.372153864567));
#134561=CARTESIAN_POINT('Ctrl Pts',(4.66402419774111,28.2970952283862,126.735862339154));
#134562=CARTESIAN_POINT('Ctrl Pts',(4.77515946857968,27.6180320483386,124.510784915466));
#134563=CARTESIAN_POINT('Ctrl Pts',(4.88629473941823,29.1191170323373,122.733472277036));
#134564=CARTESIAN_POINT('Ctrl Pts',(4.99743001025679,31.4264493813982,123.030648613378));
#134565=CARTESIAN_POINT('Ctrl Pts',(5.10856528109536,32.4281927959853,125.130316795553));
#134566=CARTESIAN_POINT('Ctrl Pts',(5.21970055193391,31.2074797487104,127.110709685895));
#134567=CARTESIAN_POINT('Ctrl Pts',(5.33083582277248,28.8815945031958,127.159229461265));
#134568=CARTESIAN_POINT('Ctrl Pts',(5.44197109361103,27.5793543024504,125.231467338112));
#134569=CARTESIAN_POINT('Ctrl Pts',(5.55310636444959,28.492662916977,123.09184968102));
#134570=CARTESIAN_POINT('Ctrl Pts',(5.66424163528815,30.7855947005978,122.698708256637));
#134571=CARTESIAN_POINT('Ctrl Pts',(5.77537690612671,32.3594937856475,124.411874335563));
#134572=CARTESIAN_POINT('Ctrl Pts',(5.88651217696527,31.7738146776866,126.663335267137));
#134573=CARTESIAN_POINT('Ctrl Pts',(5.99764744780384,29.5646129651416,127.392392286301));
#134574=CARTESIAN_POINT('Ctrl Pts',(6.10878271864238,27.7539087403712,125.931760041586));
#134575=CARTESIAN_POINT('Ctrl Pts',(6.21991798948095,27.998988571194,123.618314079298));
#134576=CARTESIAN_POINT('Ctrl Pts',(6.33105326031951,30.0755377925708,122.569486316934));
#134577=CARTESIAN_POINT('Ctrl Pts',(6.44218853115807,32.082949400372,123.745239258995));
#134578=CARTESIAN_POINT('Ctrl Pts',(6.55332380199662,32.1838961005111,126.069439359598));
#134579=CARTESIAN_POINT('Ctrl Pts',(6.66445907283519,30.2859842221016,127.414811741394));
#134580=CARTESIAN_POINT('Ctrl Pts',(6.77559434367375,28.1263190416345,126.549974963649));
#134581=CARTESIAN_POINT('Ctrl Pts',(6.8867296145123,27.6815812591212,124.266489765798));
#134582=CARTESIAN_POINT('Ctrl Pts',(6.99786488535086,29.3588268382931,122.654365821735));
#134583=CARTESIAN_POINT('Ctrl Pts',(7.10900015618942,31.6229201499055,123.189134762393));
#134584=CARTESIAN_POINT('Ctrl Pts',(7.22013542702799,32.4016003675117,125.381337641565));
#134585=CARTESIAN_POINT('Ctrl Pts',(7.33127069786654,30.9821634236429,127.224512919657));
#134586=CARTESIAN_POINT('Ctrl Pts',(7.4424059687051,28.6637799670445,127.031654189599));
#134587=CARTESIAN_POINT('Ctrl Pts',(7.55354123954367,27.5684010630509,124.97927961175));
#134588=CARTESIAN_POINT('Ctrl Pts',(7.66467651038222,28.6985961679736,122.945869824627));
#134589=CARTESIAN_POINT('Ctrl Pts',(7.77581178122078,31.0199295342495,122.792547514168));
#134590=CARTESIAN_POINT('Ctrl Pts',(7.88694705205934,32.4077501390841,124.65964429073));
#134591=CARTESIAN_POINT('Ctrl Pts',(7.99808232289791,31.5918248518981,126.838259034364));
#134592=CARTESIAN_POINT('Ctrl Pts',(8.10921759373646,29.3189471575778,127.334367120851));
#134593=CARTESIAN_POINT('Ctrl Pts',(8.22035286457502,27.6694178697268,125.693894638187));
#134594=CARTESIAN_POINT('Ctrl Pts',(8.33148813541358,28.1530049017381,123.418320152587));
#134595=CARTESIAN_POINT('Ctrl Pts',(8.44262340625213,30.3270942108819,122.590412245191));
#134596=CARTESIAN_POINT('Ctrl Pts',(8.5537586770907,32.2018040206222,123.967932997941));
#134597=CARTESIAN_POINT('Ctrl Pts',(8.66489394792926,32.0612633870717,126.290073845118));
#134598=CARTESIAN_POINT('Ctrl Pts',(8.77602921876781,30.0341089739469,127.431450004816));
#134599=CARTESIAN_POINT('Ctrl Pts',(8.88716448960638,27.9757304527538,126.347381261586));
#134600=CARTESIAN_POINT('Ctrl Pts',(8.99829976044494,27.7701192005489,124.030107005244));
#134601=CARTESIAN_POINT('Ctrl Pts',(9.10943503128349,29.6054340122852,122.600518923263));
#134602=CARTESIAN_POINT('Ctrl Pts',(9.22057030212206,31.8019265089017,123.367168133586));
#134603=CARTESIAN_POINT('Ctrl Pts',(9.3317055729606,32.3490802706817,125.628181145636));
#134604=CARTESIAN_POINT('Ctrl Pts',(9.44284084379918,30.7463615105419,127.314483085886));
#134605=CARTESIAN_POINT('Ctrl Pts',(9.55397611463773,28.4601657568688,126.881906860385));
#134606=CARTESIAN_POINT('Ctrl Pts',(9.66511138547629,27.5840528111314,124.727880922899));
#134607=CARTESIAN_POINT('Ctrl Pts',(9.77624665631484,28.9177298831183,122.820875774256));
#134608=CARTESIAN_POINT('Ctrl Pts',(9.88738192715342,31.2450022887026,122.912550183106));
#134609=CARTESIAN_POINT('Ctrl Pts',(9.96147210771245,32.0309276235346,124.241137541789));
#134610=CARTESIAN_POINT('Ctrl Pts',(9.99851719799197,32.0559424033345,124.924771188899));
#134611=CARTESIAN_POINT('',(10.0008700299984,29.229417545743,123.521225009551));
#134612=CARTESIAN_POINT('Ctrl Pts',(10.,32.0533758325287,124.92486510207));
#134613=CARTESIAN_POINT('Ctrl Pts',(10.,32.0436838801938,124.850853971349));
#134614=CARTESIAN_POINT('Ctrl Pts',(9.99999999999998,32.0296437464646,124.777580246055));
#134615=CARTESIAN_POINT('Ctrl Pts',(9.99999999999997,32.011487005396,124.705321521794));
#134616=CARTESIAN_POINT('Ctrl Pts',(9.99999999999996,31.9938051114884,124.634952555719));
#134617=CARTESIAN_POINT('Ctrl Pts',(9.99999999999999,31.9722183073752,124.565545575943));
#134618=CARTESIAN_POINT('Ctrl Pts',(9.99999999999997,31.9469006329171,124.497379595077));
#134619=CARTESIAN_POINT('Ctrl Pts',(9.99999999999996,31.9412499679373,124.482165594221));
#134620=CARTESIAN_POINT('Ctrl Pts',(9.99999999999996,31.9354125162585,124.467011522081));
#134621=CARTESIAN_POINT('Ctrl Pts',(9.99999999999998,31.9293925581285,124.451927087433));
#134622=CARTESIAN_POINT('Ctrl Pts',(10.0000000000001,31.9017664039417,124.382703197761));
#134623=CARTESIAN_POINT('Ctrl Pts',(9.99999999999996,31.870356225898,124.315080819697));
#134624=CARTESIAN_POINT('Ctrl Pts',(10.0000000000001,31.8353723366309,124.249352545652));
#134625=CARTESIAN_POINT('Ctrl Pts',(10.0000000000001,31.810811842914,124.20320790892));
#134626=CARTESIAN_POINT('Ctrl Pts',(10.,31.7844889480599,124.157997341092));
#134627=CARTESIAN_POINT('Ctrl Pts',(10.0000000000001,31.7564653772615,124.113832752978));
#134628=CARTESIAN_POINT('Ctrl Pts',(10.0000000000001,31.745815848242,124.097049307851));
#134629=CARTESIAN_POINT('Ctrl Pts',(10.,31.7349206335243,124.080417022449));
#134630=CARTESIAN_POINT('Ctrl Pts',(9.99999999999998,31.7237828414283,124.063942444803));
#134631=CARTESIAN_POINT('Ctrl Pts',(9.99999999999993,31.7131612362719,124.048231390282));
#134632=CARTESIAN_POINT('Ctrl Pts',(10.0000000000001,31.702315414293,124.032658992084));
#134633=CARTESIAN_POINT('Ctrl Pts',(10.0000000000001,31.6912678340984,124.017258102486));
#134634=CARTESIAN_POINT('Ctrl Pts',(10.0000000000001,31.648949962443,123.958264833559));
#134635=CARTESIAN_POINT('Ctrl Pts',(10.,31.6036337000859,123.901720305621));
#134636=CARTESIAN_POINT('Ctrl Pts',(10.,31.5555120295465,123.847896734174));
#134637=CARTESIAN_POINT('Ctrl Pts',(10.,31.5084230386781,123.795228203843));
#134638=CARTESIAN_POINT('Ctrl Pts',(10.0000000000001,31.4586469877109,123.745164560953));
#134639=CARTESIAN_POINT('Ctrl Pts',(10.0000000000001,31.4063360139386,123.698000619784));
#134640=CARTESIAN_POINT('Ctrl Pts',(10.0000000000001,31.3551727086319,123.65187142456));
#134641=CARTESIAN_POINT('Ctrl Pts',(9.99999999999992,31.3015838507054,123.608515661013));
#134642=CARTESIAN_POINT('Ctrl Pts',(9.99999999999988,31.2456942589875,123.568254646092));
#134643=CARTESIAN_POINT('Ctrl Pts',(9.99999999999987,31.2275284079873,123.555168567348));
#134644=CARTESIAN_POINT('Ctrl Pts',(10.0000000000001,31.2091193946461,123.542409825234));
#134645=CARTESIAN_POINT('Ctrl Pts',(10.0000000000001,31.1904712619119,123.529990635087));
#134646=CARTESIAN_POINT('Ctrl Pts',(10.0000000000001,31.179965598328,123.522994125811));
#134647=CARTESIAN_POINT('Ctrl Pts',(10.0000000000002,31.1693828915675,123.516104777863));
#134648=CARTESIAN_POINT('Ctrl Pts',(10.0000000000001,31.1587390473461,123.509334179643));
#134649=CARTESIAN_POINT('Ctrl Pts',(9.99999999999996,31.1011038925273,123.472672192814));
#134650=CARTESIAN_POINT('Ctrl Pts',(10.,31.041579032397,123.439421075485));
#134651=CARTESIAN_POINT('Ctrl Pts',(9.99999999999991,30.9803088822866,123.409847885084));
#134652=CARTESIAN_POINT('Ctrl Pts',(9.9999999999999,30.9714786041448,123.405585785247));
#134653=CARTESIAN_POINT('Ctrl Pts',(10.,30.9626120424464,123.401400160729));
#134654=CARTESIAN_POINT('Ctrl Pts',(10.,30.9537095988913,123.39729189634));
#134655=CARTESIAN_POINT('Ctrl Pts',(9.99999999999998,30.8907195264398,123.368223487207));
#134656=CARTESIAN_POINT('Ctrl Pts',(9.9999999999998,30.8259335006331,123.343023769821));
#134657=CARTESIAN_POINT('Ctrl Pts',(9.99999999999985,30.7597192517224,123.321677672926));
#134658=CARTESIAN_POINT('Ctrl Pts',(9.99999999999989,30.6979479251232,123.301763881792));
#134659=CARTESIAN_POINT('Ctrl Pts',(10.,30.6349327477613,123.285204520595));
#134660=CARTESIAN_POINT('Ctrl Pts',(10.,30.5709758239915,123.272027286914));
#134661=CARTESIAN_POINT('Ctrl Pts',(10.,30.5569222627032,123.269131790223));
#134662=CARTESIAN_POINT('Ctrl Pts',(9.99999999999973,30.5428232716055,123.26639973771));
#134663=CARTESIAN_POINT('Ctrl Pts',(9.99999999999988,30.5286821398607,123.263831663828));
#134664=CARTESIAN_POINT('Ctrl Pts',(9.99999999999999,30.5175493411139,123.261809912654));
#134665=CARTESIAN_POINT('Ctrl Pts',(10.0000000000001,30.506390968432,123.259889975947));
#134666=CARTESIAN_POINT('Ctrl Pts',(10.0000000000001,30.4952217650004,123.258074005347));
#134667=CARTESIAN_POINT('Ctrl Pts',(9.99999999999998,30.4277390447172,123.247102172233));
#134668=CARTESIAN_POINT('Ctrl Pts',(10.0000000000001,30.3597367395742,123.23989796486));
#134669=CARTESIAN_POINT('Ctrl Pts',(9.99999999999997,30.2915660703205,123.236428532288));
#134670=CARTESIAN_POINT('Ctrl Pts',(9.99999999999985,30.2237084738309,123.232975033033));
#134671=CARTESIAN_POINT('Ctrl Pts',(9.99999999999983,30.1556829478191,123.233222328895));
#134672=CARTESIAN_POINT('Ctrl Pts',(9.99999999999995,30.0878446921053,123.237188390519));
#134673=CARTESIAN_POINT('Ctrl Pts',(10.0000000000001,30.0214572536015,123.241069632296));
#134674=CARTESIAN_POINT('Ctrl Pts',(9.99999999999994,29.9552482504001,123.248512619597));
#134675=CARTESIAN_POINT('Ctrl Pts',(9.99999999999983,29.8895737838068,123.259578024576));
#134676=CARTESIAN_POINT('Ctrl Pts',(9.9999999999998,29.8704842081868,123.262794402205));
#134677=CARTESIAN_POINT('Ctrl Pts',(10.0000000000001,29.8514399947749,123.266317103788));
#134678=CARTESIAN_POINT('Ctrl Pts',(10.0000000000001,29.8324504331394,123.270148273509));
#134679=CARTESIAN_POINT('Ctrl Pts',(10.0000000000002,29.821877140126,123.272281449662));
#134680=CARTESIAN_POINT('Ctrl Pts',(9.99999999999979,29.8113302806734,123.274508350105));
#134681=CARTESIAN_POINT('Ctrl Pts',(9.9999999999998,29.8008115170796,123.276828838321));
#134682=CARTESIAN_POINT('Ctrl Pts',(9.99999999999982,29.7370705081107,123.29089040163));
#134683=CARTESIAN_POINT('Ctrl Pts',(9.9999999999999,29.6743561255583,123.308385480754));
#134684=CARTESIAN_POINT('Ctrl Pts',(9.9999999999999,29.6129879890306,123.329323310669));
#134685=CARTESIAN_POINT('Ctrl Pts',(9.99999999999991,29.5501643704022,123.350757727875));
#134686=CARTESIAN_POINT('Ctrl Pts',(10.0000000000001,29.4887504504911,123.375800193779));
#134687=CARTESIAN_POINT('Ctrl Pts',(10.0000000000002,29.4291213825965,123.404508661191));
#134688=CARTESIAN_POINT('Ctrl Pts',(10.0000000000002,29.3738779432933,123.431105663844));
#134689=CARTESIAN_POINT('Ctrl Pts',(10.0000000000001,29.3201661528932,123.460849885524));
#134690=CARTESIAN_POINT('Ctrl Pts',(10.0000000000002,29.2683211125717,123.493821880151));
#134691=CARTESIAN_POINT('Ctrl Pts',(10.0000000000002,29.2642052737676,123.496439438438));
#134692=CARTESIAN_POINT('Ctrl Pts',(10.0000000000001,29.260101221769,123.499077355755));
#134693=CARTESIAN_POINT('Ctrl Pts',(10.0000000000002,29.2560091359247,123.501735680849));
#134694=CARTESIAN_POINT('Ctrl Pts',(10.0000000000003,29.2468933389776,123.507657538966));
#134695=CARTESIAN_POINT('Ctrl Pts',(10.,29.2378369215811,123.513680670008));
#134696=CARTESIAN_POINT('Ctrl Pts',(10.,29.2288409619357,123.519803760817));
#134697=CARTESIAN_POINT('Ctrl Pts',(-2.78639958328775E-16,28.7309291201476,
126.079358653049));
#134698=CARTESIAN_POINT('Ctrl Pts',(2.43951905577452E-13,28.6856045121037,
126.037075604188));
#134699=CARTESIAN_POINT('Ctrl Pts',(2.32264696777501E-14,28.6430101816999,
125.992223094823));
#134700=CARTESIAN_POINT('Ctrl Pts',(-1.23824561715224E-14,28.6031444611115,
125.945146237493));
#134701=CARTESIAN_POINT('Ctrl Pts',(-5.0440039678236E-14,28.5606416816283,
125.894955315159));
#134702=CARTESIAN_POINT('Ctrl Pts',(-1.53712585429092E-14,28.5212397133509,
125.842235804835));
#134703=CARTESIAN_POINT('Ctrl Pts',(-5.82867087928207E-16,28.4849653865329,
125.787351197263));
#134704=CARTESIAN_POINT('Ctrl Pts',(1.27498972438004E-14,28.4532253505671,
125.739327165638));
#134705=CARTESIAN_POINT('Ctrl Pts',(7.95844567888735E-14,28.4238801589872,
125.689644255155));
#134706=CARTESIAN_POINT('Ctrl Pts',(-1.85268467234323E-14,28.396970688999,
125.638518410175));
#134707=CARTESIAN_POINT('Ctrl Pts',(-6.76177436159774E-14,28.383472104572,
125.612872177263));
#134708=CARTESIAN_POINT('Ctrl Pts',(5.0431355625446E-14,28.3705867868154,
125.586862499757));
#134709=CARTESIAN_POINT('Ctrl Pts',(5.70862801474448E-14,28.3583222370606,
125.560514794078));
#134710=CARTESIAN_POINT('Ctrl Pts',(6.02689641839324E-14,28.3527132731747,
125.548465160574));
#134711=CARTESIAN_POINT('Ctrl Pts',(3.48561988117052E-14,28.3472335647089,
125.536343140102));
#134712=CARTESIAN_POINT('Ctrl Pts',(3.5978164891759E-14,28.3418923437833,
125.524171131458));
#134713=CARTESIAN_POINT('Ctrl Pts',(4.15921821842815E-14,28.3149790658411,
125.46283896484));
#134714=CARTESIAN_POINT('Ctrl Pts',(5.59872842514893E-14,28.2915266892741,
125.400131282304));
#134715=CARTESIAN_POINT('Ctrl Pts',(-1.64451785522601E-15,28.2715585090975,
125.336405988326));
#134716=CARTESIAN_POINT('Ctrl Pts',(-6.05299641908085E-14,28.2511803715366,
125.27137238009));
#134717=CARTESIAN_POINT('Ctrl Pts',(-1.51360821367708E-14,28.2344303837891,
125.205278113985));
#134718=CARTESIAN_POINT('Ctrl Pts',(-2.14273043752655E-14,28.2213730031473,
125.138466741869));
#134719=CARTESIAN_POINT('Ctrl Pts',(-2.6658648028734E-14,28.2105153918976,
125.082911043112));
#134720=CARTESIAN_POINT('Ctrl Pts',(6.74653547581201E-15,28.202211586376,
125.026858558113));
#134721=CARTESIAN_POINT('Ctrl Pts',(7.89646126264643E-15,28.196523242066,
124.970494651124));
#134722=CARTESIAN_POINT('Ctrl Pts',(8.51570007836861E-15,28.1938947698915,
124.944449996811));
#134723=CARTESIAN_POINT('Ctrl Pts',(-8.72662611035027E-15,28.1918250788729,
124.918338736059));
#134724=CARTESIAN_POINT('Ctrl Pts',(3.3584246494911E-15,28.1903220501733,
124.892178757629));
#134725=CARTESIAN_POINT('Ctrl Pts',(8.48608315006128E-15,28.1896651687426,
124.880745839508));
#134726=CARTESIAN_POINT('Ctrl Pts',(-2.44137855573384E-14,28.1891166383197,
124.86930381891));
#134727=CARTESIAN_POINT('Ctrl Pts',(-2.27873275804313E-14,28.1886774510598,
124.857868328144));
#134728=CARTESIAN_POINT('Ctrl Pts',(-1.28244564203572E-14,28.1859840496925,
124.787737954891));
#134729=CARTESIAN_POINT('Ctrl Pts',(-2.61029113609051E-14,28.1873908986415,
124.717721796522));
#134730=CARTESIAN_POINT('Ctrl Pts',(1.55431223447522E-15,28.1929524150393,
124.648180880013));
#134731=CARTESIAN_POINT('Ctrl Pts',(2.62922359085441E-14,28.1979245136766,
124.586010013027));
#134732=CARTESIAN_POINT('Ctrl Pts',(-1.89380643560603E-14,28.2062176594135,
124.524218028094));
#134733=CARTESIAN_POINT('Ctrl Pts',(5.73152636462737E-15,28.2179038679988,
124.463050764826));
#134734=CARTESIAN_POINT('Ctrl Pts',(3.25218004191036E-14,28.2306365799094,
124.396405955617));
#134735=CARTESIAN_POINT('Ctrl Pts',(-4.75594221305812E-14,28.2473961773284,
124.330501931656));
#134736=CARTESIAN_POINT('Ctrl Pts',(3.12527781431982E-14,28.267937556801,
124.265552134843));
#134737=CARTESIAN_POINT('Ctrl Pts',(6.17662707231035E-14,28.2758645232437,
124.240487856152));
#134738=CARTESIAN_POINT('Ctrl Pts',(-4.83646106192593E-14,28.2843552288597,
124.215565728878));
#134739=CARTESIAN_POINT('Ctrl Pts',(-8.82627304576999E-15,28.2933975953373,
124.190798339915));
#134740=CARTESIAN_POINT('Ctrl Pts',(8.52941477985801E-15,28.2973639657865,
124.179934298967));
#134741=CARTESIAN_POINT('Ctrl Pts',(-9.62032087635259E-15,28.3014363742385,
124.169100609291));
#134742=CARTESIAN_POINT('Ctrl Pts',(-2.72004641033163E-15,28.3056087226356,
124.158310852064));
#134743=CARTESIAN_POINT('Ctrl Pts',(3.85734597192918E-14,28.3308312619704,
124.093084976808));
#134744=CARTESIAN_POINT('Ctrl Pts',(6.02936583413694E-14,28.3597443603586,
124.029345353138));
#134745=CARTESIAN_POINT('Ctrl Pts',(9.81992265280951E-14,28.3920354848392,
123.967310636409));
#134746=CARTESIAN_POINT('Ctrl Pts',(1.37087657368489E-13,28.4250737751078,
123.90384053399));
#134747=CARTESIAN_POINT('Ctrl Pts',(1.3210876930124E-13,28.461648526632,
123.84215432989));
#134748=CARTESIAN_POINT('Ctrl Pts',(1.9595436384634E-14,28.5014811380923,
123.782489939349));
#134749=CARTESIAN_POINT('Ctrl Pts',(-6.6418823366357E-14,28.5319599761612,
123.736836359754));
#134750=CARTESIAN_POINT('Ctrl Pts',(3.98228911114656E-15,28.5643474730915,
123.692366499728));
#134751=CARTESIAN_POINT('Ctrl Pts',(8.70137295549966E-14,28.5985383356841,
123.649193044353));
#134752=CARTESIAN_POINT('Ctrl Pts',(1.38648056659717E-13,28.619824456337,
123.622314653156));
#134753=CARTESIAN_POINT('Ctrl Pts',(1.22190750202126E-13,28.6418098672274,
123.595938858562));
#134754=CARTESIAN_POINT('Ctrl Pts',(1.34087185799103E-13,28.6644720642652,
123.570094538783));
#134755=CARTESIAN_POINT('Ctrl Pts',(1.40798623008578E-13,28.6771664952139,
123.555617613518));
#134756=CARTESIAN_POINT('Ctrl Pts',(3.97015826307881E-14,28.6900777714248,
123.541302901776));
#134757=CARTESIAN_POINT('Ctrl Pts',(1.19348975147204E-14,28.7031781914608,
123.527180952641));
#134758=CARTESIAN_POINT('Ctrl Pts',(-9.64246718465023E-14,28.7540452177212,
123.472347477413));
#134759=CARTESIAN_POINT('Ctrl Pts',(-6.96814581978678E-14,28.8078087436982,
123.420359024874));
#134760=CARTESIAN_POINT('Ctrl Pts',(-7.75213226944516E-14,28.864184000068,
123.371479324179));
#134761=CARTESIAN_POINT('Ctrl Pts',(-8.33770163543804E-14,28.9063445726748,
123.334924347707));
#134762=CARTESIAN_POINT('Ctrl Pts',(1.58152049026456E-13,28.9499670126063,
123.300108259198));
#134763=CARTESIAN_POINT('Ctrl Pts',(-9.90596493721796E-14,28.9949486028232,
123.267151117223));
#134764=CARTESIAN_POINT('Ctrl Pts',(-1.7947882528363E-13,29.0089990364185,
123.256856636024));
#134765=CARTESIAN_POINT('Ctrl Pts',(1.56627630403963E-13,29.0231821727827,
123.246743606353));
#134766=CARTESIAN_POINT('Ctrl Pts',(3.36675132217579E-14,29.0374951222103,
123.236815913378));
#134767=CARTESIAN_POINT('Ctrl Pts',(-8.47289291612157E-14,29.0512877290505,
123.227249138428));
#134768=CARTESIAN_POINT('Ctrl Pts',(5.31593884409529E-14,29.0651938482479,
123.217859411298));
#134769=CARTESIAN_POINT('Ctrl Pts',(1.44884104713583E-14,29.0792055012066,
123.208652961744));
#134770=CARTESIAN_POINT('Ctrl Pts',(-1.59719470102946E-13,29.1421550047024,
123.167291572758));
#134771=CARTESIAN_POINT('Ctrl Pts',(-3.90017336220626E-14,29.2072623202427,
123.129605449444));
#134772=CARTESIAN_POINT('Ctrl Pts',(-9.32032229172819E-14,29.2742663398359,
123.095873566138));
#134773=CARTESIAN_POINT('Ctrl Pts',(-1.34974257368109E-13,29.3255152870948,
123.070073270588));
#134774=CARTESIAN_POINT('Ctrl Pts',(-1.96225293566553E-13,29.3778748117198,
123.046586677912));
#134775=CARTESIAN_POINT('Ctrl Pts',(-2.60125254669674E-13,29.4312419689629,
123.025553895645));
#134776=CARTESIAN_POINT('Ctrl Pts',(-2.74819563164584E-13,29.4435211852116,
123.020714475764));
#134777=CARTESIAN_POINT('Ctrl Pts',(-1.97358671919277E-13,29.4558537898234,
123.016005028946));
#134778=CARTESIAN_POINT('Ctrl Pts',(-5.10702591327572E-15,29.468237921027,
123.011424990249));
#134779=CARTESIAN_POINT('Ctrl Pts',(10.,29.2076925604819,123.534460876918));
#134780=CARTESIAN_POINT('Ctrl Pts',(10.0002900099995,29.215135678433,123.530436939492));
#134781=CARTESIAN_POINT('Ctrl Pts',(10.0005800199989,29.2226094518746,123.526469705855));
#134782=CARTESIAN_POINT('Ctrl Pts',(10.0008700299984,29.230113013341,123.522559636475));
#134783=CARTESIAN_POINT('Ctrl Pts',(0.00155432571019262,30.5308648559221,
123.01222466255));
#134784=CARTESIAN_POINT('Ctrl Pts',(0.0385994159897124,31.1918318661709,
123.188745695915));
#134785=CARTESIAN_POINT('Ctrl Pts',(0.112689596548752,32.3122910244663,
124.250671109051));
#134786=CARTESIAN_POINT('Ctrl Pts',(0.223824867387312,31.8837750190762,
126.540127999121));
#134787=CARTESIAN_POINT('Ctrl Pts',(0.334960138225871,29.72768122948,127.416072798206));
#134788=CARTESIAN_POINT('Ctrl Pts',(0.44609540906443,27.8224997759096,126.082528680968));
#134789=CARTESIAN_POINT('Ctrl Pts',(0.55723067990299,27.9095008630876,123.757255622762));
#134790=CARTESIAN_POINT('Ctrl Pts',(0.66836595074155,29.9102827683814,122.569885979054));
#134791=CARTESIAN_POINT('Ctrl Pts',(0.779501221580109,31.9929799341018,
123.606506840134));
#134792=CARTESIAN_POINT('Ctrl Pts',(0.890636492418669,32.251657659651,125.918663536734));
#134793=CARTESIAN_POINT('Ctrl Pts',(1.00177176325722,30.4494077016117,127.389938666344));
#134794=CARTESIAN_POINT('Ctrl Pts',(1.11290703409579,28.2358516598168,126.673797276444));
#134795=CARTESIAN_POINT('Ctrl Pts',(1.22404230493434,27.6369589836974,124.425663052317));
#134796=CARTESIAN_POINT('Ctrl Pts',(1.3351775757729,29.2008970629833,122.703209843518));
#134797=CARTESIAN_POINT('Ctrl Pts',(1.44631284661146,31.4962286446548,123.082940710024));
#134798=CARTESIAN_POINT('Ctrl Pts',(1.55744811745002,32.422105732079,125.217303545347));
#134799=CARTESIAN_POINT('Ctrl Pts',(1.66858338828858,31.1310969676118,127.152773774276));
#134800=CARTESIAN_POINT('Ctrl Pts',(1.77971865912714,28.8048273623399,127.117871204668));
#134801=CARTESIAN_POINT('Ctrl Pts',(1.8908539299657,27.5724654306094,125.144540590365));
#134802=CARTESIAN_POINT('Ctrl Pts',(2.00198920080426,28.5619575897349,123.038916141001));
#134803=CARTESIAN_POINT('Ctrl Pts',(2.11312447164282,30.8676494139743,122.728216455201));
#134804=CARTESIAN_POINT('Ctrl Pts',(2.22425974248138,32.3792061928279,124.496816273114));
#134805=CARTESIAN_POINT('Ctrl Pts',(2.33539501331994,31.7131425574306,126.725965969629));
#134806=CARTESIAN_POINT('Ctrl Pts',(2.4465302841585,29.4790878050011,127.37538764178));
#134807=CARTESIAN_POINT('Ctrl Pts',(2.55766555499706,27.7218093076021,125.850683919345));
#134808=CARTESIAN_POINT('Ctrl Pts',(2.66880082583561,28.0496945735768,123.547373171422));
#134809=CARTESIAN_POINT('Ctrl Pts',(2.77993609667418,30.1626394539462,122.573610837253));
#134810=CARTESIAN_POINT('Ctrl Pts',(2.89107136751274,32.1267250241147,123.82065415059));
#134811=CARTESIAN_POINT('Ctrl Pts',(3.00220663835129,32.1442790912563,126.147119496527));
#134812=CARTESIAN_POINT('Ctrl Pts',(3.11334190918986,30.1992349124517,127.42365868273));
#134813=CARTESIAN_POINT('Ctrl Pts',(3.22447718002841,28.0718366308647,126.481891353163));
#134814=CARTESIAN_POINT('Ctrl Pts',(3.33561245086697,27.7092319630256,124.183790614235));
#134815=CARTESIAN_POINT('Ctrl Pts',(3.44674772170553,29.443302746492,122.632743332759));
#134816=CARTESIAN_POINT('Ctrl Pts',(3.55788299254409,31.6869028434527,123.248379391135));
#134817=CARTESIAN_POINT('Ctrl Pts',(3.66901826338265,32.3865282893196,125.467224448126));
#134818=CARTESIAN_POINT('Ctrl Pts',(3.78015353422121,30.9018316225513,127.258432129867));
#134819=CARTESIAN_POINT('Ctrl Pts',(3.89128880505977,28.5917138770426,126.982560505139));
#134820=CARTESIAN_POINT('Ctrl Pts',(4.00242407589833,27.5705607472319,124.89210710051));
#134821=CARTESIAN_POINT('Ctrl Pts',(4.11355934673689,28.7730049260626,122.900405027348));
#134822=CARTESIAN_POINT('Ctrl Pts',(4.22469461757545,31.0984831305496,122.830403085237));
#134823=CARTESIAN_POINT('Ctrl Pts',(4.33582988841401,32.41855067087,124.746172079776));
#134824=CARTESIAN_POINT('Ctrl Pts',(4.44696515925257,31.5249869148193,126.894262619143));
#134825=CARTESIAN_POINT('Ctrl Pts',(4.55810043009113,29.2356455958426,127.308587946233));
#134826=CARTESIAN_POINT('Ctrl Pts',(4.6692357009297,27.6458963304626,125.609927761068));
#134827=CARTESIAN_POINT('Ctrl Pts',(4.78037097176824,28.210791836662,123.353017878392));
#134828=CARTESIAN_POINT('Ctrl Pts',(4.89150624260681,30.4132991712142,122.603544334705));
#134829=CARTESIAN_POINT('Ctrl Pts',(5.00264151344537,32.2375254173512,124.047479151221));
#134830=CARTESIAN_POINT('Ctrl Pts',(5.11377678428393,32.0138076820242,126.363229467284));
#134831=CARTESIAN_POINT('Ctrl Pts',(5.22491205512248,29.9469085060545,127.431254255301));
#134832=CARTESIAN_POINT('Ctrl Pts',(5.33604732596105,27.9286024788597,126.274020513989));
#134833=CARTESIAN_POINT('Ctrl Pts',(5.44718259679961,27.8061882496944,123.950711686488));
#134834=CARTESIAN_POINT('Ctrl Pts',(5.55831786763816,29.6917081139984,122.587786892981));
#134835=CARTESIAN_POINT('Ctrl Pts',(5.66945313847672,31.8593988567091,123.432692802186));
#134836=CARTESIAN_POINT('Ctrl Pts',(5.78058840931528,32.3252342067572,125.712110837143));
#134837=CARTESIAN_POINT('Ctrl Pts',(5.89172368015384,30.6628481912308,127.339753883645));
#134838=CARTESIAN_POINT('Ctrl Pts',(6.00285895099241,28.3937758992811,126.825886113349));
#134839=CARTESIAN_POINT('Ctrl Pts',(6.11399422183096,27.5948352779891,124.640836220304));
#134840=CARTESIAN_POINT('Ctrl Pts',(6.22512949266952,28.9972741711713,122.784518816859));
#134841=CARTESIAN_POINT('Ctrl Pts',(6.33626476350808,31.3174797678214,122.95596892831));
#134842=CARTESIAN_POINT('Ctrl Pts',(6.44740003434664,32.431833247536,124.998263097546));
#134843=CARTESIAN_POINT('Ctrl Pts',(6.55853530518519,31.3203982626383,127.042147004667));
#134844=CARTESIAN_POINT('Ctrl Pts',(6.66967057602377,29.0004399447169,127.216911287475));
#134845=CARTESIAN_POINT('Ctrl Pts',(6.78080584686232,27.5953507869168,125.362599121175));
#134846=CARTESIAN_POINT('Ctrl Pts',(6.89194111770087,28.3911693127978,123.176410193999));
#134847=CARTESIAN_POINT('Ctrl Pts',(7.00307638853944,30.6595052445024,122.65930164414));
#134848=CARTESIAN_POINT('Ctrl Pts',(7.11421165937799,32.3242146047758,124.2845683599));
#134849=CARTESIAN_POINT('Ctrl Pts',(7.22534693021657,31.8616358123939,126.564649501493));
#134850=CARTESIAN_POINT('Ctrl Pts',(7.33648220105513,29.6951542049319,127.412651031946));
#134851=CARTESIAN_POINT('Ctrl Pts',(7.44761747189367,27.8076893657145,126.05242103926));
#134852=CARTESIAN_POINT('Ctrl Pts',(7.55875274273224,27.9267846911862,123.728939717111));
#134853=CARTESIAN_POINT('Ctrl Pts',(7.66988801357079,29.9434355836753,122.568824064703));
#134854=CARTESIAN_POINT('Ctrl Pts',(7.78102328440936,32.0118582947014,123.633895258166));
#134855=CARTESIAN_POINT('Ctrl Pts',(7.89215855524792,32.2388837808543,125.949323636188));
#134856=CARTESIAN_POINT('Ctrl Pts',(8.00329382608648,30.4167220208466,127.395862835877));
#134857=CARTESIAN_POINT('Ctrl Pts',(8.11442909692502,28.2131463200964,126.649536270169));
#134858=CARTESIAN_POINT('Ctrl Pts',(8.2255643677636,27.6450274846715,124.393435635898));
#134859=CARTESIAN_POINT('Ctrl Pts',(8.33669963860214,29.2323485914987,122.692506255073));
#134860=CARTESIAN_POINT('Ctrl Pts',(8.44783490944072,31.5222795274243,123.103560938559));
#134861=CARTESIAN_POINT('Ctrl Pts',(8.55897018027927,32.4189106521937,125.250372782172));
#134862=CARTESIAN_POINT('Ctrl Pts',(8.67010545111782,31.1015814932564,127.168025650657));
#134863=CARTESIAN_POINT('Ctrl Pts',(8.7812407219564,28.7760048267531,127.101345353396));
#134864=CARTESIAN_POINT('Ctrl Pts',(8.89237599279495,27.5707184851016,125.111363585784));
#134865=CARTESIAN_POINT('Ctrl Pts',(9.00351126363351,28.5888809804667,123.019452377014));
#134866=CARTESIAN_POINT('Ctrl Pts',(9.11464653447208,30.8986092624814,122.740283627933));
#134867=CARTESIAN_POINT('Ctrl Pts',(9.22578180531062,32.3858489908478,124.529363511801));
#134868=CARTESIAN_POINT('Ctrl Pts',(9.3369170761492,31.6894223937398,126.749216077424));
#134869=CARTESIAN_POINT('Ctrl Pts',(9.44805234698775,29.4466461250334,127.368035407967));
#134870=CARTESIAN_POINT('Ctrl Pts',(9.55918761782632,27.7104787022057,125.819509343078));
#134871=CARTESIAN_POINT('Ctrl Pts',(9.67032288866486,28.0695628376466,123.520806777059));
#134872=CARTESIAN_POINT('Ctrl Pts',(9.78145815950342,30.1960944686997,122.576176052107));
#134873=CARTESIAN_POINT('Ctrl Pts',(9.89259343034199,32.1419859270096,123.849582003139));
#134874=CARTESIAN_POINT('Ctrl Pts',(10.0037287011806,32.1297374742994,126.176784120702));
#134875=CARTESIAN_POINT('Ctrl Pts',(10.1148770421612,30.1631027296072,127.425328374009));
#134876=CARTESIAN_POINT('Ctrl Pts',(10.1889802928623,28.7606569526153,126.779199041105));
#134877=CARTESIAN_POINT('Ctrl Pts',(10.2260384532841,28.3512768063378,126.230764021361));
#134878=CARTESIAN_POINT('Ctrl Pts',(-0.0743653418493182,30.4969358400317,
123.139268787356));
#134879=CARTESIAN_POINT('Ctrl Pts',(-0.0373202515697984,31.1156586520752,
123.304507881675));
#134880=CARTESIAN_POINT('Ctrl Pts',(0.0367699289892414,32.164506220034,
124.298562755228));
#134881=CARTESIAN_POINT('Ctrl Pts',(0.147905199827801,31.7633778373016,
126.441694232461));
#134882=CARTESIAN_POINT('Ctrl Pts',(0.25904047066636,29.7450858622959,127.261655018524));
#134883=CARTESIAN_POINT('Ctrl Pts',(0.37017574150492,27.9616697339138,126.013341330537));
#134884=CARTESIAN_POINT('Ctrl Pts',(0.481311012343479,28.0431103451318,
123.836682793825));
#134885=CARTESIAN_POINT('Ctrl Pts',(0.59244628318204,29.9160168405154,122.725201171447));
#134886=CARTESIAN_POINT('Ctrl Pts',(0.703581554020597,31.8656031693769,
123.695568775648));
#134887=CARTESIAN_POINT('Ctrl Pts',(0.814716824859158,32.1077480983721,
125.859949253074));
#134888=CARTESIAN_POINT('Ctrl Pts',(0.925852095697717,30.4206848338627,
127.237191190064));
#134889=CARTESIAN_POINT('Ctrl Pts',(1.03698736653628,28.348603175385,126.566820342944));
#134890=CARTESIAN_POINT('Ctrl Pts',(1.14812263737483,27.7879873580519,124.462370487754));
#134891=CARTESIAN_POINT('Ctrl Pts',(1.25925790821339,29.2519699037367,122.850003945343));
#134892=CARTESIAN_POINT('Ctrl Pts',(1.37039317905195,31.4006006050627,123.205465180021));
#134893=CARTESIAN_POINT('Ctrl Pts',(1.48152844989051,32.2673023711948,125.203415085109));
#134894=CARTESIAN_POINT('Ctrl Pts',(1.59266372072907,31.0588054859671,127.015184150888));
#134895=CARTESIAN_POINT('Ctrl Pts',(1.70379899156763,28.881214094222,126.982512299373));
#134896=CARTESIAN_POINT('Ctrl Pts',(1.81493426240619,27.7276157632423,125.135302608358));
#134897=CARTESIAN_POINT('Ctrl Pts',(1.92606953324475,28.6538667889307,123.164254340868));
#134898=CARTESIAN_POINT('Ctrl Pts',(2.03720480408331,30.8121955815617,122.873412316505));
#134899=CARTESIAN_POINT('Ctrl Pts',(2.14834007492187,32.2271446581029,124.528976112807));
#134900=CARTESIAN_POINT('Ctrl Pts',(2.25947534576043,31.6036509600772,126.615654793147));
#134901=CARTESIAN_POINT('Ctrl Pts',(2.37061061659899,29.5123807192795,127.223570161032));
#134902=CARTESIAN_POINT('Ctrl Pts',(2.48174588743755,27.8674146671234,125.796314397807));
#134903=CARTESIAN_POINT('Ctrl Pts',(2.59288115827611,28.1743438945219,123.640214500434));
#134904=CARTESIAN_POINT('Ctrl Pts',(2.70401642911466,30.1522447243727,122.728687963833));
#134905=CARTESIAN_POINT('Ctrl Pts',(2.81515169995323,31.9908002471535,123.896029349415));
#134906=CARTESIAN_POINT('Ctrl Pts',(2.92628697079178,32.0072323861502,126.073803971508));
#134907=CARTESIAN_POINT('Ctrl Pts',(3.03742224163035,30.1865012676549,127.268756068548));
#134908=CARTESIAN_POINT('Ctrl Pts',(3.1485575124689,28.195070792744,126.38717964884));
#134909=CARTESIAN_POINT('Ctrl Pts',(3.25969278330746,27.8556411748254,124.235956774625));
#134910=CARTESIAN_POINT('Ctrl Pts',(3.37082805414602,29.4788827811274,122.784041140824));
#134911=CARTESIAN_POINT('Ctrl Pts',(3.48196332498458,31.5790882975421,123.360330225342));
#134912=CARTESIAN_POINT('Ctrl Pts',(3.59309859582314,32.2339987795056,125.437362863679));
#134913=CARTESIAN_POINT('Ctrl Pts',(3.7042338666617,30.8441931122775,127.114089593783));
#134914=CARTESIAN_POINT('Ctrl Pts',(3.81536913750026,28.6817212710357,126.85584967444));
#134915=CARTESIAN_POINT('Ctrl Pts',(3.92650440833882,27.7258328133566,124.899002828982));
#134916=CARTESIAN_POINT('Ctrl Pts',(4.03763967917738,28.8514255163441,123.034595848978));
#134917=CARTESIAN_POINT('Ctrl Pts',(4.14877495001594,31.0282760878795,122.96906792126));
#134918=CARTESIAN_POINT('Ctrl Pts',(4.2599102208545,32.2639745236107,124.76239491209));
#134919=CARTESIAN_POINT('Ctrl Pts',(4.37104549169305,31.4275208560128,126.773195146342));
#134920=CARTESIAN_POINT('Ctrl Pts',(4.48218076253162,29.2844975634107,127.161039815597));
#134921=CARTESIAN_POINT('Ctrl Pts',(4.59331603337017,27.7963534946927,125.570945620008));
#134922=CARTESIAN_POINT('Ctrl Pts',(4.70445130420873,28.3251449936434,123.45828098246));
#134923=CARTESIAN_POINT('Ctrl Pts',(4.8155865750473,30.3868840977898,122.756708330102));
#134924=CARTESIAN_POINT('Ctrl Pts',(4.92672184588585,32.0945190860907,124.108357347723));
#134925=CARTESIAN_POINT('Ctrl Pts',(5.03785711672442,31.8850997593176,126.276101766624));
#134926=CARTESIAN_POINT('Ctrl Pts',(5.14899238756297,29.950301727741,127.275866187431));
#134927=CARTESIAN_POINT('Ctrl Pts',(5.26012765840153,28.0609911247196,126.192594400014));
#134928=CARTESIAN_POINT('Ctrl Pts',(5.3712629292401,27.9464007216756,124.017774554685));
#134929=CARTESIAN_POINT('Ctrl Pts',(5.48239820007865,29.7114118864037,122.741957989307));
#134930=CARTESIAN_POINT('Ctrl Pts',(5.59353347091722,31.7405596217284,123.532863665309));
#134931=CARTESIAN_POINT('Ctrl Pts',(5.70466874175577,32.1766221683637,125.666597897947));
#134932=CARTESIAN_POINT('Ctrl Pts',(5.81580401259433,30.6204837616357,127.190213853235));
#134933=CARTESIAN_POINT('Ctrl Pts',(5.9269392834329,28.4964340474499,126.709188768887));
#134934=CARTESIAN_POINT('Ctrl Pts',(6.03807455427144,27.7485558928723,124.66379135371));
#134935=CARTESIAN_POINT('Ctrl Pts',(6.14920982511002,29.0613611044097,122.926116241192));
#134936=CARTESIAN_POINT('Ctrl Pts',(6.26034509594857,31.2332760548066,123.086608510001));
#134937=CARTESIAN_POINT('Ctrl Pts',(6.37148036678712,32.2764081746986,124.998374107703));
#134938=CARTESIAN_POINT('Ctrl Pts',(6.4826156376257,31.2360080206869,126.911627838821));
#134939=CARTESIAN_POINT('Ctrl Pts',(6.59375090846424,29.0643245447631,127.075222461286));
#134940=CARTESIAN_POINT('Ctrl Pts',(6.70488617930281,27.7490384542232,125.339424425757));
#134941=CARTESIAN_POINT('Ctrl Pts',(6.81602145014137,28.4939940549937,123.292960775216));
#134942=CARTESIAN_POINT('Ctrl Pts',(6.92715672097993,30.6173544717193,122.808902038335));
#134943=CARTESIAN_POINT('Ctrl Pts',(7.03829199181848,32.1756677319163,124.330293540639));
#134944=CARTESIAN_POINT('Ctrl Pts',(7.14942726265705,31.7426536074951,126.464648498966));
#134945=CARTESIAN_POINT('Ctrl Pts',(7.2605625334956,29.7146377282987,127.258451946646));
#134946=CARTESIAN_POINT('Ctrl Pts',(7.37169780433417,27.9478058972905,125.985157950046));
#134947=CARTESIAN_POINT('Ctrl Pts',(7.48283307517272,28.0592895167973,123.81017663467));
#134948=CARTESIAN_POINT('Ctrl Pts',(7.59396834601129,29.9470507692709,122.724207126928));
#134949=CARTESIAN_POINT('Ctrl Pts',(7.70510361684984,31.8832749626372,123.721206725438));
#134950=CARTESIAN_POINT('Ctrl Pts',(7.8162388876884,32.0957906328901,125.888649782234));
#134951=CARTESIAN_POINT('Ctrl Pts',(7.92737415852696,30.3900881837985,127.24273672982));
#134952=CARTESIAN_POINT('Ctrl Pts',(8.03850942936553,28.3273489956417,126.544109923524));
#134953=CARTESIAN_POINT('Ctrl Pts',(8.14964470020408,27.7955401791978,124.432202813116));
#134954=CARTESIAN_POINT('Ctrl Pts',(8.26077997104264,29.281411279576,122.839984452331));
#134955=CARTESIAN_POINT('Ctrl Pts',(8.37191524188121,31.4249865051052,123.224767513704));
#134956=CARTESIAN_POINT('Ctrl Pts',(8.48305051271975,32.2643114975497,125.234370777121));
#134957=CARTESIAN_POINT('Ctrl Pts',(8.59418578355832,31.031176425804,127.029461238393));
#134958=CARTESIAN_POINT('Ctrl Pts',(8.70532105439688,28.8542336852274,126.967042660175));
#134959=CARTESIAN_POINT('Ctrl Pts',(8.81645632523543,27.7259804697702,125.104246036319));
#134960=CARTESIAN_POINT('Ctrl Pts',(8.927591596074,28.6790694325801,123.146034558943));
#134961=CARTESIAN_POINT('Ctrl Pts',(9.03872686691255,30.8411767019984,122.884708243426));
#134962=CARTESIAN_POINT('Ctrl Pts',(9.14986213775112,32.2333628968455,124.559443169003));
#134963=CARTESIAN_POINT('Ctrl Pts',(9.26099740858968,31.581446816522,126.637418923356));
#134964=CARTESIAN_POINT('Ctrl Pts',(9.37213267942823,29.4820124752587,127.216687828466));
#134965=CARTESIAN_POINT('Ctrl Pts',(9.48326795026681,27.8568082315158,125.767132273447));
#134966=CARTESIAN_POINT('Ctrl Pts',(9.59440322110534,28.1929423238309,123.615346036546));
#134967=CARTESIAN_POINT('Ctrl Pts',(9.70553849194393,30.1835615381989,122.731089228834));
#134968=CARTESIAN_POINT('Ctrl Pts',(9.81667376278246,32.0050857842635,123.92310834428));
#134969=CARTESIAN_POINT('Ctrl Pts',(9.92780903362104,31.9936201634588,126.10157264892));
#134970=CARTESIAN_POINT('Ctrl Pts',(10.0389573746017,30.152678390827,127.270319045319));
#134971=CARTESIAN_POINT('Ctrl Pts',(10.1130606253029,28.839866735443,126.665485594332));
#134972=CARTESIAN_POINT('Ctrl Pts',(10.1501187857246,28.4566511870538,126.152102547405));
#134973=CARTESIAN_POINT('Ctrl Pts',(-0.150285009408829,30.4630068241413,
123.266312912162));
#134974=CARTESIAN_POINT('Ctrl Pts',(-0.113239919129309,31.0394854379795,
123.420270067436));
#134975=CARTESIAN_POINT('Ctrl Pts',(-0.0391497385702692,32.0167214156017,
124.346454401407));
#134976=CARTESIAN_POINT('Ctrl Pts',(0.07198553226829,31.6429806555269,126.343260465802));
#134977=CARTESIAN_POINT('Ctrl Pts',(0.183120803106849,29.7624904951118,
127.107237238841));
#134978=CARTESIAN_POINT('Ctrl Pts',(0.294256073945408,28.100839691918,125.944153980106));
#134979=CARTESIAN_POINT('Ctrl Pts',(0.405391344783969,28.1767198271761,
123.91610996489));
#134980=CARTESIAN_POINT('Ctrl Pts',(0.516526615622528,29.9217509126493,
122.88051636384));
#134981=CARTESIAN_POINT('Ctrl Pts',(0.627661886461087,31.7382264046522,
123.78463071116));
#134982=CARTESIAN_POINT('Ctrl Pts',(0.738797157299648,31.9638385370933,
125.801234969414));
#134983=CARTESIAN_POINT('Ctrl Pts',(0.849932428138205,30.3919619661137,
127.084443713786));
#134984=CARTESIAN_POINT('Ctrl Pts',(0.961067698976766,28.4613546909533,
126.459843409443));
#134985=CARTESIAN_POINT('Ctrl Pts',(1.07220296981532,27.9390157324064,124.49907792319));
#134986=CARTESIAN_POINT('Ctrl Pts',(1.18333824065389,29.3030427444903,122.99679804717));
#134987=CARTESIAN_POINT('Ctrl Pts',(1.29447351149244,31.3049725654706,123.32798965002));
#134988=CARTESIAN_POINT('Ctrl Pts',(1.405608782331,32.1124990103107,125.189526624871));
#134989=CARTESIAN_POINT('Ctrl Pts',(1.51674405316956,30.9865140043224,126.8775945275));
#134990=CARTESIAN_POINT('Ctrl Pts',(1.62787932400812,28.9576008261042,126.847153394078));
#134991=CARTESIAN_POINT('Ctrl Pts',(1.73901459484668,27.8827660958751,125.12606462635));
#134992=CARTESIAN_POINT('Ctrl Pts',(1.85014986568524,28.7457759881265,123.289592540736));
#134993=CARTESIAN_POINT('Ctrl Pts',(1.9612851365238,30.7567417491492,123.018608177807));
#134994=CARTESIAN_POINT('Ctrl Pts',(2.07242040736236,32.0750831233779,124.561135952501));
#134995=CARTESIAN_POINT('Ctrl Pts',(2.18355567820092,31.494159362724,126.505343616665));
#134996=CARTESIAN_POINT('Ctrl Pts',(2.29469094903948,29.545673633558,127.071752680283));
#134997=CARTESIAN_POINT('Ctrl Pts',(2.40582621987804,28.0130200266448,125.741944876271));
#134998=CARTESIAN_POINT('Ctrl Pts',(2.5169614907166,28.298993215467,123.733055829446));
#134999=CARTESIAN_POINT('Ctrl Pts',(2.62809676155516,30.1418499947993,122.883765090414));
#135000=CARTESIAN_POINT('Ctrl Pts',(2.73923203239372,31.8548754701923,123.971404548242));
#135001=CARTESIAN_POINT('Ctrl Pts',(2.85036730323227,31.8701856810441,126.00048844649));
#135002=CARTESIAN_POINT('Ctrl Pts',(2.96150257407084,30.1737676228579,127.113853454367));
#135003=CARTESIAN_POINT('Ctrl Pts',(3.07263784490939,28.3183049546232,126.292467944518));
#135004=CARTESIAN_POINT('Ctrl Pts',(3.18377311574795,28.0020503866253,124.288122935015));
#135005=CARTESIAN_POINT('Ctrl Pts',(3.29490838658652,29.5144628157628,122.935338948888));
#135006=CARTESIAN_POINT('Ctrl Pts',(3.40604365742507,31.4712737516316,123.472281059551));
#135007=CARTESIAN_POINT('Ctrl Pts',(3.51717892826364,32.0814692696916,125.407501279233));
#135008=CARTESIAN_POINT('Ctrl Pts',(3.62831419910219,30.7865546020038,126.969747057699));
#135009=CARTESIAN_POINT('Ctrl Pts',(3.73944946994076,28.7717286650289,126.729138843742));
#135010=CARTESIAN_POINT('Ctrl Pts',(3.8505847407793,27.8811048794813,124.905898557453));
#135011=CARTESIAN_POINT('Ctrl Pts',(3.96172001161788,28.9298461066255,123.168786670608));
#135012=CARTESIAN_POINT('Ctrl Pts',(4.07285528245642,30.9580690452094,123.107732757283));
#135013=CARTESIAN_POINT('Ctrl Pts',(4.183990553295,32.1093983763515,124.778617744403));
#135014=CARTESIAN_POINT('Ctrl Pts',(4.29512582413354,31.3300547972064,126.65212767354));
#135015=CARTESIAN_POINT('Ctrl Pts',(4.40626109497212,29.3333495309789,127.01349168496));
#135016=CARTESIAN_POINT('Ctrl Pts',(4.51739636581066,27.9468106589228,125.531963478948));
#135017=CARTESIAN_POINT('Ctrl Pts',(4.62853163664923,28.4394981506248,123.563544086529));
#135018=CARTESIAN_POINT('Ctrl Pts',(4.73966690748779,30.3604690243655,122.909872325498));
#135019=CARTESIAN_POINT('Ctrl Pts',(4.85080217832634,31.9515127548303,124.169235544223));
#135020=CARTESIAN_POINT('Ctrl Pts',(4.96193744916491,31.7563918366111,126.188974065964));
#135021=CARTESIAN_POINT('Ctrl Pts',(5.07307272000346,29.9536949494275,127.120478119561));
#135022=CARTESIAN_POINT('Ctrl Pts',(5.18420799084203,28.1933797705796,126.111168286038));
#135023=CARTESIAN_POINT('Ctrl Pts',(5.29534326168058,28.0866131936566,124.084837422881));
#135024=CARTESIAN_POINT('Ctrl Pts',(5.40647853251915,29.7311156588089,122.896129085635));
#135025=CARTESIAN_POINT('Ctrl Pts',(5.5176138033577,31.6217203867477,123.633034528433));
#135026=CARTESIAN_POINT('Ctrl Pts',(5.62874907419627,32.0280101299703,125.621084958751));
#135027=CARTESIAN_POINT('Ctrl Pts',(5.73988434503482,30.5781193320407,127.040673822826));
#135028=CARTESIAN_POINT('Ctrl Pts',(5.85101961587339,28.5990921956187,126.592491424426));
#135029=CARTESIAN_POINT('Ctrl Pts',(5.96215488671193,27.9022765077555,124.686746487118));
#135030=CARTESIAN_POINT('Ctrl Pts',(6.0732901575505,29.125448037648,123.067713665527));
#135031=CARTESIAN_POINT('Ctrl Pts',(6.18442542838907,31.1490723417917,123.217248091692));
#135032=CARTESIAN_POINT('Ctrl Pts',(6.29556069922761,32.1209831018612,124.998485117859));
#135033=CARTESIAN_POINT('Ctrl Pts',(6.40669597006619,31.1516177787356,126.781108672975));
#135034=CARTESIAN_POINT('Ctrl Pts',(6.51783124090473,29.1282091448092,126.933533635097));
#135035=CARTESIAN_POINT('Ctrl Pts',(6.62896651174331,27.9027261215296,125.316249730339));
#135036=CARTESIAN_POINT('Ctrl Pts',(6.74010178258185,28.5968187971898,123.409511356433));
#135037=CARTESIAN_POINT('Ctrl Pts',(6.85123705342043,30.5752036989361,122.958502432531));
#135038=CARTESIAN_POINT('Ctrl Pts',(6.96237232425897,32.0271208590569,124.37601872138));
#135039=CARTESIAN_POINT('Ctrl Pts',(7.07350759509754,31.6236714025963,126.364647496437));
#135040=CARTESIAN_POINT('Ctrl Pts',(7.1846428659361,29.7341212516656,127.104252861346));
#135041=CARTESIAN_POINT('Ctrl Pts',(7.29577813677465,28.0879224288666,125.917894860832));
#135042=CARTESIAN_POINT('Ctrl Pts',(7.40691340761322,28.1917943424084,123.89141355223));
#135043=CARTESIAN_POINT('Ctrl Pts',(7.51804867845177,29.9506659548665,122.879590189155));
#135044=CARTESIAN_POINT('Ctrl Pts',(7.62918394929034,31.754691630573,123.808518192709));
#135045=CARTESIAN_POINT('Ctrl Pts',(7.74031922012889,31.952697484926,125.827975928281));
#135046=CARTESIAN_POINT('Ctrl Pts',(7.85145449096745,30.3634543467503,127.089610623763));
#135047=CARTESIAN_POINT('Ctrl Pts',(7.96258976180602,28.4415516711872,126.438683576878));
#135048=CARTESIAN_POINT('Ctrl Pts',(8.07372503264457,27.946052873724,124.470969990334));
#135049=CARTESIAN_POINT('Ctrl Pts',(8.18486030348314,29.3304739676535,122.987462649588));
#135050=CARTESIAN_POINT('Ctrl Pts',(8.29599557432169,31.3276934827861,123.345974088848));
#135051=CARTESIAN_POINT('Ctrl Pts',(8.40713084516025,32.1097123429055,125.218368772072));
#135052=CARTESIAN_POINT('Ctrl Pts',(8.51826611599881,30.9607713583517,126.890896826131));
#135053=CARTESIAN_POINT('Ctrl Pts',(8.62940138683738,28.9324625437016,126.832739966954));
#135054=CARTESIAN_POINT('Ctrl Pts',(8.74053665767593,27.8812424544389,125.097128486853));
#135055=CARTESIAN_POINT('Ctrl Pts',(8.85167192851449,28.7692578846935,123.272616740873));
#135056=CARTESIAN_POINT('Ctrl Pts',(8.96280719935305,30.7837441415154,123.029132858921));
#135057=CARTESIAN_POINT('Ctrl Pts',(9.0739424701916,32.0808768028432,124.589522826205));
#135058=CARTESIAN_POINT('Ctrl Pts',(9.18507774103017,31.4734712393041,126.525621769289));
#135059=CARTESIAN_POINT('Ctrl Pts',(9.29621301186872,29.5173788254838,127.065340248965));
#135060=CARTESIAN_POINT('Ctrl Pts',(9.4073482827073,28.0031377608259,125.714755203815));
#135061=CARTESIAN_POINT('Ctrl Pts',(9.51848355354583,28.3163218100152,123.709885296032));
#135062=CARTESIAN_POINT('Ctrl Pts',(9.62961882438441,30.1710286076982,122.886002405562));
#135063=CARTESIAN_POINT('Ctrl Pts',(9.74075409522296,31.8681856415175,123.996634685421));
#135064=CARTESIAN_POINT('Ctrl Pts',(9.85188936606152,31.857502852618,126.026361177139));
#135065=CARTESIAN_POINT('Ctrl Pts',(9.96303770704222,30.1422540520468,127.11530971663));
#135066=CARTESIAN_POINT('Ctrl Pts',(10.0371409577434,28.9190765182705,126.551772147558));
#135067=CARTESIAN_POINT('Ctrl Pts',(10.074199118165,28.5620255677698,126.073441073449));
#135068=CARTESIAN_POINT('Ctrl Pts',(-0.22620467696834,30.4290778082509,
123.393357036968));
#135069=CARTESIAN_POINT('Ctrl Pts',(-0.189159586688819,30.9633122238839,
123.536032253196));
#135070=CARTESIAN_POINT('Ctrl Pts',(-0.115069406129781,31.8689366111695,
124.394346047585));
#135071=CARTESIAN_POINT('Ctrl Pts',(-0.00393413529122068,31.5225834737523,
126.244826699143));
#135072=CARTESIAN_POINT('Ctrl Pts',(0.107201135547339,29.7798951279279,
126.95281945916));
#135073=CARTESIAN_POINT('Ctrl Pts',(0.218336406385899,28.2400096499221,
125.874966629674));
#135074=CARTESIAN_POINT('Ctrl Pts',(0.329471677224458,28.3103293092203,
123.995537135953));
#135075=CARTESIAN_POINT('Ctrl Pts',(0.440606948063018,29.9274849847832,
123.035831556234));
#135076=CARTESIAN_POINT('Ctrl Pts',(0.551742218901577,31.6108496399274,
123.873692646674));
#135077=CARTESIAN_POINT('Ctrl Pts',(0.662877489740137,31.8199289758145,
125.742520685753));
#135078=CARTESIAN_POINT('Ctrl Pts',(0.774012760578696,30.3632390983645,
126.931696237506));
#135079=CARTESIAN_POINT('Ctrl Pts',(0.885148031417255,28.5741062065216,
126.352866475942));
#135080=CARTESIAN_POINT('Ctrl Pts',(0.996283302255815,28.090044106761,124.535785358627));
#135081=CARTESIAN_POINT('Ctrl Pts',(1.10741857309438,29.3541155852438,123.143592148996));
#135082=CARTESIAN_POINT('Ctrl Pts',(1.21855384393294,31.2093445258783,123.450514120018));
#135083=CARTESIAN_POINT('Ctrl Pts',(1.32968911477149,31.9576956494266,125.175638164633));
#135084=CARTESIAN_POINT('Ctrl Pts',(1.44082438561006,30.9142225226776,126.740004904113));
#135085=CARTESIAN_POINT('Ctrl Pts',(1.55195965644861,29.0339875579863,126.711794488784));
#135086=CARTESIAN_POINT('Ctrl Pts',(1.66309492728717,28.037916428508,125.116826644344));
#135087=CARTESIAN_POINT('Ctrl Pts',(1.77423019812573,28.8376851873223,123.414930740604));
#135088=CARTESIAN_POINT('Ctrl Pts',(1.88536546896429,30.7012879167365,123.163804039111));
#135089=CARTESIAN_POINT('Ctrl Pts',(1.99650073980285,31.923021588653,124.593295792194));
#135090=CARTESIAN_POINT('Ctrl Pts',(2.10763601064141,31.3846677653708,126.395032440182));
#135091=CARTESIAN_POINT('Ctrl Pts',(2.21877128147997,29.5789665478364,126.919935199536));
#135092=CARTESIAN_POINT('Ctrl Pts',(2.32990655231853,28.1586253861661,125.687575354735));
#135093=CARTESIAN_POINT('Ctrl Pts',(2.44104182315709,28.4236425364121,123.825897158459));
#135094=CARTESIAN_POINT('Ctrl Pts',(2.55217709399565,30.1314552652258,123.038842216995));
#135095=CARTESIAN_POINT('Ctrl Pts',(2.66331236483421,31.7189506932312,124.046779747068));
#135096=CARTESIAN_POINT('Ctrl Pts',(2.77444763567277,31.733138975938,125.927172921471));
#135097=CARTESIAN_POINT('Ctrl Pts',(2.88558290651133,30.1610339780609,126.958950840186));
#135098=CARTESIAN_POINT('Ctrl Pts',(2.99671817734989,28.4415391165025,126.197756240195));
#135099=CARTESIAN_POINT('Ctrl Pts',(3.10785344818845,28.1484595984251,124.340289095405));
#135100=CARTESIAN_POINT('Ctrl Pts',(3.21898871902701,29.5500428503983,123.086636756953));
#135101=CARTESIAN_POINT('Ctrl Pts',(3.33012398986556,31.3634592057211,123.584231893759));
#135102=CARTESIAN_POINT('Ctrl Pts',(3.44125926070413,31.9289397598776,125.377639694786));
#135103=CARTESIAN_POINT('Ctrl Pts',(3.55239453154268,30.72891609173,126.825404521615));
#135104=CARTESIAN_POINT('Ctrl Pts',(3.66352980238124,28.861736059022,126.602428013043));
#135105=CARTESIAN_POINT('Ctrl Pts',(3.7746650732198,28.0363769456059,124.912794285924));
#135106=CARTESIAN_POINT('Ctrl Pts',(3.88580034405837,29.0082666969071,123.302977492238));
#135107=CARTESIAN_POINT('Ctrl Pts',(3.99693561489692,30.8878620025393,123.246397593306));
#135108=CARTESIAN_POINT('Ctrl Pts',(4.10807088573548,31.9548222290924,124.794840576717));
#135109=CARTESIAN_POINT('Ctrl Pts',(4.21920615657404,31.2325887383998,126.531060200739));
#135110=CARTESIAN_POINT('Ctrl Pts',(4.3303414274126,29.382201498547,126.865943554323));
#135111=CARTESIAN_POINT('Ctrl Pts',(4.44147669825116,28.0972678231528,125.492981337888));
#135112=CARTESIAN_POINT('Ctrl Pts',(4.55261196908972,28.5538513076063,123.668807190598));
#135113=CARTESIAN_POINT('Ctrl Pts',(4.66374723992828,30.334053950941,123.063036320894));
#135114=CARTESIAN_POINT('Ctrl Pts',(4.77488251076683,31.8085064235698,124.230113740723));
#135115=CARTESIAN_POINT('Ctrl Pts',(4.8860177816054,31.6276839139044,126.101846365303));
#135116=CARTESIAN_POINT('Ctrl Pts',(4.99715305244395,29.9570881711141,126.965090051692));
#135117=CARTESIAN_POINT('Ctrl Pts',(5.10828832328252,28.3257684164394,126.029742172062));
#135118=CARTESIAN_POINT('Ctrl Pts',(5.21942359412107,28.2268256656377,124.151900291077));
#135119=CARTESIAN_POINT('Ctrl Pts',(5.33055886495964,29.7508194312142,123.050300181963));
#135120=CARTESIAN_POINT('Ctrl Pts',(5.44169413579819,31.502881151767,123.733205391558));
#135121=CARTESIAN_POINT('Ctrl Pts',(5.55282940663676,31.8793980915768,125.575572019554));
#135122=CARTESIAN_POINT('Ctrl Pts',(5.66396467747531,30.5357549024456,126.891133792417));
#135123=CARTESIAN_POINT('Ctrl Pts',(5.77509994831388,28.7017503437876,126.475794079966));
#135124=CARTESIAN_POINT('Ctrl Pts',(5.88623521915243,28.0559971226385,124.709701620524));
#135125=CARTESIAN_POINT('Ctrl Pts',(5.99737048999099,29.1895349708864,123.209311089859));
#135126=CARTESIAN_POINT('Ctrl Pts',(6.10850576082955,31.0648686287769,123.347887673383));
#135127=CARTESIAN_POINT('Ctrl Pts',(6.21964103166811,31.9655580290238,124.998596128017));
#135128=CARTESIAN_POINT('Ctrl Pts',(6.33077630250668,31.0672275367842,126.650589507129));
#135129=CARTESIAN_POINT('Ctrl Pts',(6.44191157334522,29.1920937448553,126.791844808909));
#135130=CARTESIAN_POINT('Ctrl Pts',(6.5530468441838,28.0564137888359,125.29307503492));
#135131=CARTESIAN_POINT('Ctrl Pts',(6.66418211502234,28.6996435393857,123.52606193765));
#135132=CARTESIAN_POINT('Ctrl Pts',(6.77531738586092,30.533052926153,123.108102826727));
#135133=CARTESIAN_POINT('Ctrl Pts',(6.88645265669946,31.8785739861974,124.421743902119));
#135134=CARTESIAN_POINT('Ctrl Pts',(6.99758792753804,31.5046891976975,126.264646493909));
#135135=CARTESIAN_POINT('Ctrl Pts',(7.10872319837658,29.7536047750324,126.950053776046));
#135136=CARTESIAN_POINT('Ctrl Pts',(7.21985846921515,28.2280389604426,125.850631771618));
#135137=CARTESIAN_POINT('Ctrl Pts',(7.33099374005371,28.3242991680195,123.97265046979));
#135138=CARTESIAN_POINT('Ctrl Pts',(7.44212901089227,29.954281140462,123.03497325138));
#135139=CARTESIAN_POINT('Ctrl Pts',(7.55326428173082,31.626108298509,123.895829659981));
#135140=CARTESIAN_POINT('Ctrl Pts',(7.66439955256939,31.8096043369618,125.767302074327));
#135141=CARTESIAN_POINT('Ctrl Pts',(7.77553482340794,30.3368205097023,126.936484517706));
#135142=CARTESIAN_POINT('Ctrl Pts',(7.8866700942465,28.5557543467325,126.333257230232));
#135143=CARTESIAN_POINT('Ctrl Pts',(7.99780536508506,28.0965655682502,124.509737167552));
#135144=CARTESIAN_POINT('Ctrl Pts',(8.10894063592362,29.3795366557309,123.134940846845));
#135145=CARTESIAN_POINT('Ctrl Pts',(8.22007590676218,31.230400460467,123.467180663992));
#135146=CARTESIAN_POINT('Ctrl Pts',(8.33121117760075,31.9551131882614,125.202366767024));
#135147=CARTESIAN_POINT('Ctrl Pts',(8.44234644843929,30.8903662908993,126.752332413868));
#135148=CARTESIAN_POINT('Ctrl Pts',(8.55348171927787,29.0106914021759,126.698437273733));
#135149=CARTESIAN_POINT('Ctrl Pts',(8.6646169901164,28.0365044391075,125.090010937387));
#135150=CARTESIAN_POINT('Ctrl Pts',(8.77575226095499,28.8594463368069,123.399198922802));
#135151=CARTESIAN_POINT('Ctrl Pts',(8.88688753179353,30.7263115810325,123.173557474415));
#135152=CARTESIAN_POINT('Ctrl Pts',(8.9980228026321,31.928390708841,124.619602483407));
#135153=CARTESIAN_POINT('Ctrl Pts',(9.10915807347066,31.3654956620864,126.413824615221));
#135154=CARTESIAN_POINT('Ctrl Pts',(9.22029334430921,29.552745175709,126.913992669463));
#135155=CARTESIAN_POINT('Ctrl Pts',(9.33142861514778,28.1494672901359,125.662378134184));
#135156=CARTESIAN_POINT('Ctrl Pts',(9.44256388598633,28.4397012961995,123.804424555518));
#135157=CARTESIAN_POINT('Ctrl Pts',(9.5536991568249,30.1584956771975,123.040915582288));
#135158=CARTESIAN_POINT('Ctrl Pts',(9.66483442766346,31.7312854987716,124.070161026561));
#135159=CARTESIAN_POINT('Ctrl Pts',(9.77596969850201,31.7213855417773,125.951149705358));
#135160=CARTESIAN_POINT('Ctrl Pts',(9.8871180394827,30.1318297132667,126.960300387941));
#135161=CARTESIAN_POINT('Ctrl Pts',(9.96122129018386,28.9982863010982,126.438058700785));
#135162=CARTESIAN_POINT('Ctrl Pts',(9.99827945060551,28.6673999484858,125.994779599494));
#135163=CARTESIAN_POINT('Ctrl Pts',(10.,28.6653082844465,125.997072727755));
#135164=CARTESIAN_POINT('Ctrl Pts',(10.0000000000001,28.6967050287084,126.051116487996));
#135165=CARTESIAN_POINT('Ctrl Pts',(10.,28.7312952913176,126.103084852867));
#135166=CARTESIAN_POINT('Ctrl Pts',(10.,28.7687526561708,126.152891945816));
#135167=CARTESIAN_POINT('Ctrl Pts',(10.0000000000001,28.7925064920188,126.184477443477));
#135168=CARTESIAN_POINT('Ctrl Pts',(9.99999999999996,28.8174144318639,126.215193579688));
#135169=CARTESIAN_POINT('Ctrl Pts',(10.,28.8434032080411,126.245015253039));
#135170=CARTESIAN_POINT('Ctrl Pts',(10.0000000000001,28.8610650760105,126.265281942542));
#135171=CARTESIAN_POINT('Ctrl Pts',(9.99999999999991,28.8792262859797,126.285135469238));
#135172=CARTESIAN_POINT('Ctrl Pts',(9.99999999999992,28.8978656284541,126.304567075492));
#135173=CARTESIAN_POINT('Ctrl Pts',(9.99999999999992,28.9078692983068,126.314995950541));
#135174=CARTESIAN_POINT('Ctrl Pts',(10.0000000000001,28.9180108113656,126.325303204012));
#135175=CARTESIAN_POINT('Ctrl Pts',(10.0000000000001,28.9282763435345,126.335477297132));
#135176=CARTESIAN_POINT('Ctrl Pts',(9.99999999999998,28.9751289989059,126.381912617854));
#135177=CARTESIAN_POINT('Ctrl Pts',(9.99999999999992,29.0246129144767,126.425630794521));
#135178=CARTESIAN_POINT('Ctrl Pts',(9.99999999999994,29.0763924472693,126.466522146034));
#135179=CARTESIAN_POINT('Ctrl Pts',(9.99999999999995,29.1137524290861,126.496026084493));
#135180=CARTESIAN_POINT('Ctrl Pts',(9.99999999999988,29.1523086592386,126.524058047823));
#135181=CARTESIAN_POINT('Ctrl Pts',(9.99999999999993,29.191949375433,126.55056814615));
#135182=CARTESIAN_POINT('Ctrl Pts',(9.99999999999994,29.2027336731786,126.557780245755));
#135183=CARTESIAN_POINT('Ctrl Pts',(10.0000000000001,29.2135982956353,126.564879660816));
#135184=CARTESIAN_POINT('Ctrl Pts',(10.0000000000001,29.224541120581,126.571865272476));
#135185=CARTESIAN_POINT('Ctrl Pts',(10.0000000000001,29.2359307117797,126.579136087962));
#135186=CARTESIAN_POINT('Ctrl Pts',(9.99999999999999,29.2473984635858,126.586279379619));
#135187=CARTESIAN_POINT('Ctrl Pts',(9.99999999999997,29.2589365233135,126.593291232705));
#135188=CARTESIAN_POINT('Ctrl Pts',(9.99999999999987,29.3169202191603,126.628528800049));
#135189=CARTESIAN_POINT('Ctrl Pts',(10.0000000000002,29.3767154320219,126.660474363582));
#135190=CARTESIAN_POINT('Ctrl Pts',(10.0000000000001,29.4379816057261,126.6890174197));
#135191=CARTESIAN_POINT('Ctrl Pts',(10.0000000000001,29.5001391867863,126.717975770077));
#135192=CARTESIAN_POINT('Ctrl Pts',(10.0000000000001,29.5638116094751,126.74343262034));
#135193=CARTESIAN_POINT('Ctrl Pts',(9.99999999999995,29.6286835625344,126.76523838423));
#135194=CARTESIAN_POINT('Ctrl Pts',(9.99999999999989,29.6688787895444,126.778749425417));
#135195=CARTESIAN_POINT('Ctrl Pts',(10.0000000000001,29.7095352866061,126.790858044881));
#135196=CARTESIAN_POINT('Ctrl Pts',(9.99999999999995,29.7505836069801,126.801520293352));
#135197=CARTESIAN_POINT('Ctrl Pts',(9.99999999999985,29.7841900744798,126.810249530102));
#135198=CARTESIAN_POINT('Ctrl Pts',(9.9999999999998,29.8180592674631,126.818009191325));
#135199=CARTESIAN_POINT('Ctrl Pts',(9.99999999999999,29.8521544944741,126.82477142239));
#135200=CARTESIAN_POINT('Ctrl Pts',(10.0000000000001,29.8661247094476,126.827542186217));
#135201=CARTESIAN_POINT('Ctrl Pts',(10.0000000000001,29.8801354878125,126.830145768473));
#135202=CARTESIAN_POINT('Ctrl Pts',(10.,29.8941603582459,126.832576321549));
#135203=CARTESIAN_POINT('Ctrl Pts',(9.9999999999998,29.9636137929348,126.844612814874));
#135204=CARTESIAN_POINT('Ctrl Pts',(10.0000000000002,30.0335315560267,126.852435094899));
#135205=CARTESIAN_POINT('Ctrl Pts',(9.99999999999991,30.1035784530787,126.85590279931));
#135206=CARTESIAN_POINT('Ctrl Pts',(9.99999999999988,30.1113621962958,126.85628813716));
#135207=CARTESIAN_POINT('Ctrl Pts',(10.0000000000001,30.119147563991,126.856619660668));
#135208=CARTESIAN_POINT('Ctrl Pts',(10.0000000000001,30.1269341171633,126.856897143374));
#135209=CARTESIAN_POINT('Ctrl Pts',(10.0000000000001,30.1968734287048,126.859389510539));
#135210=CARTESIAN_POINT('Ctrl Pts',(10.0000000000001,30.2669070801432,126.857526934753));
#135211=CARTESIAN_POINT('Ctrl Pts',(10.0000000000001,30.3367420640854,126.851551839746));
#135212=CARTESIAN_POINT('Ctrl Pts',(10.,30.4065770480275,126.845576744738));
#135213=CARTESIAN_POINT('Ctrl Pts',(9.99999999999998,30.4762143055634,126.835488833351));
#135214=CARTESIAN_POINT('Ctrl Pts',(9.9999999999999,30.5453683176971,126.821473427802));
#135215=CARTESIAN_POINT('Ctrl Pts',(9.99999999999988,30.558412278624,126.818829815426));
#135216=CARTESIAN_POINT('Ctrl Pts',(9.99999999999984,30.5714390442574,126.816046313978));
#135217=CARTESIAN_POINT('Ctrl Pts',(9.99999999999995,30.584446685237,126.813123952926));
#135218=CARTESIAN_POINT('Ctrl Pts',(10.,30.5957697829836,126.8105800497));
#135219=CARTESIAN_POINT('Ctrl Pts',(9.99999999999987,30.6070694510325,126.807932918437));
#135220=CARTESIAN_POINT('Ctrl Pts',(9.99999999999987,30.6183425063254,126.805184212759));
#135221=CARTESIAN_POINT('Ctrl Pts',(9.99999999999988,30.6873871245024,126.788349084293));
#135222=CARTESIAN_POINT('Ctrl Pts',(9.9999999999999,30.7554558673819,126.767702776233));
#135223=CARTESIAN_POINT('Ctrl Pts',(10.,30.8222618925395,126.743495436202));
#135224=CARTESIAN_POINT('Ctrl Pts',(10.0000000000002,30.8904746787203,126.71877835259));
#135225=CARTESIAN_POINT('Ctrl Pts',(9.99999999999986,30.9573719317382,126.690348530093));
#135226=CARTESIAN_POINT('Ctrl Pts',(9.99999999999997,31.0226523342096,126.658417278966));
#135227=CARTESIAN_POINT('Ctrl Pts',(10.0000000000001,31.0883272019745,126.626293079115));
#135228=CARTESIAN_POINT('Ctrl Pts',(9.99999999999989,31.1523666455233,126.590624692189));
#135229=CARTESIAN_POINT('Ctrl Pts',(9.99999999999989,31.2144530767094,126.551575995527));
#135230=CARTESIAN_POINT('Ctrl Pts',(9.99999999999989,31.2297926762732,126.541928293785));
#135231=CARTESIAN_POINT('Ctrl Pts',(9.99999999999993,31.2450129650166,126.532074017689));
#135232=CARTESIAN_POINT('Ctrl Pts',(10.,31.2601089384186,126.522015195508));
#135233=CARTESIAN_POINT('Ctrl Pts',(10.0000000000001,31.2719311826033,126.51413774045));
#135234=CARTESIAN_POINT('Ctrl Pts',(10.0000000000001,31.283678470288,126.506133794645));
#135235=CARTESIAN_POINT('Ctrl Pts',(10.0000000000001,31.2953308003886,126.49801690638));
#135236=CARTESIAN_POINT('Ctrl Pts',(10.,31.3572558121971,126.454880606831));
#135237=CARTESIAN_POINT('Ctrl Pts',(10.,31.4166138612528,126.408484217952));
#135238=CARTESIAN_POINT('Ctrl Pts',(10.,31.4730903954254,126.359062410629));
#135239=CARTESIAN_POINT('Ctrl Pts',(10.,31.5294280870934,126.309762102396));
#135240=CARTESIAN_POINT('Ctrl Pts',(10.,31.5828994498296,126.25745079026));
#135241=CARTESIAN_POINT('Ctrl Pts',(10.,31.6331764759971,126.202312206008));
#135242=CARTESIAN_POINT('Ctrl Pts',(10.,31.6823970284773,126.148332251608));
#135243=CARTESIAN_POINT('Ctrl Pts',(10.0000000000001,31.7285569678729,126.091642060811));
#135244=CARTESIAN_POINT('Ctrl Pts',(9.99999999999998,31.7713193360823,126.03237423032));
#135245=CARTESIAN_POINT('Ctrl Pts',(9.99999999999995,31.7804981155288,126.019652616267));
#135246=CARTESIAN_POINT('Ctrl Pts',(9.99999999999993,31.7895202218754,126.006812110665));
#135247=CARTESIAN_POINT('Ctrl Pts',(10.,31.7983820815757,125.993853814881));
#135248=CARTESIAN_POINT('Ctrl Pts',(10.0000000000001,31.8058537413279,125.982928345472));
#135249=CARTESIAN_POINT('Ctrl Pts',(10.0000000000001,31.8132114861588,125.97191914214));
#135250=CARTESIAN_POINT('Ctrl Pts',(10.,31.8204553240174,125.960828035951));
#135251=CARTESIAN_POINT('',(-0.00087680738617197,31.2702792793494,126.080257521478));
#135252=CARTESIAN_POINT('Ctrl Pts',(-0.000876807386172018,31.2691344289485,
126.079283929862));
#135253=CARTESIAN_POINT('Ctrl Pts',(-0.000584538257448223,31.2636353971113,
126.085750264102));
#135254=CARTESIAN_POINT('Ctrl Pts',(-0.000292269128723795,31.2580869446366,
126.092174570554));
#135255=CARTESIAN_POINT('Ctrl Pts',(0.,31.2524897196664,126.098556098763));
#135256=CARTESIAN_POINT('Ctrl Pts',(-2.77772596590786E-16,30.5301702171886,
123.014825674328));
#135257=CARTESIAN_POINT('Ctrl Pts',(-8.75743131328376E-15,30.598829973896,
123.040247836712));
#135258=CARTESIAN_POINT('Ctrl Pts',(-2.39681854255766E-13,30.6657864177248,
123.069560482627));
#135259=CARTESIAN_POINT('Ctrl Pts',(-2.5254277835618E-13,30.7308507067716,
123.102469346234));
#135260=CARTESIAN_POINT('Ctrl Pts',(-2.65638855218647E-13,30.7977302451018,
123.136296344688));
#135261=CARTESIAN_POINT('Ctrl Pts',(-6.11451911266343E-14,30.8626113478622,
123.173923712712));
#135262=CARTESIAN_POINT('Ctrl Pts',(-1.69683711526147E-13,30.9252577077206,
123.21507651753));
#135263=CARTESIAN_POINT('Ctrl Pts',(-2.61344823476963E-13,30.9781920191894,
123.24984941404));
#135264=CARTESIAN_POINT('Ctrl Pts',(-8.4631591032592E-14,31.0295304465062,
123.287140434778));
#135265=CARTESIAN_POINT('Ctrl Pts',(-1.73687453308702E-13,31.0791076863594,
123.326801732865));
#135266=CARTESIAN_POINT('Ctrl Pts',(-2.13342330293228E-13,31.1011385797417,
123.34442622814));
#135267=CARTESIAN_POINT('Ctrl Pts',(-1.10073476274008E-13,31.1228213894366,
123.362518959318));
#135268=CARTESIAN_POINT('Ctrl Pts',(3.95516952522712E-15,31.1441400562127,
123.381067676726));
#135269=CARTESIAN_POINT('Ctrl Pts',(6.66452089179545E-14,31.1558506001259,
123.391256661432));
#135270=CARTESIAN_POINT('Ctrl Pts',(-1.34022555091032E-13,31.1674512495831,
123.401583242396));
#135271=CARTESIAN_POINT('Ctrl Pts',(-8.07479083597684E-14,31.178939208613,
123.412045430858));
#135272=CARTESIAN_POINT('Ctrl Pts',(-3.16896073044118E-14,31.1895349701113,
123.421695086938));
#135273=CARTESIAN_POINT('Ctrl Pts',(-6.15876490622071E-14,31.200036303322,
123.43146162442));
#135274=CARTESIAN_POINT('Ctrl Pts',(-7.96654409107589E-14,31.2104251173888,
123.441328016445));
#135275=CARTESIAN_POINT('Ctrl Pts',(-1.71607632518157E-13,31.2635091616281,
123.491742624636));
#135276=CARTESIAN_POINT('Ctrl Pts',(5.49748712918573E-14,31.3137531838448,
123.544845896782));
#135277=CARTESIAN_POINT('Ctrl Pts',(4.07729405793589E-14,31.3609385689379,
123.600378065046));
#135278=CARTESIAN_POINT('Ctrl Pts',(2.6523705644377E-14,31.4077587712736,
123.655480452134));
#135279=CARTESIAN_POINT('Ctrl Pts',(-1.80781432573089E-13,31.4515680052721,
123.712975168858));
#135280=CARTESIAN_POINT('Ctrl Pts',(-9.5215502149415E-14,31.4921078981635,
123.77263267036));
#135281=CARTESIAN_POINT('Ctrl Pts',(-2.38087088306119E-14,31.5257972460783,
123.822209079681));
#135282=CARTESIAN_POINT('Ctrl Pts',(-4.4744082398028E-14,31.5572281772826,
123.873279737524));
#135283=CARTESIAN_POINT('Ctrl Pts',(-4.78783679369599E-14,31.5862248073375,
123.925719379271));
#135284=CARTESIAN_POINT('Ctrl Pts',(-4.95707857465004E-14,31.5983293795196,
123.947610179255));
#135285=CARTESIAN_POINT('Ctrl Pts',(-1.23896470668944E-13,31.6100094226953,
123.969739580722));
#135286=CARTESIAN_POINT('Ctrl Pts',(-6.71823707776298E-14,31.6212507011121,
123.992098553664));
#135287=CARTESIAN_POINT('Ctrl Pts',(-4.1055023269343E-14,31.626451748782,
124.002443469946));
#135288=CARTESIAN_POINT('Ctrl Pts',(4.20872296912592E-14,31.6315588588845,
124.012837529915));
#135289=CARTESIAN_POINT('Ctrl Pts',(-1.66672231571852E-14,31.6365705562371,
124.023279837204));
#135290=CARTESIAN_POINT('Ctrl Pts',(-7.76815753353117E-14,31.6418017627402,
124.034179510898));
#135291=CARTESIAN_POINT('Ctrl Pts',(-6.18625599143113E-14,31.6469254048826,
124.045124295143));
#135292=CARTESIAN_POINT('Ctrl Pts',(-5.67601521339611E-14,31.6519384284677,
124.05610888875));
#135293=CARTESIAN_POINT('Ctrl Pts',(-2.74607999713858E-14,31.6804790658224,
124.118647454013));
#135294=CARTESIAN_POINT('Ctrl Pts',(-4.39722585003227E-15,31.7054587309027,
124.182518376153));
#135295=CARTESIAN_POINT('Ctrl Pts',(1.14908083048704E-14,31.7266539957321,
124.247516921405));
#135296=CARTESIAN_POINT('Ctrl Pts',(2.48997376757104E-14,31.7458595519117,
124.306413718519));
#135297=CARTESIAN_POINT('Ctrl Pts',(1.79531194258059E-14,31.7619575585816,
124.366236962781));
#135298=CARTESIAN_POINT('Ctrl Pts',(2.72004641033163E-15,31.7747450702918,
124.426839150922));
#135299=CARTESIAN_POINT('Ctrl Pts',(-1.50013263895926E-14,31.7898767105001,
124.498550561833));
#135300=CARTESIAN_POINT('Ctrl Pts',(-1.25000641635101E-14,31.8003734925573,
124.571354192565));
#135301=CARTESIAN_POINT('Ctrl Pts',(-5.63438184997267E-15,31.8063105084585,
124.644827210979));
#135302=CARTESIAN_POINT('Ctrl Pts',(-4.15408756744793E-15,31.8076174032829,
124.661000573001));
#135303=CARTESIAN_POINT('Ctrl Pts',(-1.03439185283564E-14,31.808703127552,
124.677206288828));
#135304=CARTESIAN_POINT('Ctrl Pts',(3.02535774210355E-15,31.8095681127238,
124.693439683831));
#135305=CARTESIAN_POINT('Ctrl Pts',(1.65497979186504E-14,31.8104620745258,
124.710216890567));
#135306=CARTESIAN_POINT('Ctrl Pts',(-9.80120482820878E-15,31.811120270022,
124.727029834275));
#135307=CARTESIAN_POINT('Ctrl Pts',(-1.05193631583234E-14,31.8115426155158,
124.743839163738));
#135308=CARTESIAN_POINT('Ctrl Pts',(-1.34948166120589E-14,31.8132672489494,
124.812479487862));
#135309=CARTESIAN_POINT('Ctrl Pts',(-1.60405791084441E-14,31.8110709449073,
124.881146605068));
#135310=CARTESIAN_POINT('Ctrl Pts',(-1.80688797257744E-14,31.8050746611966,
124.949501213653));
#135311=CARTESIAN_POINT('Ctrl Pts',(-2.00918682248362E-14,31.7990940817499,
125.017676801554));
#135312=CARTESIAN_POINT('Ctrl Pts',(1.91766302506283E-15,31.7893329284663,
125.085542577925));
#135313=CARTESIAN_POINT('Ctrl Pts',(-1.30451205393456E-14,31.7758617893156,
125.152746909433));
#135314=CARTESIAN_POINT('Ctrl Pts',(-2.4101450158528E-14,31.7661004735783,
125.201443808146));
#135315=CARTESIAN_POINT('Ctrl Pts',(6.03490530108545E-14,31.7543901513868,
125.249793146236));
#135316=CARTESIAN_POINT('Ctrl Pts',(3.41393580072236E-15,31.7407434738878,
125.297651488221));
#135317=CARTESIAN_POINT('Ctrl Pts',(-3.93869884415215E-14,31.7305056909709,
125.333554975794));
#135318=CARTESIAN_POINT('Ctrl Pts',(-1.37967821082287E-15,31.7191778680749,
125.369181973231));
#135319=CARTESIAN_POINT('Ctrl Pts',(-1.89293025698589E-14,31.7067614289762,
125.404467741074));
#135320=CARTESIAN_POINT('Ctrl Pts',(-2.47700547482771E-14,31.7026354143409,
125.416193292448));
#135321=CARTESIAN_POINT('Ctrl Pts',(1.15236377331479E-14,31.6983923938271,
125.427871943742));
#135322=CARTESIAN_POINT('Ctrl Pts',(-2.44249065417534E-15,31.6940329877996,
125.439501206732));
#135323=CARTESIAN_POINT('Ctrl Pts',(-7.59147689133786E-14,31.6709092331424,
125.501186725936));
#135324=CARTESIAN_POINT('Ctrl Pts',(6.73746093792032E-14,31.6445127108641,
125.561488649643));
#135325=CARTESIAN_POINT('Ctrl Pts',(-3.60822483003176E-15,31.6148933850985,
125.620073088418));
#135326=CARTESIAN_POINT('Ctrl Pts',(-5.37075275596212E-14,31.594056103009,
125.661287412014));
#135327=CARTESIAN_POINT('Ctrl Pts',(1.77541335953307E-14,31.5716229476758,
125.701651195217));
#135328=CARTESIAN_POINT('Ctrl Pts',(4.9960036108132E-16,31.5476009047189,
125.741036831029));
#135329=CARTESIAN_POINT('Ctrl Pts',(-5.33872078257124E-15,31.5398884957193,
125.753681806006));
#135330=CARTESIAN_POINT('Ctrl Pts',(3.16358140217142E-14,31.5320111431503,
125.766227577131));
#135331=CARTESIAN_POINT('Ctrl Pts',(2.75057754350883E-14,31.5239724343926,
125.778664238771));
#135332=CARTESIAN_POINT('Ctrl Pts',(1.03649137560407E-14,31.4897260852599,
125.831646660379));
#135333=CARTESIAN_POINT('Ctrl Pts',(-5.08270772809619E-14,31.4526236846046,
125.882545515417));
#135334=CARTESIAN_POINT('Ctrl Pts',(1.04083408558608E-14,31.4126994357374,
125.931045747963));
#135335=CARTESIAN_POINT('Ctrl Pts',(6.66773404040496E-14,31.3759099756901,
125.975737819026));
#135336=CARTESIAN_POINT('Ctrl Pts',(-1.45729917785235E-13,31.3367238178986,
126.018393245589));
#135337=CARTESIAN_POINT('Ctrl Pts',(3.38895578266829E-14,31.2951462810091,
126.058732615753));
#135338=CARTESIAN_POINT('Ctrl Pts',(6.77098686975264E-14,31.287343182337,
126.06630334046));
#135339=CARTESIAN_POINT('Ctrl Pts',(-1.39523139557582E-13,31.2794558011521,
126.073792385657));
#135340=CARTESIAN_POINT('Ctrl Pts',(-2.51743070833754E-14,31.2714857203022,
126.08119908863));
#135341=CARTESIAN_POINT('Ctrl Pts',(0.00172044862969348,-31.2663699642227,
126.077829790033));
#135342=CARTESIAN_POINT('Ctrl Pts',(0.0387786082858811,-31.6249060139602,
125.656600524761));
#135343=CARTESIAN_POINT('Ctrl Pts',(0.112881858221588,-31.8818178994089,
124.435268666319));
#135344=CARTESIAN_POINT('Ctrl Pts',(0.224030198436815,-30.5442576915066,
123.110121958068));
#135345=CARTESIAN_POINT('Ctrl Pts',(0.335165469275375,-28.7082269099583,
123.519030297083));
#135346=CARTESIAN_POINT('Ctrl Pts',(0.446300740113934,-28.0547651464445,
125.281415280471));
#135347=CARTESIAN_POINT('Ctrl Pts',(0.557436010952494,-29.181599264857,
126.787219487406));
#135348=CARTESIAN_POINT('Ctrl Pts',(0.668571281791053,-31.0575532184307,
126.656742998468));
#135349=CARTESIAN_POINT('Ctrl Pts',(0.779706552629611,-31.9655285234099,
125.010137807065));
#135350=CARTESIAN_POINT('Ctrl Pts',(0.890841823468172,-31.074525746938,
123.354134510974));
#135351=CARTESIAN_POINT('Ctrl Pts',(1.00197709430673,-29.2000325132351,
123.204604423553));
#135352=CARTESIAN_POINT('Ctrl Pts',(1.11311236514529,-28.0577305949802,
124.698320246674));
#135353=CARTESIAN_POINT('Ctrl Pts',(1.22424763598385,-28.6931313646975,
126.468169411394));
#135354=CARTESIAN_POINT('Ctrl Pts',(1.33538290682241,-30.5246730611939,
126.894237381088));
#135355=CARTESIAN_POINT('Ctrl Pts',(1.44651817766097,-31.8759958504512,
125.58656674063));
#135356=CARTESIAN_POINT('Ctrl Pts',(1.55765344849953,-31.5102727009557,
123.742026356952));
#135357=CARTESIAN_POINT('Ctrl Pts',(1.66878871933809,-29.7622393879308,
123.048874664683));
#135358=CARTESIAN_POINT('Ctrl Pts',(1.77992399017665,-28.2318217175757,
124.141532605131));
#135359=CARTESIAN_POINT('Ctrl Pts',(1.89105926101521,-28.3197677921431,
126.019921776628));
#135360=CARTESIAN_POINT('Ctrl Pts',(2.00219453185377,-29.9455830857295,
126.964805175196));
#135361=CARTESIAN_POINT('Ctrl Pts',(2.11332980269233,-31.6212046416694,
126.111357797976));
#135362=CARTESIAN_POINT('Ctrl Pts',(2.22446507353089,-31.8129832629486,
124.240715911099));
#135363=CARTESIAN_POINT('Ctrl Pts',(2.33560034436945,-30.3453893754288,
123.065025373487));
#135364=CARTESIAN_POINT('Ctrl Pts',(2.44673561520801,-28.5616703232575,
123.660362595487));
#135365=CARTESIAN_POINT('Ctrl Pts',(2.55787088604656,-28.0944139048355,
125.481832198108));
#135366=CARTESIAN_POINT('Ctrl Pts',(2.66900615688513,-29.3712867574847,
126.86229436194));
#135367=CARTESIAN_POINT('Ctrl Pts',(2.78014142772368,-31.2236031295178,
126.538250959478));
#135368=CARTESIAN_POINT('Ctrl Pts',(2.89127669856224,-31.9559900271131,
124.80628978731));
#135369=CARTESIAN_POINT('Ctrl Pts',(3.00241196940081,-30.89811435481,123.251626116011));
#135370=CARTESIAN_POINT('Ctrl Pts',(3.11354724023936,-29.0182199142231,
123.297199807425));
#135371=CARTESIAN_POINT('Ctrl Pts',(3.22468251107792,-28.0369211285432,
124.901298545784));
#135372=CARTESIAN_POINT('Ctrl Pts',(3.33581778191648,-28.852373132271,126.595735944659));
#135373=CARTESIAN_POINT('Ctrl Pts',(3.44695305275504,-30.7182156783826,
126.829641186668));
#135374=CARTESIAN_POINT('Ctrl Pts',(3.5580883235936,-31.9266956468316,125.388927393098));
#135375=CARTESIAN_POINT('Ctrl Pts',(3.66922359443216,-31.3717253664279,
123.59223931305));
#135376=CARTESIAN_POINT('Ctrl Pts',(3.78035886527072,-29.5612535008297,
123.084034931924));
#135377=CARTESIAN_POINT('Ctrl Pts',(3.89149413610928,-28.1523539460514,
124.329459403205));
#135378=CARTESIAN_POINT('Ctrl Pts',(4.00262940694784,-28.4345527746557,
126.18861079302));
#135379=CARTESIAN_POINT('Ctrl Pts',(4.1137646777864,-30.1495613486075,126.959860208184));
#135380=CARTESIAN_POINT('Ctrl Pts',(4.22489994862496,-31.7276806334521,
125.937304785764));
#135381=CARTESIAN_POINT('Ctrl Pts',(4.33603521946352,-31.7245025047645,
124.056860697625));
#135382=CARTESIAN_POINT('Ctrl Pts',(4.44717049030208,-30.1429358142016,
123.039645443895));
#135383=CARTESIAN_POINT('Ctrl Pts',(4.55830576114063,-28.4305439995263,
123.816687490475));
#135384=CARTESIAN_POINT('Ctrl Pts',(4.6694410319792,-28.1546310491437,125.67678214208));
#135385=CARTESIAN_POINT('Ctrl Pts',(4.78057630281775,-29.5677323138313,
126.917437164581));
#135386=CARTESIAN_POINT('Ctrl Pts',(4.89171157365632,-31.3764760143124,
126.403115966214));
#135387=CARTESIAN_POINT('Ctrl Pts',(5.00284684449487,-31.92536999542,124.604562250968));
#135388=CARTESIAN_POINT('Ctrl Pts',(5.11398211533343,-30.7120270590674,
123.167941567586));
#135389=CARTESIAN_POINT('Ctrl Pts',(5.225117386172,-28.8469858139721,123.408152356713));
#135390=CARTESIAN_POINT('Ctrl Pts',(5.33625265701055,-28.0372659719354,
125.105336450006));
#135391=CARTESIAN_POINT('Ctrl Pts',(5.44738792784911,-29.0239812938614,
126.70610905803));
#135392=CARTESIAN_POINT('Ctrl Pts',(5.55852319868768,-30.9040190422199,
126.745328107815));
#135393=CARTESIAN_POINT('Ctrl Pts',(5.66965846952622,-31.9566336282375,
125.187097507927));
#135394=CARTESIAN_POINT('Ctrl Pts',(5.7807937403648,-31.2183965744007,123.457621829735));
#135395=CARTESIAN_POINT('Ctrl Pts',(5.89192901120334,-29.3649954593064,
123.139841440651));
#135396=CARTESIAN_POINT('Ctrl Pts',(6.00306428204191,-28.0927961116786,
124.524611778654));
#135397=CARTESIAN_POINT('Ctrl Pts',(6.11419955288046,-28.5662067554389,
126.344491563556));
#135398=CARTESIAN_POINT('Ctrl Pts',(6.22533482371902,-30.3519279647429,
126.933796095832));
#135399=CARTESIAN_POINT('Ctrl Pts',(6.33647009455759,-31.8155394220347,
125.753151538311));
#135400=CARTESIAN_POINT('Ctrl Pts',(6.44760536539615,-31.6174387916631,
123.883168594708));
#135401=CARTESIAN_POINT('Ctrl Pts',(6.5587406362347,-29.9389419999398,123.035389974257));
#135402=CARTESIAN_POINT('Ctrl Pts',(6.66987590707327,-28.3163298756153,
123.985763565594));
#135403=CARTESIAN_POINT('Ctrl Pts',(6.78101117791182,-28.2347335856866,
125.864439193422));
#135404=CARTESIAN_POINT('Ctrl Pts',(6.89214644875039,-29.7688359156915,
126.951917979511));
#135405=CARTESIAN_POINT('Ctrl Pts',(7.00328171958894,-31.5145162199645,
126.252861226189));
#135406=CARTESIAN_POINT('Ctrl Pts',(7.1144169904275,-31.8740024933559,124.40709588671));
#135407=CARTESIAN_POINT('Ctrl Pts',(7.22555226126606,-30.5182670768337,
123.103998979536));
#135408=CARTESIAN_POINT('Ctrl Pts',(7.33668753210462,-28.6881764049717,
123.536258394322));
#135409=CARTESIAN_POINT('Ctrl Pts',(7.44782280294318,-28.0587609143225,
125.308239266059));
#135410=CARTESIAN_POINT('Ctrl Pts',(7.55895807378174,-29.2061068726125,
126.798097420642));
#135411=CARTESIAN_POINT('Ctrl Pts',(7.6700933446203,-31.0800808453102,126.642207660685));
#135412=CARTESIAN_POINT('Ctrl Pts',(7.78122861545886,-31.9654872479834,
124.983251490096));
#135413=CARTESIAN_POINT('Ctrl Pts',(7.89236388629742,-31.0519385402995,
123.339624761284));
#135414=CARTESIAN_POINT('Ctrl Pts',(8.00349915713598,-29.1755801242742,
123.215692709229));
#135415=CARTESIAN_POINT('Ctrl Pts',(8.11463442797453,-28.0537899886445,
124.724886865103));
#135416=CARTESIAN_POINT('Ctrl Pts',(8.2257696988131,-28.7133110646225,126.485884302567));
#135417=CARTESIAN_POINT('Ctrl Pts',(8.33690496965165,-30.5505022463529,
126.886893738269));
#135418=CARTESIAN_POINT('Ctrl Pts',(8.44804024049022,-31.8838342901685,
125.560882406281));
#135419=CARTESIAN_POINT('Ctrl Pts',(8.55917551132877,-31.4929457558537,
123.721511379461));
#135420=CARTESIAN_POINT('Ctrl Pts',(8.67031078216733,-29.7356062750041,
123.052304624424));
#135421=CARTESIAN_POINT('Ctrl Pts',(8.78144605300589,-28.220258423856,124.165769279955));
#135422=CARTESIAN_POINT('Ctrl Pts',(8.89258132384446,-28.3338589101122,
126.042780391858));
#135423=CARTESIAN_POINT('Ctrl Pts',(9.00371659468301,-29.9724293548191,
126.965366863976));
#135424=CARTESIAN_POINT('Ctrl Pts',(9.11485186552158,-31.6362385744073,
126.089102586015));
#135425=CARTESIAN_POINT('Ctrl Pts',(9.22598713636013,-31.8024363376022,
124.216025188734));
#135426=CARTESIAN_POINT('Ctrl Pts',(9.3371224071987,-30.3189318736382,123.060473962851));
#135427=CARTESIAN_POINT('Ctrl Pts',(9.44825767803725,-28.5434836732957,
123.680164653635));
#135428=CARTESIAN_POINT('Ctrl Pts',(9.55939294887581,-28.1012134484641,
125.507765501478));
#135429=CARTESIAN_POINT('Ctrl Pts',(9.67052821971438,-29.3967080968805,
126.870821247227));
#135430=CARTESIAN_POINT('Ctrl Pts',(9.78166349055292,-31.2446643127262,
126.521165324413));
#135431=CARTESIAN_POINT('Ctrl Pts',(9.89279876139149,-31.9528358863139,
124.780043235528));
#135432=CARTESIAN_POINT('Ctrl Pts',(10.00393403223,-30.8748102268758,123.238590758769));
#135433=CARTESIAN_POINT('Ctrl Pts',(10.1150693030686,-28.9936519546155,
123.312692143422));
#135434=CARTESIAN_POINT('Ctrl Pts',(10.1891594836276,-28.3583796691399,
124.386603429246));
#135435=CARTESIAN_POINT('Ctrl Pts',(10.2262045739072,-28.3381599574103,
124.939191754379));
#135436=CARTESIAN_POINT('Ctrl Pts',(-0.0741753502519805,-31.3664757556195,
126.163031592958));
#135437=CARTESIAN_POINT('Ctrl Pts',(-0.0371171905957929,-31.7533538665377,
125.708504405161));
#135438=CARTESIAN_POINT('Ctrl Pts',(0.0369860593399143,-32.0305744835093,
124.390626990756));
#135439=CARTESIAN_POINT('Ctrl Pts',(0.148134399555141,-30.5872809378495,
122.960728224503));
#135440=CARTESIAN_POINT('Ctrl Pts',(0.259269670393701,-28.6061130165961,
123.401960524163));
#135441=CARTESIAN_POINT('Ctrl Pts',(0.37040494123226,-27.9009954898912,
125.303660990775));
#135442=CARTESIAN_POINT('Ctrl Pts',(0.481540212070819,-29.1169051741997,
126.928498123382));
#135443=CARTESIAN_POINT('Ctrl Pts',(0.59267548290938,-31.1411521704481,
126.787707545708));
#135444=CARTESIAN_POINT('Ctrl Pts',(0.703810753747938,-32.1209023824778,
125.010939194675));
#135445=CARTESIAN_POINT('Ctrl Pts',(0.814946024586498,-31.1594663672247,
123.224029824376));
#135446=CARTESIAN_POINT('Ctrl Pts',(0.926081295425056,-29.1367955598828,
123.062679472607));
#135447=CARTESIAN_POINT('Ctrl Pts',(1.03721656626361,-27.9041953553674,
124.67447264186));
#135448=CARTESIAN_POINT('Ctrl Pts',(1.14835183710217,-28.5898241774735,
126.584227328894));
#135449=CARTESIAN_POINT('Ctrl Pts',(1.25948710794074,-30.5661481541757,
127.043975717818));
#135450=CARTESIAN_POINT('Ctrl Pts',(1.37062237877929,-32.0242922050491,
125.632934492105));
#135451=CARTESIAN_POINT('Ctrl Pts',(1.48175764961785,-31.6296588584181,
123.642584289743));
#135452=CARTESIAN_POINT('Ctrl Pts',(1.59289292045641,-29.7434445531617,
122.894639369055));
#135453=CARTESIAN_POINT('Ctrl Pts',(1.70402819129497,-28.0920482775119,
124.073671268887));
#135454=CARTESIAN_POINT('Ctrl Pts',(1.81516346213353,-28.1869464368915,
126.100545985585));
#135455=CARTESIAN_POINT('Ctrl Pts',(1.92629873297209,-29.9412814610682,
127.120121854019));
#135456=CARTESIAN_POINT('Ctrl Pts',(2.03743400381065,-31.7493599029718,
126.19920996996));
#135457=CARTESIAN_POINT('Ctrl Pts',(2.14856927464921,-31.9562985100362,
124.180694956115));
#135458=CARTESIAN_POINT('Ctrl Pts',(2.25970454548777,-30.3726921998356,
122.91206678177));
#135459=CARTESIAN_POINT('Ctrl Pts',(2.37083981632633,-28.4479712190086,
123.554465056575));
#135460=CARTESIAN_POINT('Ctrl Pts',(2.48197508716489,-27.9437784590173,
125.519920746379));
#135461=CARTESIAN_POINT('Ctrl Pts',(2.59311035800345,-29.3215873501379,
127.009507622032));
#135462=CARTESIAN_POINT('Ctrl Pts',(2.70424562884201,-31.320328228104,126.659848781613));
#135463=CARTESIAN_POINT('Ctrl Pts',(2.81538089968056,-32.11060987373,124.790977110375));
#135464=CARTESIAN_POINT('Ctrl Pts',(2.92651617051912,-30.9691097596231,
123.113418201847));
#135465=CARTESIAN_POINT('Ctrl Pts',(3.03765144135768,-28.9406107832101,
123.162594466423));
#135466=CARTESIAN_POINT('Ctrl Pts',(3.14878671219624,-27.8817409130031,
124.893496254617));
#135467=CARTESIAN_POINT('Ctrl Pts',(3.2599219830348,-28.7616539119262,126.721877920633));
#135468=CARTESIAN_POINT('Ctrl Pts',(3.37105725387336,-30.7749901999753,
126.974273232704));
#135469=CARTESIAN_POINT('Ctrl Pts',(3.48219252471192,-32.0789997901358,
125.41967187187));
#135470=CARTESIAN_POINT('Ctrl Pts',(3.59332779555048,-31.4801594396173,
123.480956669238));
#135471=CARTESIAN_POINT('Ctrl Pts',(3.70446306638904,-29.5265708513964,
122.932579034479));
#135472=CARTESIAN_POINT('Ctrl Pts',(3.8155983372276,-28.0062986259812,124.276453568415));
#135473=CARTESIAN_POINT('Ctrl Pts',(3.92673360806616,-28.3108051039036,
126.282569768248));
#135474=CARTESIAN_POINT('Ctrl Pts',(4.03786887890472,-30.1613840841332,
127.11478599031));
#135475=CARTESIAN_POINT('Ctrl Pts',(4.14900414974328,-31.8642527584858,
126.011398170802));
#135476=CARTESIAN_POINT('Ctrl Pts',(4.26013942058184,-31.8608234006184,
123.982306097525));
#135477=CARTESIAN_POINT('Ctrl Pts',(4.37127469142039,-30.1542348051788,
122.884680583861));
#135478=CARTESIAN_POINT('Ctrl Pts',(4.48240996225896,-28.3064794374878,
123.723147341401));
#135479=CARTESIAN_POINT('Ctrl Pts',(4.59354523309752,-28.0087557327167,
125.730281367306));
#135480=CARTESIAN_POINT('Ctrl Pts',(4.70468050393607,-29.5335618107069,
127.069009430378));
#135481=CARTESIAN_POINT('Ctrl Pts',(4.81581577477464,-31.4852856233874,
126.51403144762));
#135482=CARTESIAN_POINT('Ctrl Pts',(4.92695104561319,-32.0775693467696,
124.573303132439));
#135483=CARTESIAN_POINT('Ctrl Pts',(5.03808631645175,-30.7683123739893,
123.023118439714));
#135484=CARTESIAN_POINT('Ctrl Pts',(5.14922158729032,-28.7558407293246,
123.282317748647));
#135485=CARTESIAN_POINT('Ctrl Pts',(5.26035685812887,-27.8821130160601,
125.11366323364));
#135486=CARTESIAN_POINT('Ctrl Pts',(5.37149212896743,-28.946827596477,126.840975962874));
#135487=CARTESIAN_POINT('Ctrl Pts',(5.48262739980599,-30.9754812090559,
126.883295255185));
#135488=CARTESIAN_POINT('Ctrl Pts',(5.59376267064455,-32.1113043511401,
125.20188745449));
#135489=CARTESIAN_POINT('Ctrl Pts',(5.70489794148311,-31.3147100979059,
123.335697754046));
#135490=CARTESIAN_POINT('Ctrl Pts',(5.81603321232167,-29.3147987285858,
122.992797014481));
#135491=CARTESIAN_POINT('Ctrl Pts',(5.92716848316023,-27.942032780275,124.487032622907));
#135492=CARTESIAN_POINT('Ctrl Pts',(6.03830375399879,-28.4528662534518,
126.45077282085));
#135493=CARTESIAN_POINT('Ctrl Pts',(6.14943902483735,-30.3797476607406,
127.0866615254));
#135494=CARTESIAN_POINT('Ctrl Pts',(6.26057429567591,-31.9590567319754,
125.812687718823));
#135495=CARTESIAN_POINT('Ctrl Pts',(6.37170956651447,-31.7452963647656,
123.794883737326));
#135496=CARTESIAN_POINT('Ctrl Pts',(6.48284483735302,-29.9341154014023,
122.880088721882));
#135497=CARTESIAN_POINT('Ctrl Pts',(6.59398010819159,-28.1832367551099,
123.905588779554));
#135498=CARTESIAN_POINT('Ctrl Pts',(6.70511537903014,-28.0951903270626,
125.932772596785));
#135499=CARTESIAN_POINT('Ctrl Pts',(6.81625064986871,-29.7505625325129,
127.10621593319));
#135500=CARTESIAN_POINT('Ctrl Pts',(6.92738592070726,-31.6342378250768,
126.35189915989));
#135501=CARTESIAN_POINT('Ctrl Pts',(7.03852119154583,-32.0221412742628,
124.360227169699));
#135502=CARTESIAN_POINT('Ctrl Pts',(7.14965646238439,-30.5592357805672,
122.954121228164));
#135503=CARTESIAN_POINT('Ctrl Pts',(7.26079173322294,-28.5844775311327,
123.420550492226));
#135504=CARTESIAN_POINT('Ctrl Pts',(7.37192700406151,-27.90530712084,125.332605396447));
#135505=CARTESIAN_POINT('Ctrl Pts',(7.48306227490006,-29.1433500937509,
126.94023595076));
#135506=CARTESIAN_POINT('Ctrl Pts',(7.59419754573863,-31.1654605928145,
126.772023198131));
#135507=CARTESIAN_POINT('Ctrl Pts',(7.70533281657718,-32.1208578442534,
124.981927530364));
#135508=CARTESIAN_POINT('Ctrl Pts',(7.81646808741574,-31.1350936553549,
123.208373087617));
#135509=CARTESIAN_POINT('Ctrl Pts',(7.9276033582543,-29.1104102241388,123.074644280663));
#135510=CARTESIAN_POINT('Ctrl Pts',(8.03873862909285,-27.8999432464479,
124.703139335652));
#135511=CARTESIAN_POINT('Ctrl Pts',(8.14987389993142,-28.6115990706583,
126.603342571663));
#135512=CARTESIAN_POINT('Ctrl Pts',(8.26100917076997,-30.594019121037,127.036051564408));
#135513=CARTESIAN_POINT('Ctrl Pts',(8.37214444160854,-32.0327502687575,
125.605219826424));
#135514=CARTESIAN_POINT('Ctrl Pts',(8.48327971244709,-31.6109622286261,
123.620447615501));
#135515=CARTESIAN_POINT('Ctrl Pts',(8.59441498328566,-29.7147061085213,
122.898340465071));
#135516=CARTESIAN_POINT('Ctrl Pts',(8.70555025412421,-28.079570912311,124.09982383842));
#135517=CARTESIAN_POINT('Ctrl Pts',(8.81668552496278,-28.2021514493431,
126.125211560733));
#135518=CARTESIAN_POINT('Ctrl Pts',(8.92782079580133,-29.9702499117393,
127.120727943962));
#135519=CARTESIAN_POINT('Ctrl Pts',(9.03895606663989,-31.7655822591382,
126.175195496748));
#135520=CARTESIAN_POINT('Ctrl Pts',(9.15009133747845,-31.9449178565231,
124.154052446854));
#135521=CARTESIAN_POINT('Ctrl Pts',(9.26122660831701,-30.3441432482872,
122.907155584834));
#135522=CARTESIAN_POINT('Ctrl Pts',(9.37236187915557,-28.4283469251996,
123.575832455625));
#135523=CARTESIAN_POINT('Ctrl Pts',(9.48349714999413,-27.9511155025199,
125.547904061935));
#135524=CARTESIAN_POINT('Ctrl Pts',(9.59463242083269,-29.3490182312716,
127.018708552522));
#135525=CARTESIAN_POINT('Ctrl Pts',(9.70576769167125,-31.3430542853006,
126.641412537272));
#135526=CARTESIAN_POINT('Ctrl Pts',(9.81690296250981,-32.1072063999793,
124.762655784306));
#135527=CARTESIAN_POINT('Ctrl Pts',(9.92803823334836,-30.9439634542561,
123.09935240738));
#135528=CARTESIAN_POINT('Ctrl Pts',(10.0391735041869,-28.9141007410287,
123.179311462354));
#135529=CARTESIAN_POINT('Ctrl Pts',(10.113263684746,-28.2286105597669,124.338114795679));
#135530=CARTESIAN_POINT('Ctrl Pts',(10.1503087750255,-28.2067924918683,
124.934384898781));
#135531=CARTESIAN_POINT('Ctrl Pts',(-0.150071149133654,-31.4665815470164,
126.248233395883));
#135532=CARTESIAN_POINT('Ctrl Pts',(-0.113012989477467,-31.8818017191152,
125.760408285559));
#135533=CARTESIAN_POINT('Ctrl Pts',(-0.0389097395417594,-32.1793310676097,
124.345985315194));
#135534=CARTESIAN_POINT('Ctrl Pts',(0.0722386006734674,-30.6303041841925,
122.811334490936));
#135535=CARTESIAN_POINT('Ctrl Pts',(0.183373871512027,-28.5039991232338,
123.284890751242));
#135536=CARTESIAN_POINT('Ctrl Pts',(0.294509142350586,-27.747225833338,
125.32590670108));
#135537=CARTESIAN_POINT('Ctrl Pts',(0.405644413189146,-29.0522110835422,
127.069776759358));
#135538=CARTESIAN_POINT('Ctrl Pts',(0.516779684027705,-31.2247511224655,
126.918672092948));
#135539=CARTESIAN_POINT('Ctrl Pts',(0.627914954866265,-32.2762762415459,
125.011740582285));
#135540=CARTESIAN_POINT('Ctrl Pts',(0.739050225704823,-31.2444069875114,
123.093925137778));
#135541=CARTESIAN_POINT('Ctrl Pts',(0.850185496543384,-29.0735586065304,
122.920754521663));
#135542=CARTESIAN_POINT('Ctrl Pts',(0.961320767381941,-27.7506601157544,
124.650625037046));
#135543=CARTESIAN_POINT('Ctrl Pts',(1.07245603822051,-28.4865169902498,
126.700285246394));
#135544=CARTESIAN_POINT('Ctrl Pts',(1.18359130905906,-30.6076232471574,
127.193714054548));
#135545=CARTESIAN_POINT('Ctrl Pts',(1.29472657989762,-32.1725885596471,
125.679302243581));
#135546=CARTESIAN_POINT('Ctrl Pts',(1.40586185073618,-31.7490450158803,
123.543142222534));
#135547=CARTESIAN_POINT('Ctrl Pts',(1.51699712157474,-29.7246497183924,
122.740404073427));
#135548=CARTESIAN_POINT('Ctrl Pts',(1.6281323924133,-27.9522748374482,124.005809932643));
#135549=CARTESIAN_POINT('Ctrl Pts',(1.73926766325186,-28.0541250816399,
126.181170194542));
#135550=CARTESIAN_POINT('Ctrl Pts',(1.85040293409042,-29.9369798364069,
127.275438532842));
#135551=CARTESIAN_POINT('Ctrl Pts',(1.96153820492898,-31.8775151642743,
126.287062141943));
#135552=CARTESIAN_POINT('Ctrl Pts',(2.07267347576754,-32.0996137571237,
124.120674001133));
#135553=CARTESIAN_POINT('Ctrl Pts',(2.1838087466061,-30.3999950242426,122.759108190054));
#135554=CARTESIAN_POINT('Ctrl Pts',(2.29494401744466,-28.3342721147596,
123.448567517662));
#135555=CARTESIAN_POINT('Ctrl Pts',(2.40607928828322,-27.7931430131993,
125.55800929465));
#135556=CARTESIAN_POINT('Ctrl Pts',(2.51721455912178,-29.2718879427911,
127.156720882125));
#135557=CARTESIAN_POINT('Ctrl Pts',(2.62834982996034,-31.4170533266902,
126.781446603746));
#135558=CARTESIAN_POINT('Ctrl Pts',(2.7394851007989,-32.265229720347,124.775664433439));
#135559=CARTESIAN_POINT('Ctrl Pts',(2.85062037163745,-31.0401051644362,
122.975210287685));
#135560=CARTESIAN_POINT('Ctrl Pts',(2.96175564247602,-28.863001652197,123.027989125423));
#135561=CARTESIAN_POINT('Ctrl Pts',(3.07289091331457,-27.726560697463,124.88569396345));
#135562=CARTESIAN_POINT('Ctrl Pts',(3.18402618415313,-28.6709346915815,
126.848019896607));
#135563=CARTESIAN_POINT('Ctrl Pts',(3.2951614549917,-30.831764721568,127.11890527874));
#135564=CARTESIAN_POINT('Ctrl Pts',(3.40629672583025,-32.2313039334398,
125.450416350642));
#135565=CARTESIAN_POINT('Ctrl Pts',(3.51743199666881,-31.5885935128067,
123.369674025424));
#135566=CARTESIAN_POINT('Ctrl Pts',(3.62856726750737,-29.491888201963,122.781123137034));
#135567=CARTESIAN_POINT('Ctrl Pts',(3.73970253834593,-27.8602433059111,
124.223447733626));
#135568=CARTESIAN_POINT('Ctrl Pts',(3.85083780918449,-28.1870574331513,
126.376528743476));
#135569=CARTESIAN_POINT('Ctrl Pts',(3.96197308002305,-30.173206819659,127.269711772436));
#135570=CARTESIAN_POINT('Ctrl Pts',(4.07310835086161,-32.0008248835195,
126.085491555839));
#135571=CARTESIAN_POINT('Ctrl Pts',(4.18424362170017,-31.9971442964722,
123.907751497425));
#135572=CARTESIAN_POINT('Ctrl Pts',(4.29537889253873,-30.165533796156,122.729715723827));
#135573=CARTESIAN_POINT('Ctrl Pts',(4.40651416337728,-28.1824148754493,
123.629607192327));
#135574=CARTESIAN_POINT('Ctrl Pts',(4.51764943421585,-27.8628804162897,
125.783780592533));
#135575=CARTESIAN_POINT('Ctrl Pts',(4.6287847050544,-29.4993913075824,127.220581696175));
#135576=CARTESIAN_POINT('Ctrl Pts',(4.73991997589297,-31.5940952324625,
126.624946929026));
#135577=CARTESIAN_POINT('Ctrl Pts',(4.85105524673152,-32.2297686981192,
124.542044013908));
#135578=CARTESIAN_POINT('Ctrl Pts',(4.96219051757009,-30.8245976889112,
122.878295311842));
#135579=CARTESIAN_POINT('Ctrl Pts',(5.07332578840864,-28.6646956446771,
123.156483140581));
#135580=CARTESIAN_POINT('Ctrl Pts',(5.1844610592472,-27.7269600601847,125.121990017272));
#135581=CARTESIAN_POINT('Ctrl Pts',(5.29559633008576,-28.8696738990929,
126.975842867719));
#135582=CARTESIAN_POINT('Ctrl Pts',(5.40673160092433,-31.0469433758917,
127.021262402556));
#135583=CARTESIAN_POINT('Ctrl Pts',(5.51786687176288,-32.2659750740426,
125.216677401053));
#135584=CARTESIAN_POINT('Ctrl Pts',(5.62900214260144,-31.4110236214113,
123.213773678358));
#135585=CARTESIAN_POINT('Ctrl Pts',(5.74013741344,-29.2646019978652,122.845752588311));
#135586=CARTESIAN_POINT('Ctrl Pts',(5.85127268427856,-27.7912694488716,
124.44945346716));
#135587=CARTESIAN_POINT('Ctrl Pts',(5.96240795511712,-28.3395257514648,
126.557054078143));
#135588=CARTESIAN_POINT('Ctrl Pts',(6.07354322595567,-30.4075673567382,
127.239526954969));
#135589=CARTESIAN_POINT('Ctrl Pts',(6.18467849679424,-32.1025740419161,
125.872223899334));
#135590=CARTESIAN_POINT('Ctrl Pts',(6.2958137676328,-31.8731539378682,123.706598879945));
#135591=CARTESIAN_POINT('Ctrl Pts',(6.40694903847135,-29.9292888028649,
122.724787469508));
#135592=CARTESIAN_POINT('Ctrl Pts',(6.51808430930992,-28.0501436346044,
123.825413993513));
#135593=CARTESIAN_POINT('Ctrl Pts',(6.62921958014847,-27.9556470684387,
126.001106000148));
#135594=CARTESIAN_POINT('Ctrl Pts',(6.74035485098703,-29.7322891493341,
127.260513886869));
#135595=CARTESIAN_POINT('Ctrl Pts',(6.85149012182559,-31.7539594301893,
126.450937093592));
#135596=CARTESIAN_POINT('Ctrl Pts',(6.96262539266416,-32.1702800551697,
124.313358452689));
#135597=CARTESIAN_POINT('Ctrl Pts',(7.07376066350271,-30.6002044843009,
122.804243476792));
#135598=CARTESIAN_POINT('Ctrl Pts',(7.18489593434127,-28.4807786572938,
123.304842590131));
#135599=CARTESIAN_POINT('Ctrl Pts',(7.29603120517984,-27.7518533273575,
125.356971526835));
#135600=CARTESIAN_POINT('Ctrl Pts',(7.40716647601839,-29.0805933148894,
127.08237448088));
#135601=CARTESIAN_POINT('Ctrl Pts',(7.51830174685695,-31.2508403403189,
126.901838735577));
#135602=CARTESIAN_POINT('Ctrl Pts',(7.62943701769551,-32.2762284405235,
124.980603570633));
#135603=CARTESIAN_POINT('Ctrl Pts',(7.74057228853406,-31.2182487704101,
123.077121413948));
#135604=CARTESIAN_POINT('Ctrl Pts',(7.85170755937263,-29.0452403240035,
122.933595852095));
#135605=CARTESIAN_POINT('Ctrl Pts',(7.96284283021118,-27.7460965042514,
124.681391806202));
#135606=CARTESIAN_POINT('Ctrl Pts',(8.07397810104976,-28.509887076694,126.720800840759));
#135607=CARTESIAN_POINT('Ctrl Pts',(8.1851133718883,-30.6375359957213,127.185209390547));
#135608=CARTESIAN_POINT('Ctrl Pts',(8.29624864272688,-32.1816662473463,
125.649557246568));
#135609=CARTESIAN_POINT('Ctrl Pts',(8.40738391356542,-31.7289787013983,
123.51938385154));
#135610=CARTESIAN_POINT('Ctrl Pts',(8.51851918440399,-29.6938059420385,
122.744376305717));
#135611=CARTESIAN_POINT('Ctrl Pts',(8.62965445524254,-27.9388834007661,
124.033878396884));
#135612=CARTESIAN_POINT('Ctrl Pts',(8.74078972608111,-28.070443988574,126.207642729609));
#135613=CARTESIAN_POINT('Ctrl Pts',(8.85192499691966,-29.9680704686594,
127.276089023948));
#135614=CARTESIAN_POINT('Ctrl Pts',(8.96306026775823,-31.8949259438691,
126.261288407482));
#135615=CARTESIAN_POINT('Ctrl Pts',(9.07419553859677,-32.0873993754438,
124.092079704975));
#135616=CARTESIAN_POINT('Ctrl Pts',(9.18533080943535,-30.3693546229362,
122.753837206818));
#135617=CARTESIAN_POINT('Ctrl Pts',(9.2964660802739,-28.3132101771035,123.471500257614));
#135618=CARTESIAN_POINT('Ctrl Pts',(9.40760135111246,-27.8010175565758,
125.588042622392));
#135619=CARTESIAN_POINT('Ctrl Pts',(9.51873662195103,-29.3013283656625,
127.166595857817));
#135620=CARTESIAN_POINT('Ctrl Pts',(9.62987189278957,-31.4414442578748,
126.76165975013));
#135621=CARTESIAN_POINT('Ctrl Pts',(9.74100716362815,-32.2615769136449,
124.745268333085));
#135622=CARTESIAN_POINT('Ctrl Pts',(9.85214243446669,-31.0131166816364,
122.960114055991));
#135623=CARTESIAN_POINT('Ctrl Pts',(9.96327770530527,-28.8345495274418,
123.045930781285));
#135624=CARTESIAN_POINT('Ctrl Pts',(10.0373678858643,-28.0988414503939,
124.289626162113));
#135625=CARTESIAN_POINT('Ctrl Pts',(10.0744129761438,-28.0754250263263,
124.929578043184));
#135626=CARTESIAN_POINT('Ctrl Pts',(-0.225966948015328,-31.5666873384132,
126.333435198808));
#135627=CARTESIAN_POINT('Ctrl Pts',(-0.188908788359141,-32.0102495716926,
125.812312165957));
#135628=CARTESIAN_POINT('Ctrl Pts',(-0.114805538423433,-32.3280876517101,
124.301343639632));
#135629=CARTESIAN_POINT('Ctrl Pts',(-0.00365719820820642,-30.6733274305354,
122.661940757371));
#135630=CARTESIAN_POINT('Ctrl Pts',(0.107478072630353,-28.4018852298716,
123.167820978322));
#135631=CARTESIAN_POINT('Ctrl Pts',(0.218613343468912,-27.5934561767846,
125.348152411385));
#135632=CARTESIAN_POINT('Ctrl Pts',(0.329748614307472,-28.9875169928847,
127.211055395334));
#135633=CARTESIAN_POINT('Ctrl Pts',(0.440883885146031,-31.3083500744829,
127.049636640188));
#135634=CARTESIAN_POINT('Ctrl Pts',(0.55201915598459,-32.4316501006138,
125.012541969895));
#135635=CARTESIAN_POINT('Ctrl Pts',(0.66315442682315,-31.329347607798,122.963820451181));
#135636=CARTESIAN_POINT('Ctrl Pts',(0.77428969766171,-29.0103216531781,
122.778829570717));
#135637=CARTESIAN_POINT('Ctrl Pts',(0.885424968500269,-27.5971248761416,
124.626777432233));
#135638=CARTESIAN_POINT('Ctrl Pts',(0.996560239338828,-28.3832098030258,
126.816343163895));
#135639=CARTESIAN_POINT('Ctrl Pts',(1.10769551017739,-30.6490983401391,
127.343452391279));
#135640=CARTESIAN_POINT('Ctrl Pts',(1.21883078101594,-32.3208849142452,
125.725669995058));
#135641=CARTESIAN_POINT('Ctrl Pts',(1.3299660518545,-31.8684311733427,123.443700155325));
#135642=CARTESIAN_POINT('Ctrl Pts',(1.44110132269306,-29.7058548836233,
122.586168777798));
#135643=CARTESIAN_POINT('Ctrl Pts',(1.55223659353162,-27.8125013973844,
123.937948596399));
#135644=CARTESIAN_POINT('Ctrl Pts',(1.66337186437018,-27.9213037263882,
126.261794403498));
#135645=CARTESIAN_POINT('Ctrl Pts',(1.77450713520874,-29.9326782117456,
127.430755211664));
#135646=CARTESIAN_POINT('Ctrl Pts',(1.8856424060473,-32.0056704255768,126.374914313927));
#135647=CARTESIAN_POINT('Ctrl Pts',(1.99677767688586,-32.2429290042112,
124.06065304615));
#135648=CARTESIAN_POINT('Ctrl Pts',(2.10791294772442,-30.4272978486494,
122.606149598337));
#135649=CARTESIAN_POINT('Ctrl Pts',(2.21904821856298,-28.2205730105108,
123.34266997875));
#135650=CARTESIAN_POINT('Ctrl Pts',(2.33018348940154,-27.6425075673812,
125.596097842922));
#135651=CARTESIAN_POINT('Ctrl Pts',(2.4413187602401,-29.2221885354442,127.303934142217));
#135652=CARTESIAN_POINT('Ctrl Pts',(2.55245403107866,-31.5137784252764,
126.903044425881));
#135653=CARTESIAN_POINT('Ctrl Pts',(2.66358930191722,-32.4198495669641,
124.760351756503));
#135654=CARTESIAN_POINT('Ctrl Pts',(2.77472457275578,-31.1111005692493,
122.837002373521));
#135655=CARTESIAN_POINT('Ctrl Pts',(2.88585984359434,-28.7853925211838,
122.893383784421));
#135656=CARTESIAN_POINT('Ctrl Pts',(2.99699511443289,-27.5713804819229,
124.877891672283));
#135657=CARTESIAN_POINT('Ctrl Pts',(3.10813038527145,-28.5802154712366,
126.97416187258));
#135658=CARTESIAN_POINT('Ctrl Pts',(3.21926565611002,-30.8885392431607,
127.263537324776));
#135659=CARTESIAN_POINT('Ctrl Pts',(3.33040092694857,-32.3836080767439,
125.481160829412));
#135660=CARTESIAN_POINT('Ctrl Pts',(3.44153619778713,-31.6970275859962,
123.258391381611));
#135661=CARTESIAN_POINT('Ctrl Pts',(3.55267146862569,-29.4572055525297,
122.629667239589));
#135662=CARTESIAN_POINT('Ctrl Pts',(3.66380673946425,-27.7141879858409,
124.170441898836));
#135663=CARTESIAN_POINT('Ctrl Pts',(3.77494201030281,-28.0633097623991,
126.470487718705));
#135664=CARTESIAN_POINT('Ctrl Pts',(3.88607728114137,-30.1850295551847,
127.424637554561));
#135665=CARTESIAN_POINT('Ctrl Pts',(3.99721255197993,-32.1373970085532,
126.159584940877));
#135666=CARTESIAN_POINT('Ctrl Pts',(4.10834782281849,-32.1334651923261,
123.833196897325));
#135667=CARTESIAN_POINT('Ctrl Pts',(4.21948309365705,-30.1768327871333,
122.574750863792));
#135668=CARTESIAN_POINT('Ctrl Pts',(4.33061836449561,-28.0583503134108,
123.536067043254));
#135669=CARTESIAN_POINT('Ctrl Pts',(4.44175363533417,-27.7170050998627,
125.83727981776));
#135670=CARTESIAN_POINT('Ctrl Pts',(4.55288890617273,-29.4652208044579,
127.372153961972));
#135671=CARTESIAN_POINT('Ctrl Pts',(4.66402417701129,-31.7029048415377,
126.735862410431));
#135672=CARTESIAN_POINT('Ctrl Pts',(4.77515944784984,-32.3819680494687,
124.510784895378));
#135673=CARTESIAN_POINT('Ctrl Pts',(4.88629471868841,-30.8808830038331,
122.733472183969));
#135674=CARTESIAN_POINT('Ctrl Pts',(4.99742998952697,-28.5735505600296,
123.030648532515));
#135675=CARTESIAN_POINT('Ctrl Pts',(5.10856526036552,-27.5718071043093,
125.130316800904));
#135676=CARTESIAN_POINT('Ctrl Pts',(5.21970053120408,-28.7925202017086,
127.110709772564));
#135677=CARTESIAN_POINT('Ctrl Pts',(5.33083580204264,-31.1184055427276,
127.159229549927));
#135678=CARTESIAN_POINT('Ctrl Pts',(5.4419710728812,-32.4206457969451,125.231467347616));
#135679=CARTESIAN_POINT('Ctrl Pts',(5.55310634371976,-31.5073371449166,
123.091849602668));
#135680=CARTESIAN_POINT('Ctrl Pts',(5.66424161455832,-29.2144052671446,
122.698708162142));
#135681=CARTESIAN_POINT('Ctrl Pts',(5.77537688539688,-27.6405061174681,
124.411874311414));
#135682=CARTESIAN_POINT('Ctrl Pts',(5.88651215623544,-28.2261852494778,
126.663335335437));
#135683=CARTESIAN_POINT('Ctrl Pts',(5.997647427074,-30.435387052736,127.392392384537));
#135684=CARTESIAN_POINT('Ctrl Pts',(6.10878269791256,-32.2460913518569,
125.931760079845));
#135685=CARTESIAN_POINT('Ctrl Pts',(6.21991796875111,-32.0010115109706,
123.618314022564));
#135686=CARTESIAN_POINT('Ctrl Pts',(6.33105323958968,-29.9244622043275,
122.569486217133));
#135687=CARTESIAN_POINT('Ctrl Pts',(6.44218851042824,-27.9170505140989,
123.745239207473));
#135688=CARTESIAN_POINT('Ctrl Pts',(6.55332378126679,-27.8161038098147,
126.069439403511));
#135689=CARTESIAN_POINT('Ctrl Pts',(6.66445905210537,-29.7140157661554,
127.414811840549));
#135690=CARTESIAN_POINT('Ctrl Pts',(6.77559432294391,-31.8736810353017,
126.549975027294));
#135691=CARTESIAN_POINT('Ctrl Pts',(6.88672959378247,-32.3184188360767,
124.266489735679));
#135692=CARTESIAN_POINT('Ctrl Pts',(6.99786486462104,-30.6411731880345,
122.65436572542));
#135693=CARTESIAN_POINT('Ctrl Pts',(7.10900013545958,-28.3770797834548,
123.189134688036));
#135694=CARTESIAN_POINT('Ctrl Pts',(7.22013540629817,-27.598399533875,125.381337657224));
#135695=CARTESIAN_POINT('Ctrl Pts',(7.3312706771367,-29.0178365360278,127.224513010999));
#135696=CARTESIAN_POINT('Ctrl Pts',(7.44240594797528,-31.3362200878231,
127.031654273023));
#135697=CARTESIAN_POINT('Ctrl Pts',(7.55354121881383,-32.4315990367936,
124.9792796109));
#135698=CARTESIAN_POINT('Ctrl Pts',(7.66467648965239,-31.3014038854654,
122.94586974028));
#135699=CARTESIAN_POINT('Ctrl Pts',(7.77581176049095,-28.980070423868,122.792547423528));
#135700=CARTESIAN_POINT('Ctrl Pts',(7.88694703132951,-27.5922497620548,
124.65964427675));
#135701=CARTESIAN_POINT('Ctrl Pts',(7.99808230216807,-28.4081750827298,
126.838259109854));
#135702=CARTESIAN_POINT('Ctrl Pts',(8.10921757300663,-30.6810528704055,
127.334367216686));
#135703=CARTESIAN_POINT('Ctrl Pts',(8.22035284384519,-32.3305822259353,
125.693894666712));
#135704=CARTESIAN_POINT('Ctrl Pts',(8.33148811468374,-31.8469951741706,
123.41832008758));
#135705=CARTESIAN_POINT('Ctrl Pts',(8.44262338552231,-29.6729057755557,
122.590412146364));
#135706=CARTESIAN_POINT('Ctrl Pts',(8.55375865636087,-27.798195889221,123.967932955349));
#135707=CARTESIAN_POINT('Ctrl Pts',(8.66489392719942,-27.9387365278048,
126.290073898485));
#135708=CARTESIAN_POINT('Ctrl Pts',(8.77602919803799,-29.9658910255794,
127.431450103935));
#135709=CARTESIAN_POINT('Ctrl Pts',(8.88716446887655,-32.0242696285999,
126.347381318216));
#135710=CARTESIAN_POINT('Ctrl Pts',(8.9982997397151,-32.2298808943646,124.030106963096));
#135711=CARTESIAN_POINT('Ctrl Pts',(9.10943501055366,-30.3945659975851,
122.600518828802));
#135712=CARTESIAN_POINT('Ctrl Pts',(9.22057028139223,-28.1980734290074,
123.367168059605));
#135713=CARTESIAN_POINT('Ctrl Pts',(9.33170555223079,-27.6509196106317,
125.628181182848));
#135714=CARTESIAN_POINT('Ctrl Pts',(9.44284082306934,-29.2536385000535,
127.314483163113));
#135715=CARTESIAN_POINT('Ctrl Pts',(9.5539760939079,-31.5398342304492,126.881906962989));
#135716=CARTESIAN_POINT('Ctrl Pts',(9.66511136474646,-32.4159474273104,
124.727880881864));
#135717=CARTESIAN_POINT('Ctrl Pts',(9.77624663558503,-31.0822699090167,
122.820875704601));
#135718=CARTESIAN_POINT('Ctrl Pts',(9.88738190642358,-28.7549983138549,
122.912550100216));
#135719=CARTESIAN_POINT('Ctrl Pts',(9.96147208698262,-27.9690723410208,
124.241137528545));
#135720=CARTESIAN_POINT('Ctrl Pts',(9.99851717726214,-27.9440575607844,
124.924771187586));
#135721=CARTESIAN_POINT('',(10.0008700344079,-30.7705824472418,123.521224995955));
#135722=CARTESIAN_POINT('Ctrl Pts',(10.,-27.9466241674713,124.92486510207));
#135723=CARTESIAN_POINT('Ctrl Pts',(10.,-27.9563161184906,124.850853981395));
#135724=CARTESIAN_POINT('Ctrl Pts',(10.,-27.9703562534103,124.777580265674));
#135725=CARTESIAN_POINT('Ctrl Pts',(10.,-27.9885129974625,124.705321550446));
#135726=CARTESIAN_POINT('Ctrl Pts',(10.,-28.0061948969839,124.63495258239));
#135727=CARTESIAN_POINT('Ctrl Pts',(9.99999999999999,-28.0277817096079,
124.565545600416));
#135728=CARTESIAN_POINT('Ctrl Pts',(10.0000000000001,-28.0530993947356,
124.497379617191));
#135729=CARTESIAN_POINT('Ctrl Pts',(10.0000000000001,-28.0587500616534,
124.482165617002));
#135730=CARTESIAN_POINT('Ctrl Pts',(10.,-28.0645875153452,124.46701154552));
#135731=CARTESIAN_POINT('Ctrl Pts',(10.,-28.0706074755671,124.45192711149));
#135732=CARTESIAN_POINT('Ctrl Pts',(10.,-28.0982336410484,124.382703220408));
#135733=CARTESIAN_POINT('Ctrl Pts',(9.99999999999995,-28.1296438323157,
124.315080840735));
#135734=CARTESIAN_POINT('Ctrl Pts',(9.99999999999993,-28.1646277359223,
124.249352564926));
#135735=CARTESIAN_POINT('Ctrl Pts',(9.99999999999992,-28.1891882402768,
124.203207925883));
#135736=CARTESIAN_POINT('Ctrl Pts',(10.0000000000001,-28.2155111464007,
124.157997355713));
#135737=CARTESIAN_POINT('Ctrl Pts',(10.0000000000001,-28.2435347288156,
124.113832765246));
#135738=CARTESIAN_POINT('Ctrl Pts',(10.0000000000001,-28.2541842563361,
124.097049328544));
#135739=CARTESIAN_POINT('Ctrl Pts',(10.,-28.2650794693322,124.080417051398));
#135740=CARTESIAN_POINT('Ctrl Pts',(9.99999999999997,-28.276217259473,124.063942481829));
#135741=CARTESIAN_POINT('Ctrl Pts',(9.99999999999989,-28.2868388799486,
124.048231409593));
#135742=CARTESIAN_POINT('Ctrl Pts',(9.99999999999993,-28.2976847177624,
124.032658993963));
#135743=CARTESIAN_POINT('Ctrl Pts',(9.99999999999997,-28.3087323142363,
124.017258087294));
#135744=CARTESIAN_POINT('Ctrl Pts',(10.0000000000001,-28.3509004273892,
123.958473610816));
#135745=CARTESIAN_POINT('Ctrl Pts',(10.0000000000001,-28.3960457650924,
123.902120594903));
#135746=CARTESIAN_POINT('Ctrl Pts',(10.,-28.4439773242738,123.848468307574));
#135747=CARTESIAN_POINT('Ctrl Pts',(9.99999999999994,-28.4912171255121,
123.795590340892));
#135748=CARTESIAN_POINT('Ctrl Pts',(9.9999999999999,-28.5411640434952,123.745335118217));
#135749=CARTESIAN_POINT('Ctrl Pts',(9.99999999999988,-28.5936642386043,
123.698000585234));
#135750=CARTESIAN_POINT('Ctrl Pts',(9.99999999999987,-28.6448275591752,
123.651871387427));
#135751=CARTESIAN_POINT('Ctrl Pts',(9.99999999999992,-28.698416431159,123.608515621588));
#135752=CARTESIAN_POINT('Ctrl Pts',(9.99999999999992,-28.7543060349939,
123.568254604751));
#135753=CARTESIAN_POINT('Ctrl Pts',(9.99999999999991,-28.7724718760314,
123.555168535398));
#135754=CARTESIAN_POINT('Ctrl Pts',(10.0000000000001,-28.7908808788323,
123.542409802214));
#135755=CARTESIAN_POINT('Ctrl Pts',(10.,-28.8095290004319,123.529990620511));
#135756=CARTESIAN_POINT('Ctrl Pts',(9.99999999999998,-28.8200346714515,
123.522994106862));
#135757=CARTESIAN_POINT('Ctrl Pts',(9.99999999999988,-28.8306173856636,
123.516104754664));
#135758=CARTESIAN_POINT('Ctrl Pts',(9.99999999999992,-28.8412612373231,
123.509334152335));
#135759=CARTESIAN_POINT('Ctrl Pts',(10.0000000000001,-28.8988964024382,
123.47267216233));
#135760=CARTESIAN_POINT('Ctrl Pts',(10.0000000000001,-28.9584212706046,
123.439421042338));
#135761=CARTESIAN_POINT('Ctrl Pts',(10.0000000000002,-29.019691425777,123.40984784988));
#135762=CARTESIAN_POINT('Ctrl Pts',(10.0000000000002,-29.0285216998097,
123.405585752082));
#135763=CARTESIAN_POINT('Ctrl Pts',(10.,-29.0373882572974,123.401400129531));
#135764=CARTESIAN_POINT('Ctrl Pts',(10.,-29.0462906965386,123.397291867037));
#135765=CARTESIAN_POINT('Ctrl Pts',(10.0000000000002,-29.109280769285,123.368223457094));
#135766=CARTESIAN_POINT('Ctrl Pts',(9.99999999999996,-29.1740667919833,
123.343023739063));
#135767=CARTESIAN_POINT('Ctrl Pts',(9.99999999999996,-29.2402810350378,
123.321677641666));
#135768=CARTESIAN_POINT('Ctrl Pts',(9.99999999999997,-29.3020523561828,
123.30176385006));
#135769=CARTESIAN_POINT('Ctrl Pts',(9.99999999999982,-29.3650675256982,
123.285204488516));
#135770=CARTESIAN_POINT('Ctrl Pts',(10.0000000000001,-29.4290244397517,
123.272027254596));
#135771=CARTESIAN_POINT('Ctrl Pts',(10.0000000000002,-29.4430780050743,
123.269131756582));
#135772=CARTESIAN_POINT('Ctrl Pts',(9.99999999999994,-29.4571770001559,
123.266399702894));
#135773=CARTESIAN_POINT('Ctrl Pts',(10.0000000000001,-29.4713181358355,
123.263831627986));
#135774=CARTESIAN_POINT('Ctrl Pts',(10.0000000000002,-29.4824509309542,
123.261809877226));
#135775=CARTESIAN_POINT('Ctrl Pts',(10.0000000000002,-29.493609299935,123.259889940904));
#135776=CARTESIAN_POINT('Ctrl Pts',(10.0000000000001,-29.5047784996148,
123.258073970657));
#135777=CARTESIAN_POINT('Ctrl Pts',(10.0000000000001,-29.5722612076497,
123.247102137987));
#135778=CARTESIAN_POINT('Ctrl Pts',(10.0000000000001,-29.640263498764,123.239897931082));
#135779=CARTESIAN_POINT('Ctrl Pts',(10.0000000000001,-29.7084341528629,
123.236428498985));
#135780=CARTESIAN_POINT('Ctrl Pts',(10.0000000000001,-29.776291735959,123.232975000116));
#135781=CARTESIAN_POINT('Ctrl Pts',(9.99999999999987,-29.8443172474683,
123.233222296554));
#135782=CARTESIAN_POINT('Ctrl Pts',(9.99999999999985,-29.9121554881824,
123.237188358926));
#135783=CARTESIAN_POINT('Ctrl Pts',(9.99999999999982,-29.9785429160644,
123.241069601673));
#135784=CARTESIAN_POINT('Ctrl Pts',(10.0000000000002,-30.0447519081449,
123.248512590545));
#135785=CARTESIAN_POINT('Ctrl Pts',(10.0000000000002,-30.1104263636383,
123.259577997692));
#135786=CARTESIAN_POINT('Ctrl Pts',(10.0000000000002,-30.129515952431,123.262794378714));
#135787=CARTESIAN_POINT('Ctrl Pts',(10.0000000000001,-30.1485601789394,
123.266317084266));
#135788=CARTESIAN_POINT('Ctrl Pts',(10.0000000000001,-30.1675497535845,
123.270148258539));
#135789=CARTESIAN_POINT('Ctrl Pts',(10.0000000000001,-30.178123023576,123.272281431121));
#135790=CARTESIAN_POINT('Ctrl Pts',(10.0000000000001,-30.1886698600177,
123.274508327613));
#135791=CARTESIAN_POINT('Ctrl Pts',(10.0000000000001,-30.1991886007708,
123.276828811527));
#135792=CARTESIAN_POINT('Ctrl Pts',(9.99999999999994,-30.2629295969814,
123.290890376484));
#135793=CARTESIAN_POINT('Ctrl Pts',(10.0000000000001,-30.3256439671593,
123.30838545758));
#135794=CARTESIAN_POINT('Ctrl Pts',(10.0000000000001,-30.3870120922313,
123.329323289776));
#135795=CARTESIAN_POINT('Ctrl Pts',(10.0000000000001,-30.4498356918113,
123.35075770682));
#135796=CARTESIAN_POINT('Ctrl Pts',(10.0000000000001,-30.5112495939634,
123.375800172046));
#135797=CARTESIAN_POINT('Ctrl Pts',(10.,-30.5708786461142,123.404508638235));
#135798=CARTESIAN_POINT('Ctrl Pts',(9.99999999999995,-30.6261220841815,
123.431105646182));
#135799=CARTESIAN_POINT('Ctrl Pts',(10.,-30.6798338743358,123.460849874209));
#135800=CARTESIAN_POINT('Ctrl Pts',(9.9999999999999,-30.7316789157771,123.493821876261));
#135801=CARTESIAN_POINT('Ctrl Pts',(9.99999999999989,-30.7357947411469,
123.496439426537));
#135802=CARTESIAN_POINT('Ctrl Pts',(10.0000000000002,-30.7398987797973,
123.499077335717));
#135803=CARTESIAN_POINT('Ctrl Pts',(10.0000000000002,-30.7439908523812,
123.501735652545));
#135804=CARTESIAN_POINT('Ctrl Pts',(10.,-30.753106648206,123.50765751071));
#135805=CARTESIAN_POINT('Ctrl Pts',(10.0000000000001,-30.7621630645469,
123.5136806418));
#135806=CARTESIAN_POINT('Ctrl Pts',(9.99999999999995,-30.7711590232015,
123.519803732655));
#135807=CARTESIAN_POINT('Ctrl Pts',(-5.55328352747075E-16,-31.2690708798524,
126.079358653049));
#135808=CARTESIAN_POINT('Ctrl Pts',(1.40620977341373E-13,-31.3143954758567,
126.03707561542));
#135809=CARTESIAN_POINT('Ctrl Pts',(-1.82722262030262E-14,-31.3569897935278,
125.992223116373));
#135810=CARTESIAN_POINT('Ctrl Pts',(5.40453098940574E-14,-31.3968555011726,
125.945146268677));
#135811=CARTESIAN_POINT('Ctrl Pts',(1.30912518458065E-13,-31.4393582794698,
125.894955341718));
#135812=CARTESIAN_POINT('Ctrl Pts',(6.08222559450276E-14,-31.478760244481,
125.842235824494));
#135813=CARTESIAN_POINT('Ctrl Pts',(2.52541043632704E-14,-31.5150345664964,
125.787351208348));
#135814=CARTESIAN_POINT('Ctrl Pts',(-5.65129697731147E-15,-31.5467745982599,
125.739327169221));
#135815=CARTESIAN_POINT('Ctrl Pts',(1.45041605914566E-15,-31.57611978446,
125.689644249953));
#135816=CARTESIAN_POINT('Ctrl Pts',(-5.9834082133392E-14,-31.6030292482344,
125.638518395284));
#135817=CARTESIAN_POINT('Ctrl Pts',(-9.02967013637418E-14,-31.6165278248273,
125.612872166473));
#135818=CARTESIAN_POINT('Ctrl Pts',(-3.10225958482436E-15,-31.6294131349682,
125.586862493095));
#135819=CARTESIAN_POINT('Ctrl Pts',(3.85247389544929E-14,-31.6416776773763,
125.560514791589));
#135820=CARTESIAN_POINT('Ctrl Pts',(5.75210116800135E-14,-31.6472866465359,
125.548465141447));
#135821=CARTESIAN_POINT('Ctrl Pts',(-3.60961809090547E-14,-31.6527663599446,
125.536343104099));
#135822=CARTESIAN_POINT('Ctrl Pts',(-2.28012053682392E-14,-31.6581075854569,
125.524171078425));
#135823=CARTESIAN_POINT('Ctrl Pts',(4.36540846169443E-14,-31.6850208488875,
125.462838911733));
#135824=CARTESIAN_POINT('Ctrl Pts',(4.94852571796735E-14,-31.7084732116299,
125.400131228953));
#135825=CARTESIAN_POINT('Ctrl Pts',(-8.56953397132543E-15,-31.7284413792091,
125.336405934918));
#135826=CARTESIAN_POINT('Ctrl Pts',(-6.74212432052424E-14,-31.7487645533631,
125.27154769274));
#135827=CARTESIAN_POINT('Ctrl Pts',(-3.05921264967593E-14,-31.7654790997968,
125.205634492719));
#135828=CARTESIAN_POINT('Ctrl Pts',(3.73312492030209E-15,-31.7785211409705,
125.139007153357));
#135829=CARTESIAN_POINT('Ctrl Pts',(3.2589687151767E-14,-31.7894305875867,
125.083274512103));
#135830=CARTESIAN_POINT('Ctrl Pts',(-2.04083765805674E-14,-31.7977698129652,
125.027041243318));
#135831=CARTESIAN_POINT('Ctrl Pts',(-5.9535709695524E-15,-31.8034765988388,
124.970494534412));
#135832=CARTESIAN_POINT('Ctrl Pts',(9.02866769369479E-16,-31.8061050671481,
124.944449885875));
#135833=CARTESIAN_POINT('Ctrl Pts',(1.54065700236016E-15,-31.8081747548663,
124.918338631073));
#135834=CARTESIAN_POINT('Ctrl Pts',(-5.13478148889135E-15,-31.809677780871,
124.892178658778));
#135835=CARTESIAN_POINT('Ctrl Pts',(-8.15445944510913E-15,-31.8103346621044,
124.880745726271));
#135836=CARTESIAN_POINT('Ctrl Pts',(5.75406636603668E-16,-31.8108831921244,
124.869303691251));
#135837=CARTESIAN_POINT('Ctrl Pts',(1.41553435639707E-15,-31.8113223787737,
124.857868186114));
#135838=CARTESIAN_POINT('Ctrl Pts',(6.29323886627523E-15,-31.8140157734359,
124.787737801816));
#135839=CARTESIAN_POINT('Ctrl Pts',(-6.06599144194739E-15,-31.8126089190124,
124.717721633684));
#135840=CARTESIAN_POINT('Ctrl Pts',(-1.77635683940025E-15,-31.8070473989234,
124.648180709286));
#135841=CARTESIAN_POINT('Ctrl Pts',(1.9596435517566E-15,-31.8020752960732,
124.586009823832));
#135842=CARTESIAN_POINT('Ctrl Pts',(2.43016174079474E-14,-31.7937821463294,
124.524217822068));
#135843=CARTESIAN_POINT('Ctrl Pts',(1.95399252334028E-14,-31.7820959342962,
124.463050544159));
#135844=CARTESIAN_POINT('Ctrl Pts',(1.43444283326989E-14,-31.7693632197095,
124.396405724654));
#135845=CARTESIAN_POINT('Ctrl Pts',(8.99293850601339E-15,-31.75260362096,
124.330501692871));
#135846=CARTESIAN_POINT('Ctrl Pts',(2.66175970153881E-14,-31.7320622411714,
124.265551890376));
#135847=CARTESIAN_POINT('Ctrl Pts',(3.37988617717994E-14,-31.7241352767211,
124.240487616178));
#135848=CARTESIAN_POINT('Ctrl Pts',(5.56272031405345E-14,-31.7156445735492,
124.215565493641));
#135849=CARTESIAN_POINT('Ctrl Pts',(4.77395900588817E-14,-31.706602209939,
124.19079810963));
#135850=CARTESIAN_POINT('Ctrl Pts',(4.43131798314357E-14,-31.7026358405724,
124.179934070373));
#135851=CARTESIAN_POINT('Ctrl Pts',(5.36000528057561E-14,-31.6985634332776,
124.16910038244));
#135852=CARTESIAN_POINT('Ctrl Pts',(6.00353100566053E-14,-31.6943910861053,
124.158310626993));
#135853=CARTESIAN_POINT('Ctrl Pts',(9.76408670109977E-14,-31.6691685481284,
124.093084746864));
#135854=CARTESIAN_POINT('Ctrl Pts',(-2.81031955616449E-14,-31.6402554518206,
124.029345120458));
#135855=CARTESIAN_POINT('Ctrl Pts',(-2.42861286636753E-14,-31.6079643298064,
123.96731040277));
#135856=CARTESIAN_POINT('Ctrl Pts',(-2.01425376075046E-14,-31.5748912639704,
123.903773486918));
#135857=CARTESIAN_POINT('Ctrl Pts',(5.74024171858222E-14,-31.5382742971337,
123.842024226929));
#135858=CARTESIAN_POINT('Ctrl Pts',(1.85407245112401E-14,-31.4983928835297,
123.782301295738));
#135859=CARTESIAN_POINT('Ctrl Pts',(-1.11230404567022E-14,-31.4679507489155,
123.736713806565));
#135860=CARTESIAN_POINT('Ctrl Pts',(4.72011644752096E-14,-31.4356053574396,
123.692306933135));
#135861=CARTESIAN_POINT('Ctrl Pts',(1.03889119529299E-13,-31.4014615571113,
123.649192900504));
#135862=CARTESIAN_POINT('Ctrl Pts',(1.39474512305205E-13,-31.3801754456228,
123.622314518588));
#135863=CARTESIAN_POINT('Ctrl Pts',(-5.99846713652865E-14,-31.3581900442438,
123.595938733229));
#135864=CARTESIAN_POINT('Ctrl Pts',(-3.4777736246383E-14,-31.3355278570067,
123.57009442258));
#135865=CARTESIAN_POINT('Ctrl Pts',(-2.07796655249921E-14,-31.3228334211773,
123.555617490602));
#135866=CARTESIAN_POINT('Ctrl Pts',(-7.74124701957694E-14,-31.3099221398224,
123.541302772379));
#135867=CARTESIAN_POINT('Ctrl Pts',(-4.70179450928754E-14,-31.2968217144024,
123.527180817023));
#135868=CARTESIAN_POINT('Ctrl Pts',(7.0510271335355E-14,-31.2459805955745,
123.472375267789));
#135869=CARTESIAN_POINT('Ctrl Pts',(-3.08159693383178E-14,-31.1922459214608,
123.420411847386));
#135870=CARTESIAN_POINT('Ctrl Pts',(-2.18713935851156E-14,-31.1359020383884,
123.371553876303));
#135871=CARTESIAN_POINT('Ctrl Pts',(-1.51741762347561E-14,-31.0937147685043,
123.334971654778));
#135872=CARTESIAN_POINT('Ctrl Pts',(-1.86234104118756E-14,-31.0500635672472,
123.300130609683));
#135873=CARTESIAN_POINT('Ctrl Pts',(7.78266340262235E-14,-31.0050513657681,
123.267151041331));
#135874=CARTESIAN_POINT('Ctrl Pts',(1.08037011731502E-13,-30.9910009326709,
123.256856561091));
#135875=CARTESIAN_POINT('Ctrl Pts',(5.25799844816238E-14,-30.976817796727,
123.246743532399));
#135876=CARTESIAN_POINT('Ctrl Pts',(4.6074255521944E-15,-30.9625048476372,
123.236815840421));
#135877=CARTESIAN_POINT('Ctrl Pts',(-4.16956105884885E-14,-30.9487122452095,
123.227249069267));
#135878=CARTESIAN_POINT('Ctrl Pts',(-1.04201132457139E-13,-30.9348061304262,
123.21785934585));
#135879=CARTESIAN_POINT('Ctrl Pts',(-6.62525589945062E-14,-30.92079448186,
123.20865289991));
#135880=CARTESIAN_POINT('Ctrl Pts',(1.04251430563816E-13,-30.8578449890432,
123.167291521208));
#135881=CARTESIAN_POINT('Ctrl Pts',(6.69980452307654E-14,-30.7927376832244,
123.129605407283));
#135882=CARTESIAN_POINT('Ctrl Pts',(-1.89015469942433E-14,-30.7257336719143,
123.095873532002));
#135883=CARTESIAN_POINT('Ctrl Pts',(-8.47522016279924E-14,-30.6744847329293,
123.070073243566));
#135884=CARTESIAN_POINT('Ctrl Pts',(-2.96517112328656E-13,-30.622125215821,
123.046586657031));
#135885=CARTESIAN_POINT('Ctrl Pts',(-1.39083189409916E-13,-30.5687580651082,
123.025553879704));
#135886=CARTESIAN_POINT('Ctrl Pts',(-1.03033770214677E-13,-30.5564788506438,
123.020714461071));
#135887=CARTESIAN_POINT('Ctrl Pts',(-1.42521024204696E-13,-30.5441462477664,
123.016005015431));
#135888=CARTESIAN_POINT('Ctrl Pts',(-1.66533453693773E-15,-30.5317621182487,
123.011424977843));
#135889=CARTESIAN_POINT('Ctrl Pts',(10.,-30.7923075365013,123.534460929349));
#135890=CARTESIAN_POINT('Ctrl Pts',(10.0002900114693,-30.7848643828255,
123.530436971974));
#135891=CARTESIAN_POINT('Ctrl Pts',(10.0005800229386,-30.7773905733591,
123.526469718933));
#135892=CARTESIAN_POINT('Ctrl Pts',(10.0008700344079,-30.7698869755801,
123.522559630702));
#135893=CARTESIAN_POINT('Ctrl Pts',(0.00155434972953121,-29.4691351333435,
123.012224622356));
#135894=CARTESIAN_POINT('Ctrl Pts',(0.038599440009051,-28.8081681097297,
123.188745659291));
#135895=CARTESIAN_POINT('Ctrl Pts',(0.112689620568091,-27.6877090541907,
124.250671923409));
#135896=CARTESIAN_POINT('Ctrl Pts',(0.223824891406651,-28.1162248339476,
126.540127744107));
#135897=CARTESIAN_POINT('Ctrl Pts',(0.33496016224521,-30.2723187871224,
127.416073114121));
#135898=CARTESIAN_POINT('Ctrl Pts',(0.44609543308377,-32.1775003475611,
126.082528630612));
#135899=CARTESIAN_POINT('Ctrl Pts',(0.557230703922329,-32.090499234442,
123.757255617341));
#135900=CARTESIAN_POINT('Ctrl Pts',(0.668365974760889,-30.0897172445553,
122.569885820561));
#135901=CARTESIAN_POINT('Ctrl Pts',(0.779501245599448,-28.0070199569619,
123.606506785386));
#135902=CARTESIAN_POINT('Ctrl Pts',(0.890636516438007,-27.7483422269096,
125.918663574952));
#135903=CARTESIAN_POINT('Ctrl Pts',(1.00177178727657,-29.5505922730324,
127.389938795433));
#135904=CARTESIAN_POINT('Ctrl Pts',(1.11290705811512,-31.7641484329131,
126.673797360623));
#135905=CARTESIAN_POINT('Ctrl Pts',(1.22404232895368,-32.3630411382761,
124.425663023932));
#135906=CARTESIAN_POINT('Ctrl Pts',(1.33517759979224,-30.799102978858,122.70320972357));
#135907=CARTESIAN_POINT('Ctrl Pts',(1.4463128706308,-28.503771277491,123.082940610925));
#135908=CARTESIAN_POINT('Ctrl Pts',(1.55744814146936,-27.5778941423288,
125.21730355642));
#135909=CARTESIAN_POINT('Ctrl Pts',(1.66858341230792,-28.868902973627,127.152773886107));
#135910=CARTESIAN_POINT('Ctrl Pts',(1.77971868314648,-31.1951726997191,
127.117871314526));
#135911=CARTESIAN_POINT('Ctrl Pts',(1.89085395398504,-32.427534695358,125.144540597895));
#135912=CARTESIAN_POINT('Ctrl Pts',(2.0019892248236,-31.4380424849057,123.038916039209));
#135913=CARTESIAN_POINT('Ctrl Pts',(2.11312449566216,-29.1323505409916,
122.728216337308));
#135914=CARTESIAN_POINT('Ctrl Pts',(2.22425976650072,-27.6207936836985,
124.496816246995));
#135915=CARTESIAN_POINT('Ctrl Pts',(2.33539503733928,-28.2868573536594,
126.725966059205));
#135916=CARTESIAN_POINT('Ctrl Pts',(2.44653030817784,-30.5209122220338,
127.375387765058));
#135917=CARTESIAN_POINT('Ctrl Pts',(2.5576655790164,-32.2781908106313,125.850683963494));
#135918=CARTESIAN_POINT('Ctrl Pts',(2.66880084985495,-31.9503055276404,
123.547373096034));
#135919=CARTESIAN_POINT('Ctrl Pts',(2.77993612069352,-29.8373605376131,
122.573610711328));
#135920=CARTESIAN_POINT('Ctrl Pts',(2.89107139153207,-27.8732748655125,
123.820654089384));
#135921=CARTESIAN_POINT('Ctrl Pts',(3.00220666237064,-27.8557207974597,
126.14711955606));
#135922=CARTESIAN_POINT('Ctrl Pts',(3.11334193320919,-29.8007650772084,
127.423658808513));
#135923=CARTESIAN_POINT('Ctrl Pts',(3.22447720404775,-31.9281634692032,
126.48189143007));
#135924=CARTESIAN_POINT('Ctrl Pts',(3.33561247488631,-32.2907681558608,
124.183790571875));
#135925=CARTESIAN_POINT('Ctrl Pts',(3.44674774572488,-30.5566972823996,
122.632743209903));
#135926=CARTESIAN_POINT('Ctrl Pts',(3.55788301656343,-28.3130970690004,
123.248379300229));
#135927=CARTESIAN_POINT('Ctrl Pts',(3.669018287402,-27.6134715868242,125.467224472374));
#135928=CARTESIAN_POINT('Ctrl Pts',(3.78015355824055,-29.0981683306454,
127.258432247076));
#135929=CARTESIAN_POINT('Ctrl Pts',(3.89128882907911,-31.4082861960447,
126.982560608029));
#135930=CARTESIAN_POINT('Ctrl Pts',(4.00242409991767,-32.4294393788512,
124.892107094911));
#135931=CARTESIAN_POINT('Ctrl Pts',(4.11355937075623,-31.2269951376161,
122.900404918383));
#135932=CARTESIAN_POINT('Ctrl Pts',(4.22469464159479,-28.9015168124413,
122.83040297264));
#135933=CARTESIAN_POINT('Ctrl Pts',(4.33582991243335,-27.581449203612,124.746172066603));
#135934=CARTESIAN_POINT('Ctrl Pts',(4.44696518327191,-28.4750130060368,
126.894262717451));
#135935=CARTESIAN_POINT('Ctrl Pts',(4.55810045411047,-30.7643544438259,
127.308588066045));
#135936=CARTESIAN_POINT('Ctrl Pts',(4.66923572494902,-32.3541037917107,
125.609927792723));
#135937=CARTESIAN_POINT('Ctrl Pts',(4.78037099578759,-31.7892082561945,
123.353017792917));
#135938=CARTESIAN_POINT('Ctrl Pts',(4.89150626662615,-29.5867008073364,
122.603544210334));
#135939=CARTESIAN_POINT('Ctrl Pts',(5.0026415374647,-27.7624744665255,124.047479101787));
#135940=CARTESIAN_POINT('Ctrl Pts',(5.11377680830327,-27.9861922134631,
126.363229538033));
#135941=CARTESIAN_POINT('Ctrl Pts',(5.22491207914182,-30.0530914967008,
127.431254381478));
#135942=CARTESIAN_POINT('Ctrl Pts',(5.33604734998039,-32.0713976286418,
126.274020580108));
#135943=CARTESIAN_POINT('Ctrl Pts',(5.44718262081894,-32.1938118641602,
123.950711632033));
#135944=CARTESIAN_POINT('Ctrl Pts',(5.5583178916575,-30.3082919020013,122.587786767791));
#135945=CARTESIAN_POINT('Ctrl Pts',(5.66945316249606,-28.1406010467917,
123.432692720846));
#135946=CARTESIAN_POINT('Ctrl Pts',(5.78058843333462,-27.6747656725676,
125.7121108741));
#135947=CARTESIAN_POINT('Ctrl Pts',(5.89172370417318,-29.3371517743687,
127.339754005074));
#135948=CARTESIAN_POINT('Ctrl Pts',(6.00285897501174,-31.6062241840789,
126.825886208109));
#135949=CARTESIAN_POINT('Ctrl Pts',(6.1139942458503,-32.4051648468343,124.640836201665));
#135950=CARTESIAN_POINT('Ctrl Pts',(6.22512951668886,-31.0027258808682,
122.78451870188));
#135951=CARTESIAN_POINT('Ctrl Pts',(6.33626478752742,-28.682520163804,122.955968822229));
#135952=CARTESIAN_POINT('Ctrl Pts',(6.44740005836598,-27.5681666262566,
124.998263097456));
#135953=CARTESIAN_POINT('Ctrl Pts',(6.55853532920454,-28.6796016688356,
127.042147110651));
#135954=CARTESIAN_POINT('Ctrl Pts',(6.6696706000431,-30.9995601071582,127.216911402528));
#135955=CARTESIAN_POINT('Ctrl Pts',(6.78080587088166,-32.4046493378798,
125.362599139994));
#135956=CARTESIAN_POINT('Ctrl Pts',(6.89194114172022,-31.6088307706975,
123.176410099358));
#135957=CARTESIAN_POINT('Ctrl Pts',(7.00307641255877,-29.3404947212706,
122.659301522662));
#135958=CARTESIAN_POINT('Ctrl Pts',(7.11421168339733,-27.6757852746021,
124.284568322771));
#135959=CARTESIAN_POINT('Ctrl Pts',(7.22534695423589,-28.1383640909908,
126.564649582695));
#135960=CARTESIAN_POINT('Ctrl Pts',(7.33648222507445,-30.3048458108891,
127.412651157157));
#135961=CARTESIAN_POINT('Ctrl Pts',(7.44761749591301,-32.1923107480619,
126.052421093879));
#135962=CARTESIAN_POINT('Ctrl Pts',(7.55875276675157,-32.0732154164101,
123.728939651145));
#135963=CARTESIAN_POINT('Ctrl Pts',(7.66988803759013,-30.0565644192597,
122.56882393853));
#135964=CARTESIAN_POINT('Ctrl Pts',(7.7810233084287,-27.9881416008883,123.633895187267));
#135965=CARTESIAN_POINT('Ctrl Pts',(7.89215857926725,-27.7611161029497,
125.949323685456));
#135966=CARTESIAN_POINT('Ctrl Pts',(8.00329385010582,-29.583277957531,127.395862960217));
#135967=CARTESIAN_POINT('Ctrl Pts',(8.11442912094438,-31.7868537726289,
126.649536355778));
#135968=CARTESIAN_POINT('Ctrl Pts',(8.22556439178294,-32.3549726375641,
124.393435604416));
#135969=CARTESIAN_POINT('Ctrl Pts',(8.33669966262149,-30.767651448308,122.692506135324));
#135970=CARTESIAN_POINT('Ctrl Pts',(8.44783493346005,-28.4777203936358,
123.103560840128));
#135971=CARTESIAN_POINT('Ctrl Pts',(8.55897020429861,-27.5810892221483,
125.250372795181));
#135972=CARTESIAN_POINT('Ctrl Pts',(8.67010547513716,-28.8984184498051,
127.168025763146));
#135973=CARTESIAN_POINT('Ctrl Pts',(8.78124074597574,-31.22399523633,127.101345462494));
#135974=CARTESIAN_POINT('Ctrl Pts',(8.89237601681429,-32.4292816418055,
125.1113635915));
#135975=CARTESIAN_POINT('Ctrl Pts',(9.00351128765285,-31.4111190912015,
123.019452274317));
#135976=CARTESIAN_POINT('Ctrl Pts',(9.11464655849142,-29.1013906938143,
122.740283510567));
#135977=CARTESIAN_POINT('Ctrl Pts',(9.22578182932996,-27.6141508798812,
124.529363487384));
#135978=CARTESIAN_POINT('Ctrl Pts',(9.33691710016854,-28.3105775286338,
126.749216168547));
#135979=CARTESIAN_POINT('Ctrl Pts',(9.4480523710071,-30.5533538853258,127.368035529446));
#135980=CARTESIAN_POINT('Ctrl Pts',(9.55918764184564,-32.289521449751,125.81950938995));
#135981=CARTESIAN_POINT('Ctrl Pts',(9.67032291268421,-31.93043720362,123.520806688524));
#135982=CARTESIAN_POINT('Ctrl Pts',(9.78145818352276,-29.8039056239228,
122.576175956181));
#135983=CARTESIAN_POINT('Ctrl Pts',(9.89259345436133,-27.858013785853,123.84958187036));
#135984=CARTESIAN_POINT('Ctrl Pts',(10.0037287251999,-27.8702627078603,
126.176784351898));
#135985=CARTESIAN_POINT('Ctrl Pts',(10.1148770665318,-29.8368965496469,
127.425328002316));
#135986=CARTESIAN_POINT('Ctrl Pts',(10.1889803175841,-31.2393430859939,
126.779199071106));
#135987=CARTESIAN_POINT('Ctrl Pts',(10.226038478357,-31.6487232386396,126.230764030654));
#135988=CARTESIAN_POINT('Ctrl Pts',(-0.0743653415986168,-29.5030641598563,
123.139268786936));
#135989=CARTESIAN_POINT('Ctrl Pts',(-0.037320251319097,-28.8843413476733,
123.304507881293));
#135990=CARTESIAN_POINT('Ctrl Pts',(0.0367699292399429,-27.8354938968754,
124.298563531564));
#135991=CARTESIAN_POINT('Ctrl Pts',(0.147905200078501,-28.2366220603748,
126.441693964919));
#135992=CARTESIAN_POINT('Ctrl Pts',(0.259040470917062,-30.2549141481483,
127.261655269027));
#135993=CARTESIAN_POINT('Ctrl Pts',(0.370175741755621,-32.0383303409089,
126.013341263137));
#135994=CARTESIAN_POINT('Ctrl Pts',(0.481311012594181,-31.9568897070361,
123.836682812011));
#135995=CARTESIAN_POINT('Ctrl Pts',(0.592446283432741,-30.0839831699153,
122.725201068568));
#135996=CARTESIAN_POINT('Ctrl Pts',(0.703581554271301,-28.1343967659521,
123.695568750481));
#135997=CARTESIAN_POINT('Ctrl Pts',(0.814716825109859,-27.8922518375834,
125.859949271654));
#135998=CARTESIAN_POINT('Ctrl Pts',(0.925852095948419,-29.5793151508136,
127.237191266171));
#135999=CARTESIAN_POINT('Ctrl Pts',(1.03698736678697,-31.6513968783983,
126.566820390414));
#136000=CARTESIAN_POINT('Ctrl Pts',(1.14812263762554,-32.2120127118963,
124.462370471932));
#136001=CARTESIAN_POINT('Ctrl Pts',(1.25925790846409,-30.7480301204735,
122.850003876052));
#136002=CARTESIAN_POINT('Ctrl Pts',(1.37039317930265,-28.5993993500641,
123.205465123138));
#136003=CARTESIAN_POINT('Ctrl Pts',(1.48152845014121,-27.7326975565748,
125.203415091407));
#136004=CARTESIAN_POINT('Ctrl Pts',(1.59266372097977,-28.9411944801982,
127.015184215278));
#136005=CARTESIAN_POINT('Ctrl Pts',(1.70379899181833,-31.1187859415003,
126.982512362569));
#136006=CARTESIAN_POINT('Ctrl Pts',(1.81493426265689,-32.2723843092376,
125.135302612701));
#136007=CARTESIAN_POINT('Ctrl Pts',(1.92606953349545,-31.3461332540233,
123.164254282289));
#136008=CARTESIAN_POINT('Ctrl Pts',(2.03720480433401,-29.1878043925225,
122.873412248667));
#136009=CARTESIAN_POINT('Ctrl Pts',(2.14834007517257,-27.7728552708471,
124.528976097777));
#136010=CARTESIAN_POINT('Ctrl Pts',(2.25947534601113,-28.3963489887604,
126.615654844693));
#136011=CARTESIAN_POINT('Ctrl Pts',(2.37061061684969,-30.4876192962776,
127.22357023197));
#136012=CARTESIAN_POINT('Ctrl Pts',(2.48174588768825,-32.1325854009119,
125.796314423213));
#136013=CARTESIAN_POINT('Ctrl Pts',(2.59288115852681,-31.825656163722,123.640214457053));
#136014=CARTESIAN_POINT('Ctrl Pts',(2.70401642936537,-29.8477552707702,
122.728687891372));
#136015=CARTESIAN_POINT('Ctrl Pts',(2.81515170020393,-28.0091996893342,
123.896029314195));
#136016=CARTESIAN_POINT('Ctrl Pts',(2.92628697104248,-27.9927675498132,
126.073804005766));
#136017=CARTESIAN_POINT('Ctrl Pts',(3.03742224188105,-29.8134987263952,
127.268756140928));
#136018=CARTESIAN_POINT('Ctrl Pts',(3.1485575127196,-31.8049292648385,126.387179693095));
#136019=CARTESIAN_POINT('Ctrl Pts',(3.25969278355817,-32.1443588935859,
124.23595675025));
#136020=CARTESIAN_POINT('Ctrl Pts',(3.37082805439672,-30.5211172354979,
122.784041070128));
#136021=CARTESIAN_POINT('Ctrl Pts',(3.48196332523528,-28.4209116520804,
123.360330173033));
#136022=CARTESIAN_POINT('Ctrl Pts',(3.59309859607384,-27.7660011492234,
125.437362877633));
#136023=CARTESIAN_POINT('Ctrl Pts',(3.7042338669124,-29.1558068607902,127.114089661229));
#136024=CARTESIAN_POINT('Ctrl Pts',(3.81536913775096,-31.3182787710212,
126.855849733647));
#136025=CARTESIAN_POINT('Ctrl Pts',(3.92650440858952,-32.274167259196,124.89900282576));
#136026=CARTESIAN_POINT('Ctrl Pts',(4.03763967942808,-31.1485745202988,
123.034595786276));
#136027=CARTESIAN_POINT('Ctrl Pts',(4.14877495026664,-28.9717238793155,
122.969067856468));
#136028=CARTESIAN_POINT('Ctrl Pts',(4.2599102211052,-27.7360254041619,124.762394904509));
#136029=CARTESIAN_POINT('Ctrl Pts',(4.37104549194376,-28.572479098445,126.773195202911));
#136030=CARTESIAN_POINT('Ctrl Pts',(4.48218076278232,-30.7155024594159,
127.16103988454));
#136031=CARTESIAN_POINT('Ctrl Pts',(4.59331603362088,-32.2036465756101,
125.570945638223));
#136032=CARTESIAN_POINT('Ctrl Pts',(4.70445130445944,-31.6748550597894,
123.458280933275));
#136033=CARTESIAN_POINT('Ctrl Pts',(4.815586575298,-29.6131158898675,122.756708258534));
#136034=CARTESIAN_POINT('Ctrl Pts',(4.92672184613655,-27.905480847088,124.108357319276));
#136035=CARTESIAN_POINT('Ctrl Pts',(5.03785711697512,-28.1149001805423,
126.276101807335));
#136036=CARTESIAN_POINT('Ctrl Pts',(5.14899238781368,-30.0496982738444,
127.275866260038));
#136037=CARTESIAN_POINT('Ctrl Pts',(5.26012765865223,-31.9390089371404,
126.192594438061));
#136038=CARTESIAN_POINT('Ctrl Pts',(5.3712629294908,-32.0535993438403,124.017774523349));
#136039=CARTESIAN_POINT('Ctrl Pts',(5.48239820032934,-30.2885881228032,
122.741957917269));
#136040=CARTESIAN_POINT('Ctrl Pts',(5.59353347116793,-28.2594403227427,
123.532863618504));
#136041=CARTESIAN_POINT('Ctrl Pts',(5.70466874200646,-27.8233777621957,
125.666597919213));
#136042=CARTESIAN_POINT('Ctrl Pts',(5.81580401284504,-29.379516218569,127.19021392311));
#136043=CARTESIAN_POINT('Ctrl Pts',(5.92693928368359,-31.5035660005183,
126.709188823416));
#136044=CARTESIAN_POINT('Ctrl Pts',(6.03807455452215,-32.2514441789554,
124.663791342985));
#136045=CARTESIAN_POINT('Ctrl Pts',(6.14920982536071,-30.9386389255357,
122.92611617503));
#136046=CARTESIAN_POINT('Ctrl Pts',(6.26034509619927,-28.7667239058484,
123.086608448958));
#136047=CARTESIAN_POINT('Ctrl Pts',(6.37148036703783,-27.7235917526774,
124.99837410765));
#136048=CARTESIAN_POINT('Ctrl Pts',(6.48261563787639,-28.7639919398808,
126.911627899808));
#136049=CARTESIAN_POINT('Ctrl Pts',(6.59375090871494,-30.9356754850877,
127.075222527492));
#136050=CARTESIAN_POINT('Ctrl Pts',(6.70488617955351,-32.250961617589,125.339424436586));
#136051=CARTESIAN_POINT('Ctrl Pts',(6.81602145039206,-31.5060059930522,
123.292960720756));
#136052=CARTESIAN_POINT('Ctrl Pts',(6.92715672123063,-29.3826455085853,
122.808901968433));
#136053=CARTESIAN_POINT('Ctrl Pts',(7.03829199206918,-27.8243321986736,
124.330293519274));
#136054=CARTESIAN_POINT('Ctrl Pts',(7.14942726290775,-28.2573463369091,
126.464648545692));
#136055=CARTESIAN_POINT('Ctrl Pts',(7.2605625337463,-30.2853622808052,127.258452018697));
#136056=CARTESIAN_POINT('Ctrl Pts',(7.37169780458487,-32.0521941681802,
125.985157981475));
#136057=CARTESIAN_POINT('Ctrl Pts',(7.48283307542342,-31.9407105451174,
123.810176596711));
#136058=CARTESIAN_POINT('Ctrl Pts',(7.59396834626198,-30.0529492324178,
122.724207054324));
#136059=CARTESIAN_POINT('Ctrl Pts',(7.70510361710054,-28.1167249772821,
123.72120668464));
#136060=CARTESIAN_POINT('Ctrl Pts',(7.8162388879391,-27.9042093002458,125.888649810584));
#136061=CARTESIAN_POINT('Ctrl Pts',(7.92737415877766,-29.6099118037608,
127.242736801369));
#136062=CARTESIAN_POINT('Ctrl Pts',(8.03850942961621,-31.6726510577123,
126.544109972787));
#136063=CARTESIAN_POINT('Ctrl Pts',(8.14964470045479,-32.204459891147,124.432202794999));
#136064=CARTESIAN_POINT('Ctrl Pts',(8.26077997129334,-30.7185887433181,
122.839984383425));
#136065=CARTESIAN_POINT('Ctrl Pts',(8.3719152421319,-28.575013449493,123.224767457061));
#136066=CARTESIAN_POINT('Ctrl Pts',(8.48305051297046,-27.7356884300987,
125.234370784613));
#136067=CARTESIAN_POINT('Ctrl Pts',(8.59418578380902,-28.9688235415151,
127.029461303115));
#136068=CARTESIAN_POINT('Ctrl Pts',(8.70532105464758,-31.1457663509141,
126.96704272297));
#136069=CARTESIAN_POINT('Ctrl Pts',(8.81645632548615,-32.2740196035565,
125.104246039584));
#136070=CARTESIAN_POINT('Ctrl Pts',(8.92759159632469,-31.3209306080953,
123.146034499879));
#136071=CARTESIAN_POINT('Ctrl Pts',(9.03872686716326,-29.1588232739099,
122.884708175857));
#136072=CARTESIAN_POINT('Ctrl Pts',(9.14986213800182,-27.766637026802,124.559443154956));
#136073=CARTESIAN_POINT('Ctrl Pts',(9.26099740884039,-28.4185531424342,
126.637418975915));
#136074=CARTESIAN_POINT('Ctrl Pts',(9.37213267967894,-30.5179875240813,
127.216687897858));
#136075=CARTESIAN_POINT('Ctrl Pts',(9.48326795051749,-32.1431918678755,
125.767132301983));
#136076=CARTESIAN_POINT('Ctrl Pts',(9.59440322135606,-31.8070576786659,
123.615345981355));
#136077=CARTESIAN_POINT('Ctrl Pts',(9.70553849219461,-29.8164385521741,
122.731089184406));
#136078=CARTESIAN_POINT('Ctrl Pts',(9.81667376303317,-27.9949139870427,
123.92310824152));
#136079=CARTESIAN_POINT('Ctrl Pts',(9.92780903387173,-28.0063800469214,
126.101572843314));
#136080=CARTESIAN_POINT('Ctrl Pts',(10.0389573752036,-29.8473209375447,
127.270318651986));
#136081=CARTESIAN_POINT('Ctrl Pts',(10.1130606262561,-31.1601332775016,
126.665485589114));
#136082=CARTESIAN_POINT('Ctrl Pts',(10.1501187870289,-31.5433488241895,
126.152102533069));
#136083=CARTESIAN_POINT('Ctrl Pts',(-0.150285032926765,-29.5369931863691,
123.266312951517));
#136084=CARTESIAN_POINT('Ctrl Pts',(-0.113239942647244,-28.960514585617,
123.420270103296));
#136085=CARTESIAN_POINT('Ctrl Pts',(-0.039149762088205,-27.98327873956,
124.34645513972));
#136086=CARTESIAN_POINT('Ctrl Pts',(0.0719855087503543,-28.3570192868022,
126.343260185732));
#136087=CARTESIAN_POINT('Ctrl Pts',(0.183120779588914,-30.2375095091741,
127.107237423931));
#136088=CARTESIAN_POINT('Ctrl Pts',(0.294256050427474,-31.8991603342567,
125.944153895663));
#136089=CARTESIAN_POINT('Ctrl Pts',(0.405391321266033,-31.8232801796302,
123.916110006682));
#136090=CARTESIAN_POINT('Ctrl Pts',(0.516526592104593,-30.0782490952753,
122.880516316575));
#136091=CARTESIAN_POINT('Ctrl Pts',(0.627661862943152,-28.2617735749423,
123.784630715575));
#136092=CARTESIAN_POINT('Ctrl Pts',(0.738797133781711,-28.0361614482572,
125.801234968357));
#136093=CARTESIAN_POINT('Ctrl Pts',(0.849932404620271,-29.6080380285948,
127.084443736908));
#136094=CARTESIAN_POINT('Ctrl Pts',(0.96106767545883,-31.5386453238836,
126.459843420204));
#136095=CARTESIAN_POINT('Ctrl Pts',(1.07220294629739,-32.0609842855166,
124.499077919934));
#136096=CARTESIAN_POINT('Ctrl Pts',(1.18333821713595,-30.6969572620888,
122.996798028534));
#136097=CARTESIAN_POINT('Ctrl Pts',(1.2944734879745,-28.6950274226374,123.327989635352));
#136098=CARTESIAN_POINT('Ctrl Pts',(1.40560875881306,-27.887500970821,125.189526626394));
#136099=CARTESIAN_POINT('Ctrl Pts',(1.51674402965162,-29.0134859867694,
126.877594544449));
#136100=CARTESIAN_POINT('Ctrl Pts',(1.62787930049018,-31.0423991832815,
126.847153410613));
#136101=CARTESIAN_POINT('Ctrl Pts',(1.73901457132874,-32.1172339231171,
125.126064627507));
#136102=CARTESIAN_POINT('Ctrl Pts',(1.8501498421673,-31.2542240231409,123.289592525368));
#136103=CARTESIAN_POINT('Ctrl Pts',(1.96128511300586,-29.2432582440533,
123.018608160027));
#136104=CARTESIAN_POINT('Ctrl Pts',(2.07242038384442,-27.9249168579956,
124.561135948557));
#136105=CARTESIAN_POINT('Ctrl Pts',(2.18355565468298,-28.5058406238613,
126.50534363018));
#136106=CARTESIAN_POINT('Ctrl Pts',(2.29469092552154,-30.4543263705213,
127.071752698882));
#136107=CARTESIAN_POINT('Ctrl Pts',(2.4058261963601,-31.9869799911926,125.741944882932));
#136108=CARTESIAN_POINT('Ctrl Pts',(2.51696146719866,-31.7010067998036,
123.733055818073));
#136109=CARTESIAN_POINT('Ctrl Pts',(2.62809673803722,-29.8581500039272,
122.883765071417));
#136110=CARTESIAN_POINT('Ctrl Pts',(2.73923200887578,-28.145124513156,123.971404539008));
#136111=CARTESIAN_POINT('Ctrl Pts',(2.85036727971433,-28.1298143021666,
126.000488455471));
#136112=CARTESIAN_POINT('Ctrl Pts',(2.9615025505529,-29.8262323755821,127.113853473344));
#136113=CARTESIAN_POINT('Ctrl Pts',(3.07263782139145,-31.6816950604738,
126.29246795612));
#136114=CARTESIAN_POINT('Ctrl Pts',(3.18377309223002,-31.9979496313109,
124.288122928624));
#136115=CARTESIAN_POINT('Ctrl Pts',(3.29490836306857,-30.485537188596,122.935338930354));
#136116=CARTESIAN_POINT('Ctrl Pts',(3.40604363390714,-28.5287262351604,
123.472281045836));
#136117=CARTESIAN_POINT('Ctrl Pts',(3.51717890474571,-27.9185307116224,
125.40750128289));
#136118=CARTESIAN_POINT('Ctrl Pts',(3.62831417558425,-29.2134453909351,
126.969747075382));
#136119=CARTESIAN_POINT('Ctrl Pts',(3.73944944642281,-31.2282713459977,
126.729138859265));
#136120=CARTESIAN_POINT('Ctrl Pts',(3.85058471726137,-32.1188951395408,
124.905898556608));
#136121=CARTESIAN_POINT('Ctrl Pts',(3.96171998809993,-31.0701539029816,
123.168786654169));
#136122=CARTESIAN_POINT('Ctrl Pts',(4.07285525893849,-29.0419309461898,
123.107732740296));
#136123=CARTESIAN_POINT('Ctrl Pts',(4.18399052977705,-27.8906016047118,
124.778617742416));
#136124=CARTESIAN_POINT('Ctrl Pts',(4.29512580061561,-28.6699451908533,
126.652127688372));
#136125=CARTESIAN_POINT('Ctrl Pts',(4.40626107145418,-30.6666504750058,
127.013491703035));
#136126=CARTESIAN_POINT('Ctrl Pts',(4.51739634229273,-32.0531893595093,
125.531963483724));
#136127=CARTESIAN_POINT('Ctrl Pts',(4.62853161313129,-31.5605018633842,
123.563544073634));
#136128=CARTESIAN_POINT('Ctrl Pts',(4.73966688396984,-29.6395309723986,
122.909872306734));
#136129=CARTESIAN_POINT('Ctrl Pts',(4.85080215480841,-28.0484872276504,
124.169235536765));
#136130=CARTESIAN_POINT('Ctrl Pts',(4.96193742564696,-28.2436081476214,
126.188974076638));
#136131=CARTESIAN_POINT('Ctrl Pts',(5.07307269648554,-30.0463050509881,
127.120478138598));
#136132=CARTESIAN_POINT('Ctrl Pts',(5.18420796732408,-31.806620245639,126.111168296014));
#136133=CARTESIAN_POINT('Ctrl Pts',(5.29534323816265,-31.9133868235204,
124.084837414666));
#136134=CARTESIAN_POINT('Ctrl Pts',(5.40647850900121,-30.268884343605,122.896129066749));
#136135=CARTESIAN_POINT('Ctrl Pts',(5.51761377983977,-28.3782795986937,
123.633034516162));
#136136=CARTESIAN_POINT('Ctrl Pts',(5.62874905067832,-27.9719898518237,
125.621084964325));
#136137=CARTESIAN_POINT('Ctrl Pts',(5.7398843215169,-29.4218806627693,127.040673841146));
#136138=CARTESIAN_POINT('Ctrl Pts',(5.85101959235544,-31.4009078169576,
126.592491438723));
#136139=CARTESIAN_POINT('Ctrl Pts',(5.962154863194,-32.0977235110765,124.686746484305));
#136140=CARTESIAN_POINT('Ctrl Pts',(6.07329013403256,-30.8745519702031,
123.06771364818));
#136141=CARTESIAN_POINT('Ctrl Pts',(6.18442540487112,-28.8509276478927,
123.217248075688));
#136142=CARTESIAN_POINT('Ctrl Pts',(6.29556067570968,-27.8790168790981,
124.998485117847));
#136143=CARTESIAN_POINT('Ctrl Pts',(6.40669594654826,-28.848382210926,126.781108688965));
#136144=CARTESIAN_POINT('Ctrl Pts',(6.51783121738679,-30.8717908630171,
126.933533652455));
#136145=CARTESIAN_POINT('Ctrl Pts',(6.62896648822536,-32.0972738972983,
125.316249733178));
#136146=CARTESIAN_POINT('Ctrl Pts',(6.74010175906393,-31.403181215407,123.409511342155));
#136147=CARTESIAN_POINT('Ctrl Pts',(6.85123702990247,-29.4247962959002,
122.958502414204));
#136148=CARTESIAN_POINT('Ctrl Pts',(6.96237230074105,-27.9728791227451,
124.376018715778));
#136149=CARTESIAN_POINT('Ctrl Pts',(7.0735075715796,-28.3763285828275,126.364647508688));
#136150=CARTESIAN_POINT('Ctrl Pts',(7.18464284241815,-30.2658787507214,
127.104252880237));
#136151=CARTESIAN_POINT('Ctrl Pts',(7.29577811325673,-31.9120775882985,
125.917894869072));
#136152=CARTESIAN_POINT('Ctrl Pts',(7.40691338409527,-31.8082056738248,
123.891413542278));
#136153=CARTESIAN_POINT('Ctrl Pts',(7.51804865493385,-30.049334045576,122.879590170119));
#136154=CARTESIAN_POINT('Ctrl Pts',(7.62918392577238,-28.2453083536756,
123.808518182013));
#136155=CARTESIAN_POINT('Ctrl Pts',(7.74031919661097,-28.047302497542,125.827975935714));
#136156=CARTESIAN_POINT('Ctrl Pts',(7.85145446744951,-29.6365456499907,
127.089610642521));
#136157=CARTESIAN_POINT('Ctrl Pts',(7.96258973828808,-31.5584483427957,
126.438683589794));
#136158=CARTESIAN_POINT('Ctrl Pts',(8.07372500912664,-32.0539471447299,
124.470969985582));
#136159=CARTESIAN_POINT('Ctrl Pts',(8.18486027996519,-30.6695260383283,
122.987462631525));
#136160=CARTESIAN_POINT('Ctrl Pts',(8.29599555080376,-28.6723065053501,
123.345974073992));
#136161=CARTESIAN_POINT('Ctrl Pts',(8.40713082164232,-27.8902876380491,
125.218368774047));
#136162=CARTESIAN_POINT('Ctrl Pts',(8.51826609248088,-29.0392286332251,
126.890896843083));
#136163=CARTESIAN_POINT('Ctrl Pts',(8.62940136331943,-31.0675374654984,
126.832739983445));
#136164=CARTESIAN_POINT('Ctrl Pts',(8.74053663415801,-32.1187575653075,
125.097128487668));
#136165=CARTESIAN_POINT('Ctrl Pts',(8.85167190499654,-31.2307421249892,
123.272616725442));
#136166=CARTESIAN_POINT('Ctrl Pts',(8.96280717583512,-29.2162558540056,
123.029132841148));
#136167=CARTESIAN_POINT('Ctrl Pts',(9.07394244667367,-27.9191231737227,
124.589522822528));
#136168=CARTESIAN_POINT('Ctrl Pts',(9.18507771751223,-28.5265287562346,
126.525621783282));
#136169=CARTESIAN_POINT('Ctrl Pts',(9.2962129883508,-30.4826211628368,127.065340266269));
#136170=CARTESIAN_POINT('Ctrl Pts',(9.40734825918934,-31.9968622860001,
125.714755214017));
#136171=CARTESIAN_POINT('Ctrl Pts',(9.51848353002791,-31.6836781537117,
123.709885274187));
#136172=CARTESIAN_POINT('Ctrl Pts',(9.62961880086647,-29.8289714804254,
122.886002412632));
#136173=CARTESIAN_POINT('Ctrl Pts',(9.74075407170503,-28.1318141882324,
123.99663461268));
#136174=CARTESIAN_POINT('Ctrl Pts',(9.85188934254358,-28.1424973859825,
126.026361334731));
#136175=CARTESIAN_POINT('Ctrl Pts',(9.96303768387549,-29.8577453254426,
127.115309301658));
#136176=CARTESIAN_POINT('Ctrl Pts',(10.0371409349279,-31.0809234690093,
126.551772107121));
#136177=CARTESIAN_POINT('Ctrl Pts',(10.0741990957007,-31.4379744097394,
126.073441035482));
#136178=CARTESIAN_POINT('Ctrl Pts',(-0.226204724254913,-29.570922212882,
123.393357116098));
#136179=CARTESIAN_POINT('Ctrl Pts',(-0.189159633975392,-29.0366878235607,
123.536032325299));
#136180=CARTESIAN_POINT('Ctrl Pts',(-0.115069453416353,-28.1310635822448,
124.394346747875));
#136181=CARTESIAN_POINT('Ctrl Pts',(-0.00393418257779361,-28.4774165132295,
126.244826406544));
#136182=CARTESIAN_POINT('Ctrl Pts',(0.107201088260766,-30.2201048702,126.952819578836));
#136183=CARTESIAN_POINT('Ctrl Pts',(0.218336359099326,-31.7599903276045,
125.874966528187));
#136184=CARTESIAN_POINT('Ctrl Pts',(0.329471629937885,-31.6896706522244,
123.995537201353));
#136185=CARTESIAN_POINT('Ctrl Pts',(0.440606900776445,-30.0725150206353,
123.035831564584));
#136186=CARTESIAN_POINT('Ctrl Pts',(0.551742171615005,-28.3891503839325,
123.87369268067));
#136187=CARTESIAN_POINT('Ctrl Pts',(0.662877442453563,-28.1800710589308,
125.742520665059));
#136188=CARTESIAN_POINT('Ctrl Pts',(0.774012713292123,-29.6367609063761,
126.931696207645));
#136189=CARTESIAN_POINT('Ctrl Pts',(0.885147984130682,-31.4258937693687,
126.352866449995));
#136190=CARTESIAN_POINT('Ctrl Pts',(0.996283254969241,-31.909955859137,
124.535785367934));
#136191=CARTESIAN_POINT('Ctrl Pts',(1.10741852580781,-30.6458844037042,
123.143592181016));
#136192=CARTESIAN_POINT('Ctrl Pts',(1.21855379664637,-28.7906554952107,
123.450514147566));
#136193=CARTESIAN_POINT('Ctrl Pts',(1.32968906748491,-28.042304385067,125.175638161381));
#136194=CARTESIAN_POINT('Ctrl Pts',(1.44082433832348,-29.0857774933408,
126.740004873621));
#136195=CARTESIAN_POINT('Ctrl Pts',(1.55195960916203,-30.9660124250627,
126.711794458656));
#136196=CARTESIAN_POINT('Ctrl Pts',(1.6630948800006,-31.9620835369967,125.116826642314));
#136197=CARTESIAN_POINT('Ctrl Pts',(1.77423015083916,-31.1623147922585,
123.414930768448));
#136198=CARTESIAN_POINT('Ctrl Pts',(1.88536542167772,-29.2987120955841,
123.163804071385));
#136199=CARTESIAN_POINT('Ctrl Pts',(1.99650069251628,-28.0769784451441,
124.593295799339));
#136200=CARTESIAN_POINT('Ctrl Pts',(2.10763596335484,-28.6153322589623,
126.395032415667));
#136201=CARTESIAN_POINT('Ctrl Pts',(2.21877123419339,-30.4210334447649,
126.919935165794));
#136202=CARTESIAN_POINT('Ctrl Pts',(2.32990650503196,-31.8413745814733,
125.687575342652));
#136203=CARTESIAN_POINT('Ctrl Pts',(2.44104177587052,-31.5763574358852,
123.825897179092));
#136204=CARTESIAN_POINT('Ctrl Pts',(2.55217704670908,-29.8685447370843,
123.038842251461));
#136205=CARTESIAN_POINT('Ctrl Pts',(2.66331231754763,-28.2810493369777,
124.04677976382));
#136206=CARTESIAN_POINT('Ctrl Pts',(2.77444758838619,-28.2668610545202,
125.927172905177));
#136207=CARTESIAN_POINT('Ctrl Pts',(2.88558285922476,-29.8389660247691,
126.958950805759));
#136208=CARTESIAN_POINT('Ctrl Pts',(2.99671813006331,-31.5584608561091,
126.197756219146));
#136209=CARTESIAN_POINT('Ctrl Pts',(3.10785340090188,-31.851540369036,124.340289106999));
#136210=CARTESIAN_POINT('Ctrl Pts',(3.21898867174044,-30.4499571416943,
123.086636790579));
#136211=CARTESIAN_POINT('Ctrl Pts',(3.330123942579,-28.6365408182404,123.584231918639));
#136212=CARTESIAN_POINT('Ctrl Pts',(3.44125921341756,-28.0710602740216,
125.377639688149));
#136213=CARTESIAN_POINT('Ctrl Pts',(3.55239448425611,-29.2710839210799,
126.825404489536));
#136214=CARTESIAN_POINT('Ctrl Pts',(3.66352975509468,-31.1382639209742,
126.602427984882));
#136215=CARTESIAN_POINT('Ctrl Pts',(3.77466502593323,-31.9636230198854,
124.912794287456));
#136216=CARTESIAN_POINT('Ctrl Pts',(3.8858002967718,-30.9917332856643,123.302977522061));
#136217=CARTESIAN_POINT('Ctrl Pts',(3.99693556761035,-29.112138013064,123.246397624124));
#136218=CARTESIAN_POINT('Ctrl Pts',(4.10807083844891,-28.0451778052617,
124.794840580322));
#136219=CARTESIAN_POINT('Ctrl Pts',(4.21920610928747,-28.7674112832615,
126.531060173832));
#136220=CARTESIAN_POINT('Ctrl Pts',(4.33034138012603,-30.6177984905958,
126.865943521531));
#136221=CARTESIAN_POINT('Ctrl Pts',(4.44147665096459,-31.9027321434086,
125.492981329225));
#136222=CARTESIAN_POINT('Ctrl Pts',(4.55261192180315,-31.4461486669792,
123.668807213992));
#136223=CARTESIAN_POINT('Ctrl Pts',(4.66374719264171,-29.6659460549298,
123.063036354934));
#136224=CARTESIAN_POINT('Ctrl Pts',(4.77488246348027,-28.1914936082128,
124.230113754254));
#136225=CARTESIAN_POINT('Ctrl Pts',(4.88601773431883,-28.3723161147005,
126.10184634594));
#136226=CARTESIAN_POINT('Ctrl Pts',(4.99715300515739,-30.0429118281317,
126.965090017157));
#136227=CARTESIAN_POINT('Ctrl Pts',(5.10828827599595,-31.6742315541376,
126.029742153966));
#136228=CARTESIAN_POINT('Ctrl Pts',(5.21942354683449,-31.7731743032006,
124.151900305982));
#136229=CARTESIAN_POINT('Ctrl Pts',(5.33055881767307,-30.2491805644068,
123.050300216227));
#136230=CARTESIAN_POINT('Ctrl Pts',(5.44169408851162,-28.4971188746447,
123.73320541382));
#136231=CARTESIAN_POINT('Ctrl Pts',(5.55282935935019,-28.1206019414517,
125.575572009438));
#136232=CARTESIAN_POINT('Ctrl Pts',(5.66396463018875,-29.4642451069697,
126.891133759182));
#136233=CARTESIAN_POINT('Ctrl Pts',(5.7750999010273,-31.298249633397,126.47579405403));
#136234=CARTESIAN_POINT('Ctrl Pts',(5.88623517186586,-31.9440028431976,
124.709701625626));
#136235=CARTESIAN_POINT('Ctrl Pts',(5.99737044270442,-30.8104650148705,
123.209311121329));
#136236=CARTESIAN_POINT('Ctrl Pts',(6.10850571354298,-28.9351313899371,
123.347887702416));
#136237=CARTESIAN_POINT('Ctrl Pts',(6.21964098438154,-28.0344420055189,
124.998596128041));
#136238=CARTESIAN_POINT('Ctrl Pts',(6.3307762552201,-28.9327724819712,126.650589478122));
#136239=CARTESIAN_POINT('Ctrl Pts',(6.44191152605866,-30.8079062409465,
126.791844777419));
#136240=CARTESIAN_POINT('Ctrl Pts',(6.55304679689722,-31.9435861770076,
125.29307502977));
#136241=CARTESIAN_POINT('Ctrl Pts',(6.66418206773578,-31.3003564377619,
123.526061963553));
#136242=CARTESIAN_POINT('Ctrl Pts',(6.77531733857434,-29.4669470832149,
123.108102859975));
#136243=CARTESIAN_POINT('Ctrl Pts',(6.8864526094129,-28.1214260468166,124.421743912282));
#136244=CARTESIAN_POINT('Ctrl Pts',(6.99758788025146,-28.4953108287459,
126.264646471684));
#136245=CARTESIAN_POINT('Ctrl Pts',(7.10872315109001,-30.2463952206375,
126.950053741776));
#136246=CARTESIAN_POINT('Ctrl Pts',(7.21985842192858,-31.7719610084168,
125.850631756669));
#136247=CARTESIAN_POINT('Ctrl Pts',(7.33099369276713,-31.6757008025321,
123.972650487844));
#136248=CARTESIAN_POINT('Ctrl Pts',(7.4421289636057,-30.0457188587341,123.034973285914));
#136249=CARTESIAN_POINT('Ctrl Pts',(7.55326423444425,-28.3738917300693,
123.895829679386));
#136250=CARTESIAN_POINT('Ctrl Pts',(7.66439950528281,-28.1903956948382,
125.767302060842));
#136251=CARTESIAN_POINT('Ctrl Pts',(7.77553477612138,-29.6631794962207,
126.936484483674));
#136252=CARTESIAN_POINT('Ctrl Pts',(7.88667004695993,-31.4442456278791,
126.333257206803));
#136253=CARTESIAN_POINT('Ctrl Pts',(7.9978053177985,-31.9034343983128,124.509737176165));
#136254=CARTESIAN_POINT('Ctrl Pts',(8.10894058863705,-30.6204633333385,
123.134940879626));
#136255=CARTESIAN_POINT('Ctrl Pts',(8.22007585947561,-28.7695995612073,
123.467180690923));
#136256=CARTESIAN_POINT('Ctrl Pts',(8.33121113031418,-28.0448868459996,
125.20236676348));
#136257=CARTESIAN_POINT('Ctrl Pts',(8.44234640115272,-29.109633724935,126.75233238305));
#136258=CARTESIAN_POINT('Ctrl Pts',(8.55348167199129,-30.9893085800826,
126.698437243919));
#136259=CARTESIAN_POINT('Ctrl Pts',(8.66461694282985,-31.9634955270585,
125.090010935753));
#136260=CARTESIAN_POINT('Ctrl Pts',(8.7757522136684,-31.1405536418831,123.399198951005));
#136261=CARTESIAN_POINT('Ctrl Pts',(8.88688748450698,-29.2736884341012,
123.173557506439));
#136262=CARTESIAN_POINT('Ctrl Pts',(8.99802275534552,-28.0716093206434,
124.619602490099));
#136263=CARTESIAN_POINT('Ctrl Pts',(9.10915802618409,-28.634504370035,126.41382459065));
#136264=CARTESIAN_POINT('Ctrl Pts',(9.22029329702265,-30.4472548015924,
126.913992634681));
#136265=CARTESIAN_POINT('Ctrl Pts',(9.3314285678612,-31.8505327041246,125.662378126051));
#136266=CARTESIAN_POINT('Ctrl Pts',(9.44256383869977,-31.5602986287577,
123.804424567018));
#136267=CARTESIAN_POINT('Ctrl Pts',(9.55369910953832,-29.8415044086767,
123.040915640856));
#136268=CARTESIAN_POINT('Ctrl Pts',(9.66483438037689,-28.2687143894222,
124.070160983838));
#136269=CARTESIAN_POINT('Ctrl Pts',(9.77596965121544,-28.2786147250435,
125.951149826147));
#136270=CARTESIAN_POINT('Ctrl Pts',(9.88711799254734,-29.8681697133404,
126.960299951329));
#136271=CARTESIAN_POINT('Ctrl Pts',(9.96122124359971,-31.0017136605171,
126.438058625129));
#136272=CARTESIAN_POINT('Ctrl Pts',(9.99827940437256,-31.3325999952893,
125.994779537896));
#136273=CARTESIAN_POINT('Ctrl Pts',(10.,-31.3346917155535,125.997072727755));
#136274=CARTESIAN_POINT('Ctrl Pts',(9.99999999999997,-31.3032949818861,
126.051116469759));
#136275=CARTESIAN_POINT('Ctrl Pts',(9.99999999999998,-31.2687047283496,
126.103084815638));
#136276=CARTESIAN_POINT('Ctrl Pts',(10.,-31.2312473715225,126.152891889409));
#136277=CARTESIAN_POINT('Ctrl Pts',(10.,-31.2074935522595,126.184477359623));
#136278=CARTESIAN_POINT('Ctrl Pts',(9.9999999999999,-31.1825856296951,126.215193469153));
#136279=CARTESIAN_POINT('Ctrl Pts',(9.99999999999999,-31.1565968715116,
126.24501511677));
#136280=CARTESIAN_POINT('Ctrl Pts',(10.,-31.1389352785806,126.265281487214));
#136281=CARTESIAN_POINT('Ctrl Pts',(10.0000000000001,-31.1207743588366,
126.285134707583));
#136282=CARTESIAN_POINT('Ctrl Pts',(10.,-31.1021353208467,126.304566020695));
#136283=CARTESIAN_POINT('Ctrl Pts',(9.99999999999995,-31.092131473339,126.314995093985));
#136284=CARTESIAN_POINT('Ctrl Pts',(10.0000000000001,-31.0819897769253,
126.325302541625));
#136285=CARTESIAN_POINT('Ctrl Pts',(10.,-31.0717240566778,126.335476823968));
#136286=CARTESIAN_POINT('Ctrl Pts',(9.99999999999984,-31.0248714183304,
126.381912140689));
#136287=CARTESIAN_POINT('Ctrl Pts',(9.99999999999995,-30.9753875180743,
126.425630314061));
#136288=CARTESIAN_POINT('Ctrl Pts',(9.99999999999986,-30.9236079996157,
126.466521663676));
#136289=CARTESIAN_POINT('Ctrl Pts',(9.99999999999981,-30.8862479946937,
126.496025627181));
#136290=CARTESIAN_POINT('Ctrl Pts',(9.99999999999995,-30.847691738784,126.524057613651));
#136291=CARTESIAN_POINT('Ctrl Pts',(10.,-30.8080509947417,126.550567733346));
#136292=CARTESIAN_POINT('Ctrl Pts',(10.,-30.7972669055174,126.557779694248));
#136293=CARTESIAN_POINT('Ctrl Pts',(9.99999999999982,-30.7864024946457,
126.564878974989));
#136294=CARTESIAN_POINT('Ctrl Pts',(9.9999999999999,-30.7754598842327,126.571864456785));
#136295=CARTESIAN_POINT('Ctrl Pts',(9.99999999999999,-30.7640699579655,
126.579135493548));
#136296=CARTESIAN_POINT('Ctrl Pts',(10.0000000000001,-30.7526018652892,
126.586278999636));
#136297=CARTESIAN_POINT('Ctrl Pts',(10.0000000000001,-30.7410634609561,
126.593291059087));
#136298=CARTESIAN_POINT('Ctrl Pts',(10.0000000000001,-30.6830797616217,
126.628528613187));
#136299=CARTESIAN_POINT('Ctrl Pts',(9.99999999999987,-30.623284545528,126.660474164912));
#136300=CARTESIAN_POINT('Ctrl Pts',(9.99999999999988,-30.5620183695342,
126.689017211284));
#136301=CARTESIAN_POINT('Ctrl Pts',(9.9999999999999,-30.4998607710709,126.717975558798));
#136302=CARTESIAN_POINT('Ctrl Pts',(10.,-30.4361883312143,126.74343240662));
#136303=CARTESIAN_POINT('Ctrl Pts',(9.99999999999992,-30.3713163621627,
126.765238169052));
#136304=CARTESIAN_POINT('Ctrl Pts',(9.99999999999985,-30.3311211104448,
126.778749214311));
#136305=CARTESIAN_POINT('Ctrl Pts',(10.,-30.2904645887863,126.790857837192));
#136306=CARTESIAN_POINT('Ctrl Pts',(9.99999999999999,-30.2494162442241,
126.801520088512));
#136307=CARTESIAN_POINT('Ctrl Pts',(9.99999999999994,-30.21580979325,126.810249318157));
#136308=CARTESIAN_POINT('Ctrl Pts',(9.99999999999999,-30.1819406176338,
126.81800897399));
#136309=CARTESIAN_POINT('Ctrl Pts',(9.9999999999999,-30.1478454088751,126.824771201514));
#136310=CARTESIAN_POINT('Ctrl Pts',(9.99999999999986,-30.1338751424326,
126.827541975581));
#136311=CARTESIAN_POINT('Ctrl Pts',(10.0000000000001,-30.1198643123212,
126.830145566994));
#136312=CARTESIAN_POINT('Ctrl Pts',(10.0000000000001,-30.1058393901247,
126.832576128087));
#136313=CARTESIAN_POINT('Ctrl Pts',(10.0000000000002,-30.0363859437807,
126.844612618707));
#136314=CARTESIAN_POINT('Ctrl Pts',(9.99999999999996,-29.9664681718509,
126.852434897851));
#136315=CARTESIAN_POINT('Ctrl Pts',(9.99999999999994,-29.8964212696988,
126.855902603765));
#136316=CARTESIAN_POINT('Ctrl Pts',(9.99999999999994,-29.8886375030675,
126.856287942913));
#136317=CARTESIAN_POINT('Ctrl Pts',(9.99999999999996,-29.8808521119947,
126.856619467432));
#136318=CARTESIAN_POINT('Ctrl Pts',(9.99999999999997,-29.8730655354866,
126.856896950862));
#136319=CARTESIAN_POINT('Ctrl Pts',(10.,-29.8056773383807,126.85929840522));
#136320=CARTESIAN_POINT('Ctrl Pts',(9.99999999999989,-29.7382014882899,
126.857656501328));
#136321=CARTESIAN_POINT('Ctrl Pts',(9.99999999999988,-29.6709003004103,
126.852189051701));
#136322=CARTESIAN_POINT('Ctrl Pts',(9.99999999999987,-29.5985034520534,
126.846307638102));
#136323=CARTESIAN_POINT('Ctrl Pts',(9.99999999999992,-29.5263078059746,
126.835999878972));
#136324=CARTESIAN_POINT('Ctrl Pts',(9.99999999999983,-29.4546313182209,
126.8214732487));
#136325=CARTESIAN_POINT('Ctrl Pts',(9.99999999999982,-29.4415872896375,
126.818829623343));
#136326=CARTESIAN_POINT('Ctrl Pts',(9.99999999999981,-29.4285604566208,
126.816046107482));
#136327=CARTESIAN_POINT('Ctrl Pts',(9.99999999999985,-29.4155527485577,
126.813123730597));
#136328=CARTESIAN_POINT('Ctrl Pts',(9.99999999999989,-29.4042297181811,
126.810579841844));
#136329=CARTESIAN_POINT('Ctrl Pts',(10.,-29.392930117574,126.807932726357));
#136330=CARTESIAN_POINT('Ctrl Pts',(10.,-29.3816571293467,126.805184037638));
#136331=CARTESIAN_POINT('Ctrl Pts',(10.0000000000001,-29.3126125113312,
126.78834891293));
#136332=CARTESIAN_POINT('Ctrl Pts',(9.99999999999981,-29.244543771198,126.767702608814));
#136333=CARTESIAN_POINT('Ctrl Pts',(9.99999999999989,-29.1777377507782,
126.743495272553));
#136334=CARTESIAN_POINT('Ctrl Pts',(9.99999999999997,-29.1095249755724,
126.718778195015));
#136335=CARTESIAN_POINT('Ctrl Pts',(9.99999999999996,-29.0426277353696,
126.690348379079));
#136336=CARTESIAN_POINT('Ctrl Pts',(9.99999999999993,-28.977347346887,126.658417134553));
#136337=CARTESIAN_POINT('Ctrl Pts',(9.9999999999999,-28.9116724977334,126.626292943562));
#136338=CARTESIAN_POINT('Ctrl Pts',(10.,-28.8476330737593,126.590624566029));
#136339=CARTESIAN_POINT('Ctrl Pts',(10.,-28.7855466623976,126.551575878805));
#136340=CARTESIAN_POINT('Ctrl Pts',(9.99999999999999,-28.7702070472662,
126.541928166524));
#136341=CARTESIAN_POINT('Ctrl Pts',(10.,-28.7549867432889,126.53207387934));
#136342=CARTESIAN_POINT('Ctrl Pts',(10.,-28.7398907549959,126.522015045523));
#136343=CARTESIAN_POINT('Ctrl Pts',(10.,-28.7280685454367,126.514137612195));
#136344=CARTESIAN_POINT('Ctrl Pts',(10.0000000000001,-28.7163212920593,
126.506133688814));
#136345=CARTESIAN_POINT('Ctrl Pts',(10.0000000000001,-28.7046689957787,
126.498016823557));
#136346=CARTESIAN_POINT('Ctrl Pts',(10.,-28.6428534396378,126.45495676673));
#136347=CARTESIAN_POINT('Ctrl Pts',(10.0000000000002,-28.5835957840056,
126.408648117515));
#136348=CARTESIAN_POINT('Ctrl Pts',(10.0000000000001,-28.5272089070883,
126.359324350215));
#136349=CARTESIAN_POINT('Ctrl Pts',(10.0000000000001,-28.4707612462639,
126.309947412896));
#136350=CARTESIAN_POINT('Ctrl Pts',(9.99999999999986,-28.4171895082972,
126.257548438498));
#136351=CARTESIAN_POINT('Ctrl Pts',(9.99999999999999,-28.3668234268913,
126.202312178068));
#136352=CARTESIAN_POINT('Ctrl Pts',(10.0000000000001,-28.3176028887393,
126.148332229897));
#136353=CARTESIAN_POINT('Ctrl Pts',(9.99999999999988,-28.271442962171,126.091642044011));
#136354=CARTESIAN_POINT('Ctrl Pts',(9.99999999999992,-28.2286806046144,
126.032374216658));
#136355=CARTESIAN_POINT('Ctrl Pts',(9.99999999999993,-28.2195018418537,
126.019652623235));
#136356=CARTESIAN_POINT('Ctrl Pts',(10.,-28.2104797516011,126.006812138555));
#136357=CARTESIAN_POINT('Ctrl Pts',(10.,-28.2016179073793,125.993853863974));
#136358=CARTESIAN_POINT('Ctrl Pts',(10.0000000000001,-28.1941462419212,
125.982928385015));
#136359=CARTESIAN_POINT('Ctrl Pts',(10.0000000000001,-28.1867884914522,
125.971919171957));
#136360=CARTESIAN_POINT('Ctrl Pts',(9.99999999999996,-28.1795446482253,
125.960828055739));
#136361=CARTESIAN_POINT('',(-0.000876815277413574,-28.7297206906101,126.080257502575));
#136362=CARTESIAN_POINT('Ctrl Pts',(-0.000876815277414122,-28.7308655491349,
126.07928390409));
#136363=CARTESIAN_POINT('Ctrl Pts',(-0.000584543518276265,-28.7363646204801,
126.085750285054));
#136364=CARTESIAN_POINT('Ctrl Pts',(-0.000292271759137858,-28.7419131131761,
126.092174637624));
#136365=CARTESIAN_POINT('Ctrl Pts',(0.,-28.7475103790669,126.098556211331));
#136366=CARTESIAN_POINT('Ctrl Pts',(-2.7820627745978E-16,-29.4698297828114,
123.014825674328));
#136367=CARTESIAN_POINT('Ctrl Pts',(-1.97609861837893E-13,-29.401170043366,
123.040247830321));
#136368=CARTESIAN_POINT('Ctrl Pts',(-5.5152163697422E-14,-29.334213616656,
123.069560472599));
#136369=CARTESIAN_POINT('Ctrl Pts',(-1.60201713006458E-13,-29.2691493442699,
123.102469334512));
#136370=CARTESIAN_POINT('Ctrl Pts',(-2.68200217276662E-13,-29.2022698079646,
123.136296338862));
#136371=CARTESIAN_POINT('Ctrl Pts',(-2.29820772041161E-13,-29.1373887076476,
123.17392371655));
#136372=CARTESIAN_POINT('Ctrl Pts',(-9.11840047912449E-14,-29.0747423504468,
123.215076533735));
#136373=CARTESIAN_POINT('Ctrl Pts',(2.61392724717173E-14,-29.0218080377509,
123.249849442975));
#136374=CARTESIAN_POINT('Ctrl Pts',(-9.38998899934961E-14,-28.9704696095689,
123.287140478707));
#136375=CARTESIAN_POINT('Ctrl Pts',(-7.41143257876331E-14,-28.920892369119,
123.326801793383));
#136376=CARTESIAN_POINT('Ctrl Pts',(-6.55476793573773E-14,-28.8988614666167,
123.344426303114));
#136377=CARTESIAN_POINT('Ctrl Pts',(-1.32835642465106E-13,-28.8771786481344,
123.36251904944));
#136378=CARTESIAN_POINT('Ctrl Pts',(-8.67986238439755E-14,-28.8558599729151,
123.381067782614));
#136379=CARTESIAN_POINT('Ctrl Pts',(-6.15038739588855E-14,-28.8441494340358,
123.391256767565));
#136380=CARTESIAN_POINT('Ctrl Pts',(-1.86758897242026E-13,-28.8325487895349,
123.401583348733));
#136381=CARTESIAN_POINT('Ctrl Pts',(-1.02785835398578E-13,-28.8210608353787,
123.412045537351));
#136382=CARTESIAN_POINT('Ctrl Pts',(-2.52615601302705E-14,-28.8104650682277,
123.421695202817));
#136383=CARTESIAN_POINT('Ctrl Pts',(-3.88065258281064E-14,-28.7999637294668,
123.431461749876));
#136384=CARTESIAN_POINT('Ctrl Pts',(-4.03774236268362E-14,-28.789574909979,
123.441328151629));
#136385=CARTESIAN_POINT('Ctrl Pts',(-4.90462452237839E-14,-28.7365434906851,
123.491692804601));
#136386=CARTESIAN_POINT('Ctrl Pts',(-1.84085511397076E-13,-28.6863464726686,
123.544740799507));
#136387=CARTESIAN_POINT('Ctrl Pts',(-1.0035722253221E-13,-28.6392018003405,
123.60021312434));
#136388=CARTESIAN_POINT('Ctrl Pts',(-1.71114058750102E-14,-28.5923287923977,
123.655365797888));
#136389=CARTESIAN_POINT('Ctrl Pts',(-1.31233249041967E-13,-28.5484725296676,
123.712915819897));
#136390=CARTESIAN_POINT('Ctrl Pts',(-9.71167590790856E-14,-28.507892135908,
123.772632946222));
#136391=CARTESIAN_POINT('Ctrl Pts',(-6.85507458244374E-14,-28.4742027907302,
123.822209372063));
#136392=CARTESIAN_POINT('Ctrl Pts',(-1.73770042367498E-13,-28.4427718620505,
123.873280045604));
#136393=CARTESIAN_POINT('Ctrl Pts',(-1.43815515052381E-13,-28.4137752342028,
123.925719701626));
#136394=CARTESIAN_POINT('Ctrl Pts',(-1.31281996901083E-13,-28.4016706643393,
123.947610505042));
#136395=CARTESIAN_POINT('Ctrl Pts',(-1.70300290126942E-14,-28.389990623329,
123.969739909637));
#136396=CARTESIAN_POINT('Ctrl Pts',(-9.5590202420226E-14,-28.378749346911,
123.992098885363));
#136397=CARTESIAN_POINT('Ctrl Pts',(-1.31953464075218E-13,-28.3735483020346,
124.002443799216));
#136398=CARTESIAN_POINT('Ctrl Pts',(2.40083866636569E-14,-28.3684411946227,
124.012837856646));
#136399=CARTESIAN_POINT('Ctrl Pts',(-1.70835567914196E-14,-28.3634294998546,
124.023280161284));
#136400=CARTESIAN_POINT('Ctrl Pts',(-5.97973873750489E-14,-28.3581982914169,
124.034179841862));
#136401=CARTESIAN_POINT('Ctrl Pts',(-9.27396819412998E-14,-28.3530746474019,
124.045124632974));
#136402=CARTESIAN_POINT('Ctrl Pts',(-1.00863761787195E-13,-28.348061622022,
124.056109233392));
#136403=CARTESIAN_POINT('Ctrl Pts',(-1.47355037682488E-13,-28.3195209836541,
124.118647817258));
#136404=CARTESIAN_POINT('Ctrl Pts',(-2.85071571274172E-14,-28.2945413176299,
124.182518755638));
#136405=CARTESIAN_POINT('Ctrl Pts',(-3.02674552088433E-14,-28.2733460518275,
124.247517313807));
#136406=CARTESIAN_POINT('Ctrl Pts',(-3.16869797246774E-14,-28.2541404972774,
124.306414114924));
#136407=CARTESIAN_POINT('Ctrl Pts',(-3.55485677518699E-14,-28.2380424914015,
124.366237360219));
#136408=CARTESIAN_POINT('Ctrl Pts',(-4.01484401280072E-14,-28.2252549794995,
124.42683954573));
#136409=CARTESIAN_POINT('Ctrl Pts',(-4.59179637818739E-14,-28.2101233382629,
124.498550957328));
#136410=CARTESIAN_POINT('Ctrl Pts',(-5.45851067606379E-15,-28.1996265542869,
124.57135458373));
#136411=CARTESIAN_POINT('Ctrl Pts',(-1.19071419391048E-14,-28.1936895357657,
124.644827593783));
#136412=CARTESIAN_POINT('Ctrl Pts',(-1.33052481531539E-14,-28.1923826402661,
124.661000955183));
#136413=CARTESIAN_POINT('Ctrl Pts',(9.44554714602467E-15,-28.1912969153211,
124.677206670197));
#136414=CARTESIAN_POINT('Ctrl Pts',(2.38697950294409E-15,-28.1904319294748,
124.693440064206));
#136415=CARTESIAN_POINT('Ctrl Pts',(-4.91010865300255E-15,-28.1895379671049,
124.710217267488));
#136416=CARTESIAN_POINT('Ctrl Pts',(-1.03906427062131E-14,-28.1888797709736,
124.727030207538));
#136417=CARTESIAN_POINT('Ctrl Pts',(-6.30051566474776E-15,-28.1884574247814,
124.74383953316));
#136418=CARTESIAN_POINT('Ctrl Pts',(1.08928320408804E-14,-28.1867348754449,
124.812396781292));
#136419=CARTESIAN_POINT('Ctrl Pts',(-5.5157119594787E-15,-28.1889237895494,
124.880980752938));
#136420=CARTESIAN_POINT('Ctrl Pts',(-5.52335954751015E-15,-28.1949036163297,
124.949253382792));
#136421=CARTESIAN_POINT('Ctrl Pts',(-5.57772555860731E-15,-28.2008822534432,
125.017512430031));
#136422=CARTESIAN_POINT('Ctrl Pts',(3.50880129321791E-14,-28.2106507485166,
125.085461330334));
#136423=CARTESIAN_POINT('Ctrl Pts',(1.07414077632484E-14,-28.2241382280736,
125.152747182718));
#136424=CARTESIAN_POINT('Ctrl Pts',(-6.8258769737951E-15,-28.2338995436464,
125.201444082382));
#136425=CARTESIAN_POINT('Ctrl Pts',(-2.91457997124025E-14,-28.2456098667842,
125.249793420514));
#136426=CARTESIAN_POINT('Ctrl Pts',(4.16333634234434E-16,-28.2592565463921,
125.297651761821));
#136427=CARTESIAN_POINT('Ctrl Pts',(2.27944565755811E-14,-28.2694943306151,
125.333555247918));
#136428=CARTESIAN_POINT('Ctrl Pts',(7.45391254632543E-14,-28.2808221554132,
125.369182243487));
#136429=CARTESIAN_POINT('Ctrl Pts',(4.55191440096314E-15,-28.2932385970371,
125.404468009152));
#136430=CARTESIAN_POINT('Ctrl Pts',(-1.88360276278269E-14,-28.2973646052875,
125.416193539273));
#136431=CARTESIAN_POINT('Ctrl Pts',(8.25076564039632E-14,-28.3016076190464,
125.427872169366));
#136432=CARTESIAN_POINT('Ctrl Pts',(8.58757509547559E-14,-28.3059670179929,
125.439501411337));
#136433=CARTESIAN_POINT('Ctrl Pts',(1.03680549446333E-13,-28.3290907711057,
125.501186915127));
#136434=CARTESIAN_POINT('Ctrl Pts',(-3.99986743471012E-14,-28.3554872924869,
125.561488823148));
#136435=CARTESIAN_POINT('Ctrl Pts',(3.84969833788773E-14,-28.3851066181449,
125.620073246654));
#136436=CARTESIAN_POINT('Ctrl Pts',(9.41574255422266E-14,-28.4059439023546,
125.661287563851));
#136437=CARTESIAN_POINT('Ctrl Pts',(7.40228323442486E-14,-28.428377060535,
125.70165134068));
#136438=CARTESIAN_POINT('Ctrl Pts',(-9.99200722162641E-15,-28.4523991071197,
125.741036970346));
#136439=CARTESIAN_POINT('Ctrl Pts',(-3.69244381206805E-14,-28.460111515178,
125.753681939897));
#136440=CARTESIAN_POINT('Ctrl Pts',(9.89854782698033E-14,-28.4679888668089,
125.766227705693));
#136441=CARTESIAN_POINT('Ctrl Pts',(8.2794882061421E-14,-28.4760275745915,
125.778664362048));
#136442=CARTESIAN_POINT('Ctrl Pts',(1.33122388715207E-14,-28.5102739274187,
125.831646773282));
#136443=CARTESIAN_POINT('Ctrl Pts',(9.60593437654786E-14,-28.5473763329624,
125.882545618706));
#136444=CARTESIAN_POINT('Ctrl Pts',(4.16888745746746E-14,-28.5873005880483,
125.931045842962));
#136445=CARTESIAN_POINT('Ctrl Pts',(-8.43323934842311E-15,-28.6240900287733,
125.975737875952));
#136446=CARTESIAN_POINT('Ctrl Pts',(-1.05109709785338E-13,-28.6632761651105,
126.018393268337));
#136447=CARTESIAN_POINT('Ctrl Pts',(-1.17544862732188E-13,-28.7048536785431,
126.058732609253));
#136448=CARTESIAN_POINT('Ctrl Pts',(-1.1948434771856E-13,-28.7126567769435,
126.066303332478));
#136449=CARTESIAN_POINT('Ctrl Pts',(2.25053579668865E-14,-28.7205441578753,
126.073792376282));
#136450=CARTESIAN_POINT('Ctrl Pts',(-5.02375918642883E-15,-28.7285142384905,
126.081199077946));
#136451=CARTESIAN_POINT('Origin',(10.,30.,55.));
#136452=CARTESIAN_POINT('Origin',(10.,-30.,55.));
#136453=CARTESIAN_POINT('Origin',(10.,-30.,125.));
#136454=CARTESIAN_POINT('Origin',(10.,30.,125.));
#136455=CARTESIAN_POINT('Origin',(60.,0.,90.));
#136456=CARTESIAN_POINT('',(120.,-22.,90.));
#136457=CARTESIAN_POINT('Origin',(120.,0.,90.));
#136458=CARTESIAN_POINT('',(0.,-22.,90.));
#136459=CARTESIAN_POINT('',(60.,-22.,90.));
#136460=CARTESIAN_POINT('Origin',(0.,0.,90.));
#136461=CARTESIAN_POINT('Origin',(60.,0.,40.));
#136462=CARTESIAN_POINT('',(-20.,50.,40.));
#136463=CARTESIAN_POINT('',(-20.,-50.,40.));
#136464=CARTESIAN_POINT('',(-20.,50.,40.));
#136465=CARTESIAN_POINT('',(140.,-50.,40.));
#136466=CARTESIAN_POINT('',(-20.,-50.,40.));
#136467=CARTESIAN_POINT('',(140.,50.,40.));
#136468=CARTESIAN_POINT('',(140.,-50.,40.));
#136469=CARTESIAN_POINT('',(140.,50.,40.));
#136470=CARTESIAN_POINT('',(120.,40.,40.));
#136471=CARTESIAN_POINT('',(0.,40.,40.));
#136472=CARTESIAN_POINT('',(120.,40.,40.));
#136473=CARTESIAN_POINT('',(120.,-40.,40.));
#136474=CARTESIAN_POINT('',(120.,-40.,40.));
#136475=CARTESIAN_POINT('',(0.,-40.,40.));
#136476=CARTESIAN_POINT('',(0.,-40.,40.));
#136477=CARTESIAN_POINT('',(0.,40.,40.));
#136478=CARTESIAN_POINT('Origin',(140.,50.,30.));
#136479=CARTESIAN_POINT('',(140.,50.,30.));
#136480=CARTESIAN_POINT('',(-20.,50.,30.));
#136481=CARTESIAN_POINT('',(140.,50.,30.));
#136482=CARTESIAN_POINT('',(-20.,50.,30.));
#136483=CARTESIAN_POINT('',(140.,50.,30.));
#136484=CARTESIAN_POINT('Origin',(140.,-50.,30.));
#136485=CARTESIAN_POINT('',(140.,-50.,30.));
#136486=CARTESIAN_POINT('',(140.,-50.,30.));
#136487=CARTESIAN_POINT('',(140.,-50.,30.));
#136488=CARTESIAN_POINT('Origin',(-20.,-50.,30.));
#136489=CARTESIAN_POINT('',(-20.,-50.,30.));
#136490=CARTESIAN_POINT('',(-20.,-50.,30.));
#136491=CARTESIAN_POINT('',(-20.,-50.,30.));
#136492=CARTESIAN_POINT('Origin',(-20.,50.,30.));
#136493=CARTESIAN_POINT('',(-20.,50.,30.));
#136494=CARTESIAN_POINT('Origin',(60.,0.,30.));
#136495=CARTESIAN_POINT('Origin',(120.,40.,40.));
#136496=CARTESIAN_POINT('',(0.,40.,140.));
#136497=CARTESIAN_POINT('',(0.,40.,40.));
#136498=CARTESIAN_POINT('',(120.,40.,140.));
#136499=CARTESIAN_POINT('',(120.,40.,140.));
#136500=CARTESIAN_POINT('',(120.,40.,40.));
#136501=CARTESIAN_POINT('Origin',(120.,-40.,40.));
#136502=CARTESIAN_POINT('',(120.,-40.,140.));
#136503=CARTESIAN_POINT('',(120.,-40.,140.));
#136504=CARTESIAN_POINT('',(120.,-40.,40.));
#136505=CARTESIAN_POINT('Origin',(0.,-40.,40.));
#136506=CARTESIAN_POINT('',(0.,-40.,140.));
#136507=CARTESIAN_POINT('',(0.,-40.,140.));
#136508=CARTESIAN_POINT('',(0.,-40.,40.));
#136509=CARTESIAN_POINT('Origin',(0.,40.,40.));
#136510=CARTESIAN_POINT('',(0.,40.,140.));
#136511=CARTESIAN_POINT('Origin',(60.,0.,140.));
#136512=CARTESIAN_POINT('',(0.,0.,0.));
#136513=CARTESIAN_POINT('Origin',(-4.,16.,120.));
#136514=CARTESIAN_POINT('',(-4.,19.5959179422654,0.));
#136515=CARTESIAN_POINT('',(-4.,19.5959179422654,120.));
#136516=CARTESIAN_POINT('',(-4.,19.5959179422654,0.));
#136517=CARTESIAN_POINT('',(-4.,21.6333076527839,0.));
#136518=CARTESIAN_POINT('',(-4.,8.,0.));
#136519=CARTESIAN_POINT('',(-4.,21.6333076527839,120.));
#136520=CARTESIAN_POINT('',(-4.,21.6333076527839,0.));
#136521=CARTESIAN_POINT('',(-4.,8.,120.));
#136522=CARTESIAN_POINT('Origin',(4.,24.,120.));
#136523=CARTESIAN_POINT('',(4.,19.5959179422654,120.));
#136524=CARTESIAN_POINT('',(4.,19.5959179422654,0.));
#136525=CARTESIAN_POINT('',(4.,19.5959179422654,0.));
#136526=CARTESIAN_POINT('',(4.,21.6333076527839,120.));
#136527=CARTESIAN_POINT('',(4.,12.,120.));
#136528=CARTESIAN_POINT('',(4.,21.6333076527839,0.));
#136529=CARTESIAN_POINT('',(4.,21.6333076527839,0.));
#136530=CARTESIAN_POINT('',(4.,12.,0.));
#136531=CARTESIAN_POINT('Origin',(0.,0.,0.));
#136532=CARTESIAN_POINT('Origin',(0.,0.,0.));
#136533=CARTESIAN_POINT('Origin',(0.,0.,0.));
#136534=CARTESIAN_POINT('Origin',(0.,0.,0.));
#136535=CARTESIAN_POINT('Origin',(0.,0.,120.));
#136536=CARTESIAN_POINT('Origin',(0.,0.,0.));
#136537=CARTESIAN_POINT('Origin',(0.,0.,120.));
#136538=CARTESIAN_POINT('Origin',(0.,0.,120.));
#136539=CARTESIAN_POINT('',(0.,0.,0.));
#136540=CARTESIAN_POINT('Origin',(0.,0.,50.));
#136541=CARTESIAN_POINT('',(6.57110895151819,2.44502632087623,97.3397894808225));
#136542=CARTESIAN_POINT('',(6.57110895151812,2.44502632087642,97.8872278672842));
#136543=CARTESIAN_POINT('',(6.57110895151814,2.44502632087636,50.));
#136544=CARTESIAN_POINT('',(-5.31037376991249,-4.5779424402591,99.));
#136545=CARTESIAN_POINT('Ctrl Pts',(6.57110895151812,2.44502632087642,97.8872278672842));
#136546=CARTESIAN_POINT('Ctrl Pts',(6.50938159924675,2.61092112274443,97.8952353563129));
#136547=CARTESIAN_POINT('Ctrl Pts',(6.44134635625321,2.77453469938154,97.9032428453416));
#136548=CARTESIAN_POINT('Ctrl Pts',(6.36720734438102,2.93535299345077,97.9112503343703));
#136549=CARTESIAN_POINT('Ctrl Pts',(6.29307414937843,3.09615866988426,97.9192571951398));
#136550=CARTESIAN_POINT('Ctrl Pts',(6.21283829259821,3.25416916746725,97.9272640559092));
#136551=CARTESIAN_POINT('Ctrl Pts',(6.12675141741013,3.40889184805898,97.9352709166787));
#136552=CARTESIAN_POINT('Ctrl Pts',(6.04065482482025,3.56363199359472,97.9432786812548));
#136553=CARTESIAN_POINT('Ctrl Pts',(5.94870607806213,3.7150832633239,97.9512864458308));
#136554=CARTESIAN_POINT('Ctrl Pts',(5.85120197845763,3.86277904749852,97.9592942104068));
#136555=CARTESIAN_POINT('Ctrl Pts',(5.75362458113637,4.01058586047909,97.9673079947386));
#136556=CARTESIAN_POINT('Ctrl Pts',(5.65048369152628,4.15463124245543,97.9753217790703));
#136557=CARTESIAN_POINT('Ctrl Pts',(5.54211891182822,4.29447837689935,97.9833355634021));
#136558=CARTESIAN_POINT('Ctrl Pts',(5.43371064956408,4.43438162655229,97.9913525633534));
#136559=CARTESIAN_POINT('Ctrl Pts',(5.32007455496683,4.57008299043006,97.9993695633047));
#136560=CARTESIAN_POINT('Ctrl Pts',(5.2015892770394,4.70118023005806,98.007386563256));
#136561=CARTESIAN_POINT('Ctrl Pts',(5.08296634063021,4.83242978098824,98.0154128775125));
#136562=CARTESIAN_POINT('Ctrl Pts',(4.95948322248214,4.95906425994386,98.023439191769));
#136563=CARTESIAN_POINT('Ctrl Pts',(4.8315546615639,5.08071905489963,98.0314655060255));
#136564=CARTESIAN_POINT('Ctrl Pts',(4.74373431819421,5.16423258611501,98.0369754067775));
#136565=CARTESIAN_POINT('Ctrl Pts',(4.65381976686174,5.24540023570575,98.0424853075295));
#136566=CARTESIAN_POINT('Ctrl Pts',(4.56195357994108,5.3241155225035,98.0479952082814));
#136567=CARTESIAN_POINT('Ctrl Pts',(4.42499058165131,5.44147188671584,98.0562099013319));
#136568=CARTESIAN_POINT('Ctrl Pts',(4.28336273304958,5.55365432817838,98.0644245943823));
#136569=CARTESIAN_POINT('Ctrl Pts',(4.13749531642271,5.66027906282721,98.0726392874327));
#136570=CARTESIAN_POINT('Ctrl Pts',(3.99174322317347,5.76681949952369,98.0808474859132));
#136571=CARTESIAN_POINT('Ctrl Pts',(3.84175851848353,5.86781077799742,98.0890556843936));
#136572=CARTESIAN_POINT('Ctrl Pts',(3.6880001335886,5.96290881845014,98.097263882874));
#136573=CARTESIAN_POINT('Ctrl Pts',(3.53433743431589,6.05794767829181,98.1054669732976));
#136574=CARTESIAN_POINT('Ctrl Pts',(3.37690602897598,6.14710042473671,98.1136700637211));
#136575=CARTESIAN_POINT('Ctrl Pts',(3.21619461362914,6.23006571151243,98.1218731541446));
#136576=CARTESIAN_POINT('Ctrl Pts',(3.05555571769875,6.3129935610335,98.1300725430058));
#136577=CARTESIAN_POINT('Ctrl Pts',(2.89164007015946,6.38973935585205,98.1382719318669));
#136578=CARTESIAN_POINT('Ctrl Pts',(2.72496197647721,6.46004711973941,98.146471320728));
#136579=CARTESIAN_POINT('Ctrl Pts',(2.5583282121748,6.53033618471138,98.1546685288958));
#136580=CARTESIAN_POINT('Ctrl Pts',(2.38893378668065,6.59419049689403,98.1628657370635));
#136581=CARTESIAN_POINT('Ctrl Pts',(2.21731424710863,6.65140166371488,98.1710629452312));
#136582=CARTESIAN_POINT('Ctrl Pts',(2.0456929039503,6.70861343178008,98.1792602395451));
#136583=CARTESIAN_POINT('Ctrl Pts',(1.87184672898898,6.7591818016802,98.187457533859));
#136584=CARTESIAN_POINT('Ctrl Pts',(1.69632810355969,6.80294770871963,98.195654828173));
#136585=CARTESIAN_POINT('Ctrl Pts',(1.61776226550553,6.82253825163974,98.1993241099713));
#136586=CARTESIAN_POINT('Ctrl Pts',(1.53886152202906,6.84076649049615,98.2029933917696));
#136587=CARTESIAN_POINT('Ctrl Pts',(1.4596762357207,6.8576214425537,98.2066626735679));
#136588=CARTESIAN_POINT('Ctrl Pts',(1.26036588358846,6.90004556686235,98.2158983015663));
#136589=CARTESIAN_POINT('Ctrl Pts',(1.05939543449298,6.93373583637616,98.2251339295647));
#136590=CARTESIAN_POINT('Ctrl Pts',(0.857490139543839,6.95861604222313,
98.2343695575632));
#136591=CARTESIAN_POINT('Ctrl Pts',(0.655095352708131,6.98355656674031,
98.2436275760837));
#136592=CARTESIAN_POINT('Ctrl Pts',(0.451761352173247,6.99964427887774,
98.2528855946042));
#136593=CARTESIAN_POINT('Ctrl Pts',(0.248218246296909,7.00685480545339,
98.2621436131248));
#136594=CARTESIAN_POINT('Ctrl Pts',(0.0441803191852665,7.0140828611006,
98.2714241382497));
#136595=CARTESIAN_POINT('Ctrl Pts',(-0.160067563674659,7.01239053413818,
98.2807046633747));
#136596=CARTESIAN_POINT('Ctrl Pts',(-0.363792928534682,7.00180557196843,
98.2899851884996));
#136597=CARTESIAN_POINT('Ctrl Pts',(-0.567660667947921,6.99121321244165,
98.2992721993688));
#136598=CARTESIAN_POINT('Ctrl Pts',(-0.771004994477104,6.9717158117372,
98.308559210238));
#136599=CARTESIAN_POINT('Ctrl Pts',(-0.973097359653584,6.94339312520437,
98.3178462211073));
#136600=CARTESIAN_POINT('Ctrl Pts',(-1.17520208405622,6.91506870656014,
98.3271337999359));
#136601=CARTESIAN_POINT('Ctrl Pts',(-1.37605453125945,6.87791795120786,
98.3364213787646));
#136602=CARTESIAN_POINT('Ctrl Pts',(-1.57493393018921,6.83207213647798,
98.3457089575932));
#136603=CARTESIAN_POINT('Ctrl Pts',(-1.71498653189518,6.79978711517964,
98.3522493513469));
#136604=CARTESIAN_POINT('Ctrl Pts',(-1.85406084048954,6.76319120099996,
98.3587897451006));
#136605=CARTESIAN_POINT('Ctrl Pts',(-1.99190816243168,6.72234545638188,
98.3653301388543));
#136606=CARTESIAN_POINT('Ctrl Pts',(-2.16187146483879,6.67198337791161,
98.3733943283196));
#136607=CARTESIAN_POINT('Ctrl Pts',(-2.33009322388562,6.61512101676402,
98.3814585177849));
#136608=CARTESIAN_POINT('Ctrl Pts',(-2.49603703497894,6.55190244757304,
98.3895227072502));
#136609=CARTESIAN_POINT('Ctrl Pts',(-2.66187495731322,6.48872421815607,
98.3975817509555));
#136610=CARTESIAN_POINT('Ctrl Pts',(-2.82543748715378,6.41919798424373,
98.4056407946608));
#136611=CARTESIAN_POINT('Ctrl Pts',(-2.98620339037331,6.34351762619313,
98.4136998383661));
#136612=CARTESIAN_POINT('Ctrl Pts',(-3.14689695607494,6.26787132094319,
98.4217552558597));
#136613=CARTESIAN_POINT('Ctrl Pts',(-3.30479607283688,6.18607656046159,
98.4298106733532));
#136614=CARTESIAN_POINT('Ctrl Pts',(-3.45939951679128,6.09837532017539,
98.4378660908467));
#136615=CARTESIAN_POINT('Ctrl Pts',(-3.6139828025575,6.01068551493915,98.4459204580232));
#136616=CARTESIAN_POINT('Ctrl Pts',(-3.76527095206601,5.91709093717395,
98.4539748251997));
#136617=CARTESIAN_POINT('Ctrl Pts',(-3.9127872078662,5.81787958181145,98.4620291923763));
#136618=CARTESIAN_POINT('Ctrl Pts',(-4.06029085707759,5.71867670495022,
98.4700828712348));
#136619=CARTESIAN_POINT('Ctrl Pts',(-4.20402295517393,5.61385821278636,
98.4781365500933));
#136620=CARTESIAN_POINT('Ctrl Pts',(-4.34353582520709,5.50375536317182,
98.4861902289519));
#136621=CARTESIAN_POINT('Ctrl Pts',(-4.48309818949812,5.39361345293994,
98.4942467649723));
#136622=CARTESIAN_POINT('Ctrl Pts',(-4.618438051683,5.27818366766274,98.5023033009927));
#136623=CARTESIAN_POINT('Ctrl Pts',(-4.74914061079583,5.15783772732235,
98.5103598370132));
#136624=CARTESIAN_POINT('Ctrl Pts',(-4.82288988548959,5.08993220295707,
98.514905759389));
#136625=CARTESIAN_POINT('Ctrl Pts',(-4.89516335786863,5.02046217444464,
98.5194516817649));
#136626=CARTESIAN_POINT('Ctrl Pts',(-4.96589168557372,4.94949960396501,
98.5239976041407));
#136627=CARTESIAN_POINT('Ctrl Pts',(-5.10456501019901,4.81036701181046,
98.5329105558505));
#136628=CARTESIAN_POINT('Ctrl Pts',(-5.23733419342935,4.66545741062056,
98.5418235075603));
#136629=CARTESIAN_POINT('Ctrl Pts',(-5.36375573085588,4.51527972801361,
98.55073645927));
#136630=CARTESIAN_POINT('Ctrl Pts',(-5.49025725909741,4.36500702334421,
98.5596550504799));
#136631=CARTESIAN_POINT('Ctrl Pts',(-5.610402964147,4.2094597634051,98.5685736416897));
#136632=CARTESIAN_POINT('Ctrl Pts',(-5.72378996119578,4.04917955178755,
98.5774922328996));
#136633=CARTESIAN_POINT('Ctrl Pts',(-5.83725514329902,3.88878882029207,
98.5864169738494));
#136634=CARTESIAN_POINT('Ctrl Pts',(-5.94395216187342,3.72365880958179,
98.5953417147991));
#136635=CARTESIAN_POINT('Ctrl Pts',(-6.04352085889862,3.55436101016165,
98.6042664557489));
#136636=CARTESIAN_POINT('Ctrl Pts',(-6.14310049495826,3.38504461097556,
98.6131921772081));
#136637=CARTESIAN_POINT('Ctrl Pts',(-6.23555012738276,3.21155971822971,
98.6221178986673));
#136638=CARTESIAN_POINT('Ctrl Pts',(-6.32055488329104,3.03450367108129,
98.6310436201265));
#136639=CARTESIAN_POINT('Ctrl Pts',(-6.40555790760715,2.85745123065887,
98.639969159764));
#136640=CARTESIAN_POINT('Ctrl Pts',(-6.48311625585947,2.67682799858681,
98.6488946994016));
#136641=CARTESIAN_POINT('Ctrl Pts',(-6.5529621118045,2.49325372229837,98.6578202390391));
#136642=CARTESIAN_POINT('Ctrl Pts',(-6.61776896624475,2.32292333917929,
98.6661018491684));
#136643=CARTESIAN_POINT('Ctrl Pts',(-6.6759364286139,2.15005271927232,98.6743834592978));
#136644=CARTESIAN_POINT('Ctrl Pts',(-6.72728788244172,1.97515171803403,
98.6826650694271));
#136645=CARTESIAN_POINT('Ctrl Pts',(-6.77907180886219,1.79877773241411,
98.6910164257689));
#136646=CARTESIAN_POINT('Ctrl Pts',(-6.82393755001743,1.62029056482418,
98.6993677821106));
#136647=CARTESIAN_POINT('Ctrl Pts',(-6.86172539517139,1.44026079713366,
98.7077191384523));
#136648=CARTESIAN_POINT('Ctrl Pts',(-6.89949937822043,1.26029707161937,
98.7160674311799));
#136649=CARTESIAN_POINT('Ctrl Pts',(-6.93020057416912,1.07879219770262,
98.7244157239074));
#136650=CARTESIAN_POINT('Ctrl Pts',(-6.95371995337474,0.896328830585069,
98.732764016635));
#136651=CARTESIAN_POINT('Ctrl Pts',(-6.97723395162914,0.713907208892388,
98.7411103993735));
#136652=CARTESIAN_POINT('Ctrl Pts',(-6.9935693678918,0.530527859306804,
98.749456782112));
#136653=CARTESIAN_POINT('Ctrl Pts',(-7.00266874717405,0.34678088161229,
98.7578031648505));
#136654=CARTESIAN_POINT('Ctrl Pts',(-7.01176860716349,0.163024196827935,
98.7661499885165));
#136655=CARTESIAN_POINT('Ctrl Pts',(-7.01363164572051,-0.0210998245922531,
98.7744968121825));
#136656=CARTESIAN_POINT('Ctrl Pts',(-7.00825244637519,-0.204998074079166,
98.7828436358485));
#136657=CARTESIAN_POINT('Ctrl Pts',(-7.00287315096121,-0.388899607857806,
98.7911906085828));
#136658=CARTESIAN_POINT('Ctrl Pts',(-6.99025137322791,-0.572575031011566,
98.7995375813171));
#136659=CARTESIAN_POINT('Ctrl Pts',(-6.97043378629742,-0.755433248767463,
98.8078845540514));
#136660=CARTESIAN_POINT('Ctrl Pts',(-6.95060935228493,-0.938354645013073,
98.8162344107093));
#136661=CARTESIAN_POINT('Ctrl Pts',(-6.92358418101597,-1.12045794309513,
98.8245842673672));
#136662=CARTESIAN_POINT('Ctrl Pts',(-6.88945667745396,-1.30115842693544,
98.8329341240251));
#136663=CARTESIAN_POINT('Ctrl Pts',(-6.87801469298139,-1.36174217653577,
98.8357335942546));
#136664=CARTESIAN_POINT('Ctrl Pts',(-6.8657747823401,-1.42216831972912,
98.8385330644841));
#136665=CARTESIAN_POINT('Ctrl Pts',(-6.85274193659795,-1.48241509466538,
98.8413325347136));
#136666=CARTESIAN_POINT('Ctrl Pts',(-6.81252228002241,-1.66833800403309,
98.8499717631254));
#136667=CARTESIAN_POINT('Ctrl Pts',(-6.76472908610655,-1.85263628174999,
98.8586109915372));
#136668=CARTESIAN_POINT('Ctrl Pts',(-6.70951829686725,-2.03469673084309,
98.8672502199491));
#136669=CARTESIAN_POINT('Ctrl Pts',(-6.65431427480106,-2.21673486483092,
98.8758883894528));
#136670=CARTESIAN_POINT('Ctrl Pts',(-6.59169455695587,-2.39653544071446,
98.8845265589565));
#136671=CARTESIAN_POINT('Ctrl Pts',(-6.52186501817443,-2.57350019374638,
98.8931647284602));
#136672=CARTESIAN_POINT('Ctrl Pts',(-6.44989512403187,-2.75588911919146,
98.9020676677552));
#136673=CARTESIAN_POINT('Ctrl Pts',(-6.37026650450204,-2.93526531040483,
98.9109706070502));
#136674=CARTESIAN_POINT('Ctrl Pts',(-6.28325856614577,-3.11099475304215,
98.9198735463451));
#136675=CARTESIAN_POINT('Ctrl Pts',(-6.19884731142619,-3.28147968837587,
98.9285107844039));
#136676=CARTESIAN_POINT('Ctrl Pts',(-6.10749100141248,-3.4485321420625,
98.9371480224626));
#136677=CARTESIAN_POINT('Ctrl Pts',(-6.00949230902887,-3.61159642682055,
98.9457852605213));
#136678=CARTESIAN_POINT('Ctrl Pts',(-5.90697162010975,-3.78218505820817,
98.9548210504344));
#136679=CARTESIAN_POINT('Ctrl Pts',(-5.7971811902196,-3.94840845108879,
98.9638568403475));
#136680=CARTESIAN_POINT('Ctrl Pts',(-5.68051992566416,-4.10966177886119,
98.9728926302607));
#136681=CARTESIAN_POINT('Ctrl Pts',(-5.56385866110871,-4.27091510663359,
98.9819284201738));
#136682=CARTESIAN_POINT('Ctrl Pts',(-5.44032677457857,-4.42719807501081,
98.9909642100869));
#136683=CARTESIAN_POINT('Ctrl Pts',(-5.31037376991249,-4.5779424402591,
99.));
#136684=CARTESIAN_POINT('',(6.57110895151814,2.44502632087636,99.));
#136685=CARTESIAN_POINT('Origin',(0.,0.,99.));
#136686=CARTESIAN_POINT('',(6.57110895151814,2.44502632087636,100.));
#136687=CARTESIAN_POINT('',(6.57110895151814,2.44502632087636,50.));
#136688=CARTESIAN_POINT('Origin',(0.,0.,100.));
#136689=CARTESIAN_POINT('',(5.30919883249413,-4.57930500398728,98.9999997423022));
#136690=CARTESIAN_POINT('Origin',(0.,0.,99.));
#136691=CARTESIAN_POINT('Ctrl Pts',(5.30919883249413,-4.57930500398728,
98.9999997423022));
#136692=CARTESIAN_POINT('Ctrl Pts',(5.1771100183101,-4.73244740822565,98.9907957854639));
#136693=CARTESIAN_POINT('Ctrl Pts',(5.03841024186428,-4.87985060242226,
98.9815918286256));
#136694=CARTESIAN_POINT('Ctrl Pts',(4.89359335576069,-5.02099299252198,
98.9723878717873));
#136695=CARTESIAN_POINT('Ctrl Pts',(4.74881129474558,-5.16210144116393,
98.9631861282863));
#136696=CARTESIAN_POINT('Ctrl Pts',(4.5979151966278,-5.29695196574323,98.9539843847853));
#136697=CARTESIAN_POINT('Ctrl Pts',(4.44143525768772,-5.42506031434384,
98.9447826412843));
#136698=CARTESIAN_POINT('Ctrl Pts',(4.28516511768279,-5.55299690293928,
98.9355932349301));
#136699=CARTESIAN_POINT('Ctrl Pts',(4.12332623737974,-5.67420925880788,
98.9264038285759));
#136700=CARTESIAN_POINT('Ctrl Pts',(3.95648126930452,-5.78825384102516,
98.9172144222218));
#136701=CARTESIAN_POINT('Ctrl Pts',(3.7898528000229,-5.90215043847101,98.9080369400833));
#136702=CARTESIAN_POINT('Ctrl Pts',(3.61823136495096,-6.00889772772026,
98.8988594579449));
#136703=CARTESIAN_POINT('Ctrl Pts',(3.44220988246632,-6.10809443996663,
98.8896819758064));
#136704=CARTESIAN_POINT('Ctrl Pts',(3.26664748991357,-6.2070324325884,98.8805284298921));
#136705=CARTESIAN_POINT('Ctrl Pts',(3.08670811923343,-6.298459067213,98.8713748839777));
#136706=CARTESIAN_POINT('Ctrl Pts',(2.90301021953404,-6.38201835063022,
98.8622213380634));
#136707=CARTESIAN_POINT('Ctrl Pts',(2.82012422293177,-6.41972098355495,
98.8580911831907));
#136708=CARTESIAN_POINT('Ctrl Pts',(2.73647342651385,-6.4558224925914,98.8539610283179));
#136709=CARTESIAN_POINT('Ctrl Pts',(2.65211653575429,-6.4902930937885,98.8498308734452));
#136710=CARTESIAN_POINT('Ctrl Pts',(2.484685180337,-6.55871026076219,98.8416333519125));
#136711=CARTESIAN_POINT('Ctrl Pts',(2.31456968522284,-6.62065883490146,
98.8334358303799));
#136712=CARTESIAN_POINT('Ctrl Pts',(2.14230841566089,-6.67593747833879,
98.8252383088473));
#136713=CARTESIAN_POINT('Ctrl Pts',(1.97005289241332,-6.73121427778377,
98.8170410607687));
#136714=CARTESIAN_POINT('Ctrl Pts',(1.79565206880699,-6.77982148391708,
98.8088438126901));
#136715=CARTESIAN_POINT('Ctrl Pts',(1.61966035177888,-6.82160735511621,
98.8006465646115));
#136716=CARTESIAN_POINT('Ctrl Pts',(1.44364490626395,-6.86339886019124,
98.7924482113202));
#136717=CARTESIAN_POINT('Ctrl Pts',(1.26603847867586,-6.89836711822544,
98.7842498580288));
#136718=CARTESIAN_POINT('Ctrl Pts',(1.08740676175789,-6.92641127114058,
98.7760515047374));
#136719=CARTESIAN_POINT('Ctrl Pts',(0.908653707047861,-6.95447447339171,
98.7678475826137));
#136720=CARTESIAN_POINT('Ctrl Pts',(0.728874315825774,-6.97560412070713,
98.75964366049));
#136721=CARTESIAN_POINT('Ctrl Pts',(0.548641355379238,-6.98975101313828,
98.7514397383663));
#136722=CARTESIAN_POINT('Ctrl Pts',(0.368339379079348,-7.00390332277975,
98.743232674749));
#136723=CARTESIAN_POINT('Ctrl Pts',(0.187583834699411,-7.01106752899978,
98.7350256111317));
#136724=CARTESIAN_POINT('Ctrl Pts',(0.00694885280283358,-7.0112465564937,
98.7268185475144));
#136725=CARTESIAN_POINT('Ctrl Pts',(-0.173861858941698,-7.01142575815363,
98.7186034996959));
#136726=CARTESIAN_POINT('Ctrl Pts',(-0.354551426213798,-7.0046062164084,
98.7103884518773));
#136727=CARTESIAN_POINT('Ctrl Pts',(-0.534548563102414,-6.99084289597364,
98.7021734040588));
#136728=CARTESIAN_POINT('Ctrl Pts',(-0.614960663067569,-6.98469425651313,
98.6985034054254));
#136729=CARTESIAN_POINT('Ctrl Pts',(-0.695234661301516,-6.9771604840988,
98.694833406792));
#136730=CARTESIAN_POINT('Ctrl Pts',(-0.775320191889768,-6.96824979191677,
98.6911634081586));
#136731=CARTESIAN_POINT('Ctrl Pts',(-0.953332438725084,-6.94844331346142,
98.6830058209163));
#136732=CARTESIAN_POINT('Ctrl Pts',(-1.13078883931262,-6.92178858772011,
98.674848233674));
#136733=CARTESIAN_POINT('Ctrl Pts',(-1.30712494444462,-6.888327151211,98.6666906464318));
#136734=CARTESIAN_POINT('Ctrl Pts',(-1.48330105598853,-6.85489607499189,
98.658540460746));
#136735=CARTESIAN_POINT('Ctrl Pts',(-1.65835855125987,-6.81467065416924,
98.6503902750603));
#136736=CARTESIAN_POINT('Ctrl Pts',(-1.83173834329883,-6.76774417396143,
98.6422400893746));
#136737=CARTESIAN_POINT('Ctrl Pts',(-2.00499456597536,-6.72085113868496,
98.6340957124007));
#136738=CARTESIAN_POINT('Ctrl Pts',(-2.17657512720499,-6.6672666495458,
98.6259513354268));
#136739=CARTESIAN_POINT('Ctrl Pts',(-2.34593121972154,-6.60713502774356,
98.6178069584529));
#136740=CARTESIAN_POINT('Ctrl Pts',(-2.51519956181038,-6.54703456263284,
98.609666801419));
#136741=CARTESIAN_POINT('Ctrl Pts',(-2.68224539890693,-6.48039384135971,
98.6015266443852));
#136742=CARTESIAN_POINT('Ctrl Pts',(-2.84653502872651,-6.40740703348343,
98.5933864873514));
#136743=CARTESIAN_POINT('Ctrl Pts',(-3.01077149323238,-6.33444384466663,
98.5852489645313));
#136744=CARTESIAN_POINT('Ctrl Pts',(-3.17225320489725,-6.25513880485666,
98.5771114417113));
#136745=CARTESIAN_POINT('Ctrl Pts',(-3.33046625360379,-6.16973428083466,
98.5689739188912));
#136746=CARTESIAN_POINT('Ctrl Pts',(-3.48869526370216,-6.08432114074032,
98.5608355751136));
#136747=CARTESIAN_POINT('Ctrl Pts',(-3.64365463637564,-5.99280744701719,
98.5526972313361));
#136748=CARTESIAN_POINT('Ctrl Pts',(-3.79485442333845,-5.89548186903909,
98.5445588875585));
#136749=CARTESIAN_POINT('Ctrl Pts',(-3.94606937133707,-5.79814653207519,
98.5364197277366));
#136750=CARTESIAN_POINT('Ctrl Pts',(-4.09352368424749,-5.6949983404261,
98.5282805679148));
#136751=CARTESIAN_POINT('Ctrl Pts',(-4.2367559690505,-5.58636961015067,
98.5201414080929));
#136752=CARTESIAN_POINT('Ctrl Pts',(-4.38002786946146,-5.47771083502051,
98.5119999971182));
#136753=CARTESIAN_POINT('Ctrl Pts',(-4.51907513284052,-5.36356871458079,
98.5038585861435));
#136754=CARTESIAN_POINT('Ctrl Pts',(-4.65346897011211,-5.24431626684582,
98.4957171751688));
#136755=CARTESIAN_POINT('Ctrl Pts',(-4.78792367424638,-5.12500980977154,
98.4875720769555));
#136756=CARTESIAN_POINT('Ctrl Pts',(-4.91772048849832,-5.00058864849225,
98.4794269787422));
#136757=CARTESIAN_POINT('Ctrl Pts',(-5.04246696640795,-4.87146317395345,
98.4712818805289));
#136758=CARTESIAN_POINT('Ctrl Pts',(-5.16737490010428,-4.74217057601826,
98.4631262403488));
#136759=CARTESIAN_POINT('Ctrl Pts',(-5.28721919142131,-4.60816175451725,
98.4549706001686));
#136760=CARTESIAN_POINT('Ctrl Pts',(-5.40164643868908,-4.46988168902686,
98.4468149599884));
#136761=CARTESIAN_POINT('Ctrl Pts',(-5.51614987536136,-4.33150955214528,
98.4386538895162));
#136762=CARTESIAN_POINT('Ctrl Pts',(-5.62522886349904,-4.18886078260711,
98.430492819044));
#136763=CARTESIAN_POINT('Ctrl Pts',(-5.72857299043121,-4.04240993168704,
98.4223317485718));
#136764=CARTESIAN_POINT('Ctrl Pts',(-5.83209280457585,-3.89571011120744,
98.4141568041063));
#136765=CARTESIAN_POINT('Ctrl Pts',(-5.92985807979365,-3.74519558773904,
98.4059818596407));
#136766=CARTESIAN_POINT('Ctrl Pts',(-6.02160329608752,-3.5913674703444,
98.3978069151753));
#136767=CARTESIAN_POINT('Ctrl Pts',(-6.11130449435766,-3.4409665337578,
98.3898141026454));
#136768=CARTESIAN_POINT('Ctrl Pts',(-6.19525095684959,-3.2873983863897,
98.3818212901156));
#136769=CARTESIAN_POINT('Ctrl Pts',(-6.27323931727951,-3.13114915496507,
98.3738284775858));
#136770=CARTESIAN_POINT('Ctrl Pts',(-6.35305293961989,-2.97124302180428,
98.3656485989837));
#136771=CARTESIAN_POINT('Ctrl Pts',(-6.42687058601045,-2.80803900398797,
98.3574687203816));
#136772=CARTESIAN_POINT('Ctrl Pts',(-6.49440774852088,-2.64202470814562,
98.3492888417795));
#136773=CARTESIAN_POINT('Ctrl Pts',(-6.56185810388284,-2.47622379449305,
98.3411194769732));
#136774=CARTESIAN_POINT('Ctrl Pts',(-6.62304391942586,-2.30762011976299,
98.3329501121669));
#136775=CARTESIAN_POINT('Ctrl Pts',(-6.67772617466965,-2.1367263977009,
98.3247807473606));
#136776=CARTESIAN_POINT('Ctrl Pts',(-6.73234876599036,-1.96601913813642,
98.3166202961653));
#136777=CARTESIAN_POINT('Ctrl Pts',(-6.78048182329003,-1.79302714164819,
98.3084598449701));
#136778=CARTESIAN_POINT('Ctrl Pts',(-6.82193404566059,-1.61828379438126,
98.3002993937748));
#136779=CARTESIAN_POINT('Ctrl Pts',(-6.86334908685656,-1.4436971857047,
98.2921462622151));
#136780=CARTESIAN_POINT('Ctrl Pts',(-6.8980951487709,-1.26736269732559,
98.2839931306554));
#136781=CARTESIAN_POINT('Ctrl Pts',(-6.9260304405994,-1.08982975660906,
98.2758399990957));
#136782=CARTESIAN_POINT('Ctrl Pts',(-6.95394609699602,-0.912421601986873,
98.267692598289));
#136783=CARTESIAN_POINT('Ctrl Pts',(-6.97506046598524,-0.733817021096435,
98.2595451974824));
#136784=CARTESIAN_POINT('Ctrl Pts',(-6.98928259890362,-0.55457669908059,
98.2513977966758));
#136785=CARTESIAN_POINT('Ctrl Pts',(-7.00349787038182,-0.375422851206992,
98.2432543265667));
#136786=CARTESIAN_POINT('Ctrl Pts',(-7.0108275023445,-0.195634224794824,
98.2351108564576));
#136787=CARTESIAN_POINT('Ctrl Pts',(-7.01123224688891,-0.0157779176411367,
98.2269673863485));
#136788=CARTESIAN_POINT('Ctrl Pts',(-7.01163688829294,0.164032557030121,
98.2188259914263));
#136789=CARTESIAN_POINT('Ctrl Pts',(-7.00512015578728,0.343910325018181,
98.2106845965041));
#136790=CARTESIAN_POINT('Ctrl Pts',(-6.99169489609842,0.52328676877144,
98.2025432015819));
#136791=CARTESIAN_POINT('Ctrl Pts',(-6.97827069720004,0.702649039180833,
98.1944024499482));
#136792=CARTESIAN_POINT('Ctrl Pts',(-6.95793908487443,0.881509711912927,
98.1862616983144));
#136793=CARTESIAN_POINT('Ctrl Pts',(-6.93076491789004,1.05930364647948,
98.1781209466806));
#136794=CARTESIAN_POINT('Ctrl Pts',(-6.90358812057128,1.23711479068111,
98.1699794070595));
#136795=CARTESIAN_POINT('Ctrl Pts',(-6.86956750309773,1.41385864178933,
98.1618378674384));
#136796=CARTESIAN_POINT('Ctrl Pts',(-6.8288193624975,1.58897850107521,98.1536963278174));
#136797=CARTESIAN_POINT('Ctrl Pts',(-6.7880413816028,1.76422660248681,98.1455488260607));
#136798=CARTESIAN_POINT('Ctrl Pts',(-6.74052611274211,1.93784799085549,
98.137401324304));
#136799=CARTESIAN_POINT('Ctrl Pts',(-6.686440473137,2.10929854731269,98.1292538225473));
#136800=CARTESIAN_POINT('Ctrl Pts',(-6.63233537602699,2.28081078372907,
98.1211033896973));
#136801=CARTESIAN_POINT('Ctrl Pts',(-6.57165531206145,2.45015029747929,
98.1129529568474));
#136802=CARTESIAN_POINT('Ctrl Pts',(-6.50461607236333,2.61679122469728,
98.1048025239974));
#136803=CARTESIAN_POINT('Ctrl Pts',(-6.43749721470718,2.78363006004203,
98.0966424114311));
#136804=CARTESIAN_POINT('Ctrl Pts',(-6.36400422905059,2.94776357935998,
98.0884822988648));
#136805=CARTESIAN_POINT('Ctrl Pts',(-6.28440028100436,3.10868777309853,
98.0803221862986));
#136806=CARTESIAN_POINT('Ctrl Pts',(-6.20691549353777,3.26532795560334,
98.0723793065367));
#136807=CARTESIAN_POINT('Ctrl Pts',(-6.12364114321325,3.41892726396414,
98.0644364267749));
#136808=CARTESIAN_POINT('Ctrl Pts',(-6.03485983288451,3.56904656174967,
98.056493547013));
#136809=CARTESIAN_POINT('Ctrl Pts',(-5.94312944520581,3.72415242054961,
98.0482868260585));
#136810=CARTESIAN_POINT('Ctrl Pts',(-5.84532617622673,3.87587088288904,
98.0400801051041));
#136811=CARTESIAN_POINT('Ctrl Pts',(-5.74172845038692,4.02370239512286,
98.0318733841496));
#136812=CARTESIAN_POINT('Ctrl Pts',(-5.63821157388823,4.17141853725309,
98.0236730678529));
#136813=CARTESIAN_POINT('Ctrl Pts',(-5.52890944775676,4.31525348752236,
98.0154727515562));
#136814=CARTESIAN_POINT('Ctrl Pts',(-5.41414514519593,4.45473443756767,
98.0072724352595));
#136815=CARTESIAN_POINT('Ctrl Pts',(-5.29945094383672,4.59413018880131,
97.9990771279422));
#136816=CARTESIAN_POINT('Ctrl Pts',(-5.17930143457146,4.72917697003867,
97.9908818206249));
#136817=CARTESIAN_POINT('Ctrl Pts',(-5.05406163144354,4.85943284633817,
97.9826865133076));
#136818=CARTESIAN_POINT('Ctrl Pts',(-4.92887574013236,4.98963265155837,
97.9744947338137));
#136819=CARTESIAN_POINT('Ctrl Pts',(-4.79860416295001,5.1150454105047,97.9663029543198));
#136820=CARTESIAN_POINT('Ctrl Pts',(-4.66365077155621,5.23526389434794,
97.9581111748259));
#136821=CARTESIAN_POINT('Ctrl Pts',(-4.52873164260583,5.35545185669812,
97.9499214750899));
#136822=CARTESIAN_POINT('Ctrl Pts',(-4.38913332932075,5.47044794100356,
97.9417317753539));
#136823=CARTESIAN_POINT('Ctrl Pts',(-4.24529511768192,5.57988314629313,
97.9335420756179));
#136824=CARTESIAN_POINT('Ctrl Pts',(-4.10145226324004,5.68932188392712,
97.9253521115351));
#136825=CARTESIAN_POINT('Ctrl Pts',(-3.95336951279808,5.79319917027657,
97.9171621474523));
#136826=CARTESIAN_POINT('Ctrl Pts',(-3.80151795593428,5.89118729911122,
97.9089721833696));
#136827=CARTESIAN_POINT('Ctrl Pts',(-3.73263068242256,5.93563949421112,
97.9052568161552));
#136828=CARTESIAN_POINT('Ctrl Pts',(-3.66296820624811,5.97888029959546,
97.9015414489408));
#136829=CARTESIAN_POINT('Ctrl Pts',(-3.59257642105848,6.0208820966163,97.8978260817265));
#136830=CARTESIAN_POINT('Ctrl Pts',(-3.41746583716212,6.12536814113416,
97.8885835242243));
#136831=CARTESIAN_POINT('Ctrl Pts',(-3.23796122535888,6.2221118422066,97.8793409667222));
#136832=CARTESIAN_POINT('Ctrl Pts',(-3.05472541607505,6.31080654075889,
97.87009840922));
#136833=CARTESIAN_POINT('Ctrl Pts',(-2.87104650154399,6.39971572296741,
97.8608335011427));
#136834=CARTESIAN_POINT('Ctrl Pts',(-2.68361848852826,6.48053689191889,
97.8515685930654));
#136835=CARTESIAN_POINT('Ctrl Pts',(-2.49312555264651,6.55301087602036,
97.842303684988));
#136836=CARTESIAN_POINT('Ctrl Pts',(-2.30217615924768,6.62565852165254,
97.8330165764185));
#136837=CARTESIAN_POINT('Ctrl Pts',(-2.1081472996239,6.68991889388874,97.823729467849));
#136838=CARTESIAN_POINT('Ctrl Pts',(-1.91174218984874,6.74558139540636,
97.8144423592795));
#136839=CARTESIAN_POINT('Ctrl Pts',(-1.7152055888143,6.80128116241278,97.8051490330835));
#136840=CARTESIAN_POINT('Ctrl Pts',(-1.51628971767753,6.84837151553349,
97.7958557068876));
#136841=CARTESIAN_POINT('Ctrl Pts',(-1.31571086995579,6.88669234605265,
97.7865623806916));
#136842=CARTESIAN_POINT('Ctrl Pts',(-1.1151328186216,6.92501302442102,97.7772690913943));
#136843=CARTESIAN_POINT('Ctrl Pts',(-0.91289196559286,6.95456422419558,
97.767975802097));
#136844=CARTESIAN_POINT('Ctrl Pts',(-0.70971382144022,6.97523711813131,
97.7586825127997));
#136845=CARTESIAN_POINT('Ctrl Pts',(-0.567430900862935,6.9897140675996,
97.7521745473465));
#136846=CARTESIAN_POINT('Ctrl Pts',(-0.424688526410234,6.9998381515994,
97.7456665818933));
#136847=CARTESIAN_POINT('Ctrl Pts',(-0.281737904203388,7.00558707859913,
97.7391586164402));
#136848=CARTESIAN_POINT('Ctrl Pts',(-0.104003942046718,7.01273485842714,
97.7310671057652));
#136849=CARTESIAN_POINT('Ctrl Pts',(0.074172782514224,7.01312142222496,
97.7229755950903));
#136850=CARTESIAN_POINT('Ctrl Pts',(0.252234662995551,7.00671137105586,
97.7148840844154));
#136851=CARTESIAN_POINT('Ctrl Pts',(0.430183508086654,7.00030538904875,
97.706797710309));
#136852=CARTESIAN_POINT('Ctrl Pts',(0.608017295115993,6.9871113957849,97.6987113362028));
#136853=CARTESIAN_POINT('Ctrl Pts',(0.785176856298677,6.96714603455625,
97.6906249620965));
#136854=CARTESIAN_POINT('Ctrl Pts',(0.962256743157727,6.94718965238942,
97.6825422246913));
#136855=CARTESIAN_POINT('Ctrl Pts',(1.13866265030707,6.92046800781678,97.6744594872862));
#136856=CARTESIAN_POINT('Ctrl Pts',(1.31383894351843,6.88704971616979,97.6663767498811));
#136857=CARTESIAN_POINT('Ctrl Pts',(1.48899055770657,6.85363613252741,97.6582951511807));
#136858=CARTESIAN_POINT('Ctrl Pts',(1.66291254773099,6.81352784263588,97.6502135524802));
#136859=CARTESIAN_POINT('Ctrl Pts',(1.83505767294284,6.76684489991263,97.6421319537798));
#136860=CARTESIAN_POINT('Ctrl Pts',(2.00718729147749,6.72016616234665,97.6340510830624));
#136861=CARTESIAN_POINT('Ctrl Pts',(2.17754001682589,6.66691404980923,97.6259702123451));
#136862=CARTESIAN_POINT('Ctrl Pts',(2.3455822066528,6.60725893804184,97.6178893416278));
#136863=CARTESIAN_POINT('Ctrl Pts',(2.51368048927288,6.54758391328802,97.6098057735009));
#136864=CARTESIAN_POINT('Ctrl Pts',(2.6794663562817,6.48150174259789,97.601722205374));
#136865=CARTESIAN_POINT('Ctrl Pts',(2.84242424134802,6.40923170081229,97.5936386372471));
#136866=CARTESIAN_POINT('Ctrl Pts',(2.93077163506064,6.37005059685612,97.5892561418826));
#136867=CARTESIAN_POINT('Ctrl Pts',(3.01828816611891,6.32905155411019,97.5848736465181));
#136868=CARTESIAN_POINT('Ctrl Pts',(3.10489448994278,6.28627526988939,97.5804911511536));
#136869=CARTESIAN_POINT('Ctrl Pts',(3.277718236653,6.20091478600125,97.5717458397792));
#136870=CARTESIAN_POINT('Ctrl Pts',(3.44697940374861,6.10844346605425,97.5630005284048));
#136871=CARTESIAN_POINT('Ctrl Pts',(3.61211310649003,6.00918176363663,97.5542552170304));
#136872=CARTESIAN_POINT('Ctrl Pts',(3.77730538342132,5.90988485233246,97.545506803627));
#136873=CARTESIAN_POINT('Ctrl Pts',(3.9383670408984,5.8037928900154,97.5367583902237));
#136874=CARTESIAN_POINT('Ctrl Pts',(4.09476082785114,5.69127053698872,97.5280099768203));
#136875=CARTESIAN_POINT('Ctrl Pts',(4.25295023697523,5.57745626798632,97.5191611192409));
#136876=CARTESIAN_POINT('Ctrl Pts',(4.40636368953413,5.45706319407653,97.5103122616615));
#136877=CARTESIAN_POINT('Ctrl Pts',(4.55447803405557,5.3305118328173,97.5014634040821));
#136878=CARTESIAN_POINT('Ctrl Pts',(4.70102050149525,5.20530350949996,97.4927084558163));
#136879=CARTESIAN_POINT('Ctrl Pts',(4.8423755982364,5.07406717296795,97.4839535075504));
#136880=CARTESIAN_POINT('Ctrl Pts',(4.97807157498248,4.93724922976868,97.4751985592846));
#136881=CARTESIAN_POINT('Ctrl Pts',(5.11595085121495,4.79822993504611,97.4663027470484));
#136882=CARTESIAN_POINT('Ctrl Pts',(5.24798713545722,4.65344808565009,97.4574069348122));
#136883=CARTESIAN_POINT('Ctrl Pts',(5.37372534685317,4.50341009226206,97.448511122576));
#136884=CARTESIAN_POINT('Ctrl Pts',(5.49946355824921,4.35337209887392,97.4396153103398));
#136885=CARTESIAN_POINT('Ctrl Pts',(5.6189035135465,4.19807819036032,97.4307194981035));
#136886=CARTESIAN_POINT('Ctrl Pts',(5.73163312037174,4.03806987754766,97.4218236858673));
#136887=CARTESIAN_POINT('Ctrl Pts',(5.8419003989686,3.88155659143215,97.4131221829186));
#136888=CARTESIAN_POINT('Ctrl Pts',(5.94576620740795,3.72050586677001,97.4044206799699));
#136889=CARTESIAN_POINT('Ctrl Pts',(6.04287835083162,3.55545324811767,97.3957191770212));
#136890=CARTESIAN_POINT('Ctrl Pts',(6.13996630054085,3.39044174930662,97.3870198418928));
#136891=CARTESIAN_POINT('Ctrl Pts',(6.23030380207177,3.22143058842857,97.3783205067644));
#136892=CARTESIAN_POINT('Ctrl Pts',(6.31358332201366,3.04898215778495,97.369621171636));
#136893=CARTESIAN_POINT('Ctrl Pts',(6.39683952676313,2.87658200633825,97.3609242720004));
#136894=CARTESIAN_POINT('Ctrl Pts',(6.47304157317957,2.70074675880616,97.3522273723649));
#136895=CARTESIAN_POINT('Ctrl Pts',(6.54192863471235,2.52206191455139,97.3435304727293));
#136896=CARTESIAN_POINT('Ctrl Pts',(6.55180594541976,2.49644134537427,97.342283475427));
#136897=CARTESIAN_POINT('Ctrl Pts',(6.56153294711428,2.47076222716117,97.3410364781248));
#136898=CARTESIAN_POINT('Ctrl Pts',(6.57110895151819,2.44502632087623,97.3397894808225));
#136899=CARTESIAN_POINT('Origin',(0.,0.,50.));
#136900=CARTESIAN_POINT('',(6.57110895151813,2.44502632087639,95.3399143481975));
#136901=CARTESIAN_POINT('',(6.57110895151813,2.44502632087639,95.8870186122881));
#136902=CARTESIAN_POINT('',(6.57110895151814,2.44502632087636,50.));
#136903=CARTESIAN_POINT('',(7.01124672537777,-0.00677631017023138,97.77353435695));
#136904=CARTESIAN_POINT('Ctrl Pts',(6.57110895151813,2.44502632087639,95.8870186122881));
#136905=CARTESIAN_POINT('Ctrl Pts',(6.50690586284996,2.61757476628998,95.8953914287838));
#136906=CARTESIAN_POINT('Ctrl Pts',(6.43586635978878,2.78768965768491,95.9037642452794));
#136907=CARTESIAN_POINT('Ctrl Pts',(6.35819928900439,2.95481443813382,95.912137061775));
#136908=CARTESIAN_POINT('Ctrl Pts',(6.28057652111686,3.12184388716574,95.9205051022437));
#136909=CARTESIAN_POINT('Ctrl Pts',(6.19633386208586,3.28588632875983,95.9288731427123));
#136910=CARTESIAN_POINT('Ctrl Pts',(6.1057282037835,3.44640532497597,95.9372411831809));
#136911=CARTESIAN_POINT('Ctrl Pts',(6.01245558962609,3.61164915940669,95.9458555349169));
#136912=CARTESIAN_POINT('Ctrl Pts',(5.91243979135492,3.77315861949584,95.9544698866529));
#136913=CARTESIAN_POINT('Ctrl Pts',(5.80601246713503,3.93037476507936,95.9630842383889));
#136914=CARTESIAN_POINT('Ctrl Pts',(5.70269370606814,4.08299889145352,95.9714469793981));
#136915=CARTESIAN_POINT('Ctrl Pts',(5.59333289399702,4.23157669253178,95.9798097204073));
#136916=CARTESIAN_POINT('Ctrl Pts',(5.47827803891789,4.37562524570032,95.9881724614165));
#136917=CARTESIAN_POINT('Ctrl Pts',(5.36323424519919,4.51965995005766,95.9965343984328));
#136918=CARTESIAN_POINT('Ctrl Pts',(5.24249770521805,4.65916601800551,96.004896335449));
#136919=CARTESIAN_POINT('Ctrl Pts',(5.11645738452041,4.79369277226718,96.0132582724653));
#136920=CARTESIAN_POINT('Ctrl Pts',(4.99041236351663,4.92822454331179,96.0216205213156));
#136921=CARTESIAN_POINT('Ctrl Pts',(4.85906339258932,5.05777639092602,96.0299827701659));
#136922=CARTESIAN_POINT('Ctrl Pts',(4.72283733044507,5.1819334338309,96.0383450190162));
#136923=CARTESIAN_POINT('Ctrl Pts',(4.57942491439849,5.31264015185476,96.0471484028352));
#136924=CARTESIAN_POINT('Ctrl Pts',(4.43060722800965,5.43736721747777,96.0559517866542));
#136925=CARTESIAN_POINT('Ctrl Pts',(4.27692328648132,5.55567761520175,96.0647551704732));
#136926=CARTESIAN_POINT('Ctrl Pts',(4.13082347421755,5.66814952817087,96.0731241172249));
#136927=CARTESIAN_POINT('Ctrl Pts',(3.98032640648811,5.77482263252777,96.0814930639766));
#136928=CARTESIAN_POINT('Ctrl Pts',(3.82592628730087,5.87536506156343,96.0898620107283));
#136929=CARTESIAN_POINT('Ctrl Pts',(3.67147063940784,5.97594364983906,96.0982339673014));
#136930=CARTESIAN_POINT('Ctrl Pts',(3.51310941946559,6.0703869917153,96.1066059238745));
#136931=CARTESIAN_POINT('Ctrl Pts',(3.35136345900299,6.15840803521166,96.1149778804476));
#136932=CARTESIAN_POINT('Ctrl Pts',(3.18949261930352,6.24649703713312,96.1233563007589));
#136933=CARTESIAN_POINT('Ctrl Pts',(3.02423211134264,6.32815368596556,96.1317347210702));
#136934=CARTESIAN_POINT('Ctrl Pts',(2.85612568907477,6.4031377160504,96.1401131413815));
#136935=CARTESIAN_POINT('Ctrl Pts',(2.83022624279836,6.41469018877912,96.1414039692024));
#136936=CARTESIAN_POINT('Ctrl Pts',(2.80425928187736,6.42608437221039,96.1426947970233));
#136937=CARTESIAN_POINT('Ctrl Pts',(2.77822683336898,6.43731949066135,96.1439856248442));
#136938=CARTESIAN_POINT('Ctrl Pts',(2.61956441318577,6.50579522716002,96.1518529549587));
#136939=CARTESIAN_POINT('Ctrl Pts',(2.45813828963,6.56850053935752,96.1597202850731));
#136940=CARTESIAN_POINT('Ctrl Pts',(2.29442486448392,6.6251974388495,96.1675876151876));
#136941=CARTESIAN_POINT('Ctrl Pts',(2.13083753904812,6.68185066774701,96.1754488855177));
#136942=CARTESIAN_POINT('Ctrl Pts',(1.9649667732708,6.73250456367244,96.1833101558478));
#136943=CARTESIAN_POINT('Ctrl Pts',(1.79731079745251,6.7769683826812,96.1911714261779));
#136944=CARTESIAN_POINT('Ctrl Pts',(1.62974973387468,6.82140703014054,96.1990282461401));
#136945=CARTESIAN_POINT('Ctrl Pts',(1.46040583769709,6.85966247431982,96.2068850661022));
#136946=CARTESIAN_POINT('Ctrl Pts',(1.28979418669192,6.89159324963943,96.2147418860644));
#136947=CARTESIAN_POINT('Ctrl Pts',(1.11922361556596,6.92351633666586,96.2225968142612));
#136948=CARTESIAN_POINT('Ctrl Pts',(0.947386269688777,6.94911770765578,
96.230451742458));
#136949=CARTESIAN_POINT('Ctrl Pts',(0.774809094992643,6.96830663998196,
96.2383066706548));
#136950=CARTESIAN_POINT('Ctrl Pts',(0.602260058158601,6.98749244364682,
96.2461603181441));
#136951=CARTESIAN_POINT('Ctrl Pts',(0.428971811781385,7.00026785080371,
96.2540139656333));
#136952=CARTESIAN_POINT('Ctrl Pts',(0.255477670027856,7.00659387453113,
96.2618676131226));
#136953=CARTESIAN_POINT('Ctrl Pts',(0.0819260470819263,7.0129219941644,
96.2697238626422));
#136954=CARTESIAN_POINT('Ctrl Pts',(-0.0918312262693392,7.01279644828536,
96.2775801121618));
#136955=CARTESIAN_POINT('Ctrl Pts',(-0.265259376649008,7.00623037200461,
96.2854363616814));
#136956=CARTESIAN_POINT('Ctrl Pts',(-0.391946857025348,7.00143392080481,
96.2911752711645));
#136957=CARTESIAN_POINT('Ctrl Pts',(-0.518458670809771,6.99320179469873,
96.2969141806476));
#136958=CARTESIAN_POINT('Ctrl Pts',(-0.644587821142489,6.98155663898352,
96.3026530901307));
#136959=CARTESIAN_POINT('Ctrl Pts',(-0.856167445569638,6.96202207725754,
96.3122800186389));
#136960=CARTESIAN_POINT('Ctrl Pts',(-1.06656328869337,6.93289256428335,
96.3219069471471));
#136961=CARTESIAN_POINT('Ctrl Pts',(-1.27499597529445,6.89434636680541,
96.3315338756553));
#136962=CARTESIAN_POINT('Ctrl Pts',(-1.48453805742035,6.85559500487041,
96.3412120440701));
#136963=CARTESIAN_POINT('Ctrl Pts',(-1.69209598426225,6.80732651379363,
96.350890212485));
#136964=CARTESIAN_POINT('Ctrl Pts',(-1.89689796792049,6.74977071179452,
96.3605683808998));
#136965=CARTESIAN_POINT('Ctrl Pts',(-2.10266028247225,6.6919450265952,96.3702919309265));
#136966=CARTESIAN_POINT('Ctrl Pts',(-2.30564070363407,6.62474476635467,
96.3800154809532));
#136967=CARTESIAN_POINT('Ctrl Pts',(-2.50507743216264,6.54845123837457,
96.3897390309799));
#136968=CARTESIAN_POINT('Ctrl Pts',(-2.70471732201702,6.47207999204034,
96.3994724861495));
#136969=CARTESIAN_POINT('Ctrl Pts',(-2.90080625798182,6.38659697744,96.4092059413192));
#136970=CARTESIAN_POINT('Ctrl Pts',(-3.09260159059658,6.29233199730748,
96.4189393964888));
#136971=CARTESIAN_POINT('Ctrl Pts',(-3.28417339246208,6.19817687971098,
96.4286615076571));
#136972=CARTESIAN_POINT('Ctrl Pts',(-3.47146155105454,6.09526027641103,
96.4383836188253));
#136973=CARTESIAN_POINT('Ctrl Pts',(-3.65374801208486,5.98395788978214,
96.4481057299936));
#136974=CARTESIAN_POINT('Ctrl Pts',(-3.73633925582907,5.93352845859224,
96.4525106718014));
#136975=CARTESIAN_POINT('Ctrl Pts',(-3.81790402460925,5.88137818227656,
96.4569156136093));
#136976=CARTESIAN_POINT('Ctrl Pts',(-3.89837706152892,5.82754518203378,
96.4613205554172));
#136977=CARTESIAN_POINT('Ctrl Pts',(-4.04553163005805,5.72910510537479,
96.4693755181221));
#136978=CARTESIAN_POINT('Ctrl Pts',(-4.18910593293877,5.62498673950172,
96.477430480827));
#136979=CARTESIAN_POINT('Ctrl Pts',(-4.32863101602329,5.51548548086397,
96.4854854435318));
#136980=CARTESIAN_POINT('Ctrl Pts',(-4.46806543240111,5.40605537874001,
96.493535171931));
#136981=CARTESIAN_POINT('Ctrl Pts',(-4.6034555816486,5.29124957137755,96.5015849003301));
#136982=CARTESIAN_POINT('Ctrl Pts',(-4.73436169628476,5.17140656797082,
96.5096346287293));
#136983=CARTESIAN_POINT('Ctrl Pts',(-4.86520750587478,5.0516187731223,96.5176806488277));
#136984=CARTESIAN_POINT('Ctrl Pts',(-4.99157312599786,4.92679864863973,
96.5257266689261));
#136985=CARTESIAN_POINT('Ctrl Pts',(-5.11305210603228,4.79732474651226,
96.5337726890245));
#136986=CARTESIAN_POINT('Ctrl Pts',(-5.23451372401776,4.66786934908596,
96.5418175591676));
#136987=CARTESIAN_POINT('Ctrl Pts',(-5.35108983884386,4.53376175977768,
96.5498624293107));
#136988=CARTESIAN_POINT('Ctrl Pts',(-5.46241097454425,4.39541726206723,
96.5579072994538));
#136989=CARTESIAN_POINT('Ctrl Pts',(-5.57372174640787,4.25708564402948,
96.5659514206312));
#136990=CARTESIAN_POINT('Ctrl Pts',(-5.67977828811595,4.11451818967758,
96.5739955418085));
#136991=CARTESIAN_POINT('Ctrl Pts',(-5.78025169558937,3.96816291224745,
96.5820396629858));
#136992=CARTESIAN_POINT('Ctrl Pts',(-5.88076006093902,3.8217567131874,96.5900865829674));
#136993=CARTESIAN_POINT('Ctrl Pts',(-5.97568120713409,3.67156036037432,
96.5981335029489));
#136994=CARTESIAN_POINT('Ctrl Pts',(-6.06472960806618,3.5180507875165,96.6061804229304));
#136995=CARTESIAN_POINT('Ctrl Pts',(-6.1156619111596,3.43024914244823,96.6107829555214));
#136996=CARTESIAN_POINT('Ctrl Pts',(-6.16467382061371,3.34136410660787,
96.6153854881124));
#136997=CARTESIAN_POINT('Ctrl Pts',(-6.21171869217782,3.25148849786504,
96.6199880207034));
#136998=CARTESIAN_POINT('Ctrl Pts',(-6.30054239512213,3.08179764512179,
96.6286778943084));
#136999=CARTESIAN_POINT('Ctrl Pts',(-6.38239382465838,2.90849380649444,
96.6373677679135));
#137000=CARTESIAN_POINT('Ctrl Pts',(-6.45700612408139,2.73216003851814,
96.6460576415185));
#137001=CARTESIAN_POINT('Ctrl Pts',(-6.53163751285033,2.55578115604567,
96.6547497384031));
#137002=CARTESIAN_POINT('Ctrl Pts',(-6.59902596575416,2.37637105546818,
96.6634418352877));
#137003=CARTESIAN_POINT('Ctrl Pts',(-6.65895292057026,2.1945324249436,96.6721339321723));
#137004=CARTESIAN_POINT('Ctrl Pts',(-6.72015326945551,2.00882988652709,
96.6810107283238));
#137005=CARTESIAN_POINT('Ctrl Pts',(-6.77357138147929,1.82059474687604,
96.6898875244753));
#137006=CARTESIAN_POINT('Ctrl Pts',(-6.81902811021709,1.63048526352406,
96.6987643206267));
#137007=CARTESIAN_POINT('Ctrl Pts',(-6.8635689527695,1.44420620647746,96.7074622623998));
#137008=CARTESIAN_POINT('Ctrl Pts',(-6.90046611942902,1.25612789756716,
96.7161602041728));
#137009=CARTESIAN_POINT('Ctrl Pts',(-6.92960258056959,1.06688079833843,
96.7248581459458));
#137010=CARTESIAN_POINT('Ctrl Pts',(-6.95963773426022,0.871796512590155,
96.7338243692865));
#137011=CARTESIAN_POINT('Ctrl Pts',(-6.98142572935758,0.67547049536651,
96.7427905926273));
#137012=CARTESIAN_POINT('Ctrl Pts',(-6.99489582811806,0.478600999034294,
96.751756815968));
#137013=CARTESIAN_POINT('Ctrl Pts',(-7.00836592687853,0.281731502702078,
96.7607230393087));
#137014=CARTESIAN_POINT('Ctrl Pts',(-7.01351811730091,0.0843188530022396,
96.7696892626494));
#137015=CARTESIAN_POINT('Ctrl Pts',(-7.01034036778411,-0.112935779611952,
96.7786554859901));
#137016=CARTESIAN_POINT('Ctrl Pts',(-7.00723646838223,-0.305606263220677,
96.7874133365121));
#137017=CARTESIAN_POINT('Ctrl Pts',(-6.9961850954018,-0.498159174273043,
96.7961711870341));
#137018=CARTESIAN_POINT('Ctrl Pts',(-6.97722014547328,-0.689946087822666,
96.804929037556));
#137019=CARTESIAN_POINT('Ctrl Pts',(-6.95825895555,-0.881694977554558,96.81368515174));
#137020=CARTESIAN_POINT('Ctrl Pts',(-6.93138734865063,-1.07267790346411,
96.8224412659239));
#137021=CARTESIAN_POINT('Ctrl Pts',(-6.8966911077752,-1.26225129290268,
96.8311973801078));
#137022=CARTESIAN_POINT('Ctrl Pts',(-6.86164741998785,-1.45372306346503,
96.8400411777052));
#137023=CARTESIAN_POINT('Ctrl Pts',(-6.81862155666789,-1.64375663390734,
96.8488849753026));
#137024=CARTESIAN_POINT('Ctrl Pts',(-6.76775516826958,-1.83169772202196,
96.8577287729));
#137025=CARTESIAN_POINT('Ctrl Pts',(-6.71742360910297,-2.01766272355116,
96.866479583328));
#137026=CARTESIAN_POINT('Ctrl Pts',(-6.65941568651039,-2.20157876790658,
96.8752303937559));
#137027=CARTESIAN_POINT('Ctrl Pts',(-6.59391944735461,-2.38282456011741,
96.8839812041839));
#137028=CARTESIAN_POINT('Ctrl Pts',(-6.52737925176729,-2.56695926187337,
96.892871495366));
#137029=CARTESIAN_POINT('Ctrl Pts',(-6.45311007031312,-2.748337590493,96.9017617865481));
#137030=CARTESIAN_POINT('Ctrl Pts',(-6.37136138372586,-2.92632545703087,
96.9106520777301));
#137031=CARTESIAN_POINT('Ctrl Pts',(-6.28961269713865,-3.10431332356862,
96.9195423689122));
#137032=CARTESIAN_POINT('Ctrl Pts',(-6.2003846137979,-3.2789104543812,96.9284326600943));
#137033=CARTESIAN_POINT('Ctrl Pts',(-6.10397786506111,-3.44950442605079,
96.9373229512763));
#137034=CARTESIAN_POINT('Ctrl Pts',(-6.01631887157888,-3.6046190424717,
96.9454065552459));
#137035=CARTESIAN_POINT('Ctrl Pts',(-5.92269477698949,-3.75647621605383,
96.9534901592155));
#137036=CARTESIAN_POINT('Ctrl Pts',(-5.82338398339227,-3.90459031711016,
96.9615737631851));
#137037=CARTESIAN_POINT('Ctrl Pts',(-5.72410160994706,-4.05266203178416,
96.9696550538387));
#137038=CARTESIAN_POINT('Ctrl Pts',(-5.61913597920715,-4.19699250786991,
96.9777363444922));
#137039=CARTESIAN_POINT('Ctrl Pts',(-5.50880960624656,-4.33712384935289,
96.9858176351457));
#137040=CARTESIAN_POINT('Ctrl Pts',(-5.39849438982002,-4.47724102033392,
96.9938981085949));
#137041=CARTESIAN_POINT('Ctrl Pts',(-5.28281973492689,-4.61315961982725,
97.0019785820441));
#137042=CARTESIAN_POINT('Ctrl Pts',(-5.16214935538114,-4.74445366667629,
97.0100590554932));
#137043=CARTESIAN_POINT('Ctrl Pts',(-5.04143258981634,-4.87579818331071,
97.0181426350982));
#137044=CARTESIAN_POINT('Ctrl Pts',(-4.91571650573474,-5.00251432844391,
97.0262262147031));
#137045=CARTESIAN_POINT('Ctrl Pts',(-4.78540306382844,-5.124211556835,97.034309794308));
#137046=CARTESIAN_POINT('Ctrl Pts',(-4.65506242598126,-5.24593418299459,
97.0423950609266));
#137047=CARTESIAN_POINT('Ctrl Pts',(-4.52012278783041,-5.36263556517435,
97.0504803275451));
#137048=CARTESIAN_POINT('Ctrl Pts',(-4.38102025936743,-5.47396456414473,
97.0585655941637));
#137049=CARTESIAN_POINT('Ctrl Pts',(-4.24180835106944,-5.58538110392168,
97.0666572184318));
#137050=CARTESIAN_POINT('Ctrl Pts',(-4.0984273015312,-5.69141660437987,
97.0747488427));
#137051=CARTESIAN_POINT('Ctrl Pts',(-3.95134388296962,-5.79176208774312,
97.0828404669681));
#137052=CARTESIAN_POINT('Ctrl Pts',(-3.87166727432526,-5.84612027363079,
97.0872237834997));
#137053=CARTESIAN_POINT('Ctrl Pts',(-3.79090469082852,-5.89880948512701,
97.0916071000313));
#137054=CARTESIAN_POINT('Ctrl Pts',(-3.7091334728529,-5.94978616784353,
97.095990416563));
#137055=CARTESIAN_POINT('Ctrl Pts',(-3.53577909345808,-6.05785635946724,
97.1052830153018));
#137056=CARTESIAN_POINT('Ctrl Pts',(-3.357755268331,-6.15831162867937,97.1145756140406));
#137057=CARTESIAN_POINT('Ctrl Pts',(-3.17570664581012,-6.25080105764513,
97.1238682127794));
#137058=CARTESIAN_POINT('Ctrl Pts',(-2.99361604881999,-6.34331181165382,
97.1331629540881));
#137059=CARTESIAN_POINT('Ctrl Pts',(-2.80749894708967,-6.42785298311338,
97.1424576953968));
#137060=CARTESIAN_POINT('Ctrl Pts',(-2.618023238361,-6.50412030069415,97.1517524367055));
#137061=CARTESIAN_POINT('Ctrl Pts',(-2.42873892818923,-6.58031057697701,
97.1610377889474));
#137062=CARTESIAN_POINT('Ctrl Pts',(-2.23610294378876,-6.64824364361344,
97.1703231411894));
#137063=CARTESIAN_POINT('Ctrl Pts',(-2.04080166490915,-6.70766390981272,
97.1796084934314));
#137064=CARTESIAN_POINT('Ctrl Pts',(-1.84574325224158,-6.76701028415091,
97.1888822989066));
#137065=CARTESIAN_POINT('Ctrl Pts',(-1.64802632051038,-6.81786495122178,
97.1981561043817));
#137066=CARTESIAN_POINT('Ctrl Pts',(-1.44835289836396,-6.8600218982377,
97.2074299098569));
#137067=CARTESIAN_POINT('Ctrl Pts',(-1.24927025245782,-6.90205411496957,
97.2166762768083));
#137068=CARTESIAN_POINT('Ctrl Pts',(-1.04824283215503,-6.93543994729541,
97.2259226437597));
#137069=CARTESIAN_POINT('Ctrl Pts',(-0.84598226594813,-6.96002446606341,
97.2351690107111));
#137070=CARTESIAN_POINT('Ctrl Pts',(-0.703878521063625,-6.97729699846373,
97.2416653010905));
#137071=CARTESIAN_POINT('Ctrl Pts',(-0.56116640908754,-6.99022608997791,
97.2481615914699));
#137072=CARTESIAN_POINT('Ctrl Pts',(-0.418096783378159,-6.9987728668838,
97.2546578818492));
#137073=CARTESIAN_POINT('Ctrl Pts',(-0.237722289166256,-7.00954818382404,
97.2628480555889));
#137074=CARTESIAN_POINT('Ctrl Pts',(-0.0568894238677824,-7.01334864684193,
97.2710382293286));
#137075=CARTESIAN_POINT('Ctrl Pts',(0.123828300587959,-7.01015642582058,
97.2792284030682));
#137076=CARTESIAN_POINT('Ctrl Pts',(0.30453686052778,-7.00696436668241,
97.2874181614697));
#137077=CARTESIAN_POINT('Ctrl Pts',(0.485129942473077,-6.99678033663556,
97.2956079198712));
#137078=CARTESIAN_POINT('Ctrl Pts',(0.665034749132413,-6.97963862567013,
97.3037976782726));
#137079=CARTESIAN_POINT('Ctrl Pts',(0.844960925353261,-6.96249487856762,
97.3119884094749));
#137080=CARTESIAN_POINT('Ctrl Pts',(1.02419831621588,-6.93839183785199,
97.3201791406772));
#137081=CARTESIAN_POINT('Ctrl Pts',(1.20217976787424,-6.90741560702799,
97.3283698718795));
#137082=CARTESIAN_POINT('Ctrl Pts',(1.38027861074408,-6.87641894521397,
97.3365660054417));
#137083=CARTESIAN_POINT('Ctrl Pts',(1.55711951551482,-6.8385400968028,97.3447621390039));
#137084=CARTESIAN_POINT('Ctrl Pts',(1.73214522941971,-6.79391635705788,
97.3529582725661));
#137085=CARTESIAN_POINT('Ctrl Pts',(1.90723594945678,-6.74927604365266,
97.3611574502464));
#137086=CARTESIAN_POINT('Ctrl Pts',(2.08050979910627,-6.69788594001674,
97.3693566279267));
#137087=CARTESIAN_POINT('Ctrl Pts',(2.25142498320302,-6.63993314028909,
97.377555805607));
#137088=CARTESIAN_POINT('Ctrl Pts',(2.42250439565238,-6.58192465508867,
97.3857628616829));
#137089=CARTESIAN_POINT('Ctrl Pts',(2.59122028845276,-6.51734099885269,
97.3939699177588));
#137090=CARTESIAN_POINT('Ctrl Pts',(2.75705029626706,-6.44641762736124,
97.4021769738348));
#137091=CARTESIAN_POINT('Ctrl Pts',(2.83213750636617,-6.41430378882076,
97.4058930982684));
#137092=CARTESIAN_POINT('Ctrl Pts',(2.90663335370148,-6.38089078951168,
97.4096092227021));
#137093=CARTESIAN_POINT('Ctrl Pts',(2.98049102249596,-6.34620357594373,
97.4133253471357));
#137094=CARTESIAN_POINT('Ctrl Pts',(3.1426872115658,-6.2700282248664,97.421486195306));
#137095=CARTESIAN_POINT('Ctrl Pts',(3.3021447895156,-6.18754464539115,97.4296470434764));
#137096=CARTESIAN_POINT('Ctrl Pts',(3.4583426123271,-6.09897474484545,97.4378078916467));
#137097=CARTESIAN_POINT('Ctrl Pts',(3.61439977055824,-6.01048460628149,
97.4459613905322));
#137098=CARTESIAN_POINT('Ctrl Pts',(3.76720271514291,-5.91591923681794,
97.4541148894177));
#137099=CARTESIAN_POINT('Ctrl Pts',(3.91625210871414,-5.81554778017446,
97.4622683883033));
#137100=CARTESIAN_POINT('Ctrl Pts',(4.06519620138751,-5.71524723428244,
97.4704161268785));
#137101=CARTESIAN_POINT('Ctrl Pts',(4.21039173357565,-5.60914896883006,
97.4785638654538));
#137102=CARTESIAN_POINT('Ctrl Pts',(4.35136559320438,-5.4975671016166,97.4867116040291));
#137103=CARTESIAN_POINT('Ctrl Pts',(4.49226720969654,-5.38604241538756,
97.4948551672332));
#137104=CARTESIAN_POINT('Ctrl Pts',(4.62895118739581,-5.26903994476594,
97.5029987304372));
#137105=CARTESIAN_POINT('Ctrl Pts',(4.76097481787534,-5.14691610054573,
97.5111422936413));
#137106=CARTESIAN_POINT('Ctrl Pts',(4.89295640335875,-5.02483114857942,
97.5192832633999));
#137107=CARTESIAN_POINT('Ctrl Pts',(5.0202803399946,-4.89762831270213,97.5274242331586));
#137108=CARTESIAN_POINT('Ctrl Pts',(5.14253822139877,-4.7657032223957,97.5355652029172));
#137109=CARTESIAN_POINT('Ctrl Pts',(5.26480917503177,-4.63376402620956,
97.543707043136));
#137110=CARTESIAN_POINT('Ctrl Pts',(5.38201274438944,-4.49710181989524,
97.5518488833549));
#137111=CARTESIAN_POINT('Ctrl Pts',(5.49377815387643,-4.35614831686091,
97.5599907235737));
#137112=CARTESIAN_POINT('Ctrl Pts',(5.60555517407996,-4.21518017091355,
97.5681334096052));
#137113=CARTESIAN_POINT('Ctrl Pts',(5.71189268820996,-4.06992011644646,
97.5762760956367));
#137114=CARTESIAN_POINT('Ctrl Pts',(5.81246104027801,-3.92083195479611,
97.5844187816682));
#137115=CARTESIAN_POINT('Ctrl Pts',(5.91305752228111,-3.77170209175345,
97.5925637452873));
#137116=CARTESIAN_POINT('Ctrl Pts',(6.0078814288968,-3.61874228092341,97.6007087089063));
#137117=CARTESIAN_POINT('Ctrl Pts',(6.09664710191051,-3.46244432117921,
97.6088536725254));
#137118=CARTESIAN_POINT('Ctrl Pts',(6.18545321120843,-3.3060751615161,97.6170023464984));
#137119=CARTESIAN_POINT('Ctrl Pts',(6.26819541349938,-3.14636513010987,
97.6251510204714));
#137120=CARTESIAN_POINT('Ctrl Pts',(6.34463450985768,-2.98382966987445,
97.6332996944444));
#137121=CARTESIAN_POINT('Ctrl Pts',(6.42117264675738,-2.82108361583628,
97.6414589264842));
#137122=CARTESIAN_POINT('Ctrl Pts',(6.49139120984816,-2.6555051388503,97.6496181585239));
#137123=CARTESIAN_POINT('Ctrl Pts',(6.55509911664866,-2.48762982242373,
97.6577773905637));
#137124=CARTESIAN_POINT('Ctrl Pts',(6.61884953612063,-2.31964248178336,
97.6659420673083));
#137125=CARTESIAN_POINT('Ctrl Pts',(6.67608052612848,-2.14935558071816,
97.6741067440529));
#137126=CARTESIAN_POINT('Ctrl Pts',(6.72665123373126,-1.97731882665436,
97.6822714207976));
#137127=CARTESIAN_POINT('Ctrl Pts',(6.77730780081443,-1.8049899867762,97.6904499596165));
#137128=CARTESIAN_POINT('Ctrl Pts',(6.82128139901214,-1.63090569873286,
97.6986284984353));
#137129=CARTESIAN_POINT('Ctrl Pts',(6.85848223425342,-1.45562632736915,
97.7068070372542));
#137130=CARTESIAN_POINT('Ctrl Pts',(6.8946484528475,-1.28522176471197,97.7147581174056));
#137131=CARTESIAN_POINT('Ctrl Pts',(6.92441362007722,-1.11368800155236,
97.7227091975571));
#137132=CARTESIAN_POINT('Ctrl Pts',(6.94774241808964,-0.941542274344565,
97.7306602777085));
#137133=CARTESIAN_POINT('Ctrl Pts',(6.98967385862435,-0.632125633166784,
97.7449516374424));
#137134=CARTESIAN_POINT('Ctrl Pts',(7.01094414743396,-0.319844675255263,
97.7592429971764));
#137135=CARTESIAN_POINT('Ctrl Pts',(7.01124672537693,-0.0067763110370816,
97.7735343569104));
#137136=CARTESIAN_POINT('Ctrl Pts',(7.01124672537777,-0.00677631017023138,
97.77353435695));
#137137=CARTESIAN_POINT('Ctrl Pts',(7.01141684865851,0.169245191947657,
97.7815696198356));
#137138=CARTESIAN_POINT('Ctrl Pts',(7.00495425607265,0.34555057630013,97.7896048827212));
#137139=CARTESIAN_POINT('Ctrl Pts',(6.99182159260741,0.521591199742505,
97.7976401456068));
#137140=CARTESIAN_POINT('Ctrl Pts',(6.97870710397494,0.697388193330068,
97.8056642881618));
#137141=CARTESIAN_POINT('Ctrl Pts',(6.95894096047927,0.872920793783318,
97.8136884307168));
#137142=CARTESIAN_POINT('Ctrl Pts',(6.93253776919222,1.04763860239271,97.8217125732719));
#137143=CARTESIAN_POINT('Ctrl Pts',(6.90615562336565,1.22221714689968,97.8297303199419));
#137144=CARTESIAN_POINT('Ctrl Pts',(6.87314700967083,1.3959818317732,97.8377480666119));
#137145=CARTESIAN_POINT('Ctrl Pts',(6.83357848984267,1.56838502468607,97.8457658132819));
#137146=CARTESIAN_POINT('Ctrl Pts',(6.79403798413458,1.74066615784624,97.8537778834667));
#137147=CARTESIAN_POINT('Ctrl Pts',(6.74794690239303,1.91158736264453,97.8617899536515));
#137148=CARTESIAN_POINT('Ctrl Pts',(6.69542324046895,2.08060909194597,97.8698020238363));
#137149=CARTESIAN_POINT('Ctrl Pts',(6.65734447976229,2.20314696818164,97.875610638319));
#137150=CARTESIAN_POINT('Ctrl Pts',(6.61588583364576,2.324686605734,97.8814192528015));
#137151=CARTESIAN_POINT('Ctrl Pts',(6.57110895151812,2.44502632087642,97.8872278672842));
#137152=CARTESIAN_POINT('',(7.01124999980813,5.18702180079971E-5,97.226465643065));
#137153=CARTESIAN_POINT('Ctrl Pts',(6.57110895151819,2.44502632087623,97.3397894808225));
#137154=CARTESIAN_POINT('Ctrl Pts',(6.6378710550212,2.26560041768449,97.331095649925));
#137155=CARTESIAN_POINT('Ctrl Pts',(6.69728975529657,2.08341282781443,97.3224018190275));
#137156=CARTESIAN_POINT('Ctrl Pts',(6.74915972893131,1.89907069796566,97.31370798813));
#137157=CARTESIAN_POINT('Ctrl Pts',(6.80101268375869,1.71478905172579,97.3050170097236));
#137158=CARTESIAN_POINT('Ctrl Pts',(6.84532178129947,1.52835454671171,97.2963260313171));
#137159=CARTESIAN_POINT('Ctrl Pts',(6.88193170502248,1.34038896216973,97.2876350529106));
#137160=CARTESIAN_POINT('Ctrl Pts',(6.91630329291163,1.16391561963831,97.279475442134));
#137161=CARTESIAN_POINT('Ctrl Pts',(6.94388877474474,0.986093012273329,
97.2713158313574));
#137162=CARTESIAN_POINT('Ctrl Pts',(6.9646004601257,0.807444730812538,97.2631562205808));
#137163=CARTESIAN_POINT('Ctrl Pts',(6.98611826354919,0.621843292218288,
97.25467903017));
#137164=CARTESIAN_POINT('Ctrl Pts',(7.00022244399454,0.435295819211352,
97.2462018397591));
#137165=CARTESIAN_POINT('Ctrl Pts',(7.00684800478483,0.248410145410525,
97.2377246493483));
#137166=CARTESIAN_POINT('Ctrl Pts',(7.00978125769811,0.165672553155592,
97.233971647262));
#137167=CARTESIAN_POINT('Ctrl Pts',(7.01124938711066,0.0828687677128226,
97.2302186451757));
#137168=CARTESIAN_POINT('Ctrl Pts',(7.01124999980813,5.18707570270757E-5,
97.2264656430894));
#137169=CARTESIAN_POINT('Ctrl Pts',(7.01124999980813,5.18702180126676E-5,
97.226465643065));
#137170=CARTESIAN_POINT('Ctrl Pts',(7.01125130797657,-0.176772062939251,
97.21845253687));
#137171=CARTESIAN_POINT('Ctrl Pts',(7.00455901490281,-0.35364297051039,
97.210439430675));
#137172=CARTESIAN_POINT('Ctrl Pts',(6.99118851967943,-0.530009098792206,
97.2024263244799));
#137173=CARTESIAN_POINT('Ctrl Pts',(6.97757047767512,-0.709640541229728,
97.1942648603812));
#137174=CARTESIAN_POINT('Ctrl Pts',(6.95702452002822,-0.888747936457469,
97.1861033962824));
#137175=CARTESIAN_POINT('Ctrl Pts',(6.92962233224002,-1.06675249942078,
97.1779419321836));
#137176=CARTESIAN_POINT('Ctrl Pts',(6.90270740403597,-1.24159182499501,
97.1699255934169));
#137177=CARTESIAN_POINT('Ctrl Pts',(6.86917813764389,-1.4153668476734,97.1619092546501));
#137178=CARTESIAN_POINT('Ctrl Pts',(6.82915424017152,-1.58753863778095,
97.1538929158834));
#137179=CARTESIAN_POINT('Ctrl Pts',(6.78804347219975,-1.76438584560927,
97.1456588891186));
#137180=CARTESIAN_POINT('Ctrl Pts',(6.7400804338736,-1.93954110860752,97.1374248623538));
#137181=CARTESIAN_POINT('Ctrl Pts',(6.68544970243736,-2.11243670643175,
97.1291908355889));
#137182=CARTESIAN_POINT('Ctrl Pts',(6.63081897100112,-2.28533230425599,
97.1209568088241));
#137183=CARTESIAN_POINT('Ctrl Pts',(6.56952071889578,-2.45596785500244,
97.1127227820592));
#137184=CARTESIAN_POINT('Ctrl Pts',(6.50179287697718,-2.62379800049257,
97.1044887552944));
#137185=CARTESIAN_POINT('Ctrl Pts',(6.42183274031629,-2.82193987227016,
97.0947675846985));
#137186=CARTESIAN_POINT('Ctrl Pts',(6.33286264442571,-3.01629711354463,
97.0850464141025));
#137187=CARTESIAN_POINT('Ctrl Pts',(6.23524423677151,-3.20614345753706,
97.0753252435066));
#137188=CARTESIAN_POINT('Ctrl Pts',(6.1375012290424,-3.39623212128508,97.0655916648145));
#137189=CARTESIAN_POINT('Ctrl Pts',(6.03108785350573,-3.58179832930889,
97.0558580861225));
#137190=CARTESIAN_POINT('Ctrl Pts',(5.91641222425415,-3.76213941198304,
97.0461245074304));
#137191=CARTESIAN_POINT('Ctrl Pts',(5.80193074152675,-3.94217517612877,
97.0364074077452));
#137192=CARTESIAN_POINT('Ctrl Pts',(5.67921498596527,-4.11700345416213,
97.0266903080599));
#137193=CARTESIAN_POINT('Ctrl Pts',(5.54871539220533,-4.28595194312811,
97.0169732083747));
#137194=CARTESIAN_POINT('Ctrl Pts',(5.41856219448823,-4.45445197791631,
97.007281901604));
#137195=CARTESIAN_POINT('Ctrl Pts',(5.28066643649339,-4.61710334260077,
96.9975905948333));
#137196=CARTESIAN_POINT('Ctrl Pts',(5.13551887238781,-4.77326643650327,
96.9878992880627));
#137197=CARTESIAN_POINT('Ctrl Pts',(4.9912958501846,-4.92843482322756,96.9782697117059));
#137198=CARTESIAN_POINT('Ctrl Pts',(4.83991312755717,-5.07719727213506,
96.968640135349));
#137199=CARTESIAN_POINT('Ctrl Pts',(4.68189530176782,-5.21895420039153,
96.9590105589922));
#137200=CARTESIAN_POINT('Ctrl Pts',(4.60975160851087,-5.2836739134878,96.9546141359974));
#137201=CARTESIAN_POINT('Ctrl Pts',(4.53622547744085,-5.34693377426904,
96.9502177130027));
#137202=CARTESIAN_POINT('Ctrl Pts',(4.46136984459314,-5.408678736277,96.9458212900079));
#137203=CARTESIAN_POINT('Ctrl Pts',(4.32760616633227,-5.51901423032146,
96.9379650781426));
#137204=CARTESIAN_POINT('Ctrl Pts',(4.18964934262419,-5.62446438578562,
96.9301088662772));
#137205=CARTESIAN_POINT('Ctrl Pts',(4.04791025671619,-5.72468768720809,
96.9222526544118));
#137206=CARTESIAN_POINT('Ctrl Pts',(3.90621079716929,-5.8248829689442,96.9143986389278));
#137207=CARTESIAN_POINT('Ctrl Pts',(3.76073148972796,-5.91985408365195,
96.9065446234438));
#137208=CARTESIAN_POINT('Ctrl Pts',(3.61191480974728,-6.00930095515513,
96.8986906079598));
#137209=CARTESIAN_POINT('Ctrl Pts',(3.46310945214526,-6.09874102129649,
96.8908371900307));
#137210=CARTESIAN_POINT('Ctrl Pts',(3.31096755453098,-6.18265748529902,
96.8829837721016));
#137211=CARTESIAN_POINT('Ctrl Pts',(3.15595874177031,-6.26079475647809,
96.8751303541724));
#137212=CARTESIAN_POINT('Ctrl Pts',(3.00087080883146,-6.33897191077548,
96.8672729276724));
#137213=CARTESIAN_POINT('Ctrl Pts',(2.84291337770821,-6.411363806658,96.8594155011723));
#137214=CARTESIAN_POINT('Ctrl Pts',(2.68257905108029,-6.47776166566856,
96.8515580746722));
#137215=CARTESIAN_POINT('Ctrl Pts',(2.52220354052918,-6.54417657981875,
96.8436986298916));
#137216=CARTESIAN_POINT('Ctrl Pts',(2.35945027543758,-6.60459425709406,
96.835839185111));
#137217=CARTESIAN_POINT('Ctrl Pts',(2.19482919392977,-6.65885510969969,
96.8279797403304));
#137218=CARTESIAN_POINT('Ctrl Pts',(2.03004440776971,-6.71316992109313,
96.8201124798578));
#137219=CARTESIAN_POINT('Ctrl Pts',(1.86338846140871,-6.76131557379297,
96.8122452193852));
#137220=CARTESIAN_POINT('Ctrl Pts',(1.69538428261051,-6.80318298274986,
96.8043779589125));
#137221=CARTESIAN_POINT('Ctrl Pts',(1.57277800687915,-6.83373702684237,
96.7986365808489));
#137222=CARTESIAN_POINT('Ctrl Pts',(1.44945394977167,-6.86094846313517,
96.7928952027852));
#137223=CARTESIAN_POINT('Ctrl Pts',(1.32561746232401,-6.88479229215244,
96.7871538247215));
#137224=CARTESIAN_POINT('Ctrl Pts',(1.14492041564119,-6.91958421474191,
96.7787762448872));
#137225=CARTESIAN_POINT('Ctrl Pts',(0.96273255722168,-6.94728122495442,
96.7703986650528));
#137226=CARTESIAN_POINT('Ctrl Pts',(0.779636631869397,-6.96776817099617,
96.7620210852185));
#137227=CARTESIAN_POINT('Ctrl Pts',(0.596666158169756,-6.98824108001753,
96.7536492454422));
#137228=CARTESIAN_POINT('Ctrl Pts',(0.412789183682782,-7.00151373752115,
96.7452774056659));
#137229=CARTESIAN_POINT('Ctrl Pts',(0.228596728859201,-7.00752239368915,
96.7369055658896));
#137230=CARTESIAN_POINT('Ctrl Pts',(0.0445034356030402,-7.01352781504623,
96.7285382331641));
#137231=CARTESIAN_POINT('Ctrl Pts',(-0.139904671463392,-7.01227702179111,
96.7201709004386));
#137232=CARTESIAN_POINT('Ctrl Pts',(-0.32403292833021,-7.00375822140212,
96.7118035677131));
#137233=CARTESIAN_POINT('Ctrl Pts',(-0.50808906108166,-6.99524275787707,
96.7034395125208));
#137234=CARTESIAN_POINT('Ctrl Pts',(-0.691865234286078,-6.97946497954286,
96.6950754573285));
#137235=CARTESIAN_POINT('Ctrl Pts',(-0.874767803894187,-6.9564651836813,
96.6867114021362));
#137236=CARTESIAN_POINT('Ctrl Pts',(-1.05762553124577,-6.93347102668392,
96.6783493975608));
#137237=CARTESIAN_POINT('Ctrl Pts',(-1.23960975628846,-6.90325842461056,
96.6699873929854));
#137238=CARTESIAN_POINT('Ctrl Pts',(-1.4201325112331,-6.86591947324164,
96.6616253884101));
#137239=CARTESIAN_POINT('Ctrl Pts',(-1.60066950233367,-6.82857757729583,
96.6532627244009));
#137240=CARTESIAN_POINT('Ctrl Pts',(-1.77974446992953,-6.78410826993594,
96.6449000603918));
#137241=CARTESIAN_POINT('Ctrl Pts',(-1.95677942633535,-6.7326548136059,
96.6365373963826));
#137242=CARTESIAN_POINT('Ctrl Pts',(-2.13382636960631,-6.68119787341226,
96.6281741661456));
#137243=CARTESIAN_POINT('Ctrl Pts',(-2.30883271037858,-6.6227559328789,
96.6198109359086));
#137244=CARTESIAN_POINT('Ctrl Pts',(-2.48123525206485,-6.55752225969616,
96.6114477056716));
#137245=CARTESIAN_POINT('Ctrl Pts',(-2.65367247664211,-6.49227546320124,
96.603082792971));
#137246=CARTESIAN_POINT('Ctrl Pts',(-2.82350455006597,-6.42023432597916,
96.5947178802704));
#137247=CARTESIAN_POINT('Ctrl Pts',(-2.99018749977474,-6.34164058258515,
96.5863529675697));
#137248=CARTESIAN_POINT('Ctrl Pts',(-3.1569262368509,-6.26302053453283,
96.5779852552039));
#137249=CARTESIAN_POINT('Ctrl Pts',(-3.32051345121546,-6.17784364740537,
96.5696175428381));
#137250=CARTESIAN_POINT('Ctrl Pts',(-3.48042866701478,-6.08639818417443,
96.5612498304722));
#137251=CARTESIAN_POINT('Ctrl Pts',(-3.6404921740431,-5.99486792250788,
96.5528743586299));
#137252=CARTESIAN_POINT('Ctrl Pts',(-3.79687659236227,-5.89705763219977,
96.5444988867876));
#137253=CARTESIAN_POINT('Ctrl Pts',(-3.94908834714537,-5.7933002501977,
96.5361234149453));
#137254=CARTESIAN_POINT('Ctrl Pts',(-4.10137476011892,-5.68949197634172,
96.5277438350263));
#137255=CARTESIAN_POINT('Ctrl Pts',(-4.24948416029372,-5.57973098428988,
96.5193642551072));
#137256=CARTESIAN_POINT('Ctrl Pts',(-4.39295460256064,-5.46439167907474,
96.5109846751882));
#137257=CARTESIAN_POINT('Ctrl Pts',(-4.53658908445954,-5.34892049849293,
96.5025955143186));
#137258=CARTESIAN_POINT('Ctrl Pts',(-4.67557375763408,-5.22785847120942,
96.4942063534491));
#137259=CARTESIAN_POINT('Ctrl Pts',(-4.80948121261135,-5.10161905947891,
96.4858171925795));
#137260=CARTESIAN_POINT('Ctrl Pts',(-4.89460261550108,-5.02137202746491,
96.4804844264359));
#137261=CARTESIAN_POINT('Ctrl Pts',(-4.97767315106773,-4.93903366360074,
96.4751516602922));
#137262=CARTESIAN_POINT('Ctrl Pts',(-5.05859124150688,-4.85471741853734,
96.4698188941486));
#137263=CARTESIAN_POINT('Ctrl Pts',(-5.18575276667672,-4.72221574603534,
96.4614385347936));
#137264=CARTESIAN_POINT('Ctrl Pts',(-5.30785359630069,-4.58456025632651,
96.4530581754386));
#137265=CARTESIAN_POINT('Ctrl Pts',(-5.42446601166263,-4.44216107889133,
96.4446778160836));
#137266=CARTESIAN_POINT('Ctrl Pts',(-5.54093063954025,-4.29994236951467,
96.4363080774865));
#137267=CARTESIAN_POINT('Ctrl Pts',(-5.65192050907952,-4.15299220491517,
96.4279383388894));
#137268=CARTESIAN_POINT('Ctrl Pts',(-5.75704484462385,-4.00175726643808,
96.4195686002923));
#137269=CARTESIAN_POINT('Ctrl Pts',(-5.86204990942323,-3.85069391433708,
96.4112083577357));
#137270=CARTESIAN_POINT('Ctrl Pts',(-5.9612025180922,-3.69535574506816,
96.4028481151792));
#137271=CARTESIAN_POINT('Ctrl Pts',(-6.05415201487409,-3.53622255285157,
96.3944878726226));
#137272=CARTESIAN_POINT('Ctrl Pts',(-6.14698098335289,-3.37729570982766,
96.3861384708547));
#137273=CARTESIAN_POINT('Ctrl Pts',(-6.23362271922645,-3.21458394104537,
96.3777890690868));
#137274=CARTESIAN_POINT('Ctrl Pts',(-6.31376980096844,-3.04859598223166,
96.369439667319));
#137275=CARTESIAN_POINT('Ctrl Pts',(-6.39385526815713,-2.88273562973513,
96.3610966843083));
#137276=CARTESIAN_POINT('Ctrl Pts',(-6.46745588918309,-2.7136044002763,
96.3527537012976));
#137277=CARTESIAN_POINT('Ctrl Pts',(-6.5343095759154,-2.54173659701399,
96.3444107182869));
#137278=CARTESIAN_POINT('Ctrl Pts',(-6.60110965728785,-2.3700066026878,
96.3360744249389));
#137279=CARTESIAN_POINT('Ctrl Pts',(-6.66117347513572,-2.19554471529376,
96.3277381315908));
#137280=CARTESIAN_POINT('Ctrl Pts',(-6.71428653058147,-2.01890637419179,
96.3194018382427));
#137281=CARTESIAN_POINT('Ctrl Pts',(-6.73180848478713,-1.96063352775552,
96.3166517017826));
#137282=CARTESIAN_POINT('Ctrl Pts',(-6.74857435224168,-1.90212397241415,
96.3139015653225));
#137283=CARTESIAN_POINT('Ctrl Pts',(-6.76457759240424,-1.84339810101954,
96.3111514288623));
#137284=CARTESIAN_POINT('Ctrl Pts',(-6.81310307226853,-1.66532784393885,
96.3028123868893));
#137285=CARTESIAN_POINT('Ctrl Pts',(-6.85457308635309,-1.48541385332468,
96.2944733449163));
#137286=CARTESIAN_POINT('Ctrl Pts',(-6.88887368500138,-1.30424150930549,
96.2861343029433));
#137287=CARTESIAN_POINT('Ctrl Pts',(-6.92319593805226,-1.12295478888968,
96.2777899964274));
#137288=CARTESIAN_POINT('Ctrl Pts',(-6.95033968674496,-0.940408452334087,
96.2694456899115));
#137289=CARTESIAN_POINT('Ctrl Pts',(-6.97024261627621,-0.757195108771167,
96.2611013833957));
#137290=CARTESIAN_POINT('Ctrl Pts',(-6.99016072631823,-0.573842023361132,
96.2527507124481));
#137291=CARTESIAN_POINT('Ctrl Pts',(-7.0028269656921,-0.389821241423341,
96.2444000415006));
#137292=CARTESIAN_POINT('Ctrl Pts',(-7.00823105916851,-0.205727936376796,
96.236049370553));
#137293=CARTESIAN_POINT('Ctrl Pts',(-7.0136432704791,-0.0213580930115474,
96.227686155529));
#137294=CARTESIAN_POINT('Ctrl Pts',(-7.01177152674709,0.163084163470667,
96.2193229405049));
#137295=CARTESIAN_POINT('Ctrl Pts',(-7.00265765997775,0.347004696877467,
96.2109597254809));
#137296=CARTESIAN_POINT('Ctrl Pts',(-6.99353598803808,0.531082740935358,
96.2025893481492));
#137297=CARTESIAN_POINT('Ctrl Pts',(-6.97715984707511,0.714637844944345,
96.1942189708175));
#137298=CARTESIAN_POINT('Ctrl Pts',(-6.95362270461207,0.897082964058278,
96.1858485934858));
#137299=CARTESIAN_POINT('Ctrl Pts',(-6.93004923143176,1.07980969603362,
96.177465296072));
#137300=CARTESIAN_POINT('Ctrl Pts',(-6.89929272341157,1.2614226970706,96.1690819986582));
#137301=CARTESIAN_POINT('Ctrl Pts',(-6.8614975969031,1.44134565257364,96.1606987012444));
#137302=CARTESIAN_POINT('Ctrl Pts',(-6.84915253210376,1.50011409045881,
96.1579604553549));
#137303=CARTESIAN_POINT('Ctrl Pts',(-6.83605692651224,1.55870234781369,
96.1552222094654));
#137304=CARTESIAN_POINT('Ctrl Pts',(-6.82221694956074,1.61709073821666,
96.1524839635759));
#137305=CARTESIAN_POINT('Ctrl Pts',(-6.77981297178154,1.79598554547597,
96.1440943168113));
#137306=CARTESIAN_POINT('Ctrl Pts',(-6.73033202143919,1.97336413161707,
96.1357046700468));
#137307=CARTESIAN_POINT('Ctrl Pts',(-6.67390018366913,2.1486467603869,96.1273150232822));
#137308=CARTESIAN_POINT('Ctrl Pts',(-6.61752044903762,2.32376755187741,
96.1189331226224));
#137309=CARTESIAN_POINT('Ctrl Pts',(-6.55420272091976,2.49679593235515,
96.1105512219626));
#137310=CARTESIAN_POINT('Ctrl Pts',(-6.4841235365135,2.66716488536642,96.1021693213028));
#137311=CARTESIAN_POINT('Ctrl Pts',(-6.41409874967221,2.83740159288612,
96.0937939269257));
#137312=CARTESIAN_POINT('Ctrl Pts',(-6.33732309494555,3.00498268562966,
96.0854185325486));
#137313=CARTESIAN_POINT('Ctrl Pts',(-6.25402224617961,3.1693583430705,96.0770431381715));
#137314=CARTESIAN_POINT('Ctrl Pts',(-6.17077382624229,3.33363054390435,
96.0686730151947));
#137315=CARTESIAN_POINT('Ctrl Pts',(-6.08100854927491,3.49470103960012,
96.0603028922178));
#137316=CARTESIAN_POINT('Ctrl Pts',(-5.98499950918569,3.65204154378713,
96.051932769241));
#137317=CARTESIAN_POINT('Ctrl Pts',(-5.88903681621092,3.80930609389369,
96.0435666868321));
#137318=CARTESIAN_POINT('Ctrl Pts',(-5.78683654163835,3.96284396305525,
96.0352006044232));
#137319=CARTESIAN_POINT('Ctrl Pts',(-5.67871709607843,4.11215256346437,
96.0268345220143));
#137320=CARTESIAN_POINT('Ctrl Pts',(-5.5706279211741,4.2614193613171,96.0184707818927));
#137321=CARTESIAN_POINT('Ctrl Pts',(-5.45662307117982,4.40645898464192,
96.010107041771));
#137322=CARTESIAN_POINT('Ctrl Pts',(-5.33706386300728,4.54679842138199,
96.0017433016493));
#137323=CARTESIAN_POINT('Ctrl Pts',(-5.21752307038773,4.68711624181687,
95.993380849784));
#137324=CARTESIAN_POINT('Ctrl Pts',(-5.09242983843564,4.8227350689769,95.9850183979186));
#137325=CARTESIAN_POINT('Ctrl Pts',(-4.9621855596968,4.95321522181669,95.9766559460532));
#137326=CARTESIAN_POINT('Ctrl Pts',(-4.83194397379747,5.08369267694021,
95.968293667084));
#137327=CARTESIAN_POINT('Ctrl Pts',(-4.69655178595412,5.20903143725763,
95.9599313881148));
#137328=CARTESIAN_POINT('Ctrl Pts',(-4.55644730889962,5.32882862210087,
95.9515691091456));
#137329=CARTESIAN_POINT('Ctrl Pts',(-4.41632704546271,5.44863930518636,
95.9432058879501));
#137330=CARTESIAN_POINT('Ctrl Pts',(-4.27149368437813,5.56290695473891,
95.9348426667545));
#137331=CARTESIAN_POINT('Ctrl Pts',(-4.12241899829231,5.6712686556906,95.9264794455589));
#137332=CARTESIAN_POINT('Ctrl Pts',(-3.97325651110419,5.77969417885813,
95.9181112986442));
#137333=CARTESIAN_POINT('Ctrl Pts',(-3.81984797283673,5.88220660841757,
95.9097431517295));
#137334=CARTESIAN_POINT('Ctrl Pts',(-3.66269540105741,5.97848550734824,
95.9013750048147));
#137335=CARTESIAN_POINT('Ctrl Pts',(-3.50549572968352,6.07479326165845,
95.8930043499148));
#137336=CARTESIAN_POINT('Ctrl Pts',(-3.34455007042928,6.16486359291641,
95.8846336950148));
#137337=CARTESIAN_POINT('Ctrl Pts',(-3.18038609268354,6.2484214697766,95.8762630401149));
#137338=CARTESIAN_POINT('Ctrl Pts',(-3.01608296100797,6.33205017464116,
95.8678852898123));
#137339=CARTESIAN_POINT('Ctrl Pts',(-2.84855635537664,6.40915525015822,
95.8595075395097));
#137340=CARTESIAN_POINT('Ctrl Pts',(-2.67835607620681,6.47950887734141,
95.8511297892071));
#137341=CARTESIAN_POINT('Ctrl Pts',(-2.57013572790085,6.52424261147797,
95.8458028704723));
#137342=CARTESIAN_POINT('Ctrl Pts',(-2.46083483320128,6.56624774580741,
95.8404759517375));
#137343=CARTESIAN_POINT('Ctrl Pts',(-2.3505982277259,6.60547610201656,95.8351490330028));
#137344=CARTESIAN_POINT('Ctrl Pts',(-2.18788037255691,6.66338022521259,
95.8272860841444));
#137345=CARTESIAN_POINT('Ctrl Pts',(-2.02278453155179,6.71535207099191,
95.819423135286));
#137346=CARTESIAN_POINT('Ctrl Pts',(-1.8558011838239,6.76118543811792,95.8115601864276));
#137347=CARTESIAN_POINT('Ctrl Pts',(-1.68894614424186,6.80698358739476,
95.8037032793716));
#137348=CARTESIAN_POINT('Ctrl Pts',(-1.52020684743442,6.84665253767365,
95.7958463723156));
#137349=CARTESIAN_POINT('Ctrl Pts',(-1.35009246772941,6.88003465769471,
95.7879894652596));
#137350=CARTESIAN_POINT('Ctrl Pts',(-1.1800740292694,6.9133979508408,95.7801369893483));
#137351=CARTESIAN_POINT('Ctrl Pts',(-1.00868242356118,6.94048139365944,
95.7722845134371));
#137352=CARTESIAN_POINT('Ctrl Pts',(-0.836440411773444,6.96117763026144,
95.7644320375259));
#137353=CARTESIAN_POINT('Ctrl Pts',(-0.664239081816405,6.98186897862052,
95.7565814162905));
#137354=CARTESIAN_POINT('Ctrl Pts',(-0.491188122731238,6.99617606946815,
95.748730795055));
#137355=CARTESIAN_POINT('Ctrl Pts',(-0.317818816133417,7.00404295836423,
95.7408801738196));
#137356=CARTESIAN_POINT('Ctrl Pts',(-0.144477404818297,7.01190858147057,
95.7330308157565));
#137357=CARTESIAN_POINT('Ctrl Pts',(0.0291818707769141,7.01333605117387,
95.7251814576933));
#137358=CARTESIAN_POINT('Ctrl Pts',(0.202624771202832,7.00832146555757,
95.7173320996302));
#137359=CARTESIAN_POINT('Ctrl Pts',(0.376126089240345,7.00330519096978,
95.7094800978108));
#137360=CARTESIAN_POINT('Ctrl Pts',(0.549410504846155,6.99184253813279,
95.7016280959914));
#137361=CARTESIAN_POINT('Ctrl Pts',(0.721945745383131,6.97398171084662,
95.693776094172));
#137362=CARTESIAN_POINT('Ctrl Pts',(0.848618974731505,6.96086851342602,
95.6880112520202));
#137363=CARTESIAN_POINT('Ctrl Pts',(0.974888403188787,6.94430758837837,
95.6822464098684));
#137364=CARTESIAN_POINT('Ctrl Pts',(1.1005460416562,6.92433570623889,95.6764815677167));
#137365=CARTESIAN_POINT('Ctrl Pts',(1.31100373558773,6.89088579973252,95.6668263219239));
#137366=CARTESIAN_POINT('Ctrl Pts',(1.51963775258675,6.84788416589393,95.6571710761311));
#137367=CARTESIAN_POINT('Ctrl Pts',(1.72567728557241,6.79556211571636,95.6475158303384));
#137368=CARTESIAN_POINT('Ctrl Pts',(1.93285815865945,6.74295023157737,95.6378071000562));
#137369=CARTESIAN_POINT('Ctrl Pts',(2.13741569195669,6.68091445029655,95.6280983697741));
#137370=CARTESIAN_POINT('Ctrl Pts',(2.33858964665574,6.60973713751573,95.618389639492));
#137371=CARTESIAN_POINT('Ctrl Pts',(2.54073163563266,6.5382173247394,95.6086341915136));
#137372=CARTESIAN_POINT('Ctrl Pts',(2.7394573718015,6.45746782909853,95.5988787435352));
#137373=CARTESIAN_POINT('Ctrl Pts',(2.9340196788317,6.36782184791066,95.5891232955568));
#137374=CARTESIAN_POINT('Ctrl Pts',(3.12877465505256,6.27808709300858,95.5793581870523));
#137375=CARTESIAN_POINT('Ctrl Pts',(3.31935792519388,6.17943825690808,95.5695930785477));
#137376=CARTESIAN_POINT('Ctrl Pts',(3.50504459135589,6.0722556743855,95.5598279700431));
#137377=CARTESIAN_POINT('Ctrl Pts',(3.69047816887279,5.96521918040632,95.5500761712614));
#137378=CARTESIAN_POINT('Ctrl Pts',(3.87102844850403,5.84967220599937,95.5403243724798));
#137379=CARTESIAN_POINT('Ctrl Pts',(4.04599834228836,5.72603911763619,95.5305725736982));
#137380=CARTESIAN_POINT('Ctrl Pts',(4.1223038667914,5.67212191251339,95.5263197499421));
#137381=CARTESIAN_POINT('Ctrl Pts',(4.19754838570267,5.61666740178707,95.522066926186));
#137382=CARTESIAN_POINT('Ctrl Pts',(4.27167559387061,5.55971349830458,95.51781410243));
#137383=CARTESIAN_POINT('Ctrl Pts',(4.41169191776291,5.45213523663757,95.5097810904874));
#137384=CARTESIAN_POINT('Ctrl Pts',(4.54778793700803,5.33915192180933,95.5017480785448));
#137385=CARTESIAN_POINT('Ctrl Pts',(4.67951674515514,5.22108701271226,95.4937150666022));
#137386=CARTESIAN_POINT('Ctrl Pts',(4.8111608693073,5.10309800355164,95.4856872188112));
#137387=CARTESIAN_POINT('Ctrl Pts',(4.93844309898375,4.98003414637678,95.4776593710203));
#137388=CARTESIAN_POINT('Ctrl Pts',(5.06094843304027,4.85226004255824,95.4696315232293));
#137389=CARTESIAN_POINT('Ctrl Pts',(5.18339845174301,4.72454363312346,95.4616073002866));
#137390=CARTESIAN_POINT('Ctrl Pts',(5.30107561635766,4.59212147587694,95.4535830773439));
#137391=CARTESIAN_POINT('Ctrl Pts',(5.41360077607436,4.45539596442191,95.4455588544012));
#137392=CARTESIAN_POINT('Ctrl Pts',(5.52611232760838,4.3186869878089,95.4375356018644));
#137393=CARTESIAN_POINT('Ctrl Pts',(5.63347287650376,4.17767597156114,95.4295123493277));
#137394=CARTESIAN_POINT('Ctrl Pts',(5.73534256615504,4.03279955010785,95.421489096791));
#137395=CARTESIAN_POINT('Ctrl Pts',(5.83720390686241,3.88793500230533,95.4134665018168));
#137396=CARTESIAN_POINT('Ctrl Pts',(5.93357507710645,3.73920598256375,95.4054439068425));
#137397=CARTESIAN_POINT('Ctrl Pts',(6.02415887194168,3.5870790969961,95.3974213118683));
#137398=CARTESIAN_POINT('Ctrl Pts',(6.11477671916688,3.43489502367163,95.3893957010287));
#137399=CARTESIAN_POINT('Ctrl Pts',(6.19960265977088,3.27931084955247,95.381370090189));
#137400=CARTESIAN_POINT('Ctrl Pts',(6.27838469185183,3.12081915907036,95.3733444793494));
#137401=CARTESIAN_POINT('Ctrl Pts',(6.32484158601581,3.02735835974708,95.3686118652808));
#137402=CARTESIAN_POINT('Ctrl Pts',(6.3691976891623,2.93288697901579,95.3638792512122));
#137403=CARTESIAN_POINT('Ctrl Pts',(6.41140909568922,2.83750946610113,95.3591466371436));
#137404=CARTESIAN_POINT('Ctrl Pts',(6.46858834556246,2.70831181333498,95.3527358741616));
#137405=CARTESIAN_POINT('Ctrl Pts',(6.52185266125821,2.57740462988759,95.3463251111796));
#137406=CARTESIAN_POINT('Ctrl Pts',(6.57110895151813,2.44502632087639,95.3399143481975));
#137407=CARTESIAN_POINT('Origin',(0.,0.,50.));
#137408=CARTESIAN_POINT('',(6.57110895151818,2.44502632087624,93.3398552680816));
#137409=CARTESIAN_POINT('',(6.5711089515182,2.44502632087621,93.8869739242502));
#137410=CARTESIAN_POINT('',(6.57110895151814,2.44502632087636,50.));
#137411=CARTESIAN_POINT('',(7.01124720379832,0.00626176734431896,95.7735343568769));
#137412=CARTESIAN_POINT('Ctrl Pts',(6.5711089515182,2.44502632087621,93.8869739242502));
#137413=CARTESIAN_POINT('Ctrl Pts',(6.50187635357225,2.63109177964659,93.8960060995485));
#137414=CARTESIAN_POINT('Ctrl Pts',(6.42476030326037,2.81415210874128,93.9050382748468));
#137415=CARTESIAN_POINT('Ctrl Pts',(6.34004140271719,2.99357671929948,93.9140704501451));
#137416=CARTESIAN_POINT('Ctrl Pts',(6.31324472208978,3.05032891928082,93.9169273370415));
#137417=CARTESIAN_POINT('Ctrl Pts',(6.2856877567968,3.10671754768292,93.9197842239379));
#137418=CARTESIAN_POINT('Ctrl Pts',(6.25738035770925,3.1627231338602,93.9226411108343));
#137419=CARTESIAN_POINT('Ctrl Pts',(6.17947165912967,3.31686383462762,93.9305039434245));
#137420=CARTESIAN_POINT('Ctrl Pts',(6.09575013385189,3.4683483313514,93.9383667760146));
#137421=CARTESIAN_POINT('Ctrl Pts',(6.00642878203697,3.61668907273185,93.9462296086048));
#137422=CARTESIAN_POINT('Ctrl Pts',(5.91717606190045,3.76491583381699,93.9540863996451));
#137423=CARTESIAN_POINT('Ctrl Pts',(5.82233226722473,3.91000331873197,93.9619431906854));
#137424=CARTESIAN_POINT('Ctrl Pts',(5.7221574308434,4.05148625804699,93.9697999817257));
#137425=CARTESIAN_POINT('Ctrl Pts',(5.62203908834727,4.19288940765416,93.9776523419063));
#137426=CARTESIAN_POINT('Ctrl Pts',(5.51659590430895,4.33069174515327,93.9855047020868));
#137427=CARTESIAN_POINT('Ctrl Pts',(5.40613242074995,4.46445504085507,93.9933570622674));
#137428=CARTESIAN_POINT('Ctrl Pts',(5.2956950189893,4.59818675338393,94.0012075684083));
#137429=CARTESIAN_POINT('Ctrl Pts',(5.18023991294407,4.72788102308838,94.0090580745493));
#137430=CARTESIAN_POINT('Ctrl Pts',(5.06011326816006,4.85313097658517,94.0169085806902));
#137431=CARTESIAN_POINT('Ctrl Pts',(4.94000594799955,4.97836078127818,94.02475782393));
#137432=CARTESIAN_POINT('Ctrl Pts',(4.81522885138723,5.09914741974926,94.0326070671699));
#137433=CARTESIAN_POINT('Ctrl Pts',(4.68616617400958,5.2151196680487,94.0404563104097));
#137434=CARTESIAN_POINT('Ctrl Pts',(4.55706001303342,5.33113098953945,94.0483081982044));
#137435=CARTESIAN_POINT('Ctrl Pts',(4.4236656712448,5.44232442567005,94.0561600859992));
#137436=CARTESIAN_POINT('Ctrl Pts',(4.28640185159585,5.54836784371185,94.0640119737939));
#137437=CARTESIAN_POINT('Ctrl Pts',(4.18561090108865,5.62623407916122,94.0697775079028));
#137438=CARTESIAN_POINT('Ctrl Pts',(4.08273435009313,5.70132435415834,94.0755430420118));
#137439=CARTESIAN_POINT('Ctrl Pts',(3.97794824856921,5.77352182763737,94.0813085761207));
#137440=CARTESIAN_POINT('Ctrl Pts',(3.80246749989206,5.89442781148875,94.0909638665385));
#137441=CARTESIAN_POINT('Ctrl Pts',(3.6217206210363,6.00715877938681,94.1006191569563));
#137442=CARTESIAN_POINT('Ctrl Pts',(3.43642534723564,6.1113507013897,94.110274447374));
#137443=CARTESIAN_POINT('Ctrl Pts',(3.25010359377656,6.21611981506249,94.1199832251744));
#137444=CARTESIAN_POINT('Ctrl Pts',(3.05918298027622,6.31225503790836,94.1296920029748));
#137445=CARTESIAN_POINT('Ctrl Pts',(2.86440879581883,6.39943660121231,94.1394007807752));
#137446=CARTESIAN_POINT('Ctrl Pts',(2.66869735528858,6.48703768340617,94.1491562773488));
#137447=CARTESIAN_POINT('Ctrl Pts',(2.46909521699324,6.56559873268788,94.1589117739224));
#137448=CARTESIAN_POINT('Ctrl Pts',(2.26637326359146,6.63484580021102,94.1686672704961));
#137449=CARTESIAN_POINT('Ctrl Pts',(2.06345058232361,6.70416143364852,94.1784324266057));
#137450=CARTESIAN_POINT('Ctrl Pts',(1.85740194688975,6.76414463667469,94.1881975827153));
#137451=CARTESIAN_POINT('Ctrl Pts',(1.64901461151091,6.81457096034105,94.197962738825));
#137452=CARTESIAN_POINT('Ctrl Pts',(1.44091138814327,6.86492853355188,94.2077145812746));
#137453=CARTESIAN_POINT('Ctrl Pts',(1.23047587448614,6.90575526020403,94.2174664237241));
#137454=CARTESIAN_POINT('Ctrl Pts',(1.01850554816107,6.9368777566615,94.2272182661737));
#137455=CARTESIAN_POINT('Ctrl Pts',(0.926069348082637,6.95044968137077,
94.2314708579182));
#137456=CARTESIAN_POINT('Ctrl Pts',(0.833341447425697,6.96217683158084,
94.2357234496627));
#137457=CARTESIAN_POINT('Ctrl Pts',(0.740388755512456,6.97204783784583,
94.2399760414071));
#137458=CARTESIAN_POINT('Ctrl Pts',(0.564802974259925,6.99069397182121,
94.2480091024023));
#137459=CARTESIAN_POINT('Ctrl Pts',(0.38832900081566,7.00272228021506,94.2560421633975));
#137460=CARTESIAN_POINT('Ctrl Pts',(0.211513544993474,7.00805883128733,
94.2640752243926));
#137461=CARTESIAN_POINT('Ctrl Pts',(0.0348117535537583,7.01339195180099,
94.2721031213996));
#137462=CARTESIAN_POINT('Ctrl Pts',(-0.14223071843289,7.01204186670312,
94.2801310184066));
#137463=CARTESIAN_POINT('Ctrl Pts',(-0.319061895785846,7.00398644124598,
94.2881589154136));
#137464=CARTESIAN_POINT('Ctrl Pts',(-0.495813231257835,6.99593465293208,
94.2961831877069));
#137465=CARTESIAN_POINT('Ctrl Pts',(-0.672353096625605,6.9811835691255,
94.3042074600002));
#137466=CARTESIAN_POINT('Ctrl Pts',(-0.848129418562242,6.95976314624782,
94.3122317322934));
#137467=CARTESIAN_POINT('Ctrl Pts',(-1.02388448505733,6.93834531359697,
94.3202550342658));
#137468=CARTESIAN_POINT('Ctrl Pts',(-1.19887582743081,6.91025978490584,
94.3282783362381));
#137469=CARTESIAN_POINT('Ctrl Pts',(-1.37255621721105,6.87558841068132,
94.3363016382104));
#137470=CARTESIAN_POINT('Ctrl Pts',(-1.54622237432089,6.84091987768858,
94.3443242826933));
#137471=CARTESIAN_POINT('Ctrl Pts',(-1.71857743406365,6.79966664989602,
94.3523469271762));
#137472=CARTESIAN_POINT('Ctrl Pts',(-1.88908438818062,6.75196169545061,
94.3603695716592));
#137473=CARTESIAN_POINT('Ctrl Pts',(-2.05965543778592,6.70423880817445,
94.3683952319447));
#137474=CARTESIAN_POINT('Ctrl Pts',(-2.22837664149849,6.65005945107496,
94.3764208922302));
#137475=CARTESIAN_POINT('Ctrl Pts',(-2.39472581272296,6.58960657735941,
94.3844465525158));
#137476=CARTESIAN_POINT('Ctrl Pts',(-2.49281334186375,6.55396063474021,
94.389178870575));
#137477=CARTESIAN_POINT('Ctrl Pts',(-2.59007646852318,6.51613441841792,
94.3939111886343));
#137478=CARTESIAN_POINT('Ctrl Pts',(-2.68641138928797,6.47617328443301,
94.3986435066936));
#137479=CARTESIAN_POINT('Ctrl Pts',(-2.86412647933467,6.40245446608432,
94.4073735115906));
#137480=CARTESIAN_POINT('Ctrl Pts',(-3.03877054674181,6.32143101450371,
94.4161035164877));
#137481=CARTESIAN_POINT('Ctrl Pts',(-3.20976034756245,6.23338311623117,
94.4248335213847));
#137482=CARTESIAN_POINT('Ctrl Pts',(-3.3807995820536,6.14530976304394,94.4335660501527));
#137483=CARTESIAN_POINT('Ctrl Pts',(-3.54818219765204,6.0502080350156,94.4422985789206));
#137484=CARTESIAN_POINT('Ctrl Pts',(-3.71134950975104,5.94840410353657,
94.4510311076886));
#137485=CARTESIAN_POINT('Ctrl Pts',(-3.8768361273496,5.84515310269592,94.4598877630462));
#137486=CARTESIAN_POINT('Ctrl Pts',(-4.03798644675668,5.73500806498855,
94.4687444184038));
#137487=CARTESIAN_POINT('Ctrl Pts',(-4.19424763425525,5.61835503907009,
94.4776010737614));
#137488=CARTESIAN_POINT('Ctrl Pts',(-4.34841689212475,5.5032636928313,94.4863391616101));
#137489=CARTESIAN_POINT('Ctrl Pts',(-4.4978269013566,5.38183771028731,94.4950772494587));
#137490=CARTESIAN_POINT('Ctrl Pts',(-4.64197892219142,5.25448934230821,
94.5038153373073));
#137491=CARTESIAN_POINT('Ctrl Pts',(-4.78906495095671,5.12454898068643,
94.5127312764194));
#137492=CARTESIAN_POINT('Ctrl Pts',(-4.93067643527349,4.98844275982695,
94.5216472155315));
#137493=CARTESIAN_POINT('Ctrl Pts',(-5.06632123746025,4.84664994417373,
94.5305631546437));
#137494=CARTESIAN_POINT('Ctrl Pts',(-5.20196603964701,4.70485712852052,
94.5394790937558));
#137495=CARTESIAN_POINT('Ctrl Pts',(-5.33164395503715,4.55737794082213,
94.5483950328679));
#137496=CARTESIAN_POINT('Ctrl Pts',(-5.45490408292118,4.40473018567878,
94.5573109719801));
#137497=CARTESIAN_POINT('Ctrl Pts',(-5.57574224718861,4.25508183768729,
94.5660517199699));
#137498=CARTESIAN_POINT('Ctrl Pts',(-5.69042532874712,4.10045025632833,
94.5747924679597));
#137499=CARTESIAN_POINT('Ctrl Pts',(-5.79856547132695,3.94135319874214,
94.5835332159496));
#137500=CARTESIAN_POINT('Ctrl Pts',(-5.90668616011302,3.78228476180756,
94.5922723915288));
#137501=CARTESIAN_POINT('Ctrl Pts',(-6.00826610670268,3.61875267927341,
94.6010115671081));
#137502=CARTESIAN_POINT('Ctrl Pts',(-6.10296041194246,3.45130421330302,
94.6097507426873));
#137503=CARTESIAN_POINT('Ctrl Pts',(-6.19888057477878,3.28168805653517,
94.6186030505689));
#137504=CARTESIAN_POINT('Ctrl Pts',(-6.28773541960707,3.10805364859761,
94.6274553584504));
#137505=CARTESIAN_POINT('Ctrl Pts',(-6.3692135494138,2.93099732590524,94.636307666332));
#137506=CARTESIAN_POINT('Ctrl Pts',(-6.44960915198152,2.75629339265295,
94.6450423614943));
#137507=CARTESIAN_POINT('Ctrl Pts',(-6.52282273410113,2.57825816931711,
94.6537770566566));
#137508=CARTESIAN_POINT('Ctrl Pts',(-6.58860235167932,2.39748735428277,
94.6625117518188));
#137509=CARTESIAN_POINT('Ctrl Pts',(-6.6557105536364,2.21306541919246,94.6714228660601));
#137510=CARTESIAN_POINT('Ctrl Pts',(-6.71508118046351,2.02579647755037,
94.6803339803013));
#137511=CARTESIAN_POINT('Ctrl Pts',(-6.76649883805895,1.83633331316702,
94.6892450945425));
#137512=CARTESIAN_POINT('Ctrl Pts',(-6.81791649565438,1.64687014878366,
94.6981562087838));
#137513=CARTESIAN_POINT('Ctrl Pts',(-6.86138109162555,1.45521305064215,
94.707067323025));
#137514=CARTESIAN_POINT('Ctrl Pts',(-6.89673142007993,1.26203101458811,
94.7159784372663));
#137515=CARTESIAN_POINT('Ctrl Pts',(-6.92856904036444,1.08804518252959,
94.7240040676898));
#137516=CARTESIAN_POINT('Ctrl Pts',(-6.95383899451732,0.91274237675236,
94.7320296981133));
#137517=CARTESIAN_POINT('Ctrl Pts',(-6.97244213013835,0.73666634535033,
94.7400553285368));
#137518=CARTESIAN_POINT('Ctrl Pts',(-6.99103936169987,0.560646195031391,
94.7480784118736));
#137519=CARTESIAN_POINT('Ctrl Pts',(-7.00297394870145,0.383853671762942,
94.7561014952104));
#137520=CARTESIAN_POINT('Ctrl Pts',(-7.0081983319312,0.206839799885714,
94.7641245785472));
#137521=CARTESIAN_POINT('Ctrl Pts',(-7.01342205637092,0.0298482492984376,
94.7721466501804));
#137522=CARTESIAN_POINT('Ctrl Pts',(-7.01193725225356,-0.147364227972788,
94.7801687218137));
#137523=CARTESIAN_POINT('Ctrl Pts',(-7.00374843033024,-0.324244486686702,
94.7881907934469));
#137524=CARTESIAN_POINT('Ctrl Pts',(-6.99555656518016,-0.501190479732401,
94.7962158463371));
#137525=CARTESIAN_POINT('Ctrl Pts',(-6.98065571911359,-0.677803640917794,
94.8042408992274));
#137526=CARTESIAN_POINT('Ctrl Pts',(-6.95910248079875,-0.853533376172657,
94.8122659521176));
#137527=CARTESIAN_POINT('Ctrl Pts',(-6.9375449973977,-1.02929772283331,
94.8202925856076));
#137528=CARTESIAN_POINT('Ctrl Pts',(-6.90933256489799,-1.20417793416387,
94.8283192190975));
#137529=CARTESIAN_POINT('Ctrl Pts',(-6.87457325191952,-1.37763172382634,
94.8363458525874));
#137530=CARTESIAN_POINT('Ctrl Pts',(-6.83978603289908,-1.5512247685062,
94.844378930151));
#137531=CARTESIAN_POINT('Ctrl Pts',(-6.79844151683118,-1.72338874676923,
94.8524120077145));
#137532=CARTESIAN_POINT('Ctrl Pts',(-6.7506983351773,-1.89359408267308,
94.860445085278));
#137533=CARTESIAN_POINT('Ctrl Pts',(-6.7225649830702,-1.99389000932927,
94.8651786910363));
#137534=CARTESIAN_POINT('Ctrl Pts',(-6.6922107514037,-2.09350612364148,
94.8699122967947));
#137535=CARTESIAN_POINT('Ctrl Pts',(-6.65967601729563,-2.19233708794005,
94.874645902553));
#137536=CARTESIAN_POINT('Ctrl Pts',(-6.59265675514006,-2.39592191772262,
94.8843967972185));
#137537=CARTESIAN_POINT('Ctrl Pts',(-6.51634348769129,-2.59629432248839,
94.8941476918841));
#137538=CARTESIAN_POINT('Ctrl Pts',(-6.4310532843521,-2.79270124007637,
94.9038985865496));
#137539=CARTESIAN_POINT('Ctrl Pts',(-6.34564023878688,-2.9893910396604,
94.9136635252853));
#137540=CARTESIAN_POINT('Ctrl Pts',(-6.25122441023194,-3.18210389206936,
94.9234284640211));
#137541=CARTESIAN_POINT('Ctrl Pts',(-6.14817084123131,-3.37010710060276,
94.9331934027569));
#137542=CARTESIAN_POINT('Ctrl Pts',(-6.04528905667822,-3.55779691846345,
94.9429420638943));
#137543=CARTESIAN_POINT('Ctrl Pts',(-5.93379832690609,-3.74079274956557,
94.9526907250316));
#137544=CARTESIAN_POINT('Ctrl Pts',(-5.8141078602765,-3.9183895099353,94.962439386169));
#137545=CARTESIAN_POINT('Ctrl Pts',(-5.69474588169057,-4.09549885961964,
94.9721612923048));
#137546=CARTESIAN_POINT('Ctrl Pts',(-5.56722911415492,-4.26723868643634,
94.9818831984406));
#137547=CARTESIAN_POINT('Ctrl Pts',(-5.43200899594852,-4.43293411077069,
94.9916051045764));
#137548=CARTESIAN_POINT('Ctrl Pts',(-5.29768353516487,-4.59753324378936,
95.0012626876248));
#137549=CARTESIAN_POINT('Ctrl Pts',(-5.15575632937569,-4.75616763875545,
95.0109202706731));
#137550=CARTESIAN_POINT('Ctrl Pts',(-5.00671485935146,-4.90820057451296,
95.0205778537215));
#137551=CARTESIAN_POINT('Ctrl Pts',(-4.94120089186002,-4.97502949675336,
95.0248230250941));
#137552=CARTESIAN_POINT('Ctrl Pts',(-4.87431288736589,-5.04058320985438,
95.0290681964667));
#137553=CARTESIAN_POINT('Ctrl Pts',(-4.80609502587495,-5.1048092192324,
95.0333133678393));
#137554=CARTESIAN_POINT('Ctrl Pts',(-4.67991776677221,-5.22360306074709,
95.0411653303094));
#137555=CARTESIAN_POINT('Ctrl Pts',(-4.54924017819775,-5.33780310879539,
95.0490172927794));
#137556=CARTESIAN_POINT('Ctrl Pts',(-4.41444929813963,-5.44704176197086,
95.0568692552495));
#137557=CARTESIAN_POINT('Ctrl Pts',(-4.27969663340054,-5.55624944428256,
95.0647189915657));
#137558=CARTESIAN_POINT('Ctrl Pts',(-4.14083329297538,-5.66049828982078,
95.0725687278818));
#137559=CARTESIAN_POINT('Ctrl Pts',(-3.99828058059538,-5.75945995396564,
95.0804184641979));
#137560=CARTESIAN_POINT('Ctrl Pts',(-3.85573923931381,-5.85841372416864,
95.0882675743588));
#137561=CARTESIAN_POINT('Ctrl Pts',(-3.70950942571087,-5.952080935645,95.0961166845198));
#137562=CARTESIAN_POINT('Ctrl Pts',(-3.56004247387461,-6.04017583739983,
95.1039657946807));
#137563=CARTESIAN_POINT('Ctrl Pts',(-3.41049984157576,-6.12831534475366,
95.1118188791268));
#137564=CARTESIAN_POINT('Ctrl Pts',(-3.25771712513349,-6.21087671102929,
95.1196719635728));
#137565=CARTESIAN_POINT('Ctrl Pts',(-3.10217167429069,-6.28761937983912,
95.1275250480189));
#137566=CARTESIAN_POINT('Ctrl Pts',(-2.94658671213911,-6.36438154265067,
95.135380127288));
#137567=CARTESIAN_POINT('Ctrl Pts',(-2.78823796562709,-6.43532190739377,
95.1432352065571));
#137568=CARTESIAN_POINT('Ctrl Pts',(-2.62762332416813,-6.5002478590272,
95.1510902858262));
#137569=CARTESIAN_POINT('Ctrl Pts',(-2.4668492576413,-6.56523825574577,
95.1589531619968));
#137570=CARTESIAN_POINT('Ctrl Pts',(-2.30380516267747,-6.62420218633519,
95.1668160381675));
#137571=CARTESIAN_POINT('Ctrl Pts',(-2.13900521396493,-6.67699657459331,
95.1746789143381));
#137572=CARTESIAN_POINT('Ctrl Pts',(-2.01812682854345,-6.71572049691133,
95.1804462206006));
#137573=CARTESIAN_POINT('Ctrl Pts',(-1.89630412395199,-6.75112623947254,
95.1862135268632));
#137574=CARTESIAN_POINT('Ctrl Pts',(-1.77374330284097,-6.78317486566039,
95.1919808331257));
#137575=CARTESIAN_POINT('Ctrl Pts',(-1.59570600760469,-6.82973012427239,
95.2003586784964));
#137576=CARTESIAN_POINT('Ctrl Pts',(-1.41571643005545,-6.86930273055412,
95.2087365238672));
#137577=CARTESIAN_POINT('Ctrl Pts',(-1.23434857655575,-6.90173964693358,
95.2171143692379));
#137578=CARTESIAN_POINT('Ctrl Pts',(-1.05310478568801,-6.9341543752067,
95.2254864838382));
#137579=CARTESIAN_POINT('Ctrl Pts',(-0.870484921105141,-6.95944308732083,
95.2338585984384));
#137580=CARTESIAN_POINT('Ctrl Pts',(-0.687074608833712,-6.97750349655205,
95.2422307130386));
#137581=CARTESIAN_POINT('Ctrl Pts',(-0.503762847087054,-6.99555420151535,
95.2505983291116));
#137582=CARTESIAN_POINT('Ctrl Pts',(-0.319661810950971,-7.00638431563548,
95.2589659451846));
#137583=CARTESIAN_POINT('Ctrl Pts',(-0.135364160694557,-7.0099431600049,
95.2673335612576));
#137584=CARTESIAN_POINT('Ctrl Pts',(0.0488614725772959,-7.01350061370418,
95.275697907563));
#137585=CARTESIAN_POINT('Ctrl Pts',(0.233283238565757,-7.00979245737603,
95.2840622538684));
#137586=CARTESIAN_POINT('Ctrl Pts',(0.417306087186306,-6.99882005713086,
95.2924266001739));
#137587=CARTESIAN_POINT('Ctrl Pts',(0.601283974760587,-6.98785033769734,
95.3007889028757));
#137588=CARTESIAN_POINT('Ctrl Pts',(0.784862811519938,-6.96961993374775,
95.3091512055775));
#137589=CARTESIAN_POINT('Ctrl Pts',(0.967449822504712,-6.94418227032065,
95.3175135082792));
#137590=CARTESIAN_POINT('Ctrl Pts',(1.15005142105159,-6.91874257458307,
95.3258764790768));
#137591=CARTESIAN_POINT('Ctrl Pts',(1.33166070912513,-6.88609450834035,
95.3342394498744));
#137592=CARTESIAN_POINT('Ctrl Pts',(1.51169152189781,-6.84634320678728,
95.3426024206719));
#137593=CARTESIAN_POINT('Ctrl Pts',(1.69173462934614,-6.8065891905358,95.350965962594));
#137594=CARTESIAN_POINT('Ctrl Pts',(1.87019872538201,-6.75973104237719,
95.3593295045161));
#137595=CARTESIAN_POINT('Ctrl Pts',(2.04650913221067,-6.70592476354144,
95.3676930464382));
#137596=CARTESIAN_POINT('Ctrl Pts',(2.22285509622956,-6.65210763338883,
95.3760582750676));
#137597=CARTESIAN_POINT('Ctrl Pts',(2.39704619046122,-6.59133967441151,
95.384423503697));
#137598=CARTESIAN_POINT('Ctrl Pts',(2.56852374780163,-6.52382650899601,
95.3927887323264));
#137599=CARTESIAN_POINT('Ctrl Pts',(2.74005876873132,-6.45629071934403,
95.4011567642151));
#137600=CARTESIAN_POINT('Ctrl Pts',(2.90887813371224,-6.38200533641266,
95.4095247961039));
#137601=CARTESIAN_POINT('Ctrl Pts',(3.07444357629574,-6.30122394925572,
95.4178928279926));
#137602=CARTESIAN_POINT('Ctrl Pts',(3.24016260789579,-6.22036762415512,
95.426268622599));
#137603=CARTESIAN_POINT('Ctrl Pts',(3.40262138932765,-6.1330033972065,95.4346444172054));
#137604=CARTESIAN_POINT('Ctrl Pts',(3.56130557271597,-6.03943119674711,
95.4430202118118));
#137605=CARTESIAN_POINT('Ctrl Pts',(3.72006762204644,-5.94581308063694,
95.4514001164002));
#137606=CARTESIAN_POINT('Ctrl Pts',(3.87505109998967,-5.84598108878088,
95.4597800209886));
#137607=CARTESIAN_POINT('Ctrl Pts',(4.02577050543591,-5.74027859951608,
95.468159925577));
#137608=CARTESIAN_POINT('Ctrl Pts',(4.1766622325999,-5.63445525763469,95.4765494111451));
#137609=CARTESIAN_POINT('Ctrl Pts',(4.32327988004096,-5.52274820074212,
95.4849388967131));
#137610=CARTESIAN_POINT('Ctrl Pts',(4.46516985075539,-5.40554204186825,
95.4933283822812));
#137611=CARTESIAN_POINT('Ctrl Pts',(4.55530048958543,-5.33109093076485,
95.4986575094203));
#137612=CARTESIAN_POINT('Ctrl Pts',(4.64352420715487,-5.25442173762011,
95.5039866365594));
#137613=CARTESIAN_POINT('Ctrl Pts',(4.72973243973291,-5.17564079231144,
95.5093157636985));
#137614=CARTESIAN_POINT('Ctrl Pts',(4.86532809813271,-5.05172740458693,
95.5176978692297));
#137615=CARTESIAN_POINT('Ctrl Pts',(4.99620927099563,-4.92233778541204,
95.5260799747609));
#137616=CARTESIAN_POINT('Ctrl Pts',(5.12192216727446,-4.78785336814762,
95.534462080292));
#137617=CARTESIAN_POINT('Ctrl Pts',(5.2474756029481,-4.6535395377299,95.542833553536));
#137618=CARTESIAN_POINT('Ctrl Pts',(5.36787360504213,-4.51414402568894,
95.55120502678));
#137619=CARTESIAN_POINT('Ctrl Pts',(5.48269685785472,-4.37008715329226,
95.5595765000239));
#137620=CARTESIAN_POINT('Ctrl Pts',(5.59738965582937,-4.22619394910285,
95.5679384621352));
#137621=CARTESIAN_POINT('Ctrl Pts',(5.70652012533998,-4.07765019455054,
95.5763004242465));
#137622=CARTESIAN_POINT('Ctrl Pts',(5.80970681905494,-3.92491187660647,
95.5846623863578));
#137623=CARTESIAN_POINT('Ctrl Pts',(5.91275937009221,-3.77237211844001,
95.5930134779204));
#137624=CARTESIAN_POINT('Ctrl Pts',(6.00988337499843,-3.61564894348179,
95.601364569483));
#137625=CARTESIAN_POINT('Ctrl Pts',(6.10073863513935,-3.45523004562911,
95.6097156610455));
#137626=CARTESIAN_POINT('Ctrl Pts',(6.19152385067765,-3.29493482226631,
95.6180603143579));
#137627=CARTESIAN_POINT('Ctrl Pts',(6.27604979176538,-3.13094983776781,
95.6264049676704));
#137628=CARTESIAN_POINT('Ctrl Pts',(6.3540198206988,-2.96379126806644,95.6347496209828));
#137629=CARTESIAN_POINT('Ctrl Pts',(6.43192702679084,-2.79676738314655,
95.6430875507523));
#137630=CARTESIAN_POINT('Ctrl Pts',(6.50328871748195,-2.62657530869652,
95.6514254805219));
#137631=CARTESIAN_POINT('Ctrl Pts',(6.56785435721423,-2.45375542891343,
95.6597634102914));
#137632=CARTESIAN_POINT('Ctrl Pts',(6.58907136859494,-2.39696482989859,
95.662503349856));
#137633=CARTESIAN_POINT('Ctrl Pts',(6.60955487975253,-2.33989065198608,
95.6652432894205));
#137634=CARTESIAN_POINT('Ctrl Pts',(6.62929711484721,-2.28255258988231,
95.6679832289851));
#137635=CARTESIAN_POINT('Ctrl Pts',(6.68657087311171,-2.11621041572944,
95.6759320065944));
#137636=CARTESIAN_POINT('Ctrl Pts',(6.73757578283835,-1.94772267464687,
95.6838807842038));
#137637=CARTESIAN_POINT('Ctrl Pts',(6.78216126708796,-1.77761500604372,
95.6918295618131));
#137638=CARTESIAN_POINT('Ctrl Pts',(6.82677318622033,-1.60740648003483,
95.6997830522793));
#137639=CARTESIAN_POINT('Ctrl Pts',(6.86495798444069,-1.43557646827384,
95.7077365427454));
#137640=CARTESIAN_POINT('Ctrl Pts',(6.89661578464703,-1.26266277424235,
95.7156900332116));
#137641=CARTESIAN_POINT('Ctrl Pts',(6.92828431387029,-1.08969047873084,
95.723646219163));
#137642=CARTESIAN_POINT('Ctrl Pts',(6.95342138408531,-0.915634136736948,
95.7316024051145));
#137643=CARTESIAN_POINT('Ctrl Pts',(6.97197888062647,-0.741037819951529,
95.7395585910659));
#137644=CARTESIAN_POINT('Ctrl Pts',(6.99055419794442,-0.566273838202059,
95.7475224173483));
#137645=CARTESIAN_POINT('Ctrl Pts',(7.0025373003759,-0.390969216497577,
95.7554862436306));
#137646=CARTESIAN_POINT('Ctrl Pts',(7.00793215743705,-0.215669745814628,
95.7634500699129));
#137647=CARTESIAN_POINT('Ctrl Pts',(7.01020925744758,-0.141678086348179,
95.7668114989009));
#137648=CARTESIAN_POINT('Ctrl Pts',(7.01131324795972,-0.0676873138804065,
95.7701729278889));
#137649=CARTESIAN_POINT('Ctrl Pts',(7.01124720379832,0.00626176734413354,
95.7735343568769));
#137650=CARTESIAN_POINT('Ctrl Pts',(7.01124720379766,0.00626176808250687,
95.7735343569104));
#137651=CARTESIAN_POINT('Ctrl Pts',(7.01104753157553,0.229833016751859,
95.783697010235));
#137652=CARTESIAN_POINT('Ctrl Pts',(7.00015032087312,0.453038581417428,
95.7938596635596));
#137653=CARTESIAN_POINT('Ctrl Pts',(6.97868319966095,0.67498693414758,95.8040223168842));
#137654=CARTESIAN_POINT('Ctrl Pts',(6.96275015197189,0.83971855575671,95.8115651093466));
#137655=CARTESIAN_POINT('Ctrl Pts',(6.94099549368888,1.00375802951486,95.819107901809));
#137656=CARTESIAN_POINT('Ctrl Pts',(6.91348882294048,1.16674712666332,95.8266506942714));
#137657=CARTESIAN_POINT('Ctrl Pts',(6.88289091793965,1.34805314353229,95.8350411552369));
#137658=CARTESIAN_POINT('Ctrl Pts',(6.84513049928511,1.52830961949353,95.8434316162024));
#137659=CARTESIAN_POINT('Ctrl Pts',(6.80029542651758,1.70692960446064,95.8518220771679));
#137660=CARTESIAN_POINT('Ctrl Pts',(6.75550718787773,1.88536300533929,95.8602037735682));
#137661=CARTESIAN_POINT('Ctrl Pts',(6.7036591118458,2.06216300663596,95.8685854699685));
#137662=CARTESIAN_POINT('Ctrl Pts',(6.64489020906763,2.23675225984844,95.8769671663687));
#137663=CARTESIAN_POINT('Ctrl Pts',(6.62139804949321,2.3065422066155,95.8803176483419));
#137664=CARTESIAN_POINT('Ctrl Pts',(6.59680058005374,2.37597901091167,95.883668130315));
#137665=CARTESIAN_POINT('Ctrl Pts',(6.57110895151813,2.44502632087639,95.8870186122881));
#137666=CARTESIAN_POINT('',(7.01124998147128,-0.000509724478313664,95.2264656430492));
#137667=CARTESIAN_POINT('Ctrl Pts',(6.57110895151813,2.44502632087639,95.3399143481975));
#137668=CARTESIAN_POINT('Ctrl Pts',(6.63828885140506,2.26447757269324,95.3311708067522));
#137669=CARTESIAN_POINT('Ctrl Pts',(6.69801113786194,2.08119179622191,95.3224272653069));
#137670=CARTESIAN_POINT('Ctrl Pts',(6.75008250258809,1.89578816610774,95.3136837238615));
#137671=CARTESIAN_POINT('Ctrl Pts',(6.80217888112286,1.71029547262937,95.304935982233));
#137672=CARTESIAN_POINT('Ctrl Pts',(6.84661691862439,1.52268315392854,95.2961882406044));
#137673=CARTESIAN_POINT('Ctrl Pts',(6.88325357075376,1.33358420926676,95.2874404989759));
#137674=CARTESIAN_POINT('Ctrl Pts',(6.91989559434719,1.14445753995966,95.2786914748016));
#137675=CARTESIAN_POINT('Ctrl Pts',(6.94873390074258,0.95384407704325,95.2699424506274));
#137676=CARTESIAN_POINT('Ctrl Pts',(6.9696767566655,0.762386037448659,95.2611934264531));
#137677=CARTESIAN_POINT('Ctrl Pts',(6.99062463973899,0.570882040015487,
95.2524423021516));
#137678=CARTESIAN_POINT('Ctrl Pts',(7.003673256796,0.378533331093741,95.2436911778502));
#137679=CARTESIAN_POINT('Ctrl Pts',(7.00878272003862,0.185987488256714,
95.2349400535487));
#137680=CARTESIAN_POINT('Ctrl Pts',(7.01043202006958,0.123834997970955,
95.2321152500623));
#137681=CARTESIAN_POINT('Ctrl Pts',(7.0112545014055,0.0616619882938663,
95.2292904465759));
#137682=CARTESIAN_POINT('Ctrl Pts',(7.01124998147134,-0.000509723591843963,
95.2264656430895));
#137683=CARTESIAN_POINT('Ctrl Pts',(7.01124998147128,-0.000509724478307598,
95.2264656430492));
#137684=CARTESIAN_POINT('Ctrl Pts',(7.0112361212336,-0.191157015833348,
95.2178034859852));
#137685=CARTESIAN_POINT('Ctrl Pts',(7.00344264641733,-0.381774601940022,
95.2091413289212));
#137686=CARTESIAN_POINT('Ctrl Pts',(6.98789830773228,-0.571755020347335,
95.2004791718571));
#137687=CARTESIAN_POINT('Ctrl Pts',(6.97221312830826,-0.763456771714571,
95.1917385306178));
#137688=CARTESIAN_POINT('Ctrl Pts',(6.94863424231851,-0.954522918722355,
95.1829978893785));
#137689=CARTESIAN_POINT('Ctrl Pts',(6.91723779925416,-1.14431105520722,
95.1742572481392));
#137690=CARTESIAN_POINT('Ctrl Pts',(6.885847007391,-1.33406503078608,95.1655181801712));
#137691=CARTESIAN_POINT('Ctrl Pts',(6.8466415132512,-1.52254118520631,95.1567791122032));
#137692=CARTESIAN_POINT('Ctrl Pts',(6.79974892227699,-1.70910536728807,
95.1480400442352));
#137693=CARTESIAN_POINT('Ctrl Pts',(6.75224841453578,-1.89808817227066,
95.1391876827631));
#137694=CARTESIAN_POINT('Ctrl Pts',(6.69686015602426,-2.08510880351682,
95.1303353212911));
#137695=CARTESIAN_POINT('Ctrl Pts',(6.6337698661138,-2.26952063791905,95.1214829598191));
#137696=CARTESIAN_POINT('Ctrl Pts',(6.57151893982451,-2.45147902686511,
95.1127483716239));
#137697=CARTESIAN_POINT('Ctrl Pts',(6.50176975096737,-2.63089734201636,
95.1040137834287));
#137698=CARTESIAN_POINT('Ctrl Pts',(6.42475062516298,-2.80717045563105,
95.0952791952336));
#137699=CARTESIAN_POINT('Ctrl Pts',(6.34617376224076,-2.98700875086897,
95.0863679471231));
#137700=CARTESIAN_POINT('Ctrl Pts',(6.26002985133079,-3.163572988579,95.0774566990127));
#137701=CARTESIAN_POINT('Ctrl Pts',(6.16661307742381,-3.33624185511868,
95.0685454509022));
#137702=CARTESIAN_POINT('Ctrl Pts',(6.07319630351675,-3.50891072165848,
95.0596342027918));
#137703=CARTESIAN_POINT('Ctrl Pts',(5.97250679901631,-3.67768394398257,
95.0507229546813));
#137704=CARTESIAN_POINT('Ctrl Pts',(5.8648891767254,-3.84196583889411,95.0418117065708));
#137705=CARTESIAN_POINT('Ctrl Pts',(5.76796621207698,-3.98992198170726,
95.0337860266943));
#137706=CARTESIAN_POINT('Ctrl Pts',(5.66537871576854,-4.13430281766559,
95.0257603468177));
#137707=CARTESIAN_POINT('Ctrl Pts',(5.5574298503824,-4.27464618659588,95.0177346669411));
#137708=CARTESIAN_POINT('Ctrl Pts',(5.44951524391398,-4.41494501580904,
95.009711534114));
#137709=CARTESIAN_POINT('Ctrl Pts',(5.33624287911491,-4.55120863880943,
95.001688401287));
#137710=CARTESIAN_POINT('Ctrl Pts',(5.21795829983034,-4.68300520432464,
94.9936652684599));
#137711=CARTESIAN_POINT('Ctrl Pts',(5.09968863590153,-4.8147851506603,94.9856431473275));
#137712=CARTESIAN_POINT('Ctrl Pts',(4.97640826162327,-4.94209888916911,
94.9776210261951));
#137713=CARTESIAN_POINT('Ctrl Pts',(4.84850189233173,-5.064548939694,94.9695989050627));
#137714=CARTESIAN_POINT('Ctrl Pts',(4.72054799116709,-5.18704449444433,
94.9615738027931));
#137715=CARTESIAN_POINT('Ctrl Pts',(4.58796492375905,-5.30467249466362,
94.9535487005234));
#137716=CARTESIAN_POINT('Ctrl Pts',(4.45117336090242,-5.4170732202632,94.9455235982538));
#137717=CARTESIAN_POINT('Ctrl Pts',(4.3143548565839,-5.52949608348444,94.9374969154189));
#137718=CARTESIAN_POINT('Ctrl Pts',(4.17332649436964,-5.63668939519169,
94.929470232584));
#137719=CARTESIAN_POINT('Ctrl Pts',(4.02854049785834,-5.7383349518493,94.9214435497491));
#137720=CARTESIAN_POINT('Ctrl Pts',(3.88363826725005,-5.84006210948888,
94.9134104230989));
#137721=CARTESIAN_POINT('Ctrl Pts',(3.73497268268544,-5.93623241388068,
94.9053772964486));
#137722=CARTESIAN_POINT('Ctrl Pts',(3.583023820385,-6.02657173400049,94.8973441697983));
#137723=CARTESIAN_POINT('Ctrl Pts',(3.49349193255858,-6.07980181254685,
94.8926108602937));
#137724=CARTESIAN_POINT('Ctrl Pts',(3.40282062370097,-6.13100832510659,
94.8878775507891));
#137725=CARTESIAN_POINT('Ctrl Pts',(3.31111175468953,-6.18014283900112,
94.8831442412844));
#137726=CARTESIAN_POINT('Ctrl Pts',(3.12218526897516,-6.28136326770599,
94.8733933029058));
#137727=CARTESIAN_POINT('Ctrl Pts',(2.92874330649156,-6.37384810930885,
94.8636423645271));
#137728=CARTESIAN_POINT('Ctrl Pts',(2.73153480288774,-6.45727064502589,
94.8538914261484));
#137729=CARTESIAN_POINT('Ctrl Pts',(2.53404219872951,-6.5408133600872,94.8441264404698));
#137730=CARTESIAN_POINT('Ctrl Pts',(2.33277223520612,-6.61526763987094,
94.8343614547911));
#137731=CARTESIAN_POINT('Ctrl Pts',(2.12849454646976,-6.68035459598879,
94.8245964691125));
#137732=CARTESIAN_POINT('Ctrl Pts',(1.92455734717772,-6.74533306536166,
94.814847759683));
#137733=CARTESIAN_POINT('Ctrl Pts',(1.71762247828284,-6.80097540445833,
94.8050990502535));
#137734=CARTESIAN_POINT('Ctrl Pts',(1.50847251724456,-6.84705317835475,
94.795350340824));
#137735=CARTESIAN_POINT('Ctrl Pts',(1.29989658107158,-6.89300448898136,
94.785628387324));
#137736=CARTESIAN_POINT('Ctrl Pts',(1.08911772839842,-6.92944363071684,
94.775906433824));
#137737=CARTESIAN_POINT('Ctrl Pts',(0.876928290491243,-6.9561931640687,
94.7661844803241));
#137738=CARTESIAN_POINT('Ctrl Pts',(0.666142826622615,-6.98276570628123,
94.7565268531659));
#137739=CARTESIAN_POINT('Ctrl Pts',(0.453965425095591,-6.99977640646644,
94.7468692260078));
#137740=CARTESIAN_POINT('Ctrl Pts',(0.241188204550884,-7.00710031414461,
94.7372115988496));
#137741=CARTESIAN_POINT('Ctrl Pts',(0.147663498942555,-7.01031948538743,
94.732966657899));
#137742=CARTESIAN_POINT('Ctrl Pts',(0.0540231067980854,-7.01166783076978,
94.7287217169485));
#137743=CARTESIAN_POINT('Ctrl Pts',(-0.0396647883031719,-7.01113780117528,
94.7244767759979));
#137744=CARTESIAN_POINT('Ctrl Pts',(-0.212958871141005,-7.01015740779194,
94.7166249276034));
#137745=CARTESIAN_POINT('Ctrl Pts',(-0.386344281524747,-7.00274699430326,
94.708773079209));
#137746=CARTESIAN_POINT('Ctrl Pts',(-0.559287245110139,-6.98890723503733,
94.7009212308145));
#137747=CARTESIAN_POINT('Ctrl Pts',(-0.732181163604306,-6.97507140060443,
94.6930716091346));
#137748=CARTESIAN_POINT('Ctrl Pts',(-0.904632505016229,-6.95480987765999,
94.6852219874547));
#137749=CARTESIAN_POINT('Ctrl Pts',(-1.07610975018039,-6.92817539963205,
94.6773723657749));
#137750=CARTESIAN_POINT('Ctrl Pts',(-1.24757330519985,-6.90154304800787,
94.6695233707814));
#137751=CARTESIAN_POINT('Ctrl Pts',(-1.41806254195812,-6.86853881345922,
94.6616743757879));
#137752=CARTESIAN_POINT('Ctrl Pts',(-1.58705356492891,-6.8292669844242,
94.6538253807944));
#137753=CARTESIAN_POINT('Ctrl Pts',(-1.75613014320212,-6.78997527318982,
94.6459724120802));
#137754=CARTESIAN_POINT('Ctrl Pts',(-1.92370662011442,-6.7444097139101,
94.6381194433659));
#137755=CARTESIAN_POINT('Ctrl Pts',(-2.08927142499908,-6.69272526518027,
94.6302664746516));
#137756=CARTESIAN_POINT('Ctrl Pts',(-2.25487827786347,-6.64102769031138,
94.6224115115433));
#137757=CARTESIAN_POINT('Ctrl Pts',(-2.41847208116772,-6.5832082572014,
94.6145565484349));
#137758=CARTESIAN_POINT('Ctrl Pts',(-2.57955944905294,-6.51947080761174,
94.6067015853266));
#137759=CARTESIAN_POINT('Ctrl Pts',(-2.7408067096049,-6.45567009327998,
94.5988388255113));
#137760=CARTESIAN_POINT('Ctrl Pts',(-2.89954221677495,-6.38593978369819,
94.590976065696));
#137761=CARTESIAN_POINT('Ctrl Pts',(-3.05529495226595,-6.31053082689232,
94.5831133058807));
#137762=CARTESIAN_POINT('Ctrl Pts',(-3.16955273815895,-6.25521198826018,
94.577345307491));
#137763=CARTESIAN_POINT('Ctrl Pts',(-3.28220583407523,-6.19683819014807,
94.5715773091013));
#137764=CARTESIAN_POINT('Ctrl Pts',(-3.39307799138816,-6.13552347455841,
94.5658093107116));
#137765=CARTESIAN_POINT('Ctrl Pts',(-3.55412074151983,-6.04646332941998,
94.5574312440631));
#137766=CARTESIAN_POINT('Ctrl Pts',(-3.71176189921178,-5.95099977948673,
94.5490531774146));
#137767=CARTESIAN_POINT('Ctrl Pts',(-3.86548021925314,-5.8494178545444,
94.540675110766));
#137768=CARTESIAN_POINT('Ctrl Pts',(-4.01909342862906,-5.74790539005234,
94.5323027729348));
#137769=CARTESIAN_POINT('Ctrl Pts',(-4.16878887486382,-5.64028307220438,
94.5239304351035));
#137770=CARTESIAN_POINT('Ctrl Pts',(-4.31407189674095,-5.52688069640099,
94.5155580972722));
#137771=CARTESIAN_POINT('Ctrl Pts',(-4.45927688174548,-5.41353923319868,
94.5071902565325));
#137772=CARTESIAN_POINT('Ctrl Pts',(-4.60007390954955,-5.29442410429784,
94.4988224157929));
#137773=CARTESIAN_POINT('Ctrl Pts',(-4.73599881429735,-5.16990732929267,
94.4904545750532));
#137774=CARTESIAN_POINT('Ctrl Pts',(-4.87187062076578,-5.04543919604686,
94.4820900031622));
#137775=CARTESIAN_POINT('Ctrl Pts',(-5.00287385753673,-4.91557384629412,
94.4737254312712));
#137776=CARTESIAN_POINT('Ctrl Pts',(-5.12857851876945,-4.78072263777314,
94.4653608593803));
#137777=CARTESIAN_POINT('Ctrl Pts',(-5.25425247432167,-4.64590436914542,
94.4569983306901));
#137778=CARTESIAN_POINT('Ctrl Pts',(-5.37463021182608,-4.50610291102031,
94.448635802));
#137779=CARTESIAN_POINT('Ctrl Pts',(-5.48931927309987,-4.36176575259083,
94.4402732733099));
#137780=CARTESIAN_POINT('Ctrl Pts',(-5.60401748697299,-4.21741707553731,
94.4319100772599));
#137781=CARTESIAN_POINT('Ctrl Pts',(-5.71302590843547,-4.06853222859119,
94.42354688121));
#137782=CARTESIAN_POINT('Ctrl Pts',(-5.81599252567866,-3.91559159051987,
94.41518368516));
#137783=CARTESIAN_POINT('Ctrl Pts',(-5.91896616506448,-3.76264052216538,
94.4068199187547));
#137784=CARTESIAN_POINT('Ctrl Pts',(-6.01589699479677,-3.60563338378847,
94.3984561523495));
#137785=CARTESIAN_POINT('Ctrl Pts',(-6.10647639890076,-3.44507946964479,
94.3900923859442));
#137786=CARTESIAN_POINT('Ctrl Pts',(-6.19707405672115,-3.2844932004018,
94.3817269340584));
#137787=CARTESIAN_POINT('Ctrl Pts',(-6.28131757511919,-3.12035901652222,
94.3733614821727));
#137788=CARTESIAN_POINT('Ctrl Pts',(-6.35894415134763,-2.9532111070057,
94.3649960302869));
#137789=CARTESIAN_POINT('Ctrl Pts',(-6.43659672457433,-2.78600721996028,
94.3566277768266));
#137790=CARTESIAN_POINT('Ctrl Pts',(-6.50762779842954,-2.61578789279873,
94.3482595233663));
#137791=CARTESIAN_POINT('Ctrl Pts',(-6.57182242155886,-2.44310798410473,
94.339891269906));
#137792=CARTESIAN_POINT('Ctrl Pts',(-6.63607656226229,-2.27026797649961,
94.3315152578809));
#137793=CARTESIAN_POINT('Ctrl Pts',(-6.69348147161074,-2.09496313711963,
94.3231392458558));
#137794=CARTESIAN_POINT('Ctrl Pts',(-6.743871475126,-1.91776538958285,94.3147632338307));
#137795=CARTESIAN_POINT('Ctrl Pts',(-6.79428619052218,-1.74048074207921,
94.3063831141056));
#137796=CARTESIAN_POINT('Ctrl Pts',(-6.8376790560864,-1.56130165302996,
94.2980029943806));
#137797=CARTESIAN_POINT('Ctrl Pts',(-6.87393525062261,-1.38081162102146,
94.2896228746556));
#137798=CARTESIAN_POINT('Ctrl Pts',(-6.91023287244487,-1.2001153563324,
94.2812331795843));
#137799=CARTESIAN_POINT('Ctrl Pts',(-6.93937747039629,-1.01810547921289,
94.272843484513));
#137800=CARTESIAN_POINT('Ctrl Pts',(-6.96130576314877,-0.835373350336043,
94.2644537894417));
#137801=CARTESIAN_POINT('Ctrl Pts',(-6.97522765034631,-0.719359937239801,
94.259127319674));
#137802=CARTESIAN_POINT('Ctrl Pts',(-6.98624186628942,-0.603055503846008,
94.2538008499063));
#137803=CARTESIAN_POINT('Ctrl Pts',(-6.99434311623776,-0.486611687937667,
94.2484743801386));
#137804=CARTESIAN_POINT('Ctrl Pts',(-7.00709058383352,-0.303385176043139,
94.2400930808086));
#137805=CARTESIAN_POINT('Ctrl Pts',(-7.0126488046885,-0.119443890516184,
94.2317117814786));
#137806=CARTESIAN_POINT('Ctrl Pts',(-7.01095217616346,0.0646231077001102,
94.2233304821486));
#137807=CARTESIAN_POINT('Ctrl Pts',(-7.00925769786619,0.248456827997535,
94.214959804886));
#137808=CARTESIAN_POINT('Ctrl Pts',(-7.00032669678299,0.432415618489739,
94.2065891276235));
#137809=CARTESIAN_POINT('Ctrl Pts',(-6.98414535408088,0.615906028197919,
94.1982184503609));
#137810=CARTESIAN_POINT('Ctrl Pts',(-6.96798237441505,0.79918820790225,
94.189857272375));
#137811=CARTESIAN_POINT('Ctrl Pts',(-6.94458548082508,0.982002741823236,
94.181496094389));
#137812=CARTESIAN_POINT('Ctrl Pts',(-6.91399287360932,1.16375646343191,
94.173134916403));
#137813=CARTESIAN_POINT('Ctrl Pts',(-6.8834399638653,1.34527433841344,94.1647845880196));
#137814=CARTESIAN_POINT('Ctrl Pts',(-6.84571001881183,1.52573382513217,
94.1564342596361));
#137815=CARTESIAN_POINT('Ctrl Pts',(-6.80089297609951,1.70454723904631,
94.1480839312526));
#137816=CARTESIAN_POINT('Ctrl Pts',(-6.75611041737517,1.88322306691632,
94.1397400279388));
#137817=CARTESIAN_POINT('Ctrl Pts',(-6.70425170732731,2.06025502952005,
94.1313961246251));
#137818=CARTESIAN_POINT('Ctrl Pts',(-6.645457971086,2.23506485745482,94.1230522213113));
#137819=CARTESIAN_POINT('Ctrl Pts',(-6.58671145822696,2.40973427738261,
94.1147150198566));
#137820=CARTESIAN_POINT('Ctrl Pts',(-6.52104113237696,2.58218481256943,
94.106377818402));
#137821=CARTESIAN_POINT('Ctrl Pts',(-6.4486381991627,2.75185245585582,94.0980406169473));
#137822=CARTESIAN_POINT('Ctrl Pts',(-6.42480349531027,2.80770624314788,
94.0952960495823));
#137823=CARTESIAN_POINT('Ctrl Pts',(-6.40023958291021,2.86325857395583,
94.0925514822173));
#137824=CARTESIAN_POINT('Ctrl Pts',(-6.37495445485872,2.91848972260946,
94.0898069148523));
#137825=CARTESIAN_POINT('Ctrl Pts',(-6.29813533133327,3.08628829662637,
94.0814686039287));
#137826=CARTESIAN_POINT('Ctrl Pts',(-6.21471876978014,3.25098310266206,
94.0731302930051));
#137827=CARTESIAN_POINT('Ctrl Pts',(-6.12499220819052,3.41205173057289,
94.0647919820815));
#137828=CARTESIAN_POINT('Ctrl Pts',(-6.03520919354575,3.57322169766326,
94.056448424962));
#137829=CARTESIAN_POINT('Ctrl Pts',(-5.93910841956179,3.73076064971112,
94.0481048678425));
#137830=CARTESIAN_POINT('Ctrl Pts',(-5.83702160499475,3.88417370174462,
94.0397613107229));
#137831=CARTESIAN_POINT('Ctrl Pts',(-5.73485712307489,4.03770346998374,
94.0314114058493));
#137832=CARTESIAN_POINT('Ctrl Pts',(-5.62669769781489,4.18710080451423,
94.0230615009756));
#137833=CARTESIAN_POINT('Ctrl Pts',(-5.51291665075698,4.33190218775845,
94.014711596102));
#137834=CARTESIAN_POINT('Ctrl Pts',(-5.3989649403619,4.47692076259944,94.0063491669752));
#137835=CARTESIAN_POINT('Ctrl Pts',(-5.27937496094393,4.61732935273054,
93.9979867378485));
#137836=CARTESIAN_POINT('Ctrl Pts',(-5.15455938017851,4.75269861854439,
93.9896243087217));
#137837=CARTESIAN_POINT('Ctrl Pts',(-5.0296370649608,4.88818364365972,93.9812547285704));
#137838=CARTESIAN_POINT('Ctrl Pts',(-4.89948046325432,5.01862051488014,
93.972885148419));
#137839=CARTESIAN_POINT('Ctrl Pts',(-4.76453734851546,5.14361841674723,
93.9645155682676));
#137840=CARTESIAN_POINT('Ctrl Pts',(-4.62938610035829,5.26880911274574,
93.9561330790521));
#137841=CARTESIAN_POINT('Ctrl Pts',(-4.48943383498332,5.38854386317474,
93.9477505898365));
#137842=CARTESIAN_POINT('Ctrl Pts',(-4.34516057201049,5.50247273195838,
93.939368100621));
#137843=CARTESIAN_POINT('Ctrl Pts',(-4.29795206758839,5.53975206837146,
93.9366252169359));
#137844=CARTESIAN_POINT('Ctrl Pts',(-4.25028113534035,5.57641011894225,
93.9338823332509));
#137845=CARTESIAN_POINT('Ctrl Pts',(-4.20216521516159,5.6124356626144,93.9311394495658));
#137846=CARTESIAN_POINT('Ctrl Pts',(-4.05498959952533,5.72262957658055,
93.9227495945351));
#137847=CARTESIAN_POINT('Ctrl Pts',(-3.90335144205516,5.82712488836485,
93.9143597395044));
#137848=CARTESIAN_POINT('Ctrl Pts',(-3.74771901562641,5.92555725163569,
93.9059698844737));
#137849=CARTESIAN_POINT('Ctrl Pts',(-3.5922302046576,6.02389878287717,93.8975877714857));
#137850=CARTESIAN_POINT('Ctrl Pts',(-3.43275474896218,6.11618834397735,
93.8892056584976));
#137851=CARTESIAN_POINT('Ctrl Pts',(-3.26979150759557,6.20210368015208,
93.8808235455096));
#137852=CARTESIAN_POINT('Ctrl Pts',(-3.10695469120048,6.28795236421656,
93.8724479352666));
#137853=CARTESIAN_POINT('Ctrl Pts',(-2.9406357733876,6.36743652952064,93.8640723250235));
#137854=CARTESIAN_POINT('Ctrl Pts',(-2.77136032176782,6.44027860650694,
93.8556967147804));
#137855=CARTESIAN_POINT('Ctrl Pts',(-2.60219134695188,6.51307486473176,
93.8473263729221));
#137856=CARTESIAN_POINT('Ctrl Pts',(-2.43006984759072,6.57923723554096,
93.8389560310638));
#137857=CARTESIAN_POINT('Ctrl Pts',(-2.25554400260022,6.63853506542175,
93.8305856892055));
#137858=CARTESIAN_POINT('Ctrl Pts',(-2.0811023534555,6.69780428847391,93.8222193854197));
#137859=CARTESIAN_POINT('Ctrl Pts',(-1.90425898244262,6.75021546897039,
93.8138530816339));
#137860=CARTESIAN_POINT('Ctrl Pts',(-1.72558039696885,6.79558671904765,
93.805486777848));
#137861=CARTESIAN_POINT('Ctrl Pts',(-1.54695178291362,6.84094528005129,
93.7971228138841));
#137862=CARTESIAN_POINT('Ctrl Pts',(-1.36648929573607,6.87926775432321,
93.7887588499202));
#137863=CARTESIAN_POINT('Ctrl Pts',(-1.18477343692728,6.9104224520395,93.7803948859562));
#137864=CARTESIAN_POINT('Ctrl Pts',(-1.00308554118196,6.94157235556337,
93.772032209068));
#137865=CARTESIAN_POINT('Ctrl Pts',(-0.820144982193359,6.96555662617638,
93.7636695321797));
#137866=CARTESIAN_POINT('Ctrl Pts',(-0.63654167632221,6.98229484172682,
93.7553068552914));
#137867=CARTESIAN_POINT('Ctrl Pts',(-0.452942150515298,6.99903271266728,
93.7469443505757));
#137868=CARTESIAN_POINT('Ctrl Pts',(-0.26868023236139,7.00852479657975,
93.73858184586));
#137869=CARTESIAN_POINT('Ctrl Pts',(-0.0843506078644922,7.01074258102898,
93.7302193411443));
#137870=CARTESIAN_POINT('Ctrl Pts',(0.0999997914473017,7.01296061543294,
93.721855893935));
#137871=CARTESIAN_POINT('Ctrl Pts',(0.284417583697126,7.00790271241574,
93.7134924467257));
#137872=CARTESIAN_POINT('Ctrl Pts',(0.468307997641202,6.99559248254537,
93.7051289995165));
#137873=CARTESIAN_POINT('Ctrl Pts',(0.65230669144216,6.98327500406481,93.6967606276738));
#137874=CARTESIAN_POINT('Ctrl Pts',(0.835777058083837,6.96369668652283,
93.6883922558312));
#137875=CARTESIAN_POINT('Ctrl Pts',(1.01812831911072,6.93693313275577,93.6800238839885));
#137876=CARTESIAN_POINT('Ctrl Pts',(1.20053421734851,6.91016155992746,93.6716530047626));
#137877=CARTESIAN_POINT('Ctrl Pts',(1.38182001689554,6.87620051104445,93.6632821255368));
#137878=CARTESIAN_POINT('Ctrl Pts',(1.56140433387198,6.83517688642114,93.6549112463109));
#137879=CARTESIAN_POINT('Ctrl Pts',(1.74114081073084,6.79411850291686,93.646533274528));
#137880=CARTESIAN_POINT('Ctrl Pts',(1.91917260489268,6.74598566497688,93.6381553027452));
#137881=CARTESIAN_POINT('Ctrl Pts',(2.09493158789428,6.69095570188166,93.6297773309623));
#137882=CARTESIAN_POINT('Ctrl Pts',(2.2066278814681,6.65598370324884,93.6244530603058));
#137883=CARTESIAN_POINT('Ctrl Pts',(2.31740656456287,6.61822716054034,93.6191287896493));
#137884=CARTESIAN_POINT('Ctrl Pts',(2.42712577899684,6.5777417869227,93.6138045189929));
#137885=CARTESIAN_POINT('Ctrl Pts',(2.58915804863564,6.51795338059584,93.6059416878279));
#137886=CARTESIAN_POINT('Ctrl Pts',(2.74921560712617,6.45208674590067,93.598078856663));
#137887=CARTESIAN_POINT('Ctrl Pts',(2.90678976092369,6.38029778680347,93.5902160254981));
#137888=CARTESIAN_POINT('Ctrl Pts',(3.06424283977971,6.30856398804705,93.5823592358812));
#137889=CARTESIAN_POINT('Ctrl Pts',(3.21921596389303,6.23091707131086,93.5745024462643));
#137890=CARTESIAN_POINT('Ctrl Pts',(3.37121720233194,6.14756221092566,93.5666456566475));
#137891=CARTESIAN_POINT('Ctrl Pts',(3.52313271926429,6.0642543587378,93.5587932978882));
#137892=CARTESIAN_POINT('Ctrl Pts',(3.6720793512138,5.97524514900516,93.5509409391289));
#137893=CARTESIAN_POINT('Ctrl Pts',(3.81758694488272,5.88078706303511,93.5430885803697));
#137894=CARTESIAN_POINT('Ctrl Pts',(3.96306018250727,5.7863512797237,93.5352380756441));
#137895=CARTESIAN_POINT('Ctrl Pts',(4.10509567385016,5.68646938108812,93.5273875709186));
#137896=CARTESIAN_POINT('Ctrl Pts',(4.24324966123014,5.58143878179904,93.5195370661931));
#137897=CARTESIAN_POINT('Ctrl Pts',(4.38138142398535,5.47642507862495,93.5116878243664));
#137898=CARTESIAN_POINT('Ctrl Pts',(4.51563262389453,5.36626455692521,93.5038385825398));
#137899=CARTESIAN_POINT('Ctrl Pts',(4.64559057444722,5.25129648535552,93.4959893407132));
#137900=CARTESIAN_POINT('Ctrl Pts',(4.77559231037527,5.13628967879387,93.4881374543235));
#137901=CARTESIAN_POINT('Ctrl Pts',(4.90129762168367,5.01647234001401,93.4802855679338));
#137902=CARTESIAN_POINT('Ctrl Pts',(5.02232871476421,4.89222248506289,93.4724336815441));
#137903=CARTESIAN_POINT('Ctrl Pts',(5.11120034254362,4.80098736043657,93.4666681389316));
#137904=CARTESIAN_POINT('Ctrl Pts',(5.19755245282571,4.70736313794788,93.4609025963191));
#137905=CARTESIAN_POINT('Ctrl Pts',(5.2812488557258,4.61151136682921,93.4551370537066));
#137906=CARTESIAN_POINT('Ctrl Pts',(5.42169490992746,4.45066809787859,93.4454622327801));
#137907=CARTESIAN_POINT('Ctrl Pts',(5.55459064656223,4.28363423164376,93.4357874118535));
#137908=CARTESIAN_POINT('Ctrl Pts',(5.67948977168029,4.11108531848695,93.4261125909269));
#137909=CARTESIAN_POINT('Ctrl Pts',(5.80493927127263,3.93777605959292,93.4163951374));
#137910=CARTESIAN_POINT('Ctrl Pts',(5.92232155496781,3.75890311672121,93.4066776838731));
#137911=CARTESIAN_POINT('Ctrl Pts',(6.03123283846315,3.57517230504261,93.3969602303463));
#137912=CARTESIAN_POINT('Ctrl Pts',(6.14059089548186,3.39068779678229,93.3872029140906));
#137913=CARTESIAN_POINT('Ctrl Pts',(6.24140831485485,3.20130553418335,93.377445597835));
#137914=CARTESIAN_POINT('Ctrl Pts',(6.33332481320793,3.0077605245273,93.3676882815794));
#137915=CARTESIAN_POINT('Ctrl Pts',(6.420722928028,2.82372970003056,93.3584106104134));
#137916=CARTESIAN_POINT('Ctrl Pts',(6.50007406274316,2.63593551048871,93.3491329392475));
#137917=CARTESIAN_POINT('Ctrl Pts',(6.57110895151818,2.44502632087624,93.3398552680815));
#137918=CARTESIAN_POINT('Origin',(0.,0.,50.));
#137919=CARTESIAN_POINT('',(6.57110895151809,2.44502632087648,91.3398522865014));
#137920=CARTESIAN_POINT('',(6.57110895151815,2.44502632087634,91.8867110819877));
#137921=CARTESIAN_POINT('',(6.57110895151814,2.44502632087636,50.));
#137922=CARTESIAN_POINT('',(7.01124988024546,-0.00129586190521006,93.7735343569429));
#137923=CARTESIAN_POINT('Ctrl Pts',(6.57110895151815,2.44502632087633,91.8867110819877));
#137924=CARTESIAN_POINT('Ctrl Pts',(6.49658038200761,2.64532492137524,91.8964163541283));
#137925=CARTESIAN_POINT('Ctrl Pts',(6.41296961192863,2.84199954216427,91.906121626269));
#137926=CARTESIAN_POINT('Ctrl Pts',(6.32064029350384,3.03432576409253,91.9158268984097));
#137927=CARTESIAN_POINT('Ctrl Pts',(6.22784560331244,3.22762137684042,91.9255810884858));
#137928=CARTESIAN_POINT('Ctrl Pts',(6.12624429569234,3.41652461670562,91.935335278562));
#137929=CARTESIAN_POINT('Ctrl Pts',(6.01624928643395,3.60032930243651,91.9450894686381));
#137930=CARTESIAN_POINT('Ctrl Pts',(5.90613302167974,3.78433660943589,91.9548544114672));
#137931=CARTESIAN_POINT('Ctrl Pts',(5.78760457649126,3.96323409270066,91.9646193542962));
#137932=CARTESIAN_POINT('Ctrl Pts',(5.66112132326098,4.13634282015162,91.9743842971252));
#137933=CARTESIAN_POINT('Ctrl Pts',(5.53479698692768,4.30923404922944,91.9841369710224));
#137934=CARTESIAN_POINT('Ctrl Pts',(5.40053784331265,4.47635103032932,91.9938896449196));
#137935=CARTESIAN_POINT('Ctrl Pts',(5.25884201864718,4.63704724856356,92.0036423188168));
#137936=CARTESIAN_POINT('Ctrl Pts',(5.1862496782191,4.71937370106917,92.0086387216769));
#137937=CARTESIAN_POINT('Ctrl Pts',(5.11170616989284,4.80001542755109,92.013635124537));
#137938=CARTESIAN_POINT('Ctrl Pts',(5.03528278304015,4.87888858832823,92.0186315273972));
#137939=CARTESIAN_POINT('Ctrl Pts',(4.91241187589721,5.00569815818672,92.0266645730022));
#137940=CARTESIAN_POINT('Ctrl Pts',(4.78461915748322,5.12799552921085,92.0346976186072));
#137941=CARTESIAN_POINT('Ctrl Pts',(4.6522770315614,5.24537367440169,92.0427306642123));
#137942=CARTESIAN_POINT('Ctrl Pts',(4.52001998025353,5.36267636440152,92.0507585458663));
#137943=CARTESIAN_POINT('Ctrl Pts',(4.38321961589444,5.4750658809183,92.0587864275203));
#137944=CARTESIAN_POINT('Ctrl Pts',(4.24228557003029,5.58217159399573,92.0668143091743));
#137945=CARTESIAN_POINT('Ctrl Pts',(4.10141515727746,5.68922894778763,92.0748385661606));
#137946=CARTESIAN_POINT('Ctrl Pts',(3.95641507047926,5.79100702698233,92.0828628231469));
#137947=CARTESIAN_POINT('Ctrl Pts',(3.80772838995929,5.887175135054,92.0908870801332));
#137948=CARTESIAN_POINT('Ctrl Pts',(3.65905968717411,5.98333161542145,92.098910366905));
#137949=CARTESIAN_POINT('Ctrl Pts',(3.50670558195138,6.07387927029186,92.1069336536769));
#137950=CARTESIAN_POINT('Ctrl Pts',(3.35113868181342,6.15853035210137,92.1149569404488));
#137951=CARTESIAN_POINT('Ctrl Pts',(3.19558452899533,6.24317449750979,92.1229795697838));
#137952=CARTESIAN_POINT('Ctrl Pts',(3.03681842962385,6.32192286057425,92.1310021991189));
#137953=CARTESIAN_POINT('Ctrl Pts',(2.87533789366954,6.39453349039068,92.139024828454));
#137954=CARTESIAN_POINT('Ctrl Pts',(2.71379665253087,6.46717141663416,92.1470504737265));
#137955=CARTESIAN_POINT('Ctrl Pts',(2.54953927210264,6.53366685261774,92.155076118999));
#137956=CARTESIAN_POINT('Ctrl Pts',(2.38308390612597,6.59382572251219,92.1631017642715));
#137957=CARTESIAN_POINT('Ctrl Pts',(2.2849316798991,6.62929905779812,92.1678341737422));
#137958=CARTESIAN_POINT('Ctrl Pts',(2.18601556914653,6.66257009134217,92.172566583213));
#137959=CARTESIAN_POINT('Ctrl Pts',(2.08644434055908,6.69360714235972,92.1772989926837));
#137960=CARTESIAN_POINT('Ctrl Pts',(1.90276165401402,6.75086232534996,92.1860290414915));
#137961=CARTESIAN_POINT('Ctrl Pts',(1.71675704446937,6.80054131086434,92.1947590902993));
#137962=CARTESIAN_POINT('Ctrl Pts',(1.52905784930129,6.84248556125551,92.203489139107));
#137963=CARTESIAN_POINT('Ctrl Pts',(1.34130438068395,6.8844419398774,92.2122217122189));
#137964=CARTESIAN_POINT('Ctrl Pts',(1.15185561574201,6.91865905944214,92.2209542853308));
#137965=CARTESIAN_POINT('Ctrl Pts',(0.961349496006262,6.94502942463374,
92.2296868584428));
#137966=CARTESIAN_POINT('Ctrl Pts',(0.768136931837252,6.97177442308215,
92.2385434917367));
#137967=CARTESIAN_POINT('Ctrl Pts',(0.573837028173539,6.99044797678191,
92.2474001250306));
#137968=CARTESIAN_POINT('Ctrl Pts',(0.379121580823421,7.00099231462612,
92.2562567583246));
#137969=CARTESIAN_POINT('Ctrl Pts',(0.187011414307042,7.01139556987177,
92.2649948904041));
#137970=CARTESIAN_POINT('Ctrl Pts',(-0.00550296645281556,7.01388580322916,
92.2737330224836));
#137971=CARTESIAN_POINT('Ctrl Pts',(-0.197774497688282,7.00846001704827,
92.2824711545632));
#137972=CARTESIAN_POINT('Ctrl Pts',(-0.393957232669249,7.00292385906611,
92.2913870384643));
#137973=CARTESIAN_POINT('Ctrl Pts',(-0.589886835965058,6.98914617974315,
92.3003029223654));
#137974=CARTESIAN_POINT('Ctrl Pts',(-0.784878401697783,6.96717966303786,
92.3092188062666));
#137975=CARTESIAN_POINT('Ctrl Pts',(-0.979869967430377,6.94521314633259,
92.3181346901677));
#137976=CARTESIAN_POINT('Ctrl Pts',(-1.1739231957695,6.91505783214349,92.3270505740688));
#137977=CARTESIAN_POINT('Ctrl Pts',(-1.36636015085261,6.87682241305256,
92.33596645797));
#137978=CARTESIAN_POINT('Ctrl Pts',(-1.55501567164262,6.83933832950889,
92.3447071425227));
#137979=CARTESIAN_POINT('Ctrl Pts',(-1.74213788700856,6.79408476441352,
92.3534478270754));
#137980=CARTESIAN_POINT('Ctrl Pts',(-1.9270972911706,6.74121076609113,92.3621885116282));
#137981=CARTESIAN_POINT('Ctrl Pts',(-2.11202341806955,6.68834628067759,
92.3709276235869));
#137982=CARTESIAN_POINT('Ctrl Pts',(-2.29478724772302,6.62786417534074,
92.3796667355455));
#137983=CARTESIAN_POINT('Ctrl Pts',(-2.47477335421947,6.55996367427026,
92.3884058475042));
#137984=CARTESIAN_POINT('Ctrl Pts',(-2.65709143800249,6.49118342514963,
92.3972581871503));
#137985=CARTESIAN_POINT('Ctrl Pts',(-2.83655904351329,6.41479128797725,
92.4061105267963));
#137986=CARTESIAN_POINT('Ctrl Pts',(-3.01255500788337,6.33104563930611,
92.4149628664423));
#137987=CARTESIAN_POINT('Ctrl Pts',(-3.18621080600325,6.24841353173985,
92.423697499148));
#137988=CARTESIAN_POINT('Ctrl Pts',(-3.35648646468692,6.15862238644116,
92.4324321318538));
#137989=CARTESIAN_POINT('Ctrl Pts',(-3.52280689856363,6.0619681719663,92.4411667645595));
#137990=CARTESIAN_POINT('Ctrl Pts',(-3.69248930598494,5.96336020530079,
92.4500779576757));
#137991=CARTESIAN_POINT('Ctrl Pts',(-3.85805462312663,5.85760888369109,
92.4589891507919));
#137992=CARTESIAN_POINT('Ctrl Pts',(-4.01891922819944,5.74507744070599,
92.4679003439081));
#137993=CARTESIAN_POINT('Ctrl Pts',(-4.17978383327213,5.63254599772096,
92.4768115370242));
#137994=CARTESIAN_POINT('Ctrl Pts',(-4.33594747016542,5.51323459607686,
92.4857227301405));
#137995=CARTESIAN_POINT('Ctrl Pts',(-4.48685773943029,5.38755363672739,
92.4946339232566));
#137996=CARTESIAN_POINT('Ctrl Pts',(-4.6227716646709,5.27436191958049,92.50265958805));
#137997=CARTESIAN_POINT('Ctrl Pts',(-4.75448655588055,5.15595124616417,
92.5106852528434));
#137998=CARTESIAN_POINT('Ctrl Pts',(-4.8815779151895,5.03267559260819,92.5187109176367));
#137999=CARTESIAN_POINT('Ctrl Pts',(-5.00862893881793,4.9094390637213,92.5267340352809));
#138000=CARTESIAN_POINT('Ctrl Pts',(-5.13105908918112,4.78134088362524,
92.5347571529251));
#138001=CARTESIAN_POINT('Ctrl Pts',(-5.24847882071841,4.64877366957892,
92.5427802705693));
#138002=CARTESIAN_POINT('Ctrl Pts',(-5.36588374459979,4.51622317341866,
92.5508023764281));
#138003=CARTESIAN_POINT('Ctrl Pts',(-5.47827926570231,4.37920504062483,
92.558824482287));
#138004=CARTESIAN_POINT('Ctrl Pts',(-5.58531445970553,4.23814687672624,
92.5668465881458));
#138005=CARTESIAN_POINT('Ctrl Pts',(-5.69238942835092,4.09703629513413,
92.5748716750465));
#138006=CARTESIAN_POINT('Ctrl Pts',(-5.7940998664976,3.95188297381343,92.5828967619471));
#138007=CARTESIAN_POINT('Ctrl Pts',(-5.89013647042712,3.80314592439527,
92.5909218488478));
#138008=CARTESIAN_POINT('Ctrl Pts',(-5.98619198828606,3.6543795819582,92.5989485162492));
#138009=CARTESIAN_POINT('Ctrl Pts',(-6.07657125438079,3.50202841808603,
92.6069751836506));
#138010=CARTESIAN_POINT('Ctrl Pts',(-6.1610098145062,3.34657804750737,92.6150018510521));
#138011=CARTESIAN_POINT('Ctrl Pts',(-6.2455161616141,3.1910028819117,92.6230349622342));
#138012=CARTESIAN_POINT('Ctrl Pts',(-6.32407211074119,3.03232386687623,
92.6310680734163));
#138013=CARTESIAN_POINT('Ctrl Pts',(-6.39646017369505,2.87104925224788,
92.6391011845984));
#138014=CARTESIAN_POINT('Ctrl Pts',(-6.43911385351985,2.77602038290777,
92.6438345859132));
#138015=CARTESIAN_POINT('Ctrl Pts',(-6.47962695837723,2.68009070374381,
92.6485679872279));
#138016=CARTESIAN_POINT('Ctrl Pts',(-6.51796300787231,2.58336694848179,
92.6533013885427));
#138017=CARTESIAN_POINT('Ctrl Pts',(-6.59693645836791,2.38411301390743,
92.6630523420012));
#138018=CARTESIAN_POINT('Ctrl Pts',(-6.66671560835843,2.18137117766134,
92.6728032954596));
#138019=CARTESIAN_POINT('Ctrl Pts',(-6.72706144207604,1.97592280138518,
92.6825542489181));
#138020=CARTESIAN_POINT('Ctrl Pts',(-6.78749421531238,1.77017843809784,
92.6923192504583));
#138021=CARTESIAN_POINT('Ctrl Pts',(-6.83846647645742,1.56171977214095,
92.7020842519984));
#138022=CARTESIAN_POINT('Ctrl Pts',(-6.87978909168864,1.35134326371283,
92.7118492535385));
#138023=CARTESIAN_POINT('Ctrl Pts',(-6.92104283065779,1.1413174094591,92.7215979788386));
#138024=CARTESIAN_POINT('Ctrl Pts',(-6.95267906172259,0.929380138731923,
92.7313467041387));
#138025=CARTESIAN_POINT('Ctrl Pts',(-6.9745602529191,0.716335006055907,
92.7410954294388));
#138026=CARTESIAN_POINT('Ctrl Pts',(-6.99638138871114,0.503874599846359,
92.7508173982596));
#138027=CARTESIAN_POINT('Ctrl Pts',(-7.00850093009097,0.290312441578205,
92.7605393670803));
#138028=CARTESIAN_POINT('Ctrl Pts',(-7.01083312098405,0.0764559494937864,
92.770261335901));
#138029=CARTESIAN_POINT('Ctrl Pts',(-7.01314988037477,-0.135985509638587,
92.7799189769751));
#138030=CARTESIAN_POINT('Ctrl Pts',(-7.00580835251308,-0.348717374046775,
92.7895766180492));
#138031=CARTESIAN_POINT('Ctrl Pts',(-6.98877490237346,-0.560938433747238,
92.7992342591232));
#138032=CARTESIAN_POINT('Ctrl Pts',(-6.98128811609675,-0.654216877302292,
92.8034791240253));
#138033=CARTESIAN_POINT('Ctrl Pts',(-6.97192960369455,-0.747396515695329,
92.8077239889274));
#138034=CARTESIAN_POINT('Ctrl Pts',(-6.96069965522477,-0.840408753080196,
92.8119688538295));
#138035=CARTESIAN_POINT('Ctrl Pts',(-6.93992730107195,-1.01245612628972,
92.8198207008182));
#138036=CARTESIAN_POINT('Ctrl Pts',(-6.91275659676443,-1.18385961718799,
92.827672547807));
#138037=CARTESIAN_POINT('Ctrl Pts',(-6.87924919440198,-1.35408902359475,
92.8355243947958));
#138038=CARTESIAN_POINT('Ctrl Pts',(-6.84575129446743,-1.52427015432067,
92.8433740150644));
#138039=CARTESIAN_POINT('Ctrl Pts',(-6.80592034469012,-1.69327748895823,
92.8512236353329));
#138040=CARTESIAN_POINT('Ctrl Pts',(-6.75986945775756,-1.86058901334403,
92.8590732556015));
#138041=CARTESIAN_POINT('Ctrl Pts',(-6.71382224739865,-2.02788718004698,
92.8669222491784));
#138042=CARTESIAN_POINT('Ctrl Pts',(-6.66155619039601,-2.19348943843175,
92.8747712427553));
#138043=CARTESIAN_POINT('Ctrl Pts',(-6.60323474590385,-2.3568872380723,
92.8826202363322));
#138044=CARTESIAN_POINT('Ctrl Pts',(-6.54488377497063,-2.52036776123838,
92.8904732036249));
#138045=CARTESIAN_POINT('Ctrl Pts',(-6.4804714195939,-2.68164123599705,
92.8983261709177));
#138046=CARTESIAN_POINT('Ctrl Pts',(-6.41021006923355,-2.84021714500789,
92.9061791382104));
#138047=CARTESIAN_POINT('Ctrl Pts',(-6.33993087485026,-2.99883332697316,
92.914034099893));
#138048=CARTESIAN_POINT('Ctrl Pts',(-6.2637998935171,-3.15475023550444,
92.9218890615757));
#138049=CARTESIAN_POINT('Ctrl Pts',(-6.18207600022578,-3.30750100376892,
92.9297440232583));
#138050=CARTESIAN_POINT('Ctrl Pts',(-6.10027098913611,-3.46040338994489,
92.9376067816473));
#138051=CARTESIAN_POINT('Ctrl Pts',(-6.01286217069728,-3.61013302986991,
92.9454695400363));
#138052=CARTESIAN_POINT('Ctrl Pts',(-5.92015266229698,-3.75625065958038,
92.9533322984252));
#138053=CARTESIAN_POINT('Ctrl Pts',(-5.85214229527367,-3.86344045916682,
92.959100305322));
#138054=CARTESIAN_POINT('Ctrl Pts',(-5.78128029462328,-3.96868704918374,
92.9648683122188));
#138055=CARTESIAN_POINT('Ctrl Pts',(-5.70770009220849,-4.0718283632667,
92.9706363191156));
#138056=CARTESIAN_POINT('Ctrl Pts',(-5.60082438494211,-4.22164177134705,
92.9790143854484));
#138057=CARTESIAN_POINT('Ctrl Pts',(-5.48797582339854,-4.36734428812502,
92.9873924517812));
#138058=CARTESIAN_POINT('Ctrl Pts',(-5.36949712189468,-4.50845064522888,
92.995770518114));
#138059=CARTESIAN_POINT('Ctrl Pts',(-5.25109943473359,-4.64946051546518,
93.0041428556236));
#138060=CARTESIAN_POINT('Ctrl Pts',(-5.1270794937273,-4.78588024089271,
93.0125151931331));
#138061=CARTESIAN_POINT('Ctrl Pts',(-4.99782144854968,-4.91725607741928,
93.0208875306427));
#138062=CARTESIAN_POINT('Ctrl Pts',(-4.86863283272206,-5.04856134705058,
93.0292553710554));
#138063=CARTESIAN_POINT('Ctrl Pts',(-4.73421195277145,-5.17482789599279,
93.0376232114681));
#138064=CARTESIAN_POINT('Ctrl Pts',(-4.594981422085,-5.29563709983924,93.0459910518808));
#138065=CARTESIAN_POINT('Ctrl Pts',(-4.4558052810778,-5.4163991102015,93.0543556234403));
#138066=CARTESIAN_POINT('Ctrl Pts',(-4.31182348397202,-5.53170781163574,
93.0627201949999));
#138067=CARTESIAN_POINT('Ctrl Pts',(-4.16349382203865,-5.6411830103575,
93.0710847665595));
#138068=CARTESIAN_POINT('Ctrl Pts',(-4.01520039242536,-5.7506314676953,
93.0794472949145));
#138069=CARTESIAN_POINT('Ctrl Pts',(-3.86256148044469,-5.85424906933691,
93.0878098232696));
#138070=CARTESIAN_POINT('Ctrl Pts',(-3.70606648252838,-5.95169705122663,
93.0961723516246));
#138071=CARTESIAN_POINT('Ctrl Pts',(-3.54955899581629,-6.04915280977349,
93.1045355473359));
#138072=CARTESIAN_POINT('Ctrl Pts',(-3.38919508417897,-6.14043778605298,
93.1128987430472));
#138073=CARTESIAN_POINT('Ctrl Pts',(-3.2254921973847,-6.22525715509893,
93.1212619387584));
#138074=CARTESIAN_POINT('Ctrl Pts',(-3.06177814637423,-6.3100823086597,
93.1296257048233));
#138075=CARTESIAN_POINT('Ctrl Pts',(-2.89472495800528,-6.38844082427534,
93.1379894708881));
#138076=CARTESIAN_POINT('Ctrl Pts',(-2.72487385034963,-6.46008429218852,
93.146353236953));
#138077=CARTESIAN_POINT('Ctrl Pts',(-2.55498851402849,-6.53174219780734,
93.1547186884972));
#138078=CARTESIAN_POINT('Ctrl Pts',(-2.38230443705217,-6.59668222958763,
93.1630841400415));
#138079=CARTESIAN_POINT('Ctrl Pts',(-2.20738233519697,-6.65470433518728,
93.1714495915858));
#138080=CARTESIAN_POINT('Ctrl Pts',(-2.03240165225578,-6.71274587228199,
93.1798178447042));
#138081=CARTESIAN_POINT('Ctrl Pts',(-1.85518176183064,-6.76386475995934,
93.1881860978226));
#138082=CARTESIAN_POINT('Ctrl Pts',(-1.67629844705204,-6.80791084539971,
93.196554350941));
#138083=CARTESIAN_POINT('Ctrl Pts',(-1.4972492818744,-6.8519977678564,93.2049303626261));
#138084=CARTESIAN_POINT('Ctrl Pts',(-1.31653393008176,-6.8889987055489,
93.2133063743111));
#138085=CARTESIAN_POINT('Ctrl Pts',(-1.1347394983527,-6.91881440951976,
93.2216823859962));
#138086=CARTESIAN_POINT('Ctrl Pts',(-0.952855912361967,-6.94864473548453,
93.2300625053821));
#138087=CARTESIAN_POINT('Ctrl Pts',(-0.76989251641903,-6.97128275400893,
93.238442624768));
#138088=CARTESIAN_POINT('Ctrl Pts',(-0.58644210653064,-6.98668105885677,
93.2468227441539));
#138089=CARTESIAN_POINT('Ctrl Pts',(-0.402782081247787,-7.00209695822372,
93.2552124388906));
#138090=CARTESIAN_POINT('Ctrl Pts',(-0.218634258294711,-7.01025659315699,
93.2636021336272));
#138091=CARTESIAN_POINT('Ctrl Pts',(-0.0345933559949973,-7.01116465804513,
93.2719918283639));
#138092=CARTESIAN_POINT('Ctrl Pts',(0.0822510668802292,-7.01174117292014,
93.2773183021388));
#138093=CARTESIAN_POINT('Ctrl Pts',(0.199052410905949,-7.00939580229311,
93.2826447759137));
#138094=CARTESIAN_POINT('Ctrl Pts',(0.315659425914194,-7.00414061033411,
93.2879712496886));
#138095=CARTESIAN_POINT('Ctrl Pts',(0.499142634924546,-6.99587147245649,
93.2963525507695));
#138096=CARTESIAN_POINT('Ctrl Pts',(0.682514584854368,-6.9803784966304,
93.3047338518504));
#138097=CARTESIAN_POINT('Ctrl Pts',(0.865182576579053,-6.95766380846934,
93.3131151529312));
#138098=CARTESIAN_POINT('Ctrl Pts',(1.04761906322595,-6.93497790786761,
93.3214858319335));
#138099=CARTESIAN_POINT('Ctrl Pts',(1.22935304714765,-6.90508857495471,
93.3298565109358));
#138100=CARTESIAN_POINT('Ctrl Pts',(1.40979338409746,-6.86804988163707,
93.3382271899382));
#138101=CARTESIAN_POINT('Ctrl Pts',(1.59002895207705,-6.83105322091158,
93.3465883696492));
#138102=CARTESIAN_POINT('Ctrl Pts',(1.76897348009913,-6.78692343596931,
93.3549495493602));
#138103=CARTESIAN_POINT('Ctrl Pts',(1.94604204955618,-6.73576624474597,
93.3633107290713));
#138104=CARTESIAN_POINT('Ctrl Pts',(2.12288085134561,-6.68467543610281,
93.3716610591506));
#138105=CARTESIAN_POINT('Ctrl Pts',(2.29784823671038,-6.62657550030675,
93.3800113892299));
#138106=CARTESIAN_POINT('Ctrl Pts',(2.47037064399503,-6.56162292758336,
93.3883617193093));
#138107=CARTESIAN_POINT('Ctrl Pts',(2.64276030541053,-6.49672033205339,
93.3967056242996));
#138108=CARTESIAN_POINT('Ctrl Pts',(2.81270843243221,-6.42497572208659,
93.40504952929));
#138109=CARTESIAN_POINT('Ctrl Pts',(2.9796566649287,-6.34659536457509,93.4133934342803));
#138110=CARTESIAN_POINT('Ctrl Pts',(3.14647080324539,-6.26827796280499,
93.4217306373782));
#138111=CARTESIAN_POINT('Ctrl Pts',(3.31028955678935,-6.18333558203157,
93.4300678404761));
#138112=CARTESIAN_POINT('Ctrl Pts',(3.47057445585026,-6.09202261231027,
93.438405043574));
#138113=CARTESIAN_POINT('Ctrl Pts',(3.5233392809322,-6.06196293168356,93.4411496007077));
#138114=CARTESIAN_POINT('Ctrl Pts',(3.57572131606691,-6.03121326287645,
93.4438941578413));
#138115=CARTESIAN_POINT('Ctrl Pts',(3.6277018781199,-5.99978379993691,93.446638714975));
#138116=CARTESIAN_POINT('Ctrl Pts',(3.78562535409396,-5.90429714416836,
93.4549770242474));
#138117=CARTESIAN_POINT('Ctrl Pts',(3.93971164680622,-5.80261084754877,
93.4633153335199));
#138118=CARTESIAN_POINT('Ctrl Pts',(4.08947460582195,-5.69507014977317,
93.4716536427924));
#138119=CARTESIAN_POINT('Ctrl Pts',(4.23933179035607,-5.58746179122176,
93.479997198232));
#138120=CARTESIAN_POINT('Ctrl Pts',(4.38485994949817,-5.4739918756634,93.4883407536717));
#138121=CARTESIAN_POINT('Ctrl Pts',(4.52560533671168,-5.35504648895103,
93.4966843091113));
#138122=CARTESIAN_POINT('Ctrl Pts',(4.66645780220064,-5.23601060927733,
93.5050342122795));
#138123=CARTESIAN_POINT('Ctrl Pts',(4.80251998776185,-5.11149116047647,
93.5133841154478));
#138124=CARTESIAN_POINT('Ctrl Pts',(4.93337406187235,-4.98191197515021,
93.5217340186161));
#138125=CARTESIAN_POINT('Ctrl Pts',(5.06442440724541,-4.85213843079863,
93.5300964460106));
#138126=CARTESIAN_POINT('Ctrl Pts',(5.19025079776647,-4.71729021501269,
93.5384588734052));
#138127=CARTESIAN_POINT('Ctrl Pts',(5.31047385128581,-4.57782634416266,
93.5468213007998));
#138128=CARTESIAN_POINT('Ctrl Pts',(5.43079971182085,-4.43824321278862,
93.5551908792039));
#138129=CARTESIAN_POINT('Ctrl Pts',(5.5455124713578,-4.29403680684988,93.5635604576081));
#138130=CARTESIAN_POINT('Ctrl Pts',(5.65427503039319,-4.14569661735782,
93.5719300360122));
#138131=CARTESIAN_POINT('Ctrl Pts',(5.76320534241099,-3.99712763121534,
93.5803125234703));
#138132=CARTESIAN_POINT('Ctrl Pts',(5.86616693181994,-3.8444123918016,93.5886950109283));
#138133=CARTESIAN_POINT('Ctrl Pts',(5.96286699487306,-3.6880677547943,93.5970774983864));
#138134=CARTESIAN_POINT('Ctrl Pts',(5.99450891739913,-3.63690910261397,
93.5998203923447));
#138135=CARTESIAN_POINT('Ctrl Pts',(6.02548078590497,-3.58536202772217,
93.6025632863031));
#138136=CARTESIAN_POINT('Ctrl Pts',(6.05577344516353,-3.53344513801364,
93.6053061802615));
#138137=CARTESIAN_POINT('Ctrl Pts',(6.15135272838851,-3.36963716515603,
93.6139605488419));
#138138=CARTESIAN_POINT('Ctrl Pts',(6.2403469671373,-3.20183720168851,93.6226149174223));
#138139=CARTESIAN_POINT('Ctrl Pts',(6.32243412465044,-3.03058629673461,
93.6312692860027));
#138140=CARTESIAN_POINT('Ctrl Pts',(6.40442935905294,-2.85952716253222,
93.6399139632196));
#138141=CARTESIAN_POINT('Ctrl Pts',(6.4795328162126,-2.68502505664373,93.6485586404365));
#138142=CARTESIAN_POINT('Ctrl Pts',(6.54746804963009,-2.50764604790492,
93.6572033176535));
#138143=CARTESIAN_POINT('Ctrl Pts',(6.61532939781575,-2.33045995363071,
93.665838593063));
#138144=CARTESIAN_POINT('Ctrl Pts',(6.67603797031742,-2.15040346857582,
93.6744738684725));
#138145=CARTESIAN_POINT('Ctrl Pts',(6.72936485001155,-1.9680638399018,93.683109143882));
#138146=CARTESIAN_POINT('Ctrl Pts',(6.78261394694754,-1.7859901723963,93.6917318238511));
#138147=CARTESIAN_POINT('Ctrl Pts',(6.82850275937022,-1.60164028610003,
93.7003545038201));
#138148=CARTESIAN_POINT('Ctrl Pts',(6.86685172246869,-1.41561788068984,
93.7089771837892));
#138149=CARTESIAN_POINT('Ctrl Pts',(6.90516539300715,-1.22976667174432,
93.7175919283038));
#138150=CARTESIAN_POINT('Ctrl Pts',(6.93595299467261,-1.04224629711538,
93.7262066728184));
#138151=CARTESIAN_POINT('Ctrl Pts',(6.95908526839225,-0.853673702152075,
93.734821417333));
#138152=CARTESIAN_POINT('Ctrl Pts',(6.98218948500649,-0.665329826649574,
93.7434257130349));
#138153=CARTESIAN_POINT('Ctrl Pts',(6.99765686810607,-0.475936565373441,
93.7520300087368));
#138154=CARTESIAN_POINT('Ctrl Pts',(7.00540950305875,-0.286119305455343,
93.7606343044387));
#138155=CARTESIAN_POINT('Ctrl Pts',(7.00928390103963,-0.191257672855264,
93.7649343219293));
#138156=CARTESIAN_POINT('Ctrl Pts',(7.01123232278772,-0.0962902859571281,
93.7692343394198));
#138157=CARTESIAN_POINT('Ctrl Pts',(7.01124988024532,-0.0012958626227105,
93.7735343569104));
#138158=CARTESIAN_POINT('Ctrl Pts',(7.01124988024546,-0.00129586190520921,
93.7735343569429));
#138159=CARTESIAN_POINT('Ctrl Pts',(7.01128650959441,0.196886920880268,
93.7825052986297));
#138160=CARTESIAN_POINT('Ctrl Pts',(7.00291594834133,0.394899238328634,
93.7914762403165));
#138161=CARTESIAN_POINT('Ctrl Pts',(6.98620743083789,0.59205767945829,93.8004471820033));
#138162=CARTESIAN_POINT('Ctrl Pts',(6.9694530897394,0.789756833344971,93.8094427267586));
#138163=CARTESIAN_POINT('Ctrl Pts',(6.9443150481448,0.986597201599815,93.8184382715138));
#138164=CARTESIAN_POINT('Ctrl Pts',(6.91091440251724,1.18190045417529,93.827433816269));
#138165=CARTESIAN_POINT('Ctrl Pts',(6.87747032770891,1.37745764975403,93.836441057479));
#138166=CARTESIAN_POINT('Ctrl Pts',(6.83574222156793,1.5714735175026,93.8454482986889));
#138167=CARTESIAN_POINT('Ctrl Pts',(6.78590204018911,1.7632810506148,93.8544555398989));
#138168=CARTESIAN_POINT('Ctrl Pts',(6.7359867488886,1.9553776406364,93.8634763551602));
#138169=CARTESIAN_POINT('Ctrl Pts',(6.6779349940371,2.14525902654792,93.8724971704215));
#138170=CARTESIAN_POINT('Ctrl Pts',(6.61196886361562,2.33227234882154,93.8815179856828));
#138171=CARTESIAN_POINT('Ctrl Pts',(6.59866972731505,2.36997526768381,93.8833366318719));
#138172=CARTESIAN_POINT('Ctrl Pts',(6.58504907073195,2.40756167627561,93.8851552780611));
#138173=CARTESIAN_POINT('Ctrl Pts',(6.5711089515182,2.44502632087621,93.8869739242502));
#138174=CARTESIAN_POINT('',(7.01125,-3.18920671121825E-12,93.2264656430894));
#138175=CARTESIAN_POINT('Ctrl Pts',(6.57110895151818,2.44502632087624,93.3398552680815));
#138176=CARTESIAN_POINT('Ctrl Pts',(6.64577834864258,2.24434924036419,93.3301029037909));
#138177=CARTESIAN_POINT('Ctrl Pts',(6.71125832242542,2.04023012470171,93.3203505395003));
#138178=CARTESIAN_POINT('Ctrl Pts',(6.76728319995022,1.83344066011736,93.3105981752096));
#138179=CARTESIAN_POINT('Ctrl Pts',(6.79433825794756,1.73357964828215,93.3058886462798));
#138180=CARTESIAN_POINT('Ctrl Pts',(6.81918907502626,1.63309618322025,93.3011791173499));
#138181=CARTESIAN_POINT('Ctrl Pts',(6.84180979817924,1.53207873428182,93.2964695884201));
#138182=CARTESIAN_POINT('Ctrl Pts',(6.8809812374534,1.35715068976432,93.2883142776796));
#138183=CARTESIAN_POINT('Ctrl Pts',(6.91347900255196,1.18054410538854,93.2801589669392));
#138184=CARTESIAN_POINT('Ctrl Pts',(6.93916435907465,1.00280833674639,93.2720036561988));
#138185=CARTESIAN_POINT('Ctrl Pts',(6.9648279033918,0.825223502708336,93.263855271012));
#138186=CARTESIAN_POINT('Ctrl Pts',(6.98369051606048,0.646511743539516,
93.2557068858252));
#138187=CARTESIAN_POINT('Ctrl Pts',(6.99566433661717,0.467233401933904,
93.2475585006385));
#138188=CARTESIAN_POINT('Ctrl Pts',(7.00599612160807,0.312540480804345,
93.2405275481222));
#138189=CARTESIAN_POINT('Ctrl Pts',(7.0111997408877,0.157426046800206,93.2334965956058));
#138190=CARTESIAN_POINT('Ctrl Pts',(7.01124963752017,0.00225452284965846,
93.2264656430895));
#138191=CARTESIAN_POINT('Ctrl Pts',(7.01125,-8.58630487052188E-16,93.2264656430895));
#138192=CARTESIAN_POINT('Ctrl Pts',(7.01125,-0.191009525814093,93.2177938341508));
#138193=CARTESIAN_POINT('Ctrl Pts',(7.00344006572044,-0.382018909627989,
93.209122025212));
#138194=CARTESIAN_POINT('Ctrl Pts',(6.98784625534326,-0.572390840409932,
93.2004502162732));
#138195=CARTESIAN_POINT('Ctrl Pts',(6.97225246786089,-0.762762491687998,
93.1917784200664));
#138196=CARTESIAN_POINT('Ctrl Pts',(6.9488748503355,-0.952496408756031,
93.1831066238596));
#138197=CARTESIAN_POINT('Ctrl Pts',(6.91779140296552,-1.14095953808901,
93.1744348276528));
#138198=CARTESIAN_POINT('Ctrl Pts',(6.88670800059831,-1.32942239456418,
93.165763044001));
#138199=CARTESIAN_POINT('Ctrl Pts',(6.84791883692753,-1.5166141867748,93.1570912603492));
#138200=CARTESIAN_POINT('Ctrl Pts',(6.80155333291357,-1.7019103448867,93.1484194766975));
#138201=CARTESIAN_POINT('Ctrl Pts',(6.75518789508256,-1.88720623850351,
93.139747705424));
#138202=CARTESIAN_POINT('Ctrl Pts',(6.70124620748647,-2.07060622793538,
93.1310759341505));
#138203=CARTESIAN_POINT('Ctrl Pts',(6.63990824732617,-2.25149839653282,
93.122404162877));
#138204=CARTESIAN_POINT('Ctrl Pts',(6.57857037347023,-2.43239031060956,
93.113732403805));
#138205=CARTESIAN_POINT('Ctrl Pts',(6.50983633907283,-2.61077414196143,
93.1050606447329));
#138206=CARTESIAN_POINT('Ctrl Pts',(6.43393547556373,-2.78605471209424,
93.0963888856609));
#138207=CARTESIAN_POINT('Ctrl Pts',(6.35803471730125,-2.96133503917729,
93.0877171386134));
#138208=CARTESIAN_POINT('Ctrl Pts',(6.27496726266285,-3.13351185304551,
93.0790453915659));
#138209=CARTESIAN_POINT('Ctrl Pts',(6.18501026583461,-3.30201068653941,
93.0703736445184));
#138210=CARTESIAN_POINT('Ctrl Pts',(6.09151188668885,-3.47714289831958,
93.0613605124453));
#138211=CARTESIAN_POINT('Ctrl Pts',(5.99057066119227,-3.64830137930906,
93.0523473803723));
#138212=CARTESIAN_POINT('Ctrl Pts',(5.88255038916651,-3.81486926137935,
93.0433342482993));
#138213=CARTESIAN_POINT('Ctrl Pts',(5.77621793389113,-3.97883452029231,
93.034461946415));
#138214=CARTESIAN_POINT('Ctrl Pts',(5.66302622906441,-4.13835132493652,
93.0255896445306));
#138215=CARTESIAN_POINT('Ctrl Pts',(5.54337059052969,-4.2928625715891,93.0167173426462));
#138216=CARTESIAN_POINT('Ctrl Pts',(5.42558457134711,-4.44495958001268,
93.0079836704788));
#138217=CARTESIAN_POINT('Ctrl Pts',(5.30153533575011,-4.59220608124017,
92.9992499983114));
#138218=CARTESIAN_POINT('Ctrl Pts',(5.17164269972391,-4.7341037534989,92.990516326144));
#138219=CARTESIAN_POINT('Ctrl Pts',(5.04265587431657,-4.87501189761919,
92.98184355853));
#138220=CARTESIAN_POINT('Ctrl Pts',(4.907907101642,-5.01064538261891,92.973170790916));
#138221=CARTESIAN_POINT('Ctrl Pts',(4.76784607609309,-5.14055156157233,
92.964498023302));
#138222=CARTESIAN_POINT('Ctrl Pts',(4.62778576967448,-5.27045707353458,
92.9558253002175));
#138223=CARTESIAN_POINT('Ctrl Pts',(4.48241347329876,-5.39463514506421,
92.947152577133));
#138224=CARTESIAN_POINT('Ctrl Pts',(4.33221433005583,-5.51267136340984,
92.9384798540486));
#138225=CARTESIAN_POINT('Ctrl Pts',(4.1820159457358,-5.63070698534468,92.9298071747854));
#138226=CARTESIAN_POINT('Ctrl Pts',(4.02699098676565,-5.74260064062495,
92.9211344955223));
#138227=CARTESIAN_POINT('Ctrl Pts',(3.86765680432031,-5.84797891638597,
92.9124618162592));
#138228=CARTESIAN_POINT('Ctrl Pts',(3.70832341394961,-5.95335666829543,
92.9037891801093));
#138229=CARTESIAN_POINT('Ctrl Pts',(3.54468107996629,-6.05221894875867,
92.8951165439594));
#138230=CARTESIAN_POINT('Ctrl Pts',(3.37727590612964,-6.14423583665017,
92.8864439078095));
#138231=CARTESIAN_POINT('Ctrl Pts',(3.20987155082599,-6.23625227462213,
92.8777713140647));
#138232=CARTESIAN_POINT('Ctrl Pts',(3.03870464148166,-6.32142325013675,
92.8690987203199));
#138233=CARTESIAN_POINT('Ctrl Pts',(2.86434638713045,-6.39946453518048,
92.8604261265751));
#138234=CARTESIAN_POINT('Ctrl Pts',(2.68998897107841,-6.47750544500857,
92.8517535745274));
#138235=CARTESIAN_POINT('Ctrl Pts',(2.51244050005598,-6.54841661688668,
92.8430810224797));
#138236=CARTESIAN_POINT('Ctrl Pts',(2.33229347361078,-6.61196141212671,
92.834408470432));
#138237=CARTESIAN_POINT('Ctrl Pts',(2.15214729859382,-6.67550590703519,
92.8257359593733));
#138238=CARTESIAN_POINT('Ctrl Pts',(1.96940286066775,-6.73168400046379,
92.8170634483147));
#138239=CARTESIAN_POINT('Ctrl Pts',(1.78466999315702,-6.78030822146198,
92.808390937256));
#138240=CARTESIAN_POINT('Ctrl Pts',(1.59993798367215,-6.82893221661602,
92.7997184664784));
#138241=CARTESIAN_POINT('Ctrl Pts',(1.4132178378366,-6.87000233723057,92.7910459957008));
#138242=CARTESIAN_POINT('Ctrl Pts',(1.225132650459,-6.90338153018355,92.7823735249232));
#138243=CARTESIAN_POINT('Ctrl Pts',(1.03704832132761,-6.93676057082487,
92.7737010937188));
#138244=CARTESIAN_POINT('Ctrl Pts',(0.847599242851915,-6.96244870438812,
92.7650286625143));
#138245=CARTESIAN_POINT('Ctrl Pts',(0.657417610666475,-6.98036020902114,
92.7563562313098));
#138246=CARTESIAN_POINT('Ctrl Pts',(0.467236830773526,-6.99827163338436,
92.7476838389706));
#138247=CARTESIAN_POINT('Ctrl Pts',(0.27632378658647,-7.00840647191856,
92.7390114466313));
#138248=CARTESIAN_POINT('Ctrl Pts',(0.0853155533204496,-7.0107309047532,
92.730339054292));
#138249=CARTESIAN_POINT('Ctrl Pts',(-0.105691839535918,-7.01305532736066,
92.7216667001101));
#138250=CARTESIAN_POINT('Ctrl Pts',(-0.296794136562634,-7.00756940957907,
92.7129943459281));
#138251=CARTESIAN_POINT('Ctrl Pts',(-0.487353636615438,-6.99429145770876,
92.7043219917462));
#138252=CARTESIAN_POINT('Ctrl Pts',(-0.677912313783102,-6.98101356317608,
92.6956496750137));
#138253=CARTESIAN_POINT('Ctrl Pts',(-0.867927915269078,-6.95994372163481,
92.6869773582812));
#138254=CARTESIAN_POINT('Ctrl Pts',(-1.05676637166177,-6.93115224174342,
92.6783050415487));
#138255=CARTESIAN_POINT('Ctrl Pts',(-1.24560402801049,-6.90236088383169,
92.6696327615578));
#138256=CARTESIAN_POINT('Ctrl Pts',(-1.43326426841181,-6.86584799585162,
92.660960481567));
#138257=CARTESIAN_POINT('Ctrl Pts',(-1.61912088843801,-6.82173541784814,
92.6522882015762));
#138258=CARTESIAN_POINT('Ctrl Pts',(-1.80497673621847,-6.77762302313515,
92.6436159576192));
#138259=CARTESIAN_POINT('Ctrl Pts',(-1.98902870222556,-6.72591106718967,
92.6349437136622));
#138260=CARTESIAN_POINT('Ctrl Pts',(-2.17066262759971,-6.66677210647266,
92.6262714697052));
#138261=CARTESIAN_POINT('Ctrl Pts',(-2.35229581309404,-6.60763338665627,
92.6175992610743));
#138262=CARTESIAN_POINT('Ctrl Pts',(-2.53151070755523,-6.54106781055567,
92.6089270524434));
#138263=CARTESIAN_POINT('Ctrl Pts',(-2.70770929770595,-6.46729749753456,
92.6002548438126));
#138264=CARTESIAN_POINT('Ctrl Pts',(-2.8839071844938,-6.39352747899536,
92.5915826698));
#138265=CARTESIAN_POINT('Ctrl Pts',(-3.05708852904238,-6.31255289079159,
92.5829104957875));
#138266=CARTESIAN_POINT('Ctrl Pts',(-3.22667545573632,-6.22464393084848,
92.574238321775));
#138267=CARTESIAN_POINT('Ctrl Pts',(-3.39626171929686,-6.13673531465455,
92.5655661816732));
#138268=CARTESIAN_POINT('Ctrl Pts',(-3.56225334094128,-6.04189251170875,
92.5568940415714));
#138269=CARTESIAN_POINT('Ctrl Pts',(-3.72409644021936,-5.94043199325146,
92.5482219014696));
#138270=CARTESIAN_POINT('Ctrl Pts',(-3.88593891984915,-5.83897186325582,
92.5395497945707));
#138271=CARTESIAN_POINT('Ctrl Pts',(-4.04363266822892,-5.73089421932768,
92.5308776876719));
#138272=CARTESIAN_POINT('Ctrl Pts',(-4.19665149725753,-5.61655969193475,
92.5222055807731));
#138273=CARTESIAN_POINT('Ctrl Pts',(-4.34966975290729,-5.50222559296622,
92.5135335063696));
#138274=CARTESIAN_POINT('Ctrl Pts',(-4.49801289671758,-5.38163482746752,
92.5048614319662));
#138275=CARTESIAN_POINT('Ctrl Pts',(-4.64118594512959,-5.25518977632888,
92.4961893575627));
#138276=CARTESIAN_POINT('Ctrl Pts',(-4.78435846873625,-5.12874518867858,
92.487517314947));
#138277=CARTESIAN_POINT('Ctrl Pts',(-4.92236072196935,-4.99644654635426,
92.4788452723313));
#138278=CARTESIAN_POINT('Ctrl Pts',(-5.05473222957939,-4.85873529323746,
92.4701732297156));
#138279=CARTESIAN_POINT('Ctrl Pts',(-5.18710326277656,-4.72102453367094,
92.4615012181801));
#138280=CARTESIAN_POINT('Ctrl Pts',(-5.31384339389981,-4.57790140690441,
92.4528292066446));
#138281=CARTESIAN_POINT('Ctrl Pts',(-5.4345297293063,-4.42984347170259,
92.4441571951091));
#138282=CARTESIAN_POINT('Ctrl Pts',(-5.55521564202443,-4.28178605505461,
92.4354852139461));
#138283=CARTESIAN_POINT('Ctrl Pts',(-5.66984762199887,-4.12879408471371,
92.4268132327832));
#138284=CARTESIAN_POINT('Ctrl Pts',(-5.77804317951667,-3.97137804523077,
92.4181412516203));
#138285=CARTESIAN_POINT('Ctrl Pts',(-5.88623836691936,-3.81396254423625,
92.4094693001225));
#138286=CARTESIAN_POINT('Ctrl Pts',(-5.98799701504499,-3.65212323845223,
92.4007973486246));
#138287=CARTESIAN_POINT('Ctrl Pts',(-6.08297959063156,-3.48640012942575,
92.3921253971268));
#138288=CARTESIAN_POINT('Ctrl Pts',(-6.17796184905024,-3.32067757378551,
92.3834534745866));
#138289=CARTESIAN_POINT('Ctrl Pts',(-6.26616793897712,-3.15107148727182,
92.3747815520463));
#138290=CARTESIAN_POINT('Ctrl Pts',(-6.34730354929289,-2.97814778270553,
92.366109629506));
#138291=CARTESIAN_POINT('Ctrl Pts',(-6.42843889529735,-2.80522464146391,
92.3574377352158));
#138292=CARTESIAN_POINT('Ctrl Pts',(-6.50250368714197,-2.62898416091716,
92.3487658409257));
#138293=CARTESIAN_POINT('Ctrl Pts',(-6.56925079960071,-2.45001438657929,
92.3400939466355));
#138294=CARTESIAN_POINT('Ctrl Pts',(-6.63599770006526,-2.2710451806638,
92.3314220798879));
#138295=CARTESIAN_POINT('Ctrl Pts',(-6.69542686840775,-2.08934696441046,
92.3227502131404));
#138296=CARTESIAN_POINT('Ctrl Pts',(-6.74734001400864,-1.90552598981435,
92.3140783463928));
#138297=CARTESIAN_POINT('Ctrl Pts',(-6.79925299896378,-1.72170558405405,
92.3054065064805));
#138298=CARTESIAN_POINT('Ctrl Pts',(-6.84364993053219,-1.53576270641256,
92.2967346665681));
#138299=CARTESIAN_POINT('Ctrl Pts',(-6.88038267538334,-1.34831776773313,
92.2880628266557));
#138300=CARTESIAN_POINT('Ctrl Pts',(-6.9171153095606,-1.16087339381573,
92.2793910128712));
#138301=CARTESIAN_POINT('Ctrl Pts',(-6.94618374861392,-0.97192724661815,
92.2707191990866));
#138302=CARTESIAN_POINT('Ctrl Pts',(-6.96749100433676,-0.782109753798213,
92.2620473853021));
#138303=CARTESIAN_POINT('Ctrl Pts',(-6.98879819759995,-0.592292817405416,
92.2533755969379));
#138304=CARTESIAN_POINT('Ctrl Pts',(-7.00234422137961,-0.401604822727352,
92.2447038085737));
#138305=CARTESIAN_POINT('Ctrl Pts',(-7.00808387899853,-0.210682005451052,
92.2360320202095));
#138306=CARTESIAN_POINT('Ctrl Pts',(-7.01382352026045,-0.0197597322708364,
92.2273602565584));
#138307=CARTESIAN_POINT('Ctrl Pts',(-7.01175683134601,0.171397078302522,
92.2186884929072));
#138308=CARTESIAN_POINT('Ctrl Pts',(-7.0018907077798,0.362150629996567,
92.2100167292561));
#138309=CARTESIAN_POINT('Ctrl Pts',(-6.99157808297275,0.561536923511939,
92.2009525163108));
#138310=CARTESIAN_POINT('Ctrl Pts',(-6.97274368607562,0.760482277942609,
92.1918883033654));
#138311=CARTESIAN_POINT('Ctrl Pts',(-6.94545616842847,0.958261537858469,
92.18282409042));
#138312=CARTESIAN_POINT('Ctrl Pts',(-6.9190213857078,1.14986019590195,92.1740431341292));
#138313=CARTESIAN_POINT('Ctrl Pts',(-6.88465388689334,1.34036422799403,
92.1652621778384));
#138314=CARTESIAN_POINT('Ctrl Pts',(-6.84247124235282,1.52912192452881,
92.1564812215476));
#138315=CARTESIAN_POINT('Ctrl Pts',(-6.80080846652355,1.71555332735902,
92.1478084838021));
#138316=CARTESIAN_POINT('Ctrl Pts',(-6.75152215882579,1.90028091508477,
92.1391357460566));
#138317=CARTESIAN_POINT('Ctrl Pts',(-6.69477680033991,2.08268820425202,
92.1304630083111));
#138318=CARTESIAN_POINT('Ctrl Pts',(-6.63803201373192,2.26509365512451,
92.1217903579692));
#138319=CARTESIAN_POINT('Ctrl Pts',(-6.57382841116713,2.44517858291517,
92.1131177076273));
#138320=CARTESIAN_POINT('Ctrl Pts',(-6.50238025225981,2.62234201002114,
92.1044450572853));
#138321=CARTESIAN_POINT('Ctrl Pts',(-6.43093279007748,2.79950370952224,
92.0957724915146));
#138322=CARTESIAN_POINT('Ctrl Pts',(-6.35224101919017,2.9737437018412,92.0870999257438));
#138323=CARTESIAN_POINT('Ctrl Pts',(-6.26656754386472,3.14448052636383,
92.078427359973));
#138324=CARTESIAN_POINT('Ctrl Pts',(-6.18089487601242,3.31521574169059,
92.0697548759412));
#138325=CARTESIAN_POINT('Ctrl Pts',(-6.08824076282263,3.48244760135376,
92.0610823919095));
#138326=CARTESIAN_POINT('Ctrl Pts',(-5.98891439681958,3.64561804226213,
92.0524099078777));
#138327=CARTESIAN_POINT('Ctrl Pts',(-5.8895889345435,3.80878699855434,92.043737502753));
#138328=CARTESIAN_POINT('Ctrl Pts',(-5.78359148866046,3.96789436736264,
92.0350650976284));
#138329=CARTESIAN_POINT('Ctrl Pts',(-5.67127577279352,4.12240920717792,
92.0263926925037));
#138330=CARTESIAN_POINT('Ctrl Pts',(-5.5589610421754,4.2769226915679,92.0177203634546));
#138331=CARTESIAN_POINT('Ctrl Pts',(-5.44032831952011,4.42684349778707,
92.0090480344055));
#138332=CARTESIAN_POINT('Ctrl Pts',(-5.31577347544833,4.5716713486667,92.0003757053563));
#138333=CARTESIAN_POINT('Ctrl Pts',(-5.19121968333364,4.71649797636881,
91.9917034495514));
#138334=CARTESIAN_POINT('Ctrl Pts',(-5.06074405512288,4.85623151942534,
91.9830311937464));
#138335=CARTESIAN_POINT('Ctrl Pts',(-4.92478197318928,4.99040570285121,
91.9743589379415));
#138336=CARTESIAN_POINT('Ctrl Pts',(-4.78882099517989,5.12457879686946,
91.9656867525496));
#138337=CARTESIAN_POINT('Ctrl Pts',(-4.64737385477933,5.25319242205283,
91.9570145671578));
#138338=CARTESIAN_POINT('Ctrl Pts',(-4.50091253739581,5.37581741628315,
91.948342381766));
#138339=CARTESIAN_POINT('Ctrl Pts',(-4.35445236138386,5.49844145489813,
91.9396702639564));
#138340=CARTESIAN_POINT('Ctrl Pts',(-4.20297830437918,5.61507677359995,
91.9309981461468));
#138341=CARTESIAN_POINT('Ctrl Pts',(-4.04699580206075,5.72533418593209,
91.9223260283372));
#138342=CARTESIAN_POINT('Ctrl Pts',(-3.89101446440852,5.83559077501111,
91.9136539752793));
#138343=CARTESIAN_POINT('Ctrl Pts',(-3.73052498075346,5.93946938906208,
91.9049819222213));
#138344=CARTESIAN_POINT('Ctrl Pts',(-3.56606286128534,6.03662341312272,
91.8963098691634));
#138345=CARTESIAN_POINT('Ctrl Pts',(-3.40160191612949,6.13377674347248,
91.8876378780267));
#138346=CARTESIAN_POINT('Ctrl Pts',(-3.23316863647378,6.22420543545133,
91.87896588689));
#138347=CARTESIAN_POINT('Ctrl Pts',(-3.06132503079821,6.30760775716978,
91.8702938957532));
#138348=CARTESIAN_POINT('Ctrl Pts',(-2.88948259606764,6.39100951058351,
91.8616219637076));
#138349=CARTESIAN_POINT('Ctrl Pts',(-2.71423013733803,6.46738486553202,
91.852950031662));
#138350=CARTESIAN_POINT('Ctrl Pts',(-2.53615240856791,6.53647898512764,
91.8442780996164));
#138351=CARTESIAN_POINT('Ctrl Pts',(-2.35807583511654,6.60557265645983,
91.8356062238318));
#138352=CARTESIAN_POINT('Ctrl Pts',(-2.17717429308594,6.66738508423325,
91.8269343480473));
#138353=CARTESIAN_POINT('Ctrl Pts',(-1.99405137755473,6.72171002544532,
91.8182624722627));
#138354=CARTESIAN_POINT('Ctrl Pts',(-1.81092959032606,6.77603463193701,
91.8095906499095));
#138355=CARTESIAN_POINT('Ctrl Pts',(-1.62558672926246,6.82287176341268,
91.8009188275563));
#138356=CARTESIAN_POINT('Ctrl Pts',(-1.4386412007099,6.86206514528389,91.7922470052031));
#138357=CARTESIAN_POINT('Ctrl Pts',(-1.25169676301938,6.9012582984544,91.7835752334516));
#138358=CARTESIAN_POINT('Ctrl Pts',(-1.0631499545079,6.93280773300174,91.7749034617));
#138359=CARTESIAN_POINT('Ctrl Pts',(-0.873629864328629,6.95660818378131,
91.7662316899485));
#138360=CARTESIAN_POINT('Ctrl Pts',(-0.679495509715768,6.98098810649672,
91.75734878571));
#138361=CARTESIAN_POINT('Ctrl Pts',(-0.484340182090771,6.99723686027455,
91.7484658814715));
#138362=CARTESIAN_POINT('Ctrl Pts',(-0.28884707897545,7.00529756166484,
91.7395829772331));
#138363=CARTESIAN_POINT('Ctrl Pts',(-0.0979805524009829,7.01316749698021,
91.7309102974767));
#138364=CARTESIAN_POINT('Ctrl Pts',(0.0932076478825197,7.01323255451612,
91.7222376177204));
#138365=CARTESIAN_POINT('Ctrl Pts',(0.284079486219721,7.00549251716174,
91.713564937964));
#138366=CARTESIAN_POINT('Ctrl Pts',(0.474947621911345,6.99775262995322,
91.7048924264455));
#138367=CARTESIAN_POINT('Ctrl Pts',(0.665499124046936,6.98220796234753,
91.696219914927));
#138368=CARTESIAN_POINT('Ctrl Pts',(0.8550981064148,6.95891038819339,91.6875474034084));
#138369=CARTESIAN_POINT('Ctrl Pts',(1.04469365841117,6.93561323555699,91.6788750487997));
#138370=CARTESIAN_POINT('Ctrl Pts',(1.23333644314947,6.90456349171743,91.6702026941909));
#138371=CARTESIAN_POINT('Ctrl Pts',(1.42039696672311,6.86586476850686,91.6615303395822));
#138372=CARTESIAN_POINT('Ctrl Pts',(1.60745435008797,6.82716669493668,91.6528581305574));
#138373=CARTESIAN_POINT('Ctrl Pts',(1.79292924725796,6.78081995649467,91.6441859215325));
#138374=CARTESIAN_POINT('Ctrl Pts',(1.97620275620757,6.72697920532371,91.6355137125077));
#138375=CARTESIAN_POINT('Ctrl Pts',(2.15947342778161,6.6731392876962,91.6268416377429));
#138376=CARTESIAN_POINT('Ctrl Pts',(2.34054250680113,6.61180566956913,91.6181695629782));
#138377=CARTESIAN_POINT('Ctrl Pts',(2.51880581148678,6.54318300573356,91.6094974882134));
#138378=CARTESIAN_POINT('Ctrl Pts',(2.69706658905564,6.4745613147145,91.6008255363867));
#138379=CARTESIAN_POINT('Ctrl Pts',(2.8725214068172,6.39865088680221,91.59215358456));
#138380=CARTESIAN_POINT('Ctrl Pts',(3.04458483294605,6.31570500874565,91.5834816327333));
#138381=CARTESIAN_POINT('Ctrl Pts',(3.21664604442544,6.23276019829566,91.5748097925244));
#138382=CARTESIAN_POINT('Ctrl Pts',(3.38531569578618,6.14278024223886,91.5661379523154));
#138383=CARTESIAN_POINT('Ctrl Pts',(3.5500310094209,6.04606536473516,91.5574661121065));
#138384=CARTESIAN_POINT('Ctrl Pts',(3.72225670715908,5.94494066119559,91.5483988693729));
#138385=CARTESIAN_POINT('Ctrl Pts',(3.89015872998488,5.83645264819735,91.5393316266394));
#138386=CARTESIAN_POINT('Ctrl Pts',(4.05312466659709,5.720997028449,91.5302643839058));
#138387=CARTESIAN_POINT('Ctrl Pts',(4.20899688867883,5.61056705531404,91.5215918275274));
#138388=CARTESIAN_POINT('Ctrl Pts',(4.36035338103765,5.49376336253727,91.512919271149));
#138389=CARTESIAN_POINT('Ctrl Pts',(4.50668904924943,5.37097573778501,91.5042467147705));
#138390=CARTESIAN_POINT('Ctrl Pts',(4.65301950883977,5.24819248349324,91.4955744670801));
#138391=CARTESIAN_POINT('Ctrl Pts',(4.79432928426883,5.11942590604071,91.4869022193897));
#138392=CARTESIAN_POINT('Ctrl Pts',(4.9301468417244,4.98510568408884,91.4782299716992));
#138393=CARTESIAN_POINT('Ctrl Pts',(5.0659602741979,4.85078954164274,91.4695579873979));
#138394=CARTESIAN_POINT('Ctrl Pts',(5.19628162053371,4.71092029195627,91.4608860030966));
#138395=CARTESIAN_POINT('Ctrl Pts',(5.320676040381,4.56596463365799,91.4522140187952));
#138396=CARTESIAN_POINT('Ctrl Pts',(5.44506733164305,4.42101262107094,91.4435422525989));
#138397=CARTESIAN_POINT('Ctrl Pts',(5.56353180975597,4.27097467138689,91.4348704864025));
#138398=CARTESIAN_POINT('Ctrl Pts',(5.67567421678132,4.11635138775393,91.4261987202062));
#138399=CARTESIAN_POINT('Ctrl Pts',(5.78782406006072,3.96171785092552,91.417526378978));
#138400=CARTESIAN_POINT('Ctrl Pts',(5.8936508265424,3.80249860162444,91.4088540377498));
#138401=CARTESIAN_POINT('Ctrl Pts',(5.99280137735924,3.63922494688377,91.4001816965216));
#138402=CARTESIAN_POINT('Ctrl Pts',(6.09194609290829,3.47596090122234,91.3915098656832));
#138403=CARTESIAN_POINT('Ctrl Pts',(6.18441523160457,3.30864317036824,91.3828380348449));
#138404=CARTESIAN_POINT('Ctrl Pts',(6.26990026462943,3.13783001995007,91.3741662040065));
#138405=CARTESIAN_POINT('Ctrl Pts',(6.35538670852376,2.96701405038272,91.3654942300457));
#138406=CARTESIAN_POINT('Ctrl Pts',(6.43388868897021,2.79270279979631,91.356822256085));
#138407=CARTESIAN_POINT('Ctrl Pts',(6.50514427077279,2.61547788729554,91.3481502821243));
#138408=CARTESIAN_POINT('Ctrl Pts',(6.52787183386205,2.55895052090607,91.3453842835833));
#138409=CARTESIAN_POINT('Ctrl Pts',(6.54986255129711,2.50212689664026,91.3426182850423));
#138410=CARTESIAN_POINT('Ctrl Pts',(6.5711089515181,2.44502632087648,91.3398522865014));
#138411=CARTESIAN_POINT('Origin',(0.,0.,50.));
#138412=CARTESIAN_POINT('',(6.57110895151813,2.4450263208764,89.3398405407985));
#138413=CARTESIAN_POINT('',(6.57110895151814,2.44502632087636,89.8869836046549));
#138414=CARTESIAN_POINT('',(6.57110895151814,2.44502632087636,50.));
#138415=CARTESIAN_POINT('',(7.01124941011649,-0.00287604611295131,91.7735343569377));
#138416=CARTESIAN_POINT('Ctrl Pts',(6.57110895151814,2.44502632087636,89.8869836046549));
#138417=CARTESIAN_POINT('Ctrl Pts',(6.50935320916737,2.61099742225222,89.8950062778613));
#138418=CARTESIAN_POINT('Ctrl Pts',(6.44129983113049,2.77464205694512,89.9030289510676));
#138419=CARTESIAN_POINT('Ctrl Pts',(6.36716265085894,2.93544993825598,89.911051624274));
#138420=CARTESIAN_POINT('Ctrl Pts',(6.29299667694928,3.09632027465242,89.9190774133522));
#138421=CARTESIAN_POINT('Ctrl Pts',(6.21274233312392,3.25435132291618,89.9271032024303));
#138422=CARTESIAN_POINT('Ctrl Pts',(6.12666066204817,3.40905495623222,89.9351289915085));
#138423=CARTESIAN_POINT('Ctrl Pts',(6.05220514875705,3.54286437561966,89.9420708205635));
#138424=CARTESIAN_POINT('Ctrl Pts',(5.97339090098604,3.67418472505594,89.9490126496185));
#138425=CARTESIAN_POINT('Ctrl Pts',(5.89041361735242,3.80271665773421,89.9559544786736));
#138426=CARTESIAN_POINT('Ctrl Pts',(5.78606133029722,3.96435850170953,89.9646845275077));
#138427=CARTESIAN_POINT('Ctrl Pts',(5.67507237409969,4.12167082861515,89.9734145763418));
#138428=CARTESIAN_POINT('Ctrl Pts',(5.55782685638255,4.27412999298956,89.9821446251758));
#138429=CARTESIAN_POINT('Ctrl Pts',(5.44054743697799,4.42663324112115,89.9908771983144));
#138430=CARTESIAN_POINT('Ctrl Pts',(5.3170080120053,4.57428030850853,89.999609771453));
#138431=CARTESIAN_POINT('Ctrl Pts',(5.18762953254229,4.71657994691017,90.0083423445916));
#138432=CARTESIAN_POINT('Ctrl Pts',(5.05641302523873,4.86090117884241,90.0171989778723));
#138433=CARTESIAN_POINT('Ctrl Pts',(4.91919048779769,4.99972167181726,90.026055611153));
#138434=CARTESIAN_POINT('Ctrl Pts',(4.77644072202909,5.13256666702365,90.0349122444337));
#138435=CARTESIAN_POINT('Ctrl Pts',(4.63560093879798,5.26363420487541,90.0436503765398));
#138436=CARTESIAN_POINT('Ctrl Pts',(4.48938113570517,5.38888498318307,90.052388508646));
#138437=CARTESIAN_POINT('Ctrl Pts',(4.33827621682943,5.50790214410098,90.0611266407522));
#138438=CARTESIAN_POINT('Ctrl Pts',(4.18409750996103,5.62934036134764,90.0700425246201));
#138439=CARTESIAN_POINT('Ctrl Pts',(4.02483304198778,5.74428844896389,90.0789584084881));
#138440=CARTESIAN_POINT('Ctrl Pts',(3.86104244637359,5.85234805781419,90.0878742923561));
#138441=CARTESIAN_POINT('Ctrl Pts',(3.69725185075939,5.96040766666449,90.096790176224));
#138442=CARTESIAN_POINT('Ctrl Pts',(3.52893538328009,6.06157863529025,90.105706060092));
#138443=CARTESIAN_POINT('Ctrl Pts',(3.3566832089298,6.15551008425693,90.11462194396));
#138444=CARTESIAN_POINT('Ctrl Pts',(3.18781583334146,6.24759575651066,90.1233626284565));
#138445=CARTESIAN_POINT('Ctrl Pts',(3.01514805499685,6.33273356532304,90.132103312953));
#138446=CARTESIAN_POINT('Ctrl Pts',(2.83925870842748,6.41063464480068,90.1408439974495));
#138447=CARTESIAN_POINT('Ctrl Pts',(2.6634010072735,6.48852170858,90.1495831093516));
#138448=CARTESIAN_POINT('Ctrl Pts',(2.48432314567789,6.55917453239809,90.1583222212538));
#138449=CARTESIAN_POINT('Ctrl Pts',(2.30262529376874,6.62235179668042,90.167061333156));
#138450=CARTESIAN_POINT('Ctrl Pts',(2.11857328468781,6.68634761334651,90.1759136728302));
#138451=CARTESIAN_POINT('Ctrl Pts',(1.93183318235458,6.74267269200077,90.1847660125044));
#138452=CARTESIAN_POINT('Ctrl Pts',(1.74304745914586,6.79112745556032,90.1936183521786));
#138453=CARTESIAN_POINT('Ctrl Pts',(1.55677196560573,6.8389379300126,90.2023529848286));
#138454=CARTESIAN_POINT('Ctrl Pts',(1.36850518901057,6.87908603184949,90.2110876174787));
#138455=CARTESIAN_POINT('Ctrl Pts',(1.17887830695027,6.91143056826169,90.2198222501287));
#138456=CARTESIAN_POINT('Ctrl Pts',(0.98541833592894,6.9444289122149,90.228733443315));
#138457=CARTESIAN_POINT('Ctrl Pts',(0.790542970481775,6.96930478037468,
90.2376446365013));
#138458=CARTESIAN_POINT('Ctrl Pts',(0.59493303747742,6.98596315789154,90.2465558296876));
#138459=CARTESIAN_POINT('Ctrl Pts',(0.399323104473196,7.00262153540839,
90.2554670228739));
#138460=CARTESIAN_POINT('Ctrl Pts',(0.202978904804958,7.01106238313513,
90.2643782160602));
#138461=CARTESIAN_POINT('Ctrl Pts',(0.00658751125685207,7.01124690530832,
90.2732894092465));
#138462=CARTESIAN_POINT('Ctrl Pts',(-0.170287961144518,7.01141309103551,
90.2813150740988));
#138463=CARTESIAN_POINT('Ctrl Pts',(-0.347283000346827,7.00488188201528,
90.2893407389511));
#138464=CARTESIAN_POINT('Ctrl Pts',(-0.52384488805084,6.99165310178952,
90.2973664038034));
#138465=CARTESIAN_POINT('Ctrl Pts',(-0.700350739342428,6.97842852005412,
90.3053895215065));
#138466=CARTESIAN_POINT('Ctrl Pts',(-0.876423347717666,6.95851062642809,
90.3134126392096));
#138467=CARTESIAN_POINT('Ctrl Pts',(-1.05151207542466,6.9319513066478,90.3214357569127));
#138468=CARTESIAN_POINT('Ctrl Pts',(-1.22657872291005,6.90539533623028,
90.3294578628304));
#138469=CARTESIAN_POINT('Ctrl Pts',(-1.4006613746394,6.8721996634916,90.3374799687481));
#138470=CARTESIAN_POINT('Ctrl Pts',(-1.57321663075256,6.83246778223093,
90.3455020746658));
#138471=CARTESIAN_POINT('Ctrl Pts',(-1.7458360089829,6.7927211364687,90.3535271616253));
#138472=CARTESIAN_POINT('Ctrl Pts',(-1.91692649951016,6.74643350946149,
90.3615522485847));
#138473=CARTESIAN_POINT('Ctrl Pts',(-2.08595653831519,6.69375917424284,
90.3695773355441));
#138474=CARTESIAN_POINT('Ctrl Pts',(-2.25501986674,6.64107446507761,90.3776040030042));
#138475=CARTESIAN_POINT('Ctrl Pts',(-2.42202158768804,6.58200065936432,
90.3856306704643));
#138476=CARTESIAN_POINT('Ctrl Pts',(-2.5864475293392,6.51674119023267,90.3936573379244));
#138477=CARTESIAN_POINT('Ctrl Pts',(-2.75100547155748,6.45142933102895,
90.4016904491649));
#138478=CARTESIAN_POINT('Ctrl Pts',(-2.9129831672907,6.37992203424297,90.4097235604054));
#138479=CARTESIAN_POINT('Ctrl Pts',(-3.07188800417212,6.30247020241456,
90.4177566716459));
#138480=CARTESIAN_POINT('Ctrl Pts',(-3.16552050660992,6.25683276950308,
90.4224900726082));
#138481=CARTESIAN_POINT('Ctrl Pts',(-3.25808657030009,6.20913227422691,
90.4272234735705));
#138482=CARTESIAN_POINT('Ctrl Pts',(-3.34948980370544,6.15942729621621,
90.4319568745328));
#138483=CARTESIAN_POINT('Ctrl Pts',(-3.53778330915744,6.0570334946037,90.4417078278273));
#138484=CARTESIAN_POINT('Ctrl Pts',(-3.72125190657123,5.94607109474755,
90.4514587811218));
#138485=CARTESIAN_POINT('Ctrl Pts',(-3.89921147911884,5.8269869060783,90.4612097344163));
#138486=CARTESIAN_POINT('Ctrl Pts',(-4.07742743581498,5.70773115429569,
90.4709747357882));
#138487=CARTESIAN_POINT('Ctrl Pts',(-4.25011845963373,5.58033022982133,
90.4807397371602));
#138488=CARTESIAN_POINT('Ctrl Pts',(-4.41662906056542,5.44527449297728,
90.4905047385321));
#138489=CARTESIAN_POINT('Ctrl Pts',(-4.58286212282468,5.31044386606437,
90.50025346367));
#138490=CARTESIAN_POINT('Ctrl Pts',(-4.74293532123849,5.16798395069382,
90.5100021888079));
#138491=CARTESIAN_POINT('Ctrl Pts',(-4.89622824128067,5.01842361422246,
90.5197509139457));
#138492=CARTESIAN_POINT('Ctrl Pts',(-5.04910043169596,4.86927376288338,
90.5294728826131));
#138493=CARTESIAN_POINT('Ctrl Pts',(-5.19522946545249,4.71306242274313,
90.5391948512805));
#138494=CARTESIAN_POINT('Ctrl Pts',(-5.33403220689424,4.550354599184,90.5489168199479));
#138495=CARTESIAN_POINT('Ctrl Pts',(-5.47191652684851,4.38872337079717,
90.5585744608878));
#138496=CARTESIAN_POINT('Ctrl Pts',(-5.60257113410021,4.22068136266675,
90.5682321018277));
#138497=CARTESIAN_POINT('Ctrl Pts',(-5.72545688972273,4.04682220593228,
90.5778897427676));
#138498=CARTESIAN_POINT('Ctrl Pts',(-5.77946940999854,3.9704051209684,90.5821346084516));
#138499=CARTESIAN_POINT('Ctrl Pts',(-5.83198149050525,3.89286473540746,
90.5863794741355));
#138500=CARTESIAN_POINT('Ctrl Pts',(-5.88294940643124,3.81425390395951,
90.5906243398194));
#138501=CARTESIAN_POINT('Ctrl Pts',(-5.97722618884616,3.66884524603762,
90.5984761868332));
#138502=CARTESIAN_POINT('Ctrl Pts',(-6.0661777107764,3.51983172051943,90.6063280338469));
#138503=CARTESIAN_POINT('Ctrl Pts',(-6.14951162340696,3.36765992286673,
90.6141798808607));
#138504=CARTESIAN_POINT('Ctrl Pts',(-6.23282190321341,3.21553127990596,
90.6220295011542));
#138505=CARTESIAN_POINT('Ctrl Pts',(-6.31051755964069,3.06024648068144,
90.6298791214476));
#138506=CARTESIAN_POINT('Ctrl Pts',(-6.38235100187132,2.90227880318418,
90.6377287417411));
#138507=CARTESIAN_POINT('Ctrl Pts',(-6.4541787091203,2.74432373738564,90.6455777353427));
#138508=CARTESIAN_POINT('Ctrl Pts',(-6.52014497665429,2.58368656727236,
90.6534267289444));
#138509=CARTESIAN_POINT('Ctrl Pts',(-6.58004949622673,2.42086248880567,
90.6612757225461));
#138510=CARTESIAN_POINT('Ctrl Pts',(-6.63998434370341,2.2579559772756,90.6691286898633));
#138511=CARTESIAN_POINT('Ctrl Pts',(-6.69385117954689,2.09286070368596,
90.6769816571806));
#138512=CARTESIAN_POINT('Ctrl Pts',(-6.74149881819082,1.9260893662631,90.6848346244979));
#138513=CARTESIAN_POINT('Ctrl Pts',(-6.78915855773392,1.75927567452434,
90.6926895862051));
#138514=CARTESIAN_POINT('Ctrl Pts',(-6.83059586229876,1.59078544140061,
90.7005445479122));
#138515=CARTESIAN_POINT('Ctrl Pts',(-6.86571039079761,1.42114298794801,
90.7083995096193));
#138516=CARTESIAN_POINT('Ctrl Pts',(-6.90085977340127,1.25133215017966,
90.7162622680325));
#138517=CARTESIAN_POINT('Ctrl Pts',(-6.92967378203119,1.08036718386781,
90.7241250264457));
#138518=CARTESIAN_POINT('Ctrl Pts',(-6.95210372993817,0.908779561103682,
90.731987784859));
#138519=CARTESIAN_POINT('Ctrl Pts',(-6.96855801787454,0.782905343161314,
90.7377557916079));
#138520=CARTESIAN_POINT('Ctrl Pts',(-6.98157782023667,0.656696184336185,
90.7435237983568));
#138521=CARTESIAN_POINT('Ctrl Pts',(-6.99116175634579,0.530362007602406,
90.7492918051057));
#138522=CARTESIAN_POINT('Ctrl Pts',(-7.00508248442123,0.346860813424763,
90.7576698715468));
#138523=CARTESIAN_POINT('Ctrl Pts',(-7.0117834348992,0.162689373238253,
90.7660479379878));
#138524=CARTESIAN_POINT('Ctrl Pts',(-7.01121685033776,-0.0215601493484155,
90.7744260044289));
#138525=CARTESIAN_POINT('Ctrl Pts',(-7.0106506532001,-0.205683684300519,
90.7827983420476));
#138526=CARTESIAN_POINT('Ctrl Pts',(-7.00282682965183,-0.389884867530377,
90.7911706796664));
#138527=CARTESIAN_POINT('Ctrl Pts',(-6.98774963364712,-0.573569193702466,
90.7995430172851));
#138528=CARTESIAN_POINT('Ctrl Pts',(-6.97268053616911,-0.757154856143024,
90.8079108578077));
#138529=CARTESIAN_POINT('Ctrl Pts',(-6.95036586143722,-0.940223888190426,
90.8162786983303));
#138530=CARTESIAN_POINT('Ctrl Pts',(-6.92086189661125,-1.12218410723665,
90.824646538853));
#138531=CARTESIAN_POINT('Ctrl Pts',(-6.89136945735317,-1.3040732444853,
90.8330111105229));
#138532=CARTESIAN_POINT('Ctrl Pts',(-6.85469338100169,-1.48485410850285,
90.8413756821929));
#138533=CARTESIAN_POINT('Ctrl Pts',(-6.81094158624387,-1.66394148673378,
90.8497402538628));
#138534=CARTESIAN_POINT('Ctrl Pts',(-6.76720047868659,-1.842985119497,90.8581027823285));
#138535=CARTESIAN_POINT('Ctrl Pts',(-6.71638717788038,-2.02033577251196,
90.8664653107942));
#138536=CARTESIAN_POINT('Ctrl Pts',(-6.65866041229904,-2.19541979497807,
90.8748278392598));
#138537=CARTESIAN_POINT('Ctrl Pts',(-6.60092903994172,-2.3705177896954,
90.8831910350814));
#138538=CARTESIAN_POINT('Ctrl Pts',(-6.53628319773679,-2.54334847844991,
90.8915542309029));
#138539=CARTESIAN_POINT('Ctrl Pts',(-6.46493130448406,-2.71335397447552,
90.8999174267244));
#138540=CARTESIAN_POINT('Ctrl Pts',(-6.39357454517533,-2.88337106453495,
90.9082811928991));
#138541=CARTESIAN_POINT('Ctrl Pts',(-6.31551094992987,-3.05056227438914,
90.9166449590738));
#138542=CARTESIAN_POINT('Ctrl Pts',(-6.2309969241478,-3.21439012780974,
90.9250087252485));
#138543=CARTESIAN_POINT('Ctrl Pts',(-6.14646586697067,-3.37825099606862,
90.9333741769021));
#138544=CARTESIAN_POINT('Ctrl Pts',(-6.05548193797086,-3.53874686417613,
90.9417396285557));
#138545=CARTESIAN_POINT('Ctrl Pts',(-5.95834749444242,-3.69536489375159,
90.9501050802093));
#138546=CARTESIAN_POINT('Ctrl Pts',(-5.86118052078041,-3.85203537439629,
90.9584733334361));
#138547=CARTESIAN_POINT('Ctrl Pts',(-5.75785909852066,-4.00482514760566,
90.966841586663));
#138548=CARTESIAN_POINT('Ctrl Pts',(-5.6487291231527,-4.15325003530326,
90.9752098398899));
#138549=CARTESIAN_POINT('Ctrl Pts',(-5.539497968728,-4.30181253404754,90.9835858516814));
#138550=CARTESIAN_POINT('Ctrl Pts',(-5.42444769460716,-4.44600179525974,
90.9919618634728));
#138551=CARTESIAN_POINT('Ctrl Pts',(-5.30396550338178,-4.58536547086883,
91.0003378752643));
#138552=CARTESIAN_POINT('Ctrl Pts',(-5.18342422620107,-4.72479749214649,
91.0087179947555));
#138553=CARTESIAN_POINT('Ctrl Pts',(-5.05744593946122,-4.85939896422367,
91.0170981142467));
#138554=CARTESIAN_POINT('Ctrl Pts',(-4.92645542832505,-4.98875369959539,
91.0254782337379));
#138555=CARTESIAN_POINT('Ctrl Pts',(-4.79531524393695,-5.11825623913802,
91.0338679285771));
#138556=CARTESIAN_POINT('Ctrl Pts',(-4.65915162977974,-5.24249983618741,
91.0422576234163));
#138557=CARTESIAN_POINT('Ctrl Pts',(-4.51842422645533,-5.36110707524869,
91.0506473182556));
#138558=CARTESIAN_POINT('Ctrl Pts',(-4.42907882658603,-5.43640876455007,
91.0559737907299));
#138559=CARTESIAN_POINT('Ctrl Pts',(-4.33789453137321,-5.50943939104233,
91.0613002632043));
#138560=CARTESIAN_POINT('Ctrl Pts',(-4.24499520189908,-5.58011131594647,
91.0666267356786));
#138561=CARTESIAN_POINT('Ctrl Pts',(-4.09881643320823,-5.69131486307623,
91.0750080360838));
#138562=CARTESIAN_POINT('Ctrl Pts',(-3.9480949743858,-5.79690056691435,
91.083389336489));
#138563=CARTESIAN_POINT('Ctrl Pts',(-3.79328726983489,-5.89649033332614,
91.0917706368942));
#138564=CARTESIAN_POINT('Ctrl Pts',(-3.63867576138784,-5.99595388428753,
91.1001413152281));
#138565=CARTESIAN_POINT('Ctrl Pts',(-3.47998860118239,-6.08943646595483,
91.1085119935619));
#138566=CARTESIAN_POINT('Ctrl Pts',(-3.3177143203471,-6.17660086544887,
91.1168826718958));
#138567=CARTESIAN_POINT('Ctrl Pts',(-3.15562419296002,-6.26366634831458,
91.1252438509469));
#138568=CARTESIAN_POINT('Ctrl Pts',(-2.98995534531866,-6.34442778560803,
91.133605029998));
#138569=CARTESIAN_POINT('Ctrl Pts',(-2.8212246166298,-6.41859160758979,
91.1419662090491));
#138570=CARTESIAN_POINT('Ctrl Pts',(-2.652712835964,-6.49265919326455,91.1503165384841));
#138571=CARTESIAN_POINT('Ctrl Pts',(-2.48114739766183,-6.56014610859738,
91.1586668679192));
#138572=CARTESIAN_POINT('Ctrl Pts',(-2.30706894933385,-6.62080504361211,
91.1670171973542));
#138573=CARTESIAN_POINT('Ctrl Pts',(-2.13312444395829,-6.68141730520504,
91.1753611017103));
#138574=CARTESIAN_POINT('Ctrl Pts',(-1.95667108998198,-6.73521194883545,
91.1837050060663));
#138575=CARTESIAN_POINT('Ctrl Pts',(-1.77826975363198,-6.78198962295119,
91.1920489104224));
#138576=CARTESIAN_POINT('Ctrl Pts',(-1.60001171034975,-6.82872972494688,
91.2003861129023));
#138577=CARTESIAN_POINT('Ctrl Pts',(-1.41980912114773,-6.86846401491194,
91.2087233153823));
#138578=CARTESIAN_POINT('Ctrl Pts',(-1.23823841131452,-6.90104283418422,
91.2170605178623));
#138579=CARTESIAN_POINT('Ctrl Pts',(-1.17846633592472,-6.91176760165052,
91.2198050788965));
#138580=CARTESIAN_POINT('Ctrl Pts',(-1.1185461148567,-6.9217173412299,91.2225496399308));
#138581=CARTESIAN_POINT('Ctrl Pts',(-1.0584986244227,-6.93088791026051,
91.225294200965));
#138582=CARTESIAN_POINT('Ctrl Pts',(-0.876067043634374,-6.9587492145863,
91.2336325112663));
#138583=CARTESIAN_POINT('Ctrl Pts',(-0.692609763919077,-6.9793919671487,
91.2419708215676));
#138584=CARTESIAN_POINT('Ctrl Pts',(-0.508721244211202,-6.9927697844408,
91.2503091318688));
#138585=CARTESIAN_POINT('Ctrl Pts',(-0.32471702808511,-7.0061560186017,
91.258652688352));
#138586=CARTESIAN_POINT('Ctrl Pts',(-0.140281357568597,-7.01226817658832,
91.2669962448353));
#138587=CARTESIAN_POINT('Ctrl Pts',(0.0439900195475317,-7.01111199744236,
91.2753398013185));
#138588=CARTESIAN_POINT('Ctrl Pts',(0.228401589524863,-7.00995493868035,
91.2836897055431));
#138589=CARTESIAN_POINT('Ctrl Pts',(0.412648289506366,-7.00151851485407,
91.2920396097678));
#138590=CARTESIAN_POINT('Ctrl Pts',(0.596137764433919,-6.98586045726049,
91.3003895139924));
#138591=CARTESIAN_POINT('Ctrl Pts',(0.779902459993951,-6.97017891373937,
91.3087519424554));
#138592=CARTESIAN_POINT('Ctrl Pts',(0.962907334103701,-6.94725411875867,
91.3171143709185));
#138593=CARTESIAN_POINT('Ctrl Pts',(1.1445670123845,-6.91719545167413,91.3254767993815));
#138594=CARTESIAN_POINT('Ctrl Pts',(1.32638203445439,-6.88711108033158,
91.3338463788608));
#138595=CARTESIAN_POINT('Ctrl Pts',(1.50684924536742,-6.84988073098574,
91.3422159583401));
#138596=CARTESIAN_POINT('Ctrl Pts',(1.68539621167435,-6.80566427119159,
91.3505855378195));
#138597=CARTESIAN_POINT('Ctrl Pts',(1.86421856492236,-6.76137961289561,
91.3589680263554));
#138598=CARTESIAN_POINT('Ctrl Pts',(2.0411144410396,-6.7100874031092,91.3673505148913));
#138599=CARTESIAN_POINT('Ctrl Pts',(2.2155278856756,-6.65199689945011,91.3757330034272));
#138600=CARTESIAN_POINT('Ctrl Pts',(2.27259882277569,-6.63298873475638,
91.3784758910353));
#138601=CARTESIAN_POINT('Ctrl Pts',(2.32940413616106,-6.61325305162709,
91.3812187786434));
#138602=CARTESIAN_POINT('Ctrl Pts',(2.38592487488105,-6.59279827189668,
91.3839616662515));
#138603=CARTESIAN_POINT('Ctrl Pts',(2.55880866657857,-6.53023185896195,
91.3923515213848));
#138604=CARTESIAN_POINT('Ctrl Pts',(2.72937738320644,-6.46080769298565,
91.400741376518));
#138605=CARTESIAN_POINT('Ctrl Pts',(2.89706946972923,-6.38471730384853,
91.4091312316513));
#138606=CARTESIAN_POINT('Ctrl Pts',(3.06460681234585,-6.30869712985561,
91.4175133447439));
#138607=CARTESIAN_POINT('Ctrl Pts',(3.22927251872187,-6.22602313087909,
91.4258954578365));
#138608=CARTESIAN_POINT('Ctrl Pts',(3.39052343719861,-6.13693550433007,
91.4342775709291));
#138609=CARTESIAN_POINT('Ctrl Pts',(3.55164925913813,-6.04791699089802,
91.4426531812784));
#138610=CARTESIAN_POINT('Ctrl Pts',(3.70936528807828,-5.95249492815169,
91.4510287916277));
#138611=CARTESIAN_POINT('Ctrl Pts',(3.86315107188018,-5.85095636270952,
91.4594044019771));
#138612=CARTESIAN_POINT('Ctrl Pts',(4.0168401221405,-5.74948166653276,91.4677747439431));
#138613=CARTESIAN_POINT('Ctrl Pts',(4.16660358295411,-5.64189831963237,
91.4761450859092));
#138614=CARTESIAN_POINT('Ctrl Pts',(4.31194781502063,-5.52853801678516,
91.4845154278752));
#138615=CARTESIAN_POINT('Ctrl Pts',(4.45722192923922,-5.41523240190433,
91.49288173177));
#138616=CARTESIAN_POINT('Ctrl Pts',(4.59808080742231,-5.29615559052077,
91.5012480356649));
#138617=CARTESIAN_POINT('Ctrl Pts',(4.73406151956882,-5.17168136019977,
91.5096143395597));
#138618=CARTESIAN_POINT('Ctrl Pts',(4.87000420172109,-5.04724194183251,
91.5179783036337));
#138619=CARTESIAN_POINT('Ctrl Pts',(5.00107119501868,-4.91740833511234,
91.5263422677078));
#138620=CARTESIAN_POINT('Ctrl Pts',(5.12683385474934,-4.78259356294219,
91.5347062317819));
#138621=CARTESIAN_POINT('Ctrl Pts',(5.25257716169686,-4.64779953652483,
91.5430689087809));
#138622=CARTESIAN_POINT('Ctrl Pts',(5.37301753839158,-4.50802611319689,
91.5514315857799));
#138623=CARTESIAN_POINT('Ctrl Pts',(5.48776403248056,-4.36372232002825,
91.559794262779));
#138624=CARTESIAN_POINT('Ctrl Pts',(5.60250816414852,-4.2194214978115,91.5681567676057));
#138625=CARTESIAN_POINT('Ctrl Pts',(5.71155844272837,-4.07059074922487,
91.5765192724325));
#138626=CARTESIAN_POINT('Ctrl Pts',(5.81456469406526,-3.91771157450746,
91.5848817772593));
#138627=CARTESIAN_POINT('Ctrl Pts',(5.91758255469326,-3.76481516958491,
91.5932452245798));
#138628=CARTESIAN_POINT('Ctrl Pts',(6.01455484679185,-3.60786970169083,
91.6016086719004));
#138629=CARTESIAN_POINT('Ctrl Pts',(6.10517492330863,-3.44738534520054,
91.6099721192209));
#138630=CARTESIAN_POINT('Ctrl Pts',(6.19584835947187,-3.28680649101334,
91.6183404911742));
#138631=CARTESIAN_POINT('Ctrl Pts',(6.28016194331338,-3.12268487031842,
91.6267088631274));
#138632=CARTESIAN_POINT('Ctrl Pts',(6.3578546834387,-2.9555558507287,91.6350772350807));
#138633=CARTESIAN_POINT('Ctrl Pts',(6.43557070233943,-2.78837675491686,
91.6434481144169));
#138634=CARTESIAN_POINT('Ctrl Pts',(6.50666178814667,-2.61818876376641,
91.6518189937531));
#138635=CARTESIAN_POINT('Ctrl Pts',(6.57091498856201,-2.44554754106132,
91.6601898730893));
#138636=CARTESIAN_POINT('Ctrl Pts',(6.63522263001914,-2.27276004131543,
91.668567844981));
#138637=CARTESIAN_POINT('Ctrl Pts',(6.6926806996216,-2.09751546674238,91.6769458168727));
#138638=CARTESIAN_POINT('Ctrl Pts',(6.74312567677145,-1.92038607310239,
91.6853237887645));
#138639=CARTESIAN_POINT('Ctrl Pts',(6.77518387048917,-1.80781890120051,
91.6906480581178));
#138640=CARTESIAN_POINT('Ctrl Pts',(6.8044106921968,-1.69449079644053,91.6959723274711));
#138641=CARTESIAN_POINT('Ctrl Pts',(6.83077487139509,-1.58055092256384,
91.7012965968244));
#138642=CARTESIAN_POINT('Ctrl Pts',(6.87364674711607,-1.39526860917314,
91.7099546101197));
#138643=CARTESIAN_POINT('Ctrl Pts',(6.90902110269616,-1.20804545735541,
91.718612623415));
#138644=CARTESIAN_POINT('Ctrl Pts',(6.93673266435465,-1.01949325930841,
91.7272706367104));
#138645=CARTESIAN_POINT('Ctrl Pts',(6.96437737102982,-0.831395949160153,
91.7359077622859));
#138646=CARTESIAN_POINT('Ctrl Pts',(6.98439612141707,-0.641976267561167,
91.7445448878615));
#138647=CARTESIAN_POINT('Ctrl Pts',(6.99667434903524,-0.451856853497069,
91.7531820134371));
#138648=CARTESIAN_POINT('Ctrl Pts',(7.00631840262471,-0.302525706148289,
91.7599661279282));
#138649=CARTESIAN_POINT('Ctrl Pts',(7.01118792571455,-0.152763206936516,
91.7667502424193));
#138650=CARTESIAN_POINT('Ctrl Pts',(7.01124941011624,-0.00287604671718754,
91.7735343569104));
#138651=CARTESIAN_POINT('Ctrl Pts',(7.01124941011649,-0.00287604611315284,
91.7735343569377));
#138652=CARTESIAN_POINT('Ctrl Pts',(7.01131757022026,0.163285228292073,
91.7810550618994));
#138653=CARTESIAN_POINT('Ctrl Pts',(7.00547459428384,0.329575821306189,
91.7885757668611));
#138654=CARTESIAN_POINT('Ctrl Pts',(6.99371928995571,0.49549677678211,91.7960964718228));
#138655=CARTESIAN_POINT('Ctrl Pts',(6.98196648505464,0.661382453943276,
91.803615577723));
#138656=CARTESIAN_POINT('Ctrl Pts',(6.96430388228248,0.826898246011775,
91.8111346836233));
#138657=CARTESIAN_POINT('Ctrl Pts',(6.94078235372727,0.991547719824008,
91.8186537895235));
#138658=CARTESIAN_POINT('Ctrl Pts',(6.91725260803701,1.15625471315322,91.826175522188));
#138659=CARTESIAN_POINT('Ctrl Pts',(6.88785990483666,1.32009438216346,91.8336972548524));
#138660=CARTESIAN_POINT('Ctrl Pts',(6.85270668801346,1.48257802848806,91.8412189875169));
#138661=CARTESIAN_POINT('Ctrl Pts',(6.82350465434371,1.61755437886365,91.8474673457148));
#138662=CARTESIAN_POINT('Ctrl Pts',(6.79032839184587,1.75159501383177,91.8537157039128));
#138663=CARTESIAN_POINT('Ctrl Pts',(6.75326300162656,1.88442707297518,91.8599640621107));
#138664=CARTESIAN_POINT('Ctrl Pts',(6.70037504303367,2.07396282053429,91.8688797354031));
#138665=CARTESIAN_POINT('Ctrl Pts',(6.63957404626945,2.26102355855614,91.8777954086954));
#138666=CARTESIAN_POINT('Ctrl Pts',(6.57110895151815,2.44502632087633,91.8867110819877));
#138667=CARTESIAN_POINT('',(7.01124860966183,-0.00441542920841772,91.2264656430895));
#138668=CARTESIAN_POINT('Ctrl Pts',(6.5711089515181,2.44502632087648,91.3398522865014));
#138669=CARTESIAN_POINT('Ctrl Pts',(6.63771924680903,2.26600840850791,91.3311805125692));
#138670=CARTESIAN_POINT('Ctrl Pts',(6.69700989700486,2.08426710051917,91.3225087386371));
#138671=CARTESIAN_POINT('Ctrl Pts',(6.7487830778944,1.90040877971718,91.313836964705));
#138672=CARTESIAN_POINT('Ctrl Pts',(6.80055978789547,1.7165379262389,91.3051645996626));
#138673=CARTESIAN_POINT('Ctrl Pts',(6.84481792613587,1.53055004459392,91.2964922346203));
#138674=CARTESIAN_POINT('Ctrl Pts',(6.88140980451109,1.34306577086852,91.2878198695779));
#138675=CARTESIAN_POINT('Ctrl Pts',(6.91799949925392,1.15559268532888,91.2791480220618));
#138676=CARTESIAN_POINT('Ctrl Pts',(6.94692379517697,0.966623665170273,
91.2704761745457));
#138677=CARTESIAN_POINT('Ctrl Pts',(6.96808618426394,0.776789219267382,
91.2618043270296));
#138678=CARTESIAN_POINT('Ctrl Pts',(6.98924897510681,0.586951169465677,
91.2531323148833));
#138679=CARTESIAN_POINT('Ctrl Pts',(7.0026495327686,0.396247943318909,91.2444603027372));
#138680=CARTESIAN_POINT('Ctrl Pts',(7.0082431436184,0.205315860141579,91.235788290591));
#138681=CARTESIAN_POINT('Ctrl Pts',(7.01024757124657,0.136896809746186,
91.2326807414238));
#138682=CARTESIAN_POINT('Ctrl Pts',(7.01125,0.0684484052927758,91.2295731922566));
#138683=CARTESIAN_POINT('Ctrl Pts',(7.01125,8.58630487052188E-16,91.2264656430895));
#138684=CARTESIAN_POINT('Ctrl Pts',(7.01124860966183,-0.00441542920841772,
91.2264656430895));
#138685=CARTESIAN_POINT('Ctrl Pts',(7.01111401898774,-0.218131612174622,
91.2167762696257));
#138686=CARTESIAN_POINT('Ctrl Pts',(7.00120369221107,-0.431553992030833,
91.2070868961619));
#138687=CARTESIAN_POINT('Ctrl Pts',(6.98162202993273,-0.643879176288536,
91.1973975226981));
#138688=CARTESIAN_POINT('Ctrl Pts',(6.96102990223338,-0.867160900070445,
91.1872081520074));
#138689=CARTESIAN_POINT('Ctrl Pts',(6.92974218381963,-1.08922910119445,
91.1770187813167));
#138690=CARTESIAN_POINT('Ctrl Pts',(6.88793931774568,-1.30916710833768,
91.1668294106261));
#138691=CARTESIAN_POINT('Ctrl Pts',(6.84780526563828,-1.52032496109034,
91.1570468102293));
#138692=CARTESIAN_POINT('Ctrl Pts',(6.79797927933411,-1.72951939372668,
91.1472642098326));
#138693=CARTESIAN_POINT('Ctrl Pts',(6.73867228106864,-1.93595517790499,
91.1374816094358));
#138694=CARTESIAN_POINT('Ctrl Pts',(6.67933190914448,-2.14250712910584,
91.1276935041041));
#138695=CARTESIAN_POINT('Ctrl Pts',(6.61049987072077,-2.34629729945448,
91.1179053987724));
#138696=CARTESIAN_POINT('Ctrl Pts',(6.53243709486289,-2.54654514276878,
91.1081172934407));
#138697=CARTESIAN_POINT('Ctrl Pts',(6.45451667045176,-2.74642782394416,
91.0983470372175));
#138698=CARTESIAN_POINT('Ctrl Pts',(6.36739914687599,-2.94278105315336,
91.0885767809943));
#138699=CARTESIAN_POINT('Ctrl Pts',(6.27139328918328,-3.13484493633847,
91.0788065247711));
#138700=CARTESIAN_POINT('Ctrl Pts',(6.25933489510154,-3.15896827680929,
91.0775793746507));
#138701=CARTESIAN_POINT('Ctrl Pts',(6.24713634688621,-3.18302397230467,
91.0763522245304));
#138702=CARTESIAN_POINT('Ctrl Pts',(6.23479831147988,-3.20701053594585,
91.0751250744101));
#138703=CARTESIAN_POINT('Ctrl Pts',(6.15403231604415,-3.36402894493563,
91.0670920288114));
#138704=CARTESIAN_POINT('Ctrl Pts',(6.06724655878398,-3.51815830011059,
91.0590589832128));
#138705=CARTESIAN_POINT('Ctrl Pts',(5.97467924385955,-3.66890099287155,
91.0510259376142));
#138706=CARTESIAN_POINT('Ctrl Pts',(5.88217143476943,-3.81954678242531,
91.0429980559665));
#138707=CARTESIAN_POINT('Ctrl Pts',(5.78388965703437,-3.96680993201838,
91.0349701743189));
#138708=CARTESIAN_POINT('Ctrl Pts',(5.68011830558371,-4.11021685523683,
91.0269422926712));
#138709=CARTESIAN_POINT('Ctrl Pts',(5.57639380792113,-4.25355902881582,
91.0189180356913));
#138710=CARTESIAN_POINT('Ctrl Pts',(5.46718488616196,-4.39304814644092,
91.0108937787113));
#138711=CARTESIAN_POINT('Ctrl Pts',(5.35281953637398,-4.5282391250367,91.0028695217314));
#138712=CARTESIAN_POINT('Ctrl Pts',(5.23846801452165,-4.66341375766616,
90.9948462349659));
#138713=CARTESIAN_POINT('Ctrl Pts',(5.11896153720162,-4.79429100171989,
90.9868229482003));
#138714=CARTESIAN_POINT('Ctrl Pts',(4.99466882434933,-4.92045830157852,
90.9787996614348));
#138715=CARTESIAN_POINT('Ctrl Pts',(4.87038629617602,-5.04661526315248,
90.970777032106));
#138716=CARTESIAN_POINT('Ctrl Pts',(4.74131857384571,-5.16806279091223,
90.9627544027773));
#138717=CARTESIAN_POINT('Ctrl Pts',(4.60787150227857,-5.28442492434031,
90.9547317734485));
#138718=CARTESIAN_POINT('Ctrl Pts',(4.47437426411301,-5.4008308016464,90.9467061281822));
#138719=CARTESIAN_POINT('Ctrl Pts',(4.33649466635002,-5.51214722677634,
90.938680482916));
#138720=CARTESIAN_POINT('Ctrl Pts',(4.19467220699311,-5.61803805953462,
90.9306548376498));
#138721=CARTESIAN_POINT('Ctrl Pts',(4.1110450427043,-5.6804777472111,90.9259224281411));
#138722=CARTESIAN_POINT('Ctrl Pts',(4.02604755291839,-5.74103173588268,
90.9211900186324));
#138723=CARTESIAN_POINT('Ctrl Pts',(3.93977462314144,-5.79963813365547,
90.9164576091237));
#138724=CARTESIAN_POINT('Ctrl Pts',(3.78062379549338,-5.90775149824303,
90.9077275602889));
#138725=CARTESIAN_POINT('Ctrl Pts',(3.6170516356225,-6.00928900419784,90.8989975114541));
#138726=CARTESIAN_POINT('Ctrl Pts',(3.4496124399988,-6.10391682252515,90.8902674626193));
#138727=CARTESIAN_POINT('Ctrl Pts',(3.28212482912266,-6.19857200260426,
90.88153488948));
#138728=CARTESIAN_POINT('Ctrl Pts',(3.11076818908052,-6.28631337226743,
90.8728023163407));
#138729=CARTESIAN_POINT('Ctrl Pts',(2.93612178164148,-6.36685286824429,
90.8640697432014));
#138730=CARTESIAN_POINT('Ctrl Pts',(2.75899424320109,-6.44853655632467,
90.855213109921));
#138731=CARTESIAN_POINT('Ctrl Pts',(2.57848301537317,-6.52281206155041,
90.8463564766407));
#138732=CARTESIAN_POINT('Ctrl Pts',(2.39521419140078,-6.58942907540648,
90.8374998433603));
#138733=CARTESIAN_POINT('Ctrl Pts',(2.21439749229441,-6.65515475797863,
90.8287617112534));
#138734=CARTESIAN_POINT('Ctrl Pts',(2.03089680063777,-6.71342554354831,
90.8200235791465));
#138735=CARTESIAN_POINT('Ctrl Pts',(1.84533044372671,-6.76405071802063,
90.8112854470396));
#138736=CARTESIAN_POINT('Ctrl Pts',(1.65598928160953,-6.81570571371346,
90.8023695631726));
#138737=CARTESIAN_POINT('Ctrl Pts',(1.46449779897392,-6.85940062961549,
90.7934536793055));
#138738=CARTESIAN_POINT('Ctrl Pts',(1.27152670013854,-6.89498704954076,
90.7845377954384));
#138739=CARTESIAN_POINT('Ctrl Pts',(1.07855560130315,-6.93057346946603,
90.7756219115713));
#138740=CARTESIAN_POINT('Ctrl Pts',(0.88410518476869,-6.95805134455265,
90.7667060277043));
#138741=CARTESIAN_POINT('Ctrl Pts',(0.688855744563673,-6.97732787861382,
90.7577901438372));
#138742=CARTESIAN_POINT('Ctrl Pts',(0.497443005196789,-6.99622562390965,
90.7490494593411));
#138743=CARTESIAN_POINT('Ctrl Pts',(0.305242022760735,-7.00724336029926,
90.740308774845));
#138744=CARTESIAN_POINT('Ctrl Pts',(0.112898462332252,-7.01034096886186,
90.7315680903489));
#138745=CARTESIAN_POINT('Ctrl Pts',(-0.0794104922946831,-7.01343802011322,
90.7228289784471));
#138746=CARTESIAN_POINT('Ctrl Pts',(-0.271861700023683,-7.00861778488938,
90.7140898665453));
#138747=CARTESIAN_POINT('Ctrl Pts',(-0.463808403006335,-6.99589224672598,
90.7053507546435));
#138748=CARTESIAN_POINT('Ctrl Pts',(-0.658242051788765,-6.98300183090023,
90.6964984149692));
#138749=CARTESIAN_POINT('Ctrl Pts',(-0.852157745644223,-6.96199983140183,
90.6876460752948));
#138750=CARTESIAN_POINT('Ctrl Pts',(-1.04488606461541,-6.93295317123032,
90.6787937356204));
#138751=CARTESIAN_POINT('Ctrl Pts',(-1.23505173034007,-6.90429273617812,
90.6700591029707));
#138752=CARTESIAN_POINT('Ctrl Pts',(-1.42406112570954,-6.86780030258419,
90.661324470321));
#138753=CARTESIAN_POINT('Ctrl Pts',(-1.61127801079577,-6.82359214303039,
90.6525898376714));
#138754=CARTESIAN_POINT('Ctrl Pts',(-1.80227926954812,-6.77849036645713,
90.6436786444846));
#138755=CARTESIAN_POINT('Ctrl Pts',(-1.99141449156612,-6.72535765834916,
90.6347674512979));
#138756=CARTESIAN_POINT('Ctrl Pts',(-2.17801974076475,-6.66437218133404,
90.6258562581111));
#138757=CARTESIAN_POINT('Ctrl Pts',(-2.36462498996338,-6.60338670431893,
90.6169450649244));
#138758=CARTESIAN_POINT('Ctrl Pts',(-2.54869997402439,-6.53454853975545,
90.6080338717376));
#138759=CARTESIAN_POINT('Ctrl Pts',(-2.72959694168776,-6.45809005034994,
90.5991226785509));
#138760=CARTESIAN_POINT('Ctrl Pts',(-2.8925177094081,-6.38922943895559,
90.5910970136984));
#138761=CARTESIAN_POINT('Ctrl Pts',(-3.05293536394538,-6.31415563055654,
90.583071348846));
#138762=CARTESIAN_POINT('Ctrl Pts',(-3.21034092784385,-6.2330841234104,
90.5750456839936));
#138763=CARTESIAN_POINT('Ctrl Pts',(-3.36769653507731,-6.15203834637203,
90.5670225662903));
#138764=CARTESIAN_POINT('Ctrl Pts',(-3.5220416294079,-6.06499882796826,
90.558999448587));
#138765=CARTESIAN_POINT('Ctrl Pts',(-3.67288946274933,-5.97222819029254,
90.5509763308837));
#138766=CARTESIAN_POINT('Ctrl Pts',(-3.82371827285875,-5.87946925180618,
90.5429542249658));
#138767=CARTESIAN_POINT('Ctrl Pts',(-3.97105038862194,-5.78098082615121,
90.5349321190479));
#138768=CARTESIAN_POINT('Ctrl Pts',(-4.11442586268974,-5.67707022881784,
90.5269100131299));
#138769=CARTESIAN_POINT('Ctrl Pts',(-4.25785461556809,-5.57312101795544,
90.5188849261704));
#138770=CARTESIAN_POINT('Ctrl Pts',(-4.39732349069979,-5.46374582317389,
90.5108598392108));
#138771=CARTESIAN_POINT('Ctrl Pts',(-4.53240325158435,-5.34929409618948,
90.5028347522512));
#138772=CARTESIAN_POINT('Ctrl Pts',(-4.66750961575186,-5.23481982851017,
90.4948080847909));
#138773=CARTESIAN_POINT('Ctrl Pts',(-4.79822486963941,-5.11526728055089,
90.4867814173306));
#138774=CARTESIAN_POINT('Ctrl Pts',(-4.92415497178524,-4.99102438146146,
90.4787547498703));
#138775=CARTESIAN_POINT('Ctrl Pts',(-5.05018617017328,-4.86668174061048,
90.4707216386297));
#138776=CARTESIAN_POINT('Ctrl Pts',(-5.17142429000805,-4.73764149220409,
90.462688527389));
#138777=CARTESIAN_POINT('Ctrl Pts',(-5.28751366213962,-4.60432686015957,
90.4546554161484));
#138778=CARTESIAN_POINT('Ctrl Pts',(-5.35591773737159,-4.52577303604585,
90.449922015187));
#138779=CARTESIAN_POINT('Ctrl Pts',(-5.42253493239662,-4.44573577772568,
90.4451886142256));
#138780=CARTESIAN_POINT('Ctrl Pts',(-5.48729935260437,-4.36430663191848,
90.4404552132643));
#138781=CARTESIAN_POINT('Ctrl Pts',(-5.62071607384014,-4.19656005730582,
90.4307042599703));
#138782=CARTESIAN_POINT('Ctrl Pts',(-5.74634700732499,-4.02280664304849,
90.4209533066762));
#138783=CARTESIAN_POINT('Ctrl Pts',(-5.86373659786333,-3.843724713527,90.4112023533822));
#138784=CARTESIAN_POINT('Ctrl Pts',(-5.98129531012859,-3.66438478289108,
90.4014373520107));
#138785=CARTESIAN_POINT('Ctrl Pts',(-6.09058890837239,-3.47970101359067,
90.3916723506393));
#138786=CARTESIAN_POINT('Ctrl Pts',(-6.19120518796534,-3.29038065928718,
90.3819073492678));
#138787=CARTESIAN_POINT('Ctrl Pts',(-6.29165376106743,-3.101375862788,90.3721586241303));
#138788=CARTESIAN_POINT('Ctrl Pts',(-6.38345390397528,-2.90774996034723,
90.3624098989929));
#138789=CARTESIAN_POINT('Ctrl Pts',(-6.46624073213302,-2.71023197468478,
90.3526611738555));
#138790=CARTESIAN_POINT('Ctrl Pts',(-6.54880034254809,-2.51325609930533,
90.3429392051884));
#138791=CARTESIAN_POINT('Ctrl Pts',(-6.62239600825781,-2.31240950291824,
90.3332172365214));
#138792=CARTESIAN_POINT('Ctrl Pts',(-6.68671126917638,-2.10843993634384,
90.3234952678544));
#138793=CARTESIAN_POINT('Ctrl Pts',(-6.75060097281172,-1.90581998311739,
90.3138376269148));
#138794=CARTESIAN_POINT('Ctrl Pts',(-6.80533263618203,-1.70011828668716,
90.3041799859752));
#138795=CARTESIAN_POINT('Ctrl Pts',(-6.85064147790634,-1.49209178795718,
90.2945223450356));
#138796=CARTESIAN_POINT('Ctrl Pts',(-6.87055627373543,-1.40065697983616,
90.2902774793498));
#138797=CARTESIAN_POINT('Ctrl Pts',(-6.88865126635209,-1.3087733510309,
90.2860326136639));
#138798=CARTESIAN_POINT('Ctrl Pts',(-6.90490681962776,-1.21650662750276,
90.281787747978));
#138799=CARTESIAN_POINT('Ctrl Pts',(-6.93497517205459,-1.04583828338269,
90.273935900964));
#138800=CARTESIAN_POINT('Ctrl Pts',(-6.95873380167374,-0.873928622336891,
90.2660840539501));
#138801=CARTESIAN_POINT('Ctrl Pts',(-6.97608778540285,-0.701302910911618,
90.2582322069362));
#138802=CARTESIAN_POINT('Ctrl Pts',(-6.99343684768249,-0.528726154742379,
90.2503825866425));
#138803=CARTESIAN_POINT('Ctrl Pts',(-7.00438483889646,-0.355434131303304,
90.2425329663489));
#138804=CARTESIAN_POINT('Ctrl Pts',(-7.008888457383,-0.181959210987826,
90.2346833460553));
#138805=CARTESIAN_POINT('Ctrl Pts',(-7.01339171631321,-0.00849814042606301,
90.2268343524535));
#138806=CARTESIAN_POINT('Ctrl Pts',(-7.01145161759495,0.165145416588549,
90.2189853588516));
#138807=CARTESIAN_POINT('Ctrl Pts',(-7.003076946412,0.338437357767773,90.2111363652498));
#138808=CARTESIAN_POINT('Ctrl Pts',(-6.99469803537824,0.511817031582644,
90.2032833979323));
#138809=CARTESIAN_POINT('Ctrl Pts',(-6.97987806139806,0.684844352367448,
90.1954304306148));
#138810=CARTESIAN_POINT('Ctrl Pts',(-6.95867786783009,0.856988269623172,
90.1875774632974));
#138811=CARTESIAN_POINT('Ctrl Pts',(-6.9374722901253,1.02917590564969,90.1797225015901));
#138812=CARTESIAN_POINT('Ctrl Pts',(-6.90988332535552,1.20047931452409,
90.1718675398828));
#138813=CARTESIAN_POINT('Ctrl Pts',(-6.87602316632931,1.37037658276937,
90.1640125781755));
#138814=CARTESIAN_POINT('Ctrl Pts',(-6.84212939826494,1.54044248825485,
90.1561498197621));
#138815=CARTESIAN_POINT('Ctrl Pts',(-6.80195209202393,1.70909909459969,
90.1482870613488));
#138816=CARTESIAN_POINT('Ctrl Pts',(-6.75565379071956,1.87583805869175,
90.1404243029354));
#138817=CARTESIAN_POINT('Ctrl Pts',(-6.72169002122517,1.99815537018289,
90.1346562961874));
#138818=CARTESIAN_POINT('Ctrl Pts',(-6.68443330329901,2.11944099995356,
90.1288882894395));
#138819=CARTESIAN_POINT('Ctrl Pts',(-6.643964273863,2.23950112528038,90.1231202826915));
#138820=CARTESIAN_POINT('Ctrl Pts',(-6.58518275153927,2.41388921996521,
90.1147422162505));
#138821=CARTESIAN_POINT('Ctrl Pts',(-6.51949218948702,2.58607740822059,
90.1063641498095));
#138822=CARTESIAN_POINT('Ctrl Pts',(-6.44707966720528,2.75550182856196,
90.0979860833685));
#138823=CARTESIAN_POINT('Ctrl Pts',(-6.37471665974586,2.9248103984978,90.0896137457498));
#138824=CARTESIAN_POINT('Ctrl Pts',(-6.29564098469229,3.09135866697528,
90.081241408131));
#138825=CARTESIAN_POINT('Ctrl Pts',(-6.21008852409923,3.25460091030391,
90.0728690705123));
#138826=CARTESIAN_POINT('Ctrl Pts',(-6.12458201693739,3.41775547010891,
90.0645012299897));
#138827=CARTESIAN_POINT('Ctrl Pts',(-6.03260581313292,3.57760725501141,
90.0561333894672));
#138828=CARTESIAN_POINT('Ctrl Pts',(-5.93444279739089,3.73363298236389,
90.0477655489446));
#138829=CARTESIAN_POINT('Ctrl Pts',(-5.83631812851218,3.88959775909052,
90.0394009772747));
#138830=CARTESIAN_POINT('Ctrl Pts',(-5.73201164201851,4.04173918095292,
90.0310364056048));
#138831=CARTESIAN_POINT('Ctrl Pts',(-5.62185104212229,4.18956052858633,
90.0226718339349));
#138832=CARTESIAN_POINT('Ctrl Pts',(-5.51171735102954,4.33734576806858,
90.0143093054693));
#138833=CARTESIAN_POINT('Ctrl Pts',(-5.39573259483276,4.48081277470348,
90.0059467770038));
#138834=CARTESIAN_POINT('Ctrl Pts',(-5.27426674904466,4.61949529953456,
89.9975842485382));
#138835=CARTESIAN_POINT('Ctrl Pts',(-5.15279120990197,4.7581888916651,89.9892210527167));
#138836=CARTESIAN_POINT('Ctrl Pts',(-5.02583391929403,4.89209698795139,
89.9808578568952));
#138837=CARTESIAN_POINT('Ctrl Pts',(-4.89380445365022,5.02078724224929,
89.9724946610737));
#138838=CARTESIAN_POINT('Ctrl Pts',(-4.7617659838616,5.14948627296449,89.964130894899));
#138839=CARTESIAN_POINT('Ctrl Pts',(-4.62465488460112,5.27296652245633,
89.9557671287243));
#138840=CARTESIAN_POINT('Ctrl Pts',(-4.48291695154835,5.39083316084077,
89.9474033625496));
#138841=CARTESIAN_POINT('Ctrl Pts',(-4.34115045525196,5.50872355188926,
89.939037910896));
#138842=CARTESIAN_POINT('Ctrl Pts',(-4.19475551872813,5.62099786585151,
89.9306724592425));
#138843=CARTESIAN_POINT('Ctrl Pts',(-4.04421063405544,5.72730188744167,
89.9223070075889));
#138844=CARTESIAN_POINT('Ctrl Pts',(-3.89361533219721,5.8336415100394,89.9139387543621));
#138845=CARTESIAN_POINT('Ctrl Pts',(-3.73886757933855,5.9340066637545,89.9055705011352));
#138846=CARTESIAN_POINT('Ctrl Pts',(-3.58047477208355,6.0280865097453,89.8972022479084));
#138847=CARTESIAN_POINT('Ctrl Pts',(-3.42193511209877,6.12225358117543,
89.8888262361169));
#138848=CARTESIAN_POINT('Ctrl Pts',(-3.25974392746922,6.21012353196851,
89.8804502243254));
#138849=CARTESIAN_POINT('Ctrl Pts',(-3.09443422831232,6.29143094765803,
89.8720742125339));
#138850=CARTESIAN_POINT('Ctrl Pts',(-2.9290434592364,6.37277823750882,89.8636940930428));
#138851=CARTESIAN_POINT('Ctrl Pts',(-2.76053142352426,6.44755643510048,
89.8553139735517));
#138852=CARTESIAN_POINT('Ctrl Pts',(-2.58945162578366,6.51554808440751,
89.8469338540605));
#138853=CARTESIAN_POINT('Ctrl Pts',(-2.41817634770284,6.58361742278663,
89.8385441592213));
#138854=CARTESIAN_POINT('Ctrl Pts',(-2.24432775286241,6.64488460241677,
89.8301544643821));
#138855=CARTESIAN_POINT('Ctrl Pts',(-2.06847631044855,6.6991814660907,89.8217647695429));
#138856=CARTESIAN_POINT('Ctrl Pts',(-1.9568312642801,6.7336536078512,89.8164382970682));
#138857=CARTESIAN_POINT('Ctrl Pts',(-1.84437920556466,6.76531719248766,
89.8111118245934));
#138858=CARTESIAN_POINT('Ctrl Pts',(-1.7312683729505,6.79413985603191,89.8057853521187));
#138859=CARTESIAN_POINT('Ctrl Pts',(-1.55328643993815,6.83949283641063,
89.7974040517138));
#138860=CARTESIAN_POINT('Ctrl Pts',(-1.37331386192984,6.87790078047739,
89.7890227513088));
#138861=CARTESIAN_POINT('Ctrl Pts',(-1.1919184300438,6.90919365907643,89.7806414509039));
#138862=CARTESIAN_POINT('Ctrl Pts',(-1.01075289031331,6.94044687853279,
89.7722707725703));
#138863=CARTESIAN_POINT('Ctrl Pts',(-0.828168410677595,6.9646029478222,
89.7639000942367));
#138864=CARTESIAN_POINT('Ctrl Pts',(-0.6447463745845,6.98154199836685,89.7555294159031));
#138865=CARTESIAN_POINT('Ctrl Pts',(-0.461532491010622,6.9984618259974,
89.7471682368522));
#138866=CARTESIAN_POINT('Ctrl Pts',(-0.2774832696751,7.0081809286607,89.7388070578013));
#138867=CARTESIAN_POINT('Ctrl Pts',(-0.0931891295747852,7.01063066696778,
89.7304458787505));
#138868=CARTESIAN_POINT('Ctrl Pts',(0.0908658671394547,7.01307722645044,
89.7220955493157));
#138869=CARTESIAN_POINT('Ctrl Pts',(0.27516482263553,7.00827323207731,89.7137452198809));
#138870=CARTESIAN_POINT('Ctrl Pts',(0.459113446347169,6.99620192718044,
89.7053948904462));
#138871=CARTESIAN_POINT('Ctrl Pts',(0.642920532596751,6.98413991043057,
89.6970509860904));
#138872=CARTESIAN_POINT('Ctrl Pts',(0.826377498685339,6.96482174788211,
89.6887070817346));
#138873=CARTESIAN_POINT('Ctrl Pts',(1.00889015051672,6.93828272893879,89.6803631773788));
#138874=CARTESIAN_POINT('Ctrl Pts',(1.19125620704777,6.91176502630103,89.6720259748991));
#138875=CARTESIAN_POINT('Ctrl Pts',(1.37267913869814,6.87803808122752,89.6636887724193));
#138876=CARTESIAN_POINT('Ctrl Pts',(1.55256981482732,6.83718900810758,89.6553515699396));
#138877=CARTESIAN_POINT('Ctrl Pts',(1.61178883243007,6.82374171871939,89.6526070089038));
#138878=CARTESIAN_POINT('Ctrl Pts',(1.67084185142367,6.80952302811871,89.649862447868));
#138879=CARTESIAN_POINT('Ctrl Pts',(1.72970803380717,6.79453726756156,89.6471178868322));
#138880=CARTESIAN_POINT('Ctrl Pts',(1.90855065694298,6.74900870397534,89.6387795765303));
#138881=CARTESIAN_POINT('Ctrl Pts',(2.08552113086848,6.69643353800226,89.6304412662285));
#138882=CARTESIAN_POINT('Ctrl Pts',(2.26005401679071,6.63700100977001,89.6221029559267));
#138883=CARTESIAN_POINT('Ctrl Pts',(2.43469671288225,6.57753108860776,89.6137593994429));
#138884=CARTESIAN_POINT('Ctrl Pts',(2.6068984517586,6.51119530515688,89.6054158429592));
#138885=CARTESIAN_POINT('Ctrl Pts',(2.77611294520814,6.43823139363193,89.5970722864755));
#138886=CARTESIAN_POINT('Ctrl Pts',(2.94545617630687,6.36521197148107,89.5887223822503));
#138887=CARTESIAN_POINT('Ctrl Pts',(3.1118073281852,6.28555449240028,89.5803724780252));
#138888=CARTESIAN_POINT('Ctrl Pts',(3.27464352289054,6.19954323805319,89.5720225738));
#138889=CARTESIAN_POINT('Ctrl Pts',(3.43772395983796,6.11340297318947,89.5636601453365));
#138890=CARTESIAN_POINT('Ctrl Pts',(3.59727861417787,6.02089004190102,89.5552977168729));
#138891=CARTESIAN_POINT('Ctrl Pts',(3.75281118747542,5.92233355643359,89.5469352884093));
#138892=CARTESIAN_POINT('Ctrl Pts',(3.9084767623256,5.82369279173571,89.5385657089294));
#138893=CARTESIAN_POINT('Ctrl Pts',(4.06011312459827,5.71899834695406,89.5301961294495));
#138894=CARTESIAN_POINT('Ctrl Pts',(4.20725559064723,5.60862077140786,89.5218265499696));
#138895=CARTESIAN_POINT('Ctrl Pts',(4.35462500602218,5.49807295189981,89.5134440614331));
#138896=CARTESIAN_POINT('Ctrl Pts',(4.49748642074404,5.38182469186916,89.5050615728966));
#138897=CARTESIAN_POINT('Ctrl Pts',(4.63540959520822,5.26028558608291,89.4966790843601));
#138898=CARTESIAN_POINT('Ctrl Pts',(4.68054031790502,5.22051599912723,89.4939361967553));
#138899=CARTESIAN_POINT('Ctrl Pts',(4.72514260622551,5.18018020007441,89.4911933091506));
#138900=CARTESIAN_POINT('Ctrl Pts',(4.76920229736218,5.13929333754509,89.4884504215458));
#138901=CARTESIAN_POINT('Ctrl Pts',(4.90162926069797,5.01640271109265,89.4802063266168));
#138902=CARTESIAN_POINT('Ctrl Pts',(5.02944669541314,4.8882574675471,89.4719622316878));
#138903=CARTESIAN_POINT('Ctrl Pts',(5.15222035192789,4.7552341695946,89.4637181367589));
#138904=CARTESIAN_POINT('Ctrl Pts',(5.27488004436522,4.62233434990166,89.4554816943728));
#138905=CARTESIAN_POINT('Ctrl Pts',(5.39250505224846,4.48456574878959,89.4472452519867));
#138906=CARTESIAN_POINT('Ctrl Pts',(5.50469634452335,4.34234322884446,89.4390088096006));
#138907=CARTESIAN_POINT('Ctrl Pts',(5.61726331324664,4.19964447183946,89.4307447872005));
#138908=CARTESIAN_POINT('Ctrl Pts',(5.72435984436157,4.05246214411264,89.4224807648003));
#138909=CARTESIAN_POINT('Ctrl Pts',(5.8256212148699,3.90125159703367,89.4142167424001));
#138910=CARTESIAN_POINT('Ctrl Pts',(5.92639877746629,3.75076350570144,89.4059922039552));
#138911=CARTESIAN_POINT('Ctrl Pts',(6.02139661800876,3.59628589032516,89.3977676655103));
#138912=CARTESIAN_POINT('Ctrl Pts',(6.11029646720853,3.43829952815617,89.3895431270653));
#138913=CARTESIAN_POINT('Ctrl Pts',(6.19983649537233,3.27917548637834,89.3812593626875));
#138914=CARTESIAN_POINT('Ctrl Pts',(6.28319014380522,3.11649224588375,89.3729755983097));
#138915=CARTESIAN_POINT('Ctrl Pts',(6.36007755959843,2.95076939092035,89.3646918339319));
#138916=CARTESIAN_POINT('Ctrl Pts',(6.43696497539165,2.78504653595695,89.3564080695541));
#138917=CARTESIAN_POINT('Ctrl Pts',(6.5073859965539,2.61628438718322,89.3481243051763));
#138918=CARTESIAN_POINT('Ctrl Pts',(6.57110895151813,2.4450263208764,89.3398405407985));
#138919=CARTESIAN_POINT('Origin',(0.,0.,50.));
#138920=CARTESIAN_POINT('',(6.57110895151811,2.44502632087644,87.3401045918022));
#138921=CARTESIAN_POINT('',(6.57110895151812,2.44502632087643,87.8869151327864));
#138922=CARTESIAN_POINT('',(6.57110895151814,2.44502632087636,50.));
#138923=CARTESIAN_POINT('',(7.01124990260052,-0.00116866771971296,89.7735343568779));
#138924=CARTESIAN_POINT('Ctrl Pts',(6.57110895151811,2.44502632087643,87.8869151327864));
#138925=CARTESIAN_POINT('Ctrl Pts',(6.55483330766612,2.48876778414593,87.8890358985076));
#138926=CARTESIAN_POINT('Ctrl Pts',(6.53812136703552,2.53234545570068,87.8911566642287));
#138927=CARTESIAN_POINT('Ctrl Pts',(6.52097655319228,2.57575063917618,87.8932774299499));
#138928=CARTESIAN_POINT('Ctrl Pts',(6.45031461865716,2.75464405040101,87.9020181144463));
#138929=CARTESIAN_POINT('Ctrl Pts',(6.37228337420513,2.93063761010274,87.9107587989428));
#138930=CARTESIAN_POINT('Ctrl Pts',(6.28714218852269,3.1031386794338,87.9194994834392));
#138931=CARTESIAN_POINT('Ctrl Pts',(6.20201632115372,3.27560871295731,87.9282385953413));
#138932=CARTESIAN_POINT('Ctrl Pts',(6.10978318834393,3.44458726555738,87.9369777072434));
#138933=CARTESIAN_POINT('Ctrl Pts',(6.01074900218543,3.60950453597538,87.9457168191455));
#138934=CARTESIAN_POINT('Ctrl Pts',(5.91043168561388,3.77655854698285,87.9545691588197));
#138935=CARTESIAN_POINT('Ctrl Pts',(5.80313597975122,3.93944504675674,87.963421498494));
#138936=CARTESIAN_POINT('Ctrl Pts',(5.68922732022858,4.0975991826025,87.9722738381682));
#138937=CARTESIAN_POINT('Ctrl Pts',(5.57683327151467,4.25365038821803,87.9810084708182));
#138938=CARTESIAN_POINT('Ctrl Pts',(5.45800121358397,4.40509407827471,87.9897431034681));
#138939=CARTESIAN_POINT('Ctrl Pts',(5.33312531499311,4.55141746460152,87.9984777361181));
#138940=CARTESIAN_POINT('Ctrl Pts',(5.20572519397344,4.70069860961348,88.0073889293045));
#138941=CARTESIAN_POINT('Ctrl Pts',(5.07203446343468,4.84465000920222,88.0163001224909));
#138942=CARTESIAN_POINT('Ctrl Pts',(4.93251499830874,4.9827625223323,88.0252113156773));
#138943=CARTESIAN_POINT('Ctrl Pts',(4.79299553318281,5.12087503546238,88.0341225088637));
#138944=CARTESIAN_POINT('Ctrl Pts',(4.64764753941913,5.25314843930193,88.0430337020501));
#138945=CARTESIAN_POINT('Ctrl Pts',(4.49697370569427,5.37911275702549,88.0519448952365));
#138946=CARTESIAN_POINT('Ctrl Pts',(4.36127272085518,5.49255967443044,88.0599705600887));
#138947=CARTESIAN_POINT('Ctrl Pts',(4.22118909180023,5.60094084191064,88.0679962249411));
#138948=CARTESIAN_POINT('Ctrl Pts',(4.07714709029934,5.70390201235643,88.0760218897933));
#138949=CARTESIAN_POINT('Ctrl Pts',(3.93315080419664,5.80683050545215,88.0840450074965));
#138950=CARTESIAN_POINT('Ctrl Pts',(3.78519894466758,5.9043422133058,88.0920681251996));
#138951=CARTESIAN_POINT('Ctrl Pts',(3.63374754084468,5.99612419583728,88.1000912429027));
#138952=CARTESIAN_POINT('Ctrl Pts',(3.48231523636932,6.08789460385748,88.1081133488205));
#138953=CARTESIAN_POINT('Ctrl Pts',(3.32738458037922,6.17393653640493,88.1161354547382));
#138954=CARTESIAN_POINT('Ctrl Pts',(3.1694391085387,6.25398131591112,88.124157560656));
#138955=CARTESIAN_POINT('Ctrl Pts',(3.01143494362723,6.3340558403278,88.1321826476154));
#138956=CARTESIAN_POINT('Ctrl Pts',(2.85041405075633,6.4081285912004,88.1402077345748));
#138957=CARTESIAN_POINT('Ctrl Pts',(2.68688341074461,6.47597746286732,88.1482328215342));
#138958=CARTESIAN_POINT('Ctrl Pts',(2.52332056419156,6.54383969703003,88.1562594889944));
#138959=CARTESIAN_POINT('Ctrl Pts',(2.35724732775964,6.60547547772827,88.1642861564545));
#138960=CARTESIAN_POINT('Ctrl Pts',(2.18918882383458,6.66071158781836,88.1723128239147));
#138961=CARTESIAN_POINT('Ctrl Pts',(2.02099540313495,6.71599204126293,88.1803459351552));
#138962=CARTESIAN_POINT('Ctrl Pts',(1.85081388286993,6.76486245735372,88.1883790463957));
#138963=CARTESIAN_POINT('Ctrl Pts',(1.67918324413966,6.80719987917944,88.1964121576362));
#138964=CARTESIAN_POINT('Ctrl Pts',(1.57805223696294,6.83214662611331,88.2011455585984));
#138965=CARTESIAN_POINT('Ctrl Pts',(1.47641830823632,6.85482608659915,88.2058789595606));
#138966=CARTESIAN_POINT('Ctrl Pts',(1.37439299910715,6.87522148345094,88.2106123605228));
#138967=CARTESIAN_POINT('Ctrl Pts',(1.16421768708813,6.9172366357074,88.220363313817));
#138968=CARTESIAN_POINT('Ctrl Pts',(0.952257338295142,6.94958151096976,
88.2301142671112));
#138969=CARTESIAN_POINT('Ctrl Pts',(0.739323485856769,6.97216088065677,
88.2398652204054));
#138970=CARTESIAN_POINT('Ctrl Pts',(0.526082862258542,6.9947727801616,88.2496302217771));
#138971=CARTESIAN_POINT('Ctrl Pts',(0.311865967991078,7.00759102779147,
88.2593952231488));
#138972=CARTESIAN_POINT('Ctrl Pts',(0.097490257987396,7.01057217437333,
88.2691602245204));
#138973=CARTESIAN_POINT('Ctrl Pts',(-0.11652813212578,7.01354835200152,
88.2789089496581));
#138974=CARTESIAN_POINT('Ctrl Pts',(-0.33070477101601,7.00672019781765,
88.2886576747957));
#138975=CARTESIAN_POINT('Ctrl Pts',(-0.544224464783171,6.99009630079811,
88.2984063999334));
#138976=CARTESIAN_POINT('Ctrl Pts',(-0.757158129782745,6.97351802993002,
88.3081283686006));
#138977=CARTESIAN_POINT('Ctrl Pts',(-0.969438409359905,6.94719769186361,
88.3178503372678));
#138978=CARTESIAN_POINT('Ctrl Pts',(-1.18025558019842,6.91119550641642,
88.327572305935));
#138979=CARTESIAN_POINT('Ctrl Pts',(-1.38967782887983,6.87543153802709,
88.3372299468748));
#138980=CARTESIAN_POINT('Ctrl Pts',(-1.59765621597616,6.83011340267251,
88.3468875878145));
#138981=CARTESIAN_POINT('Ctrl Pts',(-1.80339645972762,6.77535148693718,
88.3565452287543));
#138982=CARTESIAN_POINT('Ctrl Pts',(-1.89382638005402,6.75128173963559,
88.3607900944393));
#138983=CARTESIAN_POINT('Ctrl Pts',(-1.98382391001562,6.72538821539914,
88.3650349601243));
#138984=CARTESIAN_POINT('Ctrl Pts',(-2.0733216145128,6.69768348351085,88.3692798258093));
#138985=CARTESIAN_POINT('Ctrl Pts',(-2.23886802656909,6.64643726455077,
88.3771316728232));
#138986=CARTESIAN_POINT('Ctrl Pts',(-2.40263517021789,6.58901142800105,
88.3849835198372));
#138987=CARTESIAN_POINT('Ctrl Pts',(-2.56411245436094,6.52556157613206,
88.3928353668511));
#138988=CARTESIAN_POINT('Ctrl Pts',(-2.72554394485167,6.4621297181281,88.4006849871448));
#138989=CARTESIAN_POINT('Ctrl Pts',(-2.88468651288709,6.39267738239819,
88.4085346074384));
#138990=CARTESIAN_POINT('Ctrl Pts',(-3.04104683841114,6.31740933366595,
88.416384227732));
#138991=CARTESIAN_POINT('Ctrl Pts',(-3.19739468056335,6.24214729412458,
88.4242332213339));
#138992=CARTESIAN_POINT('Ctrl Pts',(-3.35096037900811,6.16107063202598,
88.4320822149357));
#138993=CARTESIAN_POINT('Ctrl Pts',(-3.50127287565799,6.0744312336779,88.4399312085376));
#138994=CARTESIAN_POINT('Ctrl Pts',(-3.65166147112327,5.98774797233953,
88.447784175855));
#138995=CARTESIAN_POINT('Ctrl Pts',(-3.79879324307845,5.89549653848571,
88.4556371431725));
#138996=CARTESIAN_POINT('Ctrl Pts',(-3.94222363728883,5.79797372847629,
88.46349011049));
#138997=CARTESIAN_POINT('Ctrl Pts',(-4.08569045799994,5.70042615094998,
88.4713450721973));
#138998=CARTESIAN_POINT('Ctrl Pts',(-4.22545372090904,5.59760475624016,
88.4792000339046));
#138999=CARTESIAN_POINT('Ctrl Pts',(-4.36110046444975,5.48984783955587,
88.4870549956119));
#139000=CARTESIAN_POINT('Ctrl Pts',(-4.49688184872204,5.38198396512444,
88.4949177540253));
#139001=CARTESIAN_POINT('Ctrl Pts',(-4.62853826331798,5.26917503242696,
88.5027805124387));
#139002=CARTESIAN_POINT('Ctrl Pts',(-4.75569182611874,5.15179792087068,
88.5106432708521));
#139003=CARTESIAN_POINT('Ctrl Pts',(-4.84896985523927,5.06569175609898,
88.5164112775999));
#139004=CARTESIAN_POINT('Ctrl Pts',(-4.93982542595665,4.97712803729308,
88.5221792843478));
#139005=CARTESIAN_POINT('Ctrl Pts',(-5.02812298621087,4.88626706167785,
88.5279472910957));
#139006=CARTESIAN_POINT('Ctrl Pts',(-5.15637575336652,4.75429091742694,
88.5363253575367));
#139007=CARTESIAN_POINT('Ctrl Pts',(-5.27951448298897,4.61717463325797,
88.5447034239777));
#139008=CARTESIAN_POINT('Ctrl Pts',(-5.39712312308541,4.47534228375403,
88.5530814904187));
#139009=CARTESIAN_POINT('Ctrl Pts',(-5.51465134379118,4.33360691752544,
88.5614538280374));
#139010=CARTESIAN_POINT('Ctrl Pts',(-5.62665680482392,4.18716216747682,
88.5698261656562));
#139011=CARTESIAN_POINT('Ctrl Pts',(-5.7327618889856,4.03646722849254,88.5781985032749));
#139012=CARTESIAN_POINT('Ctrl Pts',(-5.83880998013208,3.88585323340474,
88.5865663437974));
#139013=CARTESIAN_POINT('Ctrl Pts',(-5.93896382489068,3.73099386951992,
88.59493418432));
#139014=CARTESIAN_POINT('Ctrl Pts',(-6.03288724599317,3.57237988456337,
88.6033020248426));
#139015=CARTESIAN_POINT('Ctrl Pts',(-6.12677397640755,3.41382786132182,
88.6116665965125));
#139016=CARTESIAN_POINT('Ctrl Pts',(-6.21443496943469,3.25152442428976,
88.6200311681824));
#139017=CARTESIAN_POINT('Ctrl Pts',(-6.29557815673689,3.08598804840805,
88.6283957398523));
#139018=CARTESIAN_POINT('Ctrl Pts',(-6.37670152328574,2.92049210790714,
88.6367582683179));
#139019=CARTESIAN_POINT('Ctrl Pts',(-6.45131011497981,2.75176509848601,
88.6451207967834));
#139020=CARTESIAN_POINT('Ctrl Pts',(-6.51915828324742,2.58034917026099,
88.653483325249));
#139021=CARTESIAN_POINT('Ctrl Pts',(-6.58701186601111,2.40891956250863,
88.6618465210705));
#139022=CARTESIAN_POINT('Ctrl Pts',(-6.64810382092013,2.23480091062192,
88.670209716892));
#139023=CARTESIAN_POINT('Ctrl Pts',(-6.70223675191771,2.05855509611562,
88.6785729127135));
#139024=CARTESIAN_POINT('Ctrl Pts',(-6.75637337467263,1.88229726199818,
88.6869366788881));
#139025=CARTESIAN_POINT('Ctrl Pts',(-6.80354993041998,1.70391229025803,
88.6953004450628));
#139026=CARTESIAN_POINT('Ctrl Pts',(-6.84361894436214,1.52397713462755,
88.7036642112375));
#139027=CARTESIAN_POINT('Ctrl Pts',(-6.88369603307284,1.34400571819127,
88.7120296628911));
#139028=CARTESIAN_POINT('Ctrl Pts',(-6.9166626524395,1.16248381586834,88.7203951145446));
#139029=CARTESIAN_POINT('Ctrl Pts',(-6.94242239497053,0.979998904240033,
88.7287605661981));
#139030=CARTESIAN_POINT('Ctrl Pts',(-6.9681907643887,0.797452878773525,
88.737128819425));
#139031=CARTESIAN_POINT('Ctrl Pts',(-6.98674739830947,0.61394352633423,
88.7454970726519));
#139032=CARTESIAN_POINT('Ctrl Pts',(-6.99804768035478,0.430064211462848,
88.7538653258787));
#139033=CARTESIAN_POINT('Ctrl Pts',(-7.00935843937369,0.246014414233438,
88.7622413376702));
#139034=CARTESIAN_POINT('Ctrl Pts',(-7.01339938243069,0.0615942976434029,
88.7706173494616));
#139035=CARTESIAN_POINT('Ctrl Pts',(-7.01017800193812,-0.122600748948895,
88.7789933612531));
#139036=CARTESIAN_POINT('Ctrl Pts',(-7.00695504164076,-0.306886127067796,
88.7873734807442));
#139037=CARTESIAN_POINT('Ctrl Pts',(-6.99646266769394,-0.490945886667178,
88.7957536002354));
#139038=CARTESIAN_POINT('Ctrl Pts',(-6.97876039602643,-0.674188324841817,
88.8041337197265));
#139039=CARTESIAN_POINT('Ctrl Pts',(-6.96103789727112,-0.857640140714186,
88.8125234145657));
#139040=CARTESIAN_POINT('Ctrl Pts',(-6.93608907723636,-1.04027244236608,
88.8209131094049));
#139041=CARTESIAN_POINT('Ctrl Pts',(-6.90402505451861,-1.22150096564813,
88.8293028042441));
#139042=CARTESIAN_POINT('Ctrl Pts',(-6.88366815981473,-1.33655982767137,
88.8346292767189));
#139043=CARTESIAN_POINT('Ctrl Pts',(-6.86044432726614,-1.45105306635245,
88.8399557491938));
#139044=CARTESIAN_POINT('Ctrl Pts',(-6.83439251135128,-1.56483403697823,
88.8452822216686));
#139045=CARTESIAN_POINT('Ctrl Pts',(-6.7933995096405,-1.74387044421985,
88.8536635220735));
#139046=CARTESIAN_POINT('Ctrl Pts',(-6.74531936724503,-1.92150377135421,
88.8620448224783));
#139047=CARTESIAN_POINT('Ctrl Pts',(-6.69026031388915,-2.09715128088078,
88.8704261228831));
#139048=CARTESIAN_POINT('Ctrl Pts',(-6.63527103982333,-2.27257618290196,
88.8787968012167));
#139049=CARTESIAN_POINT('Ctrl Pts',(-6.57332057867142,-2.44601997278679,
88.8871674795502));
#139050=CARTESIAN_POINT('Ctrl Pts',(-6.50456798830475,-2.61691074513846,
88.8955381578837));
#139051=CARTESIAN_POINT('Ctrl Pts',(-6.4358934203239,-2.78760758580401,
88.9038993369344));
#139052=CARTESIAN_POINT('Ctrl Pts',(-6.36043222999064,-2.95575688132307,
88.9122605159852));
#139053=CARTESIAN_POINT('Ctrl Pts',(-6.27839317148957,-3.12080209989245,
88.920621695036));
#139054=CARTESIAN_POINT('Ctrl Pts',(-6.19646056834422,-3.28563315282204,
88.9289720244706));
#139055=CARTESIAN_POINT('Ctrl Pts',(-6.10796726726344,-3.44736787086974,
88.9373223539053));
#139056=CARTESIAN_POINT('Ctrl Pts',(-6.01316994023207,-3.60546998772552,
88.94567268334));
#139057=CARTESIAN_POINT('Ctrl Pts',(-5.91844555407317,-3.76345045445989,
88.9540165876956));
#139058=CARTESIAN_POINT('Ctrl Pts',(-5.81742697604407,-3.91780361025139,
88.9623604920514));
#139059=CARTESIAN_POINT('Ctrl Pts',(-5.71041712792692,-4.06801705841788,
88.970704396407));
#139060=CARTESIAN_POINT('Ctrl Pts',(-5.60349323078715,-4.21810985420599,
88.9790415988867));
#139061=CARTESIAN_POINT('Ctrl Pts',(-5.49058785041384,-4.36406930759813,
88.9873788013663));
#139062=CARTESIAN_POINT('Ctrl Pts',(-5.37204769194044,-4.50541120853773,
88.995716003846));
#139063=CARTESIAN_POINT('Ctrl Pts',(-5.33302492609325,-4.55194018214291,
88.9984605648823));
#139064=CARTESIAN_POINT('Ctrl Pts',(-5.29339187258074,-4.59796899144018,
89.0012051259186));
#139065=CARTESIAN_POINT('Ctrl Pts',(-5.2531619064357,-4.64348108074889,
89.0039496869549));
#139066=CARTESIAN_POINT('Ctrl Pts',(-5.1309383753439,-4.78175234457795,
89.0122879972569));
#139067=CARTESIAN_POINT('Ctrl Pts',(-5.00330256798195,-4.9151382411288,
89.0206263075589));
#139068=CARTESIAN_POINT('Ctrl Pts',(-4.87068120155903,-5.04322230278217,
89.0289646178609));
#139069=CARTESIAN_POINT('Ctrl Pts',(-4.73797639427257,-5.17138695058088,
89.0373081743447));
#139070=CARTESIAN_POINT('Ctrl Pts',(-4.60028000697832,-5.29424288232747,
89.0456517308286));
#139071=CARTESIAN_POINT('Ctrl Pts',(-4.45805313999055,-5.4114128250874,
89.0539952873125));
#139072=CARTESIAN_POINT('Ctrl Pts',(-4.3157180674225,-5.52867191022891,
89.0623451915377));
#139073=CARTESIAN_POINT('Ctrl Pts',(-4.16884589258228,-5.64023616957493,
89.070695095763));
#139074=CARTESIAN_POINT('Ctrl Pts',(-4.01792842082438,-5.74577042420176,
89.0790449999882));
#139075=CARTESIAN_POINT('Ctrl Pts',(-3.86678458402651,-5.85146297240116,
89.087407428452));
#139076=CARTESIAN_POINT('Ctrl Pts',(-3.71158359399111,-5.95110725407478,
89.0957698569157));
#139077=CARTESIAN_POINT('Ctrl Pts',(-3.55284498571996,-6.04441221873099,
89.1041322853794));
#139078=CARTESIAN_POINT('Ctrl Pts',(-3.39397063429936,-6.13779697185141,
89.1125018648594));
#139079=CARTESIAN_POINT('Ctrl Pts',(-3.23155291680686,-6.22483143730628,
89.1208714443395));
#139080=CARTESIAN_POINT('Ctrl Pts',(-3.06613377843793,-6.30527162105028,
89.1292410238195));
#139081=CARTESIAN_POINT('Ctrl Pts',(-2.90045950120278,-6.38583587397684,
89.1376235123561));
#139082=CARTESIAN_POINT('Ctrl Pts',(-2.73177485181647,-6.45978538945171,
89.1460060008928));
#139083=CARTESIAN_POINT('Ctrl Pts',(-2.56064076546608,-6.52692465352047,
89.1543884894294));
#139084=CARTESIAN_POINT('Ctrl Pts',(-2.50464288822122,-6.54889372086299,
89.1571313770334));
#139085=CARTESIAN_POINT('Ctrl Pts',(-2.44838285924254,-6.57013401149291,
89.1598742646375));
#139086=CARTESIAN_POINT('Ctrl Pts',(-2.39188062497519,-6.59063985045218,
89.1626171522415));
#139087=CARTESIAN_POINT('Ctrl Pts',(-2.2190534338493,-6.65336244177911,
89.1710070073743));
#139088=CARTESIAN_POINT('Ctrl Pts',(-2.04361021329518,-6.70933634883609,
89.1793968625071));
#139089=CARTESIAN_POINT('Ctrl Pts',(-1.86610484110356,-6.75834885785795,
89.1877867176399));
#139090=CARTESIAN_POINT('Ctrl Pts',(-1.68876326838081,-6.80731613882364,
89.1961688307319));
#139091=CARTESIAN_POINT('Ctrl Pts',(-1.5093636528376,-6.84933474068121,
89.204550943824));
#139092=CARTESIAN_POINT('Ctrl Pts',(-1.32847692186191,-6.88424110781866,
89.2129330569161));
#139093=CARTESIAN_POINT('Ctrl Pts',(-1.14773052065156,-6.91912039501342,
89.221308667265));
#139094=CARTESIAN_POINT('Ctrl Pts',(-0.965499625721542,-6.94689838581216,
89.2296842776139));
#139095=CARTESIAN_POINT('Ctrl Pts',(-0.782367750468291,-6.96746203904458,
89.2380598879627));
#139096=CARTESIAN_POINT('Ctrl Pts',(-0.599351067884293,-6.98801275743371,
89.2464302299283));
#139097=CARTESIAN_POINT('Ctrl Pts',(-0.415434860817747,-7.00135814988565,
89.2548005718939));
#139098=CARTESIAN_POINT('Ctrl Pts',(-0.231210660257582,-7.0074366349674,
89.2631709138595));
#139099=CARTESIAN_POINT('Ctrl Pts',(-0.0470753342562295,-7.01351218762942,
89.2715372177538));
#139100=CARTESIAN_POINT('Ctrl Pts',(0.137367360978798,-7.01232781312482,
89.2799035216481));
#139101=CARTESIAN_POINT('Ctrl Pts',(0.321522512185865,-7.00387391638782,
89.2882698255424));
#139102=CARTESIAN_POINT('Ctrl Pts',(0.505626160358737,-6.9954223839688,
89.296633789616));
#139103=CARTESIAN_POINT('Ctrl Pts',(0.689442096770567,-6.97970539686847,
89.3049977536896));
#139104=CARTESIAN_POINT('Ctrl Pts',(0.872376589459558,-6.95676545879354,
89.3133617177632));
#139105=CARTESIAN_POINT('Ctrl Pts',(1.05528293157012,-6.93382905079387,
89.3217243947617));
#139106=CARTESIAN_POINT('Ctrl Pts',(1.23730777438678,-6.90367194879413,
89.3300870717603));
#139107=CARTESIAN_POINT('Ctrl Pts',(1.41786325977379,-6.866388449475,89.3384497487588));
#139108=CARTESIAN_POINT('Ctrl Pts',(1.59841502785335,-6.82910571775498,
89.3468122535851));
#139109=CARTESIAN_POINT('Ctrl Pts',(1.77749717704757,-6.78469694812975,
89.3551747584114));
#139110=CARTESIAN_POINT('Ctrl Pts',(1.95453235461152,-6.73330749611784,
89.3635372632377));
#139111=CARTESIAN_POINT('Ctrl Pts',(2.13158748487358,-6.68191225227273,
89.3719007105576));
#139112=CARTESIAN_POINT('Ctrl Pts',(2.30659486809076,-6.62353484960551,
89.3802641578776));
#139113=CARTESIAN_POINT('Ctrl Pts',(2.47899220149334,-6.55837054667051,
89.3886276051976));
#139114=CARTESIAN_POINT('Ctrl Pts',(2.65149104729088,-6.49316787316256,
89.3969959771504));
#139115=CARTESIAN_POINT('Ctrl Pts',(2.821376464151,-6.42117042921992,89.4053643491032));
#139116=CARTESIAN_POINT('Ctrl Pts',(2.98810506373111,-6.34262206745795,
89.413732721056));
#139117=CARTESIAN_POINT('Ctrl Pts',(3.15488361955717,-6.26405017055391,
89.4221036003917));
#139118=CARTESIAN_POINT('Ctrl Pts',(3.31850317695323,-6.17892358688698,
89.4304744797274));
#139119=CARTESIAN_POINT('Ctrl Pts',(3.47844422945862,-6.08753253010167,
89.4388453590632));
#139120=CARTESIAN_POINT('Ctrl Pts',(3.63852079828832,-5.99606403866218,
89.4472233309544));
#139121=CARTESIAN_POINT('Ctrl Pts',(3.79491235147865,-5.8983206359863,89.4556013028457));
#139122=CARTESIAN_POINT('Ctrl Pts',(3.94712670688908,-5.79463694481915,
89.463979274737));
#139123=CARTESIAN_POINT('Ctrl Pts',(4.04386016924046,-5.72874511478165,
89.4693035440961));
#139124=CARTESIAN_POINT('Ctrl Pts',(4.13890717369779,-5.66045504662359,
89.4746278134552));
#139125=CARTESIAN_POINT('Ctrl Pts',(4.23214814517178,-5.58986123618637,
89.4799520828143));
#139126=CARTESIAN_POINT('Ctrl Pts',(4.36984553972061,-5.48560895722776,
89.4878149140036));
#139127=CARTESIAN_POINT('Ctrl Pts',(4.50388872817933,-5.37611348052323,
89.4956777451928));
#139128=CARTESIAN_POINT('Ctrl Pts',(4.63383618386507,-5.26167167196917,
89.5035405763821));
#139129=CARTESIAN_POINT('Ctrl Pts',(4.76368379208412,-5.14731779683873,
89.5113973660235));
#139130=CARTESIAN_POINT('Ctrl Pts',(4.88944164157191,-5.02802539826377,
89.5192541556649));
#139131=CARTESIAN_POINT('Ctrl Pts',(5.0106985497752,-4.90413362438063,89.5271109453062));
#139132=CARTESIAN_POINT('Ctrl Pts',(5.13188707482215,-4.78031171959336,
89.5349633040902));
#139133=CARTESIAN_POINT('Ctrl Pts',(5.24857944202502,-4.65189587085254,
89.5428156628741));
#139134=CARTESIAN_POINT('Ctrl Pts',(5.36039904202529,-4.51926417381794,
89.5506680216581));
#139135=CARTESIAN_POINT('Ctrl Pts',(5.47219224011345,-4.38666379267438,
89.5585185264085));
#139136=CARTESIAN_POINT('Ctrl Pts',(5.57911470886249,-4.24984983017631,
89.5663690311589));
#139137=CARTESIAN_POINT('Ctrl Pts',(5.68082814214389,-4.1092357174937,89.5742195359094));
#139138=CARTESIAN_POINT('Ctrl Pts',(5.78252521293952,-3.96864422519018,
89.582068777761));
#139139=CARTESIAN_POINT('Ctrl Pts',(5.87901469524462,-3.82425411056422,
89.5899180196126));
#139140=CARTESIAN_POINT('Ctrl Pts',(5.97000016640154,-3.67650983619867,
89.5977672614642));
#139141=CARTESIAN_POINT('Ctrl Pts',(6.06101629234464,-3.52871578389516,
89.6056191478791));
#139142=CARTESIAN_POINT('Ctrl Pts',(6.14652450283191,-3.37756563973382,
89.6134710342939));
#139143=CARTESIAN_POINT('Ctrl Pts',(6.22627301396429,-3.22353081543826,
89.6213229207088));
#139144=CARTESIAN_POINT('Ctrl Pts',(6.28483135307921,-3.11042496119059,
89.6270884631728));
#139145=CARTESIAN_POINT('Ctrl Pts',(6.3402851136845,-2.99576432463122,89.6328540056367));
#139146=CARTESIAN_POINT('Ctrl Pts',(6.39255086948626,-2.87974303428804,
89.6386195481007));
#139147=CARTESIAN_POINT('Ctrl Pts',(6.47849319973308,-2.68896534634728,
89.6481000223977));
#139148=CARTESIAN_POINT('Ctrl Pts',(6.55577935381089,-2.4945874012626,89.6575804966947));
#139149=CARTESIAN_POINT('Ctrl Pts',(6.62418441874926,-2.29734789461664,
89.6670609709917));
#139150=CARTESIAN_POINT('Ctrl Pts',(6.69302324126454,-2.09885768920228,
89.6766015611231));
#139151=CARTESIAN_POINT('Ctrl Pts',(6.75286798945196,-1.89746962490714,
89.6861421512546));
#139152=CARTESIAN_POINT('Ctrl Pts',(6.80354173911682,-1.69394402699595,
89.695682741386));
#139153=CARTESIAN_POINT('Ctrl Pts',(6.85433638479804,-1.48993286339886,
89.7052460931908));
#139154=CARTESIAN_POINT('Ctrl Pts',(6.89591623823064,-1.28377405662141,
89.7148094449957));
#139155=CARTESIAN_POINT('Ctrl Pts',(6.92815527618832,-1.07623930030637,
89.7243727968005));
#139156=CARTESIAN_POINT('Ctrl Pts',(6.9604478597256,-0.868359851050176,
89.7339520323056));
#139157=CARTESIAN_POINT('Ctrl Pts',(6.98336857798893,-0.659099972771663,
89.7435312678107));
#139158=CARTESIAN_POINT('Ctrl Pts',(6.99684288020564,-0.449239660109893,
89.7531105033158));
#139159=CARTESIAN_POINT('Ctrl Pts',(7.00641905063446,-0.300092187537877,
89.7599184545032));
#139160=CARTESIAN_POINT('Ctrl Pts',(7.0112249877683,-0.150641534984156,
89.7667264056905));
#139161=CARTESIAN_POINT('Ctrl Pts',(7.01124990260052,-0.00116866771990912,
89.7735343568778));
#139162=CARTESIAN_POINT('Ctrl Pts',(7.01124990260064,-0.00116866700483817,
89.7735343569104));
#139163=CARTESIAN_POINT('Ctrl Pts',(7.01127887818485,0.172666190259039,
89.7814519090693));
#139164=CARTESIAN_POINT('Ctrl Pts',(7.00484218383642,0.346555053651736,
89.7893694612282));
#139165=CARTESIAN_POINT('Ctrl Pts',(6.99193196050225,0.520109625182234,
89.7972870133871));
#139166=CARTESIAN_POINT('Ctrl Pts',(6.97883374054472,0.696191470840531,
89.805319859684));
#139167=CARTESIAN_POINT('Ctrl Pts',(6.95906597300057,0.871962073712557,
89.8133527059809));
#139168=CARTESIAN_POINT('Ctrl Pts',(6.93265382099713,1.04687036480829,89.8213855522778));
#139169=CARTESIAN_POINT('Ctrl Pts',(6.90625792285003,1.22167101854697,89.8294134552165));
#139170=CARTESIAN_POINT('Ctrl Pts',(6.87322583208172,1.39561005565585,89.8374413581551));
#139171=CARTESIAN_POINT('Ctrl Pts',(6.83363461634404,1.56814045697588,89.8454692610938));
#139172=CARTESIAN_POINT('Ctrl Pts',(6.79406011725628,1.74059801056267,89.8534937744006));
#139173=CARTESIAN_POINT('Ctrl Pts',(6.74793208756169,1.91164775566082,89.8615182877075));
#139174=CARTESIAN_POINT('Ctrl Pts',(6.69537887420091,2.08075185771975,89.8695428010143));
#139175=CARTESIAN_POINT('Ctrl Pts',(6.65730511031184,2.20326443578542,89.8753564022279));
#139176=CARTESIAN_POINT('Ctrl Pts',(6.61586002755452,2.32475596066717,89.8811700034414));
#139177=CARTESIAN_POINT('Ctrl Pts',(6.57110895151814,2.44502632087636,89.8869836046549));
#139178=CARTESIAN_POINT('',(7.01124998073505,-0.000519752638901176,89.2264656431278));
#139179=CARTESIAN_POINT('Ctrl Pts',(6.57110895151813,2.4450263208764,89.3398405407985));
#139180=CARTESIAN_POINT('Ctrl Pts',(6.63433766300281,2.27509655427943,89.3316210263686));
#139181=CARTESIAN_POINT('Ctrl Pts',(6.69097174824357,2.10270978866334,89.3234015119385));
#139182=CARTESIAN_POINT('Ctrl Pts',(6.74083387325627,1.92841521868627,89.3151819975085));
#139183=CARTESIAN_POINT('Ctrl Pts',(6.79071773222913,1.75404467699245,89.3069589003472));
#139184=CARTESIAN_POINT('Ctrl Pts',(6.83382363633967,1.57776500168886,89.2987358031858));
#139185=CARTESIAN_POINT('Ctrl Pts',(6.87002445706047,1.40013946515733,89.2905127060244));
#139186=CARTESIAN_POINT('Ctrl Pts',(6.90623358362138,1.22247317459653,89.282287722173));
#139187=CARTESIAN_POINT('Ctrl Pts',(6.93553440626854,1.043460747489,89.2740627383215));
#139188=CARTESIAN_POINT('Ctrl Pts',(6.95785121770788,0.863674125316405,
89.26583775447));
#139189=CARTESIAN_POINT('Ctrl Pts',(6.9801856822653,0.683745287734539,89.2576062644646));
#139190=CARTESIAN_POINT('Ctrl Pts',(6.99552506285632,0.503041375759832,
89.2493747744591));
#139191=CARTESIAN_POINT('Ctrl Pts',(7.00384559704583,0.322138813621992,
89.2411432844537));
#139192=CARTESIAN_POINT('Ctrl Pts',(7.00879106930715,0.214615837010341,
89.2362507373451));
#139193=CARTESIAN_POINT('Ctrl Pts',(7.01125795299141,0.10702271672289,89.2313581902364));
#139194=CARTESIAN_POINT('Ctrl Pts',(7.01124998073505,-0.000519752639105816,
89.2264656431278));
#139195=CARTESIAN_POINT('Ctrl Pts',(7.01124998073499,-0.000519753477888864,
89.2264656430896));
#139196=CARTESIAN_POINT('Ctrl Pts',(7.0112254927832,-0.330851648839633,
89.2114374931025));
#139197=CARTESIAN_POINT('Ctrl Pts',(6.98785181831592,-0.660634656290872,
89.1964093431154));
#139198=CARTESIAN_POINT('Ctrl Pts',(6.9413845472389,-0.987323214480959,
89.1813811931284));
#139199=CARTESIAN_POINT('Ctrl Pts',(6.93080397754665,-1.06171000280479,
89.1779592924099));
#139200=CARTESIAN_POINT('Ctrl Pts',(6.9190262741439,-1.13593643033091,89.1745373916915));
#139201=CARTESIAN_POINT('Ctrl Pts',(6.9060548208089,-1.20997246848107,89.171115490973));
#139202=CARTESIAN_POINT('Ctrl Pts',(6.87624906189091,-1.38009221122353,
89.1632526597835));
#139203=CARTESIAN_POINT('Ctrl Pts',(6.84010970381206,-1.54935763176299,
89.155389828594));
#139204=CARTESIAN_POINT('Ctrl Pts',(6.79769903530169,-1.71724034076727,
89.1475269974045));
#139205=CARTESIAN_POINT('Ctrl Pts',(6.75532095379201,-1.8849940540696,89.1396702077629));
#139206=CARTESIAN_POINT('Ctrl Pts',(6.70668123725754,-2.05136680136492,
89.1318134181213));
#139207=CARTESIAN_POINT('Ctrl Pts',(6.65189365013445,-2.21583786180331,
89.1239566284797));
#139208=CARTESIAN_POINT('Ctrl Pts',(6.59713696061686,-2.38021616834961,
89.1161042696955));
#139209=CARTESIAN_POINT('Ctrl Pts',(6.53623941750465,-2.54269456080801,
89.1082519109113));
#139210=CARTESIAN_POINT('Ctrl Pts',(6.46936522736334,-2.70276527236126,
89.1003995521271));
#139211=CARTESIAN_POINT('Ctrl Pts',(6.40250682699863,-2.86279818935177,
89.0925490473765));
#139212=CARTESIAN_POINT('Ctrl Pts',(6.3296747272547,-3.02042420213621,89.0846985426258));
#139213=CARTESIAN_POINT('Ctrl Pts',(6.25108206855452,-3.17515346632192,
89.0768480378752));
#139214=CARTESIAN_POINT('Ctrl Pts',(6.17250205293624,-3.3298578394454,89.0689987960233));
#139215=CARTESIAN_POINT('Ctrl Pts',(6.08816349859701,-3.48166605282902,
89.0611495541715));
#139216=CARTESIAN_POINT('Ctrl Pts',(5.99832628749871,-3.63011133592374,
89.0533003123196));
#139217=CARTESIAN_POINT('Ctrl Pts',(5.90845880848544,-3.7786066331401,89.0454484259046));
#139218=CARTESIAN_POINT('Ctrl Pts',(5.81308916995875,-3.92373641020055,
89.0375965394895));
#139219=CARTESIAN_POINT('Ctrl Pts',(5.71252162342565,-4.06506128667138,
89.0297446530744));
#139220=CARTESIAN_POINT('Ctrl Pts',(5.63867612576406,-4.16883438440243,
89.0239791106118));
#139221=CARTESIAN_POINT('Ctrl Pts',(5.56202896335448,-4.27055652372627,
89.0182135681491));
#139222=CARTESIAN_POINT('Ctrl Pts',(5.48271468558665,-4.37006478658526,
89.0124480256864));
#139223=CARTESIAN_POINT('Ctrl Pts',(5.34989049828883,-4.53670696647567,
89.0027927213265));
#139224=CARTESIAN_POINT('Ctrl Pts',(5.20965370605494,-4.6970549548856,88.9931374169666));
#139225=CARTESIAN_POINT('Ctrl Pts',(5.06258545705823,-4.85055203584938,
88.9834821126067));
#139226=CARTESIAN_POINT('Ctrl Pts',(4.91470247755191,-5.00489946184581,
88.973773319672));
#139227=CARTESIAN_POINT('Ctrl Pts',(4.75991221379916,-5.15231986845056,
88.9640645267373));
#139228=CARTESIAN_POINT('Ctrl Pts',(4.59883503057965,-5.29229089563428,
88.9543557338025));
#139229=CARTESIAN_POINT('Ctrl Pts',(4.43698273027734,-5.43293547528582,
88.9446002213318));
#139230=CARTESIAN_POINT('Ctrl Pts',(4.26878290694304,-5.56605879865805,
88.9348447088611));
#139231=CARTESIAN_POINT('Ctrl Pts',(4.09489371856678,-5.69117492229349,
88.9250891963904));
#139232=CARTESIAN_POINT('Ctrl Pts',(3.92083235314166,-5.8164149301401,88.9153240244615));
#139233=CARTESIAN_POINT('Ctrl Pts',(3.74107039234419,-5.9336318663998,88.9055588525326));
#139234=CARTESIAN_POINT('Ctrl Pts',(3.55629603072071,-6.0423824030245,88.8957936806036));
#139235=CARTESIAN_POINT('Ctrl Pts',(3.37177360474716,-6.15098466075983,
88.8860418232651));
#139236=CARTESIAN_POINT('Ctrl Pts',(3.18225246997043,-6.25114357144375,
88.8762899659266));
#139237=CARTESIAN_POINT('Ctrl Pts',(2.98844542841925,-6.34246170535228,
88.866538108588));
#139238=CARTESIAN_POINT('Ctrl Pts',(2.90393152213085,-6.38228302530952,
88.8622855925254));
#139239=CARTESIAN_POINT('Ctrl Pts',(2.81860296076562,-6.42042375869046,
88.8580330764627));
#139240=CARTESIAN_POINT('Ctrl Pts',(2.73252046822376,-6.4568536032063,88.8537805604001));
#139241=CARTESIAN_POINT('Ctrl Pts',(2.56990977430644,-6.52566994577608,
88.8457475148014));
#139242=CARTESIAN_POINT('Ctrl Pts',(2.40452796168875,-6.58841133439395,
88.8377144692026));
#139243=CARTESIAN_POINT('Ctrl Pts',(2.23687673118098,-6.64484830917916,
88.8296814236039));
#139244=CARTESIAN_POINT('Ctrl Pts',(2.06933327333954,-6.70124900410389,
88.8216535419562));
#139245=CARTESIAN_POINT('Ctrl Pts',(1.89952364748619,-6.7513532357706,88.8136256603085));
#139246=CARTESIAN_POINT('Ctrl Pts',(1.72796962998575,-6.79497958204047,
88.8055977786608));
#139247=CARTESIAN_POINT('Ctrl Pts',(1.55649307081515,-6.838586230585,88.7975735216808));
#139248=CARTESIAN_POINT('Ctrl Pts',(1.3832740427442,-6.87572072724718,88.7895492647008));
#139249=CARTESIAN_POINT('Ctrl Pts',(1.20884953838428,-6.906251469216,88.7815250077207));
#139250=CARTESIAN_POINT('Ctrl Pts',(1.03444612372354,-6.93677851970714,
88.7735017209551));
#139251=CARTESIAN_POINT('Ctrl Pts',(0.85883788263153,-6.96070333514361,
88.7654784341895));
#139252=CARTESIAN_POINT('Ctrl Pts',(0.682572236614536,-6.97794537842645,
88.7574551474239));
#139253=CARTESIAN_POINT('Ctrl Pts',(0.506321033995005,-6.99518600887764,
88.749432518095));
#139254=CARTESIAN_POINT('Ctrl Pts',(0.329412899045756,-7.00574492623365,
88.7414098887662));
#139255=CARTESIAN_POINT('Ctrl Pts',(0.15240031286515,-7.0095934765961,88.7333872594374));
#139256=CARTESIAN_POINT('Ctrl Pts',(-0.0246788174460834,-7.01344347373951,
88.725361614171));
#139257=CARTESIAN_POINT('Ctrl Pts',(-0.201862110634656,-7.01057805956335,
88.7173359689047));
#139258=CARTESIAN_POINT('Ctrl Pts',(-0.378596758095502,-7.00102071538569,
88.7093103236384));
#139259=CARTESIAN_POINT('Ctrl Pts',(-0.482810275928425,-6.99538512286208,
88.7045779141302));
#139260=CARTESIAN_POINT('Ctrl Pts',(-0.586867832591532,-6.98742373395514,
88.6998455046219));
#139261=CARTESIAN_POINT('Ctrl Pts',(-0.69065692121176,-6.97714981777533,
88.6951130951137));
#139262=CARTESIAN_POINT('Ctrl Pts',(-0.882120447475528,-6.95819714898831,
88.6863830462789));
#139263=CARTESIAN_POINT('Ctrl Pts',(-1.07276576004198,-6.93136281656169,
88.6776529974441));
#139264=CARTESIAN_POINT('Ctrl Pts',(-1.26195338716545,-6.89674562464947,
88.6689229486093));
#139265=CARTESIAN_POINT('Ctrl Pts',(-1.45119571812696,-6.86211842313309,
88.66019037547));
#139266=CARTESIAN_POINT('Ctrl Pts',(-1.63897925285721,-6.81970391947092,
88.6514578023307));
#139267=CARTESIAN_POINT('Ctrl Pts',(-1.82467467176382,-6.76965205196867,
88.6427252291914));
#139268=CARTESIAN_POINT('Ctrl Pts',(-2.0130081905177,-6.7188891177918,88.6338685959111));
#139269=CARTESIAN_POINT('Ctrl Pts',(-2.19919353137445,-6.66027023944496,
88.6250119626307));
#139270=CARTESIAN_POINT('Ctrl Pts',(-2.38258960533027,-6.59400434751693,
88.6161553293504));
#139271=CARTESIAN_POINT('Ctrl Pts',(-2.563531851823,-6.52862508888465,88.6074171972435));
#139272=CARTESIAN_POINT('Ctrl Pts',(-2.74175875493713,-6.45580229509339,
88.5986790651366));
#139273=CARTESIAN_POINT('Ctrl Pts',(-2.91667336900007,-6.37578567872743,
88.5899409330297));
#139274=CARTESIAN_POINT('Ctrl Pts',(-3.09514610969175,-6.294141358153,88.5810250491626));
#139275=CARTESIAN_POINT('Ctrl Pts',(-3.27017008926267,-6.20500752522193,
88.5721091652956));
#139276=CARTESIAN_POINT('Ctrl Pts',(-3.4411352453543,-6.10869992598101,
88.5631932814285));
#139277=CARTESIAN_POINT('Ctrl Pts',(-3.61210040144593,-6.01239232674009,
88.5542773975614));
#139278=CARTESIAN_POINT('Ctrl Pts',(-3.77900647356079,-5.90891111491378,
88.5453615136943));
#139279=CARTESIAN_POINT('Ctrl Pts',(-3.9412716704522,-5.79862088622725,
88.5364456298272));
#139280=CARTESIAN_POINT('Ctrl Pts',(-4.10034831522093,-5.69049788840432,
88.5277049453311));
#139281=CARTESIAN_POINT('Ctrl Pts',(-4.25498167604321,-5.57581950384457,
88.518964260835));
#139282=CARTESIAN_POINT('Ctrl Pts',(-4.40465029916025,-5.45496858878284,
88.5102235763389));
#139283=CARTESIAN_POINT('Ctrl Pts',(-4.55429199440605,-5.33413941680803,
88.5014844644371));
#139284=CARTESIAN_POINT('Ctrl Pts',(-4.69897052286826,-5.20714010410923,
88.4927453525354));
#139285=CARTESIAN_POINT('Ctrl Pts',(-4.83819697237339,-5.07439421202344,
88.4840062406336));
#139286=CARTESIAN_POINT('Ctrl Pts',(-4.97922730091604,-4.93992840584875,
88.4751539009592));
#139287=CARTESIAN_POINT('Ctrl Pts',(-5.11466306479463,-4.79956625222803,
88.4663015612848));
#139288=CARTESIAN_POINT('Ctrl Pts',(-5.24403314977661,-4.65378801478366,
88.4574492216104));
#139289=CARTESIAN_POINT('Ctrl Pts',(-5.37168303779884,-4.50994814880194,
88.4487145889607));
#139290=CARTESIAN_POINT('Ctrl Pts',(-5.49342737627533,-4.36083555612009,
88.4399799563111));
#139291=CARTESIAN_POINT('Ctrl Pts',(-5.6088521440018,-4.20694713411357,
88.4312453236614));
#139292=CARTESIAN_POINT('Ctrl Pts',(-5.72661009044385,-4.04994803492858,
88.4223341304747));
#139293=CARTESIAN_POINT('Ctrl Pts',(-5.83779006783849,-3.88797819358361,
88.4134229372879));
#139294=CARTESIAN_POINT('Ctrl Pts',(-5.9419964407593,-3.72159977167129,
88.4045117441011));
#139295=CARTESIAN_POINT('Ctrl Pts',(-6.04620281368011,-3.55522134975898,
88.3956005509144));
#139296=CARTESIAN_POINT('Ctrl Pts',(-6.14343540980544,-3.3844345970281,
88.3866893577276));
#139297=CARTESIAN_POINT('Ctrl Pts',(-6.23334574516367,-3.20983292146958,
88.3777781645409));
#139298=CARTESIAN_POINT('Ctrl Pts',(-6.31432145775738,-3.0525818663815,
88.3697524996884));
#139299=CARTESIAN_POINT('Ctrl Pts',(-6.38939461832771,-2.89216390866809,
88.3617268348359));
#139300=CARTESIAN_POINT('Ctrl Pts',(-6.45831249077132,-2.72907059894887,
88.3537011699835));
#139301=CARTESIAN_POINT('Ctrl Pts',(-6.5272084903727,-2.56602905104567,
88.3456780522801));
#139302=CARTESIAN_POINT('Ctrl Pts',(-6.58995294864213,-2.40031417885692,
88.3376549345769));
#139303=CARTESIAN_POINT('Ctrl Pts',(-6.64634038845979,-2.23243947358674,
88.3296318168736));
#139304=CARTESIAN_POINT('Ctrl Pts',(-6.70272071732769,-2.06458593878639,
88.3216097109556));
#139305=CARTESIAN_POINT('Ctrl Pts',(-6.75274550846451,-1.89457346102356,
88.3135876050377));
#139306=CARTESIAN_POINT('Ctrl Pts',(-6.79625849657735,-1.72293267721062,
88.3055654991198));
#139307=CARTESIAN_POINT('Ctrl Pts',(-6.83978765426365,-1.55122811110228,
88.2975404121601));
#139308=CARTESIAN_POINT('Ctrl Pts',(-6.87680008184139,-1.37789438510245,
88.2895153252005));
#139309=CARTESIAN_POINT('Ctrl Pts',(-6.90719008977293,-1.203474813298,88.2814902382409));
#139310=CARTESIAN_POINT('Ctrl Pts',(-6.93758608286446,-1.02902089043172,
88.2734635707806));
#139311=CARTESIAN_POINT('Ctrl Pts',(-6.96135700378236,-0.853481058366916,
88.2654369033203));
#139312=CARTESIAN_POINT('Ctrl Pts',(-6.9784488376788,-0.677405626194098,
88.25741023586));
#139313=CARTESIAN_POINT('Ctrl Pts',(-6.99555439283926,-0.501188841284845,
88.2493771246193));
#139314=CARTESIAN_POINT('Ctrl Pts',(-7.00597012566691,-0.324435963176175,
88.2413440133786));
#139315=CARTESIAN_POINT('Ctrl Pts',(-7.00969409651052,-0.147699816674087,
88.233310902138));
#139316=CARTESIAN_POINT('Ctrl Pts',(-7.01188839541199,-0.0435604588742939,
88.2285775011767));
#139317=CARTESIAN_POINT('Ctrl Pts',(-7.0117603066995,0.0605730947243702,
88.2238441002155));
#139318=CARTESIAN_POINT('Ctrl Pts',(-7.00931788707192,0.164588336383908,
88.2191106992543));
#139319=CARTESIAN_POINT('Ctrl Pts',(-7.00428642662566,0.378862971384742,
88.2093597459603));
#139320=CARTESIAN_POINT('Ctrl Pts',(-6.98942851048105,0.592761598639739,
88.1996087926664));
#139321=CARTESIAN_POINT('Ctrl Pts',(-6.96482894103494,0.805471529367834,
88.1898578393724));
#139322=CARTESIAN_POINT('Ctrl Pts',(-6.94019393129426,1.01848790865469,
88.180092838001));
#139323=CARTESIAN_POINT('Ctrl Pts',(-6.90578919920208,1.23031212745225,
88.1703278366296));
#139324=CARTESIAN_POINT('Ctrl Pts',(-6.86175136653043,1.44013705820586,
88.1605628352582));
#139325=CARTESIAN_POINT('Ctrl Pts',(-6.81778693580143,1.64961225427453,
88.1508141101208));
#139326=CARTESIAN_POINT('Ctrl Pts',(-6.76422150246786,1.85709478531047,
88.1410653849834));
#139327=CARTESIAN_POINT('Ctrl Pts',(-6.70124196815976,2.06179112585982,
88.131316659846));
#139328=CARTESIAN_POINT('Ctrl Pts',(-6.638435288253,2.26592565432542,88.1215946911791));
#139329=CARTESIAN_POINT('Ctrl Pts',(-6.56626610057202,2.46728922014703,
88.1118727225121));
#139330=CARTESIAN_POINT('Ctrl Pts',(-6.48497048631654,2.6651049424185,88.1021507538452));
#139331=CARTESIAN_POINT('Ctrl Pts',(-6.40421278390713,2.86161176972283,
88.0924931129057));
#139332=CARTESIAN_POINT('Ctrl Pts',(-6.31444902112373,3.05461749445678,
88.0828354719661));
#139333=CARTESIAN_POINT('Ctrl Pts',(-6.21596084663406,3.2433712885842,88.0731778310266));
#139334=CARTESIAN_POINT('Ctrl Pts',(-6.172671903195,3.32633507951881,88.0689329653404));
#139335=CARTESIAN_POINT('Ctrl Pts',(-6.12769814221996,3.40847758267797,
88.0646880996542));
#139336=CARTESIAN_POINT('Ctrl Pts',(-6.08106659565621,3.48973575241654,
88.060443233968));
#139337=CARTESIAN_POINT('Ctrl Pts',(-5.99481091721764,3.64004126608623,
88.052591386954));
#139338=CARTESIAN_POINT('Ctrl Pts',(-5.90291526748684,3.7872574119496,88.0447395399401));
#139339=CARTESIAN_POINT('Ctrl Pts',(-5.80564328722587,3.93092006837956,
88.0368876929261));
#139340=CARTESIAN_POINT('Ctrl Pts',(-5.70839889251204,4.07454198324171,
88.0290380726325));
#139341=CARTESIAN_POINT('Ctrl Pts',(-5.60578141378518,4.21461209768095,
88.0211884523389));
#139342=CARTESIAN_POINT('Ctrl Pts',(-5.49809867869656,4.35069390808123,
88.0133388320453));
#139343=CARTESIAN_POINT('Ctrl Pts',(-5.39042454069712,4.48676485408938,
88.0054898384434));
#139344=CARTESIAN_POINT('Ctrl Pts',(-5.27768618867496,4.6188478312632,87.9976408448416));
#139345=CARTESIAN_POINT('Ctrl Pts',(-5.16023255286608,4.74653837684278,
87.9897918512397));
#139346=CARTESIAN_POINT('Ctrl Pts',(-5.04271945372065,4.87429356840657,
87.9819388839223));
#139347=CARTESIAN_POINT('Ctrl Pts',(-4.92048655960672,4.99765160407217,
87.9740859166048));
#139348=CARTESIAN_POINT('Ctrl Pts',(-4.79392081655473,5.11624371654667,
87.9662329492873));
#139349=CARTESIAN_POINT('Ctrl Pts',(-4.66732293005673,5.23486594743293,
87.95837798758));
#139350=CARTESIAN_POINT('Ctrl Pts',(-4.53639029026041,5.34871959342211,
87.9505230258727));
#139351=CARTESIAN_POINT('Ctrl Pts',(-4.40154341617814,5.45747580095404,
87.9426680641654));
#139352=CARTESIAN_POINT('Ctrl Pts',(-4.26656269530157,5.56633995811281,
87.9348053057521));
#139353=CARTESIAN_POINT('Ctrl Pts',(-4.12766028587753,5.67009634325023,
87.9269425473387));
#139354=CARTESIAN_POINT('Ctrl Pts',(-3.98528667242015,5.76845878039623,
87.9190797889253));
#139355=CARTESIAN_POINT('Ctrl Pts',(-3.88084343253242,5.84061605286622,
87.9133117821774));
#139356=CARTESIAN_POINT('Ctrl Pts',(-3.77453279139011,5.90987148297301,
87.9075437754294));
#139357=CARTESIAN_POINT('Ctrl Pts',(-3.66654084010868,5.97612791281404,
87.9017757686815));
#139358=CARTESIAN_POINT('Ctrl Pts',(-3.50968184488341,6.07236579803378,
87.8933977022405));
#139359=CARTESIAN_POINT('Ctrl Pts',(-3.34892741293785,6.16248813004656,
87.8850196357995));
#139360=CARTESIAN_POINT('Ctrl Pts',(-3.1847824372808,6.24618182489814,87.8766415693584));
#139361=CARTESIAN_POINT('Ctrl Pts',(-3.02074970200762,6.32981829099568,
87.8682692317397));
#139362=CARTESIAN_POINT('Ctrl Pts',(-2.85333133717389,6.40703473506444,
87.859896894121));
#139363=CARTESIAN_POINT('Ctrl Pts',(-2.68305808667884,6.47756326607524,
87.8515245565022));
#139364=CARTESIAN_POINT('Ctrl Pts',(-2.51287629632487,6.54805391357012,
87.8431567159796));
#139365=CARTESIAN_POINT('Ctrl Pts',(-2.33984298091883,6.6118636852555,87.834788875457));
#139366=CARTESIAN_POINT('Ctrl Pts',(-2.16451059628316,6.66877203397132,
87.8264210349344));
#139367=CARTESIAN_POINT('Ctrl Pts',(-1.98924670431671,6.72565815174153,
87.8180564632645));
#139368=CARTESIAN_POINT('Ctrl Pts',(-1.81168584629373,6.77564812142904,
87.8096918915946));
#139369=CARTESIAN_POINT('Ctrl Pts',(-1.63239787270496,6.81857050617564,
87.8013273199246));
#139370=CARTESIAN_POINT('Ctrl Pts',(-1.45315369358412,6.86148240632049,
87.792964791459));
#139371=CARTESIAN_POINT('Ctrl Pts',(-1.27218355970037,6.89733008832511,
87.7846022629935));
#139372=CARTESIAN_POINT('Ctrl Pts',(-1.09007025647445,6.92599259301147,
87.7762397345279));
#139373=CARTESIAN_POINT('Ctrl Pts',(-0.907942420037334,6.95465738505535,
87.7678765387063));
#139374=CARTESIAN_POINT('Ctrl Pts',(-0.724671555730224,6.97613579714193,
87.7595133428848));
#139375=CARTESIAN_POINT('Ctrl Pts',(-0.540849134497942,6.99035827237867,
87.7511501470633));
#139376=CARTESIAN_POINT('Ctrl Pts',(-0.357014176944991,7.0045817175597,
87.7427863808886));
#139377=CARTESIAN_POINT('Ctrl Pts',(-0.172627915286944,7.01154821358835,
87.7344226147139));
#139378=CARTESIAN_POINT('Ctrl Pts',(0.0117144055360298,7.01124021377124,
87.7260588485392));
#139379=CARTESIAN_POINT('Ctrl Pts',(0.196093875303305,7.01093215188553,
87.7176933968856));
#139380=CARTESIAN_POINT('Ctrl Pts',(0.380429057793061,7.00334667154169,
87.709327945232));
#139381=CARTESIAN_POINT('Ctrl Pts',(0.564125623985237,6.98851835819749,
87.7009624935785));
#139382=CARTESIAN_POINT('Ctrl Pts',(0.747883709796349,6.97368507888029,
87.6925942403516));
#139383=CARTESIAN_POINT('Ctrl Pts',(0.931002425257209,6.9516041562705,87.6842259871247));
#139384=CARTESIAN_POINT('Ctrl Pts',(1.11289303816102,6.92236199921044,87.6758577338978));
#139385=CARTESIAN_POINT('Ctrl Pts',(1.29495228961241,6.89309273049896,87.6674817221063));
#139386=CARTESIAN_POINT('Ctrl Pts',(1.47578083824098,6.85664901190533,87.6591057103148));
#139387=CARTESIAN_POINT('Ctrl Pts',(1.65479938759216,6.81316853962418,87.6507296985234));
#139388=CARTESIAN_POINT('Ctrl Pts',(1.83390572985186,6.76966674398218,87.6423495790322));
#139389=CARTESIAN_POINT('Ctrl Pts',(2.01119998495003,6.71912139677559,87.633969459541));
#139390=CARTESIAN_POINT('Ctrl Pts',(2.18611784614881,6.66172014762326,87.6255893400499));
#139391=CARTESIAN_POINT('Ctrl Pts',(2.36123557316148,6.60425331027255,87.6171996452107));
#139392=CARTESIAN_POINT('Ctrl Pts',(2.53397117007375,6.53991502627818,87.6088099503714));
#139393=CARTESIAN_POINT('Ctrl Pts',(2.70377888892343,6.46894166632472,87.6004202555322));
#139394=CARTESIAN_POINT('Ctrl Pts',(2.81158687929119,6.42388190486002,87.5950937830577));
#139395=CARTESIAN_POINT('Ctrl Pts',(2.91821513878084,6.37614866300008,87.5897673105832));
#139396=CARTESIAN_POINT('Ctrl Pts',(3.0235291129734,6.32581206371975,87.5844408381086));
#139397=CARTESIAN_POINT('Ctrl Pts',(3.18924254878909,6.24660651784633,87.5760595377038));
#139398=CARTESIAN_POINT('Ctrl Pts',(3.35203493321549,6.16079312393803,87.567678237299));
#139399=CARTESIAN_POINT('Ctrl Pts',(3.51136137524174,6.06860509960571,87.5592969368942));
#139400=CARTESIAN_POINT('Ctrl Pts',(3.67048589432642,5.97653391009889,87.5509262585607));
#139401=CARTESIAN_POINT('Ctrl Pts',(3.82615294365552,5.87810435336198,87.5425555802273));
#139402=CARTESIAN_POINT('Ctrl Pts',(3.97783933235964,5.77359686923434,87.5341849018938));
#139403=CARTESIAN_POINT('Ctrl Pts',(4.12935358305575,5.66920798315822,87.525823722843));
#139404=CARTESIAN_POINT('Ctrl Pts',(4.27689590856263,5.55875510173926,87.5174625437923));
#139405=CARTESIAN_POINT('Ctrl Pts',(4.41996900154205,5.44256378813398,87.5091013647416));
#139406=CARTESIAN_POINT('Ctrl Pts',(4.56285644030657,5.32652324646393,87.5007510353069));
#139407=CARTESIAN_POINT('Ctrl Pts',(4.70128596083273,5.20475933060727,87.4924007058723));
#139408=CARTESIAN_POINT('Ctrl Pts',(4.8347905229894,5.07763992040711,87.4840503764376));
#139409=CARTESIAN_POINT('Ctrl Pts',(4.96819236137198,4.95061832098858,87.475706472082));
#139410=CARTESIAN_POINT('Ctrl Pts',(5.09667655680907,4.81824966407688,87.4673625677263));
#139411=CARTESIAN_POINT('Ctrl Pts',(5.21980948774704,4.68094172940938,87.4590186633706));
#139412=CARTESIAN_POINT('Ctrl Pts',(5.34284351754677,4.54374408133153,87.450681460891));
#139413=CARTESIAN_POINT('Ctrl Pts',(5.46053463681588,4.40161531085645,87.4423442584113));
#139414=CARTESIAN_POINT('Ctrl Pts',(5.57248631465527,4.25499974564979,87.4340070559317));
#139415=CARTESIAN_POINT('Ctrl Pts',(5.60934018904769,4.20673471087422,87.4312624948952));
#139416=CARTESIAN_POINT('Ctrl Pts',(5.6455723915579,4.15798373429106,87.4285179338587));
#139417=CARTESIAN_POINT('Ctrl Pts',(5.68116969739625,4.10876349184114,87.4257733728222));
#139418=CARTESIAN_POINT('Ctrl Pts',(5.78932614965062,3.95921602814664,87.4174344837487));
#139419=CARTESIAN_POINT('Ctrl Pts',(5.89152974577147,3.80545693513836,87.4090955946751));
#139420=CARTESIAN_POINT('Ctrl Pts',(5.98746751139421,3.64799388191632,87.4007567056016));
#139421=CARTESIAN_POINT('Ctrl Pts',(6.08345224150094,3.49045374569161,87.3924137343856));
#139422=CARTESIAN_POINT('Ctrl Pts',(6.17316485926343,3.32920631627555,87.3840707631696));
#139423=CARTESIAN_POINT('Ctrl Pts',(6.25633828466472,3.16478401006112,87.3757277919537));
#139424=CARTESIAN_POINT('Ctrl Pts',(6.33959903975453,3.00018906518574,87.3673760608595));
#139425=CARTESIAN_POINT('Ctrl Pts',(6.41630674350125,2.83241287896471,87.3590243297653));
#139426=CARTESIAN_POINT('Ctrl Pts',(6.48624191583394,2.66200908559286,87.3506725986712));
#139427=CARTESIAN_POINT('Ctrl Pts',(6.5157398076786,2.59013462673128,87.3471499297148));
#139428=CARTESIAN_POINT('Ctrl Pts',(6.54403342565351,2.51779291191753,87.3436272607585));
#139429=CARTESIAN_POINT('Ctrl Pts',(6.57110895151811,2.44502632087644,87.3401045918022));
#139430=CARTESIAN_POINT('Origin',(0.,0.,50.));
#139431=CARTESIAN_POINT('',(6.57110895151817,2.44502632087629,85.3396537828137));
#139432=CARTESIAN_POINT('',(6.57110895151818,2.44502632087624,85.8868857406669));
#139433=CARTESIAN_POINT('',(6.57110895151814,2.44502632087636,50.));
#139434=CARTESIAN_POINT('',(7.0112498809707,0.00129193205181663,87.7735343569467));
#139435=CARTESIAN_POINT('Ctrl Pts',(6.57110895151818,2.44502632087624,85.8868857406669));
#139436=CARTESIAN_POINT('Ctrl Pts',(6.50935605589572,2.61098977155252,85.894907851644));
#139437=CARTESIAN_POINT('Ctrl Pts',(6.44130892498698,2.77461939656621,85.9029299626212));
#139438=CARTESIAN_POINT('Ctrl Pts',(6.3671830232513,2.93540574894178,85.9109520735983));
#139439=CARTESIAN_POINT('Ctrl Pts',(6.29302610813646,3.09625937237905,85.9189775409295));
#139440=CARTESIAN_POINT('Ctrl Pts',(6.21278549548188,3.25426701379564,85.9270030082606));
#139441=CARTESIAN_POINT('Ctrl Pts',(6.12672374464935,3.40894158343171,85.9350284755918));
#139442=CARTESIAN_POINT('Ctrl Pts',(6.04064005609317,3.56365558066401,85.943055988669));
#139443=CARTESIAN_POINT('Ctrl Pts',(5.94873246003207,3.71503449823715,85.9510835017461));
#139444=CARTESIAN_POINT('Ctrl Pts',(5.85130785221275,3.86261866887393,85.9591110148233));
#139445=CARTESIAN_POINT('Ctrl Pts',(5.75380918994399,4.01031502127616,85.9671446297784));
#139446=CARTESIAN_POINT('Ctrl Pts',(5.65078535490969,4.15421056905528,85.9751782447335));
#139447=CARTESIAN_POINT('Ctrl Pts',(5.54258492985198,4.29387690297215,85.9832118596886));
#139448=CARTESIAN_POINT('Ctrl Pts',(5.51539665690139,4.32897183357445,85.9852305219633));
#139449=CARTESIAN_POINT('Ctrl Pts',(5.48788172555063,4.363799902097,85.9872491842381));
#139450=CARTESIAN_POINT('Ctrl Pts',(5.4600460449783,4.39835466387339,85.9892678465129));
#139451=CARTESIAN_POINT('Ctrl Pts',(5.32558847644155,4.56526810569665,85.9990187998067));
#139452=CARTESIAN_POINT('Ctrl Pts',(5.18356484758662,4.72590019856649,86.0087697531006));
#139453=CARTESIAN_POINT('Ctrl Pts',(5.03453725450321,4.87965789738577,86.0185207063945));
#139454=CARTESIAN_POINT('Ctrl Pts',(4.88529495921571,5.03363711301378,86.0282857077657));
#139455=CARTESIAN_POINT('Ctrl Pts',(4.72902854256956,5.18072209622687,86.038050709137));
#139456=CARTESIAN_POINT('Ctrl Pts',(4.56633782116094,5.32035576494046,86.0478157105083));
#139457=CARTESIAN_POINT('Ctrl Pts',(4.40391827147514,5.45975669326061,86.0575644356456));
#139458=CARTESIAN_POINT('Ctrl Pts',(4.23509584670664,5.59173110452241,86.0673131607829));
#139459=CARTESIAN_POINT('Ctrl Pts',(4.06050196682992,5.71576332084091,86.0770618859202));
#139460=CARTESIAN_POINT('Ctrl Pts',(3.88638727945389,5.83945511681967,86.0867838545872));
#139461=CARTESIAN_POINT('Ctrl Pts',(3.70653279230673,5.95524821136194,86.0965058232541));
#139462=CARTESIAN_POINT('Ctrl Pts',(3.52159880345178,6.06267007431767,86.106227791921));
#139463=CARTESIAN_POINT('Ctrl Pts',(3.33788847449887,6.16938115486333,86.1158854328605));
#139464=CARTESIAN_POINT('Ctrl Pts',(3.14916566698421,6.26783136975615,86.1255430738));
#139465=CARTESIAN_POINT('Ctrl Pts',(2.95611096321559,6.35759660057609,86.1352007147395));
#139466=CARTESIAN_POINT('Ctrl Pts',(2.87125677441394,6.39705150996253,86.1394455804261));
#139467=CARTESIAN_POINT('Ctrl Pts',(2.78556613655165,6.43482907719253,86.1436904461126));
#139468=CARTESIAN_POINT('Ctrl Pts',(2.69909888003785,6.47089574929765,86.1479353117992));
#139469=CARTESIAN_POINT('Ctrl Pts',(2.53915797259907,6.53760928338404,86.1557871588132));
#139470=CARTESIAN_POINT('Ctrl Pts',(2.37662409889162,6.5984380918566,86.1636390058272));
#139471=CARTESIAN_POINT('Ctrl Pts',(2.2119889880388,6.65317452644188,86.1714908528412));
#139472=CARTESIAN_POINT('Ctrl Pts',(2.04740056637242,6.70789543821682,86.1793404731349));
#139473=CARTESIAN_POINT('Ctrl Pts',(1.88071245452038,6.75652729266079,86.1871900934285));
#139474=CARTESIAN_POINT('Ctrl Pts',(1.71243461770912,6.79891125420618,86.1950397137221));
#139475=CARTESIAN_POINT('Ctrl Pts',(1.54417021573067,6.84129183193438,86.202888707324));
#139476=CARTESIAN_POINT('Ctrl Pts',(1.37431671154859,6.87742541732396,86.2107377009259));
#139477=CARTESIAN_POINT('Ctrl Pts',(1.20339716686006,6.90720361805653,86.2185866945278));
#139478=CARTESIAN_POINT('Ctrl Pts',(1.03239109061104,6.93699689462014,86.2264396618453));
#139479=CARTESIAN_POINT('Ctrl Pts',(0.860318271790911,6.96042829215117,
86.2342926291628));
#139480=CARTESIAN_POINT('Ctrl Pts',(0.687710194721222,6.97744088119538,
86.2421455964802));
#139481=CARTESIAN_POINT('Ctrl Pts',(0.515058280999615,6.99445779086558,
86.2500005581876));
#139482=CARTESIAN_POINT('Ctrl Pts',(0.341871219006416,7.00505262109014,
86.2578555198949));
#139483=CARTESIAN_POINT('Ctrl Pts',(0.16868282295875,7.00922054637594,86.2657104816022));
#139484=CARTESIAN_POINT('Ctrl Pts',(-0.00467747704870131,7.01339260867599,
86.2735732400157));
#139485=CARTESIAN_POINT('Ctrl Pts',(-0.178038732489622,7.01112503005644,
86.2814359984291));
#139486=CARTESIAN_POINT('Ctrl Pts',(-0.350869343786947,7.00246508496048,
86.2892987568425));
#139487=CARTESIAN_POINT('Ctrl Pts',(-0.477655400252421,6.99611227350142,
86.2950667635902));
#139488=CARTESIAN_POINT('Ctrl Pts',(-0.60415594756938,6.98632051437324,
86.300834770338));
#139489=CARTESIAN_POINT('Ctrl Pts',(-0.730164208890737,6.97312604149351,
86.3066027770857));
#139490=CARTESIAN_POINT('Ctrl Pts',(-0.913192008898027,6.9539609858209,
86.3149808435267));
#139491=CARTESIAN_POINT('Ctrl Pts',(-1.09558632776169,6.92757283386561,
86.3233589099677));
#139492=CARTESIAN_POINT('Ctrl Pts',(-1.27675602187379,6.89402064278234,
86.3317369764087));
#139493=CARTESIAN_POINT('Ctrl Pts',(-1.4578018343017,6.86049139428867,86.3401093140274));
#139494=CARTESIAN_POINT('Ctrl Pts',(-1.63762436927603,6.81980793286539,
86.3484816516461));
#139495=CARTESIAN_POINT('Ctrl Pts',(-1.81563949333606,6.7720809056551,86.3568539892648));
#139496=CARTESIAN_POINT('Ctrl Pts',(-1.99355899880536,6.72437951441875,
86.3652218297874));
#139497=CARTESIAN_POINT('Ctrl Pts',(-2.16967271229878,6.66964218599931,
86.37358967031));
#139498=CARTESIAN_POINT('Ctrl Pts',(-2.34340810346253,6.60803034368988,
86.3819575108326));
#139499=CARTESIAN_POINT('Ctrl Pts',(-2.51707562581287,6.54644256972139,
86.3903220825025));
#139500=CARTESIAN_POINT('Ctrl Pts',(-2.6883663691981,6.47798574682362,86.3986866541724));
#139501=CARTESIAN_POINT('Ctrl Pts',(-2.85672390664179,6.40287084702802,
86.4070512258423));
#139502=CARTESIAN_POINT('Ctrl Pts',(-3.02504031958242,6.32777429546305,
86.4154137543078));
#139503=CARTESIAN_POINT('Ctrl Pts',(-3.19042465571283,6.2460230445545,86.4237762827733));
#139504=CARTESIAN_POINT('Ctrl Pts',(-3.35234096175784,6.15787598434887,
86.4321388112388));
#139505=CARTESIAN_POINT('Ctrl Pts',(-3.51427018923155,6.06972188973156,
86.4405020070603));
#139506=CARTESIAN_POINT('Ctrl Pts',(-3.67273054213885,5.97517111794213,
86.4488652028818));
#139507=CARTESIAN_POINT('Ctrl Pts',(-3.82721047478691,5.87452862314768,
86.4572283987033));
#139508=CARTESIAN_POINT('Ctrl Pts',(-3.98170094265674,5.77387926473681,
86.465592164878));
#139509=CARTESIAN_POINT('Ctrl Pts',(-4.13221017334873,5.66713753423044,
86.4739559310527));
#139510=CARTESIAN_POINT('Ctrl Pts',(-4.27825529504834,5.55465194165133,
86.4823196972274));
#139511=CARTESIAN_POINT('Ctrl Pts',(-4.42432984798277,5.4421436808047,86.4906851488809));
#139512=CARTESIAN_POINT('Ctrl Pts',(-4.56593823760048,5.3238894504136,86.4990506005345));
#139513=CARTESIAN_POINT('Ctrl Pts',(-4.70263006057313,5.20027855752881,
86.5074160521881));
#139514=CARTESIAN_POINT('Ctrl Pts',(-4.83936766136822,5.07662626759933,
86.5157843054149));
#139515=CARTESIAN_POINT('Ctrl Pts',(-4.97118516849089,4.94761395845391,
86.5241525586418));
#139516=CARTESIAN_POINT('Ctrl Pts',(-5.09766817229645,4.81366863916242,
86.5325208118686));
#139517=CARTESIAN_POINT('Ctrl Pts',(-5.22426844389133,4.67959913345053,
86.5408968236601));
#139518=CARTESIAN_POINT('Ctrl Pts',(-5.34552410293012,4.54058771746286,
86.5492728354515));
#139519=CARTESIAN_POINT('Ctrl Pts',(-5.46105945237866,4.39709633964116,
86.557648847243));
#139520=CARTESIAN_POINT('Ctrl Pts',(-5.57665146179003,4.25353459187493,
86.5660289667341));
#139521=CARTESIAN_POINT('Ctrl Pts',(-5.68651736631053,4.10548876100266,
86.5744090862252));
#139522=CARTESIAN_POINT('Ctrl Pts',(-5.79032377509833,3.95345129501187,
86.5827892057164));
#139523=CARTESIAN_POINT('Ctrl Pts',(-5.89424879585793,3.80124010695673,
86.5911789005556));
#139524=CARTESIAN_POINT('Ctrl Pts',(-5.99210030578251,3.64502844531357,
86.5995685953948));
#139525=CARTESIAN_POINT('Ctrl Pts',(-6.08358930108757,3.48533610691895,
86.607958290234));
#139526=CARTESIAN_POINT('Ctrl Pts',(-6.14167408540737,3.38395019703713,
86.6132847627088));
#139527=CARTESIAN_POINT('Ctrl Pts',(-6.19719521531603,3.28116181133347,
86.6186112351837));
#139528=CARTESIAN_POINT('Ctrl Pts',(-6.25008864931542,3.17710850274248,
86.6239377076585));
#139529=CARTESIAN_POINT('Ctrl Pts',(-6.33331742068157,3.01337874697146,
86.6323190080634));
#139530=CARTESIAN_POINT('Ctrl Pts',(-6.41020567117982,2.84618575687431,
86.6407003084684));
#139531=CARTESIAN_POINT('Ctrl Pts',(-6.48046315699178,2.67604630628324,
86.6490816088733));
#139532=CARTESIAN_POINT('Ctrl Pts',(-6.55063160172563,2.50612248253869,
86.6574522872069));
#139533=CARTESIAN_POINT('Ctrl Pts',(-6.61418590507908,2.33325994057912,
86.6658229655405));
#139534=CARTESIAN_POINT('Ctrl Pts',(-6.67088178962929,2.15799970141156,
86.6741936438741));
#139535=CARTESIAN_POINT('Ctrl Pts',(-6.72751333408461,1.98293835252513,
86.682554822925));
#139536=CARTESIAN_POINT('Ctrl Pts',(-6.7773018721317,1.80548503948199,86.6909160019759));
#139537=CARTESIAN_POINT('Ctrl Pts',(-6.82005113331489,1.62620081830946,
86.6992771810268));
#139538=CARTESIAN_POINT('Ctrl Pts',(-6.8627449222889,1.44714923956262,86.7076275104615));
#139539=CARTESIAN_POINT('Ctrl Pts',(-6.89841757807585,1.26627180872092,
86.7159778398962));
#139540=CARTESIAN_POINT('Ctrl Pts',(-6.92692260572745,1.08414472131816,
86.724328169331));
#139541=CARTESIAN_POINT('Ctrl Pts',(-6.95540570046527,0.902157769815413,
86.7326720736867));
#139542=CARTESIAN_POINT('Ctrl Pts',(-6.97673210713103,0.718923400253159,
86.7410159780424));
#139543=CARTESIAN_POINT('Ctrl Pts',(-6.99080613463922,0.535029111722596,
86.7493598823982));
#139544=CARTESIAN_POINT('Ctrl Pts',(-7.00486885780083,0.351282528230385,
86.7576970848779));
#139545=CARTESIAN_POINT('Ctrl Pts',(-7.01169079431785,0.16687740863043,
86.7660342873576));
#139546=CARTESIAN_POINT('Ctrl Pts',(-7.01122792897929,-0.0175923392648725,
86.7743714898374));
#139547=CARTESIAN_POINT('Ctrl Pts',(-7.0110755562648,-0.0783187620189622,
86.7771160508733));
#139548=CARTESIAN_POINT('Ctrl Pts',(-7.01013415446036,-0.139052146393013,
86.7798606119091));
#139549=CARTESIAN_POINT('Ctrl Pts',(-7.00840338632719,-0.199771211683747,
86.782605172945));
#139550=CARTESIAN_POINT('Ctrl Pts',(-7.00314510219132,-0.384243118488884,
86.7909434832468));
#139551=CARTESIAN_POINT('Ctrl Pts',(-6.99060127451497,-0.568431470742194,
86.7992817935487));
#139552=CARTESIAN_POINT('Ctrl Pts',(-6.97083272321741,-0.751743112653088,
86.8076201038505));
#139553=CARTESIAN_POINT('Ctrl Pts',(-6.951051734218,-0.935170088030384,
86.8159636603343));
#139554=CARTESIAN_POINT('Ctrl Pts',(-6.92403699006115,-1.11771892707604,
86.8243072168182));
#139555=CARTESIAN_POINT('Ctrl Pts',(-6.88990082146536,-1.29880453990238,
86.832650773302));
#139556=CARTESIAN_POINT('Ctrl Pts',(-6.85573868222145,-1.48002792187275,
86.8410006775271));
#139557=CARTESIAN_POINT('Ctrl Pts',(-6.81444437212664,-1.65978553550522,
86.8493505817523));
#139558=CARTESIAN_POINT('Ctrl Pts',(-6.7661807661487,-1.83750493939454,
86.8577004859775));
#139559=CARTESIAN_POINT('Ctrl Pts',(-6.71784476833355,-2.01549090923758,
86.8660629144411));
#139560=CARTESIAN_POINT('Ctrl Pts',(-6.6625186713434,-2.19143224369014,
86.8744253429047));
#139561=CARTESIAN_POINT('Ctrl Pts',(-6.60041491324566,-2.36477261813992,
86.8827877713682));
#139562=CARTESIAN_POINT('Ctrl Pts',(-6.53825804796865,-2.5382612222399,
86.8911573508481));
#139563=CARTESIAN_POINT('Ctrl Pts',(-6.46931207971855,-2.7091441254031,
86.899526930328));
#139564=CARTESIAN_POINT('Ctrl Pts',(-6.3938368012109,-2.87688677601,86.9078965098079));
#139565=CARTESIAN_POINT('Ctrl Pts',(-6.31824511128187,-3.04488814921811,
86.9162789983444));
#139566=CARTESIAN_POINT('Ctrl Pts',(-6.23610413274333,-3.20973929850563,
86.924661486881));
#139567=CARTESIAN_POINT('Ctrl Pts',(-6.14771929897067,-3.37093072957063,
86.9330439754175));
#139568=CARTESIAN_POINT('Ctrl Pts',(-6.11879833308613,-3.42367520709833,
86.9357868630221));
#139569=CARTESIAN_POINT('Ctrl Pts',(-6.08920917596968,-3.47602807320321,
86.9385297506267));
#139570=CARTESIAN_POINT('Ctrl Pts',(-6.05896350698851,-3.5279721914269,
86.9412726382314));
#139571=CARTESIAN_POINT('Ctrl Pts',(-5.96644904131462,-3.68685716584613,
86.9496624933641));
#139572=CARTESIAN_POINT('Ctrl Pts',(-5.86760225278239,-3.8422364254221,
86.9580523484969));
#139573=CARTESIAN_POINT('Ctrl Pts',(-5.7627121365476,-3.99359179108068,
86.9664422036297));
#139574=CARTESIAN_POINT('Ctrl Pts',(-5.65791881144161,-4.1448074881297,
86.9748243167217));
#139575=CARTESIAN_POINT('Ctrl Pts',(-5.54709346211167,-4.29200642462329,
86.9832064298138));
#139576=CARTESIAN_POINT('Ctrl Pts',(-5.43056966892759,-4.43469724258869,
86.9915885429059));
#139577=CARTESIAN_POINT('Ctrl Pts',(-5.31413627351006,-4.57727736272235,
86.9999641532548));
#139578=CARTESIAN_POINT('Ctrl Pts',(-5.19201345511359,-4.71535608326536,
87.0083397636037));
#139579=CARTESIAN_POINT('Ctrl Pts',(-5.06457682105358,-4.84847276842377,
87.0167153739525));
#139580=CARTESIAN_POINT('Ctrl Pts',(-4.93722034652814,-4.98150572121115,
87.0250857159182));
#139581=CARTESIAN_POINT('Ctrl Pts',(-4.80455694766025,-5.10958262515081,
87.0334560578838));
#139582=CARTESIAN_POINT('Ctrl Pts',(-4.66700135664259,-5.2322772192991,
87.0418263998494));
#139583=CARTESIAN_POINT('Ctrl Pts',(-4.52951212603039,-5.35491262237448,
87.0501927037438));
#139584=CARTESIAN_POINT('Ctrl Pts',(-4.38713565461108,-5.47217067520983,
87.0585590076381));
#139585=CARTESIAN_POINT('Ctrl Pts',(-4.24032257778898,-5.58366286578918,
87.0669253115324));
#139586=CARTESIAN_POINT('Ctrl Pts',(-4.0935505604693,-5.69512387512795,
87.075289275606));
#139587=CARTESIAN_POINT('Ctrl Pts',(-3.94234467250425,-5.80082203787116,
87.0836532396797));
#139588=CARTESIAN_POINT('Ctrl Pts',(-3.78718802055007,-5.90040960099399,
87.0920172037533));
#139589=CARTESIAN_POINT('Ctrl Pts',(-3.63205524462613,-5.99998183924587,
87.1003798807519));
#139590=CARTESIAN_POINT('Ctrl Pts',(-3.47297319336365,-6.09344517521102,
87.1087425577504));
#139591=CARTESIAN_POINT('Ctrl Pts',(-3.31045364576688,-6.18049538643374,
87.1171052347489));
#139592=CARTESIAN_POINT('Ctrl Pts',(-3.14793744415068,-6.26754380545165,
87.1254677395753));
#139593=CARTESIAN_POINT('Ctrl Pts',(-2.98198417721644,-6.34817920818278,
87.1338302444016));
#139594=CARTESIAN_POINT('Ctrl Pts',(-2.81313026979528,-6.42214330637845,
87.1421927492279));
#139595=CARTESIAN_POINT('Ctrl Pts',(-2.64425733174381,-6.49611574067621,
87.1505561965479));
#139596=CARTESIAN_POINT('Ctrl Pts',(-2.47248340266744,-6.5634152400237,
87.1589196438678));
#139597=CARTESIAN_POINT('Ctrl Pts',(-2.29836532333784,-6.62383147453029,
87.1672830911878));
#139598=CARTESIAN_POINT('Ctrl Pts',(-2.1241447183896,-6.68428328381374,
87.1756514631406));
#139599=CARTESIAN_POINT('Ctrl Pts',(-1.94757751552329,-6.73784362051997,
87.1840198350934));
#139600=CARTESIAN_POINT('Ctrl Pts',(-1.7692371656464,-6.78435158391688,
87.1923882070462));
#139601=CARTESIAN_POINT('Ctrl Pts',(-1.59084338034021,-6.83087348231499,
87.2007590863819));
#139602=CARTESIAN_POINT('Ctrl Pts',(-1.41067570808094,-6.87033871615273,
87.2091299657177));
#139603=CARTESIAN_POINT('Ctrl Pts',(-1.22931896518779,-6.90263728181697,
87.2175008450534));
#139604=CARTESIAN_POINT('Ctrl Pts',(-1.04780856068732,-6.93496321370668,
87.2258788169447));
#139605=CARTESIAN_POINT('Ctrl Pts',(-0.86510739717758,-6.96011029163013,
87.2342567888359));
#139606=CARTESIAN_POINT('Ctrl Pts',(-0.681807762689802,-6.97802011585206,
87.2426347607272));
#139607=CARTESIAN_POINT('Ctrl Pts',(-0.565319352357486,-6.98940195498542,
87.2479590300862));
#139608=CARTESIAN_POINT('Ctrl Pts',(-0.448589341810954,-6.9978619255989,
87.2532832994453));
#139609=CARTESIAN_POINT('Ctrl Pts',(-0.331770083394625,-7.00339597440159,
87.2586075688043));
#139610=CARTESIAN_POINT('Ctrl Pts',(-0.159252495223688,-7.01156860591117,
87.2664703999936));
#139611=CARTESIAN_POINT('Ctrl Pts',(0.0138185171086572,-7.01337428630968,
87.2743332311829));
#139612=CARTESIAN_POINT('Ctrl Pts',(0.186913749327192,-7.00875807920437,
87.2821960623723));
#139613=CARTESIAN_POINT('Ctrl Pts',(0.359875980707844,-7.00414541904489,
87.2900528520137));
#139614=CARTESIAN_POINT('Ctrl Pts',(0.532862016293961,-6.99312069419043,
87.2979096416551));
#139615=CARTESIAN_POINT('Ctrl Pts',(0.705338861372208,-6.9756808738028,
87.3057664312966));
#139616=CARTESIAN_POINT('Ctrl Pts',(0.877718437672965,-6.95825088864846,
87.3136187900805));
#139617=CARTESIAN_POINT('Ctrl Pts',(1.04958901653653,-6.93441304285145,
87.3214711488644));
#139618=CARTESIAN_POINT('Ctrl Pts',(1.22041919640894,-6.90421636013361,
87.3293235076484));
#139619=CARTESIAN_POINT('Ctrl Pts',(1.39120904128379,-6.87402680720469,
87.3371740123988));
#139620=CARTESIAN_POINT('Ctrl Pts',(1.560958599501,-6.83748146354632,87.3450245171493));
#139621=CARTESIAN_POINT('Ctrl Pts',(1.72914324075803,-6.79468102381862,
87.3528750218997));
#139622=CARTESIAN_POINT('Ctrl Pts',(1.8973008264071,-6.75188746933269,87.3607242637514));
#139623=CARTESIAN_POINT('Ctrl Pts',(2.0638936272454,-6.70284091893024,87.3685735056031));
#139624=CARTESIAN_POINT('Ctrl Pts',(2.22840929069917,-6.64769272722692,
87.3764227474547));
#139625=CARTESIAN_POINT('Ctrl Pts',(2.39298038270055,-6.59252595501821,
87.3842746338697));
#139626=CARTESIAN_POINT('Ctrl Pts',(2.55547257739125,-6.53125355661724,
87.3921265202845));
#139627=CARTESIAN_POINT('Ctrl Pts',(2.71539053087561,-6.46407617740781,
87.3999784066995));
#139628=CARTESIAN_POINT('Ctrl Pts',(2.83281629365509,-6.41474866399658,
87.4057439491632));
#139629=CARTESIAN_POINT('Ctrl Pts',(2.94885442459499,-6.36223834778985,
87.4115094916269));
#139630=CARTESIAN_POINT('Ctrl Pts',(3.06331649494052,-6.30664083441616,
87.4172750340907));
#139631=CARTESIAN_POINT('Ctrl Pts',(3.25500116880469,-6.21353408572183,
87.4269303384503));
#139632=CARTESIAN_POINT('Ctrl Pts',(3.44216773556263,-6.11181628212727,
87.4365856428098));
#139633=CARTESIAN_POINT('Ctrl Pts',(3.62414572569807,-6.00193254888827,
87.4462409471694));
#139634=CARTESIAN_POINT('Ctrl Pts',(3.80713183976366,-5.89144008037898,
87.455949740104));
#139635=CARTESIAN_POINT('Ctrl Pts',(3.98487171838707,-5.77269102740675,
87.4656585330386));
#139636=CARTESIAN_POINT('Ctrl Pts',(4.1567198259205,-5.64617630359693,87.4753673259732));
#139637=CARTESIAN_POINT('Ctrl Pts',(4.32939488113772,-5.51905278019471,
87.4851228384437));
#139638=CARTESIAN_POINT('Ctrl Pts',(4.49612130481291,-5.3840887129702,87.4948783509142));
#139639=CARTESIAN_POINT('Ctrl Pts',(4.65628081749642,-5.24181986633601,
87.5046338633848));
#139640=CARTESIAN_POINT('Ctrl Pts',(4.81659891273631,-5.09941015165712,
87.5143990353134));
#139641=CARTESIAN_POINT('Ctrl Pts',(4.97033706975347,-4.94968122402455,
87.524164207242));
#139642=CARTESIAN_POINT('Ctrl Pts',(5.11691201231409,-4.7932074877618,87.5339293791707));
#139643=CARTESIAN_POINT('Ctrl Pts',(5.26328710326691,-4.63694709988742,
87.543681236509));
#139644=CARTESIAN_POINT('Ctrl Pts',(5.4025184743354,-4.47396031139054,87.5534330938473));
#139645=CARTESIAN_POINT('Ctrl Pts',(5.53406224465387,-4.30485558814656,
87.5631849511856));
#139646=CARTESIAN_POINT('Ctrl Pts',(5.59142485538193,-4.23111368164473,
87.5674374672494));
#139647=CARTESIAN_POINT('Ctrl Pts',(5.6473260762211,-4.15620885909643,87.5716899833132));
#139648=CARTESIAN_POINT('Ctrl Pts',(5.70172304235925,-4.08019373446037,
87.575942499377));
#139649=CARTESIAN_POINT('Ctrl Pts',(5.80447945829518,-3.93660039977533,
87.5839755449759));
#139650=CARTESIAN_POINT('Ctrl Pts',(5.9019152335504,-3.78897284309355,87.5920085905748));
#139651=CARTESIAN_POINT('Ctrl Pts',(5.99369660943177,-3.63775033730822,
87.6000416361736));
#139652=CARTESIAN_POINT('Ctrl Pts',(6.08541898471072,-3.48662504317239,
87.6080695178214));
#139653=CARTESIAN_POINT('Ctrl Pts',(6.17149400650488,-3.33190971203974,
87.6160973994693));
#139654=CARTESIAN_POINT('Ctrl Pts',(6.25163039143314,-3.17407372494868,
87.6241252811171));
#139655=CARTESIAN_POINT('Ctrl Pts',(6.33173059399445,-3.01630900236009,
87.6321495380973));
#139656=CARTESIAN_POINT('Ctrl Pts',(6.40589733296575,-2.85542675548335,
87.6401737950775));
#139657=CARTESIAN_POINT('Ctrl Pts',(6.47388460276936,-2.69192212229958,
87.6481980520578));
#139658=CARTESIAN_POINT('Ctrl Pts',(6.54186365221889,-2.52843725849294,
87.6562213388235));
#139659=CARTESIAN_POINT('Ctrl Pts',(6.60366457293895,-2.36233097525184,
87.6642446255892));
#139660=CARTESIAN_POINT('Ctrl Pts',(6.65908890167848,-2.19411976930214,
87.672267912355));
#139661=CARTESIAN_POINT('Ctrl Pts',(6.71450868888864,-2.02592234676039,
87.6802905416839));
#139662=CARTESIAN_POINT('Ctrl Pts',(6.76355281397507,-1.8556206945594,87.6883131710128));
#139663=CARTESIAN_POINT('Ctrl Pts',(6.80607232949424,-1.68374760822189,
87.6963358003418));
#139664=CARTESIAN_POINT('Ctrl Pts',(6.84860782932424,-1.51180990983968,
87.7043614456082));
#139665=CARTESIAN_POINT('Ctrl Pts',(6.88461373455662,-1.33829995400738,
87.7123870908747));
#139666=CARTESIAN_POINT('Ctrl Pts',(6.91399189574394,-1.16376227301248,
87.7204127361411));
#139667=CARTESIAN_POINT('Ctrl Pts',(6.93131504979576,-1.06084422050252,
87.7251451456486));
#139668=CARTESIAN_POINT('Ctrl Pts',(6.94633470816353,-0.957569012097593,
87.7298775551561));
#139669=CARTESIAN_POINT('Ctrl Pts',(6.95903917973927,-0.854049329578666,
87.7346099646636));
#139670=CARTESIAN_POINT('Ctrl Pts',(6.98457816244076,-0.645950364946275,
87.744123223348));
#139671=CARTESIAN_POINT('Ctrl Pts',(7.00076663816503,-0.436802360049345,
87.7536364820323));
#139672=CARTESIAN_POINT('Ctrl Pts',(7.00756193006239,-0.227381527042749,
87.7631497407167));
#139673=CARTESIAN_POINT('Ctrl Pts',(7.01003449670575,-0.151180684762784,
87.766611279448));
#139674=CARTESIAN_POINT('Ctrl Pts',(7.01126392857062,-0.0749437292124329,
87.7700728181792));
#139675=CARTESIAN_POINT('Ctrl Pts',(7.01124988097084,0.00129193125224031,
87.7735343569104));
#139676=CARTESIAN_POINT('Ctrl Pts',(7.0112498809707,0.00129193205161908,
87.7735343569467));
#139677=CARTESIAN_POINT('Ctrl Pts',(7.0112148332025,0.191494396890641,87.7821706459852));
#139678=CARTESIAN_POINT('Ctrl Pts',(7.00343567581073,0.381684631459496,
87.7908069350237));
#139679=CARTESIAN_POINT('Ctrl Pts',(6.98794117335139,0.571230881763605,
87.7994432240622));
#139680=CARTESIAN_POINT('Ctrl Pts',(6.97244273416072,0.760825290610734,
87.8080817073467));
#139681=CARTESIAN_POINT('Ctrl Pts',(6.94922505512906,0.949775098930185,
87.8167201906312));
#139682=CARTESIAN_POINT('Ctrl Pts',(6.91836885256738,1.13745284839657,87.8253586739157));
#139683=CARTESIAN_POINT('Ctrl Pts',(6.88751073242885,1.3251422612071,87.8339976940438));
#139684=CARTESIAN_POINT('Ctrl Pts',(6.8490131915845,1.51155917165626,87.8426367141719));
#139685=CARTESIAN_POINT('Ctrl Pts',(6.80300829948206,1.69608509211013,87.8512757343));
#139686=CARTESIAN_POINT('Ctrl Pts',(6.75699271969402,1.8806538809402,87.8599167614132));
#139687=CARTESIAN_POINT('Ctrl Pts',(6.70346637489318,2.06333052071484,87.8685577885263));
#139688=CARTESIAN_POINT('Ctrl Pts',(6.64261183550849,2.24350943061592,87.8771988156395));
#139689=CARTESIAN_POINT('Ctrl Pts',(6.61980274129825,2.31104289274028,87.8804375880218));
#139690=CARTESIAN_POINT('Ctrl Pts',(6.59596464646165,2.37822561687374,87.8836763604041));
#139691=CARTESIAN_POINT('Ctrl Pts',(6.57110895151811,2.44502632087643,87.8869151327864));
#139692=CARTESIAN_POINT('',(7.01124965431583,0.00220167122758261,87.2264656430642));
#139693=CARTESIAN_POINT('Ctrl Pts',(6.57110895151811,2.44502632087644,87.3401045918022));
#139694=CARTESIAN_POINT('Ctrl Pts',(6.63540548261139,2.27222674509633,87.3317392734252));
#139695=CARTESIAN_POINT('Ctrl Pts',(6.69282938016015,2.09703047627333,87.3233739550482));
#139696=CARTESIAN_POINT('Ctrl Pts',(6.74323173931865,1.92001361254175,87.3150086366712));
#139697=CARTESIAN_POINT('Ctrl Pts',(6.79372178829562,1.74268877559408,87.3066287643475));
#139698=CARTESIAN_POINT('Ctrl Pts',(6.83716579752875,1.56353732978274,87.2982488920238));
#139699=CARTESIAN_POINT('Ctrl Pts',(6.87346582618015,1.383146448802,87.2898690197001));
#139700=CARTESIAN_POINT('Ctrl Pts',(6.90633433108634,1.21980832547748,87.2822813156454));
#139701=CARTESIAN_POINT('Ctrl Pts',(6.93334632752058,1.05545429802191,87.2746936115906));
#139702=CARTESIAN_POINT('Ctrl Pts',(6.95446591090124,0.890522575015729,
87.2671059075359));
#139703=CARTESIAN_POINT('Ctrl Pts',(6.99217189097095,0.596060693431974,
87.2535591527205));
#139704=CARTESIAN_POINT('Ctrl Pts',(7.01115634495757,0.299346418726003,
87.240012397905));
#139705=CARTESIAN_POINT('Ctrl Pts',(7.01124965431565,0.00220167178242508,
87.2264656430895));
#139706=CARTESIAN_POINT('Ctrl Pts',(7.01124965431583,0.00220167122758728,
87.2264656430642));
#139707=CARTESIAN_POINT('Ctrl Pts',(7.0113066794161,-0.179395476228933,
87.2181866744569));
#139708=CARTESIAN_POINT('Ctrl Pts',(7.00430416044149,-0.361169552020984,
87.2099077058496));
#139709=CARTESIAN_POINT('Ctrl Pts',(6.99022718875038,-0.542540700920188,
87.2016287372423));
#139710=CARTESIAN_POINT('Ctrl Pts',(6.97616290082495,-0.723748429077766,
87.1933572282293));
#139711=CARTESIAN_POINT('Ctrl Pts',(6.95503688927996,-0.904553615145572,
87.1850857192163));
#139712=CARTESIAN_POINT('Ctrl Pts',(6.92688628859189,-1.08437673684824,
87.1768142102033));
#139713=CARTESIAN_POINT('Ctrl Pts',(6.89875615964076,-1.26406908721555,
87.1685487164139));
#139714=CARTESIAN_POINT('Ctrl Pts',(6.8636116756909,-1.44278046049112,87.1602832226244));
#139715=CARTESIAN_POINT('Ctrl Pts',(6.821541788702,-1.61993647637567,87.152017728835));
#139716=CARTESIAN_POINT('Ctrl Pts',(6.77865012864773,-1.80055297320375,
87.1435907808403));
#139717=CARTESIAN_POINT('Ctrl Pts',(6.72855974717477,-1.97955236337847,
87.1351638328456));
#139718=CARTESIAN_POINT('Ctrl Pts',(6.67141989610619,-2.15633557971353,
87.126736884851));
#139719=CARTESIAN_POINT('Ctrl Pts',(6.61542495399234,-2.32957659767665,
87.1184787872827));
#139720=CARTESIAN_POINT('Ctrl Pts',(6.55266047395911,-2.50068907097207,
87.1102206897145));
#139721=CARTESIAN_POINT('Ctrl Pts',(6.48331758590733,-2.66912338470231,
87.1019625921463));
#139722=CARTESIAN_POINT('Ctrl Pts',(6.41398579047937,-2.83753075437914,
87.0937058156071));
#139723=CARTESIAN_POINT('Ctrl Pts',(6.33807781423758,-3.00326050280816,
87.0854490390679));
#139724=CARTESIAN_POINT('Ctrl Pts',(6.2558332555195,-3.1657821848062,87.0771922625288));
#139725=CARTESIAN_POINT('Ctrl Pts',(6.17358889881209,-3.32830346761533,
87.06893550627));
#139726=CARTESIAN_POINT('Ctrl Pts',(6.08500814531612,-3.48761639543208,
87.0606787500113));
#139727=CARTESIAN_POINT('Ctrl Pts',(5.99037707635064,-3.64321410922179,
87.0524219937526));
#139728=CARTESIAN_POINT('Ctrl Pts',(5.89233640169151,-3.80441808802212,
87.0438677423535));
#139729=CARTESIAN_POINT('Ctrl Pts',(5.78780148794633,-3.96163379975225,
87.0353134909543));
#139730=CARTESIAN_POINT('Ctrl Pts',(5.67714016313336,-4.11432936584301,
87.0267592395552));
#139731=CARTESIAN_POINT('Ctrl Pts',(5.57024169369452,-4.26183277168771,
87.0184958613306));
#139732=CARTESIAN_POINT('Ctrl Pts',(5.45762683920251,-4.40511811963978,
87.010232483106));
#139733=CARTESIAN_POINT('Ctrl Pts',(5.33966885850479,-4.54373888378438,
87.0019691048814));
#139734=CARTESIAN_POINT('Ctrl Pts',(5.21548264801218,-4.6896788811706,86.993269416895));
#139735=CARTESIAN_POINT('Ctrl Pts',(5.08537409387772,-4.83044805700159,
86.9845697289086));
#139736=CARTESIAN_POINT('Ctrl Pts',(4.94982358379145,-4.96556875411488,
86.9758700409222));
#139737=CARTESIAN_POINT('Ctrl Pts',(4.81427307370527,-5.10068945122808,
86.9671703529358));
#139738=CARTESIAN_POINT('Ctrl Pts',(4.67328095355334,-5.23016139735379,
86.9584706649493));
#139739=CARTESIAN_POINT('Ctrl Pts',(4.527368704802,-5.35355575045964,86.9497709769629));
#139740=CARTESIAN_POINT('Ctrl Pts',(4.39549232231815,-5.46508032119165,
86.9419081457736));
#139741=CARTESIAN_POINT('Ctrl Pts',(4.25930025509381,-5.57189116622378,
86.9340453145843));
#139742=CARTESIAN_POINT('Ctrl Pts',(4.11917885399775,-5.67362248755395,
86.926182483395));
#139743=CARTESIAN_POINT('Ctrl Pts',(3.97916511770259,-5.77527564179207,
86.9183256937535));
#139744=CARTESIAN_POINT('Ctrl Pts',(3.83522835813542,-5.87185681133976,
86.9104689041121));
#139745=CARTESIAN_POINT('Ctrl Pts',(3.68778953694237,-5.96303906525175,
86.9026121144707));
#139746=CARTESIAN_POINT('Ctrl Pts',(3.54043386426488,-6.05416989668899,
86.8947597556866));
#139747=CARTESIAN_POINT('Ctrl Pts',(3.38958038194236,-6.13990766924507,
86.8869073969027));
#139748=CARTESIAN_POINT('Ctrl Pts',(3.23568048249427,-6.21996771516587,
86.8790550381187));
#139749=CARTESIAN_POINT('Ctrl Pts',(3.08181692060817,-6.30000885797566,
86.8712045333682));
#139750=CARTESIAN_POINT('Ctrl Pts',(2.92490870723316,-6.37437475898989,
86.8633540286177));
#139751=CARTESIAN_POINT('Ctrl Pts',(2.76543332457585,-6.44282586213731,
86.8555035238673));
#139752=CARTESIAN_POINT('Ctrl Pts',(2.60598359648129,-6.51126595365966,
86.8476542820156));
#139753=CARTESIAN_POINT('Ctrl Pts',(2.44396787300339,-6.57379299375918,
86.8398050401639));
#139754=CARTESIAN_POINT('Ctrl Pts',(2.27988474236866,-6.63021508881986,
86.8319557983122));
#139755=CARTESIAN_POINT('Ctrl Pts',(2.11574632891598,-6.6866561935886,86.8241039118973));
#139756=CARTESIAN_POINT('Ctrl Pts',(1.94953947810042,-6.73698812066281,
86.8162520254824));
#139757=CARTESIAN_POINT('Ctrl Pts',(1.78177929760037,-6.78106843330332,
86.8084001390675));
#139758=CARTESIAN_POINT('Ctrl Pts',(1.65859508513453,-6.81343605821695,
86.8026345966039));
#139759=CARTESIAN_POINT('Ctrl Pts',(1.53457370880756,-6.8424339780357,86.7968690541402));
#139760=CARTESIAN_POINT('Ctrl Pts',(1.4099228546989,-6.86802330414638,86.7911035116765));
#139761=CARTESIAN_POINT('Ctrl Pts',(1.20117546576048,-6.91087664076003,
86.7814482073168));
#139762=CARTESIAN_POINT('Ctrl Pts',(0.990769093090478,-6.94414815441042,
86.7717929029572));
#139763=CARTESIAN_POINT('Ctrl Pts',(0.779506623183717,-6.96778271668346,
86.7621375985975));
#139764=CARTESIAN_POINT('Ctrl Pts',(0.567073798822291,-6.99154820999812,
86.7524288056629));
#139765=CARTESIAN_POINT('Ctrl Pts',(0.353775418683256,-7.00556973150932,
86.7427200127282));
#139766=CARTESIAN_POINT('Ctrl Pts',(0.140422469402555,-7.00984365678628,
86.7330112197935));
#139767=CARTESIAN_POINT('Ctrl Pts',(-0.0739571523842897,-7.01413814855455,
86.7232557073229));
#139768=CARTESIAN_POINT('Ctrl Pts',(-0.288391826022229,-7.00859102897364,
86.7135001948524));
#139769=CARTESIAN_POINT('Ctrl Pts',(-0.502064877831008,-6.99325084784956,
86.7037446823818));
#139770=CARTESIAN_POINT('Ctrl Pts',(-0.715949498834876,-6.97789547758606,
86.693979510453));
#139771=CARTESIAN_POINT('Ctrl Pts',(-0.929070952150075,-6.95272766418326,
86.6842143385242));
#139772=CARTESIAN_POINT('Ctrl Pts',(-1.14061680414627,-6.91784792176,86.6744491665954));
#139773=CARTESIAN_POINT('Ctrl Pts',(-1.35187421817187,-6.88301573707434,
86.664697309257));
#139774=CARTESIAN_POINT('Ctrl Pts',(-1.56156028711736,-6.83849809557125,
86.6549454519186));
#139775=CARTESIAN_POINT('Ctrl Pts',(-1.76887308919542,-6.78444651808976,
86.6451935945802));
#139776=CARTESIAN_POINT('Ctrl Pts',(-1.85927648522427,-6.76087611570234,
86.6409410785168));
#139777=CARTESIAN_POINT('Ctrl Pts',(-1.94922867855122,-6.73549340808156,
86.6366885624534));
#139778=CARTESIAN_POINT('Ctrl Pts',(-2.03866363066388,-6.70831403286313,
86.6324360463901));
#139779=CARTESIAN_POINT('Ctrl Pts',(-2.20760715439179,-6.65697191981162,
86.6244030007912));
#139780=CARTESIAN_POINT('Ctrl Pts',(-2.37478632349822,-6.59918999176723,
86.6163699551923));
#139781=CARTESIAN_POINT('Ctrl Pts',(-2.53966891637932,-6.5351134923333,
86.6083369095934));
#139782=CARTESIAN_POINT('Ctrl Pts',(-2.70444551638085,-6.47107818374049,
86.6003090279456));
#139783=CARTESIAN_POINT('Ctrl Pts',(-2.86692813857277,-6.4007564904291,
86.5922811462977));
#139784=CARTESIAN_POINT('Ctrl Pts',(-3.02659992353864,-6.32434340191422,
86.5842532646499));
#139785=CARTESIAN_POINT('Ctrl Pts',(-3.18619961512002,-6.24796481466186,
86.5762290076697));
#139786=CARTESIAN_POINT('Ctrl Pts',(-3.34299066647081,-6.1655004663301,
86.5682047506895));
#139787=CARTESIAN_POINT('Ctrl Pts',(-3.49647645282019,-6.07719334704549,
86.5601804937094));
#139788=CARTESIAN_POINT('Ctrl Pts',(-3.64994368117478,-5.98889690499099,
86.5521572069436));
#139789=CARTESIAN_POINT('Ctrl Pts',(-3.80010611914945,-5.89475927512961,
86.5441339201778));
#139790=CARTESIAN_POINT('Ctrl Pts',(-3.94649185093902,-5.7950693380642,
86.536110633412));
#139791=CARTESIAN_POINT('Ctrl Pts',(-4.0928655877237,-5.69538756969987,
86.528088004083));
#139792=CARTESIAN_POINT('Ctrl Pts',(-4.23546293396804,-5.59015461007032,
86.520065374754));
#139793=CARTESIAN_POINT('Ctrl Pts',(-4.37384132920086,-5.4797024179671,
86.512042745425));
#139794=CARTESIAN_POINT('Ctrl Pts',(-4.51227174485862,-5.36920870370314,
86.5040171001586));
#139795=CARTESIAN_POINT('Ctrl Pts',(-4.64647975633978,-5.25349206860225,
86.4959914548921));
#139796=CARTESIAN_POINT('Ctrl Pts',(-4.776055953328,-5.13292471142722,86.4879658096256));
#139797=CARTESIAN_POINT('Ctrl Pts',(-4.85246197504882,-5.06183085063136,
86.4832334001183));
#139798=CARTESIAN_POINT('Ctrl Pts',(-4.927258172949,-4.98905113101414,86.478500990611));
#139799=CARTESIAN_POINT('Ctrl Pts',(-5.00036666384089,-4.91466782088563,
86.4737685811036));
#139800=CARTESIAN_POINT('Ctrl Pts',(-5.13523256982733,-4.77745020924617,
86.465038532269));
#139801=CARTESIAN_POINT('Ctrl Pts',(-5.26442067180578,-4.6347051536203,
86.4563084834345));
#139802=CARTESIAN_POINT('Ctrl Pts',(-5.38750327558942,-4.48691820941872,
86.4475784345999));
#139803=CARTESIAN_POINT('Ctrl Pts',(-5.51062146886109,-4.33908853243833,
86.4388458614608));
#139804=CARTESIAN_POINT('Ctrl Pts',(-5.62763046476733,-4.18621426739769,
86.4301132883218));
#139805=CARTESIAN_POINT('Ctrl Pts',(-5.73814312435031,-4.02881372701336,
86.4213807151827));
#139806=CARTESIAN_POINT('Ctrl Pts',(-5.85022579267595,-3.86917706069164,
86.4125240819023));
#139807=CARTESIAN_POINT('Ctrl Pts',(-5.95562596969108,-3.70488477014028,
86.4036674486218));
#139808=CARTESIAN_POINT('Ctrl Pts',(-6.05398527447523,-3.53650800351661,
86.3948108153414));
#139809=CARTESIAN_POINT('Ctrl Pts',(-6.15102853819702,-3.37038410701347,
86.3860726832347));
#139810=CARTESIAN_POINT('Ctrl Pts',(-6.24121805230625,-3.20028460721418,
86.3773345511281));
#139811=CARTESIAN_POINT('Ctrl Pts',(-6.32425545766644,-3.02678368382616,
86.3685964190214));
#139812=CARTESIAN_POINT('Ctrl Pts',(-6.40898201636357,-2.8497533912047,
86.3596805351541));
#139813=CARTESIAN_POINT('Ctrl Pts',(-6.48626224072858,-2.66918207420734,
86.3507646512867));
#139814=CARTESIAN_POINT('Ctrl Pts',(-6.55583000629885,-2.48570301746038,
86.3418487674193));
#139815=CARTESIAN_POINT('Ctrl Pts',(-6.62539777186917,-2.30222396071329,
86.332932883552));
#139816=CARTESIAN_POINT('Ctrl Pts',(-6.68725297711821,-2.11583744914202,
86.3240169996846));
#139817=CARTESIAN_POINT('Ctrl Pts',(-6.74118250120147,-1.92719616230293,
86.3151011158173));
#139818=CARTESIAN_POINT('Ctrl Pts',(-6.79405229650787,-1.74226172442209,
86.3063604313211));
#139819=CARTESIAN_POINT('Ctrl Pts',(-6.83931061792881,-1.55514066064912,
86.2976197468249));
#139820=CARTESIAN_POINT('Ctrl Pts',(-6.87680237159808,-1.36646101462248,
86.2888790623286));
#139821=CARTESIAN_POINT('Ctrl Pts',(-6.91428737987824,-1.17781531519754,
86.2801399504267));
#139822=CARTESIAN_POINT('Ctrl Pts',(-6.94400855764818,-0.987611861976894,
86.2714008385248));
#139823=CARTESIAN_POINT('Ctrl Pts',(-6.9658618755798,-0.796489104033331,
86.2626617266229));
#139824=CARTESIAN_POINT('Ctrl Pts',(-6.98799833469756,-0.602890075687711,
86.2538093869486));
#139825=CARTESIAN_POINT('Ctrl Pts',(-7.00206157913031,-0.408348035341609,
86.2449570472742));
#139826=CARTESIAN_POINT('Ctrl Pts',(-7.00799757267361,-0.21353356621558,
86.2361047075999));
#139827=CARTESIAN_POINT('Ctrl Pts',(-7.01385463701136,-0.0213094892736308,
86.2273700749501));
#139828=CARTESIAN_POINT('Ctrl Pts',(-7.0117992450298,0.171179535380497,
86.2186354423004));
#139829=CARTESIAN_POINT('Ctrl Pts',(-7.0018318541426,0.363286730853184,
86.2099008096506));
#139830=CARTESIAN_POINT('Ctrl Pts',(-6.9916629839309,0.559277151977933,
86.200989616464));
#139831=CARTESIAN_POINT('Ctrl Pts',(-6.97325883762919,0.7548698519352,86.1920784232773));
#139832=CARTESIAN_POINT('Ctrl Pts',(-6.94667580252165,0.949379722324112,
86.1831672300907));
#139833=CARTESIAN_POINT('Ctrl Pts',(-6.92009276741413,1.14388959271289,
86.1742560369041));
#139834=CARTESIAN_POINT('Ctrl Pts',(-6.88533087119709,1.3373163313709,86.1653448437175));
#139835=CARTESIAN_POINT('Ctrl Pts',(-6.84250272341944,1.52898104713482,
86.1564336505308));
#139836=CARTESIAN_POINT('Ctrl Pts',(-6.80393051954978,1.70159954395731,
86.1484079856783));
#139837=CARTESIAN_POINT('Ctrl Pts',(-6.75879730526788,1.87286802781756,
86.1403823208259));
#139838=CARTESIAN_POINT('Ctrl Pts',(-6.70722394941671,2.04224715812532,
86.1323566559734));
#139839=CARTESIAN_POINT('Ctrl Pts',(-6.65566696168361,2.21157253165193,
86.12433353827));
#139840=CARTESIAN_POINT('Ctrl Pts',(-6.59767400832791,2.37900939518393,
86.1163104205667));
#139841=CARTESIAN_POINT('Ctrl Pts',(-6.5334163010369,2.54403183939299,86.1082873028634));
#139842=CARTESIAN_POINT('Ctrl Pts',(-6.46916669720532,2.70903347282719,
86.1002651969454));
#139843=CARTESIAN_POINT('Ctrl Pts',(-6.39865404663154,2.87162095215027,
86.0922430910274));
#139844=CARTESIAN_POINT('Ctrl Pts',(-6.32209833132043,3.03128673200268,
86.0842209851095));
#139845=CARTESIAN_POINT('Ctrl Pts',(-6.24551416764698,3.19101184419805,
86.0761958981499));
#139846=CARTESIAN_POINT('Ctrl Pts',(-6.16288260911893,3.34781275586464,
86.0681708111903));
#139847=CARTESIAN_POINT('Ctrl Pts',(-6.07447059243358,3.50120459044592,
86.0601457242307));
#139848=CARTESIAN_POINT('Ctrl Pts',(-5.98604116344338,3.65462663478246,
86.0521190567703));
#139849=CARTESIAN_POINT('Ctrl Pts',(-5.89182919903346,3.80463795130602,
86.0440923893099));
#139850=CARTESIAN_POINT('Ctrl Pts',(-5.792145793958,3.95078139917089,86.0360657218495));
#139851=CARTESIAN_POINT('Ctrl Pts',(-5.69238236339647,4.09704217048035,
86.0280326106088));
#139852=CARTESIAN_POINT('Ctrl Pts',(-5.5871389335373,4.23942857391079,86.0199994993681));
#139853=CARTESIAN_POINT('Ctrl Pts',(-5.47676819494788,4.37751490018107,
86.0119663881273));
#139854=CARTESIAN_POINT('Ctrl Pts',(-5.41173374634506,4.45888037986663,
86.0072329871663));
#139855=CARTESIAN_POINT('Ctrl Pts',(-5.34491985472404,4.53875351225276,
86.0024995862054));
#139856=CARTESIAN_POINT('Ctrl Pts',(-5.27640478678675,4.61705307403694,
85.9977661852444));
#139857=CARTESIAN_POINT('Ctrl Pts',(-5.13526161449251,4.77835260817125,
85.9880152319506));
#139858=CARTESIAN_POINT('Ctrl Pts',(-4.98681445037594,4.9330678946744,85.9782642786568));
#139859=CARTESIAN_POINT('Ctrl Pts',(-4.83164907455954,5.08062927035696,
85.968513325363));
#139860=CARTESIAN_POINT('Ctrl Pts',(-4.67626015391105,5.22840323588296,
85.9587483239918));
#139861=CARTESIAN_POINT('Ctrl Pts',(-4.51413368902129,5.36900264783073,
85.9489833226206));
#139862=CARTESIAN_POINT('Ctrl Pts',(-4.34589168472511,5.50189531226623,
85.9392183212493));
#139863=CARTESIAN_POINT('Ctrl Pts',(-4.1779301049904,5.63456647216544,85.9294695961121));
#139864=CARTESIAN_POINT('Ctrl Pts',(-4.00387338793853,5.75955653409464,
85.9197208709749));
#139865=CARTESIAN_POINT('Ctrl Pts',(-3.82437342948381,5.87637596094381,
85.9099721458376));
#139866=CARTESIAN_POINT('Ctrl Pts',(-3.64536612881235,5.99287476376404,
85.9002501771707));
#139867=CARTESIAN_POINT('Ctrl Pts',(-3.46094544465128,6.10124767801816,
85.8905282085038));
#139868=CARTESIAN_POINT('Ctrl Pts',(-3.27179036996444,6.20104945452848,
85.8808062398369));
#139869=CARTESIAN_POINT('Ctrl Pts',(-3.08388688500338,6.30019086874981,
85.8711485988975));
#139870=CARTESIAN_POINT('Ctrl Pts',(-2.89131148268681,6.39087414896381,
85.8614909579581));
#139871=CARTESIAN_POINT('Ctrl Pts',(-2.69476145194911,6.47270324359067,
85.8518333170187));
#139872=CARTESIAN_POINT('Ctrl Pts',(-2.60837094659956,6.50866994789785,
85.8475884513318));
#139873=CARTESIAN_POINT('Ctrl Pts',(-2.52121299164009,6.5429266390945,85.8433435856449));
#139874=CARTESIAN_POINT('Ctrl Pts',(-2.43334873421181,6.57544222849002,
85.839098719958));
#139875=CARTESIAN_POINT('Ctrl Pts',(-2.27082375504642,6.63558722537196,
85.831246872944));
#139876=CARTESIAN_POINT('Ctrl Pts',(-2.10594760139136,6.68974678591728,
85.82339502593));
#139877=CARTESIAN_POINT('Ctrl Pts',(-1.93922005044005,6.73773345855053,
85.815543178916));
#139878=CARTESIAN_POINT('Ctrl Pts',(-1.77253978207427,6.78570652255137,
85.8076935586224));
#139879=CARTESIAN_POINT('Ctrl Pts',(-1.6040095270302,6.82751007544145,85.7998439383287));
#139880=CARTESIAN_POINT('Ctrl Pts',(-1.43414529570062,6.86300618048096,
85.7919943180351));
#139881=CARTESIAN_POINT('Ctrl Pts',(-1.26429462585716,6.89849945161051,
85.7841453244332));
#139882=CARTESIAN_POINT('Ctrl Pts',(-1.09311056529415,6.92768620006259,
85.7762963308313));
#139883=CARTESIAN_POINT('Ctrl Pts',(-0.921120155835015,6.95047942382498,
85.7684473372294));
#139884=CARTESIAN_POINT('Ctrl Pts',(-0.749042672667633,6.97328418712916,
85.7605943699119));
#139885=CARTESIAN_POINT('Ctrl Pts',(-0.576158403589205,6.98968890816532,
85.7527414025944));
#139886=CARTESIAN_POINT('Ctrl Pts',(-0.403000710362994,6.99965834808721,
85.7448884352769));
#139887=CARTESIAN_POINT('Ctrl Pts',(-0.229799040901227,7.00963031991184,
85.7370334735696));
#139888=CARTESIAN_POINT('Ctrl Pts',(-0.0563241903801478,7.01316374685525,
85.7291785118623));
#139889=CARTESIAN_POINT('Ctrl Pts',(0.116890273279048,7.01027554569097,
85.7213235501549));
#139890=CARTESIAN_POINT('Ctrl Pts',(0.290276666772179,7.00738447774561,
85.7134607917415));
#139891=CARTESIAN_POINT('Ctrl Pts',(0.463401776455177,6.99805907169471,
85.7055980333281));
#139892=CARTESIAN_POINT('Ctrl Pts',(0.635736368850849,6.98236821084511,
85.6977352749147));
#139893=CARTESIAN_POINT('Ctrl Pts',(0.762158552967875,6.97085762047723,
85.691967268167));
#139894=CARTESIAN_POINT('Ctrl Pts',(0.888155422128745,6.95592256172243,
85.6861992614192));
#139895=CARTESIAN_POINT('Ctrl Pts',(1.01352184654572,6.93760765891778,85.6804312546715));
#139896=CARTESIAN_POINT('Ctrl Pts',(1.19561737437222,6.91100514625288,85.6720531882305));
#139897=CARTESIAN_POINT('Ctrl Pts',(1.37678580379833,6.87721132586099,85.6636751217895));
#139898=CARTESIAN_POINT('Ctrl Pts',(1.55643888652997,6.83630927877004,85.6552970553485));
#139899=CARTESIAN_POINT('Ctrl Pts',(1.73596912461776,6.79543520001302,85.6469247177298));
#139900=CARTESIAN_POINT('Ctrl Pts',(1.9139857623391,6.7474626577391,85.6385523801111));
#139901=CARTESIAN_POINT('Ctrl Pts',(2.08990965660681,6.69252599469899,85.6301800424924));
#139902=CARTESIAN_POINT('Ctrl Pts',(2.26573905556112,6.63761884019842,85.6218122019698));
#139903=CARTESIAN_POINT('Ctrl Pts',(2.43947763931337,6.57575512128039,85.6134443614473));
#139904=CARTESIAN_POINT('Ctrl Pts',(2.61055992599161,6.50711944221917,85.6050765209247));
#139905=CARTESIAN_POINT('Ctrl Pts',(2.78157538027929,6.438510575323,85.5967119492548));
#139906=CARTESIAN_POINT('Ctrl Pts',(2.94993630212426,6.36313514586129,85.5883473775849));
#139907=CARTESIAN_POINT('Ctrl Pts',(3.1150953174239,6.28122660997545,85.579982805915));
#139908=CARTESIAN_POINT('Ctrl Pts',(3.28021398952197,6.1993380817929,85.5716202774493));
#139909=CARTESIAN_POINT('Ctrl Pts',(3.4421320208119,6.11091977595752,85.5632577489837));
#139910=CARTESIAN_POINT('Ctrl Pts',(3.60032444525188,6.01625219313667,85.554895220518));
#139911=CARTESIAN_POINT('Ctrl Pts',(3.75852949394097,5.92157705554729,85.5465320246965));
#139912=CARTESIAN_POINT('Ctrl Pts',(3.91300805665764,5.82065180820689,85.5381688288749));
#139913=CARTESIAN_POINT('Ctrl Pts',(4.06326143054369,5.71380198375443,85.5298056330534));
#139914=CARTESIAN_POINT('Ctrl Pts',(4.21352505140834,5.60694487235836,85.5214418668787));
#139915=CARTESIAN_POINT('Ctrl Pts',(4.35956264076882,5.49416256856521,85.513078100704));
#139916=CARTESIAN_POINT('Ctrl Pts',(4.50090591956449,5.37582295706707,85.5047143345293));
#139917=CARTESIAN_POINT('Ctrl Pts',(4.64227768207256,5.25745949759054,85.4963488828757));
#139918=CARTESIAN_POINT('Ctrl Pts',(4.77895299557398,5.1335367083427,85.4879834312221));
#139919=CARTESIAN_POINT('Ctrl Pts',(4.91049768391965,5.00446191500343,85.4796179795685));
#139920=CARTESIAN_POINT('Ctrl Pts',(5.04208642632258,4.87534389476987,85.4712497263417));
#139921=CARTESIAN_POINT('Ctrl Pts',(5.16854088277385,4.74107066013652,85.4628814731148));
#139922=CARTESIAN_POINT('Ctrl Pts',(5.28946437627248,4.60208574177453,85.4545132198879));
#139923=CARTESIAN_POINT('Ctrl Pts',(5.41049998310104,4.46297196456503,85.4461372080964));
#139924=CARTESIAN_POINT('Ctrl Pts',(5.52599416368788,4.31913802255369,85.4377611963049));
#139925=CARTESIAN_POINT('Ctrl Pts',(5.63559034434976,4.17106078032577,85.4293851845135));
#139926=CARTESIAN_POINT('Ctrl Pts',(5.74524027233294,4.02291091918843,85.4210050650223));
#139927=CARTESIAN_POINT('Ctrl Pts',(5.84898624206912,3.8705138759804,85.4126249455312));
#139928=CARTESIAN_POINT('Ctrl Pts',(5.94651519299266,3.71437526671814,85.40424482604));
#139929=CARTESIAN_POINT('Ctrl Pts',(6.04415558309692,3.55805824931626,85.3958551312008));
#139930=CARTESIAN_POINT('Ctrl Pts',(6.13556459098704,3.39799140545263,85.3874654363616));
#139931=CARTESIAN_POINT('Ctrl Pts',(6.22047462004968,3.23470586975352,85.3790757415223));
#139932=CARTESIAN_POINT('Ctrl Pts',(6.27438253223083,3.13103870091498,85.3737492690477));
#139933=CARTESIAN_POINT('Ctrl Pts',(6.32567180420869,3.02607461810293,85.3684227965732));
#139934=CARTESIAN_POINT('Ctrl Pts',(6.37428404911103,2.91995366808254,85.3630963240986));
#139935=CARTESIAN_POINT('Ctrl Pts',(6.44560045119588,2.76426934705427,85.3552821436703));
#139936=CARTESIAN_POINT('Ctrl Pts',(6.51127951872477,2.60582038596922,85.347467963242));
#139937=CARTESIAN_POINT('Ctrl Pts',(6.57110895151817,2.44502632087629,85.3396537828137));
#139938=CARTESIAN_POINT('Origin',(0.,0.,50.));
#139939=CARTESIAN_POINT('',(6.57110895151814,2.44502632087636,83.3399710686702));
#139940=CARTESIAN_POINT('',(6.57110895151815,2.44502632087632,83.8871228390383));
#139941=CARTESIAN_POINT('',(6.57110895151814,2.44502632087636,50.));
#139942=CARTESIAN_POINT('',(7.0112498931807,-0.00122387650377896,85.7735343569104));
#139943=CARTESIAN_POINT('Ctrl Pts',(6.57110895151815,2.44502632087633,83.8871228390383));
#139944=CARTESIAN_POINT('Ctrl Pts',(6.49738773721382,2.64315512100245,83.8967308308781));
#139945=CARTESIAN_POINT('Ctrl Pts',(6.41463613204344,2.83812450534434,83.9063388227179));
#139946=CARTESIAN_POINT('Ctrl Pts',(6.32310674446419,3.02918267204397,83.9159468145576));
#139947=CARTESIAN_POINT('Ctrl Pts',(6.28930719915407,3.09973574065968,83.9194948089682));
#139948=CARTESIAN_POINT('Ctrl Pts',(6.25431117822531,3.1697555530712,83.9230428033786));
#139949=CARTESIAN_POINT('Ctrl Pts',(6.21813317189162,3.23920459667509,83.9265907977892));
#139950=CARTESIAN_POINT('Ctrl Pts',(6.13806986340311,3.39289798019116,83.9344426448032));
#139951=CARTESIAN_POINT('Ctrl Pts',(6.0522454551493,3.54373423243355,83.9422944918172));
#139952=CARTESIAN_POINT('Ctrl Pts',(5.96090446899515,3.69123888064884,83.9501463388312));
#139953=CARTESIAN_POINT('Ctrl Pts',(5.86958938640614,3.83870169773852,83.9579959591249));
#139954=CARTESIAN_POINT('Ctrl Pts',(5.77276103852171,3.98283446620419,83.9658455794185));
#139955=CARTESIAN_POINT('Ctrl Pts',(5.67070922211792,4.12318850899238,83.9736951997122));
#139956=CARTESIAN_POINT('Ctrl Pts',(5.56866555324701,4.26353134630457,83.9815441933141));
#139957=CARTESIAN_POINT('Ctrl Pts',(5.46139947098157,4.40009575041923,83.9893931869159));
#139958=CARTESIAN_POINT('Ctrl Pts',(5.3492431453722,4.53246338475984,83.9972421805178));
#139959=CARTESIAN_POINT('Ctrl Pts',(5.23703003829871,4.66489803295845,84.0050951478353));
#139960=CARTESIAN_POINT('Ctrl Pts',(5.1199219880559,4.79313137470459,84.0129481151528));
#139961=CARTESIAN_POINT('Ctrl Pts',(4.99829060256407,4.91677919117991,84.0208010824703));
#139962=CARTESIAN_POINT('Ctrl Pts',(4.87662832678725,5.04045841004593,84.0286560441777));
#139963=CARTESIAN_POINT('Ctrl Pts',(4.75044070458944,5.1595495216934,84.036511005885));
#139964=CARTESIAN_POINT('Ctrl Pts',(4.62013451441192,5.27370682075139,84.0443659675924));
#139965=CARTESIAN_POINT('Ctrl Pts',(4.48969898444844,5.38797743047103,84.0522287260058));
#139966=CARTESIAN_POINT('Ctrl Pts',(4.35513701761826,5.49730420616521,84.0600914844192));
#139967=CARTESIAN_POINT('Ctrl Pts',(4.21688707094716,5.60138286438078,84.0679542428327));
#139968=CARTESIAN_POINT('Ctrl Pts',(4.11546889384688,5.67773347460112,84.0737222495804));
#139969=CARTESIAN_POINT('Ctrl Pts',(4.01206669415905,5.75126069485251,84.0794902563281));
#139970=CARTESIAN_POINT('Ctrl Pts',(3.90686245212008,5.82185986972499,84.0852582630758));
#139971=CARTESIAN_POINT('Ctrl Pts',(3.7540526222726,5.92440561969238,84.0936363295168));
#139972=CARTESIAN_POINT('Ctrl Pts',(3.59710154621307,6.02099952136874,84.1020143959579));
#139973=CARTESIAN_POINT('Ctrl Pts',(3.43650094856868,6.11130818998573,84.1103924623988));
#139974=CARTESIAN_POINT('Ctrl Pts',(3.27601016770459,6.20155510660821,84.1187648000176));
#139975=CARTESIAN_POINT('Ctrl Pts',(3.11187512616021,6.2855251980408,84.1271371376363));
#139976=CARTESIAN_POINT('Ctrl Pts',(2.94461521837978,6.36292918223881,84.135509475255));
#139977=CARTESIAN_POINT('Ctrl Pts',(2.77744515216083,6.4402915898576,84.1438773157776));
#139978=CARTESIAN_POINT('Ctrl Pts',(2.60715386410196,6.5110947848003,84.1522451563002));
#139979=CARTESIAN_POINT('Ctrl Pts',(2.43428437052244,6.57509590545493,84.1606129968227));
#139980=CARTESIAN_POINT('Ctrl Pts',(2.26148240749738,6.63907202440986,84.1689775684926));
#139981=CARTESIAN_POINT('Ctrl Pts',(2.08610455518692,6.69625125394156,84.1773421401625));
#139982=CARTESIAN_POINT('Ctrl Pts',(1.90871321004522,6.74643909364777,84.1857067118324));
#139983=CARTESIAN_POINT('Ctrl Pts',(1.73136519608381,6.79661467402796,84.1940692402979));
#139984=CARTESIAN_POINT('Ctrl Pts',(1.55200498623576,6.83980218131971,84.2024317687635));
#139985=CARTESIAN_POINT('Ctrl Pts',(1.37120995673436,6.87585702418634,84.2107942972291));
#139986=CARTESIAN_POINT('Ctrl Pts',(1.19040049922412,6.91191474434219,84.2191574930506));
#139987=CARTESIAN_POINT('Ctrl Pts',(1.00815631444084,6.94083859267037,84.227520688872));
#139988=CARTESIAN_POINT('Ctrl Pts',(0.825065550168112,6.9625349837847,84.2358838846935));
#139989=CARTESIAN_POINT('Ctrl Pts',(0.641962299472255,6.98423285454941,
84.2442476508682));
#139990=CARTESIAN_POINT('Ctrl Pts',(0.458012680673799,6.99870224634197,
84.2526114170429));
#139991=CARTESIAN_POINT('Ctrl Pts',(0.273810730407882,7.00590138714595,
84.2609751832175));
#139992=CARTESIAN_POINT('Ctrl Pts',(0.0895716594854847,7.01310197873171,
84.2693406348711));
#139993=CARTESIAN_POINT('Ctrl Pts',(-0.0949195157654676,7.01302938503284,
84.2777060865246));
#139994=CARTESIAN_POINT('Ctrl Pts',(-0.279067550917249,7.0056939602387,
84.2860715381781));
#139995=CARTESIAN_POINT('Ctrl Pts',(-0.463277256884167,6.99835607882522,
84.294439791405));
#139996=CARTESIAN_POINT('Ctrl Pts',(-0.647143265211987,6.98375052930749,
84.3028080446318));
#139997=CARTESIAN_POINT('Ctrl Pts',(-0.830073813264486,6.96193967418798,
84.3111762978587));
#139998=CARTESIAN_POINT('Ctrl Pts',(-1.01317396403281,6.94010859729412,
84.3195523096501));
#139999=CARTESIAN_POINT('Ctrl Pts',(-1.19533659458277,6.91105890443951,
84.3279283214416));
#140000=CARTESIAN_POINT('Ctrl Pts',(-1.37597728165275,6.87490458718341,
84.336304333233));
#140001=CARTESIAN_POINT('Ctrl Pts',(-1.55670655714751,6.83873253940344,
84.3446844527241));
#140002=CARTESIAN_POINT('Ctrl Pts',(-1.7359120798368,6.7954489899599,84.3530645722152));
#140003=CARTESIAN_POINT('Ctrl Pts',(-1.913022369512,6.74521845281876,84.3614446917064));
#140004=CARTESIAN_POINT('Ctrl Pts',(-2.09033503012848,6.69493052092602,
84.3698343865455));
#140005=CARTESIAN_POINT('Ctrl Pts',(-2.26554735930746,6.63767983593957,
84.3782240813847));
#140006=CARTESIAN_POINT('Ctrl Pts',(-2.43810443617646,6.57368034823695,
84.3866137762239));
#140007=CARTESIAN_POINT('Ctrl Pts',(-2.54765794651259,6.53304817791536,
84.3919402486987));
#140008=CARTESIAN_POINT('Ctrl Pts',(-2.65614157544202,6.4896967032441,84.3972667211736));
#140009=CARTESIAN_POINT('Ctrl Pts',(-2.76341802457471,6.44369050963465,
84.4025931936484));
#140010=CARTESIAN_POINT('Ctrl Pts',(-2.9322194500587,6.37129893510777,84.4109744940533));
#140011=CARTESIAN_POINT('Ctrl Pts',(-3.09837133545325,6.29218604120235,
84.4193557944583));
#140012=CARTESIAN_POINT('Ctrl Pts',(-3.26131974452749,6.20656266273492,
84.4277370948632));
#140013=CARTESIAN_POINT('Ctrl Pts',(-3.42406164034726,6.12104779936529,
84.4361077731968));
#140014=CARTESIAN_POINT('Ctrl Pts',(-3.58360786318481,6.02903904616464,
84.4444784515304));
#140015=CARTESIAN_POINT('Ctrl Pts',(-3.73942423594185,5.9307953046915,84.452849129864));
#140016=CARTESIAN_POINT('Ctrl Pts',(-3.89506378386816,5.83266305299731,
84.4612103089149));
#140017=CARTESIAN_POINT('Ctrl Pts',(-4.04698164255542,5.7283100892508,84.4695714879657));
#140018=CARTESIAN_POINT('Ctrl Pts',(-4.19466765943043,5.61804145494036,
84.4779326670166));
#140019=CARTESIAN_POINT('Ctrl Pts',(-4.34216203627732,5.50791590719037,
84.4862829964514));
#140020=CARTESIAN_POINT('Ctrl Pts',(-4.48543526301602,5.39189019513191,
84.4946333258861));
#140021=CARTESIAN_POINT('Ctrl Pts',(-4.6240057059312,5.2703128743952,84.5029836553209));
#140022=CARTESIAN_POINT('Ctrl Pts',(-4.76246952717969,5.14882910013415,
84.5113275596767));
#140023=CARTESIAN_POINT('Ctrl Pts',(-4.89623753039063,5.02180244494933,
84.5196714640324));
#140024=CARTESIAN_POINT('Ctrl Pts',(-5.02485984788077,4.8896226921569,84.5280153683882));
#140025=CARTESIAN_POINT('Ctrl Pts',(-5.15337885512325,4.75754910696635,
84.5363525708679));
#140026=CARTESIAN_POINT('Ctrl Pts',(-5.27676019157693,4.62033091295654,
84.5446897733477));
#140027=CARTESIAN_POINT('Ctrl Pts',(-5.39458956112217,4.47839592148034,
84.5530269758274));
#140028=CARTESIAN_POINT('Ctrl Pts',(-5.43337833917123,4.431671705752,84.5557715368633));
#140029=CARTESIAN_POINT('Ctrl Pts',(-5.47156574979735,4.38443663525802,
84.5585160978992));
#140030=CARTESIAN_POINT('Ctrl Pts',(-5.50913790009451,4.33670683355957,
84.5612606589351));
#140031=CARTESIAN_POINT('Ctrl Pts',(-5.62328666333559,4.19169788968678,
84.5695989692369));
#140032=CARTESIAN_POINT('Ctrl Pts',(-5.73165981888591,4.04223901281819,
84.5779372795388));
#140033=CARTESIAN_POINT('Ctrl Pts',(-5.8339240463015,3.88882460191832,84.5862755898406));
#140034=CARTESIAN_POINT('Ctrl Pts',(-5.93625261489894,3.73531366787678,
84.5946191463244));
#140035=CARTESIAN_POINT('Ctrl Pts',(-6.03246440722958,3.57784250843815,
84.6029627028082));
#140036=CARTESIAN_POINT('Ctrl Pts',(-6.12227082116504,3.41693233102605,
84.6113062592919));
#140037=CARTESIAN_POINT('Ctrl Pts',(-6.21214555942866,3.25589973385256,
84.6196561635171));
#140038=CARTESIAN_POINT('Ctrl Pts',(-6.29560503938557,3.09142318564503,
84.6280060677423));
#140039=CARTESIAN_POINT('Ctrl Pts',(-6.3724075710268,2.92404656447539,84.6363559719674));
#140040=CARTESIAN_POINT('Ctrl Pts',(-6.44932530078216,2.75641889075973,
84.644718400431));
#140041=CARTESIAN_POINT('Ctrl Pts',(-6.51956599242606,2.58588274967877,
84.6530808288946));
#140042=CARTESIAN_POINT('Ctrl Pts',(-6.58293633678099,2.41300139833954,
84.6614432573583));
#140043=CARTESIAN_POINT('Ctrl Pts',(-6.646360871419,2.23997220987769,84.6698128368382));
#140044=CARTESIAN_POINT('Ctrl Pts',(-6.70290323615627,2.06459412081998,
84.6781824163181));
#140045=CARTESIAN_POINT('Ctrl Pts',(-6.7524204307408,1.88744400950446,84.686551995798));
#140046=CARTESIAN_POINT('Ctrl Pts',(-6.80201399956481,1.71002066572614,
84.6949344843345));
#140047=CARTESIAN_POINT('Ctrl Pts',(-6.84456067019608,1.53082015625442,
84.703316972871));
#140048=CARTESIAN_POINT('Ctrl Pts',(-6.87996853946176,1.35042936080212,
84.7116994614076));
#140049=CARTESIAN_POINT('Ctrl Pts',(-6.89155457447877,1.29140253664688,
84.7144423490122));
#140050=CARTESIAN_POINT('Ctrl Pts',(-6.90237666812842,1.23224830520737,
84.7171852366167));
#140051=CARTESIAN_POINT('Ctrl Pts',(-6.91243280912772,1.17298730674917,
84.7199281242213));
#140052=CARTESIAN_POINT('Ctrl Pts',(-6.94319220518818,0.991721697740565,
84.7283179793541));
#140053=CARTESIAN_POINT('Ctrl Pts',(-6.96684353899479,0.809090878000783,
84.7367078344869));
#140054=CARTESIAN_POINT('Ctrl Pts',(-6.98327672178235,0.62567786401048,
84.7450976896197));
#140055=CARTESIAN_POINT('Ctrl Pts',(-6.99969474025922,0.442434100978206,
84.7534798027118));
#140056=CARTESIAN_POINT('Ctrl Pts',(-7.00890785683715,0.258409908432713,
84.7618619158039));
#140057=CARTESIAN_POINT('Ctrl Pts',(-7.01085739945249,0.0741962737761583,
84.7702440288959));
#140058=CARTESIAN_POINT('Ctrl Pts',(-7.01280542963595,-0.109874450142781,
84.7786196392448));
#140059=CARTESIAN_POINT('Ctrl Pts',(-7.00750111685177,-0.294133995636706,
84.7869952495937));
#140060=CARTESIAN_POINT('Ctrl Pts',(-6.99493774077816,-0.477988038696947,
84.7953708599425));
#140061=CARTESIAN_POINT('Ctrl Pts',(-6.98238226725466,-0.661726434833925,
84.8037412019081));
#140062=CARTESIAN_POINT('Ctrl Pts',(-6.96257685710609,-0.845059510001265,
84.8121115438737));
#140063=CARTESIAN_POINT('Ctrl Pts',(-6.93556685367154,-1.02739426743224,
84.8204818858393));
#140064=CARTESIAN_POINT('Ctrl Pts',(-6.90856988056705,-1.20964106182103,
84.8288481897336));
#140065=CARTESIAN_POINT('Ctrl Pts',(-6.87437529333649,-1.39089017429523,
84.8372144936279));
#140066=CARTESIAN_POINT('Ctrl Pts',(-6.83308018701985,-1.5705545900276,
84.8455807975222));
#140067=CARTESIAN_POINT('Ctrl Pts',(-6.79179662978701,-1.75016875865863,
84.8539447615958));
#140068=CARTESIAN_POINT('Ctrl Pts',(-6.74341658530487,-1.92819879392908,
84.8623087256695));
#140069=CARTESIAN_POINT('Ctrl Pts',(-6.6880881936738,-2.10406817288346,
84.8706726897431));
#140070=CARTESIAN_POINT('Ctrl Pts',(-6.63276831616276,-2.279910488463,84.8790353667416));
#140071=CARTESIAN_POINT('Ctrl Pts',(-6.57050232194515,-2.45359249722489,
84.8873980437401));
#140072=CARTESIAN_POINT('Ctrl Pts',(-6.50148825500511,-2.62455272999623,
84.8957607207387));
#140073=CARTESIAN_POINT('Ctrl Pts',(-6.43247560893857,-2.79550944300883,
84.904123225565));
#140074=CARTESIAN_POINT('Ctrl Pts',(-6.35671529057448,-2.96374418716424,
84.9124857303913));
#140075=CARTESIAN_POINT('Ctrl Pts',(-6.27445369610728,-3.12871497230183,
84.9208482352176));
#140076=CARTESIAN_POINT('Ctrl Pts',(-6.19218283037093,-3.29370435042393,
84.9292116825376));
#140077=CARTESIAN_POINT('Ctrl Pts',(-6.10340937482096,-3.45542874225314,
84.9375751298576));
#140078=CARTESIAN_POINT('Ctrl Pts',(-6.00842612691498,-3.61336990078589,
84.9459385771775));
#140079=CARTESIAN_POINT('Ctrl Pts',(-5.9133869502033,-3.77140405951145,
84.9543069491303));
#140080=CARTESIAN_POINT('Ctrl Pts',(-5.81213084331041,-3.92565025107858,
84.9626753210831));
#140081=CARTESIAN_POINT('Ctrl Pts',(-5.70499502510914,-4.07561753921783,
84.9710436930359));
#140082=CARTESIAN_POINT('Ctrl Pts',(-5.59782710621671,-4.22562976147604,
84.9794145723717));
#140083=CARTESIAN_POINT('Ctrl Pts',(-5.48477615858953,-4.37136025948501,
84.9877854517074));
#140084=CARTESIAN_POINT('Ctrl Pts',(-5.36622073602579,-4.5123498949823,
84.9961563310432));
#140085=CARTESIAN_POINT('Ctrl Pts',(-5.24756486273458,-4.6534589894731,
85.0045343029345));
#140086=CARTESIAN_POINT('Ctrl Pts',(-5.12339541104173,-4.78981894672686,
85.0129122748258));
#140087=CARTESIAN_POINT('Ctrl Pts',(-4.99412973283502,-4.92100546373536,
85.021290246717));
#140088=CARTESIAN_POINT('Ctrl Pts',(-4.91198034171884,-5.00437556355154,
85.0266145160761));
#140089=CARTESIAN_POINT('Ctrl Pts',(-4.8277734846779,-5.08565699865557,
85.0319387854352));
#140090=CARTESIAN_POINT('Ctrl Pts',(-4.74162354313436,-5.1647490488594,
85.0372630547943));
#140091=CARTESIAN_POINT('Ctrl Pts',(-4.6143981152607,-5.28155144881807,
85.0451258859836));
#140092=CARTESIAN_POINT('Ctrl Pts',(-4.4826686277116,-5.3938197787296,85.0529887171729));
#140093=CARTESIAN_POINT('Ctrl Pts',(-4.34680621465642,-5.50117281083992,
85.0608515483622));
#140094=CARTESIAN_POINT('Ctrl Pts',(-4.2110481939321,-5.60844335631544,
85.0687083380035));
#140095=CARTESIAN_POINT('Ctrl Pts',(-4.07116386007433,-5.71080587976405,
85.0765651276449));
#140096=CARTESIAN_POINT('Ctrl Pts',(-3.92756051208471,-5.80791657880973,
85.0844219172863));
#140097=CARTESIAN_POINT('Ctrl Pts',(-3.78403814958545,-5.90497251201818,
85.0922742760703));
#140098=CARTESIAN_POINT('Ctrl Pts',(-3.63680125991,-5.99678229956863,85.1001266348543));
#140099=CARTESIAN_POINT('Ctrl Pts',(-3.48628926875464,-6.08304312799657,
85.1079789936382));
#140100=CARTESIAN_POINT('Ctrl Pts',(-3.33581281523649,-6.16928358923646,
85.1158294983887));
#140101=CARTESIAN_POINT('Ctrl Pts',(-3.18206312559944,-6.24997750223117,
85.1236800031391));
#140102=CARTESIAN_POINT('Ctrl Pts',(-3.02550753064711,-6.32486606534064,
85.1315305078896));
#140103=CARTESIAN_POINT('Ctrl Pts',(-2.86897712055583,-6.39974258124058,
85.1393797497412));
#140104=CARTESIAN_POINT('Ctrl Pts',(-2.70964204919406,-6.46881544444646,
85.1472289915928));
#140105=CARTESIAN_POINT('Ctrl Pts',(-2.5479926768134,-6.53187261674669,
85.1550782334445));
#140106=CARTESIAN_POINT('Ctrl Pts',(-2.3862888415952,-6.59495103424251,
85.1629301198593));
#140107=CARTESIAN_POINT('Ctrl Pts',(-2.22226950364215,-6.65200957364057,
85.1707820062742));
#140108=CARTESIAN_POINT('Ctrl Pts',(-2.05644354296371,-6.70288493986753,
85.1786338926891));
#140109=CARTESIAN_POINT('Ctrl Pts',(-1.93467960403323,-6.74024208805458,
85.184399435153));
#140110=CARTESIAN_POINT('Ctrl Pts',(-1.81194197276745,-6.77426641776551,
85.1901649776169));
#140111=CARTESIAN_POINT('Ctrl Pts',(-1.6884365793264,-6.80491061514349,
85.1959305200808));
#140112=CARTESIAN_POINT('Ctrl Pts',(-1.4816074437768,-6.85622912583124,
85.2055858244408));
#140113=CARTESIAN_POINT('Ctrl Pts',(-1.27273050458853,-6.89804131974567,
85.2152411288009));
#140114=CARTESIAN_POINT('Ctrl Pts',(-1.06260573728889,-6.93025941863512,
85.2248964331609));
#140115=CARTESIAN_POINT('Ctrl Pts',(-0.851316918197482,-6.96265599974835,
85.2346052260958));
#140116=CARTESIAN_POINT('Ctrl Pts',(-0.638766462157638,-6.9853519393606,
85.2443140190308));
#140117=CARTESIAN_POINT('Ctrl Pts',(-0.425764535490945,-6.99831059062244,
85.2540228119657));
#140118=CARTESIAN_POINT('Ctrl Pts',(-0.211737625466373,-7.01133160001452,
85.2637783244366));
#140119=CARTESIAN_POINT('Ctrl Pts',(0.0027450660271163,-7.01452140358428,
85.2735338369075));
#140120=CARTESIAN_POINT('Ctrl Pts',(0.216865565674253,-7.00789525384939,
85.2832893493784));
#140121=CARTESIAN_POINT('Ctrl Pts',(0.431198077557214,-7.00126254320687,
85.2930545213075));
#140122=CARTESIAN_POINT('Ctrl Pts',(0.645167642284201,-6.98479445078955,
85.3028196932365));
#140123=CARTESIAN_POINT('Ctrl Pts',(0.857958406954577,-6.95855832298875,
85.3125848651656));
#140124=CARTESIAN_POINT('Ctrl Pts',(1.0704590362451,-6.93235796755296,85.3223367225043));
#140125=CARTESIAN_POINT('Ctrl Pts',(1.28178404017231,-6.89641620030262,
85.332088579843));
#140126=CARTESIAN_POINT('Ctrl Pts',(1.49112599183645,-6.85085176010763,
85.3418404371818));
#140127=CARTESIAN_POINT('Ctrl Pts',(1.58241424400673,-6.83098236425337,
85.3460929532436));
#140128=CARTESIAN_POINT('Ctrl Pts',(1.67332546939955,-6.8092837923712,85.3503454693054));
#140129=CARTESIAN_POINT('Ctrl Pts',(1.7637930474779,-6.7857689798702,85.3545979853672));
#140130=CARTESIAN_POINT('Ctrl Pts',(1.93468721209517,-6.74134926262067,
85.3626310309659));
#140131=CARTESIAN_POINT('Ctrl Pts',(2.10408073117386,-6.69042322326595,
85.3706640765646));
#140132=CARTESIAN_POINT('Ctrl Pts',(2.27143590990466,-6.63311431152031,
85.3786971221633));
#140133=CARTESIAN_POINT('Ctrl Pts',(2.43868350628287,-6.57584224014972,
85.386725003811));
#140134=CARTESIAN_POINT('Ctrl Pts',(2.60389502519156,-6.51219558208228,
85.3947528854587));
#140135=CARTESIAN_POINT('Ctrl Pts',(2.76654609548661,-6.44234811726655,
85.4027807671064));
#140136=CARTESIAN_POINT('Ctrl Pts',(2.92912372722047,-6.37253218926953,
85.4108050240864));
#140137=CARTESIAN_POINT('Ctrl Pts',(3.08914287607793,-6.29652117344199,
85.4188292810664));
#140138=CARTESIAN_POINT('Ctrl Pts',(3.24609743406952,-6.21453763453302,
85.4268535380464));
#140139=CARTESIAN_POINT('Ctrl Pts',(3.40303301465615,-6.13256400826907,
85.434876824812));
#140140=CARTESIAN_POINT('Ctrl Pts',(3.55690441413499,-6.04461946008426,
85.4429001115776));
#140141=CARTESIAN_POINT('Ctrl Pts',(3.70722834420979,-5.95097341334907,
85.4509233983432));
#140142=CARTESIAN_POINT('Ctrl Pts',(3.85753995657948,-5.85733504007206,
85.458946027672));
#140143=CARTESIAN_POINT('Ctrl Pts',(4.00430436948424,-5.75799629611166,
85.4669686570008));
#140144=CARTESIAN_POINT('Ctrl Pts',(4.14706587135866,-5.65327084271683,
85.4749912863297));
#140145=CARTESIAN_POINT('Ctrl Pts',(4.28988104139407,-5.54850602000731,
85.483016931596));
#140146=CARTESIAN_POINT('Ctrl Pts',(4.42869000029797,-5.438350661938,85.4910425768622));
#140147=CARTESIAN_POINT('Ctrl Pts',(4.56306852048824,-5.32315998630788,
85.4990682221285));
#140148=CARTESIAN_POINT('Ctrl Pts',(4.64230628462617,-5.25523654457371,
85.5038006316368));
#140149=CARTESIAN_POINT('Ctrl Pts',(4.7200042127329,-5.18556308635372,85.5085330411452));
#140150=CARTESIAN_POINT('Ctrl Pts',(4.79608113605184,-5.11421864011578,
85.5132654506535));
#140151=CARTESIAN_POINT('Ctrl Pts',(4.93642301783713,-4.98260693181908,
85.5219954994883));
#140152=CARTESIAN_POINT('Ctrl Pts',(5.07131689687424,-4.84524115005751,
85.5307255483232));
#140153=CARTESIAN_POINT('Ctrl Pts',(5.20031566070795,-4.70258903068253,
85.539455597158));
#140154=CARTESIAN_POINT('Ctrl Pts',(5.32935172469491,-4.55989566326953,
85.5481881702973));
#140155=CARTESIAN_POINT('Ctrl Pts',(5.45248908730617,-4.41191311035823,
85.5569207434366));
#140156=CARTESIAN_POINT('Ctrl Pts',(5.56931982371442,-4.25914348944499,
85.565653316576));
#140157=CARTESIAN_POINT('Ctrl Pts',(5.68781032722699,-4.10420353220479,
85.5745099498563));
#140158=CARTESIAN_POINT('Ctrl Pts',(5.7998134713801,-3.94433968467133,85.5833665831367));
#140159=CARTESIAN_POINT('Ctrl Pts',(5.90494791393622,-3.7801080270543,85.592223216417));
#140160=CARTESIAN_POINT('Ctrl Pts',(6.00867566453458,-3.61807377826315,
85.6009613485239));
#140161=CARTESIAN_POINT('Ctrl Pts',(6.10571724735984,-3.45178812195945,
85.6096994806309));
#140162=CARTESIAN_POINT('Ctrl Pts',(6.1957511687176,-3.28181261162706,85.6184376127378));
#140163=CARTESIAN_POINT('Ctrl Pts',(6.28761656707702,-3.10837944629839,
85.6273534966048));
#140164=CARTESIAN_POINT('Ctrl Pts',(6.37218600734555,-2.93110496034485,
85.6362693804719));
#140165=CARTESIAN_POINT('Ctrl Pts',(6.44916779686221,-2.75061107581852,
85.6451852643389));
#140166=CARTESIAN_POINT('Ctrl Pts',(6.52614958637886,-2.57011719129218,
85.654101148206));
#140167=CARTESIAN_POINT('Ctrl Pts',(6.59554361209846,-2.38640418874775,
85.663017032073));
#140168=CARTESIAN_POINT('Ctrl Pts',(6.6571103512007,-2.20011552752043,85.6719329159401));
#140169=CARTESIAN_POINT('Ctrl Pts',(6.71682758852012,-2.01942308945004,
85.6805809613062));
#140170=CARTESIAN_POINT('Ctrl Pts',(6.76919104950747,-1.83627650196859,
85.6892290066724));
#140171=CARTESIAN_POINT('Ctrl Pts',(6.81402159556653,-1.65128321545791,
85.6978770520385));
#140172=CARTESIAN_POINT('Ctrl Pts',(6.85884212225513,-1.46633127388795,
85.706523164616));
#140173=CARTESIAN_POINT('Ctrl Pts',(6.89613302745462,-1.27953373814732,
85.7151692771935));
#140174=CARTESIAN_POINT('Ctrl Pts',(6.92576572928662,-1.09151070793603,
85.723815389771));
#140175=CARTESIAN_POINT('Ctrl Pts',(6.95539404940833,-0.903515480199485,
85.7324602238704));
#140176=CARTESIAN_POINT('Ctrl Pts',(6.97736638061632,-0.714295404980135,
85.7411050579698));
#140177=CARTESIAN_POINT('Ctrl Pts',(6.99160555274235,-0.524479129577489,
85.7497498920692));
#140178=CARTESIAN_POINT('Ctrl Pts',(7.00466426059438,-0.350399115367159,
85.7576780470163));
#140179=CARTESIAN_POINT('Ctrl Pts',(7.01121941622546,-0.175817921304171,
85.7656062019633));
#140180=CARTESIAN_POINT('Ctrl Pts',(7.0112498931807,-0.00122387650377896,
85.7735343569104));
#140181=CARTESIAN_POINT('Ctrl Pts',(7.0112498931807,-0.00122387650377896,
85.7735343569104));
#140182=CARTESIAN_POINT('Ctrl Pts',(7.01128645483302,0.208227714535148,
85.783045360963));
#140183=CARTESIAN_POINT('Ctrl Pts',(7.00193253296366,0.417672943101291,
85.7925563650157));
#140184=CARTESIAN_POINT('Ctrl Pts',(6.98321925767691,0.626318897775227,
85.8020673690684));
#140185=CARTESIAN_POINT('Ctrl Pts',(6.96450598239016,0.834964852449163,
85.8115783731211));
#140186=CARTESIAN_POINT('Ctrl Pts',(6.936433353249,1.04281133667788,85.8210893771738));
#140187=CARTESIAN_POINT('Ctrl Pts',(6.89909079732583,1.24906874620818,85.8306003812265));
#140188=CARTESIAN_POINT('Ctrl Pts',(6.86758001900332,1.42311498777922,85.8386260541597));
#140189=CARTESIAN_POINT('Ctrl Pts',(6.82945868340738,1.59607951497589,85.8466517270929));
#140190=CARTESIAN_POINT('Ctrl Pts',(6.78482559613212,1.76741851087129,85.8546774000261));
#140191=CARTESIAN_POINT('Ctrl Pts',(6.7402070079453,1.93870184717851,85.862700465814));
#140192=CARTESIAN_POINT('Ctrl Pts',(6.68908097230586,2.10836034930558,85.8707235316019));
#140193=CARTESIAN_POINT('Ctrl Pts',(6.6315971395063,2.27586158230061,85.8787465973898));
#140194=CARTESIAN_POINT('Ctrl Pts',(6.6121586370834,2.3325031276681,85.8814596451489));
#140195=CARTESIAN_POINT('Ctrl Pts',(6.59199354854759,2.38889810609303,85.8841726929079));
#140196=CARTESIAN_POINT('Ctrl Pts',(6.57110895151818,2.44502632087624,85.8868857406669));
#140197=CARTESIAN_POINT('',(7.0112496259069,0.00229035375375721,85.2264656431173));
#140198=CARTESIAN_POINT('Ctrl Pts',(6.57110895151817,2.44502632087629,85.3396537828137));
#140199=CARTESIAN_POINT('Ctrl Pts',(6.63643246135932,2.26946669740855,85.3311220340025));
#140200=CARTESIAN_POINT('Ctrl Pts',(6.69478191749844,2.09111139416079,85.3225902851913));
#140201=CARTESIAN_POINT('Ctrl Pts',(6.7459248106977,1.91053003402543,85.3140585363801));
#140202=CARTESIAN_POINT('Ctrl Pts',(6.79696816595605,1.73030013419337,85.305543392666));
#140203=CARTESIAN_POINT('Ctrl Pts',(6.8408328570105,1.54785311280165,85.297028248952));
#140204=CARTESIAN_POINT('Ctrl Pts',(6.87733538502663,1.36377584828323,85.2885131052379));
#140205=CARTESIAN_POINT('Ctrl Pts',(6.91379513375401,1.17991431387664,85.2800079408818));
#140206=CARTESIAN_POINT('Ctrl Pts',(6.94290985966027,0.994426642296124,
85.2715027765256));
#140207=CARTESIAN_POINT('Ctrl Pts',(6.96454604335369,0.807913963554614,
85.2629976121695));
#140208=CARTESIAN_POINT('Ctrl Pts',(6.9861498619863,0.621680284763982,85.2545051704896));
#140209=CARTESIAN_POINT('Ctrl Pts',(7.00029741943712,0.434424959180303,
85.2460127288098));
#140210=CARTESIAN_POINT('Ctrl Pts',(7.00690637091511,0.246758326565235,
85.2375202871299));
#140211=CARTESIAN_POINT('Ctrl Pts',(7.00977400343826,0.165329533966482,
85.2338354057923));
#140212=CARTESIAN_POINT('Ctrl Pts',(7.01122299162676,0.083823429776159,
85.2301505244548));
#140213=CARTESIAN_POINT('Ctrl Pts',(7.0112496259069,0.00229035375353233,
85.2264656431173));
#140214=CARTESIAN_POINT('Ctrl Pts',(7.01124962590711,0.00229035313782153,
85.2264656430894));
#140215=CARTESIAN_POINT('Ctrl Pts',(7.0113027197677,-0.160241050471218,
85.2191200483304));
#140216=CARTESIAN_POINT('Ctrl Pts',(7.00570090552392,-0.322819188341104,
85.2117744535713));
#140217=CARTESIAN_POINT('Ctrl Pts',(6.99445468411541,-0.485005396213237,
85.2044288588122));
#140218=CARTESIAN_POINT('Ctrl Pts',(6.98168859955592,-0.669110151834753,
85.1960905485098));
#140219=CARTESIAN_POINT('Ctrl Pts',(6.96165456191588,-0.852634902371005,
85.1877522382073));
#140220=CARTESIAN_POINT('Ctrl Pts',(6.93443749546681,-1.03498946079852,
85.1794139279049));
#140221=CARTESIAN_POINT('Ctrl Pts',(6.90720330496308,-1.21745875052638,
85.1710703714206));
#140222=CARTESIAN_POINT('Ctrl Pts',(6.87277711967582,-1.39875605555216,
85.1627268149362));
#140223=CARTESIAN_POINT('Ctrl Pts',(6.83129500348328,-1.57830134571454,
85.1543832584519));
#140224=CARTESIAN_POINT('Ctrl Pts',(6.78978132787762,-1.75798323315082,
85.1460333542262));
#140225=CARTESIAN_POINT('Ctrl Pts',(6.74120108739037,-1.93591012809273,
85.1376834500005));
#140226=CARTESIAN_POINT('Ctrl Pts',(6.68574033314417,-2.1115166966589,85.1293335457747));
#140227=CARTESIAN_POINT('Ctrl Pts',(6.63019639187041,-2.28738666208392,
85.1209711173105));
#140228=CARTESIAN_POINT('Ctrl Pts',(6.56775141247074,-2.46092903365332,
85.1126086888463));
#140229=CARTESIAN_POINT('Ctrl Pts',(6.49864031173796,-2.63159659924433,
85.1042462603821));
#140230=CARTESIAN_POINT('Ctrl Pts',(6.42947011159252,-2.80241010887009,
85.0958766809016));
#140231=CARTESIAN_POINT('Ctrl Pts',(6.35362255080235,-2.97034360957441,
85.087507101421));
#140232=CARTESIAN_POINT('Ctrl Pts',(6.27137897487613,-3.13487357256742,
85.0791375219405));
#140233=CARTESIAN_POINT('Ctrl Pts',(6.18900854825477,-3.29965730298169,
85.0707550334034));
#140234=CARTESIAN_POINT('Ctrl Pts',(6.10022255077677,-3.46102671902273,
85.0623725448662));
#140235=CARTESIAN_POINT('Ctrl Pts',(6.00534691035419,-3.61848518703606,
85.0539900563291));
#140236=CARTESIAN_POINT('Ctrl Pts',(5.97430204621783,-3.67000817781451,
85.051247168728));
#140237=CARTESIAN_POINT('Ctrl Pts',(5.94260549252674,-3.72111267157982,
85.0485042811269));
#140238=CARTESIAN_POINT('Ctrl Pts',(5.9102696167998,-3.77178202170184,85.0457613935259));
#140239=CARTESIAN_POINT('Ctrl Pts',(5.81136169478708,-3.92676777723307,
85.0373715383932));
#140240=CARTESIAN_POINT('Ctrl Pts',(5.70626946418409,-4.07799285774473,
85.0289816832605));
#140241=CARTESIAN_POINT('Ctrl Pts',(5.59530278198467,-4.22495128260843,
85.0205918281278));
#140242=CARTESIAN_POINT('Ctrl Pts',(5.48443849828378,-4.3717740962981,85.0122097150358));
#140243=CARTESIAN_POINT('Ctrl Pts',(5.36771076660022,-4.51433784209083,
85.0038276019438));
#140244=CARTESIAN_POINT('Ctrl Pts',(5.24547289993513,-4.65216515383387,
84.9954454888518));
#140245=CARTESIAN_POINT('Ctrl Pts',(5.12332986394706,-4.78988554079461,
84.987069878503));
#140246=CARTESIAN_POINT('Ctrl Pts',(4.99568543275772,-4.92287657442269,
84.9786942681542));
#140247=CARTESIAN_POINT('Ctrl Pts',(4.86293366036747,-5.05069329670344,
84.9703186578054));
#140248=CARTESIAN_POINT('Ctrl Pts',(4.73026539081347,-5.17842962036775,
84.9619483158399));
#140249=CARTESIAN_POINT('Ctrl Pts',(4.59249642187637,-5.30099789488781,
84.9535779738744));
#140250=CARTESIAN_POINT('Ctrl Pts',(4.45005850014875,-5.41798910184894,
84.9452076319089));
#140251=CARTESIAN_POINT('Ctrl Pts',(4.30768929418927,-5.53492386920076,
84.9368413280147));
#140252=CARTESIAN_POINT('Ctrl Pts',(4.16065588070923,-5.64628672606212,
84.9284750241205));
#140253=CARTESIAN_POINT('Ctrl Pts',(4.00942434249912,-5.75170783370257,
84.9201087202262));
#140254=CARTESIAN_POINT('Ctrl Pts',(3.85823509951156,-5.85709945801394,
84.9117447561527));
#140255=CARTESIAN_POINT('Ctrl Pts',(3.70285034147758,-5.95655245762958,
84.9033807920791));
#140256=CARTESIAN_POINT('Ctrl Pts',(3.54376693569539,-6.04973904131179,
84.8950168280056));
#140257=CARTESIAN_POINT('Ctrl Pts',(3.38470801020584,-6.14291128512727,
84.8866541510071));
#140258=CARTESIAN_POINT('Ctrl Pts',(3.22195185526411,-6.22981886955667,
84.8782914740087));
#140259=CARTESIAN_POINT('Ctrl Pts',(3.05602221405779,-6.31017866543296,
84.8699287970103));
#140260=CARTESIAN_POINT('Ctrl Pts',(2.89009598903941,-6.39053680684799,
84.861566292184));
#140261=CARTESIAN_POINT('Ctrl Pts',(2.72099670399854,-6.46434728562765,
84.8532037873578));
#140262=CARTESIAN_POINT('Ctrl Pts',(2.54927085694879,-6.53137387234964,
84.8448412825316));
#140263=CARTESIAN_POINT('Ctrl Pts',(2.37752565558749,-6.59840801328356,
84.8364778352117));
#140264=CARTESIAN_POINT('Ctrl Pts',(2.20315360836471,-6.65865661882262,
84.8281143878918));
#140265=CARTESIAN_POINT('Ctrl Pts',(2.02671965931391,-6.71193220950946,
84.8197509405719));
#140266=CARTESIAN_POINT('Ctrl Pts',(1.85018182099553,-6.76523917036132,
84.8113825686192));
#140267=CARTESIAN_POINT('Ctrl Pts',(1.67157996945443,-6.81156481575794,
84.8030141966665));
#140268=CARTESIAN_POINT('Ctrl Pts',(1.49149363220141,-6.85077173080542,
84.7946458247138));
#140269=CARTESIAN_POINT('Ctrl Pts',(1.31135333637552,-6.88999039326925,
84.7862749453782));
#140270=CARTESIAN_POINT('Ctrl Pts',(1.12972799025958,-6.92208600756016,
84.7779040660425));
#140271=CARTESIAN_POINT('Ctrl Pts',(0.947206404689178,-6.94697247651204,
84.7695331867069));
#140272=CARTESIAN_POINT('Ctrl Pts',(0.764530170552582,-6.97188003150002,
84.7611552148157));
#140273=CARTESIAN_POINT('Ctrl Pts',(0.580956506222909,-6.98956619670947,
84.7527772429245));
#140274=CARTESIAN_POINT('Ctrl Pts',(0.397079586609618,-6.99999674031338,
84.7443992710333));
#140275=CARTESIAN_POINT('Ctrl Pts',(0.280224306853785,-7.00662543571139,
84.7390750016732));
#140276=CARTESIAN_POINT('Ctrl Pts',(0.163246613162165,-7.01032484772495,
84.7337507323131));
#140277=CARTESIAN_POINT('Ctrl Pts',(0.046298896562297,-7.01109713059783,
84.728426462953));
#140278=CARTESIAN_POINT('Ctrl Pts',(-0.126408397416104,-7.01223763072078,
84.7205636317637));
#140279=CARTESIAN_POINT('Ctrl Pts',(-0.299409378148772,-7.00699392432741,
84.7127008005744));
#140280=CARTESIAN_POINT('Ctrl Pts',(-0.47217304318999,-6.99533267113043,
84.7048379693851));
#140281=CARTESIAN_POINT('Ctrl Pts',(-0.644803962158934,-6.98368037806727,
84.6969811797436));
#140282=CARTESIAN_POINT('Ctrl Pts',(-0.817197550110116,-6.96562036978883,
84.6891243901022));
#140283=CARTESIAN_POINT('Ctrl Pts',(-0.98882113102915,-6.94117132286261,
84.6812676004608));
#140284=CARTESIAN_POINT('Ctrl Pts',(-1.16034792437314,-6.91673606404144,
84.6734152416769));
#140285=CARTESIAN_POINT('Ctrl Pts',(-1.33110519821854,-6.88591898759914,
84.6655628828929));
#140286=CARTESIAN_POINT('Ctrl Pts',(-1.50056398818207,-6.84879071660619,
84.6577105241089));
#140287=CARTESIAN_POINT('Ctrl Pts',(-1.66998276694762,-6.81167121203132,
84.6498600193585));
#140288=CARTESIAN_POINT('Ctrl Pts',(-1.83810329812025,-6.76824355199597,
84.6420095146081));
#140289=CARTESIAN_POINT('Ctrl Pts',(-2.00440548712252,-6.71862971190504,
84.6341590098576));
#140290=CARTESIAN_POINT('Ctrl Pts',(-2.17068092334406,-6.66902385311726,
84.626309768006));
#140291=CARTESIAN_POINT('Ctrl Pts',(-2.33513823495855,-6.61323390730317,
84.6184605261543));
#140292=CARTESIAN_POINT('Ctrl Pts',(-2.49727165793425,-6.55143196782034,
84.6106112843027));
#140293=CARTESIAN_POINT('Ctrl Pts',(-2.65945970683386,-6.48960920605435,
84.6027593978878));
#140294=CARTESIAN_POINT('Ctrl Pts',(-2.81932194635356,-6.42177054070239,
84.5949075114729));
#140295=CARTESIAN_POINT('Ctrl Pts',(-2.97637161427554,-6.34813662236682,
84.587055625058));
#140296=CARTESIAN_POINT('Ctrl Pts',(-3.0916912306694,-6.29406815263753,
84.5812900825942));
#140297=CARTESIAN_POINT('Ctrl Pts',(-3.20549475450005,-6.23687602814215,
84.5755245401304));
#140298=CARTESIAN_POINT('Ctrl Pts',(-3.31759780661831,-6.17666344849882,
84.5697589976666));
#140299=CARTESIAN_POINT('Ctrl Pts',(-3.50533193478754,-6.07582804811887,
84.5601036933068));
#140300=CARTESIAN_POINT('Ctrl Pts',(-3.68820103973235,-5.96657272449971,
84.5504483889469));
#140301=CARTESIAN_POINT('Ctrl Pts',(-3.86555333472027,-5.84936953687601,
84.5407930845871));
#140302=CARTESIAN_POINT('Ctrl Pts',(-4.04388812814646,-5.73151706558328,
84.5310842916527));
#140303=CARTESIAN_POINT('Ctrl Pts',(-4.21664480893165,-5.60562849867982,
84.5213754987183));
#140304=CARTESIAN_POINT('Ctrl Pts',(-4.38319836814722,-5.47222063041793,
84.5116667057838));
#140305=CARTESIAN_POINT('Ctrl Pts',(-4.55055339723575,-5.33817079216313,
84.5019111933132));
#140306=CARTESIAN_POINT('Ctrl Pts',(-4.71164544245118,-5.19652915717362,
84.4921556808426));
#140307=CARTESIAN_POINT('Ctrl Pts',(-4.86587855489121,-5.04785622334371,
84.482400168372));
#140308=CARTESIAN_POINT('Ctrl Pts',(-5.02026438184013,-4.89903608043713,
84.4726349964432));
#140309=CARTESIAN_POINT('Ctrl Pts',(-5.16777767181834,-4.7431707476206,
84.4628698245144));
#140310=CARTESIAN_POINT('Ctrl Pts',(-5.30785902361878,-4.58085790522787,
84.4531046525857));
#140311=CARTESIAN_POINT('Ctrl Pts',(-5.44774937767532,-4.41876637271192,
84.4433527952472));
#140312=CARTESIAN_POINT('Ctrl Pts',(-5.58022802157599,-4.25024492948965,
84.4336009379087));
#140313=CARTESIAN_POINT('Ctrl Pts',(-5.70477630387564,-4.07592368491352,
84.4238490805702));
#140314=CARTESIAN_POINT('Ctrl Pts',(-5.75908837518318,-3.99990699732036,
84.4195965645068));
#140315=CARTESIAN_POINT('Ctrl Pts',(-5.81189291195392,-3.92278786981612,
84.4153440484434));
#140316=CARTESIAN_POINT('Ctrl Pts',(-5.86314922750574,-3.84462061827937,
84.4110915323801));
#140317=CARTESIAN_POINT('Ctrl Pts',(-5.95997292291812,-3.6969618942268,
84.4030584867812));
#140318=CARTESIAN_POINT('Ctrl Pts',(-6.05131610743977,-3.54548896452306,
84.3950254411823));
#140319=CARTESIAN_POINT('Ctrl Pts',(-6.13686318753471,-3.39065432917916,
84.3869923955834));
#140320=CARTESIAN_POINT('Ctrl Pts',(-6.22235527467286,-3.23591922750024,
84.3789645139355));
#140321=CARTESIAN_POINT('Ctrl Pts',(-6.3020584974621,-3.07782704128684,
84.3709366322877));
#140322=CARTESIAN_POINT('Ctrl Pts',(-6.37570092852467,-2.91685862401826,
84.3629087506398));
#140323=CARTESIAN_POINT('Ctrl Pts',(-6.44931010930364,-2.75596288557692,
84.3548844936596));
#140324=CARTESIAN_POINT('Ctrl Pts',(-6.51686379487021,-2.59219383448413,
84.3468602366794));
#140325=CARTESIAN_POINT('Ctrl Pts',(-6.57813634697964,-2.42605621596975,
84.3388359796993));
#140326=CARTESIAN_POINT('Ctrl Pts',(-6.63940149061342,-2.25993868518564,
84.3308126929335));
#140327=CARTESIAN_POINT('Ctrl Pts',(-6.69438687948976,-2.09145349846441,
84.3227894061678));
#140328=CARTESIAN_POINT('Ctrl Pts',(-6.74291524803591,-1.92112480601984,
84.314766119402));
#140329=CARTESIAN_POINT('Ctrl Pts',(-6.79143964011542,-1.75081007049133,
84.306743490073));
#140330=CARTESIAN_POINT('Ctrl Pts',(-6.83350796917286,-1.57865248384781,
84.2987208607439));
#140331=CARTESIAN_POINT('Ctrl Pts',(-6.86899310809759,-1.40519046517112,
84.2906982314149));
#140332=CARTESIAN_POINT('Ctrl Pts',(-6.9044915869081,-1.23166323712545,
84.2826725861484));
#140333=CARTESIAN_POINT('Ctrl Pts',(-6.93340186116331,-1.05683095741906,
84.274646940882));
#140334=CARTESIAN_POINT('Ctrl Pts',(-6.95564803756212,-0.881241703540063,
84.2666212956155));
#140335=CARTESIAN_POINT('Ctrl Pts',(-6.96876573878057,-0.777703579582816,
84.2618888861082));
#140336=CARTESIAN_POINT('Ctrl Pts',(-6.97956731078841,-0.673902400158773,
84.2571564766009));
#140337=CARTESIAN_POINT('Ctrl Pts',(-6.98804566086238,-0.569951229670105,
84.2524240670936));
#140338=CARTESIAN_POINT('Ctrl Pts',(-7.00368598321142,-0.378188705025704,
84.2436940182591));
#140339=CARTESIAN_POINT('Ctrl Pts',(-7.01142552498646,-0.185819746794032,
84.2349639694246));
#140340=CARTESIAN_POINT('Ctrl Pts',(-7.01124697880517,0.0065088167410221,
84.22623392059));
#140341=CARTESIAN_POINT('Ctrl Pts',(-7.01106838099703,0.198892992320853,
84.217501347451));
#140342=CARTESIAN_POINT('Ctrl Pts',(-7.00296712547114,0.391236475947701,
84.2087687743119));
#140343=CARTESIAN_POINT('Ctrl Pts',(-6.98697803043323,0.582893270456414,
84.2000362011728));
#140344=CARTESIAN_POINT('Ctrl Pts',(-6.97076178477665,0.777272855676073,
84.1911795678924));
#140345=CARTESIAN_POINT('Ctrl Pts',(-6.94643189688875,0.970945803205776,
84.1823229346119));
#140346=CARTESIAN_POINT('Ctrl Pts',(-6.9140791160314,1.16324397258634,84.1734663013314));
#140347=CARTESIAN_POINT('Ctrl Pts',(-6.88215921326528,1.35296920504148,
84.1647281692248));
#140348=CARTESIAN_POINT('Ctrl Pts',(-6.84242984472171,1.54135594969713,
84.1559900371182));
#140349=CARTESIAN_POINT('Ctrl Pts',(-6.79502978745767,1.7277721927566,84.1472519050116));
#140350=CARTESIAN_POINT('Ctrl Pts',(-6.7466655145538,1.91798052948543,84.1383360211442));
#140351=CARTESIAN_POINT('Ctrl Pts',(-6.69031520398364,2.10613704969951,
84.1294201372768));
#140352=CARTESIAN_POINT('Ctrl Pts',(-6.62618024995488,2.29158500990206,
84.1205042534095));
#140353=CARTESIAN_POINT('Ctrl Pts',(-6.56204529592617,2.4770329701045,84.1115883695421));
#140354=CARTESIAN_POINT('Ctrl Pts',(-6.49012580302942,2.65977208648038,
84.1026724856747));
#140355=CARTESIAN_POINT('Ctrl Pts',(-6.41067628819547,2.83916468181548,
84.0937566018073));
#140356=CARTESIAN_POINT('Ctrl Pts',(-6.33278797640512,3.01503216731923,
84.085015917311));
#140357=CARTESIAN_POINT('Ctrl Pts',(-6.24765455686776,3.18770210982274,
84.0762752328146));
#140358=CARTESIAN_POINT('Ctrl Pts',(-6.15555931687341,3.35659292422434,
84.0675345483183));
#140359=CARTESIAN_POINT('Ctrl Pts',(-6.06348064634292,3.52545335236228,
84.0587954364164));
#140360=CARTESIAN_POINT('Ctrl Pts',(-5.96444278781828,3.69053576997316,
84.0500563245144));
#140361=CARTESIAN_POINT('Ctrl Pts',(-5.8587749031339,3.85128331818219,84.0413172126125));
#140362=CARTESIAN_POINT('Ctrl Pts',(-5.75173793892203,4.01411358223249,
84.0324648729382));
#140363=CARTESIAN_POINT('Ctrl Pts',(-5.63789808562434,4.17249561437917,
84.0236125332639));
#140364=CARTESIAN_POINT('Ctrl Pts',(-5.51764347796998,4.32587991193877,
84.0147601935896));
#140365=CARTESIAN_POINT('Ctrl Pts',(-5.39898786138037,4.47722470243869,
84.0060255609397));
#140366=CARTESIAN_POINT('Ctrl Pts',(-5.27408720561891,4.62370362733829,
83.9972909282898));
#140367=CARTESIAN_POINT('Ctrl Pts',(-5.1433562343071,4.76482037536718,83.9885562956399));
#140368=CARTESIAN_POINT('Ctrl Pts',(-5.0099826870134,4.9087896358898,83.9796451024534));
#140369=CARTESIAN_POINT('Ctrl Pts',(-4.87054078900142,5.04717740252974,
83.9707339092669));
#140370=CARTESIAN_POINT('Ctrl Pts',(-4.72551276558456,5.17949376530153,
83.9618227160803));
#140371=CARTESIAN_POINT('Ctrl Pts',(-4.5804847421677,5.31181012807331,83.9529115228938));
#140372=CARTESIAN_POINT('Ctrl Pts',(-4.42987080819885,5.43805487271669,
83.9440003297073));
#140373=CARTESIAN_POINT('Ctrl Pts',(-4.2741923740152,5.55777888300806,83.9350891365208));
#140374=CARTESIAN_POINT('Ctrl Pts',(-4.13398410882107,5.66560560848266,
83.9270634716685));
#140375=CARTESIAN_POINT('Ctrl Pts',(-3.98960312497932,5.7681923137558,83.9190378068161));
#140376=CARTESIAN_POINT('Ctrl Pts',(-3.84148776816131,5.86520232298657,
83.9110121419638));
#140377=CARTESIAN_POINT('Ctrl Pts',(-3.69341941952446,5.96218154361994,
83.9029890242606));
#140378=CARTESIAN_POINT('Ctrl Pts',(-3.54161936381682,6.05358739132223,
83.8949659065575));
#140379=CARTESIAN_POINT('Ctrl Pts',(-3.38655599560282,6.13912575625769,
83.8869427888543));
#140380=CARTESIAN_POINT('Ctrl Pts',(-3.23151218223668,6.2246533340567,83.8789206829365));
#140381=CARTESIAN_POINT('Ctrl Pts',(-3.07320619725684,6.30431472647453,
83.8708985770187));
#140382=CARTESIAN_POINT('Ctrl Pts',(-2.91213211646133,6.37786116960651,
83.8628764711009));
#140383=CARTESIAN_POINT('Ctrl Pts',(-2.75099817999322,6.45143494284522,
83.8548513841414));
#140384=CARTESIAN_POINT('Ctrl Pts',(-2.5870944253451,6.51888907226207,83.846826297182));
#140385=CARTESIAN_POINT('Ctrl Pts',(-2.42093645749568,6.58002228197354,
83.8388012102225));
#140386=CARTESIAN_POINT('Ctrl Pts',(-2.25474576566647,6.64116753156456,
83.8307745427623));
#140387=CARTESIAN_POINT('Ctrl Pts',(-2.08630032326142,6.6959892631529,83.8227478753022));
#140388=CARTESIAN_POINT('Ctrl Pts',(-1.9161318709138,6.74433578759009,83.814721207842));
#140389=CARTESIAN_POINT('Ctrl Pts',(-1.74582680793195,6.79272112444683,
83.8066880966015));
#140390=CARTESIAN_POINT('Ctrl Pts',(-1.57379632744456,6.83462078067688,
83.798654985361));
#140391=CARTESIAN_POINT('Ctrl Pts',(-1.4005839705798,6.86993385003487,83.7906218741204));
#140392=CARTESIAN_POINT('Ctrl Pts',(-1.2985209576248,6.89074159331949,83.7858884731585));
#140393=CARTESIAN_POINT('Ctrl Pts',(-1.19604776993002,6.90926345064798,
83.7811550721965));
#140394=CARTESIAN_POINT('Ctrl Pts',(-1.09327653932811,6.92548720098844,
83.7764216712345));
#140395=CARTESIAN_POINT('Ctrl Pts',(-0.881564605848198,6.95890863160438,
83.7666707179402));
#140396=CARTESIAN_POINT('Ctrl Pts',(-0.668462914409056,6.98259511557202,
83.7569197646459));
#140397=CARTESIAN_POINT('Ctrl Pts',(-0.454786202916001,6.99648455098253,
83.7471688113516));
#140398=CARTESIAN_POINT('Ctrl Pts',(-0.240801650035402,7.01039399673034,
83.7374038099798));
#140399=CARTESIAN_POINT('Ctrl Pts',(-0.0262404585607778,7.01447815828874,
83.7276388086081));
#140400=CARTESIAN_POINT('Ctrl Pts',(0.188078825298634,7.00872691135661,
83.7178738072363));
#140401=CARTESIAN_POINT('Ctrl Pts',(0.402040883318102,7.00298525056147,
83.7081250820986));
#140402=CARTESIAN_POINT('Ctrl Pts',(0.615761801679578,6.98744094641748,
83.6983763569608));
#140403=CARTESIAN_POINT('Ctrl Pts',(0.828427412456071,6.96213577753202,
83.6886276318231));
#140404=CARTESIAN_POINT('Ctrl Pts',(1.0405093385911,6.93690006152318,83.6789056631558));
#140405=CARTESIAN_POINT('Ctrl Pts',(1.25154169969661,6.901956966926,83.6691836944886));
#140406=CARTESIAN_POINT('Ctrl Pts',(1.46071789642997,6.85739963758488,83.6594617258213));
#140407=CARTESIAN_POINT('Ctrl Pts',(1.66851002890356,6.81313713245423,83.6498040848815));
#140408=CARTESIAN_POINT('Ctrl Pts',(1.87447042766209,6.75938718329072,83.6401464439417));
#140409=CARTESIAN_POINT('Ctrl Pts',(2.07780996502803,6.69629243027291,83.6304888030018));
#140410=CARTESIAN_POINT('Ctrl Pts',(2.16718469223887,6.66856011410631,83.6262439373172));
#140411=CARTESIAN_POINT('Ctrl Pts',(2.25605311895002,6.63902314186761,83.6219990716325));
#140412=CARTESIAN_POINT('Ctrl Pts',(2.34434837785268,6.6076968185412,83.6177542059479));
#140413=CARTESIAN_POINT('Ctrl Pts',(2.50767059260701,6.54975164040406,83.609902358934));
#140414=CARTESIAN_POINT('Ctrl Pts',(2.66896336522398,6.48570442701392,83.6020505119202));
#140415=CARTESIAN_POINT('Ctrl Pts',(2.82772286466146,6.41573144412785,83.5941986649063));
#140416=CARTESIAN_POINT('Ctrl Pts',(2.98643734118826,6.34577830501409,83.5863490446128));
#140417=CARTESIAN_POINT('Ctrl Pts',(3.14261962486846,6.26990289290422,83.5784994243193));
#140418=CARTESIAN_POINT('Ctrl Pts',(3.29578514339501,6.18832989190757,83.5706498040258));
#140419=CARTESIAN_POINT('Ctrl Pts',(3.44893843361477,6.10676340347126,83.562800810424));
#140420=CARTESIAN_POINT('Ctrl Pts',(3.59907510180847,6.01950041166515,83.5549518168222));
#140421=CARTESIAN_POINT('Ctrl Pts',(3.74573473808128,5.92681177653139,83.5471028232205));
#140422=CARTESIAN_POINT('Ctrl Pts',(3.89246862383267,5.83407621585626,83.5392498559031));
#140423=CARTESIAN_POINT('Ctrl Pts',(4.03572163757369,5.73590972758238,83.5313968885857));
#140424=CARTESIAN_POINT('Ctrl Pts',(4.17506168012789,5.63262696524701,83.5235439212684));
#140425=CARTESIAN_POINT('Ctrl Pts',(4.31443711037073,5.52931797256055,83.5156889595612));
#140426=CARTESIAN_POINT('Ctrl Pts',(4.44989729177311,5.42089035558698,83.507833997854));
#140427=CARTESIAN_POINT('Ctrl Pts',(4.58104338155856,5.30769894575592,83.4999790361469));
#140428=CARTESIAN_POINT('Ctrl Pts',(4.71231964480065,5.19439518398892,83.4921162777336));
#140429=CARTESIAN_POINT('Ctrl Pts',(4.83927298478556,5.07631844510113,83.4842535193203));
#140430=CARTESIAN_POINT('Ctrl Pts',(4.96154118033183,4.95386068419081,83.4763907609071));
#140431=CARTESIAN_POINT('Ctrl Pts',(5.05123537414633,4.86402742794533,83.4706227541586));
#140432=CARTESIAN_POINT('Ctrl Pts',(5.13840904119081,4.771837304849,83.4648547474101));
#140433=CARTESIAN_POINT('Ctrl Pts',(5.22293326955456,4.67745599918162,83.4590867406616));
#140434=CARTESIAN_POINT('Ctrl Pts',(5.34492379289599,4.54123914047855,83.4507620014063));
#140435=CARTESIAN_POINT('Ctrl Pts',(5.46167577438176,4.40014251146621,83.442437262151));
#140436=CARTESIAN_POINT('Ctrl Pts',(5.57279233896684,4.25459893635728,83.4341125228956));
#140437=CARTESIAN_POINT('Ctrl Pts',(5.68381015413366,4.10918470599032,83.4257951818456));
#140438=CARTESIAN_POINT('Ctrl Pts',(5.78920233765805,3.95933167666587,83.4174778407957));
#140439=CARTESIAN_POINT('Ctrl Pts',(5.88861173929042,3.80550631932087,83.4091604997457));
#140440=CARTESIAN_POINT('Ctrl Pts',(5.9879684936774,3.65176242792578,83.4008475635617));
#140441=CARTESIAN_POINT('Ctrl Pts',(6.08134859910948,3.49405068185793,83.3925346273777));
#140442=CARTESIAN_POINT('Ctrl Pts',(6.16843733730753,3.33286774088178,83.3842216911937));
#140443=CARTESIAN_POINT('Ctrl Pts',(6.25549188772779,3.17174807429315,83.3759120183573));
#140444=CARTESIAN_POINT('Ctrl Pts',(6.33625983486509,3.00716022353939,83.3676023455208));
#140445=CARTESIAN_POINT('Ctrl Pts',(6.41047150296468,2.83962703047032,83.3592926726843));
#140446=CARTESIAN_POINT('Ctrl Pts',(6.46799035248137,2.70977795460457,83.3528521380129));
#140447=CARTESIAN_POINT('Ctrl Pts',(6.52157155441489,2.57816011610822,83.3464116033416));
#140448=CARTESIAN_POINT('Ctrl Pts',(6.57110895151814,2.44502632087636,83.3399710686702));
#140449=CARTESIAN_POINT('Origin',(0.,0.,50.));
#140450=CARTESIAN_POINT('',(6.57110895151812,2.4450263208764,81.339842993376));
#140451=CARTESIAN_POINT('',(6.57110895151811,2.44502632087644,81.8868302382415));
#140452=CARTESIAN_POINT('',(6.57110895151814,2.44502632087636,50.));
#140453=CARTESIAN_POINT('',(7.01124961619472,0.00231989425607759,83.7735343569347));
#140454=CARTESIAN_POINT('Ctrl Pts',(6.57110895151811,2.44502632087644,81.8868302382415));
#140455=CARTESIAN_POINT('Ctrl Pts',(6.50690213833289,2.61758477608302,81.8952030318929));
#140456=CARTESIAN_POINT('Ctrl Pts',(6.43585859289123,2.78770811981673,81.9035758255444));
#140457=CARTESIAN_POINT('Ctrl Pts',(6.35818746868627,2.95483987307958,81.9119486191959));
#140458=CARTESIAN_POINT('Ctrl Pts',(6.28055906938963,3.12187969141926,81.9203168071867));
#140459=CARTESIAN_POINT('Ctrl Pts',(6.19631049858508,3.28593090300688,81.9286849951776));
#140460=CARTESIAN_POINT('Ctrl Pts',(6.10569894647632,3.4464571573571,81.9370531831684));
#140461=CARTESIAN_POINT('Ctrl Pts',(6.01512396242723,3.60691862820553,81.9454179940137));
#140462=CARTESIAN_POINT('Ctrl Pts',(5.9181912791183,3.7638576927618,81.953782804859));
#140463=CARTESIAN_POINT('Ctrl Pts',(5.81520414381981,3.9167623527859,81.9621476157043));
#140464=CARTESIAN_POINT('Ctrl Pts',(5.71224349526661,4.06962768802664,81.9705102752459));
#140465=CARTESIAN_POINT('Ctrl Pts',(5.60323168374978,4.2184604157847,81.9788729347874));
#140466=CARTESIAN_POINT('Ctrl Pts',(5.48851565883485,4.36277691673831,81.9872355943289));
#140467=CARTESIAN_POINT('Ctrl Pts',(5.37379223353033,4.50710272762341,81.9955987933499));
#140468=CARTESIAN_POINT('Ctrl Pts',(5.25336405922103,4.64691146843435,82.0039619923709));
#140469=CARTESIAN_POINT('Ctrl Pts',(5.12761928507243,4.7817514604853,82.0123251913918));
#140470=CARTESIAN_POINT('Ctrl Pts',(5.00186741468376,4.91659906205292,82.0206888623789));
#140471=CARTESIAN_POINT('Ctrl Pts',(4.87079857025712,5.04647711507872,82.029052533366));
#140472=CARTESIAN_POINT('Ctrl Pts',(4.73483890286805,5.17096965049954,82.037416204353));
#140473=CARTESIAN_POINT('Ctrl Pts',(4.59885343658502,5.29548580887988,82.0457814623803));
#140474=CARTESIAN_POINT('Ctrl Pts',(4.45797553927358,5.41461418987642,82.0541467204076));
#140475=CARTESIAN_POINT('Ctrl Pts',(4.31266599652032,5.52797780069325,82.0625119784349));
#140476=CARTESIAN_POINT('Ctrl Pts',(4.16730950067788,5.6413780420825,82.0708799394829));
#140477=CARTESIAN_POINT('Ctrl Pts',(4.01751876314148,5.74900959678093,82.0792479005309));
#140478=CARTESIAN_POINT('Ctrl Pts',(3.86378555145235,5.85053739197418,82.0876158615789));
#140479=CARTESIAN_POINT('Ctrl Pts',(3.70991018257048,5.95215906998034,82.0959915604855));
#140480=CARTESIAN_POINT('Ctrl Pts',(3.55208532887637,6.0476655279089,82.1043672593921));
#140481=CARTESIAN_POINT('Ctrl Pts',(3.39083056755593,6.13676581145381,82.1127429582987));
#140482=CARTESIAN_POINT('Ctrl Pts',(3.22949847165443,6.22590882572521,82.1211226740241));
#140483=CARTESIAN_POINT('Ctrl Pts',(3.06473347863258,6.30863938566825,82.1295023897495));
#140484=CARTESIAN_POINT('Ctrl Pts',(2.89707797346671,6.3847134452655,82.137882105475));
#140485=CARTESIAN_POINT('Ctrl Pts',(2.72922743845101,6.46087600009232,82.1462715691338));
#140486=CARTESIAN_POINT('Ctrl Pts',(2.55847997405498,6.53036645043005,82.1546610327927));
#140487=CARTESIAN_POINT('Ctrl Pts',(2.38539736604835,6.59298915277051,82.1630504964515));
#140488=CARTESIAN_POINT('Ctrl Pts',(2.26024876159711,6.63826894081584,82.1691165575139));
#140489=CARTESIAN_POINT('Ctrl Pts',(2.13387969783636,6.67995921662382,82.1751826185762));
#140490=CARTESIAN_POINT('Ctrl Pts',(2.00650681878623,6.71800245226692,82.1812486796386));
#140491=CARTESIAN_POINT('Ctrl Pts',(1.83051941084736,6.77056568613873,82.1896299800435));
#140492=CARTESIAN_POINT('Ctrl Pts',(1.65226018973621,6.81627070874339,82.1980112804485));
#140493=CARTESIAN_POINT('Ctrl Pts',(1.47228955156789,6.85492451007624,82.2063925808534));
#140494=CARTESIAN_POINT('Ctrl Pts',(1.29254699983778,6.89352932337439,82.214763259187));
#140495=CARTESIAN_POINT('Ctrl Pts',(1.11109767133269,6.92510065645381,82.2231339375206));
#140496=CARTESIAN_POINT('Ctrl Pts',(0.928517585887898,6.94949506476528,
82.2315046158542));
#140497=CARTESIAN_POINT('Ctrl Pts',(0.746144697492237,6.97386178961168,
82.2398657949051));
#140498=CARTESIAN_POINT('Ctrl Pts',(0.562643932535991,6.99106777960089,
82.248226973956));
#140499=CARTESIAN_POINT('Ctrl Pts',(0.378602425090457,7.00102040892723,
82.2565881530069));
#140500=CARTESIAN_POINT('Ctrl Pts',(0.194799733210726,7.01096012354299,
82.2649384824416));
#140501=CARTESIAN_POINT('Ctrl Pts',(0.0104580240394714,7.01366523329996,
82.2732888118764));
#140502=CARTESIAN_POINT('Ctrl Pts',(-0.173829587198575,7.00909479441635,
82.2816391413112));
#140503=CARTESIAN_POINT('Ctrl Pts',(-0.357975400143808,7.00452787221206,
82.2899830456669));
#140504=CARTESIAN_POINT('Ctrl Pts',(-0.54206687194791,6.99269656544896,
82.2983269500227));
#140505=CARTESIAN_POINT('Ctrl Pts',(-0.725508864328621,6.97361193717292,
82.3066708543785));
#140506=CARTESIAN_POINT('Ctrl Pts',(-0.908803514956873,6.95454263778934,
82.3150080568583));
#140507=CARTESIAN_POINT('Ctrl Pts',(-1.09144940160192,6.9282316696525,82.323345259338));
#140508=CARTESIAN_POINT('Ctrl Pts',(-1.27285433479264,6.89474208400137,
82.3316824618178));
#140509=CARTESIAN_POINT('Ctrl Pts',(-1.33257183746027,6.88371749726449,
82.3344270228535));
#140510=CARTESIAN_POINT('Ctrl Pts',(-1.39215489262231,6.87191538931436,
82.3371715838893));
#140511=CARTESIAN_POINT('Ctrl Pts',(-1.45158250318337,6.85933923923813,
82.339916144925));
#140512=CARTESIAN_POINT('Ctrl Pts',(-1.63213081342337,6.82113136542071,
82.3482544552268));
#140513=CARTESIAN_POINT('Ctrl Pts',(-1.81109548286814,6.7758064957697,82.3565927655286));
#140514=CARTESIAN_POINT('Ctrl Pts',(-1.98790383542348,6.72353068734044,
82.3649310758304));
#140515=CARTESIAN_POINT('Ctrl Pts',(-2.16482342979489,6.67122198874631,
82.3732746323142));
#140516=CARTESIAN_POINT('Ctrl Pts',(-2.33958368700241,6.61195372119245,
82.3816181887979));
#140517=CARTESIAN_POINT('Ctrl Pts',(-2.51162909084586,6.54594117545497,
82.3899617452816));
#140518=CARTESIAN_POINT('Ctrl Pts',(-2.68380538608278,6.47987840766038,
82.3983116495068));
#140519=CARTESIAN_POINT('Ctrl Pts',(-2.85326240249981,6.40706124421809,
82.4066615537319));
#140520=CARTESIAN_POINT('Ctrl Pts',(-3.01946611920712,6.3277524380668,82.415011457957));
#140521=CARTESIAN_POINT('Ctrl Pts',(-3.18591912918995,6.24832467457535,
82.4233738864206));
#140522=CARTESIAN_POINT('Ctrl Pts',(-3.34910879230402,6.16238595204779,
82.4317363148842));
#140523=CARTESIAN_POINT('Ctrl Pts',(-3.50852581951479,6.07024489920284,
82.4400987433477));
#140524=CARTESIAN_POINT('Ctrl Pts',(-3.66807917001557,5.97802505319702,
82.4484683228276));
#140525=CARTESIAN_POINT('Ctrl Pts',(-3.82385317134599,5.87959246895441,
82.4568379023075));
#140526=CARTESIAN_POINT('Ctrl Pts',(-3.97536843561313,5.77529846532894,
82.4652074817873));
#140527=CARTESIAN_POINT('Ctrl Pts',(-4.12711739371517,5.6708436009098,82.4735899703238));
#140528=CARTESIAN_POINT('Ctrl Pts',(-4.27459422692132,5.56050944734027,
82.4819724588603));
#140529=CARTESIAN_POINT('Ctrl Pts',(-4.41735237277946,5.44468773918208,
82.4903549473968));
#140530=CARTESIAN_POINT('Ctrl Pts',(-4.46406517734358,5.40678897841467,
82.4930978350016));
#140531=CARTESIAN_POINT('Ctrl Pts',(-4.51027304345832,5.36830295604337,
82.4958407226065));
#140532=CARTESIAN_POINT('Ctrl Pts',(-4.5559612031742,5.32924423137761,82.4985836102113));
#140533=CARTESIAN_POINT('Ctrl Pts',(-4.69571065576719,5.20977267846402,
82.5069734653442));
#140534=CARTESIAN_POINT('Ctrl Pts',(-4.83087709247407,5.0846989550127,82.515363320477));
#140535=CARTESIAN_POINT('Ctrl Pts',(-4.96100246275921,4.95440017832604,
82.5237531756098));
#140536=CARTESIAN_POINT('Ctrl Pts',(-5.09100775517699,4.82422163952374,
82.532135288702));
#140537=CARTESIAN_POINT('Ctrl Pts',(-5.21598102341299,4.68882789082791,
82.5405174017941));
#140538=CARTESIAN_POINT('Ctrl Pts',(-5.33549858863921,4.54863511101177,
82.5488995148863));
#140539=CARTESIAN_POINT('Ctrl Pts',(-5.45492343356569,4.40855109107991,
82.5572751252352));
#140540=CARTESIAN_POINT('Ctrl Pts',(-5.56890080123639,4.26367571187785,
82.5656507355841));
#140541=CARTESIAN_POINT('Ctrl Pts',(-5.67704476442226,4.11446099814372,
82.574026345933));
#140542=CARTESIAN_POINT('Ctrl Pts',(-5.78512070344939,3.96534014268033,
82.5823966878986));
#140543=CARTESIAN_POINT('Ctrl Pts',(-5.88737036183101,3.81188566056055,
82.5907670298642));
#140544=CARTESIAN_POINT('Ctrl Pts',(-5.98344863787123,3.65458191322304,
82.5991373718298));
#140545=CARTESIAN_POINT('Ctrl Pts',(-6.07948056324542,3.49735405331563,
82.6075036757242));
#140546=CARTESIAN_POINT('Ctrl Pts',(-6.16934687232832,3.33628091135612,
82.6158699796185));
#140547=CARTESIAN_POINT('Ctrl Pts',(-6.25274603156845,3.17187541167762,
82.6242362835129));
#140548=CARTESIAN_POINT('Ctrl Pts',(-6.33612186640129,3.00751589160932,
82.6326002475865));
#140549=CARTESIAN_POINT('Ctrl Pts',(-6.41303400803496,2.83982616433852,
82.6409642116602));
#140550=CARTESIAN_POINT('Ctrl Pts',(-6.48322683788517,2.66934380157849,
82.6493281757338));
#140551=CARTESIAN_POINT('Ctrl Pts',(-6.55340886622532,2.49888767322102,
82.6576908527324));
#140552=CARTESIAN_POINT('Ctrl Pts',(-6.6168735192609,2.32564007000848,82.666053529731));
#140553=CARTESIAN_POINT('Ctrl Pts',(-6.67341313985606,2.15015897721458,
82.6744162067296));
#140554=CARTESIAN_POINT('Ctrl Pts',(-6.72995159640377,1.97468149725567,
82.6827787115559));
#140555=CARTESIAN_POINT('Ctrl Pts',(-6.77956520439842,1.79697093234247,
82.6911412163822));
#140556=CARTESIAN_POINT('Ctrl Pts',(-6.82209591188067,1.61760128944096,
82.6995037212086));
#140557=CARTESIAN_POINT('Ctrl Pts',(-6.86463141277395,1.43821143073598,
82.7078671685286));
#140558=CARTESIAN_POINT('Ctrl Pts',(-6.90008234632228,1.25716244114014,
82.7162306158486));
#140559=CARTESIAN_POINT('Ctrl Pts',(-6.92834149970032,1.07503982532291,
82.7245940631686));
#140560=CARTESIAN_POINT('Ctrl Pts',(-6.95661729286205,0.892809970591258,
82.7329624351215));
#140561=CARTESIAN_POINT('Ctrl Pts',(-6.97769279247474,0.709505551352474,
82.7413308070743));
#140562=CARTESIAN_POINT('Ctrl Pts',(-6.99151239034198,0.525719562309206,
82.7496991790271));
#140563=CARTESIAN_POINT('Ctrl Pts',(-7.00533612892193,0.341878506180315,
82.7580700583629));
#140564=CARTESIAN_POINT('Ctrl Pts',(-7.01189961136644,0.157555920727849,
82.7664409376987));
#140565=CARTESIAN_POINT('Ctrl Pts',(-7.01119933913218,-0.0266531321334792,
82.7748118170345));
#140566=CARTESIAN_POINT('Ctrl Pts',(-7.01049847356482,-0.211018263333262,
82.7831897889258));
#140567=CARTESIAN_POINT('Ctrl Pts',(-7.00252156215909,-0.395269340835481,
82.7915677608171));
#140568=CARTESIAN_POINT('Ctrl Pts',(-6.98731721408861,-0.578813192835963,
82.7999457327085));
#140569=CARTESIAN_POINT('Ctrl Pts',(-6.97765472708107,-0.695456805376881,
82.8052700020671));
#140570=CARTESIAN_POINT('Ctrl Pts',(-6.96507433820147,-0.811814874622516,
82.8105942714257));
#140571=CARTESIAN_POINT('Ctrl Pts',(-6.94959934240903,-0.927736785132497,
82.8159185407843));
#140572=CARTESIAN_POINT('Ctrl Pts',(-6.92674601336525,-1.09892917831956,
82.8237813719736));
#140573=CARTESIAN_POINT('Ctrl Pts',(-6.89752954876146,-1.26952587813197,
82.8316442031629));
#140574=CARTESIAN_POINT('Ctrl Pts',(-6.86199066830925,-1.43899639698532,
82.8395070343521));
#140575=CARTESIAN_POINT('Ctrl Pts',(-6.82647909479559,-1.60833670011481,
82.8473638239935));
#140576=CARTESIAN_POINT('Ctrl Pts',(-6.78465484389672,-1.77655217235846,
82.8552206136349));
#140577=CARTESIAN_POINT('Ctrl Pts',(-6.73661038061163,-1.94311789203219,
82.8630774032762));
#140578=CARTESIAN_POINT('Ctrl Pts',(-6.6885930121295,-2.10958967652492,
82.8709297620602));
#140579=CARTESIAN_POINT('Ctrl Pts',(-6.63436251462618,-2.27441319399653,
82.8787821208441));
#140580=CARTESIAN_POINT('Ctrl Pts',(-6.57406228090888,-2.43707441191916,
82.886634479628));
#140581=CARTESIAN_POINT('Ctrl Pts',(-6.51377628478036,-2.59969722363028,
82.8944849843785));
#140582=CARTESIAN_POINT('Ctrl Pts',(-6.44742352927182,-2.76015839181148,
82.9023354891289));
#140583=CARTESIAN_POINT('Ctrl Pts',(-6.37519703030342,-2.91795979878244,
82.9101859938793));
#140584=CARTESIAN_POINT('Ctrl Pts',(-6.30298215030234,-3.07573582048045,
82.9180352357309));
#140585=CARTESIAN_POINT('Ctrl Pts',(-6.2248955693807,-3.23085258706953,
82.9258844775825));
#140586=CARTESIAN_POINT('Ctrl Pts',(-6.14117794585039,-3.3828331321395,
82.9337337194341));
#140587=CARTESIAN_POINT('Ctrl Pts',(-6.05743211621404,-3.53486488242996,
82.941585605849));
#140588=CARTESIAN_POINT('Ctrl Pts',(-5.96805163865431,-3.6837579661236,
82.9494374922638));
#140589=CARTESIAN_POINT('Ctrl Pts',(-5.87332261961814,-3.82906097736532,
82.9572893786786));
#140590=CARTESIAN_POINT('Ctrl Pts',(-5.80376428000776,-3.9357551699707,
82.9630549211426));
#140591=CARTESIAN_POINT('Ctrl Pts',(-5.73132307943708,-4.04051419631888,
82.9688204636066));
#140592=CARTESIAN_POINT('Ctrl Pts',(-5.65612682125141,-4.14316979430248,
82.9745860060706));
#140593=CARTESIAN_POINT('Ctrl Pts',(-5.53019890309834,-4.31508268003297,
82.9842413104306));
#140594=CARTESIAN_POINT('Ctrl Pts',(-5.39660821342806,-4.48100845535787,
82.9938966147905));
#140595=CARTESIAN_POINT('Ctrl Pts',(-5.25591274746692,-4.64036720028865,
83.0035519191505));
#140596=CARTESIAN_POINT('Ctrl Pts',(-5.11443785501876,-4.80060876277072,
83.0132607120853));
#140597=CARTESIAN_POINT('Ctrl Pts',(-4.96577932222475,-4.95421033393521,
83.0229695050201));
#140598=CARTESIAN_POINT('Ctrl Pts',(-4.81053572744779,-5.10062472423216,
83.0326782979549));
#140599=CARTESIAN_POINT('Ctrl Pts',(-4.65454508731076,-5.24774367300752,
83.0424338104257));
#140600=CARTESIAN_POINT('Ctrl Pts',(-4.49190590488925,-5.38760609160965,
83.0521893228965));
#140601=CARTESIAN_POINT('Ctrl Pts',(-4.32325600338168,-5.51969963781765,
83.0619448353673));
#140602=CARTESIAN_POINT('Ctrl Pts',(-4.1544391125254,-5.65192397695854,
83.0717100072962));
#140603=CARTESIAN_POINT('Ctrl Pts',(-3.97959963522644,-5.77636404234841,
83.0814751792252));
#140604=CARTESIAN_POINT('Ctrl Pts',(-3.79940714173115,-5.89254884866153,
83.0912403511542));
#140605=CARTESIAN_POINT('Ctrl Pts',(-3.61946033661267,-6.00857523962716,
83.1009922084928));
#140606=CARTESIAN_POINT('Ctrl Pts',(-3.43417513472253,-6.11636884740361,
83.1107440658314));
#140607=CARTESIAN_POINT('Ctrl Pts',(-3.24424756247317,-6.21550354483745,
83.12049592317));
#140608=CARTESIAN_POINT('Ctrl Pts',(-3.16142538577055,-6.25873345259116,
83.1247484392324));
#140609=CARTESIAN_POINT('Ctrl Pts',(-3.07772079202042,-6.300317342639,83.1290009552948));
#140610=CARTESIAN_POINT('Ctrl Pts',(-2.99319322076635,-6.34022246499746,
83.1332534713572));
#140611=CARTESIAN_POINT('Ctrl Pts',(-2.83351978878438,-6.41560364235889,
83.1412865169559));
#140612=CARTESIAN_POINT('Ctrl Pts',(-2.67083014928581,-6.48502775193599,
83.1493195625547));
#140613=CARTESIAN_POINT('Ctrl Pts',(-2.50561624273084,-6.54824509366162,
83.1573526081534));
#140614=CARTESIAN_POINT('Ctrl Pts',(-2.34050854203638,-6.61142179684586,
83.1653804898012));
#140615=CARTESIAN_POINT('Ctrl Pts',(-2.1728801452354,-6.66839954381496,
83.1734083714489));
#140616=CARTESIAN_POINT('Ctrl Pts',(-2.00324500790806,-6.71897581486877,
83.1814362530967));
#140617=CARTESIAN_POINT('Ctrl Pts',(-1.83368646251739,-6.76952925023765,
83.1894605100768));
#140618=CARTESIAN_POINT('Ctrl Pts',(-1.66212333123537,-6.81368686015066,
83.1974847670568));
#140619=CARTESIAN_POINT('Ctrl Pts',(-1.4890868020357,-6.85129528326601,
83.2055090240369));
#140620=CARTESIAN_POINT('Ctrl Pts',(-1.31607119471488,-6.88889915913995,
83.2135323108026));
#140621=CARTESIAN_POINT('Ctrl Pts',(-1.14158290067859,-6.91995534013052,
83.2215555975682));
#140622=CARTESIAN_POINT('Ctrl Pts',(-0.966165607669418,-6.94436106355774,
83.2295788843339));
#140623=CARTESIAN_POINT('Ctrl Pts',(-0.790762688542486,-6.96876478715365,
83.2376015136628));
#140624=CARTESIAN_POINT('Ctrl Pts',(-0.614431285773459,-6.98651909212087,
83.2456241429916));
#140625=CARTESIAN_POINT('Ctrl Pts',(-0.437722255315089,-6.99757284990316,
83.2536467723205));
#140626=CARTESIAN_POINT('Ctrl Pts',(-0.260946794841701,-7.00863076311143,
83.2616724175869));
#140627=CARTESIAN_POINT('Ctrl Pts',(-0.0837937893760947,-7.01298307725059,
83.2696980628532));
#140628=CARTESIAN_POINT('Ctrl Pts',(0.0931834548161807,-7.01063074239747,
83.2777237081196));
#140629=CARTESIAN_POINT('Ctrl Pts',(0.197540022458685,-7.00924366242379,
83.2824561176276));
#140630=CARTESIAN_POINT('Ctrl Pts',(0.301835470608092,-7.00552636419648,
83.2871885271356));
#140631=CARTESIAN_POINT('Ctrl Pts',(0.40595684536479,-6.99948752425501,
83.2919209366435));
#140632=CARTESIAN_POINT('Ctrl Pts',(0.59803335202259,-6.98834745543693,
83.3006509854783));
#140633=CARTESIAN_POINT('Ctrl Pts',(0.789613284956578,-6.96929894113836,
83.3093810343131));
#140634=CARTESIAN_POINT('Ctrl Pts',(0.980053679312014,-6.94241466264923,
83.3181110831478));
#140635=CARTESIAN_POINT('Ctrl Pts',(1.17054913974443,-6.91552261053752,
83.326843656287));
#140636=CARTESIAN_POINT('Ctrl Pts',(1.35990413264777,-6.8807903100262,83.3355762294263));
#140637=CARTESIAN_POINT('Ctrl Pts',(1.54748375458744,-6.83834194756214,
83.3443088025655));
#140638=CARTESIAN_POINT('Ctrl Pts',(1.73772824448788,-6.79529053834947,
83.3531654358459));
#140639=CARTESIAN_POINT('Ctrl Pts',(1.92614625231635,-6.74430222228833,
83.3620220691263));
#140640=CARTESIAN_POINT('Ctrl Pts',(2.11208871267477,-6.68555964989408,
83.3708787024066));
#140641=CARTESIAN_POINT('Ctrl Pts',(2.29554327508537,-6.62760304927318,
83.3796168345135));
#140642=CARTESIAN_POINT('Ctrl Pts',(2.47658786607273,-6.56209851230751,
83.3883549666203));
#140643=CARTESIAN_POINT('Ctrl Pts',(2.65461586620692,-6.48927123530697,
83.3970930987271));
#140644=CARTESIAN_POINT('Ctrl Pts',(2.83626532571248,-6.41496250019543,
83.4060089825943));
#140645=CARTESIAN_POINT('Ctrl Pts',(3.01477387673478,-6.33303002305587,
83.4149248664614));
#140646=CARTESIAN_POINT('Ctrl Pts',(3.18951910498884,-6.24376444474095,
83.4238407503286));
#140647=CARTESIAN_POINT('Ctrl Pts',(3.36426433324302,-6.15449886642596,
83.4327566341957));
#140648=CARTESIAN_POINT('Ctrl Pts',(3.53524597218751,-6.05790032992442,
83.4416725180629));
#140649=CARTESIAN_POINT('Ctrl Pts',(3.70186786591578,-5.9543094365174,83.45058840193));
#140650=CARTESIAN_POINT('Ctrl Pts',(3.86521559732683,-5.85275413034331,
83.4593290864261));
#140651=CARTESIAN_POINT('Ctrl Pts',(4.02439068243599,-5.74446793341555,
83.4680697709222));
#140652=CARTESIAN_POINT('Ctrl Pts',(4.1788565091602,-5.62981214947262,83.4768104554184));
#140653=CARTESIAN_POINT('Ctrl Pts',(4.33329454491655,-5.51517699400961,
83.4855495673201));
#140654=CARTESIAN_POINT('Ctrl Pts',(4.48302479458871,-5.39417470329896,
83.4942886792219));
#140655=CARTESIAN_POINT('Ctrl Pts',(4.62754150307087,-5.26720857759179,
83.5030277911237));
#140656=CARTESIAN_POINT('Ctrl Pts',(4.77393063350921,-5.13859742298823,
83.5118801307981));
#140657=CARTESIAN_POINT('Ctrl Pts',(4.91496995417719,-5.00386698718462,
83.5207324704725));
#140658=CARTESIAN_POINT('Ctrl Pts',(5.05016918408609,-4.86347795045966,
83.5295848101469));
#140659=CARTESIAN_POINT('Ctrl Pts',(5.18357070856565,-4.72495562653854,
83.5383194427966));
#140660=CARTESIAN_POINT('Ctrl Pts',(5.31128630094435,-4.58092446077574,
83.5470540754463));
#140661=CARTESIAN_POINT('Ctrl Pts',(5.43288204853427,-4.43186407837764,
83.5557887080959));
#140662=CARTESIAN_POINT('Ctrl Pts',(5.55693571408816,-4.27979061206111,
83.5646999012827));
#140663=CARTESIAN_POINT('Ctrl Pts',(5.67461928824213,-4.12248265532379,
83.5736110944694));
#140664=CARTESIAN_POINT('Ctrl Pts',(5.78551457111115,-3.9604857921675,83.5825222876561));
#140665=CARTESIAN_POINT('Ctrl Pts',(5.89640985398017,-3.7984889290112,83.5914334808429));
#140666=CARTESIAN_POINT('Ctrl Pts',(6.00051666321512,-3.63180340196017,
83.6003446740296));
#140667=CARTESIAN_POINT('Ctrl Pts',(6.09746263884109,-3.4610079356218,83.6092558672163));
#140668=CARTESIAN_POINT('Ctrl Pts',(6.18477484191618,-3.30718485689209,
83.6172815320687));
#140669=CARTESIAN_POINT('Ctrl Pts',(6.26631835344879,-3.14995713566829,
83.6253071969211));
#140670=CARTESIAN_POINT('Ctrl Pts',(6.34182062979834,-2.98980562277286,
83.6333328617735));
#140671=CARTESIAN_POINT('Ctrl Pts',(6.41729894357731,-2.8297049380394,83.6413559794767));
#140672=CARTESIAN_POINT('Ctrl Pts',(6.48673968328614,-2.66668264025154,
83.6493790971799));
#140673=CARTESIAN_POINT('Ctrl Pts',(6.5499166315901,-2.50124342712168,83.6574022148831));
#140674=CARTESIAN_POINT('Ctrl Pts',(6.613085612728,-2.33582507732441,83.665424320801));
#140675=CARTESIAN_POINT('Ctrl Pts',(6.66999224570556,-2.16799076186445,
83.6734464267189));
#140676=CARTESIAN_POINT('Ctrl Pts',(6.72045878597691,-1.99826431396994,
83.6814685326367));
#140677=CARTESIAN_POINT('Ctrl Pts',(6.77094407978509,-1.82847479515412,
83.6894936195962));
#140678=CARTESIAN_POINT('Ctrl Pts',(6.81498439266014,-1.65679209012733,
83.6975187065557));
#140679=CARTESIAN_POINT('Ctrl Pts',(6.852451997612,-1.48375475834902,83.7055437935152));
#140680=CARTESIAN_POINT('Ctrl Pts',(6.88992698162119,-1.31068334773399,
83.7135704609755));
#140681=CARTESIAN_POINT('Ctrl Pts',(6.92082660996158,-1.1362571390085,83.7215971284357));
#140682=CARTESIAN_POINT('Ctrl Pts',(6.94507450261422,-0.961023785157178,
83.7296237958959));
#140683=CARTESIAN_POINT('Ctrl Pts',(6.96934186138961,-0.785649754587056,
83.7376569071365));
#140684=CARTESIAN_POINT('Ctrl Pts',(6.98694677815085,-0.609467649039707,
83.7456900183771));
#140685=CARTESIAN_POINT('Ctrl Pts',(6.99786480243257,-0.433029755762056,
83.7537231296177));
#140686=CARTESIAN_POINT('Ctrl Pts',(7.00429809895839,-0.329066139584161,
83.7584565305794));
#140687=CARTESIAN_POINT('Ctrl Pts',(7.00841069794281,-0.225013749300497,
83.7631899315412));
#140688=CARTESIAN_POINT('Ctrl Pts',(7.01020606780221,-0.120985327412369,
83.7679233325029));
#140689=CARTESIAN_POINT('Ctrl Pts',(7.0109154847157,-0.0798798573698832,
83.7697936739721));
#140690=CARTESIAN_POINT('Ctrl Pts',(7.01126321422435,-0.0387764624473275,
83.7716640154413));
#140691=CARTESIAN_POINT('Ctrl Pts',(7.0112496161949,0.00231989372472653,
83.7735343569105));
#140692=CARTESIAN_POINT('Ctrl Pts',(7.01124961619472,0.00231989425587762,
83.7735343569347));
#140693=CARTESIAN_POINT('Ctrl Pts',(7.0111790285611,0.215651824307297,83.7832433334144));
#140694=CARTESIAN_POINT('Ctrl Pts',(7.00136754561913,0.428863000641898,
83.7929523098941));
#140695=CARTESIAN_POINT('Ctrl Pts',(6.98187348596674,0.64114677606196,83.8026612863738));
#140696=CARTESIAN_POINT('Ctrl Pts',(6.96237311657637,0.853499262413789,
83.8123734054056));
#140697=CARTESIAN_POINT('Ctrl Pts',(6.93318392099452,1.06492369523564,83.8220855244373));
#140698=CARTESIAN_POINT('Ctrl Pts',(6.89441601631981,1.27461929861933,83.8317976434691));
#140699=CARTESIAN_POINT('Ctrl Pts',(6.85574551333199,1.48378805626106,83.8414853614716));
#140700=CARTESIAN_POINT('Ctrl Pts',(6.80754438516368,1.69123660806533,83.8511730794741));
#140701=CARTESIAN_POINT('Ctrl Pts',(6.74997311842575,1.89617759269267,83.8608607974766));
#140702=CARTESIAN_POINT('Ctrl Pts',(6.69795058159319,2.08136632529099,83.8696148113305));
#140703=CARTESIAN_POINT('Ctrl Pts',(6.63827767335995,2.26450761414988,83.8783688251844));
#140704=CARTESIAN_POINT('Ctrl Pts',(6.57110895151815,2.44502632087633,83.8871228390383));
#140705=CARTESIAN_POINT('',(7.01124847424792,-0.00462545740594696,83.2264656430532));
#140706=CARTESIAN_POINT('Ctrl Pts',(6.57110895151814,2.44502632087636,83.3399710686702));
#140707=CARTESIAN_POINT('Ctrl Pts',(6.63500113977313,2.27331343312962,83.3316642161154));
#140708=CARTESIAN_POINT('Ctrl Pts',(6.69216465663035,2.09907831971231,83.3233573635606));
#140709=CARTESIAN_POINT('Ctrl Pts',(6.74241499103036,1.92287978075309,83.3150505110058));
#140710=CARTESIAN_POINT('Ctrl Pts',(6.79267769512076,1.74663786852284,83.3067416136249));
#140711=CARTESIAN_POINT('Ctrl Pts',(6.83602372137104,1.56843188663344,83.2984327162441));
#140712=CARTESIAN_POINT('Ctrl Pts',(6.87231865653561,1.38883506779339,83.2901238188632));
#140713=CARTESIAN_POINT('Ctrl Pts',(6.90861788899793,1.20921698480165,83.281813937714));
#140714=CARTESIAN_POINT('Ctrl Pts',(6.93786430419882,1.02820806611816,83.2735040565649));
#140715=CARTESIAN_POINT('Ctrl Pts',(6.95997478920127,0.846390864898014,
83.2651941754157));
#140716=CARTESIAN_POINT('Ctrl Pts',(6.98209784835813,0.664470264880261,
83.2568795684666));
#140717=CARTESIAN_POINT('Ctrl Pts',(6.99707683296611,0.481740797382236,
83.2485649615175));
#140718=CARTESIAN_POINT('Ctrl Pts',(7.00488051387247,0.298790141855086,
83.2402503545684));
#140719=CARTESIAN_POINT('Ctrl Pts',(7.00919306448075,0.197686064145291,
83.2356554507421));
#140720=CARTESIAN_POINT('Ctrl Pts',(7.011315198226,0.0965144795200406,83.2310605469158));
#140721=CARTESIAN_POINT('Ctrl Pts',(7.01124847424845,-0.00462545660722081,
83.2264656430895));
#140722=CARTESIAN_POINT('Ctrl Pts',(7.01124847424792,-0.00462545740615106,
83.2264656430532));
#140723=CARTESIAN_POINT('Ctrl Pts',(7.01109761289103,-0.233300454381342,
83.2160766744734));
#140724=CARTESIAN_POINT('Ctrl Pts',(6.99975542124624,-0.461583810264566,
83.2056877058936));
#140725=CARTESIAN_POINT('Ctrl Pts',(6.97735941040463,-0.688536288468472,
83.1952987373138));
#140726=CARTESIAN_POINT('Ctrl Pts',(6.95466206942481,-0.918542329295982,
83.1847699889598));
#140727=CARTESIAN_POINT('Ctrl Pts',(6.92061145572012,-1.14718165366891,
83.1742412406059));
#140728=CARTESIAN_POINT('Ctrl Pts',(6.87540077451661,-1.37349581443717,
83.1637124922519));
#140729=CARTESIAN_POINT('Ctrl Pts',(6.84396755419073,-1.53084320865742,
83.1563922648641));
#140730=CARTESIAN_POINT('Ctrl Pts',(6.80714072867915,-1.68706705158743,
83.1490720374764));
#140731=CARTESIAN_POINT('Ctrl Pts',(6.76499934449835,-1.84184973095988,
83.1417518100886));
#140732=CARTESIAN_POINT('Ctrl Pts',(6.71674953181093,-2.01906828778123,
83.1333705096839));
#140733=CARTESIAN_POINT('Ctrl Pts',(6.66147559423329,-2.19459632208125,
83.1249892092792));
#140734=CARTESIAN_POINT('Ctrl Pts',(6.59930940225604,-2.36785598713161,
83.1166079088745));
#140735=CARTESIAN_POINT('Ctrl Pts',(6.53722199682675,-2.54089607091964,
83.1082372305411));
#140736=CARTESIAN_POINT('Ctrl Pts',(6.46825985455144,-2.71167320878719,
83.0998665522077));
#140737=CARTESIAN_POINT('Ctrl Pts',(6.3926051907949,-2.87962244697497,83.0914958738744));
#140738=CARTESIAN_POINT('Ctrl Pts',(6.31703638209181,-3.04738109161432,
83.0831346948237));
#140739=CARTESIAN_POINT('Ctrl Pts',(6.23479032305727,-3.21231793589975,
83.074773515773));
#140740=CARTESIAN_POINT('Ctrl Pts',(6.14609825809439,-3.37388541067255,
83.0664123367223));
#140741=CARTESIAN_POINT('Ctrl Pts',(6.05752128154834,-3.53524323258756,
83.0580620072877));
#140742=CARTESIAN_POINT('Ctrl Pts',(5.96251513978702,-3.6932401198509,83.0497116778531));
#140743=CARTESIAN_POINT('Ctrl Pts',(5.86135813000353,-3.8473507033206,83.0413613484186));
#140744=CARTESIAN_POINT('Ctrl Pts',(5.76027895448811,-4.00134270791484,
83.033017444063));
#140745=CARTESIAN_POINT('Ctrl Pts',(5.65305852144119,-4.15145409504481,
83.0246735397075));
#140746=CARTESIAN_POINT('Ctrl Pts',(5.54002036745714,-4.29718522880502,
83.0163296353519));
#140747=CARTESIAN_POINT('Ctrl Pts',(5.4270730064231,-4.44279931041004,83.0079924328723));
#140748=CARTESIAN_POINT('Ctrl Pts',(5.30831744397997,-4.58403989713977,
82.9996552303928));
#140749=CARTESIAN_POINT('Ctrl Pts',(5.18411981592423,-4.72043729930202,
82.9913180279132));
#140750=CARTESIAN_POINT('Ctrl Pts',(5.14323464230844,-4.76533857121394,
82.9885734668762));
#140751=CARTESIAN_POINT('Ctrl Pts',(5.10176005521895,-4.80971524125113,
82.9858289058393));
#140752=CARTESIAN_POINT('Ctrl Pts',(5.05971009278301,-4.85355131213112,
82.9830843448023));
#140753=CARTESIAN_POINT('Ctrl Pts',(4.93195719158826,-4.98673062805631,
82.9747460345002));
#140754=CARTESIAN_POINT('Ctrl Pts',(4.79899544814047,-5.11480822757893,
82.9664077241982));
#140755=CARTESIAN_POINT('Ctrl Pts',(4.66126818529817,-5.23738536554521,
82.9580694138962));
#140756=CARTESIAN_POINT('Ctrl Pts',(4.52345426913576,-5.36003962488714,
82.9497258574123));
#140757=CARTESIAN_POINT('Ctrl Pts',(4.38086909784444,-5.4771863020379,82.9413823009283));
#140758=CARTESIAN_POINT('Ctrl Pts',(4.2339887527602,-5.58846721418316,82.9330387444444));
#140759=CARTESIAN_POINT('Ctrl Pts',(4.08699666174867,-5.69983278836207,
82.924688840219));
#140760=CARTESIAN_POINT('Ctrl Pts',(3.93570313971617,-5.80532349836861,
82.9163389359937));
#140761=CARTESIAN_POINT('Ctrl Pts',(3.78061323339439,-5.90462447086885,
82.9079890317683));
#140762=CARTESIAN_POINT('Ctrl Pts',(3.62529070369067,-6.004074387479,82.8996266033045));
#140763=CARTESIAN_POINT('Ctrl Pts',(3.46616068687968,-6.09731583710534,
82.8912641748407));
#140764=CARTESIAN_POINT('Ctrl Pts',(3.30375413931725,-6.18407916746254,
82.882901746377));
#140765=CARTESIAN_POINT('Ctrl Pts',(3.14120871201725,-6.27091669229485,
82.8745321668969));
#140766=CARTESIAN_POINT('Ctrl Pts',(2.97538145765003,-6.35126490224367,
82.8661625874168));
#140767=CARTESIAN_POINT('Ctrl Pts',(2.80682380791828,-6.4249020750361,82.8577930079367));
#140768=CARTESIAN_POINT('Ctrl Pts',(2.63800617854858,-6.49865282419573,
82.8494105194));
#140769=CARTESIAN_POINT('Ctrl Pts',(2.4664500429742,-6.56567173290775,82.8410280308633));
#140770=CARTESIAN_POINT('Ctrl Pts',(2.29272383290536,-6.62578629209604,
82.8326455423266));
#140771=CARTESIAN_POINT('Ctrl Pts',(2.23587777031499,-6.64545676089206,
82.829902654723));
#140772=CARTESIAN_POINT('Ctrl Pts',(2.1787994510767,-6.66438838201942,82.8271597671194));
#140773=CARTESIAN_POINT('Ctrl Pts',(2.12150903618854,-6.68257629749712,
82.8244168795158));
#140774=CARTESIAN_POINT('Ctrl Pts',(1.94627098386147,-6.7382089000961,82.816027024383));
#140775=CARTESIAN_POINT('Ctrl Pts',(1.7686938955959,-6.78699188517118,82.8076371692502));
#140776=CARTESIAN_POINT('Ctrl Pts',(1.58933985197956,-6.82873527070786,
82.7992473141174));
#140777=CARTESIAN_POINT('Ctrl Pts',(1.41015131376029,-6.87044013603358,
82.7908652010253));
#140778=CARTESIAN_POINT('Ctrl Pts',(1.22918940765217,-6.9051182775189,82.7824830879332));
#140779=CARTESIAN_POINT('Ctrl Pts',(1.04703124785321,-6.93262952482815,
82.7741009748411));
#140780=CARTESIAN_POINT('Ctrl Pts',(0.865014404179149,-6.9601194292403,
82.7657253644923));
#140781=CARTESIAN_POINT('Ctrl Pts',(0.681803480916146,-6.98045347548987,
82.7573497541434));
#140782=CARTESIAN_POINT('Ctrl Pts',(0.497986110754797,-6.99354247831493,
82.7489741437946));
#140783=CARTESIAN_POINT('Ctrl Pts',(0.314284364449178,-7.00662324796282,
82.740603801829));
#140784=CARTESIAN_POINT('Ctrl Pts',(0.129977258901961,-7.01246803762564,
82.7322334598635));
#140785=CARTESIAN_POINT('Ctrl Pts',(-0.0543416578249555,-7.01103940558922,
82.7238631178979));
#140786=CARTESIAN_POINT('Ctrl Pts',(-0.238571654299908,-7.00961146276215,
82.7154968140035));
#140787=CARTESIAN_POINT('Ctrl Pts',(-0.422813122463965,-7.00091709807069,
82.7071305101092));
#140788=CARTESIAN_POINT('Ctrl Pts',(-0.606471251804374,-6.9849709507796,
82.6987642062149));
#140789=CARTESIAN_POINT('Ctrl Pts',(-0.790078017113542,-6.96902926317897,
82.6904002421413));
#140790=CARTESIAN_POINT('Ctrl Pts',(-0.973101441646077,-6.94583986398626,
82.6820362780676));
#140791=CARTESIAN_POINT('Ctrl Pts',(-1.15495001680282,-6.91546939991691,
82.673672313994));
#140792=CARTESIAN_POINT('Ctrl Pts',(-1.3367706084858,-6.88510360935729,
82.6653096369955));
#140793=CARTESIAN_POINT('Ctrl Pts',(-1.51741638717774,-6.84755901128638,
82.6569469599969));
#140794=CARTESIAN_POINT('Ctrl Pts',(-1.69630382237394,-6.80295376323399,
82.6485842829984));
#140795=CARTESIAN_POINT('Ctrl Pts',(-1.8751875746048,-6.75834943352214,
82.6402217781721));
#140796=CARTESIAN_POINT('Ctrl Pts',(-2.05231273673736,-6.70668482359197,
82.6318592733458));
#140797=CARTESIAN_POINT('Ctrl Pts',(-2.22710835418838,-6.64812867965147,
82.6234967685195));
#140798=CARTESIAN_POINT('Ctrl Pts',(-2.4019236719289,-6.58956593615769,
82.6151333211995));
#140799=CARTESIAN_POINT('Ctrl Pts',(-2.5744086100923,-6.52411021501969,
82.6067698738795));
#140800=CARTESIAN_POINT('Ctrl Pts',(-2.74400928376417,-6.45197951121329,
82.5984064265595));
#140801=CARTESIAN_POINT('Ctrl Pts',(-2.91370982307877,-6.37980633482149,
82.5900380546067));
#140802=CARTESIAN_POINT('Ctrl Pts',(-3.08052240108897,-6.3009504497292,
82.5816696826539));
#140803=CARTESIAN_POINT('Ctrl Pts',(-3.24391401049085,-6.21567763442098,
82.5733013107011));
#140804=CARTESIAN_POINT('Ctrl Pts',(-3.4073545762892,-6.13037926914866,
82.5649304313653));
#140805=CARTESIAN_POINT('Ctrl Pts',(-3.56737184065762,-6.03866029666515,
82.5565595520296));
#140806=CARTESIAN_POINT('Ctrl Pts',(-3.72345854630218,-5.94083184549683,
82.5481886726938));
#140807=CARTESIAN_POINT('Ctrl Pts',(-3.87967750252453,-5.84292050533974,
82.5398107008025));
#140808=CARTESIAN_POINT('Ctrl Pts',(-4.03195896960849,-5.73888952217245,
82.5314327289113));
#140809=CARTESIAN_POINT('Ctrl Pts',(-4.17982480036541,-5.62909328406896,
82.52305475702));
#140810=CARTESIAN_POINT('Ctrl Pts',(-4.27379473988789,-5.55931688067971,
82.5177304876609));
#140811=CARTESIAN_POINT('Ctrl Pts',(-4.36598195812697,-5.4872129053503,
82.5124062183019));
#140812=CARTESIAN_POINT('Ctrl Pts',(-4.45627082729111,-5.41288064493706,
82.5070819489429));
#140813=CARTESIAN_POINT('Ctrl Pts',(-4.58960858476191,-5.30310745802053,
82.4992191177537));
#140814=CARTESIAN_POINT('Ctrl Pts',(-4.71908165106739,-5.18824423112896,
82.4913562865645));
#140815=CARTESIAN_POINT('Ctrl Pts',(-4.84426095490327,-5.06860556398894,
82.4834934553753));
#140816=CARTESIAN_POINT('Ctrl Pts',(-4.96934407496756,-4.94905882337256,
82.4756366657339));
#140817=CARTESIAN_POINT('Ctrl Pts',(-5.09013971962647,-4.82474420115755,
82.4677798760926));
#140818=CARTESIAN_POINT('Ctrl Pts',(-5.20625085837433,-4.69601730854738,
82.4599230864513));
#140819=CARTESIAN_POINT('Ctrl Pts',(-5.32229651593641,-4.56736301181096,
82.4520707276674));
#140820=CARTESIAN_POINT('Ctrl Pts',(-5.43366266823845,-4.4343016767349,
82.4442183688835));
#140821=CARTESIAN_POINT('Ctrl Pts',(-5.53998841533241,-4.29722642183102,
82.4363660100996));
#140822=CARTESIAN_POINT('Ctrl Pts',(-5.64628905767686,-4.16018353199426,
82.4285155053493));
#140823=CARTESIAN_POINT('Ctrl Pts',(-5.7475514233018,-4.01912890440158,
82.4206650005989));
#140824=CARTESIAN_POINT('Ctrl Pts',(-5.84345432266771,-3.87448940395971,
82.4128144958486));
#140825=CARTESIAN_POINT('Ctrl Pts',(-5.93934179427969,-3.72987317145484,
82.404965253997));
#140826=CARTESIAN_POINT('Ctrl Pts',(-6.02987130762786,-3.58167353377094,
82.3971160121454));
#140827=CARTESIAN_POINT('Ctrl Pts',(-6.11476478557853,-3.43034665588608,
82.3892667702939));
#140828=CARTESIAN_POINT('Ctrl Pts',(-6.19968686580361,-3.27896879301399,
82.3814148838791));
#140829=CARTESIAN_POINT('Ctrl Pts',(-6.27896893088145,-3.12446191841869,
82.3735629974643));
#140830=CARTESIAN_POINT('Ctrl Pts',(-6.35237860284588,-2.96730730606147,
82.3657111110495));
#140831=CARTESIAN_POINT('Ctrl Pts',(-6.40628241126132,-2.85191063026364,
82.3599455685852));
#140832=CARTESIAN_POINT('Ctrl Pts',(-6.45702090176905,-2.73508688813753,
82.3541800261209));
#140833=CARTESIAN_POINT('Ctrl Pts',(-6.50451862268203,-2.61703344450977,
82.3484144836566));
#140834=CARTESIAN_POINT('Ctrl Pts',(-6.58406099959887,-2.41933445329764,
82.3387591792965));
#140835=CARTESIAN_POINT('Ctrl Pts',(-6.65447352736375,-2.21828741596851,
82.3291038749364));
#140836=CARTESIAN_POINT('Ctrl Pts',(-6.7155581905773,-2.01467236826988,
82.3194485705763));
#140837=CARTESIAN_POINT('Ctrl Pts',(-6.77698125136581,-1.80992933140435,
82.3097397776413));
#140838=CARTESIAN_POINT('Ctrl Pts',(-6.82897285094932,-1.60258981367787,
82.3000309847063));
#140839=CARTESIAN_POINT('Ctrl Pts',(-6.87138419481227,-1.39345104319605,
82.2903221917714));
#140840=CARTESIAN_POINT('Ctrl Pts',(-6.91399962566314,-1.18330587919221,
82.2805666793004));
#140841=CARTESIAN_POINT('Ctrl Pts',(-6.94694239186077,-0.971344151625883,
82.2708111668294));
#140842=CARTESIAN_POINT('Ctrl Pts',(-6.97011401132134,-0.75837802689812,
82.2610556543585));
#140843=CARTESIAN_POINT('Ctrl Pts',(-6.99330857425006,-0.545201032942771,
82.2512904824293));
#140844=CARTESIAN_POINT('Ctrl Pts',(-7.00671264531918,-0.331017691907905,
82.2415253105001));
#140845=CARTESIAN_POINT('Ctrl Pts',(-7.01027962605566,-0.116645304273289,
82.231760138571));
#140846=CARTESIAN_POINT('Ctrl Pts',(-7.01384174329482,0.0974347914741832,
82.2220082812322));
#140847=CARTESIAN_POINT('Ctrl Pts',(-7.00759357667754,0.311703380708535,
82.2122564238934));
#140848=CARTESIAN_POINT('Ctrl Pts',(-6.9915405923592,0.525344370764156,
82.2025045665546));
#140849=CARTESIAN_POINT('Ctrl Pts',(-6.98454032858611,0.618507315016503,
82.1982520504931));
#140850=CARTESIAN_POINT('Ctrl Pts',(-6.97567625541477,0.711550891526119,
82.1939995344316));
#140851=CARTESIAN_POINT('Ctrl Pts',(-6.96495193175312,0.804407328950017,
82.1897470183701));
#140852=CARTESIAN_POINT('Ctrl Pts',(-6.9446935765245,0.97981407290384,82.1817139727713));
#140853=CARTESIAN_POINT('Ctrl Pts',(-6.91778355046248,1.15463820249654,
82.1736809271726));
#140854=CARTESIAN_POINT('Ctrl Pts',(-6.88426944093054,1.32833008968777,
82.1656478815738));
#140855=CARTESIAN_POINT('Ctrl Pts',(-6.85077687555863,1.5019103210461,82.1576199999261));
#140856=CARTESIAN_POINT('Ctrl Pts',(-6.81068874636665,1.67435940037502,
82.1495921182784));
#140857=CARTESIAN_POINT('Ctrl Pts',(-6.7641043335017,1.84513390516882,82.1415642366307));
#140858=CARTESIAN_POINT('Ctrl Pts',(-6.71754095395832,2.01583130359044,
82.1335399796506));
#140859=CARTESIAN_POINT('Ctrl Pts',(-6.66448722722162,2.18485528001888,
82.1255157226706));
#140860=CARTESIAN_POINT('Ctrl Pts',(-6.60509328167742,2.35167372372101,
82.1174914656906));
#140861=CARTESIAN_POINT('Ctrl Pts',(-6.54570651746624,2.51847199737403,
82.109468178925));
#140862=CARTESIAN_POINT('Ctrl Pts',(-6.4799811769958,2.68306492174575,82.1014448921593));
#140863=CARTESIAN_POINT('Ctrl Pts',(-6.40811696211129,2.84493647774456,
82.0934216053937));
#140864=CARTESIAN_POINT('Ctrl Pts',(-6.33625863585807,3.00679476981344,
82.0853989760649));
#140865=CARTESIAN_POINT('Ctrl Pts',(-6.25826258961516,3.16593180421338,
82.077376346736));
#140866=CARTESIAN_POINT('Ctrl Pts',(-6.17437616391519,3.32185272836952,
82.0693537174072));
#140867=CARTESIAN_POINT('Ctrl Pts',(-6.09045820289127,3.47783226769267,
82.0613280721408));
#140868=CARTESIAN_POINT('Ctrl Pts',(-6.00064561528805,3.63059295992614,
82.0533024268745));
#140869=CARTESIAN_POINT('Ctrl Pts',(-5.90523126755091,3.7796653607481,82.0452767816082));
#140870=CARTESIAN_POINT('Ctrl Pts',(-5.84896915385632,3.86756753230491,
82.0405443721));
#140871=CARTESIAN_POINT('Ctrl Pts',(-5.79076015133523,3.9541878003552,82.0358119625919));
#140872=CARTESIAN_POINT('Ctrl Pts',(-5.73067125139156,4.03943480835801,
82.0310795530837));
#140873=CARTESIAN_POINT('Ctrl Pts',(-5.61982306083956,4.19669308061698,
82.022349504249));
#140874=CARTESIAN_POINT('Ctrl Pts',(-5.50252001517792,4.34935516522828,
82.0136194554144));
#140875=CARTESIAN_POINT('Ctrl Pts',(-5.37916323089427,4.49691333004041,
82.0048894065797));
#140876=CARTESIAN_POINT('Ctrl Pts',(-5.25577077784271,4.6445141614798,81.9961568334405));
#140877=CARTESIAN_POINT('Ctrl Pts',(-5.1263212678867,4.78700791716026,81.9874242603013));
#140878=CARTESIAN_POINT('Ctrl Pts',(-4.99125530779243,4.92392089852527,
81.9786916871622));
#140879=CARTESIAN_POINT('Ctrl Pts',(-4.85427052012951,5.06277894734448,
81.9698350538818));
#140880=CARTESIAN_POINT('Ctrl Pts',(-4.71150868835908,5.195896239379,81.9609784206014));
#140881=CARTESIAN_POINT('Ctrl Pts',(-4.56346755050045,5.32281790765281,
81.9521217873209));
#140882=CARTESIAN_POINT('Ctrl Pts',(-4.41740719337723,5.44804137231201,
81.9433836552142));
#140883=CARTESIAN_POINT('Ctrl Pts',(-4.26620815229866,5.56723381446002,
81.9346455231074));
#140884=CARTESIAN_POINT('Ctrl Pts',(-4.11038189632247,5.67999887578198,
81.9259073910006));
#140885=CARTESIAN_POINT('Ctrl Pts',(-3.95138581057193,5.79505781271974,
81.9169915071334));
#140886=CARTESIAN_POINT('Ctrl Pts',(-3.78757247686647,5.90342489858673,
81.9080756232662));
#140887=CARTESIAN_POINT('Ctrl Pts',(-3.61951728623384,6.00472490436943,
81.899159739399));
#140888=CARTESIAN_POINT('Ctrl Pts',(-3.45146209560133,6.10602491015205,
81.8902438555318));
#140889=CARTESIAN_POINT('Ctrl Pts',(-3.27916531018032,6.20025768494158,
81.8813279716645));
#140890=CARTESIAN_POINT('Ctrl Pts',(-3.10323089411647,6.28709667337008,
81.8724120877973));
#140891=CARTESIAN_POINT('Ctrl Pts',(-2.93075363378354,6.37222925373341,
81.863671403301));
#140892=CARTESIAN_POINT('Ctrl Pts',(-2.7547620577083,6.45026497194727,81.8549307188046));
#140893=CARTESIAN_POINT('Ctrl Pts',(-2.57584628362454,6.52093877333913,
81.8461900343083));
#140894=CARTESIAN_POINT('Ctrl Pts',(-2.39696269946052,6.59159985934016,
81.8374509224062));
#140895=CARTESIAN_POINT('Ctrl Pts',(-2.21515622252979,6.65490157315621,
81.8287118105042));
#140896=CARTESIAN_POINT('Ctrl Pts',(-2.03103635225847,6.71062723583307,
81.8199726986022));
#140897=CARTESIAN_POINT('Ctrl Pts',(-1.84453094407761,6.76707490467175,
81.8111203589279));
#140898=CARTESIAN_POINT('Ctrl Pts',(-1.65565204426987,6.8157487324728,81.8022680192536));
#140899=CARTESIAN_POINT('Ctrl Pts',(-1.46504971956045,6.85647547080246,
81.7934156795793));
#140900=CARTESIAN_POINT('Ctrl Pts',(-1.27698177935366,6.89666067736108,
81.7846810469294));
#140901=CARTESIAN_POINT('Ctrl Pts',(-1.08723623904894,6.92910877721177,
81.7759464142796));
#140902=CARTESIAN_POINT('Ctrl Pts',(-0.89644950239847,6.95370439781197,
81.7672117816297));
#140903=CARTESIAN_POINT('Ctrl Pts',(-0.701806231655992,6.97879719054806,
81.7583005884432));
#140904=CARTESIAN_POINT('Ctrl Pts',(-0.506079508305626,6.99571660669627,
81.7493893952567));
#140905=CARTESIAN_POINT('Ctrl Pts',(-0.309953463710748,7.00439543521307,
81.7404782020702));
#140906=CARTESIAN_POINT('Ctrl Pts',(-0.113827419115738,7.01307426372988,
81.7315670088837));
#140907=CARTESIAN_POINT('Ctrl Pts',(0.0826976444860204,7.01351247775365,
81.7226558156972));
#140908=CARTESIAN_POINT('Ctrl Pts',(0.278933644379903,7.00569929304227,
81.7137446225107));
#140909=CARTESIAN_POINT('Ctrl Pts',(0.455669164993112,6.99866252472066,
81.7057189576585));
#140910=CARTESIAN_POINT('Ctrl Pts',(0.632251418387597,6.98492904811944,
81.6976932928062));
#140911=CARTESIAN_POINT('Ctrl Pts',(0.808128137561514,6.96452119501272,
81.6896676279539));
#140912=CARTESIAN_POINT('Ctrl Pts',(0.983949037778691,6.94411981885801,
81.6816445102508));
#140913=CARTESIAN_POINT('Ctrl Pts',(1.15906448588315,6.91704832570235,81.6736213925477));
#140914=CARTESIAN_POINT('Ctrl Pts',(1.33292641379869,6.88338098160328,81.6655982748446));
#140915=CARTESIAN_POINT('Ctrl Pts',(1.50676641620335,6.84971788325099,81.6575761689269));
#140916=CARTESIAN_POINT('Ctrl Pts',(1.67935285362559,6.80946066104508,81.6495540630091));
#140917=CARTESIAN_POINT('Ctrl Pts',(1.85014699148782,6.76273485155145,81.6415319570914));
#140918=CARTESIAN_POINT('Ctrl Pts',(2.02100459702882,6.71599167858911,81.633506870132));
#140919=CARTESIAN_POINT('Ctrl Pts',(2.1900682178033,6.66277521033667,81.6254817831726));
#140920=CARTESIAN_POINT('Ctrl Pts',(2.35681301311548,6.60326123848735,81.6174566962132));
#140921=CARTESIAN_POINT('Ctrl Pts',(2.52359064798068,6.5437355456591,81.6094300287531));
#140922=CARTESIAN_POINT('Ctrl Pts',(2.68804820532863,6.4779100099437,81.601403361293));
#140923=CARTESIAN_POINT('Ctrl Pts',(2.84968022415902,6.40600883409764,81.5933766938328));
#140924=CARTESIAN_POINT('Ctrl Pts',(3.01144200060452,6.334049936241,81.5853435825924));
#140925=CARTESIAN_POINT('Ctrl Pts',(3.17037337702122,6.25600581411277,81.5773104713519));
#140926=CARTESIAN_POINT('Ctrl Pts',(3.32599236705278,6.17214722254797,81.5692773601114));
#140927=CARTESIAN_POINT('Ctrl Pts',(3.41768872916274,6.1227346940603,81.5645439591491));
#140928=CARTESIAN_POINT('Ctrl Pts',(3.50823552402975,6.07130424261146,81.5598105581867));
#140929=CARTESIAN_POINT('Ctrl Pts',(3.59753882558452,6.01791832454645,81.5550771572244));
#140930=CARTESIAN_POINT('Ctrl Pts',(3.78150640606667,5.90794167186676,81.54532620393));
#140931=CARTESIAN_POINT('Ctrl Pts',(3.96030414582843,5.78960001109624,81.5355752506356));
#140932=CARTESIAN_POINT('Ctrl Pts',(4.13326669073003,5.66336764000022,81.5258242973412));
#140933=CARTESIAN_POINT('Ctrl Pts',(4.30647842062453,5.53695340749303,81.5160592959694));
#140934=CARTESIAN_POINT('Ctrl Pts',(4.47383810859282,5.40262574799317,81.5062942945975));
#140935=CARTESIAN_POINT('Ctrl Pts',(4.6347107770697,5.26090130827542,81.4965292932257));
#140936=CARTESIAN_POINT('Ctrl Pts',(4.79531530414036,5.11941309383397,81.4867805680879));
#140937=CARTESIAN_POINT('Ctrl Pts',(4.94945439310547,4.97055276469821,81.4770318429501));
#140938=CARTESIAN_POINT('Ctrl Pts',(5.09652968089175,4.81487401437353,81.4672831178123));
#140939=CARTESIAN_POINT('Ctrl Pts',(5.24320130404137,4.65962254185419,81.4575611491449));
#140940=CARTESIAN_POINT('Ctrl Pts',(5.38284780235387,4.49759003646098,81.4478391804775));
#140941=CARTESIAN_POINT('Ctrl Pts',(5.5149095323348,4.32936478165825,81.4381172118101));
#140942=CARTESIAN_POINT('Ctrl Pts',(5.64609744434046,4.1622526294293,81.4284595708702));
#140943=CARTESIAN_POINT('Ctrl Pts',(5.76980057758359,3.98902942740854,81.4188019299304));
#140944=CARTESIAN_POINT('Ctrl Pts',(5.88550441451674,3.81031026941429,81.4091442889905));
#140945=CARTESIAN_POINT('Ctrl Pts',(5.93636023427466,3.73175704657265,81.4048994233063));
#140946=CARTESIAN_POINT('Ctrl Pts',(5.98567111524841,3.65214255661752,81.4006545576221));
#140947=CARTESIAN_POINT('Ctrl Pts',(6.03339552127373,3.5715213910005,81.3964096919379));
#140948=CARTESIAN_POINT('Ctrl Pts',(6.12167101984821,3.42239698729973,81.3885579937008));
#140949=CARTESIAN_POINT('Ctrl Pts',(6.20447908329652,3.26988769268964,81.3807062954638));
#140950=CARTESIAN_POINT('Ctrl Pts',(6.28154580695363,3.11445161106145,81.3728545972267));
#140951=CARTESIAN_POINT('Ctrl Pts',(6.35859173350429,2.95905747517305,81.3650050178368));
#140952=CARTESIAN_POINT('Ctrl Pts',(6.42989923199527,2.80073846428882,81.3571554384468));
#140953=CARTESIAN_POINT('Ctrl Pts',(6.49524019261651,2.63997753829821,81.3493058590569));
#140954=CARTESIAN_POINT('Ctrl Pts',(6.52149691725951,2.57537708971348,81.3461515704966));
#140955=CARTESIAN_POINT('Ctrl Pts',(6.546790714195,2.5103825853856,81.3429972819363));
#140956=CARTESIAN_POINT('Ctrl Pts',(6.57110895151812,2.4450263208764,81.339842993376));
#140957=CARTESIAN_POINT('Origin',(0.,0.,50.));
#140958=CARTESIAN_POINT('',(6.57110895151812,2.44502632087641,79.3399816340719));
#140959=CARTESIAN_POINT('',(6.57110895151811,2.44502632087644,79.8868028110482));
#140960=CARTESIAN_POINT('',(6.57110895151814,2.44502632087636,50.));
#140961=CARTESIAN_POINT('',(7.01124984869581,0.00145659295747845,81.7735343568707));
#140962=CARTESIAN_POINT('Ctrl Pts',(6.57110895151811,2.44502632087645,79.8868028110482));
#140963=CARTESIAN_POINT('Ctrl Pts',(6.50601242163503,2.61997592635723,79.8952869682238));
#140964=CARTESIAN_POINT('Ctrl Pts',(6.43396319980227,2.79222176291496,79.9037711253993));
#140965=CARTESIAN_POINT('Ctrl Pts',(6.35522177652277,2.96121305105033,79.9122552825748));
#140966=CARTESIAN_POINT('Ctrl Pts',(6.27637096155742,3.13043911068377,79.9207512263834));
#140967=CARTESIAN_POINT('Ctrl Pts',(6.19080949862361,3.2964013010892,79.9292471701919));
#140968=CARTESIAN_POINT('Ctrl Pts',(6.09884419442367,3.45857283494864,79.9377431140004));
#140969=CARTESIAN_POINT('Ctrl Pts',(6.01888259155763,3.59957705278337,79.9451301312097));
#140970=CARTESIAN_POINT('Ctrl Pts',(5.93408053615291,3.73771588754854,79.9525171484191));
#140971=CARTESIAN_POINT('Ctrl Pts',(5.84466588621368,3.87266151903701,79.9599041656285));
#140972=CARTESIAN_POINT('Ctrl Pts',(5.74321613721439,4.02577066225192,79.9682854660334));
#140973=CARTESIAN_POINT('Ctrl Pts',(5.63562818842432,4.17506946424814,79.9766667664383));
#140974=CARTESIAN_POINT('Ctrl Pts',(5.52220866352461,4.32005069866012,79.9850480668433));
#140975=CARTESIAN_POINT('Ctrl Pts',(5.40893288126937,4.46484819058109,79.9934187451769));
#140976=CARTESIAN_POINT('Ctrl Pts',(5.28984045198937,4.60533876384297,80.0017894235105));
#140977=CARTESIAN_POINT('Ctrl Pts',(5.165281750719,4.74104323943468,80.0101601018441));
#140978=CARTESIAN_POINT('Ctrl Pts',(5.04086440218849,4.87659371374634,80.0185212808949));
#140979=CARTESIAN_POINT('Ctrl Pts',(4.91099336569956,5.00736867584645,80.0268824599458));
#140980=CARTESIAN_POINT('Ctrl Pts',(4.77606010814264,5.13292084547468,80.0352436389967));
#140981=CARTESIAN_POINT('Ctrl Pts',(4.64130194240444,5.2583100963524,80.0435939684315));
#140982=CARTESIAN_POINT('Ctrl Pts',(4.50149489656413,5.37848985043892,80.0519442978662));
#140983=CARTESIAN_POINT('Ctrl Pts',(4.35706814119611,5.49304867769019,80.060294627301));
#140984=CARTESIAN_POINT('Ctrl Pts',(4.21275251357704,5.60751935877656,80.0686385316568));
#140985=CARTESIAN_POINT('Ctrl Pts',(4.06382451569309,5.71637752914874,80.0769824360125));
#140986=CARTESIAN_POINT('Ctrl Pts',(3.91074819081436,5.81925039421249,80.0853263403683));
#140987=CARTESIAN_POINT('Ctrl Pts',(3.75779481779455,5.92204063114938,80.093663542848));
#140988=CARTESIAN_POINT('Ctrl Pts',(3.60070003406205,6.01885496829242,80.1020007453278));
#140989=CARTESIAN_POINT('Ctrl Pts',(3.43995892617383,6.10936241753074,80.1103379478075));
#140990=CARTESIAN_POINT('Ctrl Pts',(3.3870438407315,6.13915697022813,80.1130825088433));
#140991=CARTESIAN_POINT('Ctrl Pts',(3.33373384920756,6.1682683944196,80.1158270698792));
#140992=CARTESIAN_POINT('Ctrl Pts',(3.28004730242159,6.1966859091273,80.118571630915));
#140993=CARTESIAN_POINT('Ctrl Pts',(3.11694104233132,6.2830217757926,80.126909941217));
#140994=CARTESIAN_POINT('Ctrl Pts',(2.95049105754623,6.36287851805465,80.1352482515189));
#140995=CARTESIAN_POINT('Ctrl Pts',(2.78124344501291,6.43601673879681,80.1435865618209));
#140996=CARTESIAN_POINT('Ctrl Pts',(2.6118893476247,6.50920097562574,80.1519301183048));
#140997=CARTESIAN_POINT('Ctrl Pts',(2.43973441237396,6.57565812955311,80.1602736747887));
#140998=CARTESIAN_POINT('Ctrl Pts',(2.26534310331072,6.63519759967874,80.1686172312725));
#140999=CARTESIAN_POINT('Ctrl Pts',(2.09081911809993,6.69478236717365,80.1769671354978));
#141000=CARTESIAN_POINT('Ctrl Pts',(1.91405567501855,6.74743884726723,80.1853170397231));
#141001=CARTESIAN_POINT('Ctrl Pts',(1.73563114143768,6.79302665263222,80.1936669439483));
#141002=CARTESIAN_POINT('Ctrl Pts',(1.55693898425992,6.83868283633176,80.2020293724121));
#141003=CARTESIAN_POINT('Ctrl Pts',(1.37658107548468,6.87724907701494,80.2103918008758));
#141004=CARTESIAN_POINT('Ctrl Pts',(1.19514618438746,6.90863605644733,80.2187542293395));
#141005=CARTESIAN_POINT('Ctrl Pts',(1.0135561417248,6.94004987602587,80.2271238088195));
#141006=CARTESIAN_POINT('Ctrl Pts',(0.830887603208601,6.96427214199975,
80.2354933882996));
#141007=CARTESIAN_POINT('Ctrl Pts',(0.64773373001235,6.98126547106642,80.2438629677796));
#141008=CARTESIAN_POINT('Ctrl Pts',(0.464297364282296,6.9982850102727,80.2522454563162));
#141009=CARTESIAN_POINT('Ctrl Pts',(0.280374494561492,7.00805331469375,
80.2606279448528));
#141010=CARTESIAN_POINT('Ctrl Pts',(0.0965589714397479,7.01058506314092,
80.2690104333895));
#141011=CARTESIAN_POINT('Ctrl Pts',(0.0364115202877523,7.01141349271786,
80.2717533209934));
#141012=CARTESIAN_POINT('Ctrl Pts',(-0.0237244746587937,7.01146751427336,
80.2744962085974));
#141013=CARTESIAN_POINT('Ctrl Pts',(-0.0838283466075951,7.01074884522367,
80.2772390962014));
#141014=CARTESIAN_POINT('Ctrl Pts',(-0.267672109595901,7.00855060377677,
80.2856289513342));
#141015=CARTESIAN_POINT('Ctrl Pts',(-0.451586127756361,6.99911472365723,
80.2940188064669));
#141016=CARTESIAN_POINT('Ctrl Pts',(-0.634977094669979,6.98243730023725,
80.3024086615997));
#141017=CARTESIAN_POINT('Ctrl Pts',(-0.818198830970368,6.96577526650979,
80.3107907746918));
#141018=CARTESIAN_POINT('Ctrl Pts',(-1.0008981524198,6.94188504045496,80.3191728877839));
#141019=CARTESIAN_POINT('Ctrl Pts',(-1.18248311805108,6.910814730408,80.3275550008759));
#141020=CARTESIAN_POINT('Ctrl Pts',(-1.36392721223472,6.8797685243365,80.3359306112248));
#141021=CARTESIAN_POINT('Ctrl Pts',(-1.54425835130262,6.8415533948439,80.3443062215737));
#141022=CARTESIAN_POINT('Ctrl Pts',(-1.72289061495453,6.79626915972297,
80.3526818319225));
#141023=CARTESIAN_POINT('Ctrl Pts',(-1.9014105162599,6.75101340905842,80.3610521738881));
#141024=CARTESIAN_POINT('Ctrl Pts',(-2.07823335505137,6.69869749940276,
80.3694225158536));
#141025=CARTESIAN_POINT('Ctrl Pts',(-2.25278384019573,6.63947223293034,
80.3777928578192));
#141026=CARTESIAN_POINT('Ctrl Pts',(-2.42725011763388,6.58027553827103,
80.3861591617135));
#141027=CARTESIAN_POINT('Ctrl Pts',(-2.59944591677244,6.51417623927701,
80.3945254656078));
#141028=CARTESIAN_POINT('Ctrl Pts',(-2.76881109923561,6.44137498203992,
80.4028917695021));
#141029=CARTESIAN_POINT('Ctrl Pts',(-2.9381289150043,6.36859408527396,80.4112557335757));
#141030=CARTESIAN_POINT('Ctrl Pts',(-3.10461739037919,6.28911509603929,
80.4196196976493));
#141031=CARTESIAN_POINT('Ctrl Pts',(-3.26773585022894,6.20318700150403,
80.4279836617229));
#141032=CARTESIAN_POINT('Ctrl Pts',(-3.43082920885846,6.11727212987454,
80.4363463387215));
#141033=CARTESIAN_POINT('Ctrl Pts',(-3.59055329523153,6.02491028474506,
80.44470901572));
#141034=CARTESIAN_POINT('Ctrl Pts',(-3.7463911812716,5.92639685469936,80.4530716927186));
#141035=CARTESIAN_POINT('Ctrl Pts',(-3.90222585889429,5.82788545286521,
80.4614341975449));
#141036=CARTESIAN_POINT('Ctrl Pts',(-4.05417421814168,5.72322289460479,
80.4697967023711));
#141037=CARTESIAN_POINT('Ctrl Pts',(-4.20174715382017,5.61274865087188,
80.4781592071974));
#141038=CARTESIAN_POINT('Ctrl Pts',(-4.34933672166354,5.5022619561714,80.4865226545174));
#141039=CARTESIAN_POINT('Ctrl Pts',(-4.49254962001396,5.38596246748469,
80.4948861018374));
#141040=CARTESIAN_POINT('Ctrl Pts',(-4.63092841240748,5.2642310551169,80.5032495491573));
#141041=CARTESIAN_POINT('Ctrl Pts',(-4.76938868612286,5.14242796387245,
80.5116179211101));
#141042=CARTESIAN_POINT('Ctrl Pts',(-4.90300891832457,5.01518677422717,
80.5199862930629));
#141043=CARTESIAN_POINT('Ctrl Pts',(-5.03136649664168,4.88292716912424,
80.5283546650157));
#141044=CARTESIAN_POINT('Ctrl Pts',(-5.15976253424397,4.75062793558692,
80.5367255443515));
#141045=CARTESIAN_POINT('Ctrl Pts',(-5.28289254866523,4.61330752793419,
80.5450964236872));
#141046=CARTESIAN_POINT('Ctrl Pts',(-5.40037261364649,4.4714206015848,80.5534673030229));
#141047=CARTESIAN_POINT('Ctrl Pts',(-5.51795221821635,4.32941345597712,
80.5618452749142));
#141048=CARTESIAN_POINT('Ctrl Pts',(-5.62987210216362,4.182832317173,80.5702232468055));
#141049=CARTESIAN_POINT('Ctrl Pts',(-5.735789559204,4.03216377333887,80.5786012186967));
#141050=CARTESIAN_POINT('Ctrl Pts',(-5.80310096564505,3.93641268682976,
80.583925488056));
#141051=CARTESIAN_POINT('Ctrl Pts',(-5.86798902647246,3.83901142386068,
80.5892497574152));
#141052=CARTESIAN_POINT('Ctrl Pts',(-5.93037513265348,3.74009055351675,
80.5945740267744));
#141053=CARTESIAN_POINT('Ctrl Pts',(-6.02250635073442,3.5940051374472,80.6024368579636));
#141054=CARTESIAN_POINT('Ctrl Pts',(-6.1093702199643,3.44430041469925,80.6102996891528));
#141055=CARTESIAN_POINT('Ctrl Pts',(-6.19065813649915,3.29140978905649,
80.618162520342));
#141056=CARTESIAN_POINT('Ctrl Pts',(-6.27188359399999,3.13863663967828,
80.6260193099834));
#141057=CARTESIAN_POINT('Ctrl Pts',(-6.34754144108903,2.98268278996944,
80.6338760996247));
#141058=CARTESIAN_POINT('Ctrl Pts',(-6.41736637059734,2.82401052193974,
80.6417328892661));
#141059=CARTESIAN_POINT('Ctrl Pts',(-6.48715192215077,2.66542773755797,
80.64958524805));
#141060=CARTESIAN_POINT('Ctrl Pts',(-6.55111094658078,2.50412993235009,
80.6574376068339));
#141061=CARTESIAN_POINT('Ctrl Pts',(-6.60902421618718,2.34060365554517,
80.6652899656178));
#141062=CARTESIAN_POINT('Ctrl Pts',(-6.66692381179491,2.1771159892022,80.6731404703682));
#141063=CARTESIAN_POINT('Ctrl Pts',(-6.71878035852728,2.01140125473838,
80.6809909751185));
#141064=CARTESIAN_POINT('Ctrl Pts',(-6.76442292621371,1.84396557392331,
80.6888414798689));
#141065=CARTESIAN_POINT('Ctrl Pts',(-6.81005815144955,1.67655682823214,
80.6966907217205));
#141066=CARTESIAN_POINT('Ctrl Pts',(-6.849481290175,1.50742805619762,80.7045399635721));
#141067=CARTESIAN_POINT('Ctrl Pts',(-6.88257154375768,1.33709966253717,
80.7123892054236));
#141068=CARTESIAN_POINT('Ctrl Pts',(-6.91567294609449,1.16671388190697,
80.7202410918384));
#141069=CARTESIAN_POINT('Ctrl Pts',(-6.94243712858262,0.995128047188277,
80.7280929782533));
#141070=CARTESIAN_POINT('Ctrl Pts',(-6.96279456425622,0.822872054735126,
80.7359448646681));
#141071=CARTESIAN_POINT('Ctrl Pts',(-6.97774277588813,0.696386623498159,
80.7417104071323));
#141072=CARTESIAN_POINT('Ctrl Pts',(-6.9892376781195,0.569540069089464,
80.7474759495964));
#141073=CARTESIAN_POINT('Ctrl Pts',(-6.99726959917364,0.442543465639617,
80.7532414920606));
#141074=CARTESIAN_POINT('Ctrl Pts',(-7.01072030964118,0.229867751841124,
80.7628967964207));
#141075=CARTESIAN_POINT('Ctrl Pts',(-7.01445165797892,0.0168796950760844,
80.7725521007808));
#141076=CARTESIAN_POINT('Ctrl Pts',(-7.00852054169979,-0.195617941590344,
80.782207405141));
#141077=CARTESIAN_POINT('Ctrl Pts',(-7.00255656814913,-0.409292775300087,
80.7919161980759));
#141078=CARTESIAN_POINT('Ctrl Pts',(-6.98682283297508,-0.622471694557186,
80.8016249910109));
#141079=CARTESIAN_POINT('Ctrl Pts',(-6.96142836349325,-0.834351066669008,
80.8113337839458));
#141080=CARTESIAN_POINT('Ctrl Pts',(-6.93591169366798,-1.04725002031054,
80.8210892964168));
#141081=CARTESIAN_POINT('Ctrl Pts',(-6.90064111825457,-1.2588368495497,
80.8308448088877));
#141082=CARTESIAN_POINT('Ctrl Pts',(-6.85577812303943,-1.46830953485768,
80.8406003213587));
#141083=CARTESIAN_POINT('Ctrl Pts',(-6.81087070655703,-1.67798963035071,
80.8503654932878));
#141084=CARTESIAN_POINT('Ctrl Pts',(-6.7563518911193,-1.88555135962937,
80.860130665217));
#141085=CARTESIAN_POINT('Ctrl Pts',(-6.69243403458003,-2.09020411809346,
80.8698958371461));
#141086=CARTESIAN_POINT('Ctrl Pts',(-6.62860332858805,-2.29457783716434,
80.8796476944849));
#141087=CARTESIAN_POINT('Ctrl Pts',(-6.5553992061843,-2.49605047645186,
80.8893995518236));
#141088=CARTESIAN_POINT('Ctrl Pts',(-6.47308307805028,-2.69384892433839,
80.8991514091624));
#141089=CARTESIAN_POINT('Ctrl Pts',(-6.43718728457644,-2.78010337283751,
80.903403925224));
#141090=CARTESIAN_POINT('Ctrl Pts',(-6.39955940008401,-2.8656593266447,
80.9076564412856));
#141091=CARTESIAN_POINT('Ctrl Pts',(-6.36022408105774,-2.95045355856236,
80.9119089573472));
#141092=CARTESIAN_POINT('Ctrl Pts',(-6.28591926790672,-3.11063071524734,
80.9199420029459));
#141093=CARTESIAN_POINT('Ctrl Pts',(-6.20548203678863,-3.2681663545186,
80.9279750485447));
#141094=CARTESIAN_POINT('Ctrl Pts',(-6.11913013039224,-3.422553580271,80.9360080941434));
#141095=CARTESIAN_POINT('Ctrl Pts',(-6.03283373432616,-3.57684155997018,
80.9440359757911));
#141096=CARTESIAN_POINT('Ctrl Pts',(-5.94063040951043,-3.72798483622312,
80.9520638574389));
#141097=CARTESIAN_POINT('Ctrl Pts',(-5.84278502933152,-3.87549863417851,
80.9600917390866));
#141098=CARTESIAN_POINT('Ctrl Pts',(-5.74498382730625,-4.02294582820004,
80.9681159960666));
#141099=CARTESIAN_POINT('Ctrl Pts',(-5.64154584437271,-4.16676650200938,
80.9761402530466));
#141100=CARTESIAN_POINT('Ctrl Pts',(-5.5327806796164,-4.30650258490152,
80.9841645100267));
#141101=CARTESIAN_POINT('Ctrl Pts',(-5.42402866567635,-4.44622177227794,
80.9921877967923));
#141102=CARTESIAN_POINT('Ctrl Pts',(-5.30995097181349,-4.58185705860183,
81.0002110835579));
#141103=CARTESIAN_POINT('Ctrl Pts',(-5.1908992118005,-4.71298121526375,
81.0082343703235));
#141104=CARTESIAN_POINT('Ctrl Pts',(-5.07185720701735,-4.8440946274706,
81.0162569996524));
#141105=CARTESIAN_POINT('Ctrl Pts',(-4.9478421973795,-4.97069737756557,
81.0242796289812));
#141106=CARTESIAN_POINT('Ctrl Pts',(-4.81924438109398,-5.09239728986203,
81.03230225831));
#141107=CARTESIAN_POINT('Ctrl Pts',(-4.69059822118459,-5.21414295266153,
81.0403279035764));
#141108=CARTESIAN_POINT('Ctrl Pts',(-4.55736608151836,-5.33098184577353,
81.0483535488427));
#141109=CARTESIAN_POINT('Ctrl Pts',(-4.41997340705431,-5.44256021036357,
81.056379194109));
#141110=CARTESIAN_POINT('Ctrl Pts',(-4.33895831388655,-5.50835361338182,
81.0611116036171));
#141111=CARTESIAN_POINT('Ctrl Pts',(-4.25649724148683,-5.57231868471149,
81.0658440131253));
#141112=CARTESIAN_POINT('Ctrl Pts',(-4.17268247625876,-5.63438971982087,
81.0705764226334));
#141113=CARTESIAN_POINT('Ctrl Pts',(-4.01806631460807,-5.74889442757948,
81.0793064714681));
#141114=CARTESIAN_POINT('Ctrl Pts',(-3.85876470267636,-5.85700877924137,
81.0880365203028));
#141115=CARTESIAN_POINT('Ctrl Pts',(-3.695317882781,-5.95837665037206,81.0967665691375));
#141116=CARTESIAN_POINT('Ctrl Pts',(-3.53182380203384,-6.05977383214909,
81.1054991422767));
#141117=CARTESIAN_POINT('Ctrl Pts',(-3.36418235367307,-6.1544204952032,
81.1142317154159));
#141118=CARTESIAN_POINT('Ctrl Pts',(-3.19296058830227,-6.24200522621124,
81.122964288555));
#141119=CARTESIAN_POINT('Ctrl Pts',(-3.01930634443343,-6.33083423813458,
81.1318209218355));
#141120=CARTESIAN_POINT('Ctrl Pts',(-2.84196953804195,-6.41239900471871,
81.1406775551159));
#141121=CARTESIAN_POINT('Ctrl Pts',(-2.66156554982748,-6.4864239289821,
81.1495341883963));
#141122=CARTESIAN_POINT('Ctrl Pts',(-2.48357535516818,-6.55945840460365,
81.158272320503));
#141123=CARTESIAN_POINT('Ctrl Pts',(-2.30259981210271,-6.62515346606485,
81.1670104526098));
#141124=CARTESIAN_POINT('Ctrl Pts',(-2.11924896866071,-6.68329337761934,
81.1757485847166));
#141125=CARTESIAN_POINT('Ctrl Pts',(-1.93216838815308,-6.74261597576009,
81.1846644685838));
#141126=CARTESIAN_POINT('Ctrl Pts',(-1.74261511626696,-6.79407266353018,
81.1935803524511));
#141127=CARTESIAN_POINT('Ctrl Pts',(-1.55125325708558,-6.83748783508105,
81.2024962363183));
#141128=CARTESIAN_POINT('Ctrl Pts',(-1.35989139790407,-6.88090300663196,
81.2114121201855));
#141129=CARTESIAN_POINT('Ctrl Pts',(-1.1667212476906,-6.91627660098658,
81.2203280040528));
#141130=CARTESIAN_POINT('Ctrl Pts',(-0.972418757270449,-6.94348819564119,
81.22924388792));
#141131=CARTESIAN_POINT('Ctrl Pts',(-0.781934359883963,-6.97016507558495,
81.2379845724164));
#141132=CARTESIAN_POINT('Ctrl Pts',(-0.590341479405468,-6.98900058238748,
81.2467252569127));
#141133=CARTESIAN_POINT('Ctrl Pts',(-0.398283611584763,-6.99992833729339,
81.2554659414091));
#141134=CARTESIAN_POINT('Ctrl Pts',(-0.206260298165024,-7.01085412611466,
81.2642050533111));
#141135=CARTESIAN_POINT('Ctrl Pts',(-0.0137724377309688,-7.01387498880386,
81.2729441652131));
#141136=CARTESIAN_POINT('Ctrl Pts',(0.178533260358716,-7.0089765613423,
81.2816832771151));
#141137=CARTESIAN_POINT('Ctrl Pts',(0.373330555539247,-7.00401466770301,
81.2905356167893));
#141138=CARTESIAN_POINT('Ctrl Pts',(0.567940649624519,-6.99092682656626,
81.2993879564636));
#141139=CARTESIAN_POINT('Ctrl Pts',(0.76169195267159,-6.96975264494626,
81.3082402961379));
#141140=CARTESIAN_POINT('Ctrl Pts',(0.952867000153031,-6.94886001035272,
81.3169749287878));
#141141=CARTESIAN_POINT('Ctrl Pts',(1.1432056751845,-6.92009478765721,81.3257095614377));
#141142=CARTESIAN_POINT('Ctrl Pts',(1.33206753068949,-6.88354724369513,
81.3344441940876));
#141143=CARTESIAN_POINT('Ctrl Pts',(1.5247470110319,-6.84626093323517,81.343355387274));
#141144=CARTESIAN_POINT('Ctrl Pts',(1.71588904235505,-6.80087436321675,
81.3522665804605));
#141145=CARTESIAN_POINT('Ctrl Pts',(1.90482298408067,-6.7475385113253,81.361177773647));
#141146=CARTESIAN_POINT('Ctrl Pts',(2.09375692580615,-6.69420265943389,
81.3700889668335));
#141147=CARTESIAN_POINT('Ctrl Pts',(2.2804824825452,-6.63291759505681,81.37900016002));
#141148=CARTESIAN_POINT('Ctrl Pts',(2.46434297795493,-6.5638891100859,81.3879113532064));
#141149=CARTESIAN_POINT('Ctrl Pts',(2.62993277999947,-6.50172016435182,
81.3959370180587));
#141150=CARTESIAN_POINT('Ctrl Pts',(2.79327456229149,-6.43324124240426,
81.403962682911));
#141151=CARTESIAN_POINT('Ctrl Pts',(2.95385099394157,-6.35864693689549,
81.4119883477633));
#141152=CARTESIAN_POINT('Ctrl Pts',(3.11437646257088,-6.28407630578963,
81.4200114654664));
#141153=CARTESIAN_POINT('Ctrl Pts',(3.27213799583088,-6.20339430947099,
81.4280345831695));
#141154=CARTESIAN_POINT('Ctrl Pts',(3.42663855476052,-6.1168435305743,81.4360577008726));
#141155=CARTESIAN_POINT('Ctrl Pts',(3.58111962981761,-6.03030366648827,
81.4440798067903));
#141156=CARTESIAN_POINT('Ctrl Pts',(3.73234023025387,-5.93789667364881,
81.4521019127081));
#141157=CARTESIAN_POINT('Ctrl Pts',(3.87982827558596,-5.83991088240768,
81.4601240186258));
#141158=CARTESIAN_POINT('Ctrl Pts',(4.02737112797399,-5.74188867931549,
81.4681491055852));
#141159=CARTESIAN_POINT('Ctrl Pts',(4.17117834713499,-5.63828373696298,
81.4761741925446));
#141160=CARTESIAN_POINT('Ctrl Pts',(4.31080682206587,-5.52942773759911,
81.4841992795041));
#141161=CARTESIAN_POINT('Ctrl Pts',(4.45046279612595,-5.42055029959105,
81.4922259469642));
#141162=CARTESIAN_POINT('Ctrl Pts',(4.58593810276495,-5.30641997666109,
81.5002526144243));
#141163=CARTESIAN_POINT('Ctrl Pts',(4.71682322992565,-5.18740832980534,
81.5082792818844));
#141164=CARTESIAN_POINT('Ctrl Pts',(4.84781343120537,-5.06830114081873,
81.5163123931249));
#141165=CARTESIAN_POINT('Ctrl Pts',(4.97420582827055,-4.94430505470051,
81.5243455043654));
#141166=CARTESIAN_POINT('Ctrl Pts',(5.09562781225362,-4.81582846055457,
81.5323786156058));
#141167=CARTESIAN_POINT('Ctrl Pts',(5.16717405612213,-4.74012538410473,
81.5371120165682));
#141168=CARTESIAN_POINT('Ctrl Pts',(5.2369953112006,-4.66286733768816,81.5418454175305));
#141169=CARTESIAN_POINT('Ctrl Pts',(5.30502200952489,-4.58414310869072,
81.5465788184928));
#141170=CARTESIAN_POINT('Ctrl Pts',(5.44515912518696,-4.4219687469154,81.5563297717873));
#141171=CARTESIAN_POINT('Ctrl Pts',(5.57776152514571,-4.25347547125358,
81.5660807250817));
#141172=CARTESIAN_POINT('Ctrl Pts',(5.70234640900847,-4.07932249205284,
81.5758316783761));
#141173=CARTESIAN_POINT('Ctrl Pts',(5.82711078076822,-3.90491861281495,
81.585596679748));
#141174=CARTESIAN_POINT('Ctrl Pts',(5.94383450908284,-3.72483875133039,
81.5953616811198));
#141175=CARTESIAN_POINT('Ctrl Pts',(6.05207693009285,-3.53977278857526,
81.6051266824917));
#141176=CARTESIAN_POINT('Ctrl Pts',(6.16013893341424,-3.35501529243545,
81.6148754076296));
#141177=CARTESIAN_POINT('Ctrl Pts',(6.25974786357801,-3.16528833765755,
81.6246241327674));
#141178=CARTESIAN_POINT('Ctrl Pts',(6.35050945105486,-2.97130548321154,
81.6343728579052));
#141179=CARTESIAN_POINT('Ctrl Pts',(6.44102193316625,-2.77785503648549,
81.6440948265726));
#141180=CARTESIAN_POINT('Ctrl Pts',(6.52273553175952,-2.58017204505834,
81.6538167952399));
#141181=CARTESIAN_POINT('Ctrl Pts',(6.59530359895147,-2.37899075243218,
81.6635387639073));
#141182=CARTESIAN_POINT('Ctrl Pts',(6.6673915021967,-2.17914062387322,81.6731964048472));
#141183=CARTESIAN_POINT('Ctrl Pts',(6.73045445819763,-1.97583836989345,
81.6828540457871));
#141184=CARTESIAN_POINT('Ctrl Pts',(6.78419708066467,-1.7698295209429,81.6925116867271));
#141185=CARTESIAN_POINT('Ctrl Pts',(6.8078188134773,-1.67928153940495,81.6967565524112));
#141186=CARTESIAN_POINT('Ctrl Pts',(6.82964052972937,-1.58821100249732,
81.7010014180953));
#141187=CARTESIAN_POINT('Ctrl Pts',(6.8496399330534,-1.4966827820284,81.7052462837793));
#141188=CARTESIAN_POINT('Ctrl Pts',(6.88499295409772,-1.33488799985611,
81.7127499489352));
#141189=CARTESIAN_POINT('Ctrl Pts',(6.91464614817937,-1.17167025083209,
81.720253614091));
#141190=CARTESIAN_POINT('Ctrl Pts',(6.93848291677295,-1.00751246947618,
81.7277572792469));
#141191=CARTESIAN_POINT('Ctrl Pts',(6.9627194639257,-0.840601514549343,
81.7353867921842));
#141192=CARTESIAN_POINT('Ctrl Pts',(6.98094261072159,-0.672719122722579,
81.7430163051215));
#141193=CARTESIAN_POINT('Ctrl Pts',(6.99308397869138,-0.504383811665289,
81.7506458180588));
#141194=CARTESIAN_POINT('Ctrl Pts',(7.00522534666116,-0.336048500608132,
81.7582753309961));
#141195=CARTESIAN_POINT('Ctrl Pts',(7.01128489985528,-0.167260710844274,
81.7659048439334));
#141196=CARTESIAN_POINT('Ctrl Pts',(7.01124984869581,0.00145659295767842,
81.7735343568707));
#141197=CARTESIAN_POINT('Ctrl Pts',(7.01124984869562,0.00145659383634692,
81.7735343569104));
#141198=CARTESIAN_POINT('Ctrl Pts',(7.01121141547276,0.186453208018261,
81.7819000315001));
#141199=CARTESIAN_POINT('Ctrl Pts',(7.00384680112642,0.371311310975732,
81.7902657060898));
#141200=CARTESIAN_POINT('Ctrl Pts',(6.98921446351198,0.555434735621476,
81.7986313806795));
#141201=CARTESIAN_POINT('Ctrl Pts',(6.97456974963529,0.739713894767797,
81.8070041310889));
#141202=CARTESIAN_POINT('Ctrl Pts',(6.9526450844381,0.923256813954304,81.8153768814983));
#141203=CARTESIAN_POINT('Ctrl Pts',(6.92355038038384,1.10547577666217,81.8237496319077));
#141204=CARTESIAN_POINT('Ctrl Pts',(6.89440752844741,1.28799628762188,81.8321362381102));
#141205=CARTESIAN_POINT('Ctrl Pts',(6.85807098344372,1.46918814448923,81.8405228443127));
#141206=CARTESIAN_POINT('Ctrl Pts',(6.81470140780885,1.64847544261604,81.8489094505152));
#141207=CARTESIAN_POINT('Ctrl Pts',(6.78883754642808,1.75539513823684,81.8539108833654));
#141208=CARTESIAN_POINT('Ctrl Pts',(6.7604733779782,1.86163779181452,81.8589123162155));
#141209=CARTESIAN_POINT('Ctrl Pts',(6.72965120968403,1.96708443095315,81.8639137490656));
#141210=CARTESIAN_POINT('Ctrl Pts',(6.68257564105845,2.12813606267908,81.8715525787909));
#141211=CARTESIAN_POINT('Ctrl Pts',(6.62968735838444,2.28759443949406,81.8791914085162));
#141212=CARTESIAN_POINT('Ctrl Pts',(6.57110895151811,2.44502632087644,81.8868302382415));
#141213=CARTESIAN_POINT('',(7.01124960457286,-0.00235475623456128,81.2264656430635));
#141214=CARTESIAN_POINT('Ctrl Pts',(6.57110895151812,2.4450263208764,81.339842993376));
#141215=CARTESIAN_POINT('Ctrl Pts',(6.63162292022043,2.28239253733125,81.3319938011554));
#141216=CARTESIAN_POINT('Ctrl Pts',(6.68609251311296,2.11751758869187,81.3241446089348));
#141217=CARTESIAN_POINT('Ctrl Pts',(6.73435763417471,1.95091102245408,81.3162954167143));
#141218=CARTESIAN_POINT('Ctrl Pts',(6.78264982993078,1.78421099696964,81.3084418214284));
#141219=CARTESIAN_POINT('Ctrl Pts',(6.82473049864638,1.61577778120274,81.3005882261425));
#141220=CARTESIAN_POINT('Ctrl Pts',(6.86048993913609,1.44613428059516,81.2927346308566));
#141221=CARTESIAN_POINT('Ctrl Pts',(6.89626109718947,1.27643519163127,81.2848784621243));
#141222=CARTESIAN_POINT('Ctrl Pts',(6.92570683799432,1.10552540368255,81.277022293392));
#141223=CARTESIAN_POINT('Ctrl Pts',(6.94876907000676,0.933935208789922,
81.2691661246598));
#141224=CARTESIAN_POINT('Ctrl Pts',(6.97185266495945,0.762186066962772,
81.2613026786239));
#141225=CARTESIAN_POINT('Ctrl Pts',(6.98854091378289,0.589755639004955,
81.2534392325881));
#141226=CARTESIAN_POINT('Ctrl Pts',(6.9988277612455,0.41717685808219,81.2455757865522));
#141227=CARTESIAN_POINT('Ctrl Pts',(7.00224367819507,0.359869234436232,
81.2429645999187));
#141228=CARTESIAN_POINT('Ctrl Pts',(7.00495415094574,0.302545236695585,
81.2403534132851));
#141229=CARTESIAN_POINT('Ctrl Pts',(7.00696022589239,0.245224295823443,
81.2377422266515));
#141230=CARTESIAN_POINT('Ctrl Pts',(7.00984801535903,0.16270952759645,81.2339833654642));
#141231=CARTESIAN_POINT('Ctrl Pts',(7.01127732144654,0.0801718186302153,
81.2302245042769));
#141232=CARTESIAN_POINT('Ctrl Pts',(7.01124960457305,-0.00235475566470253,
81.2264656430895));
#141233=CARTESIAN_POINT('Ctrl Pts',(7.01124960457286,-0.00235475623456214,
81.2264656430635));
#141234=CARTESIAN_POINT('Ctrl Pts',(7.01118819206291,-0.185209537447951,
81.2181371047001));
#141235=CARTESIAN_POINT('Ctrl Pts',(7.00396906651109,-0.368204930512505,
81.2098085663366));
#141236=CARTESIAN_POINT('Ctrl Pts',(6.98958488172844,-0.550753795822862,
81.2014800279732));
#141237=CARTESIAN_POINT('Ctrl Pts',(6.97521163806677,-0.733163807993345,
81.1931578245913));
#141238=CARTESIAN_POINT('Ctrl Pts',(6.95368422473391,-0.915127636617246,
81.1848356212095));
#141239=CARTESIAN_POINT('Ctrl Pts',(6.92504733887556,-1.09605926702552,
81.1765134178276));
#141240=CARTESIAN_POINT('Ctrl Pts',(6.89642762265707,-1.27688241737952,
81.1681962041376));
#141241=CARTESIAN_POINT('Ctrl Pts',(6.86070698361759,-1.45667427311052,
81.1598789904475));
#141242=CARTESIAN_POINT('Ctrl Pts',(6.81798186851661,-1.63485467338192,
81.1515617767575));
#141243=CARTESIAN_POINT('Ctrl Pts',(6.77527549385069,-1.81295691872708,
81.1432482112309));
#141244=CARTESIAN_POINT('Ctrl Pts',(6.72557084669709,-1.98944879255069,
81.1349346457043));
#141245=CARTESIAN_POINT('Ctrl Pts',(6.66901539419426,-2.16376066941333,
81.1266210801777));
#141246=CARTESIAN_POINT('Ctrl Pts',(6.610564170535,-2.34391558021443,81.1180288391735));
#141247=CARTESIAN_POINT('Ctrl Pts',(6.54479495644247,-2.52174144346886,
81.1094365981694));
#141248=CARTESIAN_POINT('Ctrl Pts',(6.47192669577704,-2.69662593011868,
81.1008443571653));
#141249=CARTESIAN_POINT('Ctrl Pts',(6.40143816179019,-2.86579905115131,
81.0925327209809));
#141250=CARTESIAN_POINT('Ctrl Pts',(6.3243070972796,-3.03221956147002,81.0842210847965));
#141251=CARTESIAN_POINT('Ctrl Pts',(6.24078084161365,-3.19535303987652,
81.075909448612));
#141252=CARTESIAN_POINT('Ctrl Pts',(6.15724857152508,-3.3584982649329,81.0675972139368));
#141253=CARTESIAN_POINT('Ctrl Pts',(6.06732034485712,-3.51835568779264,
81.0592849792617));
#141254=CARTESIAN_POINT('Ctrl Pts',(5.97128977938191,-3.67441491031554,
81.0509727445865));
#141255=CARTESIAN_POINT('Ctrl Pts',(5.87523826249621,-3.83050818096483,
81.0426586963945));
#141256=CARTESIAN_POINT('Ctrl Pts',(5.77308192828184,-3.98280131386503,
81.0343446482026));
#141257=CARTESIAN_POINT('Ctrl Pts',(5.66515827864774,-4.1308120558032,81.0260306000106));
#141258=CARTESIAN_POINT('Ctrl Pts',(5.55719530357931,-4.27887673019018,
81.0177135223293));
#141259=CARTESIAN_POINT('Ctrl Pts',(5.44346102090149,-4.42265563212763,
81.0093964446479));
#141260=CARTESIAN_POINT('Ctrl Pts',(5.32433404808417,-4.56169853310274,
81.0010793669665));
#141261=CARTESIAN_POINT('Ctrl Pts',(5.20509635355595,-4.70087066650539,
80.9927545590369));
#141262=CARTESIAN_POINT('Ctrl Pts',(5.08045617410901,-4.83529775067298,
80.9844297511073));
#141263=CARTESIAN_POINT('Ctrl Pts',(4.95083065517876,-4.96456467237987,
80.9761049431777));
#141264=CARTESIAN_POINT('Ctrl Pts',(4.82113483814352,-5.09390169771843,
80.9677756205643));
#141265=CARTESIAN_POINT('Ctrl Pts',(4.68644853309016,-5.21807274983576,
80.959446297951));
#141266=CARTESIAN_POINT('Ctrl Pts',(4.54722334099428,-5.33670183255697,
80.9511169753377));
#141267=CARTESIAN_POINT('Ctrl Pts',(4.40784849322882,-5.45545843181838,
80.9427786993852));
#141268=CARTESIAN_POINT('Ctrl Pts',(4.26392527374218,-5.56866095281499,
80.9344404234328));
#141269=CARTESIAN_POINT('Ctrl Pts',(4.11593653879105,-5.67597506787554,
80.9261021474804));
#141270=CARTESIAN_POINT('Ctrl Pts',(4.08224556720107,-5.70040609502705,
80.9242038636798));
#141271=CARTESIAN_POINT('Ctrl Pts',(4.04834399747367,-5.72453211600507,
80.9223055798793));
#141272=CARTESIAN_POINT('Ctrl Pts',(4.0142377187011,-5.74834951096899,80.9204072960787));
#141273=CARTESIAN_POINT('Ctrl Pts',(3.86365171675426,-5.85350804521781,
80.9120259956738));
#141274=CARTESIAN_POINT('Ctrl Pts',(3.70875556564048,-5.95286840638953,
80.9036446952689));
#141275=CARTESIAN_POINT('Ctrl Pts',(3.55002072808798,-6.04607140155041,
80.895263394864));
#141276=CARTESIAN_POINT('Ctrl Pts',(3.39148706370504,-6.13915627555882,
80.8868927165305));
#141277=CARTESIAN_POINT('Ctrl Pts',(3.22912468852552,-6.22609917068564,
80.8785220381969));
#141278=CARTESIAN_POINT('Ctrl Pts',(3.06343546059892,-6.30658304799398,
80.8701513598634));
#141279=CARTESIAN_POINT('Ctrl Pts',(2.89793426149888,-6.38697558991984,
80.8617901808126));
#141280=CARTESIAN_POINT('Ctrl Pts',(2.72911402738103,-6.46092358098629,
80.8534290017617));
#141281=CARTESIAN_POINT('Ctrl Pts',(2.55750312363249,-6.52815474197036,
80.8450678227109));
#141282=CARTESIAN_POINT('Ctrl Pts',(2.38611490527457,-6.59529866259254,
80.8367174932762));
#141283=CARTESIAN_POINT('Ctrl Pts',(2.21194354383373,-6.65574301892428,
80.8283671638415));
#141284=CARTESIAN_POINT('Ctrl Pts',(2.03553930953716,-6.70926272267147,
80.8200168344068));
#141285=CARTESIAN_POINT('Ctrl Pts',(1.85927080774681,-6.76274124620805,
80.8116729300511));
#141286=CARTESIAN_POINT('Ctrl Pts',(1.68077316909256,-6.80930564038382,
80.8033290256953));
#141287=CARTESIAN_POINT('Ctrl Pts',(1.50061491265844,-6.84877955890005,
80.7949851213396));
#141288=CARTESIAN_POINT('Ctrl Pts',(1.32060136045926,-6.88822177171878,
80.7866479188599));
#141289=CARTESIAN_POINT('Ctrl Pts',(1.13893016972256,-6.92058479704774,
80.7783107163802));
#141290=CARTESIAN_POINT('Ctrl Pts',(0.956183382067479,-6.94574257386192,
80.7699735139005));
#141291=CARTESIAN_POINT('Ctrl Pts',(0.896024148308741,-6.95402437512166,
80.7672289528644));
#141292=CARTESIAN_POINT('Ctrl Pts',(0.8357484528534,-6.96152575851744,80.7644843918283));
#141293=CARTESIAN_POINT('Ctrl Pts',(0.77537732339638,-6.96824343495997,
80.7617398307922));
#141294=CARTESIAN_POINT('Ctrl Pts',(0.591962487992189,-6.9886525531939,
80.7534015204902));
#141295=CARTESIAN_POINT('Ctrl Pts',(0.407816762153555,-7.00180733844399,
80.7450632101883));
#141296=CARTESIAN_POINT('Ctrl Pts',(0.223536000561251,-7.00768565354876,
80.7367248998863));
#141297=CARTESIAN_POINT('Ctrl Pts',(0.0391392957665859,-7.01356766708993,
80.7283813434024));
#141298=CARTESIAN_POINT('Ctrl Pts',(-0.145392286761038,-7.01216406843352,
80.7200377869185));
#141299=CARTESIAN_POINT('Ctrl Pts',(-0.329463727115471,-7.00350485221615,
80.7116942304347));
#141300=CARTESIAN_POINT('Ctrl Pts',(-0.513675208219146,-6.99483904810485,
80.7033443262094));
#141301=CARTESIAN_POINT('Ctrl Pts',(-0.697425521947222,-6.97890663112914,
80.6949944219841));
#141302=CARTESIAN_POINT('Ctrl Pts',(-0.880125155567984,-6.95578940689239,
80.6866445177588));
#141303=CARTESIAN_POINT('Ctrl Pts',(-1.06309882511928,-6.93263750852999,
80.6782820892951));
#141304=CARTESIAN_POINT('Ctrl Pts',(-1.24501833999358,-6.90227930887797,
80.6699196608314));
#141305=CARTESIAN_POINT('Ctrl Pts',(-1.42530326558753,-6.86484793448519,
80.6615572323677));
#141306=CARTESIAN_POINT('Ctrl Pts',(-1.6057423593696,-6.82738455116459,
80.6531876528877));
#141307=CARTESIAN_POINT('Ctrl Pts',(-1.78454375773002,-6.78283600374846,
80.6448180734076));
#141308=CARTESIAN_POINT('Ctrl Pts',(-1.96114201226738,-6.73138533811725,
80.6364484939276));
#141309=CARTESIAN_POINT('Ctrl Pts',(-2.13801264809562,-6.67985531610305,
80.628066005391));
#141310=CARTESIAN_POINT('Ctrl Pts',(-2.31267303961262,-6.62140200642127,
80.6196835168544));
#141311=CARTESIAN_POINT('Ctrl Pts',(-2.48457621513433,-6.55625713297524,
80.6113010283177));
#141312=CARTESIAN_POINT('Ctrl Pts',(-2.54082575095673,-6.53494066292501,
80.6085581407138));
#141313=CARTESIAN_POINT('Ctrl Pts',(-2.59678025701267,-6.51290809479127,
80.6058152531098));
#141314=CARTESIAN_POINT('Ctrl Pts',(-2.65242114102988,-6.49016861515306,
80.6030723655058));
#141315=CARTESIAN_POINT('Ctrl Pts',(-2.82261366211158,-6.42061383657484,
80.594682510373));
#141316=CARTESIAN_POINT('Ctrl Pts',(-2.99021376345985,-6.34430126921104,
80.5862926552403));
#141317=CARTESIAN_POINT('Ctrl Pts',(-3.15466815543341,-6.26144515200719,
80.5779028001075));
#141318=CARTESIAN_POINT('Ctrl Pts',(-3.3189707911995,-6.17866549326676,
80.5695206870154));
#141319=CARTESIAN_POINT('Ctrl Pts',(-3.48013321219805,-6.08935446921641,
80.5611385739233));
#141320=CARTESIAN_POINT('Ctrl Pts',(-3.63762249876359,-5.99377419653001,
80.5527564608313));
#141321=CARTESIAN_POINT('Ctrl Pts',(-3.79498960702153,-5.89826807387763,
80.5443808504824));
#141322=CARTESIAN_POINT('Ctrl Pts',(-3.94868898201521,-5.79650256908246,
80.5360052401335));
#141323=CARTESIAN_POINT('Ctrl Pts',(-4.09821229258766,-5.68878568478225,
80.5276296297847));
#141324=CARTESIAN_POINT('Ctrl Pts',(-4.24764155077749,-5.58113655600174,
80.5192592878191));
#141325=CARTESIAN_POINT('Ctrl Pts',(-4.39289971612787,-5.4675437035836,
80.5108889458536));
#141326=CARTESIAN_POINT('Ctrl Pts',(-4.53350706626479,-5.34835864940144,
80.502518603888));
#141327=CARTESIAN_POINT('Ctrl Pts',(-4.6740465837488,-5.22923109319791,
80.4941522999937));
#141328=CARTESIAN_POINT('Ctrl Pts',(-4.80993950995811,-5.10451692730369,
80.4857859960994));
#141329=CARTESIAN_POINT('Ctrl Pts',(-4.94073852006193,-4.97460847091269,
80.4774196922051));
#141330=CARTESIAN_POINT('Ctrl Pts',(-5.07150094934882,-4.84473634627569,
80.4690557281315));
#141331=CARTESIAN_POINT('Ctrl Pts',(-5.19717206921479,-4.70967305816952,
80.4606917640579));
#141332=CARTESIAN_POINT('Ctrl Pts',(-5.31734040984741,-4.56984874238784,
80.4523277999843));
#141333=CARTESIAN_POINT('Ctrl Pts',(-5.43749025856936,-4.43004594324477,
80.4439651229857));
#141334=CARTESIAN_POINT('Ctrl Pts',(-5.55213880222743,-4.2854838263521,
80.4356024459872));
#141335=CARTESIAN_POINT('Ctrl Pts',(-5.66091369828302,-4.13662696687672,
80.4272397689887));
#141336=CARTESIAN_POINT('Ctrl Pts',(-5.76968635486227,-3.98777317209207,
80.4188772641624));
#141337=CARTESIAN_POINT('Ctrl Pts',(-5.8725854113914,-3.83462507662563,
80.4105147593361));
#141338=CARTESIAN_POINT('Ctrl Pts',(-5.96928059209372,-3.67767804128545,
80.4021522545098));
#141339=CARTESIAN_POINT('Ctrl Pts',(-6.06598667079832,-3.52071331727523,
80.3937888071898));
#141340=CARTESIAN_POINT('Ctrl Pts',(-6.15648730773457,-3.35994907984399,
80.3854253598699));
#141341=CARTESIAN_POINT('Ctrl Pts',(-6.24049688580549,-3.19590756761707,
80.3770619125499));
#141342=CARTESIAN_POINT('Ctrl Pts',(-6.32455593107694,-3.0317694631376,
80.3686935405971));
#141343=CARTESIAN_POINT('Ctrl Pts',(-6.4021161291593,-2.86435052015493,
80.3603251686443));
#141344=CARTESIAN_POINT('Ctrl Pts',(-6.47293850667418,-2.69419629042033,
80.3519567966915));
#141345=CARTESIAN_POINT('Ctrl Pts',(-6.54378210442428,-2.52399107803158,
80.3435859173558));
#141346=CARTESIAN_POINT('Ctrl Pts',(-6.60788373468279,-2.35104925021817,
80.3352150380201));
#141347=CARTESIAN_POINT('Ctrl Pts',(-6.66505324983001,-2.17593468179321,
80.3268441586843));
#141348=CARTESIAN_POINT('Ctrl Pts',(-6.72227120408923,-2.00067174068792,
80.318466186793));
#141349=CARTESIAN_POINT('Ctrl Pts',(-6.77254520996059,-1.82323269478883,
80.3100882149018));
#141350=CARTESIAN_POINT('Ctrl Pts',(-6.81573518618814,-1.64419598413845,
80.3017102430105));
#141351=CARTESIAN_POINT('Ctrl Pts',(-6.84318276777912,-1.53041669661422,
80.2963859736513));
#141352=CARTESIAN_POINT('Ctrl Pts',(-6.86777033888534,-1.41599240805197,
80.2910617042921));
#141353=CARTESIAN_POINT('Ctrl Pts',(-6.889472729271,-1.30107343187507,80.2857374349329));
#141354=CARTESIAN_POINT('Ctrl Pts',(-6.92152261639972,-1.13136216274916,
80.2778746037437));
#141355=CARTESIAN_POINT('Ctrl Pts',(-6.94734408917813,-0.960218692718378,
80.2700117725544));
#141356=CARTESIAN_POINT('Ctrl Pts',(-6.96680925618404,-0.788159470188911,
80.2621489413652));
#141357=CARTESIAN_POINT('Ctrl Pts',(-6.98625946677848,-0.616232452460369,
80.2542921517238));
#141358=CARTESIAN_POINT('Ctrl Pts',(-6.99936304151796,-0.443391457918423,
80.2464353620825));
#141359=CARTESIAN_POINT('Ctrl Pts',(-7.00604296529341,-0.270163896482813,
80.2385785724412));
#141360=CARTESIAN_POINT('Ctrl Pts',(-7.01271912190806,-0.0970340271916611,
80.2307262136572));
#141361=CARTESIAN_POINT('Ctrl Pts',(-7.01297881916433,0.0764815955293988,
80.2228738548733));
#141362=CARTESIAN_POINT('Ctrl Pts',(-7.00679681341454,0.249849910994238,
80.2150214960894));
#141363=CARTESIAN_POINT('Ctrl Pts',(-7.00061626730844,0.423177292176963,
80.207170991339));
#141364=CARTESIAN_POINT('Ctrl Pts',(-6.98799705047378,0.596357054343114,
80.1993204865887));
#141365=CARTESIAN_POINT('Ctrl Pts',(-6.96896602986842,0.768855667235388,
80.1914699818383));
#141366=CARTESIAN_POINT('Ctrl Pts',(-6.94993807075447,0.941326530537565,
80.1836207399867));
#141367=CARTESIAN_POINT('Ctrl Pts',(-6.92450040602607,1.11311608379987,
80.1757714981351));
#141368=CARTESIAN_POINT('Ctrl Pts',(-6.89273177670881,1.28369592071046,
80.1679222562835));
#141369=CARTESIAN_POINT('Ctrl Pts',(-6.8609524439185,1.45433322930696,80.1600703698687));
#141370=CARTESIAN_POINT('Ctrl Pts',(-6.8228379558657,1.62375963203353,80.1522184834539));
#141371=CARTESIAN_POINT('Ctrl Pts',(-6.77851822867896,1.7914567217678,80.1443665970391));
#141372=CARTESIAN_POINT('Ctrl Pts',(-6.74597480464092,1.91459460748116,
80.1386010545749));
#141373=CARTESIAN_POINT('Ctrl Pts',(-6.71008672266062,2.03680028130331,
80.1328355121108));
#141374=CARTESIAN_POINT('Ctrl Pts',(-6.67092249617117,2.1578738639173,80.1270699696466));
#141375=CARTESIAN_POINT('Ctrl Pts',(-6.60533586158603,2.36063055114458,
80.1174146652865));
#141376=CARTESIAN_POINT('Ctrl Pts',(-6.53059419910339,2.56010866817527,
80.1077593609264));
#141377=CARTESIAN_POINT('Ctrl Pts',(-6.44704521748296,2.75558242958364,
80.0981040565664));
#141378=CARTESIAN_POINT('Ctrl Pts',(-6.36303339017783,2.95213907896008,
80.0883952636314));
#141379=CARTESIAN_POINT('Ctrl Pts',(-6.27011646050716,3.14464686118867,
80.0786864706965));
#141380=CARTESIAN_POINT('Ctrl Pts',(-6.16869094438954,3.33239832479649,
80.0689776777616));
#141381=CARTESIAN_POINT('Ctrl Pts',(-6.06677736007615,3.52105326438949,
80.0592221652906));
#141382=CARTESIAN_POINT('Ctrl Pts',(-5.95627314588338,3.70490597294427,
80.0494666528197));
#141383=CARTESIAN_POINT('Ctrl Pts',(-5.83762301887757,3.8832697629666,80.0397111403488));
#141384=CARTESIAN_POINT('Ctrl Pts',(-5.71885540999204,4.06181016058183,
80.0299459684196));
#141385=CARTESIAN_POINT('Ctrl Pts',(-5.59192578557884,4.2348507429436,80.0201807964905));
#141386=CARTESIAN_POINT('Ctrl Pts',(-5.45732198892953,4.40173412096258,
80.0104156245614));
#141387=CARTESIAN_POINT('Ctrl Pts',(-5.32290172150337,4.56838995728151,
80.0006637672226));
#141388=CARTESIAN_POINT('Ctrl Pts',(-5.18082821859198,4.7289053387521,79.9909119098839));
#141389=CARTESIAN_POINT('Ctrl Pts',(-5.03162852562127,4.88265716005684,
79.9811600525451));
#141390=CARTESIAN_POINT('Ctrl Pts',(-4.96656665394707,4.94970408936498,
79.9769075364835));
#141391=CARTESIAN_POINT('Ctrl Pts',(-4.90015019908747,5.01546527432629,
79.9726550204218));
#141392=CARTESIAN_POINT('Ctrl Pts',(-4.8324253128829,5.07989095925381,79.9684025043601));
#141393=CARTESIAN_POINT('Ctrl Pts',(-4.7044923218825,5.20159172586908,79.9603694587613));
#141394=CARTESIAN_POINT('Ctrl Pts',(-4.57182535042884,5.31858360796275,
79.9523364131626));
#141395=CARTESIAN_POINT('Ctrl Pts',(-4.43481306854115,5.4304750813899,79.9443033675638));
#141396=CARTESIAN_POINT('Ctrl Pts',(-4.29788886342366,5.54229462666977,
79.9362754859161));
#141397=CARTESIAN_POINT('Ctrl Pts',(-4.15662519080637,5.64902005879458,
79.9282476042684));
#141398=CARTESIAN_POINT('Ctrl Pts',(-4.01144643543129,5.75029773647988,
79.9202197226206));
#141399=CARTESIAN_POINT('Ctrl Pts',(-3.86633322969545,5.8515296862953,79.9121954656406));
#141400=CARTESIAN_POINT('Ctrl Pts',(-3.71730876091136,5.9473185699505,79.9041712086606));
#141401=CARTESIAN_POINT('Ctrl Pts',(-3.56482920866232,6.03735200858522,
79.8961469516806));
#141402=CARTESIAN_POINT('Ctrl Pts',(-3.41236809274417,6.1273745612602,79.8881236649149));
#141403=CARTESIAN_POINT('Ctrl Pts',(-3.25645303700428,6.21164286210243,
79.8801003781493));
#141404=CARTESIAN_POINT('Ctrl Pts',(-3.0975679747414,6.28988864800932,79.8720770913837));
#141405=CARTESIAN_POINT('Ctrl Pts',(-2.93869593169206,6.36812802237203,
79.8640544620548));
#141406=CARTESIAN_POINT('Ctrl Pts',(-2.77685469757785,6.44034570640787,
79.856031832726));
#141407=CARTESIAN_POINT('Ctrl Pts',(-2.61255122253328,6.50632020977602,
79.8480092033971));
#141408=CARTESIAN_POINT('Ctrl Pts',(-2.44818598107929,6.57231951486054,
79.8399835581308));
#141409=CARTESIAN_POINT('Ctrl Pts',(-2.28135699111813,6.63207081687292,
79.8319579128645));
#141410=CARTESIAN_POINT('Ctrl Pts',(-2.11258987983676,6.685401301501,79.8239322675982));
#141411=CARTESIAN_POINT('Ctrl Pts',(-2.01307450685555,6.71684820504008,
79.81919985809));
#141412=CARTESIAN_POINT('Ctrl Pts',(-1.91288556627672,6.74606352631667,
79.8144674485818));
#141413=CARTESIAN_POINT('Ctrl Pts',(-1.81213302469277,6.77302004007945,
79.8097350390737));
#141414=CARTESIAN_POINT('Ctrl Pts',(-1.62627112775869,6.82274770653743,
79.8010049902389));
#141415=CARTESIAN_POINT('Ctrl Pts',(-1.43839775577256,6.8648109054016,79.7922749414041));
#141416=CARTESIAN_POINT('Ctrl Pts',(-1.24914618178807,6.89907677729595,
79.7835448925694));
#141417=CARTESIAN_POINT('Ctrl Pts',(-1.05983988547522,6.93335255720984,
79.7748123194301));
#141418=CARTESIAN_POINT('Ctrl Pts',(-0.869154861278288,6.95982646103044,
79.7660797462908));
#141419=CARTESIAN_POINT('Ctrl Pts',(-0.67773289903662,6.97841706120116,
79.7573471731516));
#141420=CARTESIAN_POINT('Ctrl Pts',(-0.483591482257702,6.99727177052316,
79.7484905398712));
#141421=CARTESIAN_POINT('Ctrl Pts',(-0.288692317572583,7.00801745122328,
79.7396339065908));
#141422=CARTESIAN_POINT('Ctrl Pts',(-0.0937089961110163,7.01062373733949,
79.7307772733105));
#141423=CARTESIAN_POINT('Ctrl Pts',(0.0986654612738358,7.01319515151808,
79.7220391412036));
#141424=CARTESIAN_POINT('Ctrl Pts',(0.291121559355534,7.00784364703478,
79.7133010090968));
#141425=CARTESIAN_POINT('Ctrl Pts',(0.483012649033695,6.99459257879781,
79.7045628769899));
#141426=CARTESIAN_POINT('Ctrl Pts',(0.678807202123559,6.98107195630424,
79.6956469931228));
#141427=CARTESIAN_POINT('Ctrl Pts',(0.87401321793027,6.95932695708805,79.6867311092557));
#141428=CARTESIAN_POINT('Ctrl Pts',(1.06794850414328,6.92943811250221,79.6778152253885));
#141429=CARTESIAN_POINT('Ctrl Pts',(1.26188379035636,6.89954926791636,79.6688993415214));
#141430=CARTESIAN_POINT('Ctrl Pts',(1.45454804901883,6.86151663003608,79.6599834576543));
#141431=CARTESIAN_POINT('Ctrl Pts',(1.64526833286611,6.8154764085402,79.6510675737872));
#141432=CARTESIAN_POINT('Ctrl Pts',(1.83224091494127,6.77034088903095,79.6423268892911));
#141433=CARTESIAN_POINT('Ctrl Pts',(2.01736507058887,6.71750477297077,79.633586204795));
#141434=CARTESIAN_POINT('Ctrl Pts',(2.20001788583994,6.65714262010995,79.6248455202989));
#141435=CARTESIAN_POINT('Ctrl Pts',(2.38263783881556,6.59679132740308,79.6161064083971));
#141436=CARTESIAN_POINT('Ctrl Pts',(2.56278707949173,6.5289167879364,79.6073672964953));
#141437=CARTESIAN_POINT('Ctrl Pts',(2.73985880537629,6.45374312233622,79.5986281845935));
#141438=CARTESIAN_POINT('Ctrl Pts',(2.91922475032313,6.37759547370322,79.5897758449191));
#141439=CARTESIAN_POINT('Ctrl Pts',(3.09543260615769,6.29395832975056,79.5809235052447));
#141440=CARTESIAN_POINT('Ctrl Pts',(3.26787224700597,6.20311514803233,79.5720711655703));
#141441=CARTESIAN_POINT('Ctrl Pts',(3.43801900734852,6.11347988207765,79.5633365329207));
#141442=CARTESIAN_POINT('Ctrl Pts',(3.6044968980425,6.01682916476232,79.554601900271));
#141443=CARTESIAN_POINT('Ctrl Pts',(3.76674336334902,5.91348213806097,79.5458672676214));
#141444=CARTESIAN_POINT('Ctrl Pts',(3.93226945405079,5.80804607026616,79.5369560744346));
#141445=CARTESIAN_POINT('Ctrl Pts',(4.09339097409204,5.69564023119062,79.5280448812479));
#141446=CARTESIAN_POINT('Ctrl Pts',(4.24953957757411,5.57665131966589,79.5191336880611));
#141447=CARTESIAN_POINT('Ctrl Pts',(4.40568818105612,5.4576624081412,79.5102224948744));
#141448=CARTESIAN_POINT('Ctrl Pts',(4.55686361870708,5.33209059717816,79.5013113016876));
#141449=CARTESIAN_POINT('Ctrl Pts',(4.7025306618469,5.2003684424173,79.4924001085009));
#141450=CARTESIAN_POINT('Ctrl Pts',(4.83372204101002,5.08173617820069,79.4843744652328));
#141451=CARTESIAN_POINT('Ctrl Pts',(4.96050536383317,4.95806030922865,79.4763488219647));
#141452=CARTESIAN_POINT('Ctrl Pts',(5.08247090262828,4.82971180159199,79.4683231786966));
#141453=CARTESIAN_POINT('Ctrl Pts',(5.20439720845569,4.70140458014898,79.4603001170577));
#141454=CARTESIAN_POINT('Ctrl Pts',(5.32150856365554,4.5684279780931,79.4522770554189));
#141455=CARTESIAN_POINT('Ctrl Pts',(5.43343174174833,4.43119014151522,79.4442539937801));
#141456=CARTESIAN_POINT('Ctrl Pts',(5.54534032455606,4.29397020136757,79.4362319783845));
#141457=CARTESIAN_POINT('Ctrl Pts',(5.65206184695248,4.15249041808088,79.4282099629889));
#141458=CARTESIAN_POINT('Ctrl Pts',(5.75326309952588,4.00719231758769,79.4201879475934));
#141459=CARTESIAN_POINT('Ctrl Pts',(5.85449755639625,3.86184654454942,79.4121633001614));
#141460=CARTESIAN_POINT('Ctrl Pts',(5.95020791413237,3.71268025162831,79.4041386527294));
#141461=CARTESIAN_POINT('Ctrl Pts',(6.04010386323041,3.56016458662926,79.3961140052974));
#141462=CARTESIAN_POINT('Ctrl Pts',(6.13001735862996,3.40761915292684,79.3880877915782));
#141463=CARTESIAN_POINT('Ctrl Pts',(6.21411400611913,3.25172336500418,79.3800615778589));
#141464=CARTESIAN_POINT('Ctrl Pts',(6.29214938284766,3.09297311763776,79.3720353641396));
#141465=CARTESIAN_POINT('Ctrl Pts',(6.37023961705004,2.93411127168734,79.3640035081357));
#141466=CARTESIAN_POINT('Ctrl Pts',(6.44225992040282,2.77239129287253,79.3559716521318));
#141467=CARTESIAN_POINT('Ctrl Pts',(6.50801376409652,2.60832962043341,79.3479397961278));
#141468=CARTESIAN_POINT('Ctrl Pts',(6.52973061026753,2.55414416293352,79.3452870754425));
#141469=CARTESIAN_POINT('Ctrl Pts',(6.5507643016582,2.49970340540043,79.3426343547572));
#141470=CARTESIAN_POINT('Ctrl Pts',(6.57110895151812,2.44502632087642,79.3399816340719));
#141471=CARTESIAN_POINT('Origin',(0.,0.,50.));
#141472=CARTESIAN_POINT('',(6.57110895151816,2.4450263208763,77.3398522865014));
#141473=CARTESIAN_POINT('',(6.57110895151815,2.44502632087633,77.886969536131));
#141474=CARTESIAN_POINT('',(6.57110895151814,2.44502632087636,50.));
#141475=CARTESIAN_POINT('',(7.01124999765299,0.000181413712741437,79.7735343568736));
#141476=CARTESIAN_POINT('Ctrl Pts',(6.57110895151815,2.44502632087633,77.886969536131));
#141477=CARTESIAN_POINT('Ctrl Pts',(6.54472329191852,2.51593886791374,77.8903887297223));
#141478=CARTESIAN_POINT('Ctrl Pts',(6.5171868554085,2.58643166442415,77.8938079233136));
#141479=CARTESIAN_POINT('Ctrl Pts',(6.48851466909111,2.6564645586737,77.897227116905));
#141480=CARTESIAN_POINT('Ctrl Pts',(6.4185924549299,2.82725219850838,77.9055654272069));
#141481=CARTESIAN_POINT('Ctrl Pts',(6.3419518830268,2.99520730994608,77.9139037375089));
#141482=CARTESIAN_POINT('Ctrl Pts',(6.25885887899737,3.1597962110389,77.9222420478109));
#141483=CARTESIAN_POINT('Ctrl Pts',(6.1757135956692,3.32448866588369,77.9305856042948));
#141484=CARTESIAN_POINT('Ctrl Pts',(6.08610793039912,3.48581039346846,77.9389291607787));
#141485=CARTESIAN_POINT('Ctrl Pts',(5.99035317373331,3.64325341095611,77.9472727172626));
#141486=CARTESIAN_POINT('Ctrl Pts',(5.894525567266,3.80081621040521,77.9556226214879));
#141487=CARTESIAN_POINT('Ctrl Pts',(5.79253970798148,3.95449413403783,77.9639725257131));
#141488=CARTESIAN_POINT('Ctrl Pts',(5.68474973206404,4.10380884621809,77.9723224299384));
#141489=CARTESIAN_POINT('Ctrl Pts',(5.57679807915941,4.25334751941701,77.9806848584022));
#141490=CARTESIAN_POINT('Ctrl Pts',(5.46302510475072,4.39850963731453,77.9890472868659));
#141491=CARTESIAN_POINT('Ctrl Pts',(5.34382565033219,4.53884941161874,77.9974097153296));
#141492=CARTESIAN_POINT('Ctrl Pts',(5.22452426413071,4.67930919556127,78.0057792948096));
#141493=CARTESIAN_POINT('Ctrl Pts',(5.09978736043104,4.8149381673483,78.0141488742897));
#141494=CARTESIAN_POINT('Ctrl Pts',(4.97004642619015,4.94532760128331,78.0225184537697));
#141495=CARTESIAN_POINT('Ctrl Pts',(4.84010538236574,5.07591814503361,78.0309009423064));
#141496=CARTESIAN_POINT('Ctrl Pts',(4.70514512454138,5.20125277945567,78.039283430843));
#141497=CARTESIAN_POINT('Ctrl Pts',(4.56563102380178,5.32096231118006,78.0476659193797));
#141498=CARTESIAN_POINT('Ctrl Pts',(4.51997972397395,5.36013323151019,78.0504088069836));
#141499=CARTESIAN_POINT('Ctrl Pts',(4.47384107816586,5.39870221087662,78.0531516945875));
#141500=CARTESIAN_POINT('Ctrl Pts',(4.42723205493097,5.43665732728225,78.0558945821914));
#141501=CARTESIAN_POINT('Ctrl Pts',(4.28466589499671,5.55275319928838,78.0642844373241));
#141502=CARTESIAN_POINT('Ctrl Pts',(4.13740883337362,5.66333692192329,78.072674292457));
#141503=CARTESIAN_POINT('Ctrl Pts',(3.98591391741904,5.76802538182914,78.0810641475897));
#141504=CARTESIAN_POINT('Ctrl Pts',(3.83455879884903,5.87261723669187,78.0894462606818));
#141505=CARTESIAN_POINT('Ctrl Pts',(3.67897389092021,5.97132448761054,78.0978283737739));
#141506=CARTESIAN_POINT('Ctrl Pts',(3.51964451587166,6.063804832314,78.106210486866));
#141507=CARTESIAN_POINT('Ctrl Pts',(3.36043874664933,6.15621343187057,78.1145860972149));
#141508=CARTESIAN_POINT('Ctrl Pts',(3.19749458510357,6.24240459184611,78.1229617075637));
#141509=CARTESIAN_POINT('Ctrl Pts',(3.03132585956824,6.32207957049047,78.1313373179126));
#141510=CARTESIAN_POINT('Ctrl Pts',(2.8652616566293,6.40170443238987,78.1397076598781));
#141511=CARTESIAN_POINT('Ctrl Pts',(2.6959772295971,6.4748211437882,78.1480780018437));
#141512=CARTESIAN_POINT('Ctrl Pts',(2.52401090989317,6.5411769192738,78.1564483438093));
#141513=CARTESIAN_POINT('Ctrl Pts',(2.35212755122628,6.60750068300292,78.1648146477036));
#141514=CARTESIAN_POINT('Ctrl Pts',(2.17756518610174,6.66706989695353,78.1731809515979));
#141515=CARTESIAN_POINT('Ctrl Pts',(2.0008824450884,6.71967975452976,78.1815472554922));
#141516=CARTESIAN_POINT('Ctrl Pts',(1.82424911728582,6.77227489860332,78.1899112195658));
#141517=CARTESIAN_POINT('Ctrl Pts',(1.64549691034441,6.81791447217705,78.1982751836394));
#141518=CARTESIAN_POINT('Ctrl Pts',(1.46520048149888,6.85644325518089,78.206639147713));
#141519=CARTESIAN_POINT('Ctrl Pts',(1.28493179727746,6.89496610924532,78.2150018247116));
#141520=CARTESIAN_POINT('Ctrl Pts',(1.10311968624668,6.9263802857582,78.2233645017101));
#141521=CARTESIAN_POINT('Ctrl Pts',(0.920350300449677,6.95058140639776,
78.2317271787086));
#141522=CARTESIAN_POINT('Ctrl Pts',(0.737584677540096,6.97478202878049,
78.2400896835349));
#141523=CARTESIAN_POINT('Ctrl Pts',(0.553862145020714,6.99176984866395,
78.2484521883612));
#141524=CARTESIAN_POINT('Ctrl Pts',(0.369775734515736,7.00149216015153,
78.2568146931876));
#141525=CARTESIAN_POINT('Ctrl Pts',(0.185668576605704,7.01121556738939,
78.2651781405075));
#141526=CARTESIAN_POINT('Ctrl Pts',(0.00119778715327035,7.01367181686934,
78.2735415878275));
#141527=CARTESIAN_POINT('Ctrl Pts',(-0.183041394468293,7.00886027899052,
78.2819050351475));
#141528=CARTESIAN_POINT('Ctrl Pts',(-0.367389061298113,7.00404590794297,
78.2902734071003));
#141529=CARTESIAN_POINT('Ctrl Pts',(-0.551504518869215,6.99195520575042,
78.2986417790531));
#141530=CARTESIAN_POINT('Ctrl Pts',(-0.734794400028367,6.97263965454884,
78.3070101510059));
#141531=CARTESIAN_POINT('Ctrl Pts',(-0.918139199626124,6.95331831590332,
78.3153810303416));
#141532=CARTESIAN_POINT('Ctrl Pts',(-1.10065760321633,6.92676785149604,
78.3237519096774));
#141533=CARTESIAN_POINT('Ctrl Pts',(-1.28176354146575,6.8930913809603,78.3321227890131));
#141534=CARTESIAN_POINT('Ctrl Pts',(-1.46302292881792,6.8593863767153,78.3405007609044));
#141535=CARTESIAN_POINT('Ctrl Pts',(-1.64286713708827,6.81854336718499,
78.3488787327957));
#141536=CARTESIAN_POINT('Ctrl Pts',(-1.82072128776991,6.77071639893162,
78.357256704687));
#141537=CARTESIAN_POINT('Ctrl Pts',(-1.93374904880257,6.74032197114941,
78.3625809740461));
#141538=CARTESIAN_POINT('Ctrl Pts',(-2.04597335456123,6.70710794305258,
78.3679052434052));
#141539=CARTESIAN_POINT('Ctrl Pts',(-2.15725019586244,6.67112420473128,
78.3732295127643));
#141540=CARTESIAN_POINT('Ctrl Pts',(-2.32158279427306,6.61798375655067,
78.3810923439535));
#141541=CARTESIAN_POINT('Ctrl Pts',(-2.48418984036486,6.55868970666489,
78.3889551751428));
#141542=CARTESIAN_POINT('Ctrl Pts',(-2.644556713752,6.49337711443354,78.396818006332));
#141543=CARTESIAN_POINT('Ctrl Pts',(-2.80480036636516,6.42811470630814,
78.4046747959733));
#141544=CARTESIAN_POINT('Ctrl Pts',(-2.96280691845336,6.35684309511312,
78.4125315856147));
#141545=CARTESIAN_POINT('Ctrl Pts',(-3.11807649192569,6.27974725231839,
78.420388375256));
#141546=CARTESIAN_POINT('Ctrl Pts',(-3.2732585007094,6.2026948879291,78.4282407340399));
#141547=CARTESIAN_POINT('Ctrl Pts',(-3.42570626087676,6.11982499477659,
78.4360930928239));
#141548=CARTESIAN_POINT('Ctrl Pts',(-3.5749397274467,6.03137069890612,78.4439454516078));
#141549=CARTESIAN_POINT('Ctrl Pts',(-3.72413795825315,5.94293728812747,
78.4517959563582));
#141550=CARTESIAN_POINT('Ctrl Pts',(-3.8701230739579,5.84892228586717,78.4596464611085));
#141551=CARTESIAN_POINT('Ctrl Pts',(-4.01243957350114,5.74960478915742,
78.4674969658589));
#141552=CARTESIAN_POINT('Ctrl Pts',(-4.15473317880556,5.65030326950232,
78.4753462077105));
#141553=CARTESIAN_POINT('Ctrl Pts',(-4.29335903163953,5.54570117428883,
78.4831954495621));
#141554=CARTESIAN_POINT('Ctrl Pts',(-4.42789097194043,5.43612068511254,
78.4910446914137));
#141555=CARTESIAN_POINT('Ctrl Pts',(-4.56246823868513,5.3265032761247,78.4988965778285));
#141556=CARTESIAN_POINT('Ctrl Pts',(-4.69294854171612,5.21190436399478,
78.5067484642433));
#141557=CARTESIAN_POINT('Ctrl Pts',(-4.81893900703761,5.09268626649546,
78.5146003506581));
#141558=CARTESIAN_POINT('Ctrl Pts',(-4.91145223755515,5.00514590137596,
78.5203658931223));
#141559=CARTESIAN_POINT('Ctrl Pts',(-5.00154533075462,4.91511581917966,
78.5261314355865));
#141560=CARTESIAN_POINT('Ctrl Pts',(-5.08907563104056,4.822751889124,78.5318969780506));
#141561=CARTESIAN_POINT('Ctrl Pts',(-5.23565883552319,4.66807401412599,
78.5415522824106));
#141562=CARTESIAN_POINT('Ctrl Pts',(-5.37497948782232,4.50692938614718,
78.5512075867705));
#141563=CARTESIAN_POINT('Ctrl Pts',(-5.50656696612014,4.33997083056263,
78.5608628911305));
#141564=CARTESIAN_POINT('Ctrl Pts',(-5.63888341436198,4.17208735590149,
78.5705716840652));
#141565=CARTESIAN_POINT('Ctrl Pts',(-5.76338078438032,3.9983254299945,78.580280477));
#141566=CARTESIAN_POINT('Ctrl Pts',(-5.87962792320045,3.8193719440795,78.5899892699348));
#141567=CARTESIAN_POINT('Ctrl Pts',(-5.99643445312336,3.63955731879496,
78.5997447824055));
#141568=CARTESIAN_POINT('Ctrl Pts',(-6.10491115573157,3.45450109818367,
78.6095002948763));
#141569=CARTESIAN_POINT('Ctrl Pts',(-6.20466818990649,3.26492254359312,
78.6192558073471));
#141570=CARTESIAN_POINT('Ctrl Pts',(-6.30452399889252,3.0751562770675,78.629020979276));
#141571=CARTESIAN_POINT('Ctrl Pts',(-6.39564286188399,2.88085875906164,
78.638786151205));
#141572=CARTESIAN_POINT('Ctrl Pts',(-6.47768131128054,2.6827730787353,78.6485513231339));
#141573=CARTESIAN_POINT('Ctrl Pts',(-6.55960790311294,2.48495748373914,
78.6583031804725));
#141574=CARTESIAN_POINT('Ctrl Pts',(-6.63247881191435,2.28336408462234,
78.6680550378112));
#141575=CARTESIAN_POINT('Ctrl Pts',(-6.69599944080937,2.07875396600478,
78.6778068951498));
#141576=CARTESIAN_POINT('Ctrl Pts',(-6.72369903538854,1.98952913572375,
78.6820594112123));
#141577=CARTESIAN_POINT('Ctrl Pts',(-6.74962119971282,1.89973091567733,
78.6863119272747));
#141578=CARTESIAN_POINT('Ctrl Pts',(-6.7737443574246,1.80942364933102,78.6905644433372));
#141579=CARTESIAN_POINT('Ctrl Pts',(-6.81931324488843,1.63883231520851,
78.6985974889361));
#141580=CARTESIAN_POINT('Ctrl Pts',(-6.85848122771586,1.46634030115257,
78.706630534535));
#141581=CARTESIAN_POINT('Ctrl Pts',(-6.89109073719558,1.29247631089987,
78.7146635801339));
#141582=CARTESIAN_POINT('Ctrl Pts',(-6.92367928402718,1.11872408711358,
78.7226914617818));
#141583=CARTESIAN_POINT('Ctrl Pts',(-6.94971768234668,0.943602001475774,
78.7307193434298));
#141584=CARTESIAN_POINT('Ctrl Pts',(-6.96909872353735,0.767651968075435,
78.7387472250777));
#141585=CARTESIAN_POINT('Ctrl Pts',(-6.98847101399679,0.591781377850374,
78.7467714820579));
#141586=CARTESIAN_POINT('Ctrl Pts',(-7.00119189229259,0.415083947803786,
78.7547957390381));
#141587=CARTESIAN_POINT('Ctrl Pts',(-7.00720559944598,0.238109742750817,
78.7628199960183));
#141588=CARTESIAN_POINT('Ctrl Pts',(-7.01321857948092,0.061156935682018,
78.7708432827841));
#141589=CARTESIAN_POINT('Ctrl Pts',(-7.01252598353081,-0.116072213854308,
78.7788665695499));
#141590=CARTESIAN_POINT('Ctrl Pts',(-7.00512407177398,-0.293024404363847,
78.7868898563157));
#141591=CARTESIAN_POINT('Ctrl Pts',(-6.99772276653778,-0.469962095219859,
78.7949124856447));
#141592=CARTESIAN_POINT('Ctrl Pts',(-6.98361325991897,-0.646622506097364,
78.8029351149737));
#141593=CARTESIAN_POINT('Ctrl Pts',(-6.96284389521981,-0.822454529624714,
78.8109577443027));
#141594=CARTESIAN_POINT('Ctrl Pts',(-6.94206672271815,-0.998352653474978,
78.8189833895692));
#141595=CARTESIAN_POINT('Ctrl Pts',(-6.91462473672402,-1.17342140394086,
78.8270090348357));
#141596=CARTESIAN_POINT('Ctrl Pts',(-6.88061795612284,-1.34711658900777,
78.8350346801022));
#141597=CARTESIAN_POINT('Ctrl Pts',(-6.8605654860123,-1.44953785457088,
78.8397670896093));
#141598=CARTESIAN_POINT('Ctrl Pts',(-6.8382314103516,-1.55148170122819,
78.8444994991165));
#141599=CARTESIAN_POINT('Ctrl Pts',(-6.8136444928177,-1.65283855472792,
78.8492319086236));
#141600=CARTESIAN_POINT('Ctrl Pts',(-6.76828810714639,-1.83981524798053,
78.8579619574581));
#141601=CARTESIAN_POINT('Ctrl Pts',(-6.71524003955458,-2.02488717757136,
78.8666920062926));
#141602=CARTESIAN_POINT('Ctrl Pts',(-6.65468693636532,-2.20743478759142,
78.8754220551271));
#141603=CARTESIAN_POINT('Ctrl Pts',(-6.59411632417112,-2.39003518147947,
78.884154628266));
#141604=CARTESIAN_POINT('Ctrl Pts',(-6.52603643101028,-2.57010953884597,
78.8928872014049));
#141605=CARTESIAN_POINT('Ctrl Pts',(-6.45068313217834,-2.74705545825523,
78.9016197745439));
#141606=CARTESIAN_POINT('Ctrl Pts',(-6.37425931944732,-2.92651517691482,
78.9104764078244));
#141607=CARTESIAN_POINT('Ctrl Pts',(-6.29035397887403,-3.10275662457441,
78.9193330411049));
#141608=CARTESIAN_POINT('Ctrl Pts',(-6.19926304083474,-3.27517393630329,
78.9281896743854));
#141609=CARTESIAN_POINT('Ctrl Pts',(-6.1093908935877,-3.44528431567993,
78.936927806492));
#141610=CARTESIAN_POINT('Ctrl Pts',(-6.01252439060037,-3.61167202221359,
78.9456659385985));
#141611=CARTESIAN_POINT('Ctrl Pts',(-5.9089937192203,-3.77378056976225,
78.9544040707051));
#141612=CARTESIAN_POINT('Ctrl Pts',(-5.8033570188948,-3.93918674195573,
78.9633199545726));
#141613=CARTESIAN_POINT('Ctrl Pts',(-5.69078227620538,-4.10013754471713,
78.97223583844));
#141614=CARTESIAN_POINT('Ctrl Pts',(-5.57166689362883,-4.25607267195245,
78.9811517223075));
#141615=CARTESIAN_POINT('Ctrl Pts',(-5.45255151105233,-4.41200779918771,
78.990067606175));
#141616=CARTESIAN_POINT('Ctrl Pts',(-5.32689567699746,-4.56292701427,78.9989834900425));
#141617=CARTESIAN_POINT('Ctrl Pts',(-5.19514124450711,-4.70830479176116,
79.0078993739099));
#141618=CARTESIAN_POINT('Ctrl Pts',(-5.06597581991057,-4.85082585918653,
79.0166400584063));
#141619=CARTESIAN_POINT('Ctrl Pts',(-4.93093553144405,-4.98803638596009,
79.0253807429026));
#141620=CARTESIAN_POINT('Ctrl Pts',(-4.79047193705433,-5.11947313527427,
79.034121427399));
#141621=CARTESIAN_POINT('Ctrl Pts',(-4.65003361439863,-5.25088623693381,
79.042860539301));
#141622=CARTESIAN_POINT('Ctrl Pts',(-4.50417413430033,-5.37652744868928,
79.051599651203));
#141623=CARTESIAN_POINT('Ctrl Pts',(-4.35338084659093,-5.49597141250164,
79.060338763105));
#141624=CARTESIAN_POINT('Ctrl Pts',(-4.20063381481317,-5.61696294477241,
79.0691911027793));
#141625=CARTESIAN_POINT('Ctrl Pts',(-4.04282444449079,-5.7315953265149,
79.0780434424536));
#141626=CARTESIAN_POINT('Ctrl Pts',(-3.88049376689191,-5.83946869908667,
79.0868957821279));
#141627=CARTESIAN_POINT('Ctrl Pts',(-3.72032155380397,-5.94590771032999,
79.0956304147778));
#141628=CARTESIAN_POINT('Ctrl Pts',(-3.55574776548765,-6.04576619744464,
79.1043650474277));
#141629=CARTESIAN_POINT('Ctrl Pts',(-3.3873219776571,-6.13870315149554,
79.1130996800776));
#141630=CARTESIAN_POINT('Ctrl Pts',(-3.21549165655506,-6.23351871900755,
79.1220108732641));
#141631=CARTESIAN_POINT('Ctrl Pts',(-3.03965219366928,-6.32112979232783,
79.1309220664505));
#141632=CARTESIAN_POINT('Ctrl Pts',(-2.86041524350073,-6.40122263300135,
79.139833259637));
#141633=CARTESIAN_POINT('Ctrl Pts',(-2.68117829333212,-6.48131547367489,
79.1487444528235));
#141634=CARTESIAN_POINT('Ctrl Pts',(-2.49854412713904,-6.5538899457306,
79.15765564601));
#141635=CARTESIAN_POINT('Ctrl Pts',(-2.31314879546303,-6.61868334433277,
79.1665668391964));
#141636=CARTESIAN_POINT('Ctrl Pts',(-2.14617667780427,-6.67703805519365,
79.1745925040487));
#141637=CARTESIAN_POINT('Ctrl Pts',(-1.9768879904652,-6.7291076329979,79.182618168901));
#141638=CARTESIAN_POINT('Ctrl Pts',(-1.80580461755494,-6.77471004882993,
79.1906438337533));
#141639=CARTESIAN_POINT('Ctrl Pts',(-1.63477554231082,-6.82029799157374,
79.1986669514565));
#141640=CARTESIAN_POINT('Ctrl Pts',(-1.4619532692763,-6.8594227644161,79.2066900691596));
#141641=CARTESIAN_POINT('Ctrl Pts',(-1.28787484801487,-6.89195218630764,
79.2147131868628));
#141642=CARTESIAN_POINT('Ctrl Pts',(-1.11381837956589,-6.92447750595439,
79.2227352927805));
#141643=CARTESIAN_POINT('Ctrl Pts',(-0.93850643876666,-6.95040906463028,
79.2307573986983));
#141644=CARTESIAN_POINT('Ctrl Pts',(-0.762486221034689,-6.96966579724109,
79.2387795046161));
#141645=CARTESIAN_POINT('Ctrl Pts',(-0.586400593594999,-6.98892968571881,
79.2468045915755));
#141646=CARTESIAN_POINT('Ctrl Pts',(-0.409606527847007,-7.00151375021534,
79.254829678535));
#141647=CARTESIAN_POINT('Ctrl Pts',(-0.232656750421843,-7.00738877178819,
79.2628547654944));
#141648=CARTESIAN_POINT('Ctrl Pts',(-0.0556721236238324,-7.01326495041713,
79.2708814329546));
#141649=CARTESIAN_POINT('Ctrl Pts',(0.12146790929119,-7.01242945049088,
79.2789081004147));
#141650=CARTESIAN_POINT('Ctrl Pts',(0.29821087019992,-7.00490519845876,
79.2869347678748));
#141651=CARTESIAN_POINT('Ctrl Pts',(0.475095719735005,-6.99737490598362,
79.2949678791153));
#141652=CARTESIAN_POINT('Ctrl Pts',(0.651582494832487,-6.98314516162781,
79.3030009903559));
#141653=CARTESIAN_POINT('Ctrl Pts',(0.827123457383149,-6.96229081184825,
79.3110341015964));
#141654=CARTESIAN_POINT('Ctrl Pts',(0.930558569403216,-6.95000267138114,
79.3157675025585));
#141655=CARTESIAN_POINT('Ctrl Pts',(1.03366543804422,-6.93541544974835,
79.3205009035206));
#141656=CARTESIAN_POINT('Ctrl Pts',(1.1363337643828,-6.91855274883582,79.3252343044827));
#141657=CARTESIAN_POINT('Ctrl Pts',(1.34783371186954,-6.88381506015738,
79.334985257777));
#141658=CARTESIAN_POINT('Ctrl Pts',(1.55759675624886,-6.83939833325074,
79.3447362110712));
#141659=CARTESIAN_POINT('Ctrl Pts',(1.7648298584535,-6.7854994019019,79.3544871643655));
#141660=CARTESIAN_POINT('Ctrl Pts',(1.97236151882041,-6.73152281903059,
79.3642521657373));
#141661=CARTESIAN_POINT('Ctrl Pts',(2.17735590883776,-6.66803671563266,
79.3740171671091));
#141662=CARTESIAN_POINT('Ctrl Pts',(2.3790326926166,-6.59528847056453,79.3837821684809));
#141663=CARTESIAN_POINT('Ctrl Pts',(2.58037332298278,-6.52266148174805,
79.3935308936186));
#141664=CARTESIAN_POINT('Ctrl Pts',(2.77840736319922,-6.44080321855899,
79.4032796187564));
#141665=CARTESIAN_POINT('Ctrl Pts',(2.97237492974255,-6.35000896373682,
79.4130283438942));
#141666=CARTESIAN_POINT('Ctrl Pts',(3.16581013052874,-6.25946390393769,
79.4227503125616));
#141667=CARTESIAN_POINT('Ctrl Pts',(3.35520110237369,-6.16003183124972,
79.432472281229));
#141668=CARTESIAN_POINT('Ctrl Pts',(3.53981127429961,-6.05205442018175,
79.4421942498964));
#141669=CARTESIAN_POINT('Ctrl Pts',(3.72319992893165,-5.94479146744286,
79.4518518908362));
#141670=CARTESIAN_POINT('Ctrl Pts',(3.90187078627441,-5.82909588572984,
79.461509531776));
#141671=CARTESIAN_POINT('Ctrl Pts',(4.0751194034755,-5.70535085774026,79.4711671727158));
#141672=CARTESIAN_POINT('Ctrl Pts',(4.15126813530641,-5.65096065766813,
79.4754120384003));
#141673=CARTESIAN_POINT('Ctrl Pts',(4.2263695763594,-5.59501601050443,79.4796569040848));
#141674=CARTESIAN_POINT('Ctrl Pts',(4.30036504556434,-5.53755244105087,
79.4839017697693));
#141675=CARTESIAN_POINT('Ctrl Pts',(4.43723653858589,-5.43126046628587,
79.4917536167832));
#141676=CARTESIAN_POINT('Ctrl Pts',(4.57026540768275,-5.31981216424357,
79.499605463797));
#141677=CARTESIAN_POINT('Ctrl Pts',(4.69902863801117,-5.20353307106344,
79.5074573108108));
#141678=CARTESIAN_POINT('Ctrl Pts',(4.82775535212855,-5.08728695369399,
79.5153069311043));
#141679=CARTESIAN_POINT('Ctrl Pts',(4.95221855094749,-4.96621302570767,
79.5231565513978));
#141680=CARTESIAN_POINT('Ctrl Pts',(5.07202870601448,-4.8406767468883,79.5310061716913));
#141681=CARTESIAN_POINT('Ctrl Pts',(5.19182929577332,-4.71515049053481,
79.538855165293));
#141682=CARTESIAN_POINT('Ctrl Pts',(5.30697731848026,-4.5851628690408,79.5467041588948));
#141683=CARTESIAN_POINT('Ctrl Pts',(5.41712068376836,-4.45111559723954,
79.5545531524965));
#141684=CARTESIAN_POINT('Ctrl Pts',(5.52731981141706,-4.31700046122976,
79.5624061198139));
#141685=CARTESIAN_POINT('Ctrl Pts',(5.63250897667486,-4.17882186347203,
79.5702590871312));
#141686=CARTESIAN_POINT('Ctrl Pts',(5.73237671782133,-4.03701420947214,
79.5781120544486));
#141687=CARTESIAN_POINT('Ctrl Pts',(5.83226982201799,-3.8951705410936,79.5859670161557));
#141688=CARTESIAN_POINT('Ctrl Pts',(5.92683860173875,-3.74969630017751,
79.5938219778629));
#141689=CARTESIAN_POINT('Ctrl Pts',(6.01581578436125,-3.60105359736982,
79.6016769395701));
#141690=CARTESIAN_POINT('Ctrl Pts',(6.10488128427494,-3.45226335425481,
79.6095396979833));
#141691=CARTESIAN_POINT('Ctrl Pts',(6.18834391851647,-3.3002987021646,79.6174024563965));
#141692=CARTESIAN_POINT('Ctrl Pts',(6.26598283969305,-3.14564550055665,
79.6252652148098));
#141693=CARTESIAN_POINT('Ctrl Pts',(6.3229376382212,-3.032194130988,79.6310332215584));
#141694=CARTESIAN_POINT('Ctrl Pts',(6.37675939458197,-2.91729641314543,
79.636801228307));
#141695=CARTESIAN_POINT('Ctrl Pts',(6.42737773349409,-2.80115012690938,
79.6425692350556));
#141696=CARTESIAN_POINT('Ctrl Pts',(6.5095962779528,-2.61249560359139,79.651938114586));
#141697=CARTESIAN_POINT('Ctrl Pts',(6.58350384587159,-2.42022175213591,
79.6613069941165));
#141698=CARTESIAN_POINT('Ctrl Pts',(6.64882690551553,-2.22502299830648,
79.6706758736469));
#141699=CARTESIAN_POINT('Ctrl Pts',(6.71403384970503,-2.03017122136595,
79.680028099461));
#141700=CARTESIAN_POINT('Ctrl Pts',(6.77068672594478,-1.83240506785728,
79.6893803252751));
#141701=CARTESIAN_POINT('Ctrl Pts',(6.81856188813345,-1.63243387008294,
79.6987325510892));
#141702=CARTESIAN_POINT('Ctrl Pts',(6.86635127364715,-1.43282095546948,
79.7080680207652));
#141703=CARTESIAN_POINT('Ctrl Pts',(6.90539431044331,-1.23101102657837,
79.7174034904411));
#141704=CARTESIAN_POINT('Ctrl Pts',(6.93551768568856,-1.02772612791602,
79.726738960117));
#141705=CARTESIAN_POINT('Ctrl Pts',(6.96552096875996,-0.825251660528144,
79.7360372122886));
#141706=CARTESIAN_POINT('Ctrl Pts',(6.98667551784331,-0.621314102134208,
79.7453354644603));
#141707=CARTESIAN_POINT('Ctrl Pts',(6.99885966834505,-0.416641218931813,
79.7546337166319));
#141708=CARTESIAN_POINT('Ctrl Pts',(7.00711527886316,-0.277961086320631,
79.7609339300458));
#141709=CARTESIAN_POINT('Ctrl Pts',(7.01125359746706,-0.138943660978469,
79.7672341434597));
#141710=CARTESIAN_POINT('Ctrl Pts',(7.01124999765299,0.000181413712756845,
79.7735343568736));
#141711=CARTESIAN_POINT('Ctrl Pts',(7.01124999765297,0.000181414525455699,
79.7735343569104));
#141712=CARTESIAN_POINT('Ctrl Pts',(7.0112451663169,0.186901331078262,79.7819898802984));
#141713=CARTESIAN_POINT('Ctrl Pts',(7.00377706110129,0.373576221296077,
79.7904454036863));
#141714=CARTESIAN_POINT('Ctrl Pts',(6.98888240313398,0.559597460380375,
79.7989009270743));
#141715=CARTESIAN_POINT('Ctrl Pts',(6.97397616886368,0.745763277355162,
79.8073630221943));
#141716=CARTESIAN_POINT('Ctrl Pts',(6.95163187211473,0.93127411459491,79.8158251173143));
#141717=CARTESIAN_POINT('Ctrl Pts',(6.92193813567668,1.11552633692123,79.8242872124343));
#141718=CARTESIAN_POINT('Ctrl Pts',(6.89223239538575,1.29985304420077,79.8327527284018));
#141719=CARTESIAN_POINT('Ctrl Pts',(6.85517134370744,1.48291981239697,79.8412182443693));
#141720=CARTESIAN_POINT('Ctrl Pts',(6.81089471507894,1.66413333077905,79.8496837603369));
#141721=CARTESIAN_POINT('Ctrl Pts',(6.76657913587012,1.84550626445363,79.858156723501));
#141722=CARTESIAN_POINT('Ctrl Pts',(6.71503537560351,2.02502238667251,79.8666296866652));
#141723=CARTESIAN_POINT('Ctrl Pts',(6.65645336339179,2.20210244618414,79.8751026498293));
#141724=CARTESIAN_POINT('Ctrl Pts',(6.62948841720056,2.28361132742592,79.8790027035689));
#141725=CARTESIAN_POINT('Ctrl Pts',(6.60103295687948,2.36460432385478,79.8829027573086));
#141726=CARTESIAN_POINT('Ctrl Pts',(6.57110895151811,2.44502632087645,79.8868028110482));
#141727=CARTESIAN_POINT('',(7.01125,-8.5868812060852E-16,79.2264656430895));
#141728=CARTESIAN_POINT('Ctrl Pts',(6.57110895151812,2.44502632087642,79.3399816340719));
#141729=CARTESIAN_POINT('Ctrl Pts',(6.58708418927795,2.40209221135377,79.3378986371194));
#141730=CARTESIAN_POINT('Ctrl Pts',(6.60263458483066,2.35901238930181,79.3358156401668));
#141731=CARTESIAN_POINT('Ctrl Pts',(6.6177575476705,2.31579610560822,79.3337326432143));
#141732=CARTESIAN_POINT('Ctrl Pts',(6.69106165165094,2.10631791095325,79.3236359295732));
#141733=CARTESIAN_POINT('Ctrl Pts',(6.75435454450706,1.89353185207257,79.3135392159322));
#141734=CARTESIAN_POINT('Ctrl Pts',(6.80741833042684,1.67829742211227,79.3034425022911));
#141735=CARTESIAN_POINT('Ctrl Pts',(6.86056137941765,1.46274148961281,79.2933307068665));
#141736=CARTESIAN_POINT('Ctrl Pts',(6.90344478033023,1.24472979699255,79.283218911442));
#141737=CARTESIAN_POINT('Ctrl Pts',(6.9359012343375,1.02513444484885,79.2731071160174));
#141738=CARTESIAN_POINT('Ctrl Pts',(6.96825526148659,0.806232096998995,
79.26302723164));
#141739=CARTESIAN_POINT('Ctrl Pts',(6.99024806641698,0.585755995141008,
79.2529473472627));
#141740=CARTESIAN_POINT('Ctrl Pts',(7.00176464561119,0.364579771749844,
79.2428674628853));
#141741=CARTESIAN_POINT('Ctrl Pts',(7.00801117416039,0.244615017414701,
79.2374001896201));
#141742=CARTESIAN_POINT('Ctrl Pts',(7.01117655918056,0.12444446885573,79.2319329163549));
#141743=CARTESIAN_POINT('Ctrl Pts',(7.01124873670978,0.00420885798236834,
79.2264656430896));
#141744=CARTESIAN_POINT('Ctrl Pts',(7.01125,-8.58630487052188E-16,79.2264656430895));
#141745=CARTESIAN_POINT('Ctrl Pts',(7.01125,-0.191009525814093,79.2177938341507));
#141746=CARTESIAN_POINT('Ctrl Pts',(7.00344006572044,-0.382018909627989,
79.209122025212));
#141747=CARTESIAN_POINT('Ctrl Pts',(6.98784625534326,-0.572390840409932,
79.2004502162732));
#141748=CARTESIAN_POINT('Ctrl Pts',(6.9722524678609,-0.762762491687932,
79.1917784200664));
#141749=CARTESIAN_POINT('Ctrl Pts',(6.94887485033552,-0.952496408755896,
79.1831066238596));
#141750=CARTESIAN_POINT('Ctrl Pts',(6.91779140296556,-1.14095953808881,
79.1744348276528));
#141751=CARTESIAN_POINT('Ctrl Pts',(6.88670800059848,-1.32942239456319,
79.165763044001));
#141752=CARTESIAN_POINT('Ctrl Pts',(6.8479188369279,-1.51661418677304,79.1570912603493));
#141753=CARTESIAN_POINT('Ctrl Pts',(6.8015533329142,-1.70191034488418,79.1484194766976));
#141754=CARTESIAN_POINT('Ctrl Pts',(6.75518789508329,-1.88720623850088,
79.1397477054241));
#141755=CARTESIAN_POINT('Ctrl Pts',(6.70124620748731,-2.07060622793265,
79.1310759341506));
#141756=CARTESIAN_POINT('Ctrl Pts',(6.63990824732713,-2.25149839652999,
79.1224041628771));
#141757=CARTESIAN_POINT('Ctrl Pts',(6.57857037347114,-2.43239031060713,
79.1137324038051));
#141758=CARTESIAN_POINT('Ctrl Pts',(6.50983633907366,-2.61077414195939,
79.105060644733));
#141759=CARTESIAN_POINT('Ctrl Pts',(6.43393547556444,-2.7860547120926,79.0963888856609));
#141760=CARTESIAN_POINT('Ctrl Pts',(6.35803471730222,-2.96133503917517,
79.0877171386134));
#141761=CARTESIAN_POINT('Ctrl Pts',(6.27496726266411,-3.13351185304295,
79.079045391566));
#141762=CARTESIAN_POINT('Ctrl Pts',(6.18501026583621,-3.30201068653642,
79.0703736445185));
#141763=CARTESIAN_POINT('Ctrl Pts',(6.09151188669053,-3.47714289831664,
79.0613605124455));
#141764=CARTESIAN_POINT('Ctrl Pts',(5.99057066119403,-3.64830137930616,
79.0523473803725));
#141765=CARTESIAN_POINT('Ctrl Pts',(5.88255038916835,-3.8148692613765,79.0433342482995));
#141766=CARTESIAN_POINT('Ctrl Pts',(5.77621793389306,-3.97883452028952,
79.0344619464151));
#141767=CARTESIAN_POINT('Ctrl Pts',(5.66302622906641,-4.13835132493379,
79.0255896445307));
#141768=CARTESIAN_POINT('Ctrl Pts',(5.54337059053176,-4.29286257158642,
79.0167173426464));
#141769=CARTESIAN_POINT('Ctrl Pts',(5.42558457134922,-4.44495958001011,
79.0079836704789));
#141770=CARTESIAN_POINT('Ctrl Pts',(5.30153533575225,-4.59220608123771,
78.9992499983115));
#141771=CARTESIAN_POINT('Ctrl Pts',(5.17164269972606,-4.73410375349655,
78.9905163261441));
#141772=CARTESIAN_POINT('Ctrl Pts',(5.04265587431879,-4.8750118976169,78.9818435585301));
#141773=CARTESIAN_POINT('Ctrl Pts',(4.90790710164428,-5.01064538261667,
78.9731707909161));
#141774=CARTESIAN_POINT('Ctrl Pts',(4.76784607609543,-5.14055156157016,
78.9644980233021));
#141775=CARTESIAN_POINT('Ctrl Pts',(4.62778576967683,-5.27045707353252,
78.9558253002177));
#141776=CARTESIAN_POINT('Ctrl Pts',(4.48241347330112,-5.39463514506226,
78.9471525771332));
#141777=CARTESIAN_POINT('Ctrl Pts',(4.33221433005818,-5.512671363408,78.9384798540487));
#141778=CARTESIAN_POINT('Ctrl Pts',(4.18201594573821,-5.6307069853429,78.9298071747856));
#141779=CARTESIAN_POINT('Ctrl Pts',(4.0269909867681,-5.74260064062323,78.9211344955224));
#141780=CARTESIAN_POINT('Ctrl Pts',(3.86765680432281,-5.84797891638432,
78.9124618162593));
#141781=CARTESIAN_POINT('Ctrl Pts',(3.70832341395226,-5.95335666829377,
78.9037891801094));
#141782=CARTESIAN_POINT('Ctrl Pts',(3.5446810799691,-6.05221894875703,78.8951165439595));
#141783=CARTESIAN_POINT('Ctrl Pts',(3.37727590613261,-6.14423583664854,
78.8864439078096));
#141784=CARTESIAN_POINT('Ctrl Pts',(3.20987155082895,-6.23625227462061,
78.8777713140648));
#141785=CARTESIAN_POINT('Ctrl Pts',(3.0387046414846,-6.32142325013534,78.86909872032));
#141786=CARTESIAN_POINT('Ctrl Pts',(2.86434638713337,-6.39946453517918,
78.8604261265752));
#141787=CARTESIAN_POINT('Ctrl Pts',(2.68998897108135,-6.47750544500735,
78.8517535745275));
#141788=CARTESIAN_POINT('Ctrl Pts',(2.51244050005896,-6.54841661688554,
78.8430810224798));
#141789=CARTESIAN_POINT('Ctrl Pts',(2.33229347361379,-6.61196141212564,
78.8344084704321));
#141790=CARTESIAN_POINT('Ctrl Pts',(2.15214729859692,-6.67550590703419,
78.8257359593735));
#141791=CARTESIAN_POINT('Ctrl Pts',(1.96940286067094,-6.73168400046285,
78.8170634483148));
#141792=CARTESIAN_POINT('Ctrl Pts',(1.7846699931603,-6.78030822146112,78.8083909372561));
#141793=CARTESIAN_POINT('Ctrl Pts',(1.59993798367519,-6.82893221661531,
78.7997184664786));
#141794=CARTESIAN_POINT('Ctrl Pts',(1.4132178378394,-6.87000233723,78.791045995701));
#141795=CARTESIAN_POINT('Ctrl Pts',(1.22513265046155,-6.90338153018309,
78.7823735249234));
#141796=CARTESIAN_POINT('Ctrl Pts',(1.03704832133025,-6.93676057082447,
78.7737010937189));
#141797=CARTESIAN_POINT('Ctrl Pts',(0.847599242854621,-6.96244870438779,
78.7650286625144));
#141798=CARTESIAN_POINT('Ctrl Pts',(0.657417610669254,-6.98036020902087,
78.75635623131));
#141799=CARTESIAN_POINT('Ctrl Pts',(0.467236830776379,-6.99827163338416,
78.7476838389707));
#141800=CARTESIAN_POINT('Ctrl Pts',(0.276323786589392,-7.00840647191844,
78.7390114466314));
#141801=CARTESIAN_POINT('Ctrl Pts',(0.0853155533234384,-7.01073090475317,
78.7303390542921));
#141802=CARTESIAN_POINT('Ctrl Pts',(-0.105691839532995,-7.01305532736071,
78.7216667001102));
#141803=CARTESIAN_POINT('Ctrl Pts',(-0.296794136559777,-7.00756940957919,
78.7129943459282));
#141804=CARTESIAN_POINT('Ctrl Pts',(-0.487353636612654,-6.99429145770895,
78.7043219917463));
#141805=CARTESIAN_POINT('Ctrl Pts',(-0.677912313780389,-6.98101356317634,
78.6956496750138));
#141806=CARTESIAN_POINT('Ctrl Pts',(-0.867927915266441,-6.95994372163514,
78.6869773582813));
#141807=CARTESIAN_POINT('Ctrl Pts',(-1.05676637165921,-6.93115224174381,
78.6783050415488));
#141808=CARTESIAN_POINT('Ctrl Pts',(-1.245604028008,-6.90236088383214,78.669632761558));
#141809=CARTESIAN_POINT('Ctrl Pts',(-1.4332642684094,-6.86584799585212,
78.6609604815671));
#141810=CARTESIAN_POINT('Ctrl Pts',(-1.61912088843568,-6.82173541784869,
78.6522882015763));
#141811=CARTESIAN_POINT('Ctrl Pts',(-1.80497673621616,-6.77762302313577,
78.6436159576193));
#141812=CARTESIAN_POINT('Ctrl Pts',(-1.98902870222326,-6.72591106719035,
78.6349437136623));
#141813=CARTESIAN_POINT('Ctrl Pts',(-2.17066262759744,-6.6667721064734,
78.6262714697053));
#141814=CARTESIAN_POINT('Ctrl Pts',(-2.35229581309165,-6.60763338665712,
78.6175992610744));
#141815=CARTESIAN_POINT('Ctrl Pts',(-2.53151070755275,-6.54106781055663,
78.6089270524435));
#141816=CARTESIAN_POINT('Ctrl Pts',(-2.70770929770338,-6.46729749753564,
78.6002548438127));
#141817=CARTESIAN_POINT('Ctrl Pts',(-2.88390718449131,-6.39352747899649,
78.5915826698002));
#141818=CARTESIAN_POINT('Ctrl Pts',(-3.05708852903999,-6.31255289079275,
78.5829104957876));
#141819=CARTESIAN_POINT('Ctrl Pts',(-3.22667545573402,-6.22464393084967,
78.5742383217751));
#141820=CARTESIAN_POINT('Ctrl Pts',(-3.39626171929477,-6.13673531465571,
78.5655661816733));
#141821=CARTESIAN_POINT('Ctrl Pts',(-3.56225334093939,-6.04189251170987,
78.5568940415715));
#141822=CARTESIAN_POINT('Ctrl Pts',(-3.72409644021767,-5.94043199325252,
78.5482219014696));
#141823=CARTESIAN_POINT('Ctrl Pts',(-3.88593891984732,-5.83897186325703,
78.5395497945708));
#141824=CARTESIAN_POINT('Ctrl Pts',(-4.04363266822696,-5.73089421932905,
78.530877687672));
#141825=CARTESIAN_POINT('Ctrl Pts',(-4.19665149725545,-5.6165596919363,
78.5222055807732));
#141826=CARTESIAN_POINT('Ctrl Pts',(-4.34966975290526,-5.50222559296783,
78.5135335063697));
#141827=CARTESIAN_POINT('Ctrl Pts',(-4.49801289671559,-5.38163482746919,
78.5048614319663));
#141828=CARTESIAN_POINT('Ctrl Pts',(-4.64118594512765,-5.2551897763306,
78.4961893575628));
#141829=CARTESIAN_POINT('Ctrl Pts',(-4.78435846873431,-5.12874518868039,
78.4875173149472));
#141830=CARTESIAN_POINT('Ctrl Pts',(-4.9223607219674,-4.99644654635617,
78.4788452723314));
#141831=CARTESIAN_POINT('Ctrl Pts',(-5.05473222957746,-4.85873529323948,
78.4701732297158));
#141832=CARTESIAN_POINT('Ctrl Pts',(-5.18710326277472,-4.72102453367296,
78.4615012181802));
#141833=CARTESIAN_POINT('Ctrl Pts',(-5.31384339389808,-4.57790140690643,
78.4528292066447));
#141834=CARTESIAN_POINT('Ctrl Pts',(-5.43452972930466,-4.4298434717046,
78.4441571951092));
#141835=CARTESIAN_POINT('Ctrl Pts',(-5.55521564202289,-4.28178605505662,
78.4354852139463));
#141836=CARTESIAN_POINT('Ctrl Pts',(-5.66984762199742,-4.1287940847157,
78.4268132327833));
#141837=CARTESIAN_POINT('Ctrl Pts',(-5.77804317951531,-3.97137804523274,
78.4181412516204));
#141838=CARTESIAN_POINT('Ctrl Pts',(-5.88623836691802,-3.81396254423831,
78.4094693001226));
#141839=CARTESIAN_POINT('Ctrl Pts',(-5.98799701504367,-3.65212323845438,
78.4007973486247));
#141840=CARTESIAN_POINT('Ctrl Pts',(-6.08297959063027,-3.486400129428,78.3921253971269));
#141841=CARTESIAN_POINT('Ctrl Pts',(-6.17796184904904,-3.32067757378774,
78.3834534745867));
#141842=CARTESIAN_POINT('Ctrl Pts',(-6.26616793897602,-3.15107148727402,
78.3747815520464));
#141843=CARTESIAN_POINT('Ctrl Pts',(-6.34730354929188,-2.97814778270769,
78.3661096295061));
#141844=CARTESIAN_POINT('Ctrl Pts',(-6.42843889529631,-2.80522464146629,
78.357437735216));
#141845=CARTESIAN_POINT('Ctrl Pts',(-6.50250368714091,-2.62898416091975,
78.3487658409258));
#141846=CARTESIAN_POINT('Ctrl Pts',(-6.56925079959966,-2.45001438658209,
78.3400939466356));
#141847=CARTESIAN_POINT('Ctrl Pts',(-6.63599770006415,-2.27104518066701,
78.3314220798881));
#141848=CARTESIAN_POINT('Ctrl Pts',(-6.69542686840661,-2.08934696441408,
78.3227502131406));
#141849=CARTESIAN_POINT('Ctrl Pts',(-6.7473400140075,-1.90552598981838,
78.314078346393));
#141850=CARTESIAN_POINT('Ctrl Pts',(-6.79925299896266,-1.72170558405843,
78.3054065064807));
#141851=CARTESIAN_POINT('Ctrl Pts',(-6.84364993053112,-1.53576270641729,
78.2967346665683));
#141852=CARTESIAN_POINT('Ctrl Pts',(-6.88038267538234,-1.34831776773821,
78.288062826656));
#141853=CARTESIAN_POINT('Ctrl Pts',(-6.91711530955977,-1.16087339382071,
78.2793910128714));
#141854=CARTESIAN_POINT('Ctrl Pts',(-6.94618374861324,-0.971927246623025,
78.2707191990868));
#141855=CARTESIAN_POINT('Ctrl Pts',(-6.96749100433623,-0.78210975380297,
78.2620473853023));
#141856=CARTESIAN_POINT('Ctrl Pts',(-6.98879819759952,-0.592292817410386,
78.2533755969381));
#141857=CARTESIAN_POINT('Ctrl Pts',(-7.00234422137931,-0.401604822732526,
78.2447038085739));
#141858=CARTESIAN_POINT('Ctrl Pts',(-7.00808387899837,-0.21068200545643,
78.2360320202097));
#141859=CARTESIAN_POINT('Ctrl Pts',(-7.01382352026046,-0.0197597322755547,
78.2273602565586));
#141860=CARTESIAN_POINT('Ctrl Pts',(-7.01175683134613,0.171397078298468,
78.2186884929074));
#141861=CARTESIAN_POINT('Ctrl Pts',(-7.00189070777997,0.362150629993181,
78.2100167292563));
#141862=CARTESIAN_POINT('Ctrl Pts',(-6.99157808297303,0.561536923508558,
78.2009525163109));
#141863=CARTESIAN_POINT('Ctrl Pts',(-6.97274368607599,0.760482277939237,
78.1918883033655));
#141864=CARTESIAN_POINT('Ctrl Pts',(-6.94545616842894,0.95826153785511,
78.1828240904202));
#141865=CARTESIAN_POINT('Ctrl Pts',(-6.91902138570836,1.1498601958986,78.1740431341294));
#141866=CARTESIAN_POINT('Ctrl Pts',(-6.88465388689399,1.3403642279907,78.1652621778385));
#141867=CARTESIAN_POINT('Ctrl Pts',(-6.84247124235356,1.5291219245255,78.1564812215477));
#141868=CARTESIAN_POINT('Ctrl Pts',(-6.80080846652437,1.7155533273558,78.1478084838022));
#141869=CARTESIAN_POINT('Ctrl Pts',(-6.75152215882668,1.90028091508163,
78.1391357460567));
#141870=CARTESIAN_POINT('Ctrl Pts',(-6.69477680034086,2.08268820424897,
78.1304630083112));
#141871=CARTESIAN_POINT('Ctrl Pts',(-6.63803201373298,2.26509365512142,
78.1217903579693));
#141872=CARTESIAN_POINT('Ctrl Pts',(-6.57382841116829,2.44517858291205,
78.1131177076274));
#141873=CARTESIAN_POINT('Ctrl Pts',(-6.50238025226108,2.62234201001799,
78.1044450572855));
#141874=CARTESIAN_POINT('Ctrl Pts',(-6.43093279007886,2.79950370951906,
78.0957724915147));
#141875=CARTESIAN_POINT('Ctrl Pts',(-6.35224101919167,2.97374370183801,
78.087099925744));
#141876=CARTESIAN_POINT('Ctrl Pts',(-6.26656754386633,3.14448052636062,
78.0784273599732));
#141877=CARTESIAN_POINT('Ctrl Pts',(-6.18089487601409,3.31521574168748,
78.0697548759414));
#141878=CARTESIAN_POINT('Ctrl Pts',(-6.08824076282435,3.48244760135076,
78.0610823919096));
#141879=CARTESIAN_POINT('Ctrl Pts',(-5.98891439682134,3.64561804225924,
78.0524099078778));
#141880=CARTESIAN_POINT('Ctrl Pts',(-5.88958893454527,3.80878699855161,
78.0437375027532));
#141881=CARTESIAN_POINT('Ctrl Pts',(-5.78359148866223,3.96789436736006,
78.0350650976285));
#141882=CARTESIAN_POINT('Ctrl Pts',(-5.67127577279528,4.1224092071755,78.0263926925039));
#141883=CARTESIAN_POINT('Ctrl Pts',(-5.55896104217726,4.27692269156547,
78.0177203634547));
#141884=CARTESIAN_POINT('Ctrl Pts',(-5.44032831952208,4.42684349778465,
78.0090480344056));
#141885=CARTESIAN_POINT('Ctrl Pts',(-5.31577347545041,4.57167134866428,
78.0003757053565));
#141886=CARTESIAN_POINT('Ctrl Pts',(-5.19121968333579,4.71649797636645,
77.9917034495515));
#141887=CARTESIAN_POINT('Ctrl Pts',(-5.06074405512509,4.85623151942303,
77.9830311937466));
#141888=CARTESIAN_POINT('Ctrl Pts',(-4.92478197319156,4.99040570284897,
77.9743589379416));
#141889=CARTESIAN_POINT('Ctrl Pts',(-4.78882099518222,5.12457879686728,
77.9656867525498));
#141890=CARTESIAN_POINT('Ctrl Pts',(-4.64737385478172,5.25319242205071,
77.9570145671579));
#141891=CARTESIAN_POINT('Ctrl Pts',(-4.50091253739826,5.3758174162811,77.9483423817661));
#141892=CARTESIAN_POINT('Ctrl Pts',(-4.35445236138621,5.49844145489627,
77.9396702639565));
#141893=CARTESIAN_POINT('Ctrl Pts',(-4.20297830438142,5.61507677359828,
77.9309981461469));
#141894=CARTESIAN_POINT('Ctrl Pts',(-4.04699580206287,5.72533418593059,
77.9223260283373));
#141895=CARTESIAN_POINT('Ctrl Pts',(-3.89101446441063,5.83559077500971,
77.9136539752794));
#141896=CARTESIAN_POINT('Ctrl Pts',(-3.73052498075555,5.93946938906078,
77.9049819222214));
#141897=CARTESIAN_POINT('Ctrl Pts',(-3.56606286128741,6.0366234131215,77.8963098691635));
#141898=CARTESIAN_POINT('Ctrl Pts',(-3.40160191613153,6.13377674347135,
77.8876378780268));
#141899=CARTESIAN_POINT('Ctrl Pts',(-3.23316863647579,6.22420543545029,
77.8789658868901));
#141900=CARTESIAN_POINT('Ctrl Pts',(-3.06132503080019,6.30760775716882,
77.8702938957534));
#141901=CARTESIAN_POINT('Ctrl Pts',(-2.8894825960697,6.39100951058258,77.8616219637077));
#141902=CARTESIAN_POINT('Ctrl Pts',(-2.71423013734018,6.46738486553112,
77.8529500316621));
#141903=CARTESIAN_POINT('Ctrl Pts',(-2.53615240857015,6.53647898512677,
77.8442780996165));
#141904=CARTESIAN_POINT('Ctrl Pts',(-2.35807583511879,6.60557265645903,
77.8356062238319));
#141905=CARTESIAN_POINT('Ctrl Pts',(-2.17717429308822,6.66738508423251,
77.8269343480474));
#141906=CARTESIAN_POINT('Ctrl Pts',(-1.99405137755703,6.72171002544464,
77.8182624722629));
#141907=CARTESIAN_POINT('Ctrl Pts',(-1.81092959032806,6.77603463193649,
77.8095906499096));
#141908=CARTESIAN_POINT('Ctrl Pts',(-1.62558672926414,6.82287176341229,
77.8009188275564));
#141909=CARTESIAN_POINT('Ctrl Pts',(-1.43864120071127,6.8620651452836,77.7922470052032));
#141910=CARTESIAN_POINT('Ctrl Pts',(-1.25169676302043,6.90125829845422,
77.7835752334516));
#141911=CARTESIAN_POINT('Ctrl Pts',(-1.06314995450863,6.93280773300164,
77.7749034617001));
#141912=CARTESIAN_POINT('Ctrl Pts',(-0.873629864329032,6.95660818378126,
77.7662316899485));
#141913=CARTESIAN_POINT('Ctrl Pts',(-0.679495509716173,6.98098810649668,
77.7573487857101));
#141914=CARTESIAN_POINT('Ctrl Pts',(-0.484340182091174,6.99723686027452,
77.7484658814716));
#141915=CARTESIAN_POINT('Ctrl Pts',(-0.288847078975853,7.00529756166482,
77.7395829772331));
#141916=CARTESIAN_POINT('Ctrl Pts',(-0.0979805524013863,7.01316749698021,
77.7309102974768));
#141917=CARTESIAN_POINT('Ctrl Pts',(0.0932076478821179,7.01323255451612,
77.7222376177204));
#141918=CARTESIAN_POINT('Ctrl Pts',(0.28407948621932,7.00549251716176,77.7135649379641));
#141919=CARTESIAN_POINT('Ctrl Pts',(0.474947621910944,6.99775262995324,
77.7048924264455));
#141920=CARTESIAN_POINT('Ctrl Pts',(0.665499124046535,6.98220796234756,
77.696219914927));
#141921=CARTESIAN_POINT('Ctrl Pts',(0.855098106414399,6.95891038819344,
77.6875474034084));
#141922=CARTESIAN_POINT('Ctrl Pts',(1.04469365841084,6.93561323555704,77.6788750487997));
#141923=CARTESIAN_POINT('Ctrl Pts',(1.2333364431492,6.90456349171748,77.6702026941909));
#141924=CARTESIAN_POINT('Ctrl Pts',(1.4203969667229,6.86586476850691,77.6615303395822));
#141925=CARTESIAN_POINT('Ctrl Pts',(1.60745435008764,6.82716669493675,77.6528581305574));
#141926=CARTESIAN_POINT('Ctrl Pts',(1.79292924725751,6.78081995649478,77.6441859215326));
#141927=CARTESIAN_POINT('Ctrl Pts',(1.97620275620699,6.72697920532388,77.6355137125077));
#141928=CARTESIAN_POINT('Ctrl Pts',(2.15947342778097,6.6731392876964,77.626841637743));
#141929=CARTESIAN_POINT('Ctrl Pts',(2.34054250680043,6.61180566956937,77.6181695629782));
#141930=CARTESIAN_POINT('Ctrl Pts',(2.51880581148603,6.54318300573385,77.6094974882134));
#141931=CARTESIAN_POINT('Ctrl Pts',(2.69706658905484,6.47456131471483,77.6008255363868));
#141932=CARTESIAN_POINT('Ctrl Pts',(2.87252140681634,6.39865088680259,77.5921535845601));
#141933=CARTESIAN_POINT('Ctrl Pts',(3.04458483294514,6.31570500874609,77.5834816327334));
#141934=CARTESIAN_POINT('Ctrl Pts',(3.21664604442449,6.23276019829615,77.5748097925244));
#141935=CARTESIAN_POINT('Ctrl Pts',(3.38531569578518,6.14278024223941,77.5661379523155));
#141936=CARTESIAN_POINT('Ctrl Pts',(3.55003100941986,6.04606536473576,77.5574661121066));
#141937=CARTESIAN_POINT('Ctrl Pts',(3.72225670715806,5.94494066119623,77.548398869373));
#141938=CARTESIAN_POINT('Ctrl Pts',(3.89015872998388,5.83645264819801,77.5393316266395));
#141939=CARTESIAN_POINT('Ctrl Pts',(4.05312466659611,5.72099702844969,77.5302643839059));
#141940=CARTESIAN_POINT('Ctrl Pts',(4.20899688867782,5.6105670553148,77.5215918275275));
#141941=CARTESIAN_POINT('Ctrl Pts',(4.36035338103661,5.4937633625381,77.5129192711491));
#141942=CARTESIAN_POINT('Ctrl Pts',(4.50668904924836,5.37097573778591,77.5042467147706));
#141943=CARTESIAN_POINT('Ctrl Pts',(4.65301950883883,5.24819248349408,77.4955744670802));
#141944=CARTESIAN_POINT('Ctrl Pts',(4.794329284268,5.11942590604149,77.4869022193897));
#141945=CARTESIAN_POINT('Ctrl Pts',(4.93014684172369,4.98510568408955,77.4782299716993));
#141946=CARTESIAN_POINT('Ctrl Pts',(5.06596027419711,4.85078954164356,77.469557987398));
#141947=CARTESIAN_POINT('Ctrl Pts',(5.19628162053286,4.71092029195721,77.4608860030966));
#141948=CARTESIAN_POINT('Ctrl Pts',(5.32067604038009,4.56596463365905,77.4522140187953));
#141949=CARTESIAN_POINT('Ctrl Pts',(5.44506733164208,4.42101262107213,77.443542252599));
#141950=CARTESIAN_POINT('Ctrl Pts',(5.56353180975496,4.27097467138821,77.4348704864026));
#141951=CARTESIAN_POINT('Ctrl Pts',(5.67567421678027,4.11635138775539,77.4261987202063));
#141952=CARTESIAN_POINT('Ctrl Pts',(5.78782406005978,3.9617178509269,77.4175263789781));
#141953=CARTESIAN_POINT('Ctrl Pts',(5.89365082654157,3.80249860162573,77.4088540377499));
#141954=CARTESIAN_POINT('Ctrl Pts',(5.99280137735851,3.63922494688497,77.4001816965217));
#141955=CARTESIAN_POINT('Ctrl Pts',(6.09194609290756,3.47596090122362,77.3915098656833));
#141956=CARTESIAN_POINT('Ctrl Pts',(6.18441523160385,3.30864317036959,77.3828380348449));
#141957=CARTESIAN_POINT('Ctrl Pts',(6.26990026462871,3.1378300199515,77.3741662040066));
#141958=CARTESIAN_POINT('Ctrl Pts',(6.35538670852299,2.96701405038435,77.3654942300458));
#141959=CARTESIAN_POINT('Ctrl Pts',(6.43388868896941,2.79270279979814,77.3568222560851));
#141960=CARTESIAN_POINT('Ctrl Pts',(6.50514427077197,2.61547788729758,77.3481502821244));
#141961=CARTESIAN_POINT('Ctrl Pts',(6.52787183386155,2.55895052090738,77.3453842835834));
#141962=CARTESIAN_POINT('Ctrl Pts',(6.5498625512969,2.50212689664082,77.3426182850423));
#141963=CARTESIAN_POINT('Ctrl Pts',(6.57110895151816,2.4450263208763,77.3398522865014));
#141964=CARTESIAN_POINT('Origin',(0.,0.,50.));
#141965=CARTESIAN_POINT('',(6.57110895151811,2.44502632087644,75.339916226746));
#141966=CARTESIAN_POINT('',(6.57110895151814,2.44502632087635,75.8870038120088));
#141967=CARTESIAN_POINT('',(6.57110895151814,2.44502632087636,50.));
#141968=CARTESIAN_POINT('',(7.01124789938016,-0.00542733243554445,77.7735343569458));
#141969=CARTESIAN_POINT('Ctrl Pts',(6.57110895151814,2.44502632087635,75.8870038120088));
#141970=CARTESIAN_POINT('Ctrl Pts',(6.50691177316196,2.61755888208302,75.895378926296));
#141971=CARTESIAN_POINT('Ctrl Pts',(6.43587702619422,2.78766482296899,75.9037540405832));
#141972=CARTESIAN_POINT('Ctrl Pts',(6.35821200936702,2.954787066176,75.9121291548703));
#141973=CARTESIAN_POINT('Ctrl Pts',(6.28059487615379,3.12180627178249,75.9204991055619));
#141974=CARTESIAN_POINT('Ctrl Pts',(6.19635576211538,3.28584515032049,75.9288690562535));
#141975=CARTESIAN_POINT('Ctrl Pts',(6.10575007356766,3.44636657969353,75.9372390069451));
#141976=CARTESIAN_POINT('Ctrl Pts',(6.0151869665541,3.6068125695568,75.9456050240498));
#141977=CARTESIAN_POINT('Ctrl Pts',(5.91826341307935,3.76374412102792,75.9539710411546));
#141978=CARTESIAN_POINT('Ctrl Pts',(5.81528096216037,3.91664829843517,75.9623370582594));
#141979=CARTESIAN_POINT('Ctrl Pts',(5.71232566496845,4.06951215908689,75.9707008694685));
#141980=CARTESIAN_POINT('Ctrl Pts',(5.6033148379879,4.21835048985813,75.9790646806775));
#141981=CARTESIAN_POINT('Ctrl Pts',(5.4885938955949,4.36267849053061,75.9874284918866));
#141982=CARTESIAN_POINT('Ctrl Pts',(5.37388930617439,4.50698591787292,75.9957911108707));
#141983=CARTESIAN_POINT('Ctrl Pts',(5.25347642868758,4.6467840397992,76.0041537298548));
#141984=CARTESIAN_POINT('Ctrl Pts',(5.12774183317567,4.78162004500569,76.0125163488389));
#141985=CARTESIAN_POINT('Ctrl Pts',(5.00200840094346,4.91645480272745,76.0208788904531));
#141986=CARTESIAN_POINT('Ctrl Pts',(4.87095357332457,5.04632729521203,76.0292414320674));
#141987=CARTESIAN_POINT('Ctrl Pts',(4.73500203658974,5.17082027109733,76.0376039736816));
#141988=CARTESIAN_POINT('Ctrl Pts',(4.5990336361189,5.29532868937284,76.0459675526045));
#141989=CARTESIAN_POINT('Ctrl Pts',(4.45816755827911,5.41445603912424,76.0543311315273));
#141990=CARTESIAN_POINT('Ctrl Pts',(4.31286325154248,5.52782390602256,76.0626947104501));
#141991=CARTESIAN_POINT('Ctrl Pts',(4.16747266331511,5.64125909059903,76.0710632556542));
#141992=CARTESIAN_POINT('Ctrl Pts',(4.01763883908727,5.74892775566056,76.0794318008583));
#141993=CARTESIAN_POINT('Ctrl Pts',(3.8638528494694,5.85049294676502,76.0878003460624));
#141994=CARTESIAN_POINT('Ctrl Pts',(3.71001917849709,5.9520896281625,76.0961714859343));
#141995=CARTESIAN_POINT('Ctrl Pts',(3.55223117598703,6.04757888555163,76.1045426258063));
#141996=CARTESIAN_POINT('Ctrl Pts',(3.39100704846998,6.13666829474487,76.1129137656783));
#141997=CARTESIAN_POINT('Ctrl Pts',(3.2296486081688,6.225831922647,76.1212918793892));
#141998=CARTESIAN_POINT('Ctrl Pts',(3.06484861387916,6.30858489553324,76.1296699931002));
#141999=CARTESIAN_POINT('Ctrl Pts',(2.89714890824418,6.38468125797675,76.1380481068111));
#142000=CARTESIAN_POINT('Ctrl Pts',(2.80482730357157,6.42657362900944,76.1426604041255));
#142001=CARTESIAN_POINT('Ctrl Pts',(2.71162725246564,6.46644942872256,76.1472727014399));
#142002=CARTESIAN_POINT('Ctrl Pts',(2.61764153474929,6.50427393012129,76.1518849987543));
#142003=CARTESIAN_POINT('Ctrl Pts',(2.45741902907857,6.56875539110389,76.1597478299436));
#142004=CARTESIAN_POINT('Ctrl Pts',(2.29457898084834,6.62740651627268,76.1676106611329));
#142005=CARTESIAN_POINT('Ctrl Pts',(2.12960305163939,6.68000130276546,76.1754734923222));
#142006=CARTESIAN_POINT('Ctrl Pts',(1.96475388465543,6.73255567710726,76.1833302819636));
#142007=CARTESIAN_POINT('Ctrl Pts',(1.7977724612511,6.77906285186163,76.191187071605));
#142008=CARTESIAN_POINT('Ctrl Pts',(1.62916110100275,6.81934459236953,76.1990438612465));
#142009=CARTESIAN_POINT('Ctrl Pts',(1.46064482958017,6.85960361588256,76.2068962200304));
#142010=CARTESIAN_POINT('Ctrl Pts',(1.2905008195074,6.89364410071723,76.2147485788144));
#142011=CARTESIAN_POINT('Ctrl Pts',(1.11924701355265,6.92133749250486,76.2226009375983));
#142012=CARTESIAN_POINT('Ctrl Pts',(0.948033642619447,6.94902434555961,
76.2304514423488));
#142013=CARTESIAN_POINT('Ctrl Pts',(0.775711372021637,6.97036701910394,
76.2383019470992));
#142014=CARTESIAN_POINT('Ctrl Pts',(0.602808751726681,6.98528798055898,
76.2461524518497));
#142015=CARTESIAN_POINT('Ctrl Pts',(0.42993394601388,7.00020654170159,76.2540016937013));
#142016=CARTESIAN_POINT('Ctrl Pts',(0.256479356831333,7.00870541744972,
76.261850935553));
#142017=CARTESIAN_POINT('Ctrl Pts',(0.0829786088306314,7.01075895413446,
76.2697001774047));
#142018=CARTESIAN_POINT('Ctrl Pts',(-0.0905805949680287,7.0128131826959,
76.2775520638195));
#142019=CARTESIAN_POINT('Ctrl Pts',(-0.264185606812616,7.00841773011404,
76.2854039502344));
#142020=CARTESIAN_POINT('Ctrl Pts',(-0.43730264539801,6.9975990853169,76.2932558366493));
#142021=CARTESIAN_POINT('Ctrl Pts',(-0.564420332083106,6.98965508909955,
76.2990213791131));
#142022=CARTESIAN_POINT('Ctrl Pts',(-0.691274897770224,6.97824893703673,
76.3047869215769));
#142023=CARTESIAN_POINT('Ctrl Pts',(-0.817656948322948,6.96340891211763,
76.3105524640407));
#142024=CARTESIAN_POINT('Ctrl Pts',(-1.02930349699573,6.93855696484656,
76.3202077684005));
#142025=CARTESIAN_POINT('Ctrl Pts',(-1.23951683000672,6.90408683421318,
76.3298630727602));
#142026=CARTESIAN_POINT('Ctrl Pts',(-1.44751734984712,6.86019825401508,
76.3395183771199));
#142027=CARTESIAN_POINT('Ctrl Pts',(-1.65667015354632,6.81606653931623,
76.3492271700545));
#142028=CARTESIAN_POINT('Ctrl Pts',(-1.86358552416067,6.76241179639644,
76.358935962989));
#142029=CARTESIAN_POINT('Ctrl Pts',(-2.06749234383549,6.69948520191527,
76.3686447559236));
#142030=CARTESIAN_POINT('Ctrl Pts',(-2.27238038044039,6.63625579931833,
76.3784002683941));
#142031=CARTESIAN_POINT('Ctrl Pts',(-2.47423080736855,6.56366513227131,
76.3881557808646));
#142032=CARTESIAN_POINT('Ctrl Pts',(-2.67228348793353,6.4820156990413,76.3979112933351));
#142033=CARTESIAN_POINT('Ctrl Pts',(-2.87053227112194,6.40028542031092,
76.4076764652639));
#142034=CARTESIAN_POINT('Ctrl Pts',(-3.06497575519559,6.30947845915102,
76.4174416371926));
#142035=CARTESIAN_POINT('Ctrl Pts',(-3.25487414386932,6.20994531941071,
76.4272068091213));
#142036=CARTESIAN_POINT('Ctrl Pts',(-3.44451361039866,6.11054789084815,
76.4369586664596));
#142037=CARTESIAN_POINT('Ctrl Pts',(-3.62962033378246,6.00244808107711,
76.446710523798));
#142038=CARTESIAN_POINT('Ctrl Pts',(-3.80948051215684,5.88604152126004,
76.4564623811363));
#142039=CARTESIAN_POINT('Ctrl Pts',(-3.88791257603977,5.8352798306041,76.4607148971999));
#142040=CARTESIAN_POINT('Ctrl Pts',(-3.9653472594436,5.78293913193116,76.4649674132635));
#142041=CARTESIAN_POINT('Ctrl Pts',(-4.04172677262675,5.72905500566474,
76.4692199293271));
#142042=CARTESIAN_POINT('Ctrl Pts',(-4.18600844094889,5.62726734939678,
76.477252974926));
#142043=CARTESIAN_POINT('Ctrl Pts',(-4.3265931194642,5.51991943857155,76.4852860205249));
#142044=CARTESIAN_POINT('Ctrl Pts',(-4.46302109857391,5.40731626929516,
76.4933190661238));
#142045=CARTESIAN_POINT('Ctrl Pts',(-4.59936137652575,5.29478548567155,
76.5013469477717));
#142046=CARTESIAN_POINT('Ctrl Pts',(-4.7315499923933,5.17700640051699,76.5093748294196));
#142047=CARTESIAN_POINT('Ctrl Pts',(-4.85915744024665,5.05432641737706,
76.5174027110675));
#142048=CARTESIAN_POINT('Ctrl Pts',(-4.98670727207932,4.93170182545892,
76.5254269680476));
#142049=CARTESIAN_POINT('Ctrl Pts',(-5.10967979069723,4.8041809950259,76.5334512250278));
#142050=CARTESIAN_POINT('Ctrl Pts',(-5.22767977197113,4.67215055025241,
76.541475482008));
#142051=CARTESIAN_POINT('Ctrl Pts',(-5.34566548584541,4.54013606930449,
76.5494987687738));
#142052=CARTESIAN_POINT('Ctrl Pts',(-5.45867961004383,4.40361332809949,
76.5575220555395));
#142053=CARTESIAN_POINT('Ctrl Pts',(-5.56636478781921,4.26300476324229,
76.5655453423053));
#142054=CARTESIAN_POINT('Ctrl Pts',(-5.67404114175487,4.12240772000269,
76.5735679716343));
#142055=CARTESIAN_POINT('Ctrl Pts',(-5.77638919931279,3.97772581352337,
76.5815906009633));
#142056=CARTESIAN_POINT('Ctrl Pts',(-5.87309299960993,3.82941316397603,
76.5896132302923));
#142057=CARTESIAN_POINT('Ctrl Pts',(-5.96983315365138,3.68104475943121,
76.5976388755588));
#142058=CARTESIAN_POINT('Ctrl Pts',(-6.0609246138721,3.52904319411107,76.6056645208253));
#142059=CARTESIAN_POINT('Ctrl Pts',(-6.14609552710443,3.37389038562413,
76.6136901660917));
#142060=CARTESIAN_POINT('Ctrl Pts',(-6.19631748759975,3.28240283520521,
76.618422575599));
#142061=CARTESIAN_POINT('Ctrl Pts',(-6.24448173017626,3.18982009089237,
76.6231549851063));
#142062=CARTESIAN_POINT('Ctrl Pts',(-6.29054013873538,3.09624471343256,
76.6278873946135));
#142063=CARTESIAN_POINT('Ctrl Pts',(-6.37550576889593,2.9236227935245,76.6366174434481));
#142064=CARTESIAN_POINT('Ctrl Pts',(-6.45334528794706,2.74753552575064,
76.6453474922826));
#142065=CARTESIAN_POINT('Ctrl Pts',(-6.52380507287336,2.56857819301883,
76.6540775411171));
#142066=CARTESIAN_POINT('Ctrl Pts',(-6.59428523133428,2.38956911455122,
76.6628101142562));
#142067=CARTESIAN_POINT('Ctrl Pts',(-6.65738129601282,2.20768856953147,
76.6715426873952));
#142068=CARTESIAN_POINT('Ctrl Pts',(-6.71288843299128,2.02355020909092,
76.6802752605343));
#142069=CARTESIAN_POINT('Ctrl Pts',(-6.76918413745766,1.83679586929658,
76.6891318938148));
#142070=CARTESIAN_POINT('Ctrl Pts',(-6.81767356152349,1.64771935091506,
76.6979885270952));
#142071=CARTESIAN_POINT('Ctrl Pts',(-6.85819576343266,1.45697544005871,
76.7068451603757));
#142072=CARTESIAN_POINT('Ctrl Pts',(-6.89817578093152,1.26878367024989,
76.7155832924824));
#142073=CARTESIAN_POINT('Ctrl Pts',(-6.93040041898706,1.07896912657834,
76.724321424589));
#142074=CARTESIAN_POINT('Ctrl Pts',(-6.95476667447427,0.888170628945882,
76.7330595566956));
#142075=CARTESIAN_POINT('Ctrl Pts',(-6.97962859021963,0.693490893482653,
76.741975440563));
#142076=CARTESIAN_POINT('Ctrl Pts',(-6.99630894588668,0.497787037273467,
76.7508913244304));
#142077=CARTESIAN_POINT('Ctrl Pts',(-7.00475389972484,0.301743876142743,
76.7598072082978));
#142078=CARTESIAN_POINT('Ctrl Pts',(-7.013198853563,0.105700715012085,76.7687230921652));
#142079=CARTESIAN_POINT('Ctrl Pts',(-7.0134083986347,-0.0906814486463031,
76.7776389760326));
#142080=CARTESIAN_POINT('Ctrl Pts',(-7.005385105977,-0.286716025808756,
76.7865548598999));
#142081=CARTESIAN_POINT('Ctrl Pts',(-6.99751947304752,-0.478898473991935,
76.7952955443963));
#142082=CARTESIAN_POINT('Ctrl Pts',(-6.9817407183158,-0.670767280903081,
76.8040362288926));
#142083=CARTESIAN_POINT('Ctrl Pts',(-6.95809877101564,-0.861677465929471,
76.8127769133889));
#142084=CARTESIAN_POINT('Ctrl Pts',(-6.93446107729452,-1.05255330304236,
76.8215160252909));
#142085=CARTESIAN_POINT('Ctrl Pts',(-6.9029630499438,-1.24247059108854,
76.8302551371929));
#142086=CARTESIAN_POINT('Ctrl Pts',(-6.86370636760534,-1.43079050241251,
76.8389942490949));
#142087=CARTESIAN_POINT('Ctrl Pts',(-6.82394105844773,-1.62155036922371,
76.8478465887692));
#142088=CARTESIAN_POINT('Ctrl Pts',(-6.77621467986333,-1.8106708945318,
76.8566989284435));
#142089=CARTESIAN_POINT('Ctrl Pts',(-6.72068646462178,-1.99749843723333,
76.8655512681178));
#142090=CARTESIAN_POINT('Ctrl Pts',(-6.66589659214933,-2.18184178762613,
76.8742859007677));
#142091=CARTESIAN_POINT('Ctrl Pts',(-6.60351116548221,-2.3639524896423,
76.8830205334175));
#142092=CARTESIAN_POINT('Ctrl Pts',(-6.53373368134623,-2.54321661360998,
76.8917551660674));
#142093=CARTESIAN_POINT('Ctrl Pts',(-6.46254572575269,-2.72610435532991,
76.9006663592539));
#142094=CARTESIAN_POINT('Ctrl Pts',(-6.38366377114332,-2.90602893428911,
76.9095775524404));
#142095=CARTESIAN_POINT('Ctrl Pts',(-6.2973564506595,-3.08235758727588,
76.9184887456269));
#142096=CARTESIAN_POINT('Ctrl Pts',(-6.21104913017568,-3.25868624026265,
76.9273999388134));
#142097=CARTESIAN_POINT('Ctrl Pts',(-6.11731656498037,-3.43141868908865,
76.9363111319999));
#142098=CARTESIAN_POINT('Ctrl Pts',(-6.01647881569091,-3.59994572498566,
76.9452223251864));
#142099=CARTESIAN_POINT('Ctrl Pts',(-5.92566157457395,-3.7517257930815,
76.9532479900388));
#142100=CARTESIAN_POINT('Ctrl Pts',(-5.82903892466044,-3.90016421168517,
76.9612736548911));
#142101=CARTESIAN_POINT('Ctrl Pts',(-5.72689495486187,-4.04478685946215,
76.9692993197434));
#142102=CARTESIAN_POINT('Ctrl Pts',(-5.62478340305396,-4.189363607558,76.9773224374466));
#142103=CARTESIAN_POINT('Ctrl Pts',(-5.51715423131131,-4.330126696814,76.9853455551497));
#142104=CARTESIAN_POINT('Ctrl Pts',(-5.40433510896873,-4.46663056368758,
76.9933686728529));
#142105=CARTESIAN_POINT('Ctrl Pts',(-5.29153021410495,-4.60311721622875,
77.0013907787707));
#142106=CARTESIAN_POINT('Ctrl Pts',(-5.17353690624581,-4.73534543418048,
77.0094128846885));
#142107=CARTESIAN_POINT('Ctrl Pts',(-5.05072339346041,-4.86290240137018,
77.0174349906062));
#142108=CARTESIAN_POINT('Ctrl Pts',(-4.92786424275859,-4.99050676915997,
77.0254600775657));
#142109=CARTESIAN_POINT('Ctrl Pts',(-4.80018156119482,-5.11343615210699,
77.0334851645252));
#142110=CARTESIAN_POINT('Ctrl Pts',(-4.66808102020432,-5.23131399853882,
77.0415102514846));
#142111=CARTESIAN_POINT('Ctrl Pts',(-4.53595446267337,-5.34921506042259,
77.0495369189448));
#142112=CARTESIAN_POINT('Ctrl Pts',(-4.39940859175142,-5.46206236635242,
77.057563586405));
#142113=CARTESIAN_POINT('Ctrl Pts',(-4.25888229620412,-5.56951956182749,
77.0655902538652));
#142114=CARTESIAN_POINT('Ctrl Pts',(-4.11824318664188,-5.67706302356049,
77.0736233651057));
#142115=CARTESIAN_POINT('Ctrl Pts',(-3.97361756707955,-5.77920751717179,
77.0816564763462));
#142116=CARTESIAN_POINT('Ctrl Pts',(-3.82547395057441,-5.87565958986535,
77.0896895875867));
#142117=CARTESIAN_POINT('Ctrl Pts',(-3.73818235011123,-5.93249265491422,
77.0944229885488));
#142118=CARTESIAN_POINT('Ctrl Pts',(-3.64966982055057,-5.98735015673688,
77.0991563895108));
#142119=CARTESIAN_POINT('Ctrl Pts',(-3.56003617203288,-6.04017955166214,
77.1038897904728));
#142120=CARTESIAN_POINT('Ctrl Pts',(-3.37538806651773,-6.1490097493589,
77.113640743767));
#142121=CARTESIAN_POINT('Ctrl Pts',(-3.18587248217892,-6.2492954597494,
77.1233916970612));
#142122=CARTESIAN_POINT('Ctrl Pts',(-2.99222443154484,-6.34067973594047,
77.1331426503554));
#142123=CARTESIAN_POINT('Ctrl Pts',(-2.79829739456617,-6.43219566832475,
77.142907651727));
#142124=CARTESIAN_POINT('Ctrl Pts',(-2.60022601729286,-6.51478449787616,
77.1526726530986));
#142125=CARTESIAN_POINT('Ctrl Pts',(-2.39876794143145,-6.58813622549358,
77.1624376544703));
#142126=CARTESIAN_POINT('Ctrl Pts',(-2.19764565444117,-6.66136569097924,
77.1721863796079));
#142127=CARTESIAN_POINT('Ctrl Pts',(-1.99314798639645,-6.72538881258191,
77.1819351047455));
#142128=CARTESIAN_POINT('Ctrl Pts',(-1.7860475661107,-6.7799454757461,77.1916838298831));
#142129=CARTESIAN_POINT('Ctrl Pts',(-1.57951555617596,-6.83435240202412,
77.2014057985502));
#142130=CARTESIAN_POINT('Ctrl Pts',(-1.37039509353772,-6.87934472802349,
77.2111277672174));
#142131=CARTESIAN_POINT('Ctrl Pts',(-1.15947062925996,-6.91471289515216,
77.2208497358845));
#142132=CARTESIAN_POINT('Ctrl Pts',(-0.949941797071313,-6.94984704035668,
77.2305073768243));
#142133=CARTESIAN_POINT('Ctrl Pts',(-0.738632798804169,-6.97548393062048,
77.240165017764));
#142134=CARTESIAN_POINT('Ctrl Pts',(-0.52633001027022,-6.99146646153645,
77.2498226587038));
#142135=CARTESIAN_POINT('Ctrl Pts',(-0.433015625573714,-6.99849133411874,
77.2540675243889));
#142136=CARTESIAN_POINT('Ctrl Pts',(-0.339509473258997,-7.00365170974024,
77.2583123900741));
#142137=CARTESIAN_POINT('Ctrl Pts',(-0.245879369247421,-7.00693726946934,
77.2625572557593));
#142138=CARTESIAN_POINT('Ctrl Pts',(-0.0726891420112815,-7.01301466137325,
77.2704091027732));
#142139=CARTESIAN_POINT('Ctrl Pts',(0.100854183990988,-7.01267108832776,
77.2782609497872));
#142140=CARTESIAN_POINT('Ctrl Pts',(0.274217249885417,-7.00588548738597,
77.2861127968011));
#142141=CARTESIAN_POINT('Ctrl Pts',(0.447531151415979,-6.99910181078574,
77.2939624170948));
#142142=CARTESIAN_POINT('Ctrl Pts',(0.620664513729673,-6.98587975522444,
77.3018120373884));
#142143=CARTESIAN_POINT('Ctrl Pts',(0.793084111274112,-6.9662503655083,
77.309661657682));
#142144=CARTESIAN_POINT('Ctrl Pts',(0.965489943318995,-6.94662254294786,
77.3175106512839));
#142145=CARTESIAN_POINT('Ctrl Pts',(1.13718174510511,-6.92058844846989,
77.3253596448858));
#142146=CARTESIAN_POINT('Ctrl Pts',(1.3076318089385,-6.88823094958003,77.3332086384876));
#142147=CARTESIAN_POINT('Ctrl Pts',(1.47816816664811,-6.85585706903597,
77.3410616058051));
#142148=CARTESIAN_POINT('Ctrl Pts',(1.64746115506012,-6.81715345885096,
77.3489145731226));
#142149=CARTESIAN_POINT('Ctrl Pts',(1.81499331769497,-6.77225411655695,
77.35676754044));
#142150=CARTESIAN_POINT('Ctrl Pts',(1.98256802787003,-6.72734337133864,
77.3646225021474));
#142151=CARTESIAN_POINT('Ctrl Pts',(2.14838065677686,-6.6762338715936,77.3724774638547));
#142152=CARTESIAN_POINT('Ctrl Pts',(2.31192992701016,-6.61910919800352,
77.380332425562));
#142153=CARTESIAN_POINT('Ctrl Pts',(2.47564153356501,-6.56192782339994,
77.3881951839754));
#142154=CARTESIAN_POINT('Ctrl Pts',(2.6370849394132,-6.49871948922789,77.3960579423888));
#142155=CARTESIAN_POINT('Ctrl Pts',(2.79577929786902,-6.42971575422328,
77.4039207008022));
#142156=CARTESIAN_POINT('Ctrl Pts',(2.91219520209637,-6.37909560437175,
77.40968870755));
#142157=CARTESIAN_POINT('Ctrl Pts',(3.02713214894396,-6.32535767299892,
77.4154567142979));
#142158=CARTESIAN_POINT('Ctrl Pts',(3.1404093910841,-6.26860873072254,77.4212247210457));
#142159=CARTESIAN_POINT('Ctrl Pts',(3.30494530485699,-6.18618053158314,
77.4296027874867));
#142160=CARTESIAN_POINT('Ctrl Pts',(3.46634321095442,-6.09721571817509,
77.4379808539277));
#142161=CARTESIAN_POINT('Ctrl Pts',(3.62407068942216,-6.00197785738761,
77.4463589203687));
#142162=CARTESIAN_POINT('Ctrl Pts',(3.78169031571435,-5.90680511911766,
77.4547312579875));
#142163=CARTESIAN_POINT('Ctrl Pts',(3.93564423765779,-5.80536805470691,
77.4631035956062));
#142164=CARTESIAN_POINT('Ctrl Pts',(4.08542477426931,-5.69797604209482,
77.4714759332249));
#142165=CARTESIAN_POINT('Ctrl Pts',(4.23512485814405,-5.59064171375545,
77.4798437737475));
#142166=CARTESIAN_POINT('Ctrl Pts',(4.3806557598339,-5.47735900608948,77.4882116142701));
#142167=CARTESIAN_POINT('Ctrl Pts',(4.52153854894201,-5.3584807280545,77.4965794547927));
#142168=CARTESIAN_POINT('Ctrl Pts',(4.66236630293313,-5.23964888919054,
77.5049440264626));
#142169=CARTESIAN_POINT('Ctrl Pts',(4.79854931437359,-5.11522605058764,
77.5133085981325));
#142170=CARTESIAN_POINT('Ctrl Pts',(4.92964118259504,-4.9856057178003,77.5216731698024));
#142171=CARTESIAN_POINT('Ctrl Pts',(5.06070102915595,-4.85601704722321,
77.5300356982679));
#142172=CARTESIAN_POINT('Ctrl Pts',(5.18667197933735,-4.72123364552564,
77.5383982267335));
#142173=CARTESIAN_POINT('Ctrl Pts',(5.30714367761709,-4.58168664878219,
77.5467607551991));
#142174=CARTESIAN_POINT('Ctrl Pts',(5.42762498991515,-4.44212851575194,
77.5551239510205));
#142175=CARTESIAN_POINT('Ctrl Pts',(5.54260595418539,-4.2978062730279,77.563487146842));
#142176=CARTESIAN_POINT('Ctrl Pts',(5.65171528838159,-4.14918556605677,
77.5718503426635));
#142177=CARTESIAN_POINT('Ctrl Pts',(5.76083206361579,-4.00055472345117,
77.5802141088382));
#142178=CARTESIAN_POINT('Ctrl Pts',(5.86407621553605,-3.84762509699095,
77.5885778750129));
#142179=CARTESIAN_POINT('Ctrl Pts',(5.9611186444202,-3.69089299081481,77.5969416411876));
#142180=CARTESIAN_POINT('Ctrl Pts',(6.05818062944185,-3.53412929974686,
77.6053070928411));
#142181=CARTESIAN_POINT('Ctrl Pts',(6.14903822626462,-3.37356188052684,
77.6136725444947));
#142182=CARTESIAN_POINT('Ctrl Pts',(6.23340709661391,-3.20971377701867,
77.6220379961482));
#142183=CARTESIAN_POINT('Ctrl Pts',(6.31780422193185,-3.04581080110305,
77.6304062493751));
#142184=CARTESIAN_POINT('Ctrl Pts',(6.39570813717459,-2.87862524226243,
77.6387745026019));
#142185=CARTESIAN_POINT('Ctrl Pts',(6.46688147404923,-2.70870274542978,
77.6471427558287));
#142186=CARTESIAN_POINT('Ctrl Pts',(6.53812079876125,-2.53862270620021,
77.6555187676202));
#142187=CARTESIAN_POINT('Ctrl Pts',(6.60261694815901,-2.36580096180234,
77.6638947794116));
#142188=CARTESIAN_POINT('Ctrl Pts',(6.66018109501871,-2.19080221472762,
77.6722707912031));
#142189=CARTESIAN_POINT('Ctrl Pts',(6.7177734720473,-2.01571764610502,77.6806509106942));
#142190=CARTESIAN_POINT('Ctrl Pts',(6.76842697074315,-1.8384542599116,77.6890310301853));
#142191=CARTESIAN_POINT('Ctrl Pts',(6.81200310361949,-1.65959039488016,
77.6974111496765));
#142192=CARTESIAN_POINT('Ctrl Pts',(6.85562902774758,-1.48052215522559,
77.7058008445157));
#142193=CARTESIAN_POINT('Ctrl Pts',(6.89216135548311,-1.29985010354622,
77.7141905393549));
#142194=CARTESIAN_POINT('Ctrl Pts',(6.92151277629054,-1.11816253297399,
77.7225802341941));
#142195=CARTESIAN_POINT('Ctrl Pts',(6.94014748685212,-1.00281222974806,
77.7279067066689));
#142196=CARTESIAN_POINT('Ctrl Pts',(6.95588878622549,-0.88705273944197,
77.7332331791438));
#142197=CARTESIAN_POINT('Ctrl Pts',(6.96872520897279,-0.771035358675027,
77.7385596516186));
#142198=CARTESIAN_POINT('Ctrl Pts',(6.99682073277446,-0.51710409239379,
77.7502178867158));
#142199=CARTESIAN_POINT('Ctrl Pts',(7.01104969501972,-0.261475717699596,
77.7618761218131));
#142200=CARTESIAN_POINT('Ctrl Pts',(7.01124789937955,-0.00542733321403496,
77.7735343569104));
#142201=CARTESIAN_POINT('Ctrl Pts',(7.01124789938016,-0.00542733243554912,
77.7735343569458));
#142202=CARTESIAN_POINT('Ctrl Pts',(7.01138511916316,0.171838741963074,
77.781605525113));
#142203=CARTESIAN_POINT('Ctrl Pts',(7.00479546290913,0.349352178619966,
77.7896766932801));
#142204=CARTESIAN_POINT('Ctrl Pts',(6.99144932896976,0.526557540016621,
77.7977478614472));
#142205=CARTESIAN_POINT('Ctrl Pts',(6.9781197110538,0.703543607353173,77.8058090414333));
#142206=CARTESIAN_POINT('Ctrl Pts',(6.9580503022769,0.880222000904489,77.8138702214194));
#142207=CARTESIAN_POINT('Ctrl Pts',(6.93126350620007,1.05603634886262,77.8219314014055));
#142208=CARTESIAN_POINT('Ctrl Pts',(6.90449585387803,1.23172504734945,77.8299868202974));
#142209=CARTESIAN_POINT('Ctrl Pts',(6.87102042328743,1.40655057346108,77.8380422391893));
#142210=CARTESIAN_POINT('Ctrl Pts',(6.83091153713191,1.57996016860493,77.8460976580813));
#142211=CARTESIAN_POINT('Ctrl Pts',(6.79082655032157,1.75326643562958,77.8541482770585));
#142212=CARTESIAN_POINT('Ctrl Pts',(6.74411606152931,1.92515810053984,77.8621988960356));
#142213=CARTESIAN_POINT('Ctrl Pts',(6.69090572305961,2.0950912074724,77.8702495150127));
#142214=CARTESIAN_POINT('Ctrl Pts',(6.65406888747181,2.21273372020634,77.8758228553855));
#142215=CARTESIAN_POINT('Ctrl Pts',(6.61411799969896,2.32943773228563,77.8813961957583));
#142216=CARTESIAN_POINT('Ctrl Pts',(6.57110895151815,2.44502632087633,77.886969536131));
#142217=CARTESIAN_POINT('',(7.01124999865213,-0.000137478976900538,77.2264656430895));
#142218=CARTESIAN_POINT('Ctrl Pts',(6.57110895151816,2.4450263208763,77.3398522865014));
#142219=CARTESIAN_POINT('Ctrl Pts',(6.637719246809,2.26600840850797,77.3311805125692));
#142220=CARTESIAN_POINT('Ctrl Pts',(6.69700989700475,2.08426710051949,77.3225087386371));
#142221=CARTESIAN_POINT('Ctrl Pts',(6.74878307789424,1.90040877971777,77.313836964705));
#142222=CARTESIAN_POINT('Ctrl Pts',(6.8005597878953,1.71653792623955,77.3051645996627));
#142223=CARTESIAN_POINT('Ctrl Pts',(6.84481792613571,1.53055004459464,77.2964922346203));
#142224=CARTESIAN_POINT('Ctrl Pts',(6.88140980451094,1.34306577086931,77.287819869578));
#142225=CARTESIAN_POINT('Ctrl Pts',(6.91799949925379,1.15559268532967,77.2791480220618));
#142226=CARTESIAN_POINT('Ctrl Pts',(6.94692379517685,0.966623665171066,
77.2704761745457));
#142227=CARTESIAN_POINT('Ctrl Pts',(6.96808618426385,0.776789219268177,
77.2618043270296));
#142228=CARTESIAN_POINT('Ctrl Pts',(6.98924897510674,0.586951169466541,
77.2531323148834));
#142229=CARTESIAN_POINT('Ctrl Pts',(7.00264953276855,0.396247943319841,
77.2444603027372));
#142230=CARTESIAN_POINT('Ctrl Pts',(7.00824314361837,0.205315860142578,
77.235788290591));
#142231=CARTESIAN_POINT('Ctrl Pts',(7.01024757124656,0.136896809746853,
77.2326807414238));
#142232=CARTESIAN_POINT('Ctrl Pts',(7.01125,0.0684484052931081,77.2295731922567));
#142233=CARTESIAN_POINT('Ctrl Pts',(7.01125,8.58630487052188E-16,77.2264656430895));
#142234=CARTESIAN_POINT('Ctrl Pts',(7.01124999865213,-0.000137478976900539,
77.2264656430895));
#142235=CARTESIAN_POINT('Ctrl Pts',(7.01124653751549,-0.176650970735805,
77.2184682469791));
#142236=CARTESIAN_POINT('Ctrl Pts',(7.00457294202628,-0.353199053916174,
77.2104708508687));
#142237=CARTESIAN_POINT('Ctrl Pts',(6.99124740153013,-0.529231833035602,
77.2024734547584));
#142238=CARTESIAN_POINT('Ctrl Pts',(6.97791746639215,-0.705322666161424,
77.1944734211796));
#142239=CARTESIAN_POINT('Ctrl Pts',(6.95793122676564,-0.880897487063261,
77.1864733876009));
#142240=CARTESIAN_POINT('Ctrl Pts',(6.93135887638516,-1.05541019952274,
77.1784733540221));
#142241=CARTESIAN_POINT('Ctrl Pts',(6.9047823209948,-1.22995052819495,77.1704720544575));
#142242=CARTESIAN_POINT('Ctrl Pts',(6.87161764258769,-1.40342804999125,
77.1624707548929));
#142243=CARTESIAN_POINT('Ctrl Pts',(6.8319863010249,-1.57530623851623,77.1544694553283));
#142244=CARTESIAN_POINT('Ctrl Pts',(6.79232266651492,-1.74732447915767,
77.1464616360363));
#142245=CARTESIAN_POINT('Ctrl Pts',(6.74618193427857,-1.91774042548032,
77.1384538167442));
#142246=CARTESIAN_POINT('Ctrl Pts',(6.69373582543948,-2.08603146230541,
77.1304459974522));
#142247=CARTESIAN_POINT('Ctrl Pts',(6.65431331897053,-2.21253187644019,
77.1244267080362));
#142248=CARTESIAN_POINT('Ctrl Pts',(6.6113292075835,-2.33783196150945,77.1184074186203));
#142249=CARTESIAN_POINT('Ctrl Pts',(6.56487433029689,-2.46171720347991,
77.1123881292043));
#142250=CARTESIAN_POINT('Ctrl Pts',(6.48961971012751,-2.6624052124388,77.1026371759106));
#142251=CARTESIAN_POINT('Ctrl Pts',(6.40520950385572,-2.85950492702172,
77.0928862226169));
#142252=CARTESIAN_POINT('Ctrl Pts',(6.31199119298207,-3.05227681284264,
77.0831352693232));
#142253=CARTESIAN_POINT('Ctrl Pts',(6.21863858364407,-3.24532642272864,
77.073370267952));
#142254=CARTESIAN_POINT('Ctrl Pts',(6.11645250333443,-3.43403569713888,
77.0636052665808));
#142255=CARTESIAN_POINT('Ctrl Pts',(6.0058275377292,-3.61768740351534,77.0538402652096));
#142256=CARTESIAN_POINT('Ctrl Pts',(5.895386961021,-3.80103300054849,77.0440915400724));
#142257=CARTESIAN_POINT('Ctrl Pts',(5.77653563054599,-3.97933784505743,
77.0343428149353));
#142258=CARTESIAN_POINT('Ctrl Pts',(5.64971113665204,-4.15191409290822,
77.0245940897981));
#142259=CARTESIAN_POINT('Ctrl Pts',(5.52323472681706,-4.32401668587588,
77.0148721211314));
#142260=CARTESIAN_POINT('Ctrl Pts',(5.38882886352657,-4.49042203795991,
77.0051501524646));
#142261=CARTESIAN_POINT('Ctrl Pts',(5.24697210171365,-4.65047420445901,
76.9954281837979));
#142262=CARTESIAN_POINT('Ctrl Pts',(5.10605396904297,-4.80946734757541,
76.9857705428585));
#142263=CARTESIAN_POINT('Ctrl Pts',(4.95778322259031,-4.96219104787508,
76.9761129019192));
#142264=CARTESIAN_POINT('Ctrl Pts',(4.80267287525534,-5.10802895604426,
76.9664552609799));
#142265=CARTESIAN_POINT('Ctrl Pts',(4.73449653744279,-5.17212973761073,
76.9622103952926));
#142266=CARTESIAN_POINT('Ctrl Pts',(4.6649994254643,-5.23490060213245,76.9579655296053));
#142267=CARTESIAN_POINT('Ctrl Pts',(4.59422781015657,-5.29629090882327,
76.953720663918));
#142268=CARTESIAN_POINT('Ctrl Pts',(4.46331957011717,-5.40984627942531,
76.945868816904));
#142269=CARTESIAN_POINT('Ctrl Pts',(4.32810190270061,-5.51862856870583,
76.93801696989));
#142270=CARTESIAN_POINT('Ctrl Pts',(4.1889764798803,-5.62228624435911,76.9301651228759));
#142271=CARTESIAN_POINT('Ctrl Pts',(4.04989051190508,-5.72591452353364,
76.9223155025823));
#142272=CARTESIAN_POINT('Ctrl Pts',(3.90689929853329,-5.82442085225462,
76.9144658822886));
#142273=CARTESIAN_POINT('Ctrl Pts',(3.76043715101642,-5.91749431734037,
76.9066162619949));
#142274=CARTESIAN_POINT('Ctrl Pts',(3.613986696629,-6.01056035170019,76.8987672683931));
#142275=CARTESIAN_POINT('Ctrl Pts',(3.46406618210344,-6.09819418192818,
76.8909182747912));
#142276=CARTESIAN_POINT('Ctrl Pts',(3.31113819014348,-6.18012867570518,
76.8830692811893));
#142277=CARTESIAN_POINT('Ctrl Pts',(3.15813277521908,-6.26210465051724,
76.8752163138718));
#142278=CARTESIAN_POINT('Ctrl Pts',(3.00211717731695,-6.3383753433048,76.8673633465543));
#142279=CARTESIAN_POINT('Ctrl Pts',(2.84357813319388,-6.40871983807388,
76.8595103792368));
#142280=CARTESIAN_POINT('Ctrl Pts',(2.68499882548059,-6.47908219798101,
76.8516554175295));
#142281=CARTESIAN_POINT('Ctrl Pts',(2.52389514901132,-6.54351521977476,
76.8438004558221));
#142282=CARTESIAN_POINT('Ctrl Pts',(2.36077241121885,-6.60184672534344,
76.8359454941148));
#142283=CARTESIAN_POINT('Ctrl Pts',(2.19748776047387,-6.66023612980727,
76.8280827357014));
#142284=CARTESIAN_POINT('Ctrl Pts',(2.03218040928632,-6.71251180717497,
76.8202199772879));
#142285=CARTESIAN_POINT('Ctrl Pts',(1.86536991975555,-6.75855174020079,
76.8123572188745));
#142286=CARTESIAN_POINT('Ctrl Pts',(1.74300013823561,-6.79232597443157,
76.8065892121269));
#142287=CARTESIAN_POINT('Ctrl Pts',(1.61982173542334,-6.8227455092496,76.8008212053792));
#142288=CARTESIAN_POINT('Ctrl Pts',(1.49604240872743,-6.84977982666516,
76.7950531986315));
#142289=CARTESIAN_POINT('Ctrl Pts',(1.31625215042021,-6.88904734444093,
76.7866751321905));
#142290=CARTESIAN_POINT('Ctrl Pts',(1.13479557452042,-6.92125810630842,
76.7782970657495));
#142291=CARTESIAN_POINT('Ctrl Pts',(0.952252475682059,-6.94628258747493,
76.7699189993085));
#142292=CARTESIAN_POINT('Ctrl Pts',(0.769834197645653,-6.97128995719856,
76.7615466616898));
#142293=CARTESIAN_POINT('Ctrl Pts',(0.586331202536263,-6.98912079856636,
76.7531743240711));
#142294=CARTESIAN_POINT('Ctrl Pts',(0.402332826543463,-6.99969676908833,
76.7448019864524));
#142295=CARTESIAN_POINT('Ctrl Pts',(0.21843328297071,-7.01026705886037,
76.7364341459298));
#142296=CARTESIAN_POINT('Ctrl Pts',(0.0340392165169123,-7.01359022894083,
76.7280663054072));
#142297=CARTESIAN_POINT('Ctrl Pts',(-0.150255111326989,-7.00963978846418,
76.7196984648847));
#142298=CARTESIAN_POINT('Ctrl Pts',(-0.334477445565594,-7.00569089120622,
76.7113338932148));
#142299=CARTESIAN_POINT('Ctrl Pts',(-0.518599790738046,-6.99447405657724,
76.7029693215449));
#142300=CARTESIAN_POINT('Ctrl Pts',(-0.702027618129939,-6.97601489289428,
76.694604749875));
#142301=CARTESIAN_POINT('Ctrl Pts',(-0.885410639816613,-6.95756023821009,
76.6862422214094));
#142302=CARTESIAN_POINT('Ctrl Pts',(-1.06809915534184,-6.93186681574628,
76.6778796929438));
#142303=CARTESIAN_POINT('Ctrl Pts',(-1.24950303009345,-6.89901215684444,
76.6695171644783));
#142304=CARTESIAN_POINT('Ctrl Pts',(-1.43092138144191,-6.866154876038,76.6611539686568));
#142305=CARTESIAN_POINT('Ctrl Pts',(-1.61105456271462,-6.82613526966803,
76.6527907728353));
#142306=CARTESIAN_POINT('Ctrl Pts',(-1.78932115041994,-6.77908226702995,
76.6444275770138));
#142307=CARTESIAN_POINT('Ctrl Pts',(-1.96759989554915,-6.73202605547142,
76.6360638108391));
#142308=CARTESIAN_POINT('Ctrl Pts',(-2.14401147528783,-6.6779355748947,
76.6277000446644));
#142309=CARTESIAN_POINT('Ctrl Pts',(-2.31798801533611,-6.6169901105607,
76.6193362784898));
#142310=CARTESIAN_POINT('Ctrl Pts',(-2.49199961540088,-6.55603236440421,
76.6109708268362));
#142311=CARTESIAN_POINT('Ctrl Pts',(-2.66357488698875,-6.48821698860404,
76.6026053751826));
#142312=CARTESIAN_POINT('Ctrl Pts',(-2.83216397389218,-6.41377219641353,
76.5942399235291));
#142313=CARTESIAN_POINT('Ctrl Pts',(-3.00080952094936,-6.33930247280848,
76.5858716703022));
#142314=CARTESIAN_POINT('Ctrl Pts',(-3.16646658851368,-6.25819903847252,
76.5775034170754));
#142315=CARTESIAN_POINT('Ctrl Pts',(-3.32860765713012,-6.17073720291139,
76.5691351638485));
#142316=CARTESIAN_POINT('Ctrl Pts',(-3.49089905364909,-6.08319427775093,
76.5607591520571));
#142317=CARTESIAN_POINT('Ctrl Pts',(-3.6496676474343,-5.98928132735913,
76.5523831402656));
#142318=CARTESIAN_POINT('Ctrl Pts',(-3.80441170459272,-5.88931898817324,
76.5440071284742));
#142319=CARTESIAN_POINT('Ctrl Pts',(-3.95923165014872,-5.78930762622113,
76.535627008983));
#142320=CARTESIAN_POINT('Ctrl Pts',(-4.11002285072763,-5.68324114309494,
76.5272468894919));
#142321=CARTESIAN_POINT('Ctrl Pts',(-4.25631416380471,-5.57148241507549,
76.5188667700008));
#142322=CARTESIAN_POINT('Ctrl Pts',(-4.40277263323834,-5.45959598855232,
76.5104770751616));
#142323=CARTESIAN_POINT('Ctrl Pts',(-4.54472068365802,-5.3420045253851,
76.5020873803224));
#142324=CARTESIAN_POINT('Ctrl Pts',(-4.68172072875001,-5.21911080362282,
76.4936976854832));
#142325=CARTESIAN_POINT('Ctrl Pts',(-4.76869969320849,-5.14108770041762,
76.4883712130083));
#142326=CARTESIAN_POINT('Ctrl Pts',(-4.85368495392375,-5.06092814975111,
76.4830447405335));
#142327=CARTESIAN_POINT('Ctrl Pts',(-4.93657252139308,-4.97874264282929,
76.4777182680587));
#142328=CARTESIAN_POINT('Ctrl Pts',(-5.06699760217106,-4.84942226697167,
76.4693369676537));
#142329=CARTESIAN_POINT('Ctrl Pts',(-5.19249008304766,-4.71482309815668,
76.4609556672488));
#142330=CARTESIAN_POINT('Ctrl Pts',(-5.31261214948045,-4.57534465496237,
76.4525743668439));
#142331=CARTESIAN_POINT('Ctrl Pts',(-5.43258197877855,-4.43604298027674,
76.4442036885103));
#142332=CARTESIAN_POINT('Ctrl Pts',(-5.54719474562804,-4.29187460107287,
76.4358330101767));
#142333=CARTESIAN_POINT('Ctrl Pts',(-5.65604866498148,-4.14327648870568,
76.4274623318431));
#142334=CARTESIAN_POINT('Ctrl Pts',(-5.76477905382583,-3.99484700968288,
76.4191011527923));
#142335=CARTESIAN_POINT('Ctrl Pts',(-5.86776342830509,-3.84199807954641,
76.4107399737414));
#142336=CARTESIAN_POINT('Ctrl Pts',(-5.96463929270948,-3.68520076391587,
76.4023787946905));
#142337=CARTESIAN_POINT('Ctrl Pts',(-6.06138944925228,-3.52860691129825,
76.3940284652558));
#142338=CARTESIAN_POINT('Ctrl Pts',(-6.15204673458512,-3.36807516996693,
76.385678135821));
#142339=CARTESIAN_POINT('Ctrl Pts',(-6.23629115844991,-3.2041066070809,
76.3773278063863));
#142340=CARTESIAN_POINT('Ctrl Pts',(-6.32047076126999,-3.04026420819551,
76.3689839020305));
#142341=CARTESIAN_POINT('Ctrl Pts',(-6.39824718671091,-2.87299054781785,
76.3606399976748));
#142342=CARTESIAN_POINT('Ctrl Pts',(-6.46934513066078,-2.70281337552108,
76.352296093319));
#142343=CARTESIAN_POINT('Ctrl Pts',(-6.54038596829858,-2.53277289059061,
76.3439588908393));
#142344=CARTESIAN_POINT('Ctrl Pts',(-6.60475889663115,-2.35983384627065,
76.3356216883595));
#142345=CARTESIAN_POINT('Ctrl Pts',(-6.66223566239757,-2.18454630099204,
76.3272844858798));
#142346=CARTESIAN_POINT('Ctrl Pts',(-6.68115669642255,-2.12684260865401,
76.3245399248439));
#142347=CARTESIAN_POINT('Ctrl Pts',(-6.69933078348043,-2.0688845826821,
76.321795363808));
#142348=CARTESIAN_POINT('Ctrl Pts',(-6.7167509220829,-2.01069232186293,
76.3190508027721));
#142349=CARTESIAN_POINT('Ctrl Pts',(-6.76967542231036,-1.83389715442817,
76.3107124924702));
#142350=CARTESIAN_POINT('Ctrl Pts',(-6.81559374010485,-1.65508383051262,
76.3023741821684));
#142351=CARTESIAN_POINT('Ctrl Pts',(-6.85437739255984,-1.47483460864757,
76.2940358718665));
#142352=CARTESIAN_POINT('Ctrl Pts',(-6.89318544637291,-1.29447198008848,
76.2856923153827));
#142353=CARTESIAN_POINT('Ctrl Pts',(-6.92484981227638,-1.11267197191921,
76.277348758899));
#142354=CARTESIAN_POINT('Ctrl Pts',(-6.94929344594752,-0.930025356971954,
76.2690052024152));
#142355=CARTESIAN_POINT('Ctrl Pts',(-6.97375567622863,-0.747239785276085,
76.26065529819));
#142356=CARTESIAN_POINT('Ctrl Pts',(-6.99098617312171,-0.563606646431596,
76.2523053939649));
#142357=CARTESIAN_POINT('Ctrl Pts',(-7.0009598519598,-0.379720573247087,
76.2439554897397));
#142358=CARTESIAN_POINT('Ctrl Pts',(-7.01094849057808,-0.195558684560555,
76.2355930612761));
#142359=CARTESIAN_POINT('Ctrl Pts',(-7.01365854234673,-0.0111434308617165,
76.2272306328125));
#142360=CARTESIAN_POINT('Ctrl Pts',(-7.00911703962843,0.172930296045726,
76.2188682043489));
#142361=CARTESIAN_POINT('Ctrl Pts',(-7.0045716533062,0.357161431082704,
76.2104986248689));
#142362=CARTESIAN_POINT('Ctrl Pts',(-6.99276236071144,0.541050130409365,
76.202129045389));
#142363=CARTESIAN_POINT('Ctrl Pts',(-6.97376799027683,0.724007306793444,
76.1937594659091));
#142364=CARTESIAN_POINT('Ctrl Pts',(-6.95474432334008,0.907246672330727,
76.1853769773726));
#142365=CARTESIAN_POINT('Ctrl Pts',(-6.92851347978127,1.08955132016771,
76.1769944888361));
#142366=CARTESIAN_POINT('Ctrl Pts',(-6.89520548792931,1.27034162402465,
76.1686120002996));
#142367=CARTESIAN_POINT('Ctrl Pts',(-6.88430656721078,1.32949917387554,
76.165869112695));
#142368=CARTESIAN_POINT('Ctrl Pts',(-6.87265029112176,1.38849469943314,
76.1631262250904));
#142369=CARTESIAN_POINT('Ctrl Pts',(-6.86024236830199,1.44730826386583,
76.1603833374859));
#142370=CARTESIAN_POINT('Ctrl Pts',(-6.82228941872304,1.62720527627431,
76.1519934823531));
#142371=CARTESIAN_POINT('Ctrl Pts',(-6.77722367749001,1.80576193640422,
76.1436036272203));
#142372=CARTESIAN_POINT('Ctrl Pts',(-6.72515683921795,1.98239553329299,
76.1352137720875));
#142373=CARTESIAN_POINT('Ctrl Pts',(-6.67313804749433,2.15886613517478,
76.1268316589955));
#142374=CARTESIAN_POINT('Ctrl Pts',(-6.61413113025583,2.3334168976397,76.1184495459034));
#142375=CARTESIAN_POINT('Ctrl Pts',(-6.54829853369401,2.50547657664582,
76.1100674328113));
#142376=CARTESIAN_POINT('Ctrl Pts',(-6.48251700927431,2.67740277380803,
76.1016918224624));
#142377=CARTESIAN_POINT('Ctrl Pts',(-6.40992047975667,2.8468414345137,76.0933162121136));
#142378=CARTESIAN_POINT('Ctrl Pts',(-6.33072093878141,3.01323728866059,
76.0849406017647));
#142379=CARTESIAN_POINT('Ctrl Pts',(-6.25157121549357,3.17952847734418,
76.0765702597991));
#142380=CARTESIAN_POINT('Ctrl Pts',(-6.16582690315319,3.34278037969969,
76.0681999178336));
#142381=CARTESIAN_POINT('Ctrl Pts',(-6.07374793431603,3.50245807867729,
76.059829575868));
#142382=CARTESIAN_POINT('Ctrl Pts',(-5.98171338677479,3.6620587449686,76.0514632719737));
#142383=CARTESIAN_POINT('Ctrl Pts',(-5.88335044082332,3.8180883621323,76.0430969680794));
#142384=CARTESIAN_POINT('Ctrl Pts',(-5.77896496849459,3.97003658111765,
76.0347306641851));
#142385=CARTESIAN_POINT('Ctrl Pts',(-5.67460868985666,4.12194230444509,
76.0263667001115));
#142386=CARTESIAN_POINT('Ctrl Pts',(-5.56423342811717,4.26976863416483,
76.0180027360379));
#142387=CARTESIAN_POINT('Ctrl Pts',(-5.44818868140137,4.41303372458788,
76.0096387719642));
#142388=CARTESIAN_POINT('Ctrl Pts',(-5.33216179204368,4.55627676889428,
76.0012760949657));
#142389=CARTESIAN_POINT('Ctrl Pts',(-5.21046736398403,4.69495971803615,
75.9929134179672));
#142390=CARTESIAN_POINT('Ctrl Pts',(-5.08349578478998,4.82863305382823,
75.9845507409687));
#142391=CARTESIAN_POINT('Ctrl Pts',(-4.95652681970868,4.96230363753063,
75.9761882361424));
#142392=CARTESIAN_POINT('Ctrl Pts',(-4.82428114676611,5.09096457553284,
75.9678257313161));
#142393=CARTESIAN_POINT('Ctrl Pts',(-4.68718697469538,5.21420222342268,
75.9594632264898));
#142394=CARTESIAN_POINT('Ctrl Pts',(-4.55007735146583,5.3374537607758,75.9510997791698));
#142395=CARTESIAN_POINT('Ctrl Pts',(-4.40811838440878,5.45528057009708,
75.9427363318498));
#142396=CARTESIAN_POINT('Ctrl Pts',(-4.26177272292003,5.56730813056676,
75.9343728845299));
#142397=CARTESIAN_POINT('Ctrl Pts',(-4.11534088899297,5.67940165601243,
75.9260045125771));
#142398=CARTESIAN_POINT('Ctrl Pts',(-3.96451745982751,5.78568890835623,
75.9176361406243));
#142399=CARTESIAN_POINT('Ctrl Pts',(-3.80979637388745,5.88583708167446,
75.9092677686715));
#142400=CARTESIAN_POINT('Ctrl Pts',(-3.65502892946641,5.98601526200278,
75.9008968893357));
#142401=CARTESIAN_POINT('Ctrl Pts',(-3.49636177845906,6.08005052134992,
75.89252601));
#142402=CARTESIAN_POINT('Ctrl Pts',(-3.33431562974891,6.16765480905929,
75.8841551306643));
#142403=CARTESIAN_POINT('Ctrl Pts',(-3.17213218108927,6.25533332293431,
75.875777158773));
#142404=CARTESIAN_POINT('Ctrl Pts',(-3.00656430586399,6.33656982562424,
75.8673991868817));
#142405=CARTESIAN_POINT('Ctrl Pts',(-2.8381560084519,6.41112291523009,75.8590212149904));
#142406=CARTESIAN_POINT('Ctrl Pts',(-2.7311311640895,6.45850201076407,75.8536969456313));
#142407=CARTESIAN_POINT('Ctrl Pts',(-2.62295958428094,6.50318283201099,
75.8483726762721));
#142408=CARTESIAN_POINT('Ctrl Pts',(-2.51378464525668,6.54511369800187,
75.843048406913));
#142409=CARTESIAN_POINT('Ctrl Pts',(-2.35255611646706,6.60703680869931,
75.8351855757237));
#142410=CARTESIAN_POINT('Ctrl Pts',(-2.18880317525655,6.66308866001884,
75.8273227445343));
#142411=CARTESIAN_POINT('Ctrl Pts',(-2.0230110193665,6.71305094409552,75.819459913345));
#142412=CARTESIAN_POINT('Ctrl Pts',(-1.85734625286391,6.76297483875184,
75.8116031237035));
#142413=CARTESIAN_POINT('Ctrl Pts',(-1.68964575031866,6.80681836178648,
75.8037463340621));
#142414=CARTESIAN_POINT('Ctrl Pts',(-1.52041460454805,6.84441129628962,
75.7958895444206));
#142415=CARTESIAN_POINT('Ctrl Pts',(-1.35127889713284,6.88198303015723,
75.7880371856366));
#142416=CARTESIAN_POINT('Ctrl Pts',(-1.1806146346543,6.91331110517551,75.7801848268526));
#142417=CARTESIAN_POINT('Ctrl Pts',(-1.00894174040602,6.93827522709834,
75.7723324680686));
#142418=CARTESIAN_POINT('Ctrl Pts',(-0.837309380130855,6.96323345470074,
75.7644819633181));
#142419=CARTESIAN_POINT('Ctrl Pts',(-0.664669237816469,6.98183065663988,
75.7566314585676));
#142420=CARTESIAN_POINT('Ctrl Pts',(-0.491551030523516,6.99399772282572,
75.7487809538171));
#142421=CARTESIAN_POINT('Ctrl Pts',(-0.318460672493938,7.00616283171408,
75.7409317119654));
#142422=CARTESIAN_POINT('Ctrl Pts',(-0.144892783383574,7.01189984029959,
75.7330824701137));
#142423=CARTESIAN_POINT('Ctrl Pts',(0.0286186714364771,7.01119159160162,
75.725233228262));
#142424=CARTESIAN_POINT('Ctrl Pts',(0.202188585661757,7.0104831042808,75.7173813418471));
#142425=CARTESIAN_POINT('Ctrl Pts',(0.375701645758201,7.0033250237297,75.7095294554322));
#142426=CARTESIAN_POINT('Ctrl Pts',(0.548624559648844,6.98975233145282,
75.7016775690173));
#142427=CARTESIAN_POINT('Ctrl Pts',(0.675599702981625,6.9797860724505,75.6959120265537));
#142428=CARTESIAN_POINT('Ctrl Pts',(0.802256653232083,6.96636228413978,
75.6901464840901));
#142429=CARTESIAN_POINT('Ctrl Pts',(0.928386492955239,6.94951257874956,
75.6843809416265));
#142430=CARTESIAN_POINT('Ctrl Pts',(1.13961067507704,6.92129510659661,75.6747256372668));
#142431=CARTESIAN_POINT('Ctrl Pts',(1.34924873524208,6.88348348125227,75.6650703329071));
#142432=CARTESIAN_POINT('Ctrl Pts',(1.55652435376117,6.83628981967912,75.6554150285474));
#142433=CARTESIAN_POINT('Ctrl Pts',(1.76494824032233,6.78883471407431,75.6457062356129));
#142434=CARTESIAN_POINT('Ctrl Pts',(1.97098340391546,6.73189339869494,75.6359974426784));
#142435=CARTESIAN_POINT('Ctrl Pts',(2.17386282222187,6.66572929188259,75.6262886497439));
#142436=CARTESIAN_POINT('Ctrl Pts',(2.37771851351549,6.59924679777033,75.6165331372734));
#142437=CARTESIAN_POINT('Ctrl Pts',(2.57838798132566,6.52345257317632,75.6067776248029));
#142438=CARTESIAN_POINT('Ctrl Pts',(2.77511599997138,6.43866117676671,75.5970221123325));
#142439=CARTESIAN_POINT('Ctrl Pts',(2.97203880962188,6.35378582382962,75.5872569404038));
#142440=CARTESIAN_POINT('Ctrl Pts',(3.16501233314907,6.25989550531329,75.5774917684751));
#142441=CARTESIAN_POINT('Ctrl Pts',(3.35330244677766,6.15735245563667,75.5677265965464));
#142442=CARTESIAN_POINT('Ctrl Pts',(3.54133583110839,6.05494922108171,75.557974739208));
#142443=CARTESIAN_POINT('Ctrl Pts',(3.7246985350011,5.94391685311914,75.5482228818697));
#142444=CARTESIAN_POINT('Ctrl Pts',(3.90268314407793,5.82466229402444,75.5384710245314));
#142445=CARTESIAN_POINT('Ctrl Pts',(3.98029732391505,5.77265866941902,75.5342185084676));
#142446=CARTESIAN_POINT('Ctrl Pts',(4.05688911733023,5.71909211162802,75.5299659924039));
#142447=CARTESIAN_POINT('Ctrl Pts',(4.13240130821834,5.66399911637841,75.5257134763401));
#142448=CARTESIAN_POINT('Ctrl Pts',(4.27504459599869,5.55992789445191,75.5176804307412));
#142449=CARTESIAN_POINT('Ctrl Pts',(4.41390286247982,5.45035596546751,75.5096473851423));
#142450=CARTESIAN_POINT('Ctrl Pts',(4.5485213107685,5.33559560386512,75.5016143395435));
#142451=CARTESIAN_POINT('Ctrl Pts',(4.68305322113534,5.22090901464186,75.4935864578956));
#142452=CARTESIAN_POINT('Ctrl Pts',(4.81335046072279,5.10104086866301,75.4855585762478));
#142453=CARTESIAN_POINT('Ctrl Pts',(4.93898910745856,4.97634536169926,75.4775306945999));
#142454=CARTESIAN_POINT('Ctrl Pts',(5.06457102710724,4.85170615598569,75.4695064376198));
#142455=CARTESIAN_POINT('Ctrl Pts',(5.18549828237782,4.72224418681249,75.4614821806396));
#142456=CARTESIAN_POINT('Ctrl Pts',(5.30138185291129,4.58835231996442,75.4534579236594));
#142457=CARTESIAN_POINT('Ctrl Pts',(5.4172514119404,4.45447664200721,75.4454346368937));
#142458=CARTESIAN_POINT('Ctrl Pts',(5.52807825533282,4.31617240520348,75.4374113501279));
#142459=CARTESIAN_POINT('Ctrl Pts',(5.63351179532338,4.17386768051557,75.4293880633622));
#142460=CARTESIAN_POINT('Ctrl Pts',(5.73893669597605,4.03157461643016,75.4213654340332));
#142461=CARTESIAN_POINT('Ctrl Pts',(5.83896895847622,3.88528201440496,75.4133428047042));
#142462=CARTESIAN_POINT('Ctrl Pts',(5.93329988997063,3.73544896607818,75.4053201753752));
#142463=CARTESIAN_POINT('Ctrl Pts',(6.02766628317955,3.58555959119234,75.3972945301088));
#142464=CARTESIAN_POINT('Ctrl Pts',(6.11632687090332,3.43212742321844,75.3892688848423));
#142465=CARTESIAN_POINT('Ctrl Pts',(6.19901750485473,3.27563864566967,75.3812432395759));
#142466=CARTESIAN_POINT('Ctrl Pts',(6.24777694154722,3.18336332647866,75.3765108300685));
#142467=CARTESIAN_POINT('Ctrl Pts',(6.29446148932598,3.09002570380226,75.371778420561));
#142468=CARTESIAN_POINT('Ctrl Pts',(6.33902467059603,2.99572909123554,75.3670460110536));
#142469=CARTESIAN_POINT('Ctrl Pts',(6.42418139636258,2.81553569955649,75.3580027496178));
#142470=CARTESIAN_POINT('Ctrl Pts',(6.50163293414364,2.63174597938776,75.3489594881819));
#142471=CARTESIAN_POINT('Ctrl Pts',(6.57110895151811,2.44502632087644,75.339916226746));
#142472=CARTESIAN_POINT('Origin',(0.,0.,50.));
#142473=CARTESIAN_POINT('',(6.57110895151811,2.44502632087643,73.339830038482));
#142474=CARTESIAN_POINT('',(6.57110895151812,2.44502632087642,73.8869619471141));
#142475=CARTESIAN_POINT('',(6.57110895151814,2.44502632087636,50.));
#142476=CARTESIAN_POINT('',(7.01124707280511,0.0064067606328066,75.7735343568825));
#142477=CARTESIAN_POINT('Ctrl Pts',(6.57110895151812,2.44502632087642,73.8869619471141));
#142478=CARTESIAN_POINT('Ctrl Pts',(6.50275899109119,2.62871965495729,73.8958758490847));
#142479=CARTESIAN_POINT('Ctrl Pts',(6.42672848959599,2.80947512617339,73.9047897510554));
#142480=CARTESIAN_POINT('Ctrl Pts',(6.34329324847321,2.98667998392432,73.913703653026));
#142481=CARTESIAN_POINT('Ctrl Pts',(6.2907616291823,3.09824984335786,73.9193159302655));
#142482=CARTESIAN_POINT('Ctrl Pts',(6.23529565958854,3.20841264439689,73.9249282075049));
#142483=CARTESIAN_POINT('Ctrl Pts',(6.17697358078328,3.31702034133128,73.9305404847443));
#142484=CARTESIAN_POINT('Ctrl Pts',(6.09526402854701,3.46918032032569,73.9384033159336));
#142485=CARTESIAN_POINT('Ctrl Pts',(6.00780935259603,3.61854067465666,73.946266147123));
#142486=CARTESIAN_POINT('Ctrl Pts',(5.91483458550851,3.76461928866285,73.9541289783124));
#142487=CARTESIAN_POINT('Ctrl Pts',(5.82193125725678,3.91058566053664,73.9619857679538));
#142488=CARTESIAN_POINT('Ctrl Pts',(5.72351647602113,4.05327498704915,73.9698425575953));
#142489=CARTESIAN_POINT('Ctrl Pts',(5.61986173966912,4.19222859461447,73.9776993472368));
#142490=CARTESIAN_POINT('Ctrl Pts',(5.51626545968203,4.33110383892233,73.9855517060208));
#142491=CARTESIAN_POINT('Ctrl Pts',(5.40743533018594,4.46624725047326,73.9934040648048));
#142492=CARTESIAN_POINT('Ctrl Pts',(5.2936866735676,4.5972282915462,74.0012564235888));
#142493=CARTESIAN_POINT('Ctrl Pts',(5.17996487433408,4.72817840646733,74.0091069283393));
#142494=CARTESIAN_POINT('Ctrl Pts',(5.06132710273039,4.85496781378237,74.0169574330898));
#142495=CARTESIAN_POINT('Ctrl Pts',(4.93812951377572,4.97719835526747,74.0248079378403));
#142496=CARTESIAN_POINT('Ctrl Pts',(4.81495174343018,5.09940923371089,74.032657179692));
#142497=CARTESIAN_POINT('Ctrl Pts',(4.68721588893935,5.21706243968238,74.0405064215437));
#142498=CARTESIAN_POINT('Ctrl Pts',(4.55531523914614,5.32979639709651,74.0483556633954));
#142499=CARTESIAN_POINT('Ctrl Pts',(4.4233701494424,5.44256833678737,74.0562075498104));
#142500=CARTESIAN_POINT('Ctrl Pts',(4.28725775191128,5.5504174692811,74.0640594362253));
#142501=CARTESIAN_POINT('Ctrl Pts',(4.14740486202403,5.65302215394204,74.0719113226402));
#142502=CARTESIAN_POINT('Ctrl Pts',(4.04471262570295,5.72836349678697,74.0776768651037));
#142503=CARTESIAN_POINT('Ctrl Pts',(3.9400043080111,5.80087797358243,74.0834424075672));
#142504=CARTESIAN_POINT('Ctrl Pts',(3.83345880483194,5.87045314725844,74.0892079500307));
#142505=CARTESIAN_POINT('Ctrl Pts',(3.65503166326317,5.98696767854079,74.0988632543904));
#142506=CARTESIAN_POINT('Ctrl Pts',(3.47154285547476,6.09517901204123,74.1085185587502));
#142507=CARTESIAN_POINT('Ctrl Pts',(3.28371893133776,6.19474103917783,74.1181738631099));
#142508=CARTESIAN_POINT('Ctrl Pts',(3.09485449789795,6.29485462126632,74.1278826560444));
#142509=CARTESIAN_POINT('Ctrl Pts',(2.90160685091477,6.38622282672841,74.1375914489789));
#142510=CARTESIAN_POINT('Ctrl Pts',(2.70472898750889,6.46854447821371,74.1473002419134));
#142511=CARTESIAN_POINT('Ctrl Pts',(2.50690373110709,6.55126226847603,74.1570557543839));
#142512=CARTESIAN_POINT('Ctrl Pts',(2.30541328557382,6.62484623515333,74.1668112668544));
#142513=CARTESIAN_POINT('Ctrl Pts',(2.10103509689751,6.68904164167819,74.1765667793249));
#142514=CARTESIAN_POINT('Ctrl Pts',(1.89645454237132,6.75330061153182,74.1863319512536));
#142515=CARTESIAN_POINT('Ctrl Pts',(1.68898056535691,6.80815242604585,74.1960971231823));
#142516=CARTESIAN_POINT('Ctrl Pts',(1.47940575007312,6.85339223955193,74.205862295111));
#142517=CARTESIAN_POINT('Ctrl Pts',(1.27011668529535,6.89857036959865,74.2156141524493));
#142518=CARTESIAN_POINT('Ctrl Pts',(1.05873254434566,6.93416268434599,74.2253660097876));
#142519=CARTESIAN_POINT('Ctrl Pts',(0.846054864409197,6.96001564142708,
74.2351178671259));
#142520=CARTESIAN_POINT('Ctrl Pts',(0.753311993082726,6.97128940307755,
74.2393703831896));
#142521=CARTESIAN_POINT('Ctrl Pts',(0.660323296795574,6.98071178572122,
74.2436228992534));
#142522=CARTESIAN_POINT('Ctrl Pts',(0.567155942729901,6.98827308418369,
74.2478754153171));
#142523=CARTESIAN_POINT('Ctrl Pts',(0.391161874201906,7.00255645300005,
74.2559084609159));
#142524=CARTESIAN_POINT('Ctrl Pts',(0.214444101747809,7.0102020196953,74.2639415065147));
#142525=CARTESIAN_POINT('Ctrl Pts',(0.037550999544158,7.01114944106409,
74.2719745521135));
#142526=CARTESIAN_POINT('Ctrl Pts',(-0.139228388962058,7.01209625339394,
74.2800024337614));
#142527=CARTESIAN_POINT('Ctrl Pts',(-0.316182517833347,7.00635348929289,
74.2880303154091));
#142528=CARTESIAN_POINT('Ctrl Pts',(-0.492759034395258,6.99391271725076,
74.296058197057));
#142529=CARTESIAN_POINT('Ctrl Pts',(-0.669255824920555,6.98147756233975,
74.3040824540371));
#142530=CARTESIAN_POINT('Ctrl Pts',(-0.845374977708918,6.96235044675942,
74.3121067110173));
#142531=CARTESIAN_POINT('Ctrl Pts',(-1.0205653345377,6.93657501656545,74.3201309679974));
#142532=CARTESIAN_POINT('Ctrl Pts',(-1.19573450906741,6.9108027028836,74.3281542547631));
#142533=CARTESIAN_POINT('Ctrl Pts',(-1.36997474774586,6.87838372141755,
74.3361775415289));
#142534=CARTESIAN_POINT('Ctrl Pts',(-1.54274102340186,6.83941347611131,
74.3442008282946));
#142535=CARTESIAN_POINT('Ctrl Pts',(-1.71549314240272,6.80044642406904,
74.3522234576236));
#142536=CARTESIAN_POINT('Ctrl Pts',(-1.88677118218473,6.7549292620711,74.3602460869525));
#142537=CARTESIAN_POINT('Ctrl Pts',(-2.05604160109687,6.70300824235351,
74.3682687162814));
#142538=CARTESIAN_POINT('Ctrl Pts',(-2.22537565363579,6.65106770402887,
74.3762943615479));
#142539=CARTESIAN_POINT('Ctrl Pts',(-2.39270022781168,6.59271860925155,
74.3843200068143));
#142540=CARTESIAN_POINT('Ctrl Pts',(-2.55749783942897,6.52815681213435,
74.3923456520807));
#142541=CARTESIAN_POINT('Ctrl Pts',(-2.65467255350605,6.4900872423536,74.3970780615883));
#142542=CARTESIAN_POINT('Ctrl Pts',(-2.75096898407742,6.44985844336226,
74.401810471096));
#142543=CARTESIAN_POINT('Ctrl Pts',(-2.84628447904245,6.40751833605352,
74.4065428806036));
#142544=CARTESIAN_POINT('Ctrl Pts',(-3.02211645732264,6.32941199215401,
74.4152729294383));
#142545=CARTESIAN_POINT('Ctrl Pts',(-3.1946970624525,6.24407939971055,74.4240029782731));
#142546=CARTESIAN_POINT('Ctrl Pts',(-3.36345017752929,6.15181513585854,
74.4327330271079));
#142547=CARTESIAN_POINT('Ctrl Pts',(-3.53225208777979,6.05952419367955,
74.4414656002472));
#142548=CARTESIAN_POINT('Ctrl Pts',(-3.69722405853467,5.96029771081409,
74.4501981733864));
#142549=CARTESIAN_POINT('Ctrl Pts',(-3.85781566581852,5.85447562562739,
74.4589307465257));
#142550=CARTESIAN_POINT('Ctrl Pts',(-4.02068873323303,5.74715016879892,
74.4677873798061));
#142551=CARTESIAN_POINT('Ctrl Pts',(-4.17905578647582,5.63304043873274,
74.4766440130864));
#142552=CARTESIAN_POINT('Ctrl Pts',(-4.33237374851898,5.51254607832385,
74.4855006463668));
#142553=CARTESIAN_POINT('Ctrl Pts',(-4.4836403262669,5.3936639245691,74.4942387784736));
#142554=CARTESIAN_POINT('Ctrl Pts',(-4.62999188267125,5.26856712114457,
74.5029769105805));
#142555=CARTESIAN_POINT('Ctrl Pts',(-4.77094005591142,5.13768017157549,
74.5117150426874));
#142556=CARTESIAN_POINT('Ctrl Pts',(-4.9147554078106,5.00413070953874,74.5206309265545));
#142557=CARTESIAN_POINT('Ctrl Pts',(-5.05294497011473,4.86455320967521,
74.5295468104216));
#142558=CARTESIAN_POINT('Ctrl Pts',(-5.18502865945245,4.71943898818034,
74.5384626942887));
#142559=CARTESIAN_POINT('Ctrl Pts',(-5.31711234879022,4.57432476668543,
74.5473785781558));
#142560=CARTESIAN_POINT('Ctrl Pts',(-5.44308996609929,4.42367405129665,
74.5562944620229));
#142561=CARTESIAN_POINT('Ctrl Pts',(-5.56252360649307,4.26801566183951,
74.56521034589));
#142562=CARTESIAN_POINT('Ctrl Pts',(-5.67961034567175,4.1154159990707,74.5739510303861));
#142563=CARTESIAN_POINT('Ctrl Pts',(-5.79042033806903,3.95798743193976,
74.5826917148821));
#142564=CARTESIAN_POINT('Ctrl Pts',(-5.89457869846284,3.79625717386587,
74.5914323993782));
#142565=CARTESIAN_POINT('Ctrl Pts',(-5.99871831903719,3.63455601375231,
74.6001715112799));
#142566=CARTESIAN_POINT('Ctrl Pts',(-6.09620854939378,3.46855493842968,
74.6089106231816));
#142567=CARTESIAN_POINT('Ctrl Pts',(-6.18671818026086,3.29880959143291,
74.6176497350833));
#142568=CARTESIAN_POINT('Ctrl Pts',(-6.27840049366468,3.12686494915442,
74.6265020747577));
#142569=CARTESIAN_POINT('Ctrl Pts',(-6.36291990525096,2.95107857490478,
74.6353544144322));
#142570=CARTESIAN_POINT('Ctrl Pts',(-6.43997990603593,2.77205435955961,
74.6442067541066));
#142571=CARTESIAN_POINT('Ctrl Pts',(-6.51601526206472,2.59541057792342,
74.6529413867562));
#142572=CARTESIAN_POINT('Ctrl Pts',(-6.58478824835034,2.41561478930709,
74.6616760194057));
#142573=CARTESIAN_POINT('Ctrl Pts',(-6.64606178442928,2.23326875231099,
74.6704106520553));
#142574=CARTESIAN_POINT('Ctrl Pts',(-6.70857389445685,2.04723680022803,
74.6793218452422));
#142575=CARTESIAN_POINT('Ctrl Pts',(-6.7632800266812,1.8585506693742,74.688233038429));
#142576=CARTESIAN_POINT('Ctrl Pts',(-6.80998104714929,1.66786831013946,
74.6971442316159));
#142577=CARTESIAN_POINT('Ctrl Pts',(-6.8566820676174,1.47718595090465,74.7060554248027));
#142578=CARTESIAN_POINT('Ctrl Pts',(-6.89537789113214,1.28450765451162,
74.7149666179896));
#142579=CARTESIAN_POINT('Ctrl Pts',(-6.92592396116717,1.09050623410895,
74.7238778111764));
#142580=CARTESIAN_POINT('Ctrl Pts',(-6.95343458915171,0.915783237040895,
74.7319034760289));
#142581=CARTESIAN_POINT('Ctrl Pts',(-6.97434683907087,0.739906637123656,
74.7399291408814));
#142582=CARTESIAN_POINT('Ctrl Pts',(-6.98857508167542,0.563422479393069,
74.7479548057339));
#142583=CARTESIAN_POINT('Ctrl Pts',(-7.00279880858477,0.386994333405122,
74.7559779234372));
#142584=CARTESIAN_POINT('Ctrl Pts',(-7.01034272214564,0.209959378448671,
74.7640010411405));
#142585=CARTESIAN_POINT('Ctrl Pts',(-7.01117295096855,0.0328696532836382,
74.7720241588438));
#142586=CARTESIAN_POINT('Ctrl Pts',(-7.01200307509234,-0.144197739317557,
74.7800462647618));
#142587=CARTESIAN_POINT('Ctrl Pts',(-7.00612119978994,-0.321319521904239,
74.7880683706797));
#142588=CARTESIAN_POINT('Ctrl Pts',(-6.99354556022944,-0.497942827536565,
74.7960904765977));
#142589=CARTESIAN_POINT('Ctrl Pts',(-6.98096524751879,-0.67463176698591,
74.8041155635573));
#142590=CARTESIAN_POINT('Ctrl Pts',(-6.96168622452595,-0.850821493238382,
74.812140650517));
#142591=CARTESIAN_POINT('Ctrl Pts',(-6.93577872499585,-1.02596298198083,
74.8201657374766));
#142592=CARTESIAN_POINT('Ctrl Pts',(-6.90986612311346,-1.20113896396232,
74.8281924049369));
#142593=CARTESIAN_POINT('Ctrl Pts',(-6.87732250638558,-1.37526593583321,
74.8362190723972));
#142594=CARTESIAN_POINT('Ctrl Pts',(-6.83826936652441,-1.5478044557869,
74.8442457398576));
#142595=CARTESIAN_POINT('Ctrl Pts',(-6.79918487494009,-1.72048148905682,
74.8522788510982));
#142596=CARTESIAN_POINT('Ctrl Pts',(-6.75358051291989,-1.8915671681038,
74.8603119623389));
#142597=CARTESIAN_POINT('Ctrl Pts',(-6.70162800407903,-2.06053601216861,
74.8683450735796));
#142598=CARTESIAN_POINT('Ctrl Pts',(-6.6710156985963,-2.16009859320625,
74.8730784745407));
#142599=CARTESIAN_POINT('Ctrl Pts',(-6.63820025694383,-2.25892652539235,
74.8778118755017));
#142600=CARTESIAN_POINT('Ctrl Pts',(-6.60322465143507,-2.35691551931336,
74.8825452764628));
#142601=CARTESIAN_POINT('Ctrl Pts',(-6.53117381556781,-2.55877589642768,
74.8922962297567));
#142602=CARTESIAN_POINT('Ctrl Pts',(-6.44991144028724,-2.75719415863265,
74.9020471830505));
#142603=CARTESIAN_POINT('Ctrl Pts',(-6.35977319227492,-2.95142533453267,
74.9117981363444));
#142604=CARTESIAN_POINT('Ctrl Pts',(-6.269505083206,-3.14593633688021,74.9215631377158));
#142605=CARTESIAN_POINT('Ctrl Pts',(-6.17033553918559,-3.33624815153717,
74.9313281390871));
#142606=CARTESIAN_POINT('Ctrl Pts',(-6.06264768007091,-3.52163735637712,
74.9410931404585));
#142607=CARTESIAN_POINT('Ctrl Pts',(-5.95513931430501,-3.70671755582428,
74.9508418655959));
#142608=CARTESIAN_POINT('Ctrl Pts',(-5.83914102905413,-3.88689151107827,
74.9605905907332));
#142609=CARTESIAN_POINT('Ctrl Pts',(-5.71507941116065,-4.06146450022989,
74.9703393158706));
#142610=CARTESIAN_POINT('Ctrl Pts',(-5.59135829430299,-4.23555835421754,
74.9800612845376));
#142611=CARTESIAN_POINT('Ctrl Pts',(-5.45961804830347,-4.40408189819558,
74.9897832532045));
#142612=CARTESIAN_POINT('Ctrl Pts',(-5.32032672712792,-4.56637165363358,
74.9995052218715));
#142613=CARTESIAN_POINT('Ctrl Pts',(-5.18195706024321,-4.72758758014818,
75.0091628628111));
#142614=CARTESIAN_POINT('Ctrl Pts',(-5.03613592336463,-4.88265188593332,
75.0188205037506));
#142615=CARTESIAN_POINT('Ctrl Pts',(-4.8833664542797,-5.03094013438003,
75.0284781446902));
#142616=CARTESIAN_POINT('Ctrl Pts',(-4.81621901306715,-5.09611792484255,
75.0327230103765));
#142617=CARTESIAN_POINT('Ctrl Pts',(-4.7477297973699,-5.15998698883543,
75.0369678760629));
#142618=CARTESIAN_POINT('Ctrl Pts',(-4.67794426613898,-5.22249595551757,
75.0412127417492));
#142619=CARTESIAN_POINT('Ctrl Pts',(-4.54886001342036,-5.33812054287909,
75.0490645887632));
#142620=CARTESIAN_POINT('Ctrl Pts',(-4.41539090845857,-5.44904124456751,
75.0569164357772));
#142621=CARTESIAN_POINT('Ctrl Pts',(-4.27793297717984,-5.55490017959434,
75.0647682827911));
#142622=CARTESIAN_POINT('Ctrl Pts',(-4.14051402785882,-5.66072909388326,
75.0726179030848));
#142623=CARTESIAN_POINT('Ctrl Pts',(-3.99910880429848,-5.76149886439636,
75.0804675233784));
#142624=CARTESIAN_POINT('Ctrl Pts',(-3.85414661408296,-5.85689170462053,
75.0883171436721));
#142625=CARTESIAN_POINT('Ctrl Pts',(-3.70919599724444,-5.95227692894638,
75.0961661372739));
#142626=CARTESIAN_POINT('Ctrl Pts',(-3.56068929814396,-6.04228586849202,
75.1040151308758));
#142627=CARTESIAN_POINT('Ctrl Pts',(-3.40908478907484,-6.12664406207824,
75.1118641244776));
#142628=CARTESIAN_POINT('Ctrl Pts',(-3.25740352708227,-6.21104496374759,
75.1197170917951));
#142629=CARTESIAN_POINT('Ctrl Pts',(-3.10262165528774,-6.28978921769999,
75.1275700591125));
#142630=CARTESIAN_POINT('Ctrl Pts',(-2.94522233258021,-6.36264818877885,
75.13542302643));
#142631=CARTESIAN_POINT('Ctrl Pts',(-2.78778303573294,-6.43552566358849,
75.1432779881373));
#142632=CARTESIAN_POINT('Ctrl Pts',(-2.62772531557513,-6.50251473051098,
75.1511329498446));
#142633=CARTESIAN_POINT('Ctrl Pts',(-2.46555167505598,-6.56343519051789,
75.158987911552));
#142634=CARTESIAN_POINT('Ctrl Pts',(-2.30321706364293,-6.62441611917355,
75.1668506699654));
#142635=CARTESIAN_POINT('Ctrl Pts',(-2.1387626988558,-6.67931628951148,
75.1747134283787));
#142636=CARTESIAN_POINT('Ctrl Pts',(-1.97270613489017,-6.72800543013059,
75.1825761867921));
#142637=CARTESIAN_POINT('Ctrl Pts',(-1.85088942234223,-6.76372308503902,
75.18834419354));
#142638=CARTESIAN_POINT('Ctrl Pts',(-1.72821079584976,-6.79609933591651,
75.1941122002878));
#142639=CARTESIAN_POINT('Ctrl Pts',(-1.60487744077161,-6.82510036282269,
75.1998802070357));
#142640=CARTESIAN_POINT('Ctrl Pts',(-1.42573495907739,-6.86722453862543,
75.2082582734767));
#142641=CARTESIAN_POINT('Ctrl Pts',(-1.24481405199275,-6.90231937438806,
75.2166363399177));
#142642=CARTESIAN_POINT('Ctrl Pts',(-1.06269237914407,-6.9302461334219,
75.2250144063587));
#142643=CARTESIAN_POINT('Ctrl Pts',(-0.88069523893112,-6.95815379646976,
75.2333867439775));
#142644=CARTESIAN_POINT('Ctrl Pts',(-0.69749929381418,-6.97890310515552,
75.2417590815962));
#142645=CARTESIAN_POINT('Ctrl Pts',(-0.513692558389837,-6.99240634674179,
75.250131419215));
#142646=CARTESIAN_POINT('Ctrl Pts',(-0.329984552447882,-7.00590233523122,
75.2584992597376));
#142647=CARTESIAN_POINT('Ctrl Pts',(-0.145666737463464,-7.0121599931371,
75.2668671002602));
#142648=CARTESIAN_POINT('Ctrl Pts',(0.038667121992827,-7.01114337438458,
75.2752349407828));
#142649=CARTESIAN_POINT('Ctrl Pts',(0.222928972401273,-7.0101271527688,
75.2835995124528));
#142650=CARTESIAN_POINT('Ctrl Pts',(0.40720652655978,-7.00184232297566,
75.2919640841227));
#142651=CARTESIAN_POINT('Ctrl Pts',(0.590904923471322,-6.98630502725993,
75.3003286557926));
#142652=CARTESIAN_POINT('Ctrl Pts',(0.77455844858733,-6.9707715268215,75.3086911842583));
#142653=CARTESIAN_POINT('Ctrl Pts',(0.957632771390947,-6.94798912146856,
75.317053712724));
#142654=CARTESIAN_POINT('Ctrl Pts',(1.1395365979978,-6.91802593984177,75.3254162411897));
#142655=CARTESIAN_POINT('Ctrl Pts',(1.32145494109673,-6.88806036705973,
75.3337794370112));
#142656=CARTESIAN_POINT('Ctrl Pts',(1.50220227609893,-6.85091292059187,
75.3421426328327));
#142657=CARTESIAN_POINT('Ctrl Pts',(1.68119520106125,-6.80670325917243,
75.3505058286542));
#142658=CARTESIAN_POINT('Ctrl Pts',(1.8602003329826,-6.76249058274263,75.3588695948289));
#142659=CARTESIAN_POINT('Ctrl Pts',(2.03745049700454,-6.71121480962025,
75.3672333610036));
#142660=CARTESIAN_POINT('Ctrl Pts',(2.21237503716852,-6.65304616378194,
75.3755971271783));
#142661=CARTESIAN_POINT('Ctrl Pts',(2.3873348283923,-6.59486579570951,75.3839625788319));
#142662=CARTESIAN_POINT('Ctrl Pts',(2.55996774924811,-6.52978988885687,
75.3923280304855));
#142663=CARTESIAN_POINT('Ctrl Pts',(2.72972038082471,-6.45803787578009,
75.4006934821391));
#142664=CARTESIAN_POINT('Ctrl Pts',(2.89952986222396,-6.38626183309517,
75.409061735366));
#142665=CARTESIAN_POINT('Ctrl Pts',(3.06645682817716,-6.30780535386422,
75.4174299885929));
#142666=CARTESIAN_POINT('Ctrl Pts',(3.22996944408843,-6.22293531645276,
75.4257982418199));
#142667=CARTESIAN_POINT('Ctrl Pts',(3.39363365952154,-6.13798659240899,
75.4341742536114));
#142668=CARTESIAN_POINT('Ctrl Pts',(3.55387690700227,-6.0466125793586,75.4425502654029));
#142669=CARTESIAN_POINT('Ctrl Pts',(3.71019241278406,-5.94912588727282,
75.4509262771944));
#142670=CARTESIAN_POINT('Ctrl Pts',(3.86658457762135,-5.85159138650868,
75.4593063966855));
#142671=CARTESIAN_POINT('Ctrl Pts',(4.01904488418193,-5.74793840807308,
75.4676865161767));
#142672=CARTESIAN_POINT('Ctrl Pts',(4.16709647390175,-5.63852228333768,
75.4760666356679));
#142673=CARTESIAN_POINT('Ctrl Pts',(4.31531723131679,-5.52898113681984,
75.4844563305071));
#142674=CARTESIAN_POINT('Ctrl Pts',(4.45911894531299,-5.41366388624698,
75.4928460253463));
#142675=CARTESIAN_POINT('Ctrl Pts',(4.59805767418991,-5.29296629380192,
75.5012357201855));
#142676=CARTESIAN_POINT('Ctrl Pts',(4.68626747551973,-5.21633747520954,
75.5065621926599));
#142677=CARTESIAN_POINT('Ctrl Pts',(4.77251783043358,-5.13754074699948,
75.5118886651343));
#142678=CARTESIAN_POINT('Ctrl Pts',(4.85670300396802,-5.05668493123193,
75.5172151376086));
#142679=CARTESIAN_POINT('Ctrl Pts',(4.98916989127781,-4.92945684835293,
75.5255964380134));
#142680=CARTESIAN_POINT('Ctrl Pts',(5.11678882345246,-4.79687213146762,
75.5339777384181));
#142681=CARTESIAN_POINT('Ctrl Pts',(5.23911568247115,-4.65932328006813,
75.5423590388229));
#142682=CARTESIAN_POINT('Ctrl Pts',(5.36128751010322,-4.52194875170229,
75.5507297171563));
#142683=CARTESIAN_POINT('Ctrl Pts',(5.47818041481491,-4.37962286960814,
75.5591003954898));
#142684=CARTESIAN_POINT('Ctrl Pts',(5.5893857073991,-4.23277615477391,75.5674710738232));
#142685=CARTESIAN_POINT('Ctrl Pts',(5.70046480106886,-4.08609608574916,
75.5758322528738));
#142686=CARTESIAN_POINT('Ctrl Pts',(5.80586895046219,-3.93490566899011,
75.5841934319245));
#142687=CARTESIAN_POINT('Ctrl Pts',(5.90522820807114,-3.77967014077961,
75.5925546109751));
#142688=CARTESIAN_POINT('Ctrl Pts',(6.00445853532294,-3.62463604897852,
75.6009049404097));
#142689=CARTESIAN_POINT('Ctrl Pts',(6.09765944060215,-3.46556759009271,
75.6092552698443));
#142690=CARTESIAN_POINT('Ctrl Pts',(6.18450299894852,-3.30296067468216,
75.6176055992788));
#142691=CARTESIAN_POINT('Ctrl Pts',(6.27127973637222,-3.14047887556491,
75.6259495036344));
#142692=CARTESIAN_POINT('Ctrl Pts',(6.35170872122839,-2.97446433341784,
75.6342934079901));
#142693=CARTESIAN_POINT('Ctrl Pts',(6.42550628435155,-2.80544034908225,
75.6426373123457));
#142694=CARTESIAN_POINT('Ctrl Pts',(6.49924457281158,-2.63655212586543,
75.6509745148253));
#142695=CARTESIAN_POINT('Ctrl Pts',(6.56636193155825,-2.46465958063462,
75.6593117173048));
#142696=CARTESIAN_POINT('Ctrl Pts',(6.62662138123789,-2.29030906914783,
75.6676489197844));
#142697=CARTESIAN_POINT('Ctrl Pts',(6.64645845945428,-2.23291384314066,
75.6703934808212));
#142698=CARTESIAN_POINT('Ctrl Pts',(6.66555273342515,-2.17525242693332,
75.6731380418581));
#142699=CARTESIAN_POINT('Ctrl Pts',(6.68389688264667,-2.11734480532722,
75.6758826028949));
#142700=CARTESIAN_POINT('Ctrl Pts',(6.73828743675348,-1.94564822849889,
75.6840202490606));
#142701=CARTESIAN_POINT('Ctrl Pts',(6.7860549329571,-1.77186261854291,75.6921578952262));
#142702=CARTESIAN_POINT('Ctrl Pts',(6.82705109833968,-1.5965587565633,75.7002955413919));
#142703=CARTESIAN_POINT('Ctrl Pts',(6.86695367326183,-1.42593120099797,
75.7082161123229));
#142704=CARTESIAN_POINT('Ctrl Pts',(6.90044152218364,-1.25386574377441,
75.716136683254));
#142705=CARTESIAN_POINT('Ctrl Pts',(6.92742985515551,-1.08089877620435,
75.724057254185));
#142706=CARTESIAN_POINT('Ctrl Pts',(6.95552767229749,-0.900821176322602,
75.7323034379679));
#142707=CARTESIAN_POINT('Ctrl Pts',(6.97658018198766,-0.719766819359412,
75.7405496217509));
#142708=CARTESIAN_POINT('Ctrl Pts',(6.99055149854564,-0.538345900589294,
75.7487958055338));
#142709=CARTESIAN_POINT('Ctrl Pts',(7.00452281510362,-0.356924981819176,
75.7570419893167));
#142710=CARTESIAN_POINT('Ctrl Pts',(7.01141296534025,-0.175137957217851,
75.7652881730996));
#142711=CARTESIAN_POINT('Ctrl Pts',(7.01124707280511,0.00640676063271148,
75.7735343568825));
#142712=CARTESIAN_POINT('Ctrl Pts',(7.01124707280455,0.00640676124637189,
75.7735343569104));
#142713=CARTESIAN_POINT('Ctrl Pts',(7.01104249227247,0.23028971888088,75.7837036421222));
#142714=CARTESIAN_POINT('Ctrl Pts',(7.00010998406542,0.453798136459291,
75.7938729273341));
#142715=CARTESIAN_POINT('Ctrl Pts',(6.97858319956023,0.676020036179168,
75.8040422125459));
#142716=CARTESIAN_POINT('Ctrl Pts',(6.95705641505505,0.898241935899045,
75.8142114977577));
#142717=CARTESIAN_POINT('Ctrl Pts',(6.92493548555935,1.11917735600817,75.8243807829695));
#142718=CARTESIAN_POINT('Ctrl Pts',(6.8824094301673,1.33793385413639,75.8345500681813));
#142719=CARTESIAN_POINT('Ctrl Pts',(6.84585080011827,1.5259935698133,75.8432923588192));
#142720=CARTESIAN_POINT('Ctrl Pts',(6.80154666212197,1.71272100934492,75.8520346494571));
#142721=CARTESIAN_POINT('Ctrl Pts',(6.74961410355704,1.89745514191085,75.860776940095));
#142722=CARTESIAN_POINT('Ctrl Pts',(6.69768154499209,2.08218927447684,75.8695192307329));
#142723=CARTESIAN_POINT('Ctrl Pts',(6.6381206211002,2.26492969856719,75.8782615213709));
#142724=CARTESIAN_POINT('Ctrl Pts',(6.57110895151814,2.44502632087635,75.8870038120088));
#142725=CARTESIAN_POINT('',(7.01124999042383,-0.000366444890689146,75.2264656430566));
#142726=CARTESIAN_POINT('Ctrl Pts',(6.57110895151811,2.44502632087644,75.339916226746));
#142727=CARTESIAN_POINT('Ctrl Pts',(6.63820287688893,2.26470863274675,75.3311830274232));
#142728=CARTESIAN_POINT('Ctrl Pts',(6.69785902018697,2.08165885386196,75.3224498281004));
#142729=CARTESIAN_POINT('Ctrl Pts',(6.74988410723788,1.89649442428854,75.3137166287776));
#142730=CARTESIAN_POINT('Ctrl Pts',(6.80193302667208,1.71124517198998,75.3049794288281));
#142731=CARTESIAN_POINT('Ctrl Pts',(6.84634382896498,1.52387959651581,75.2962422288786));
#142732=CARTESIAN_POINT('Ctrl Pts',(6.88297349805567,1.3350289837915,75.287505028929));
#142733=CARTESIAN_POINT('Ctrl Pts',(6.91960826284139,1.1461520993275,75.2787666135138));
#142734=CARTESIAN_POINT('Ctrl Pts',(6.94845968467338,0.955790034550496,
75.2700281980986));
#142735=CARTESIAN_POINT('Ctrl Pts',(6.96943605429437,0.76458331632448,75.2612897826833));
#142736=CARTESIAN_POINT('Ctrl Pts',(6.9904174952856,0.573330370840038,75.2525492546175));
#142737=CARTESIAN_POINT('Ctrl Pts',(7.00352005089385,0.38123263605352,75.2438087265516));
#142738=CARTESIAN_POINT('Ctrl Pts',(7.00870385634683,0.188936011731862,
75.2350681984858));
#142739=CARTESIAN_POINT('Ctrl Pts',(7.01040451536259,0.125848962879511,
75.2322006800204));
#142740=CARTESIAN_POINT('Ctrl Pts',(7.01125328872049,0.0627405290793296,
75.2293331615549));
#142741=CARTESIAN_POINT('Ctrl Pts',(7.01124999042387,-0.000366444165664637,
75.2264656430895));
#142742=CARTESIAN_POINT('Ctrl Pts',(7.01124999042383,-0.000366444890591926,
75.2264656430566));
#142743=CARTESIAN_POINT('Ctrl Pts',(7.01124305565536,-0.133050503537697,
75.2204366106267));
#142744=CARTESIAN_POINT('Ctrl Pts',(7.00746885027525,-0.26572305004299,
75.2144075781969));
#142745=CARTESIAN_POINT('Ctrl Pts',(6.99993417826155,-0.39818094191683,
75.2083785457671));
#142746=CARTESIAN_POINT('Ctrl Pts',(6.98901066912309,-0.590213851871724,
75.1996378612723));
#142747=CARTESIAN_POINT('Ctrl Pts',(6.97018003265678,-0.781807211055622,
75.1908971767776));
#142748=CARTESIAN_POINT('Ctrl Pts',(6.94350245760761,-0.972316915258118,
75.1821564922828));
#142749=CARTESIAN_POINT('Ctrl Pts',(6.91682968229739,-1.16279234359993,
75.1734173803823));
#142750=CARTESIAN_POINT('Ctrl Pts',(6.88231282582201,-1.35218423527349,
75.1646782684819));
#142751=CARTESIAN_POINT('Ctrl Pts',(6.84006372184559,-1.5398554619158,75.1559391565815));
#142752=CARTESIAN_POINT('Ctrl Pts',(6.79726721990968,-1.72995823945147,
75.1470868169064));
#142753=CARTESIAN_POINT('Ctrl Pts',(6.74653674960314,-1.91829517075989,
75.1382344772314));
#142754=CARTESIAN_POINT('Ctrl Pts',(6.68804192720558,-2.1042152319666,75.1293821375563));
#142755=CARTESIAN_POINT('Ctrl Pts',(6.63032489371786,-2.28766316733728,
75.120647504908));
#142756=CARTESIAN_POINT('Ctrl Pts',(6.56504880416474,-2.46875784249007,
75.1119128722598));
#142757=CARTESIAN_POINT('Ctrl Pts',(6.49242690110756,-2.64688864447957,
75.1031782396115));
#142758=CARTESIAN_POINT('Ctrl Pts',(6.41833702991177,-2.8286201554951,75.094267046423));
#142759=CARTESIAN_POINT('Ctrl Pts',(6.3366012975286,-3.00726641754748,75.0853558532346));
#142760=CARTESIAN_POINT('Ctrl Pts',(6.24749837444822,-3.18219902328042,
75.0764446600462));
#142761=CARTESIAN_POINT('Ctrl Pts',(6.15839545136785,-3.35713162901335,
75.0675334668577));
#142762=CARTESIAN_POINT('Ctrl Pts',(6.06192546316565,-3.52835030220223,
75.0586222736693));
#142763=CARTESIAN_POINT('Ctrl Pts',(5.95841812638889,-3.69525100549615,
75.0497110804809));
#142764=CARTESIAN_POINT('Ctrl Pts',(5.86519658161795,-3.8455663538465,75.0416854156281));
#142765=CARTESIAN_POINT('Ctrl Pts',(5.76622355082883,-3.99244807420047,
75.0336597507752));
#142766=CARTESIAN_POINT('Ctrl Pts',(5.66179063329981,-4.13542662698524,
75.0256340859224));
#142767=CARTESIAN_POINT('Ctrl Pts',(5.55739086021743,-4.27835980188414,
75.0176109682188));
#142768=CARTESIAN_POINT('Ctrl Pts',(5.44753486626134,-4.41739197982342,
75.0095878505151));
#142769=CARTESIAN_POINT('Ctrl Pts',(5.33255737107235,-4.55208286905258,
75.0015647328115));
#142770=CARTESIAN_POINT('Ctrl Pts',(5.21759437555166,-4.68675677258193,
74.9935426268932));
#142771=CARTESIAN_POINT('Ctrl Pts',(5.09751140366893,-4.81709019956761,
74.985520520975));
#142772=CARTESIAN_POINT('Ctrl Pts',(4.97268318744038,-4.94267624671572,
74.9774984150567));
#142773=CARTESIAN_POINT('Ctrl Pts',(4.84780858462505,-5.06830896206314,
74.9694733280968));
#142774=CARTESIAN_POINT('Ctrl Pts',(4.71818547138304,-5.189190511028,74.9614482411368));
#142775=CARTESIAN_POINT('Ctrl Pts',(4.58422546114696,-5.30495084650857,
74.9534231541769));
#142776=CARTESIAN_POINT('Ctrl Pts',(4.45023906815718,-5.42073398040796,
74.9453964867162));
#142777=CARTESIAN_POINT('Ctrl Pts',(4.31191435971892,-5.53139365852342,
74.9373698192556));
#142778=CARTESIAN_POINT('Ctrl Pts',(4.16969552258898,-5.63660055453652,
74.9293431517949));
#142779=CARTESIAN_POINT('Ctrl Pts',(4.02736251267753,-5.74189191027517,
74.9213100405539));
#142780=CARTESIAN_POINT('Ctrl Pts',(3.88112943045361,-5.84172153050869,
74.9132769293129));
#142781=CARTESIAN_POINT('Ctrl Pts',(3.73146940036782,-5.93580345670396,
74.9052438180719));
#142782=CARTESIAN_POINT('Ctrl Pts',(3.64328427399438,-5.99123994529901,
74.9005104171127));
#142783=CARTESIAN_POINT('Ctrl Pts',(3.55390981724565,-6.04468168800366,
74.8957770161535));
#142784=CARTESIAN_POINT('Ctrl Pts',(3.46344666392992,-6.09607773643125,
74.8910436151943));
#142785=CARTESIAN_POINT('Ctrl Pts',(3.27708975261288,-6.20195519579238,
74.8812926619006));
#142786=CARTESIAN_POINT('Ctrl Pts',(3.08600197742468,-6.29921177698256,
74.8715417086069));
#142787=CARTESIAN_POINT('Ctrl Pts',(2.89092393913194,-6.3875022771545,74.8617907553132));
#142788=CARTESIAN_POINT('Ctrl Pts',(2.69556485432981,-6.4759199763546,74.8520257539421));
#142789=CARTESIAN_POINT('Ctrl Pts',(2.49620404248284,-6.55534574016212,
74.842260752571));
#142790=CARTESIAN_POINT('Ctrl Pts',(2.2936039834245,-6.62548166775211,74.8324957511999));
#142791=CARTESIAN_POINT('Ctrl Pts',(2.09134161668606,-6.6955006932829,74.8227470260628));
#142792=CARTESIAN_POINT('Ctrl Pts',(1.88585082927563,-6.75626081688636,
74.8129983009257));
#142793=CARTESIAN_POINT('Ctrl Pts',(1.67790829224755,-6.80751425450633,
74.8032495757885));
#142794=CARTESIAN_POINT('Ctrl Pts',(1.47053647685398,-6.85862702131354,
74.7935276071218));
#142795=CARTESIAN_POINT('Ctrl Pts',(1.2607263841683,-6.90028518132652,74.7838056384552));
#142796=CARTESIAN_POINT('Ctrl Pts',(1.04926570132366,-6.93229168821724,
74.7740836697885));
#142797=CARTESIAN_POINT('Ctrl Pts',(0.839204198585687,-6.96408641641168,
74.7644260288492));
#142798=CARTESIAN_POINT('Ctrl Pts',(0.627513918363548,-6.98635675871692,
74.7547683879098));
#142799=CARTESIAN_POINT('Ctrl Pts',(0.414983637407091,-6.99895814698048,
74.7451107469705));
#142800=CARTESIAN_POINT('Ctrl Pts',(0.321569261902796,-7.00449689096477,
74.740865881283));
#142801=CARTESIAN_POINT('Ctrl Pts',(0.227992819344614,-7.00816832190245,
74.7366210155955));
#142802=CARTESIAN_POINT('Ctrl Pts',(0.1343222813047,-7.00996320156141,74.732376149908));
#142803=CARTESIAN_POINT('Ctrl Pts',(-0.0389427377908712,-7.01328324076362,
74.724524302894));
#142804=CARTESIAN_POINT('Ctrl Pts',(-0.212458611612996,-7.01017750829806,
74.71667245588));
#142805=CARTESIAN_POINT('Ctrl Pts',(-0.385691713602764,-7.00063343309434,
74.7088206088661));
#142806=CARTESIAN_POINT('Ctrl Pts',(-0.558875688085379,-6.99109206451318,
74.7009709885724));
#142807=CARTESIAN_POINT('Ctrl Pts',(-0.731776669740262,-6.97511600610928,
74.6931213682788));
#142808=CARTESIAN_POINT('Ctrl Pts',(-0.903861994686435,-6.9527447858426,
74.6852717479852));
#142809=CARTESIAN_POINT('Ctrl Pts',(-1.07593358082064,-6.9303753516317,
74.6774227543833));
#142810=CARTESIAN_POINT('Ctrl Pts',(-1.24718926169736,-6.9016118218864,
74.6695737607814));
#142811=CARTESIAN_POINT('Ctrl Pts',(-1.41710271543123,-6.86654545287639,
74.6617247671796));
#142812=CARTESIAN_POINT('Ctrl Pts',(-1.58710219137103,-6.83146133079063,
74.6538717998621));
#142813=CARTESIAN_POINT('Ctrl Pts',(-1.75575770835422,-6.79006807097766,
74.6460188325446));
#142814=CARTESIAN_POINT('Ctrl Pts',(-1.92255400822254,-6.74250789009308,
74.6381658652272));
#142815=CARTESIAN_POINT('Ctrl Pts',(-2.08939266874659,-6.6949356305206,
74.6303109035198));
#142816=CARTESIAN_POINT('Ctrl Pts',(-2.25437080871741,-6.64119344782468,
74.6224559418125));
#142817=CARTESIAN_POINT('Ctrl Pts',(-2.41699013619184,-6.58147287801533,
74.6146009801052));
#142818=CARTESIAN_POINT('Ctrl Pts',(-2.57977087694202,-6.52169303054844,
74.6067382216918));
#142819=CARTESIAN_POINT('Ctrl Pts',(-2.74018777618854,-6.45592308880591,
74.5988754632784));
#142820=CARTESIAN_POINT('Ctrl Pts',(-2.89776373376264,-6.3844022355887,
74.591012704865));
#142821=CARTESIAN_POINT('Ctrl Pts',(-3.01335919515147,-6.33193556393495,
74.5852446981172));
#142822=CARTESIAN_POINT('Ctrl Pts',(-3.12742626232804,-6.27637504553682,
74.5794766913693));
#142823=CARTESIAN_POINT('Ctrl Pts',(-3.23978591027583,-6.21783031435229,
74.5737086846215));
#142824=CARTESIAN_POINT('Ctrl Pts',(-3.40298901265608,-6.13279372041624,
74.5653306181805));
#142825=CARTESIAN_POINT('Ctrl Pts',(-3.56295046482632,-6.0412712863507,
74.5569525517394));
#142826=CARTESIAN_POINT('Ctrl Pts',(-3.71914210934023,-5.94353501992142,
74.5485744852984));
#142827=CARTESIAN_POINT('Ctrl Pts',(-3.87522695186342,-5.84586558438987,
74.5402021476796));
#142828=CARTESIAN_POINT('Ctrl Pts',(-4.02754684822451,-5.74199096145036,
74.5318298100608));
#142829=CARTESIAN_POINT('Ctrl Pts',(-4.17559910596613,-5.63222857035782,
74.5234574724421));
#142830=CARTESIAN_POINT('Ctrl Pts',(-4.32357183929446,-5.52252513675695,
74.5150896319195));
#142831=CARTESIAN_POINT('Ctrl Pts',(-4.46728124117143,-5.40694043614627,
74.5067217913969));
#142832=CARTESIAN_POINT('Ctrl Pts',(-4.60625405735394,-5.2858348556884,
74.4983539508742));
#142833=CARTESIAN_POINT('Ctrl Pts',(-4.74517258454004,-5.1647765844857,
74.4899893792043));
#142834=CARTESIAN_POINT('Ctrl Pts',(-4.87935796838435,-5.03820194984778,
74.4816248075344));
#142835=CARTESIAN_POINT('Ctrl Pts',(-5.00837012799905,-4.90651151261941,
74.4732602358644));
#142836=CARTESIAN_POINT('Ctrl Pts',(-5.13735077396163,-4.77485324326295,
74.4648977073988));
#142837=CARTESIAN_POINT('Ctrl Pts',(-5.26116048622779,-4.63808189826811,
74.4565351789332));
#142838=CARTESIAN_POINT('Ctrl Pts',(-5.37939582343618,-4.49663509052017,
74.4481726504676));
#142839=CARTESIAN_POINT('Ctrl Pts',(-5.4976405961943,-4.35517699487457,
74.4398094546461));
#142840=CARTESIAN_POINT('Ctrl Pts',(-5.61030988971596,-4.20904293933965,
74.4314462588245));
#142841=CARTESIAN_POINT('Ctrl Pts',(-5.71703988043465,-4.05870441988817,
74.423083063003));
#142842=CARTESIAN_POINT('Ctrl Pts',(-5.82377714992473,-3.90835564765107,
74.4147192968283));
#142843=CARTESIAN_POINT('Ctrl Pts',(-5.92457411841075,-3.75380210773928,
74.4063555306535));
#142844=CARTESIAN_POINT('Ctrl Pts',(-6.01910962728595,-3.59554527953878,
74.3979917644788));
#142845=CARTESIAN_POINT('Ctrl Pts',(-6.11366418710039,-3.43725655918205,
74.3896263128252));
#142846=CARTESIAN_POINT('Ctrl Pts',(-6.20195460260811,-3.27526334467866,
74.3812608611716));
#142847=CARTESIAN_POINT('Ctrl Pts',(-6.28370489658267,-3.11009313930677,
74.3728954095181));
#142848=CARTESIAN_POINT('Ctrl Pts',(-6.36548256856999,-2.94486761875777,
74.3645271562912));
#142849=CARTESIAN_POINT('Ctrl Pts',(-6.44071560577069,-2.77646328030718,
74.3561589030643));
#142850=CARTESIAN_POINT('Ctrl Pts',(-6.50917535472009,-2.60542947784135,
74.3477906498374));
#142851=CARTESIAN_POINT('Ctrl Pts',(-6.5776985756236,-2.43423710264003,
74.3394146380459));
#142852=CARTESIAN_POINT('Ctrl Pts',(-6.63943583704861,-2.26041069735044,
74.3310386262544));
#142853=CARTESIAN_POINT('Ctrl Pts',(-6.69420732378028,-2.08451789839918,
74.3226626144629));
#142854=CARTESIAN_POINT('Ctrl Pts',(-6.74900567112578,-1.90853883944601,
74.3142824949717));
#142855=CARTESIAN_POINT('Ctrl Pts',(-6.79683133996748,-1.73049168160572,
74.3059023754806));
#142856=CARTESIAN_POINT('Ctrl Pts',(-6.837555065492,-1.55095689458627,74.2975222559894));
#142857=CARTESIAN_POINT('Ctrl Pts',(-6.87832532303154,-1.37121696633039,
74.2891325611502));
#142858=CARTESIAN_POINT('Ctrl Pts',(-6.91197735568421,-1.18998633446477,
74.2807428663109));
#142859=CARTESIAN_POINT('Ctrl Pts',(-6.93843322754421,-1.00785460727745,
74.2723531714717));
#142860=CARTESIAN_POINT('Ctrl Pts',(-6.95522960404522,-0.892222316691677,
74.2670266989973));
#142861=CARTESIAN_POINT('Ctrl Pts',(-6.96912642305545,-0.776226943848889,
74.2617002265229));
#142862=CARTESIAN_POINT('Ctrl Pts',(-6.9801146287026,-0.660019948692465,
74.2563737540485));
#142863=CARTESIAN_POINT('Ctrl Pts',(-6.99740476826138,-0.477166148128354,
74.2479924536438));
#142864=CARTESIAN_POINT('Ctrl Pts',(-7.00752560932667,-0.293419399647785,
74.239611153239));
#142865=CARTESIAN_POINT('Ctrl Pts',(-7.01039695250091,-0.10936695509142,
74.2312298528342));
#142866=CARTESIAN_POINT('Ctrl Pts',(-7.01326465666801,0.0744522299348578,
74.2228591745008));
#142867=CARTESIAN_POINT('Ctrl Pts',(-7.00890116796128,0.258576013983379,
74.2144884961673));
#142868=CARTESIAN_POINT('Ctrl Pts',(-6.99727794591041,0.442411471569036,
74.2061178178339));
#142869=CARTESIAN_POINT('Ctrl Pts',(-6.98566791422094,0.626038307473389,
74.1977566387832));
#142870=CARTESIAN_POINT('Ctrl Pts',(-6.96681459007466,0.809377144052614,
74.1893954597325));
#142871=CARTESIAN_POINT('Ctrl Pts',(-6.94074144317346,0.991834049382468,
74.1810342806818));
#142872=CARTESIAN_POINT('Ctrl Pts',(-6.91470212925596,1.17405419535501,
74.1726839512472));
#142873=CARTESIAN_POINT('Ctrl Pts',(-6.88146172532469,1.35539436990032,
74.1643336218126));
#142874=CARTESIAN_POINT('Ctrl Pts',(-6.84109555853296,1.53526483758362,
74.155983292378));
#142875=CARTESIAN_POINT('Ctrl Pts',(-6.80076045109191,1.7149969057017,74.1476393880224));
#142876=CARTESIAN_POINT('Ctrl Pts',(-6.75331057855019,1.89326120219734,
74.1392954836668));
#142877=CARTESIAN_POINT('Ctrl Pts',(-6.69887267340664,2.06947613370769,
74.1309515793112));
#142878=CARTESIAN_POINT('Ctrl Pts',(-6.644478493128,2.24554952828614,74.1226143768316));
#142879=CARTESIAN_POINT('Ctrl Pts',(-6.58310757067069,2.41957652857064,
74.114277174352));
#142880=CARTESIAN_POINT('Ctrl Pts',(-6.51493705751346,2.59098855635022,
74.1059399718724));
#142881=CARTESIAN_POINT('Ctrl Pts',(-6.49249570086895,2.64741644973706,
74.1031954108357));
#142882=CARTESIAN_POINT('Ctrl Pts',(-6.46931788326026,2.70356107537436,
74.100450849799));
#142883=CARTESIAN_POINT('Ctrl Pts',(-6.44541110559441,2.75940251546966,
74.0977062887623));
#142884=CARTESIAN_POINT('Ctrl Pts',(-6.3727794068148,2.92905560352325,74.0893679784603));
#142885=CARTESIAN_POINT('Ctrl Pts',(-6.29347528529295,3.09576958922796,
74.0810296681583));
#142886=CARTESIAN_POINT('Ctrl Pts',(-6.20777312730868,3.25901509084634,
74.0726913578563));
#142887=CARTESIAN_POINT('Ctrl Pts',(-6.12201704843473,3.42236330099496,
74.0643478013724));
#142888=CARTESIAN_POINT('Ctrl Pts',(-6.02985505618335,3.58223838418103,
74.0560042448885));
#142889=CARTESIAN_POINT('Ctrl Pts',(-5.9316064869784,3.7381373765735,74.0476606884046));
#142890=CARTESIAN_POINT('Ctrl Pts',(-5.83328317069005,3.89415497624015,
74.0393107841793));
#142891=CARTESIAN_POINT('Ctrl Pts',(-5.72886421532385,4.04619017435708,
74.030960879954));
#142892=CARTESIAN_POINT('Ctrl Pts',(-5.61871132563447,4.19377033249163,
74.0226109757286));
#142893=CARTESIAN_POINT('Ctrl Pts',(-5.50839321476202,4.34157184994224,
74.0142485472649));
#142894=CARTESIAN_POINT('Ctrl Pts',(-5.3923241792621,4.48490471141038,74.0058861188011));
#142895=CARTESIAN_POINT('Ctrl Pts',(-5.27090610600303,4.6233294695706,73.9975236903374));
#142896=CARTESIAN_POINT('Ctrl Pts',(-5.14938420373964,4.76187259976909,
73.9891541108573));
#142897=CARTESIAN_POINT('Ctrl Pts',(-5.02250436216349,4.89549901532504,
73.9807845313772));
#142898=CARTESIAN_POINT('Ctrl Pts',(-4.89070451905666,5.02380691008111,
73.9724149518972));
#142899=CARTESIAN_POINT('Ctrl Pts',(-4.7587013907501,5.15231270413205,73.9640324633605));
#142900=CARTESIAN_POINT('Ctrl Pts',(-4.62176333995414,5.27548336631318,
73.9556499748238));
#142901=CARTESIAN_POINT('Ctrl Pts',(-4.48036155506989,5.3929571571033,73.9472674862872));
#142902=CARTESIAN_POINT('Ctrl Pts',(-4.43409257406062,5.43139650636332,
73.9445245986834));
#142903=CARTESIAN_POINT('Ctrl Pts',(-4.38734588960136,5.46922623406694,
73.9417817110796));
#142904=CARTESIAN_POINT('Ctrl Pts',(-4.34013865785259,5.50643468980733,
73.9390388234758));
#142905=CARTESIAN_POINT('Ctrl Pts',(-4.19574271722301,5.62024670053062,
73.930648968343));
#142906=CARTESIAN_POINT('Ctrl Pts',(-4.04674420327156,5.72847259738453,
73.9222591132102));
#142907=CARTESIAN_POINT('Ctrl Pts',(-3.89360220379064,5.83073652647217,
73.9138692580775));
#142908=CARTESIAN_POINT('Ctrl Pts',(-3.74060152159998,5.93290608783965,
73.9054871449854));
#142909=CARTESIAN_POINT('Ctrl Pts',(-3.58346524818031,6.0291244672418,73.8971050318933));
#142910=CARTESIAN_POINT('Ctrl Pts',(-3.42268409254751,6.1190571304019,73.8887229188012));
#142911=CARTESIAN_POINT('Ctrl Pts',(-3.26202766901513,6.20892002487592,
73.8803473084524));
#142912=CARTESIAN_POINT('Ctrl Pts',(-3.09773228662066,6.29250676523242,
73.8719716981035));
#142913=CARTESIAN_POINT('Ctrl Pts',(-2.93031646353258,6.36952682591493,
73.8635960877547));
#142914=CARTESIAN_POINT('Ctrl Pts',(-2.76300594748313,6.44649843983563,
73.8552257457891));
#142915=CARTESIAN_POINT('Ctrl Pts',(-2.59257920226384,6.51691147297106,
73.8468554038236));
#142916=CARTESIAN_POINT('Ctrl Pts',(-2.41957851456268,6.58052174028524,
73.838485061858));
#142917=CARTESIAN_POINT('Ctrl Pts',(-2.24666128690485,6.64410132034761,
73.8301187579637));
#142918=CARTESIAN_POINT('Ctrl Pts',(-2.0711729009687,6.70088456585241,73.8217524540694));
#142919=CARTESIAN_POINT('Ctrl Pts',(-1.89367517636312,6.75067558759315,
73.813386150175));
#142920=CARTESIAN_POINT('Ctrl Pts',(-1.71622709289637,6.80045268418061,
73.8050221861015));
#142921=CARTESIAN_POINT('Ctrl Pts',(-1.53677110706267,6.84324136622197,
73.7966582220278));
#142922=CARTESIAN_POINT('Ctrl Pts',(-1.35588427386249,6.87889557984364,
73.7882942579542));
#142923=CARTESIAN_POINT('Ctrl Pts',(-1.17502527613985,6.91454430687436,
73.7799315809557));
#142924=CARTESIAN_POINT('Ctrl Pts',(-0.992736192412884,6.94306069089118,
73.7715689039572));
#142925=CARTESIAN_POINT('Ctrl Pts',(-0.809604761811532,6.96434969628551,
73.7632062269587));
#142926=CARTESIAN_POINT('Ctrl Pts',(-0.626477101551507,6.98563826337814,
73.7548437221324));
#142927=CARTESIAN_POINT('Ctrl Pts',(-0.442507455494422,6.99969971100225,
73.7464812173061));
#142928=CARTESIAN_POINT('Ctrl Pts',(-0.258289619035452,7.00649077892767,
73.7381187124798));
#142929=CARTESIAN_POINT('Ctrl Pts',(-0.0740510203588375,7.01328261223843,
73.7297552651598));
#142930=CARTESIAN_POINT('Ctrl Pts',(0.110435496055611,7.0128024206199,73.7213918178398));
#142931=CARTESIAN_POINT('Ctrl Pts',(0.29457475621586,7.00505904868049,73.7130283705199));
#142932=CARTESIAN_POINT('Ctrl Pts',(0.478822442747335,6.99731111722607,
73.7046599985671));
#142933=CARTESIAN_POINT('Ctrl Pts',(0.662722135685751,6.98229147231949,
73.6962916266143));
#142934=CARTESIAN_POINT('Ctrl Pts',(0.845681362458587,6.96006103390554,
73.6879232546615));
#142935=CARTESIAN_POINT('Ctrl Pts',(1.0286954085976,6.93782393467121,73.6795523753258));
#142936=CARTESIAN_POINT('Ctrl Pts',(1.2107681010083,6.90837177876362,73.67118149599));
#142937=CARTESIAN_POINT('Ctrl Pts',(1.39131508590212,6.87181700092786,73.6628106166543));
#142938=CARTESIAN_POINT('Ctrl Pts',(1.57201504630374,6.83523125062416,73.654432644763));
#142939=CARTESIAN_POINT('Ctrl Pts',(1.75118639480659,6.79153092394869,73.6460546728717));
#142940=CARTESIAN_POINT('Ctrl Pts',(1.92825677760947,6.74087919800549,73.6376767009805));
#142941=CARTESIAN_POINT('Ctrl Pts',(2.04078644777437,6.70868961370886,73.6323524316213));
#142942=CARTESIAN_POINT('Ctrl Pts',(2.15246788626534,6.67369357447061,73.6270281622621));
#142943=CARTESIAN_POINT('Ctrl Pts',(2.26315789621714,6.63594325618371,73.6217038929029));
#142944=CARTESIAN_POINT('Ctrl Pts',(2.42662386757941,6.58019393923369,73.6138410617136));
#142945=CARTESIAN_POINT('Ctrl Pts',(2.58826656138551,6.51831926484873,73.6059782305243));
#142946=CARTESIAN_POINT('Ctrl Pts',(2.74757357211221,6.45046246623686,73.598115399335));
#142947=CARTESIAN_POINT('Ctrl Pts',(2.90675817642966,6.38265780661764,73.5902586096936));
#142948=CARTESIAN_POINT('Ctrl Pts',(3.06361031810684,6.30888031196602,73.5824018200522));
#142949=CARTESIAN_POINT('Ctrl Pts',(3.2176331264742,6.22932288663189,73.5745450304108));
#142950=CARTESIAN_POINT('Ctrl Pts',(3.37156907326855,6.14981032791968,73.5666926716268));
#142951=CARTESIAN_POINT('Ctrl Pts',(3.52267852309253,6.06452449706037,73.5588403128428));
#142952=CARTESIAN_POINT('Ctrl Pts',(3.67048520232653,5.97370613120548,73.5509879540589));
#142953=CARTESIAN_POINT('Ctrl Pts',(3.81825698267898,5.88290920862642,73.5431374493084));
#142954=CARTESIAN_POINT('Ctrl Pts',(3.96272721553292,5.78658254317437,73.535286944558));
#142955=CARTESIAN_POINT('Ctrl Pts',(4.10344489977822,5.68501244651093,73.5274364398075));
#142956=CARTESIAN_POINT('Ctrl Pts',(4.24413994698325,5.58345868927477,73.5195871979559));
#142957=CARTESIAN_POINT('Ctrl Pts',(4.38108333970336,5.47666340572829,73.5117379561042));
#142958=CARTESIAN_POINT('Ctrl Pts',(4.51385409986448,5.36495551963263,73.5038887142526));
#142959=CARTESIAN_POINT('Ctrl Pts',(4.64666959309339,5.25320999696372,73.4960368278377));
#142960=CARTESIAN_POINT('Ctrl Pts',(4.77530935348191,5.13654881152433,73.4881849414228));
#142961=CARTESIAN_POINT('Ctrl Pts',(4.89938632363381,5.01534048837065,73.4803330550079));
#142962=CARTESIAN_POINT('Ctrl Pts',(4.99049449845879,4.92633872533108,73.4745675125441));
#142963=CARTESIAN_POINT('Ctrl Pts',(5.07914321494787,4.83488608072522,73.4688019700803));
#142964=CARTESIAN_POINT('Ctrl Pts',(5.16519231646955,4.74114067460395,73.4630364276165));
#142965=CARTESIAN_POINT('Ctrl Pts',(5.3091382818708,4.58432006000798,73.4533916252729));
#142966=CARTESIAN_POINT('Ctrl Pts',(5.44573570756597,4.42116291705853,73.4437468229294));
#142967=CARTESIAN_POINT('Ctrl Pts',(5.57452589644171,4.25232731482429,73.4341020205858));
#142968=CARTESIAN_POINT('Ctrl Pts',(5.70432389576355,4.08217053832135,73.4243817456256));
#142969=CARTESIAN_POINT('Ctrl Pts',(5.82619199054581,3.90624614694125,73.4146614706654));
#142970=CARTESIAN_POINT('Ctrl Pts',(5.93970849948159,3.72525026054441,73.4049411957052));
#142971=CARTESIAN_POINT('Ctrl Pts',(6.05356126387142,3.54371823315333,73.3951921276162));
#142972=CARTESIAN_POINT('Ctrl Pts',(6.1590129034956,3.35708467698042,73.3854430595271));
#142973=CARTESIAN_POINT('Ctrl Pts',(6.25568581308494,3.16607352575203,73.375693991438));
#142974=CARTESIAN_POINT('Ctrl Pts',(6.35251836848934,2.9747469383683,73.3659288237206));
#142975=CARTESIAN_POINT('Ctrl Pts',(6.44054316953447,2.77902832587818,73.3561636560031));
#142976=CARTESIAN_POINT('Ctrl Pts',(6.51942859313609,2.57966613760379,73.3463984882856));
#142977=CARTESIAN_POINT('Ctrl Pts',(6.53711577681312,2.53496642653839,73.3442090050178));
#142978=CARTESIAN_POINT('Ctrl Pts',(6.55434369867958,2.49008362846496,73.3420195217499));
#142979=CARTESIAN_POINT('Ctrl Pts',(6.57110895151812,2.44502632087643,73.339830038482));
#142980=CARTESIAN_POINT('Origin',(0.,0.,50.));
#142981=CARTESIAN_POINT('',(6.57110895151817,2.44502632087629,71.3398522865014));
#142982=CARTESIAN_POINT('',(6.57110895151816,2.44502632087631,71.8867112926201));
#142983=CARTESIAN_POINT('',(6.57110895151814,2.44502632087636,50.));
#142984=CARTESIAN_POINT('',(7.0112497650765,-0.00181499715760335,73.7735343569104));
#142985=CARTESIAN_POINT('Ctrl Pts',(6.57110895151816,2.44502632087631,71.8867112926201));
#142986=CARTESIAN_POINT('Ctrl Pts',(6.49663749355182,2.64517143174769,71.896403236564));
#142987=CARTESIAN_POINT('Ctrl Pts',(6.41310542934644,2.84167750050844,71.9060951805078));
#142988=CARTESIAN_POINT('Ctrl Pts',(6.32088104020746,3.03382422662321,71.9157871244517));
#142989=CARTESIAN_POINT('Ctrl Pts',(6.22811547998219,3.22709846633247,71.9255359405514));
#142990=CARTESIAN_POINT('Ctrl Pts',(6.12655532786914,3.41596202306511,71.935284756651));
#142991=CARTESIAN_POINT('Ctrl Pts',(6.01661860960486,3.59971208141103,71.9450335727507));
#142992=CARTESIAN_POINT('Ctrl Pts',(5.90651695262479,3.78373782106823,71.9547970150575));
#142993=CARTESIAN_POINT('Ctrl Pts',(5.78801361952856,3.96263468803567,71.9645604573643));
#142994=CARTESIAN_POINT('Ctrl Pts',(5.6615710320532,4.13572726512714,71.9743238996711));
#142995=CARTESIAN_POINT('Ctrl Pts',(5.53523478523948,4.30867426801344,71.9840791307341));
#142996=CARTESIAN_POINT('Ctrl Pts',(5.40097266211013,4.47582671490287,71.9938343617971));
#142997=CARTESIAN_POINT('Ctrl Pts',(5.25928775646086,4.63654169152407,72.00358959286));
#142998=CARTESIAN_POINT('Ctrl Pts',(5.148221290281,4.76252578583319,72.0112366956757));
#142999=CARTESIAN_POINT('Ctrl Pts',(5.03259437926697,4.88455467989839,72.0188837984914));
#143000=CARTESIAN_POINT('Ctrl Pts',(4.91266726452391,5.00233214716648,72.0265309013071));
#143001=CARTESIAN_POINT('Ctrl Pts',(4.78668753017622,5.12605374315723,72.0345639469058));
#143002=CARTESIAN_POINT('Ctrl Pts',(4.65589946607834,5.24514239954313,72.0425969925046));
#143003=CARTESIAN_POINT('Ctrl Pts',(4.52068546131911,5.35920045550808,72.0506300381033));
#143004=CARTESIAN_POINT('Ctrl Pts',(4.38555837732815,5.4731851905632,72.058657919751));
#143005=CARTESIAN_POINT('Ctrl Pts',(4.24601129507244,5.58214552691228,72.0666858013987));
#143006=CARTESIAN_POINT('Ctrl Pts',(4.10246291680207,5.68572111334735,72.0747136830464));
#143007=CARTESIAN_POINT('Ctrl Pts',(3.95897935203999,5.78924993438382,72.0827379400264));
#143008=CARTESIAN_POINT('Ctrl Pts',(3.81149838510998,5.88739863239531,72.0907621970064));
#143009=CARTESIAN_POINT('Ctrl Pts',(3.66047116582932,5.97984760730841,72.0987864539863));
#143010=CARTESIAN_POINT('Ctrl Pts',(3.50946220727736,6.07228540419905,72.106809740752));
#143011=CARTESIAN_POINT('Ctrl Pts',(3.35490815886445,6.15902465282508,72.1148330275176));
#143012=CARTESIAN_POINT('Ctrl Pts',(3.19728862277623,6.23978942154026,72.1228563142832));
#143013=CARTESIAN_POINT('Ctrl Pts',(3.03968200220254,6.32054757230331,72.130878943612));
#143014=CARTESIAN_POINT('Ctrl Pts',(2.87901072243325,6.39533205468025,72.1389015729409));
#143015=CARTESIAN_POINT('Ctrl Pts',(2.71577814403288,6.46391333751415,72.1469242022697));
#143016=CARTESIAN_POINT('Ctrl Pts',(2.55248420180427,6.53252040202779,72.154949847536));
#143017=CARTESIAN_POINT('Ctrl Pts',(2.38662737680296,6.59491946920017,72.1629754928023));
#143018=CARTESIAN_POINT('Ctrl Pts',(2.21873047903218,6.65092938046358,72.1710011380686));
#143019=CARTESIAN_POINT('Ctrl Pts',(2.11972823696198,6.68395623722421,72.1757335475769));
#143020=CARTESIAN_POINT('Ctrl Pts',(2.02001699363196,6.71476251525016,72.1804659570852));
#143021=CARTESIAN_POINT('Ctrl Pts',(1.91970626837374,6.7433192424552,72.1851983665935));
#143022=CARTESIAN_POINT('Ctrl Pts',(1.73465940617335,6.79599888115189,72.1939284154283));
#143023=CARTESIAN_POINT('Ctrl Pts',(1.54747933220094,6.84104703880505,72.2026584642631));
#143024=CARTESIAN_POINT('Ctrl Pts',(1.35879712463329,6.87832079337598,72.2113885130979));
#143025=CARTESIAN_POINT('Ctrl Pts',(1.17006035937003,6.91560532569952,72.2201210862372));
#143026=CARTESIAN_POINT('Ctrl Pts',(0.979820862286258,6.94511091476385,
72.2288536593765));
#143027=CARTESIAN_POINT('Ctrl Pts',(0.788719045880268,6.96674592827711,
72.2375862325158));
#143028=CARTESIAN_POINT('Ctrl Pts',(0.594902323120467,6.98868830169284,
72.2464428657961));
#143029=CARTESIAN_POINT('Ctrl Pts',(0.400198881060796,7.00253473439962,
72.2552994990765));
#143030=CARTESIAN_POINT('Ctrl Pts',(0.205281742183532,7.00824414306652,
72.2641561323568));
#143031=CARTESIAN_POINT('Ctrl Pts',(0.0129725818632786,7.01387716021924,
72.2728942644637));
#143032=CARTESIAN_POINT('Ctrl Pts',(-0.179544313973932,7.01158956178464,
72.2816323965706));
#143033=CARTESIAN_POINT('Ctrl Pts',(-0.371622006413891,7.0013944073198,
72.2903705286775));
#143034=CARTESIAN_POINT('Ctrl Pts',(-0.567606958151783,6.99099186223312,
72.2992864125446));
#143035=CARTESIAN_POINT('Ctrl Pts',(-0.763134350480073,6.97235661479577,
72.3082022964117));
#143036=CARTESIAN_POINT('Ctrl Pts',(-0.957520795727762,6.9455583280431,
72.3171181802788));
#143037=CARTESIAN_POINT('Ctrl Pts',(-1.15190724097545,6.91876004129044,
72.3260340641458));
#143038=CARTESIAN_POINT('Ctrl Pts',(-1.34515244039453,6.88379876254866,
72.3349499480129));
#143039=CARTESIAN_POINT('Ctrl Pts',(-1.53658136398455,6.84079997327472,
72.34386583188));
#143040=CARTESIAN_POINT('Ctrl Pts',(-1.72424866085302,6.79864612107556,
72.3526065163761));
#143041=CARTESIAN_POINT('Ctrl Pts',(-1.91019033201575,6.74876322731733,
72.3613472008722));
#143042=CARTESIAN_POINT('Ctrl Pts',(-2.0937807640309,6.69131591502555,72.3700878853683));
#143043=CARTESIAN_POINT('Ctrl Pts',(-2.27733816507752,6.63387893845956,
72.3788269972701));
#143044=CARTESIAN_POINT('Ctrl Pts',(-2.45854491058638,6.56888034304456,
72.3875661091718));
#143045=CARTESIAN_POINT('Ctrl Pts',(-2.63679070771567,6.49653456284228,
72.3963052210736));
#143046=CARTESIAN_POINT('Ctrl Pts',(-2.81734593569057,6.42325143893238,
72.405157560748));
#143047=CARTESIAN_POINT('Ctrl Pts',(-2.9948626811838,6.34242950270267,72.4140099004224));
#143048=CARTESIAN_POINT('Ctrl Pts',(-3.16872638395628,6.25434246472956,
72.4228622400968));
#143049=CARTESIAN_POINT('Ctrl Pts',(-3.34027827087986,6.16742669486601,
72.4315968727465));
#143050=CARTESIAN_POINT('Ctrl Pts',(-3.50827341436658,6.07343796675173,
72.4403315053962));
#143051=CARTESIAN_POINT('Ctrl Pts',(-3.67214425031528,5.97268642801348,
72.4490661380458));
#143052=CARTESIAN_POINT('Ctrl Pts',(-3.83932754644016,5.86989831298131,
72.4579773312326));
#143053=CARTESIAN_POINT('Ctrl Pts',(-4.00221776424444,5.76007120420412,
72.4668885244193));
#143054=CARTESIAN_POINT('Ctrl Pts',(-4.16024047493172,5.64358270544872,
72.4757997176061));
#143055=CARTESIAN_POINT('Ctrl Pts',(-4.318263185619,5.52709420669332,72.4847109107928));
#143056=CARTESIAN_POINT('Ctrl Pts',(-4.47141813719525,5.40394448698109,
72.4936221039796));
#143057=CARTESIAN_POINT('Ctrl Pts',(-4.61916328400746,5.27455752818921,
72.5025332971663));
#143058=CARTESIAN_POINT('Ctrl Pts',(-4.75222661313086,5.15802808642092,
72.5105589620188));
#143059=CARTESIAN_POINT('Ctrl Pts',(-4.88096269756898,5.03638549043432,
72.5185846268712));
#143060=CARTESIAN_POINT('Ctrl Pts',(-5.00495595374574,4.90999414088907,
72.5266102917237));
#143061=CARTESIAN_POINT('Ctrl Pts',(-5.12890985750446,4.78364290485789,
72.534633409427));
#143062=CARTESIAN_POINT('Ctrl Pts',(-5.24812367342293,4.65254617720194,
72.5426565271303));
#143063=CARTESIAN_POINT('Ctrl Pts',(-5.36221771831549,4.51710612050275,
72.5506796448336));
#143064=CARTESIAN_POINT('Ctrl Pts',(-5.47629737495057,4.38168314397993,
72.5587017507515));
#143065=CARTESIAN_POINT('Ctrl Pts',(-5.58525831096701,4.24191821008803,
72.5667238566694));
#143066=CARTESIAN_POINT('Ctrl Pts',(-5.68876032072863,4.09824750055478,
72.5747459625874));
#143067=CARTESIAN_POINT('Ctrl Pts',(-5.79230079218675,3.95452340250049,
72.582771049547));
#143068=CARTESIAN_POINT('Ctrl Pts',(-5.89037806807313,3.80689092531865,
72.5907961365066));
#143069=CARTESIAN_POINT('Ctrl Pts',(-5.98269432985107,3.65581661439244,
72.5988212234662));
#143070=CARTESIAN_POINT('Ctrl Pts',(-6.07502877285522,3.50471255013602,
72.6068478909265));
#143071=CARTESIAN_POINT('Ctrl Pts',(-6.16159975781812,3.35016561912344,
72.6148745583869));
#143072=CARTESIAN_POINT('Ctrl Pts',(-6.24215496203757,3.19266784874496,
72.6229012258472));
#143073=CARTESIAN_POINT('Ctrl Pts',(-6.3227748356905,3.0350436397126,72.6309343370879));
#143074=CARTESIAN_POINT('Ctrl Pts',(-6.39736912436822,2.87446419050912,
72.6389674483285));
#143075=CARTESIAN_POINT('Ctrl Pts',(-6.46573301858888,2.71144299125568,
72.6470005595691));
#143076=CARTESIAN_POINT('Ctrl Pts',(-6.50601550851415,2.61538497859571,
72.6517339605304));
#143077=CARTESIAN_POINT('Ctrl Pts',(-6.54413573015642,2.51847954998675,
72.6564673614917));
#143078=CARTESIAN_POINT('Ctrl Pts',(-6.5800598628589,2.42083431149125,72.6612007624529));
#143079=CARTESIAN_POINT('Ctrl Pts',(-6.65406469426367,2.21968208125696,
72.6709517157469));
#143080=CARTESIAN_POINT('Ctrl Pts',(-6.71879150752435,2.01527117142247,
72.680702669041));
#143081=CARTESIAN_POINT('Ctrl Pts',(-6.77402074923543,1.80838863395782,
72.690453622335));
#143082=CARTESIAN_POINT('Ctrl Pts',(-6.82932955902953,1.60120804338932,
72.7002186237063));
#143083=CARTESIAN_POINT('Ctrl Pts',(-6.87511341721585,1.39154873978261,
72.7099836250777));
#143084=CARTESIAN_POINT('Ctrl Pts',(-6.91120301163148,1.18021163124076,
72.7197486264491));
#143085=CARTESIAN_POINT('Ctrl Pts',(-6.94723245217097,0.969226777869918,
72.7294973515865));
#143086=CARTESIAN_POINT('Ctrl Pts',(-6.97359991649599,0.756569746106266,
72.7392460767239));
#143087=CARTESIAN_POINT('Ctrl Pts',(-6.99018785445205,0.543047255744024,
72.7489948018613));
#143088=CARTESIAN_POINT('Ctrl Pts',(-7.00673026495013,0.330110801827794,
72.7587167705281));
#143089=CARTESIAN_POINT('Ctrl Pts',(-7.01354672967137,0.11631367112125,
72.7684387391949));
#143090=CARTESIAN_POINT('Ctrl Pts',(-7.01057155428257,-0.0975348388223232,
72.7781607078618));
#143091=CARTESIAN_POINT('Ctrl Pts',(-7.00761606485217,-0.309968369034859,
72.7878183488014));
#143092=CARTESIAN_POINT('Ctrl Pts',(-6.99499805624747,-0.522452553737243,
72.797475989741));
#143093=CARTESIAN_POINT('Ctrl Pts',(-6.97270378508319,-0.734185595055159,
72.8071336306806));
#143094=CARTESIAN_POINT('Ctrl Pts',(-6.96290468535936,-0.827249556259204,
72.8113784963668));
#143095=CARTESIAN_POINT('Ctrl Pts',(-6.95123688691363,-0.920168297538873,
72.815623362053));
#143096=CARTESIAN_POINT('Ctrl Pts',(-6.93770238185834,-1.0128732513287,
72.8198682277392));
#143097=CARTESIAN_POINT('Ctrl Pts',(-6.91266722857916,-1.18435220223127,
72.8277200747532));
#143098=CARTESIAN_POINT('Ctrl Pts',(-6.88125167260411,-1.35502869998371,
72.8355719217671));
#143099=CARTESIAN_POINT('Ctrl Pts',(-6.84353050352245,-1.5243742355005,
72.8434237687811));
#143100=CARTESIAN_POINT('Ctrl Pts',(-6.80582003185933,-1.69367174599276,
72.8512733890747));
#143101=CARTESIAN_POINT('Ctrl Pts',(-6.7618075870222,-1.86163867309074,
72.8591230093683));
#143102=CARTESIAN_POINT('Ctrl Pts',(-6.71161920016452,-2.027755970151,72.866972629662));
#143103=CARTESIAN_POINT('Ctrl Pts',(-6.66143482020766,-2.1938600048696,
72.8748216232638));
#143104=CARTESIAN_POINT('Ctrl Pts',(-6.60507559083961,-2.35811433857433,
72.8826706168656));
#143105=CARTESIAN_POINT('Ctrl Pts',(-6.54271754008799,-2.52001463351406,
72.8905196104675));
#143106=CARTESIAN_POINT('Ctrl Pts',(-6.48032791928116,-2.68199689383255,
72.8983725777849));
#143107=CARTESIAN_POINT('Ctrl Pts',(-6.41193354624365,-2.84162237771152,
72.9062255451024));
#143108=CARTESIAN_POINT('Ctrl Pts',(-6.33775891676812,-2.99840598909256,
72.9140785124199));
#143109=CARTESIAN_POINT('Ctrl Pts',(-6.26356544942902,-3.15522941824288,
72.9219334741272));
#143110=CARTESIAN_POINT('Ctrl Pts',(-6.1835889769201,-3.30920919845494,
72.9297884358345));
#143111=CARTESIAN_POINT('Ctrl Pts',(-6.09809987938691,-3.45988503039066,
72.9376433975418));
#143112=CARTESIAN_POINT('Ctrl Pts',(-6.01252592677857,-3.61071042068424,
72.9455061559552));
#143113=CARTESIAN_POINT('Ctrl Pts',(-5.92142862103154,-3.75822498839262,
72.9533689143686));
#143114=CARTESIAN_POINT('Ctrl Pts',(-5.82512188612499,-3.90199712638127,
72.9612316727819));
#143115=CARTESIAN_POINT('Ctrl Pts',(-5.75447264732019,-4.00746630379749,
72.9669996795299));
#143116=CARTESIAN_POINT('Ctrl Pts',(-5.681020872031,-4.11092210946462,72.9727676862778));
#143117=CARTESIAN_POINT('Ctrl Pts',(-5.60490397254818,-4.21220583792075,
72.9785356930257));
#143118=CARTESIAN_POINT('Ctrl Pts',(-5.49434369253786,-4.35932109688012,
72.9869137594667));
#143119=CARTESIAN_POINT('Ctrl Pts',(-5.3779144051963,-4.50217851939186,
72.9952918259078));
#143120=CARTESIAN_POINT('Ctrl Pts',(-5.25597076081091,-4.64030149063623,
73.0036698923488));
#143121=CARTESIAN_POINT('Ctrl Pts',(-5.13411050004045,-4.77833001503422,
73.0120422299675));
#143122=CARTESIAN_POINT('Ctrl Pts',(-5.0067436166585,-4.91163029686378,
73.0204145675863));
#143123=CARTESIAN_POINT('Ctrl Pts',(-4.87426540130468,-5.03975826405832,
73.0287869052051));
#143124=CARTESIAN_POINT('Ctrl Pts',(-4.74185834496281,-5.16781740892216,
73.0371547457277));
#143125=CARTESIAN_POINT('Ctrl Pts',(-4.60434566665396,-5.29070955068605,
73.0455225862503));
#143126=CARTESIAN_POINT('Ctrl Pts',(-4.46216023742459,-5.40802668059681,
73.0538904267729));
#143127=CARTESIAN_POINT('Ctrl Pts',(-4.32003035218113,-5.52529798119126,
73.0622549984428));
#143128=CARTESIAN_POINT('Ctrl Pts',(-4.17323160927016,-5.63699840398013,
73.0706195701128));
#143129=CARTESIAN_POINT('Ctrl Pts',(-4.02223109316965,-5.7427592319058,
73.0789841417828));
#143130=CARTESIAN_POINT('Ctrl Pts',(-3.87126746179388,-5.84849422575403,
73.0873466702483));
#143131=CARTESIAN_POINT('Ctrl Pts',(-3.71610437327186,-5.94829233005877,
73.0957091987138));
#143132=CARTESIAN_POINT('Ctrl Pts',(-3.55723947947013,-6.0418270289871,
73.1040717271793));
#143133=CARTESIAN_POINT('Ctrl Pts',(-3.39836190775218,-6.13536919227743,
73.1124349230008));
#143134=CARTESIAN_POINT('Ctrl Pts',(-3.23578222071624,-6.22264677962249,
73.1207981188223));
#143135=CARTESIAN_POINT('Ctrl Pts',(-3.07002502461947,-6.30337789686691,
73.1291613146439));
#143136=CARTESIAN_POINT('Ctrl Pts',(-2.90425652421417,-6.3841145198117,
73.1375250808185));
#143137=CARTESIAN_POINT('Ctrl Pts',(-2.73531037817286,-6.45830363823736,
73.1458888469932));
#143138=CARTESIAN_POINT('Ctrl Pts',(-2.56373380198725,-6.5257103486937,
73.1542526131679));
#143139=CARTESIAN_POINT('Ctrl Pts',(-2.39212264942908,-6.59313064305283,
73.1626180648215));
#143140=CARTESIAN_POINT('Ctrl Pts',(-2.21788031573932,-6.65376568379617,
73.1709835164751));
#143141=CARTESIAN_POINT('Ctrl Pts',(-2.04157230816635,-6.70742939381611,
73.1793489681286));
#143142=CARTESIAN_POINT('Ctrl Pts',(-1.86520525538916,-6.76111107570676,
73.1877172213555));
#143143=CARTESIAN_POINT('Ctrl Pts',(-1.68677146369094,-6.80781667574779,
73.1960854745823));
#143144=CARTESIAN_POINT('Ctrl Pts',(-1.50685026482488,-6.84741037487145,
73.2044537278092));
#143145=CARTESIAN_POINT('Ctrl Pts',(-1.32676225333829,-6.887040783003,73.2128297396006));
#143146=CARTESIAN_POINT('Ctrl Pts',(-1.14518440038569,-6.91954604320939,
73.2212057513921));
#143147=CARTESIAN_POINT('Ctrl Pts',(-0.962706094649794,-6.94484150559422,
73.2295817631836));
#143148=CARTESIAN_POINT('Ctrl Pts',(-0.780138299297698,-6.97014937318639,
73.2379618826748));
#143149=CARTESIAN_POINT('Ctrl Pts',(-0.596669496899309,-6.98824035330358,
73.2463420021659));
#143150=CARTESIAN_POINT('Ctrl Pts',(-0.41289347728538,-6.9990817639827,
73.2547221216571));
#143151=CARTESIAN_POINT('Ctrl Pts',(-0.228907470289866,-7.00993556234682,
73.2631118164963));
#143152=CARTESIAN_POINT('Ctrl Pts',(-0.0446138732872293,-7.01352322616916,
73.2715015113355));
#143153=CARTESIAN_POINT('Ctrl Pts',(0.139392894994874,-7.00986420576925,
73.2798912061747));
#143154=CARTESIAN_POINT('Ctrl Pts',(0.25621561681979,-7.00754115686012,
73.2852176786493));
#143155=CARTESIAN_POINT('Ctrl Pts',(0.372922769238492,-7.00229819252731,
73.2905441511239));
#143156=CARTESIAN_POINT('Ctrl Pts',(0.489363448128481,-6.99415112634377,
73.2958706235985));
#143157=CARTESIAN_POINT('Ctrl Pts',(0.672584954252464,-6.98133157091975,
73.3042519240034));
#143158=CARTESIAN_POINT('Ctrl Pts',(0.855515982900771,-6.96129316380664,
73.3126332244083));
#143159=CARTESIAN_POINT('Ctrl Pts',(1.0375640702819,-6.93405273722086,73.3210145248132));
#143160=CARTESIAN_POINT('Ctrl Pts',(1.21938143836258,-6.90684683388801,
73.3293852031467));
#143161=CARTESIAN_POINT('Ctrl Pts',(1.40031777380758,-6.8724571493474,73.3377558814803));
#143162=CARTESIAN_POINT('Ctrl Pts',(1.57978345622159,-6.83095240753063,
73.3461265598139));
#143163=CARTESIAN_POINT('Ctrl Pts',(1.75904547590016,-6.7894947664695,73.3544877388648));
#143164=CARTESIAN_POINT('Ctrl Pts',(1.93683985164169,-6.74093823461438,
73.3628489179157));
#143165=CARTESIAN_POINT('Ctrl Pts',(2.11258446832033,-6.68540301154027,
73.3712100969666));
#143166=CARTESIAN_POINT('Ctrl Pts',(2.28810103562714,-6.62993985196931,
73.3795604264014));
#143167=CARTESIAN_POINT('Ctrl Pts',(2.46157283818407,-6.56751616194294,
73.3879107558361));
#143168=CARTESIAN_POINT('Ctrl Pts',(2.63243037418638,-6.49830261588063,
73.3962610852709));
#143169=CARTESIAN_POINT('Ctrl Pts',(2.80315644553242,-6.42914232550287,
73.4046049896265));
#143170=CARTESIAN_POINT('Ctrl Pts',(2.97127195653029,-6.35320271284023,
73.4129488939821));
#143171=CARTESIAN_POINT('Ctrl Pts',(3.13622383738162,-6.27070383643968,
73.4212927983377));
#143172=CARTESIAN_POINT('Ctrl Pts',(3.30104322785578,-6.18827122365004,
73.4296300008175));
#143173=CARTESIAN_POINT('Ctrl Pts',(3.46270376374544,-6.09929000041611,
73.4379672032972));
#143174=CARTESIAN_POINT('Ctrl Pts',(3.62067345368134,-6.00402784006764,
73.4463044057769));
#143175=CARTESIAN_POINT('Ctrl Pts',(3.6726762036358,-5.97266806271583,73.449048966813));
#143176=CARTESIAN_POINT('Ctrl Pts',(3.72427915896821,-5.94062800628213,
73.451793527849));
#143177=CARTESIAN_POINT('Ctrl Pts',(3.77546389517341,-5.90791832532763,
73.454538088885));
#143178=CARTESIAN_POINT('Ctrl Pts',(3.93096935035945,-5.8085423354734,73.4628763991868));
#143179=CARTESIAN_POINT('Ctrl Pts',(4.08248496435823,-5.70306382850212,
73.4712147094886));
#143180=CARTESIAN_POINT('Ctrl Pts',(4.22953330314882,-5.59184000129251,
73.4795530197905));
#143181=CARTESIAN_POINT('Ctrl Pts',(4.3766741597659,-5.48054619582384,73.4878965762743));
#143182=CARTESIAN_POINT('Ctrl Pts',(4.51934187364946,-5.36350005768225,
73.496240132758));
#143183=CARTESIAN_POINT('Ctrl Pts',(4.6570924182614,-5.24109881325207,73.5045836892418));
#143184=CARTESIAN_POINT('Ctrl Pts',(4.79494776288413,-5.11860444649141,
73.5129335934668));
#143185=CARTESIAN_POINT('Ctrl Pts',(4.92787823158848,-4.99074706424958,
73.5212834976919));
#143186=CARTESIAN_POINT('Ctrl Pts',(5.05547663844316,-4.85796073683758,
73.5296334019169));
#143187=CARTESIAN_POINT('Ctrl Pts',(5.18326643346779,-4.72497523975861,
73.5379958303805));
#143188=CARTESIAN_POINT('Ctrl Pts',(5.30570795750625,-4.58704626032255,
73.546358258844));
#143189=CARTESIAN_POINT('Ctrl Pts',(5.42243333521388,-4.44464208768955,
73.5547206873076));
#143190=CARTESIAN_POINT('Ctrl Pts',(5.53925852903079,-4.30211614007721,
73.5630902667875));
#143191=CARTESIAN_POINT('Ctrl Pts',(5.65035762644575,-4.15510762439005,
73.5714598462673));
#143192=CARTESIAN_POINT('Ctrl Pts',(5.75540577794039,-4.00411424584144,
73.5798294257471));
#143193=CARTESIAN_POINT('Ctrl Pts',(5.86061595341033,-3.85288797840247,
73.5882119142836));
#143194=CARTESIAN_POINT('Ctrl Pts',(5.95975635712508,-3.69766484182881,
73.5965944028201));
#143195=CARTESIAN_POINT('Ctrl Pts',(6.0525471007111,-3.53896879841764,73.6049768913566));
#143196=CARTESIAN_POINT('Ctrl Pts',(6.08290975248512,-3.48704085261408,
73.6077197789615));
#143197=CARTESIAN_POINT('Ctrl Pts',(6.11259292135486,-3.43474123220562,
73.6104626665664));
#143198=CARTESIAN_POINT('Ctrl Pts',(6.14158791671023,-3.38208876640145,
73.6132055541713));
#143199=CARTESIAN_POINT('Ctrl Pts',(6.23397316448646,-3.21432494924165,
73.6219450744885));
#143200=CARTESIAN_POINT('Ctrl Pts',(6.31953798906509,-3.04266953665,73.6306845948056));
#143201=CARTESIAN_POINT('Ctrl Pts',(6.39796990775004,-2.86768331968942,
73.6394241151227));
#143202=CARTESIAN_POINT('Ctrl Pts',(6.47630853837843,-2.69290523386191,
73.6481532405281));
#143203=CARTESIAN_POINT('Ctrl Pts',(6.54753107721928,-2.51480449984745,
73.6568823659336));
#143204=CARTESIAN_POINT('Ctrl Pts',(6.61137137601919,-2.33396552906296,
73.665611491339));
#143205=CARTESIAN_POINT('Ctrl Pts',(6.67714570110341,-2.1476480857572,73.67460506347));
#143206=CARTESIAN_POINT('Ctrl Pts',(6.73508331753212,-1.95842413667652,
73.6835986356009));
#143207=CARTESIAN_POINT('Ctrl Pts',(6.78494573670534,-1.76695724692594,
73.6925922077319));
#143208=CARTESIAN_POINT('Ctrl Pts',(6.83320011183776,-1.5816650914979,73.7012957405845));
#143209=CARTESIAN_POINT('Ctrl Pts',(6.87389189068418,-1.39427269803777,
73.7099992734372));
#143210=CARTESIAN_POINT('Ctrl Pts',(6.90685442182102,-1.20539975040292,
73.7187028062899));
#143211=CARTESIAN_POINT('Ctrl Pts',(6.9414646336589,-1.00708571010822,73.72784139806));
#143212=CARTESIAN_POINT('Ctrl Pts',(6.96755298493941,-0.807139581817272,
73.73697998983));
#143213=CARTESIAN_POINT('Ctrl Pts',(6.98498622485248,-0.606295308509952,
73.7461185816001));
#143214=CARTESIAN_POINT('Ctrl Pts',(7.0015461796038,-0.415511948984274,
73.7547993929099));
#143215=CARTESIAN_POINT('Ctrl Pts',(7.01029680999461,-0.223918551223194,
73.7634802042197));
#143216=CARTESIAN_POINT('Ctrl Pts',(7.01117626839302,-0.0321542535674641,
73.7721610155295));
#143217=CARTESIAN_POINT('Ctrl Pts',(7.01122264641647,-0.0220416102536277,
73.7726187959898));
#143218=CARTESIAN_POINT('Ctrl Pts',(7.01124714700305,-0.0119284933641162,
73.7730765764501));
#143219=CARTESIAN_POINT('Ctrl Pts',(7.0112497650765,-0.00181499715760335,
73.7735343569104));
#143220=CARTESIAN_POINT('Ctrl Pts',(7.01124976619934,-0.00181065449666946,
73.773534553478));
#143221=CARTESIAN_POINT('Ctrl Pts',(7.01130032134908,0.193949929554239,
73.7823955219703));
#143222=CARTESIAN_POINT('Ctrl Pts',(7.00314781087931,0.38956846135378,73.7912564904627));
#143223=CARTESIAN_POINT('Ctrl Pts',(6.98685399846189,0.584378102496293,
73.8001174589551));
#143224=CARTESIAN_POINT('Ctrl Pts',(6.97052503348697,0.7796080293851,73.8089975442567));
#143225=CARTESIAN_POINT('Ctrl Pts',(6.94601965073969,0.974025329710912,
73.8178776295584));
#143226=CARTESIAN_POINT('Ctrl Pts',(6.91345145316409,1.16696853738365,73.82675771486));
#143227=CARTESIAN_POINT('Ctrl Pts',(6.88084931454048,1.36011282141808,73.8356470545701));
#143228=CARTESIAN_POINT('Ctrl Pts',(6.840167620754,1.55177970339379,73.8445363942802));
#143229=CARTESIAN_POINT('Ctrl Pts',(6.79157087268327,1.74131893799506,73.8534257339902));
#143230=CARTESIAN_POINT('Ctrl Pts',(6.7429094431003,1.93111044635558,73.8623269052725));
#143231=CARTESIAN_POINT('Ctrl Pts',(6.6863119604482,2.11876840904201,73.8712280765548));
#143232=CARTESIAN_POINT('Ctrl Pts',(6.62199304558498,2.30365680315539,73.8801292478371));
#143233=CARTESIAN_POINT('Ctrl Pts',(6.60553559337101,2.35096468945151,73.8824068142628));
#143234=CARTESIAN_POINT('Ctrl Pts',(6.58857286076634,2.39809134540819,73.8846843806884));
#143235=CARTESIAN_POINT('Ctrl Pts',(6.57110895151812,2.44502632087642,73.8869619471141));
#143236=CARTESIAN_POINT('',(7.01125,-1.99357674465772E-12,73.2264656430894));
#143237=CARTESIAN_POINT('Ctrl Pts',(6.57110895151812,2.44502632087643,73.339830038482));
#143238=CARTESIAN_POINT('Ctrl Pts',(6.64576037121474,2.24439755544203,73.330080824681));
#143239=CARTESIAN_POINT('Ctrl Pts',(6.71123467403681,2.04030721866428,73.3203316108801));
#143240=CARTESIAN_POINT('Ctrl Pts',(6.76726039322619,1.83352483832973,73.3105823970792));
#143241=CARTESIAN_POINT('Ctrl Pts',(6.77916262307297,1.78959552417517,73.3085112521628));
#143242=CARTESIAN_POINT('Ctrl Pts',(6.79063859508601,1.74554478499926,73.3064401072465));
#143243=CARTESIAN_POINT('Ctrl Pts',(6.80168598724614,1.70138011431884,73.3043689623301));
#143244=CARTESIAN_POINT('Ctrl Pts',(6.8449702867887,1.52834046774678,73.2962541008627));
#143245=CARTESIAN_POINT('Ctrl Pts',(6.88169100112489,1.35347215331281,73.2881392393953));
#143246=CARTESIAN_POINT('Ctrl Pts',(6.9116968681817,1.1773160004295,73.2800243779279));
#143247=CARTESIAN_POINT('Ctrl Pts',(6.94168248721581,1.00127871809161,73.2719149923863));
#143248=CARTESIAN_POINT('Ctrl Pts',(6.96496221977511,0.823955678815036,
73.2638056068446));
#143249=CARTESIAN_POINT('Ctrl Pts',(6.98143534720025,0.645900189938756,
73.2556962213029));
#143250=CARTESIAN_POINT('Ctrl Pts',(6.99789894399179,0.46794771620836,73.2475915274983));
#143251=CARTESIAN_POINT('Ctrl Pts',(7.00756374903666,0.289263992916175,
73.2394868336937));
#143252=CARTESIAN_POINT('Ctrl Pts',(7.01038060736404,0.11040970244574,73.2313821398891));
#143253=CARTESIAN_POINT('Ctrl Pts',(7.01095019807634,0.0742439706740013,
73.2297433076226));
#143254=CARTESIAN_POINT('Ctrl Pts',(7.01123995951458,0.0380712819471819,
73.228104475356));
#143255=CARTESIAN_POINT('Ctrl Pts',(7.01124974356013,0.00189629324868483,
73.2264656430895));
#143256=CARTESIAN_POINT('Ctrl Pts',(7.01125,-8.58630487052188E-16,73.2264656430895));
#143257=CARTESIAN_POINT('Ctrl Pts',(7.01125,-0.191009525814159,73.2177938341507));
#143258=CARTESIAN_POINT('Ctrl Pts',(7.00344006572044,-0.38201890962812,
73.209122025212));
#143259=CARTESIAN_POINT('Ctrl Pts',(6.98784625534325,-0.572390840410128,
73.2004502162732));
#143260=CARTESIAN_POINT('Ctrl Pts',(6.97225246786088,-0.762762491688126,
73.1917784200664));
#143261=CARTESIAN_POINT('Ctrl Pts',(6.94887485033549,-0.952496408756088,
73.1831066238596));
#143262=CARTESIAN_POINT('Ctrl Pts',(6.91779140296553,-1.140959538089,73.1744348276527));
#143263=CARTESIAN_POINT('Ctrl Pts',(6.88670800059844,-1.32942239456338,
73.165763044001));
#143264=CARTESIAN_POINT('Ctrl Pts',(6.84791883692786,-1.51661418677323,
73.1570912603493));
#143265=CARTESIAN_POINT('Ctrl Pts',(6.80155333291415,-1.70191034488437,
73.1484194766976));
#143266=CARTESIAN_POINT('Ctrl Pts',(6.75518789508331,-1.88720623850081,
73.1397477054241));
#143267=CARTESIAN_POINT('Ctrl Pts',(6.7012462074874,-2.07060622793232,73.1310759341506));
#143268=CARTESIAN_POINT('Ctrl Pts',(6.63990824732733,-2.25149839652942,
73.1224041628772));
#143269=CARTESIAN_POINT('Ctrl Pts',(6.57857037347141,-2.43239031060637,
73.1137324038051));
#143270=CARTESIAN_POINT('Ctrl Pts',(6.50983633907402,-2.61077414195845,
73.105060644733));
#143271=CARTESIAN_POINT('Ctrl Pts',(6.43393547556492,-2.78605471209149,
73.096388885661));
#143272=CARTESIAN_POINT('Ctrl Pts',(6.35803471730284,-2.96133503917383,
73.0877171386135));
#143273=CARTESIAN_POINT('Ctrl Pts',(6.27496726266488,-3.13351185304139,
73.0790453915661));
#143274=CARTESIAN_POINT('Ctrl Pts',(6.18501026583716,-3.30201068653465,
73.0703736445186));
#143275=CARTESIAN_POINT('Ctrl Pts',(6.09151188669153,-3.47714289831489,
73.0613605124456));
#143276=CARTESIAN_POINT('Ctrl Pts',(5.99057066119507,-3.64830137930445,
73.0523473803726));
#143277=CARTESIAN_POINT('Ctrl Pts',(5.88255038916944,-3.81486926137482,
73.0433342482996));
#143278=CARTESIAN_POINT('Ctrl Pts',(5.7762179338942,-3.97883452028786,73.0344619464152));
#143279=CARTESIAN_POINT('Ctrl Pts',(5.66302622906759,-4.13835132493216,
73.0255896445308));
#143280=CARTESIAN_POINT('Ctrl Pts',(5.54337059053299,-4.29286257158483,
73.0167173426465));
#143281=CARTESIAN_POINT('Ctrl Pts',(5.4255845713505,-4.44495958000855,73.007983670479));
#143282=CARTESIAN_POINT('Ctrl Pts',(5.30153533575357,-4.59220608123619,
72.9992499983116));
#143283=CARTESIAN_POINT('Ctrl Pts',(5.17164269972743,-4.73410375349506,
72.9905163261442));
#143284=CARTESIAN_POINT('Ctrl Pts',(5.04265587432023,-4.8750118976154,72.9818435585302));
#143285=CARTESIAN_POINT('Ctrl Pts',(4.90790710164581,-5.01064538261517,
72.9731707909162));
#143286=CARTESIAN_POINT('Ctrl Pts',(4.76784607609706,-5.14055156156865,
72.9644980233022));
#143287=CARTESIAN_POINT('Ctrl Pts',(4.62778576967854,-5.27045707353101,
72.9558253002178));
#143288=CARTESIAN_POINT('Ctrl Pts',(4.48241347330293,-5.39463514506075,
72.9471525771333));
#143289=CARTESIAN_POINT('Ctrl Pts',(4.33221433006009,-5.5126713634065,72.9384798540488));
#143290=CARTESIAN_POINT('Ctrl Pts',(4.18201594574026,-5.63070698534137,
72.9298071747857));
#143291=CARTESIAN_POINT('Ctrl Pts',(4.0269909867703,-5.74260064062169,72.9211344955226));
#143292=CARTESIAN_POINT('Ctrl Pts',(3.86765680432516,-5.84797891638276,
72.9124618162595));
#143293=CARTESIAN_POINT('Ctrl Pts',(3.70832341395466,-5.95335666829228,
72.9037891801095));
#143294=CARTESIAN_POINT('Ctrl Pts',(3.54468107997153,-6.0522189487556,72.8951165439596));
#143295=CARTESIAN_POINT('Ctrl Pts',(3.37727590613509,-6.14423583664718,
72.8864439078097));
#143296=CARTESIAN_POINT('Ctrl Pts',(3.20987155083152,-6.23625227461928,
72.877771314065));
#143297=CARTESIAN_POINT('Ctrl Pts',(3.03870464148727,-6.32142325013406,
72.8690987203202));
#143298=CARTESIAN_POINT('Ctrl Pts',(2.86434638713613,-6.39946453517794,
72.8604261265754));
#143299=CARTESIAN_POINT('Ctrl Pts',(2.68998897108409,-6.47750544500621,
72.8517535745277));
#143300=CARTESIAN_POINT('Ctrl Pts',(2.51244050006166,-6.5484166168845,72.84308102248));
#143301=CARTESIAN_POINT('Ctrl Pts',(2.33229347361646,-6.6119614121247,72.8344084704323));
#143302=CARTESIAN_POINT('Ctrl Pts',(2.15214729859961,-6.67550590703332,
72.8257359593736));
#143303=CARTESIAN_POINT('Ctrl Pts',(1.96940286067366,-6.73168400046206,
72.8170634483149));
#143304=CARTESIAN_POINT('Ctrl Pts',(1.78466999316304,-6.7803082214604,72.8083909372563));
#143305=CARTESIAN_POINT('Ctrl Pts',(1.59993798367808,-6.82893221661463,
72.7997184664787));
#143306=CARTESIAN_POINT('Ctrl Pts',(1.41321783784243,-6.87000233722938,
72.7910459957011));
#143307=CARTESIAN_POINT('Ctrl Pts',(1.22513265046473,-6.90338153018253,
72.7823735249235));
#143308=CARTESIAN_POINT('Ctrl Pts',(1.03704832133351,-6.93676057082398,
72.773701093719));
#143309=CARTESIAN_POINT('Ctrl Pts',(0.847599242857963,-6.96244870438738,
72.7650286625146));
#143310=CARTESIAN_POINT('Ctrl Pts',(0.657417610672671,-6.98036020902055,
72.7563562313101));
#143311=CARTESIAN_POINT('Ctrl Pts',(0.467236830779674,-6.99827163338395,
72.7476838389708));
#143312=CARTESIAN_POINT('Ctrl Pts',(0.276323786592565,-7.00840647191832,
72.7390114466316));
#143313=CARTESIAN_POINT('Ctrl Pts',(0.0853155533264802,-7.01073090475313,
72.7303390542923));
#143314=CARTESIAN_POINT('Ctrl Pts',(-0.105691839529951,-7.01305532736075,
72.7216667001103));
#143315=CARTESIAN_POINT('Ctrl Pts',(-0.296794136556739,-7.00756940957932,
72.7129943459284));
#143316=CARTESIAN_POINT('Ctrl Pts',(-0.48735363660962,-6.99429145770917,
72.7043219917464));
#143317=CARTESIAN_POINT('Ctrl Pts',(-0.677912313777361,-6.98101356317664,
72.6956496750139));
#143318=CARTESIAN_POINT('Ctrl Pts',(-0.867927915263419,-6.95994372163552,
72.6869773582814));
#143319=CARTESIAN_POINT('Ctrl Pts',(-1.0567663716562,-6.93115224174427,
72.678305041549));
#143320=CARTESIAN_POINT('Ctrl Pts',(-1.2456040280048,-6.90236088383271,
72.6696327615581));
#143321=CARTESIAN_POINT('Ctrl Pts',(-1.43326426840602,-6.86584799585282,
72.6609604815673));
#143322=CARTESIAN_POINT('Ctrl Pts',(-1.61912088843213,-6.82173541784953,
72.6522882015764));
#143323=CARTESIAN_POINT('Ctrl Pts',(-1.80497673621251,-6.77762302313673,
72.6436159576195));
#143324=CARTESIAN_POINT('Ctrl Pts',(-1.98902870221951,-6.72591106719145,
72.6349437136625));
#143325=CARTESIAN_POINT('Ctrl Pts',(-2.17066262759359,-6.66677210647466,
72.6262714697055));
#143326=CARTESIAN_POINT('Ctrl Pts',(-2.35229581308771,-6.60763338665851,
72.6175992610746));
#143327=CARTESIAN_POINT('Ctrl Pts',(-2.53151070754872,-6.54106781055818,
72.6089270524437));
#143328=CARTESIAN_POINT('Ctrl Pts',(-2.70770929769928,-6.46729749753735,
72.6002548438129));
#143329=CARTESIAN_POINT('Ctrl Pts',(-2.88390718448732,-6.39352747899829,
72.5915826698004));
#143330=CARTESIAN_POINT('Ctrl Pts',(-3.05708852903611,-6.31255289079463,
72.5829104957879));
#143331=CARTESIAN_POINT('Ctrl Pts',(-3.22667545573025,-6.22464393085163,
72.5742383217753));
#143332=CARTESIAN_POINT('Ctrl Pts',(-3.39626171929099,-6.1367353146578,
72.5655661816735));
#143333=CARTESIAN_POINT('Ctrl Pts',(-3.56225334093561,-6.04189251171209,
72.5568940415717));
#143334=CARTESIAN_POINT('Ctrl Pts',(-3.72409644021389,-5.94043199325489,
72.5482219014698));
#143335=CARTESIAN_POINT('Ctrl Pts',(-3.88593891984383,-5.83897186325936,
72.539549794571));
#143336=CARTESIAN_POINT('Ctrl Pts',(-4.04363266822376,-5.73089421933132,
72.5308776876722));
#143337=CARTESIAN_POINT('Ctrl Pts',(-4.19665149725252,-5.61655969193849,
72.5222055807734));
#143338=CARTESIAN_POINT('Ctrl Pts',(-4.34966975290223,-5.50222559297022,
72.5135335063699));
#143339=CARTESIAN_POINT('Ctrl Pts',(-4.49801289671247,-5.38163482747179,
72.5048614319665));
#143340=CARTESIAN_POINT('Ctrl Pts',(-4.64118594512446,-5.25518977633341,
72.496189357563));
#143341=CARTESIAN_POINT('Ctrl Pts',(-4.78435846873139,-5.12874518868312,
72.4875173149473));
#143342=CARTESIAN_POINT('Ctrl Pts',(-4.92236072196475,-4.9964465463588,
72.4788452723316));
#143343=CARTESIAN_POINT('Ctrl Pts',(-5.05473222957506,-4.85873529324198,
72.4701732297159));
#143344=CARTESIAN_POINT('Ctrl Pts',(-5.18710326277225,-4.72102453367566,
72.4615012181804));
#143345=CARTESIAN_POINT('Ctrl Pts',(-5.31384339389555,-4.57790140690936,
72.4528292066449));
#143346=CARTESIAN_POINT('Ctrl Pts',(-5.43452972930209,-4.42984347170775,
72.4441571951094));
#143347=CARTESIAN_POINT('Ctrl Pts',(-5.55521564202016,-4.28178605506015,
72.4354852139465));
#143348=CARTESIAN_POINT('Ctrl Pts',(-5.66984762199455,-4.12879408471962,
72.4268132327835));
#143349=CARTESIAN_POINT('Ctrl Pts',(-5.77804317951233,-3.97137804523707,
72.4181412516206));
#143350=CARTESIAN_POINT('Ctrl Pts',(-5.88623836691534,-3.81396254424245,
72.4094693001228));
#143351=CARTESIAN_POINT('Ctrl Pts',(-5.98799701504128,-3.65212323845831,
72.400797348625));
#143352=CARTESIAN_POINT('Ctrl Pts',(-6.08297959062815,-3.4864001294317,
72.3921253971271));
#143353=CARTESIAN_POINT('Ctrl Pts',(-6.17796184904699,-3.32067757379155,
72.3834534745869));
#143354=CARTESIAN_POINT('Ctrl Pts',(-6.26616793897404,-3.15107148727796,
72.3747815520466));
#143355=CARTESIAN_POINT('Ctrl Pts',(-6.34730354928998,-2.97814778271174,
72.3661096295063));
#143356=CARTESIAN_POINT('Ctrl Pts',(-6.42843889529457,-2.80522464147027,
72.3574377352162));
#143357=CARTESIAN_POINT('Ctrl Pts',(-6.50250368713934,-2.62898416092365,
72.348765840926));
#143358=CARTESIAN_POINT('Ctrl Pts',(-6.56925079959824,-2.45001438658591,
72.3400939466358));
#143359=CARTESIAN_POINT('Ctrl Pts',(-6.6359977000629,-2.27104518067068,
72.3314220798883));
#143360=CARTESIAN_POINT('Ctrl Pts',(-6.69542686840552,-2.08934696441759,
72.3227502131407));
#143361=CARTESIAN_POINT('Ctrl Pts',(-6.74734001400655,-1.90552598982173,
72.3140783463932));
#143362=CARTESIAN_POINT('Ctrl Pts',(-6.79925299896168,-1.72170558406226,
72.3054065064808));
#143363=CARTESIAN_POINT('Ctrl Pts',(-6.84364993053014,-1.53576270642159,
72.2967346665685));
#143364=CARTESIAN_POINT('Ctrl Pts',(-6.8803826753814,-1.348317767743,72.2880628266562));
#143365=CARTESIAN_POINT('Ctrl Pts',(-6.917115309559,-1.16087339382533,72.2793910128716));
#143366=CARTESIAN_POINT('Ctrl Pts',(-6.94618374861263,-0.971927246627463,
72.270719199087));
#143367=CARTESIAN_POINT('Ctrl Pts',(-6.96749100433575,-0.782109753807224,
72.2620473853025));
#143368=CARTESIAN_POINT('Ctrl Pts',(-6.98879819759914,-0.592292817414787,
72.2533755969383));
#143369=CARTESIAN_POINT('Ctrl Pts',(-7.00234422137905,-0.401604822737071,
72.2447038085741));
#143370=CARTESIAN_POINT('Ctrl Pts',(-7.00808387899823,-0.210682005461113,
72.23603202021));
#143371=CARTESIAN_POINT('Ctrl Pts',(-7.01382352026043,-0.0197597322806402,
72.2273602565588));
#143372=CARTESIAN_POINT('Ctrl Pts',(-7.01175683134626,0.171397078292984,
72.2186884929077));
#143373=CARTESIAN_POINT('Ctrl Pts',(-7.00189070778028,0.362150629987307,
72.2100167292565));
#143374=CARTESIAN_POINT('Ctrl Pts',(-6.99157808297349,0.561536923502758,
72.2009525163112));
#143375=CARTESIAN_POINT('Ctrl Pts',(-6.97274368607662,0.76048227793352,
72.1918883033658));
#143376=CARTESIAN_POINT('Ctrl Pts',(-6.94545616842971,0.958261537849481,
72.1828240904204));
#143377=CARTESIAN_POINT('Ctrl Pts',(-6.91902138570928,1.14986019589306,
72.1740431341296));
#143378=CARTESIAN_POINT('Ctrl Pts',(-6.88465388689505,1.34036422798524,
72.1652621778388));
#143379=CARTESIAN_POINT('Ctrl Pts',(-6.84247124235475,1.52912192452015,
72.156481221548));
#143380=CARTESIAN_POINT('Ctrl Pts',(-6.80080846652573,1.71555332735041,
72.1478084838025));
#143381=CARTESIAN_POINT('Ctrl Pts',(-6.7515221588282,1.90028091507621,72.139135746057));
#143382=CARTESIAN_POINT('Ctrl Pts',(-6.69477680034255,2.08268820424354,
72.1304630083115));
#143383=CARTESIAN_POINT('Ctrl Pts',(-6.63803201373481,2.26509365511603,
72.1217903579696));
#143384=CARTESIAN_POINT('Ctrl Pts',(-6.57382841117027,2.44517858290671,
72.1131177076277));
#143385=CARTESIAN_POINT('Ctrl Pts',(-6.5023802522632,2.62234201001271,72.1044450572858));
#143386=CARTESIAN_POINT('Ctrl Pts',(-6.43093279008113,2.79950370951384,
72.095772491515));
#143387=CARTESIAN_POINT('Ctrl Pts',(-6.35224101919408,2.97374370183285,
72.0870999257442));
#143388=CARTESIAN_POINT('Ctrl Pts',(-6.26656754386888,3.14448052635553,
72.0784273599734));
#143389=CARTESIAN_POINT('Ctrl Pts',(-6.18089487601678,3.31521574168246,
72.0697548759417));
#143390=CARTESIAN_POINT('Ctrl Pts',(-6.08824076282718,3.48244760134581,
72.0610823919099));
#143391=CARTESIAN_POINT('Ctrl Pts',(-5.98891439682431,3.64561804225437,
72.0524099078781));
#143392=CARTESIAN_POINT('Ctrl Pts',(-5.88958893454844,3.80878699854671,
72.0437375027534));
#143393=CARTESIAN_POINT('Ctrl Pts',(-5.7835914886656,3.96789436735514,72.0350650976288));
#143394=CARTESIAN_POINT('Ctrl Pts',(-5.67127577279886,4.12240920717057,
72.0263926925041));
#143395=CARTESIAN_POINT('Ctrl Pts',(-5.55896104218094,4.27692269156069,
72.017720363455));
#143396=CARTESIAN_POINT('Ctrl Pts',(-5.44032831952585,4.42684349778002,
72.0090480344059));
#143397=CARTESIAN_POINT('Ctrl Pts',(-5.31577347545426,4.5716713486598,72.0003757053567));
#143398=CARTESIAN_POINT('Ctrl Pts',(-5.19121968333993,4.71649797636188,
71.9917034495518));
#143399=CARTESIAN_POINT('Ctrl Pts',(-5.06074405512955,4.85623151941838,
71.9830311937469));
#143400=CARTESIAN_POINT('Ctrl Pts',(-4.92478197319633,4.99040570284426,
71.9743589379419));
#143401=CARTESIAN_POINT('Ctrl Pts',(-4.78882099518712,5.1245787968627,71.9656867525501));
#143402=CARTESIAN_POINT('Ctrl Pts',(-4.64737385478674,5.25319242204627,
71.9570145671583));
#143403=CARTESIAN_POINT('Ctrl Pts',(-4.5009125374034,5.37581741627679,71.9483423817664));
#143404=CARTESIAN_POINT('Ctrl Pts',(-4.35445236139157,5.49844145489202,
71.9396702639568));
#143405=CARTESIAN_POINT('Ctrl Pts',(-4.20297830438701,5.6150767735941,71.9309981461472));
#143406=CARTESIAN_POINT('Ctrl Pts',(-4.04699580206867,5.72533418592649,
71.9223260283377));
#143407=CARTESIAN_POINT('Ctrl Pts',(-3.89101446441665,5.83559077500569,
71.9136539752797));
#143408=CARTESIAN_POINT('Ctrl Pts',(-3.73052498076179,5.93946938905685,
71.9049819222218));
#143409=CARTESIAN_POINT('Ctrl Pts',(-3.56606286129387,6.03662341311769,
71.8963098691638));
#143410=CARTESIAN_POINT('Ctrl Pts',(-3.40160191613826,6.13377674346761,
71.8876378780271));
#143411=CARTESIAN_POINT('Ctrl Pts',(-3.2331686364828,6.22420543544664,71.8789658868904));
#143412=CARTESIAN_POINT('Ctrl Pts',(-3.06132503080748,6.30760775716528,
71.8702938957537));
#143413=CARTESIAN_POINT('Ctrl Pts',(-2.88948259607709,6.39100951057923,
71.8616219637081));
#143414=CARTESIAN_POINT('Ctrl Pts',(-2.71423013734766,6.46738486552798,
71.8529500316625));
#143415=CARTESIAN_POINT('Ctrl Pts',(-2.53615240857771,6.53647898512383,
71.8442780996169));
#143416=CARTESIAN_POINT('Ctrl Pts',(-2.35807583512656,6.60557265645625,
71.8356062238323));
#143417=CARTESIAN_POINT('Ctrl Pts',(-2.17717429309618,6.66738508422991,
71.8269343480478));
#143418=CARTESIAN_POINT('Ctrl Pts',(-1.99405137756518,6.72171002544222,
71.8182624722632));
#143419=CARTESIAN_POINT('Ctrl Pts',(-1.8109295903359,6.77603463193441,71.80959064991));
#143420=CARTESIAN_POINT('Ctrl Pts',(-1.62558672927165,6.82287176341051,
71.8009188275567));
#143421=CARTESIAN_POINT('Ctrl Pts',(-1.43864120071842,6.8620651452821,71.7922470052035));
#143422=CARTESIAN_POINT('Ctrl Pts',(-1.25169676302724,6.90125829845299,
71.7835752334519));
#143423=CARTESIAN_POINT('Ctrl Pts',(-1.06314995451508,6.93280773300066,
71.7749034617004));
#143424=CARTESIAN_POINT('Ctrl Pts',(-0.873629864335108,6.9566081837805,
71.7662316899488));
#143425=CARTESIAN_POINT('Ctrl Pts',(-0.67949550972214,6.98098810649611,
71.7573487857103));
#143426=CARTESIAN_POINT('Ctrl Pts',(-0.484340182097022,6.99723686027412,
71.7484658814718));
#143427=CARTESIAN_POINT('Ctrl Pts',(-0.288847078981576,7.00529756166459,
71.7395829772334));
#143428=CARTESIAN_POINT('Ctrl Pts',(-0.0979805524071825,7.01316749698012,
71.730910297477));
#143429=CARTESIAN_POINT('Ctrl Pts',(0.0932076478762551,7.0132325545162,
71.7222376177207));
#143430=CARTESIAN_POINT('Ctrl Pts',(0.284079486213397,7.005492517162,71.7135649379643));
#143431=CARTESIAN_POINT('Ctrl Pts',(0.474947621905027,6.99775262995365,
71.7048924264458));
#143432=CARTESIAN_POINT('Ctrl Pts',(0.665499124040627,6.98220796234813,
71.6962199149273));
#143433=CARTESIAN_POINT('Ctrl Pts',(0.855098106408511,6.95891038819416,
71.6875474034087));
#143434=CARTESIAN_POINT('Ctrl Pts',(1.0446936584049,6.93561323555793,71.6788750488));
#143435=CARTESIAN_POINT('Ctrl Pts',(1.23333644314323,6.90456349171855,71.6702026941912));
#143436=CARTESIAN_POINT('Ctrl Pts',(1.4203969667169,6.86586476850815,71.6615303395825));
#143437=CARTESIAN_POINT('Ctrl Pts',(1.60745435008166,6.82716669493816,71.6528581305576));
#143438=CARTESIAN_POINT('Ctrl Pts',(1.79292924725158,6.78081995649635,71.6441859215328));
#143439=CARTESIAN_POINT('Ctrl Pts',(1.9762027562011,6.72697920532561,71.635513712508));
#143440=CARTESIAN_POINT('Ctrl Pts',(2.15947342777526,6.67313928769825,71.6268416377432));
#143441=CARTESIAN_POINT('Ctrl Pts',(2.3405425067949,6.61180566957133,71.6181695629785));
#143442=CARTESIAN_POINT('Ctrl Pts',(2.51880581148067,6.54318300573591,71.6094974882137));
#143443=CARTESIAN_POINT('Ctrl Pts',(2.69706658904941,6.47456131471709,71.600825536387));
#143444=CARTESIAN_POINT('Ctrl Pts',(2.87252140681086,6.39865088680505,71.5921535845603));
#143445=CARTESIAN_POINT('Ctrl Pts',(3.04458483293961,6.31570500874875,71.5834816327337));
#143446=CARTESIAN_POINT('Ctrl Pts',(3.21664604441903,6.23276019829896,71.5748097925247));
#143447=CARTESIAN_POINT('Ctrl Pts',(3.3853156957798,6.14278024224237,71.5661379523158));
#143448=CARTESIAN_POINT('Ctrl Pts',(3.55003100941456,6.04606536473888,71.5574661121068));
#143449=CARTESIAN_POINT('Ctrl Pts',(3.72225670715308,5.94494066119936,71.5483988693733));
#143450=CARTESIAN_POINT('Ctrl Pts',(3.89015872997921,5.83645264820113,71.5393316266397));
#143451=CARTESIAN_POINT('Ctrl Pts',(4.05312466659174,5.72099702845279,71.5302643839061));
#143452=CARTESIAN_POINT('Ctrl Pts',(4.20899688867359,5.61056705531797,71.5215918275277));
#143453=CARTESIAN_POINT('Ctrl Pts',(4.36035338103252,5.49376336254134,71.5129192711493));
#143454=CARTESIAN_POINT('Ctrl Pts',(4.50668904924442,5.37097573778922,71.5042467147709));
#143455=CARTESIAN_POINT('Ctrl Pts',(4.65301950883502,5.24819248349745,71.4955744670804));
#143456=CARTESIAN_POINT('Ctrl Pts',(4.79432928426434,5.11942590604493,71.48690221939));
#143457=CARTESIAN_POINT('Ctrl Pts',(4.93014684172017,4.98510568409303,71.4782299716995));
#143458=CARTESIAN_POINT('Ctrl Pts',(5.06596027419377,4.85078954164705,71.4695579873982));
#143459=CARTESIAN_POINT('Ctrl Pts',(5.19628162052971,4.71092029196069,71.4608860030969));
#143460=CARTESIAN_POINT('Ctrl Pts',(5.32067604037713,4.56596463366251,71.4522140187955));
#143461=CARTESIAN_POINT('Ctrl Pts',(5.44506733163951,4.42101262107531,71.4435422525992));
#143462=CARTESIAN_POINT('Ctrl Pts',(5.56353180975275,4.2709746713911,71.4348704864028));
#143463=CARTESIAN_POINT('Ctrl Pts',(5.67567421677841,4.11635138775795,71.4261987202064));
#143464=CARTESIAN_POINT('Ctrl Pts',(5.78782406005803,3.96171785092946,71.4175263789782));
#143465=CARTESIAN_POINT('Ctrl Pts',(5.89365082653992,3.80249860162828,71.40885403775));
#143466=CARTESIAN_POINT('Ctrl Pts',(5.99280137735697,3.63922494688751,71.4001816965218));
#143467=CARTESIAN_POINT('Ctrl Pts',(6.09194609290613,3.47596090122614,71.3915098656834));
#143468=CARTESIAN_POINT('Ctrl Pts',(6.18441523160251,3.3086431703721,71.3828380348451));
#143469=CARTESIAN_POINT('Ctrl Pts',(6.26990026462747,3.13783001995398,71.3741662040067));
#143470=CARTESIAN_POINT('Ctrl Pts',(6.35538670852191,2.96701405038669,71.365494230046));
#143471=CARTESIAN_POINT('Ctrl Pts',(6.43388868896847,2.79270279980033,71.3568222560852));
#143472=CARTESIAN_POINT('Ctrl Pts',(6.50514427077116,2.6154778872996,71.3481502821245));
#143473=CARTESIAN_POINT('Ctrl Pts',(6.52787183386102,2.55895052090873,71.3453842835834));
#143474=CARTESIAN_POINT('Ctrl Pts',(6.54986255129665,2.5021268966415,71.3426182850424));
#143475=CARTESIAN_POINT('Ctrl Pts',(6.57110895151817,2.44502632087629,71.3398522865014));
#143476=CARTESIAN_POINT('Origin',(0.,0.,50.));
#143477=CARTESIAN_POINT('',(6.57110895151815,2.44502632087633,69.3398494195812));
#143478=CARTESIAN_POINT('',(6.57110895151813,2.44502632087638,69.887000105296));
#143479=CARTESIAN_POINT('',(6.57110895151814,2.44502632087636,50.));
#143480=CARTESIAN_POINT('',(7.01124919374723,-0.00336239182316637,71.7735343569455));
#143481=CARTESIAN_POINT('Ctrl Pts',(6.57110895151813,2.44502632087638,69.887000105296));
#143482=CARTESIAN_POINT('Ctrl Pts',(6.50935707499648,2.61098703267723,69.8950229664158));
#143483=CARTESIAN_POINT('Ctrl Pts',(6.4413031944783,2.77463542245891,69.9030458275357));
#143484=CARTESIAN_POINT('Ctrl Pts',(6.36715806475345,2.93545988576665,69.9110686886556));
#143485=CARTESIAN_POINT('Ctrl Pts',(6.29301396543497,3.09628211407184,69.9190914382805));
#143486=CARTESIAN_POINT('Ctrl Pts',(6.21277894391802,3.25428016343137,69.9271141879055));
#143487=CARTESIAN_POINT('Ctrl Pts',(6.12671087069771,3.40896472105162,69.9351369375304));
#143488=CARTESIAN_POINT('Ctrl Pts',(6.04061153883583,3.563705457798,69.9431626008985));
#143489=CARTESIAN_POINT('Ctrl Pts',(5.94867510931066,3.71512998294193,69.9511882642665));
#143490=CARTESIAN_POINT('Ctrl Pts',(5.85120427308608,3.86277557167372,69.9592139276345));
#143491=CARTESIAN_POINT('Ctrl Pts',(5.8324204731663,3.89122864856521,69.9607605692842));
#143492=CARTESIAN_POINT('Ctrl Pts',(5.8134312644223,3.91954147243274,69.9623072109338));
#143493=CARTESIAN_POINT('Ctrl Pts',(5.79423899333395,3.94771086208556,69.9638538525834));
#143494=CARTESIAN_POINT('Ctrl Pts',(5.68590784636475,4.10671352917298,69.9725839014183));
#143495=CARTESIAN_POINT('Ctrl Pts',(5.57104950672155,4.26122332956056,69.9813139502533));
#143496=CARTESIAN_POINT('Ctrl Pts',(5.45005695875983,4.41072621104207,69.9900439990882));
#143497=CARTESIAN_POINT('Ctrl Pts',(5.32902942565171,4.56027232146855,69.9987765722276));
#143498=CARTESIAN_POINT('Ctrl Pts',(5.20186431613109,4.70480841024443,70.0075091453671));
#143499=CARTESIAN_POINT('Ctrl Pts',(5.0689946415254,4.84385382590007,70.0162417185065));
#143500=CARTESIAN_POINT('Ctrl Pts',(4.93423734109838,4.98487460363671,70.0250983517868));
#143501=CARTESIAN_POINT('Ctrl Pts',(4.79361235559935,5.1202473021447,70.0339549850671));
#143502=CARTESIAN_POINT('Ctrl Pts',(4.64761012010458,5.24950918981971,70.0428116183474));
#143503=CARTESIAN_POINT('Ctrl Pts',(4.50356138495889,5.37704156190312,70.0515497504545));
#143504=CARTESIAN_POINT('Ctrl Pts',(4.35427862401281,5.49862546533893,70.0602878825615));
#143505=CARTESIAN_POINT('Ctrl Pts',(4.200266932895,5.61385645122217,70.0690260146685));
#143506=CARTESIAN_POINT('Ctrl Pts',(4.04312232403179,5.73143147474227,70.0779418985354));
#143507=CARTESIAN_POINT('Ctrl Pts',(3.88105456657115,5.84239216862962,70.0868577824024));
#143508=CARTESIAN_POINT('Ctrl Pts',(3.71463300631888,5.94635419318984,70.0957736662693));
#143509=CARTESIAN_POINT('Ctrl Pts',(3.54821144606662,6.05031621775005,70.1046895501362));
#143510=CARTESIAN_POINT('Ctrl Pts',(3.37743634272625,6.1472794179211,70.1136054340031));
#143511=CARTESIAN_POINT('Ctrl Pts',(3.20290638631624,6.23690766670428,70.1225213178701));
#143512=CARTESIAN_POINT('Ctrl Pts',(3.03180598765053,6.3247746977513,70.1312620023661));
#143513=CARTESIAN_POINT('Ctrl Pts',(2.85707876118995,6.40560170126693,70.1400026868622));
#143514=CARTESIAN_POINT('Ctrl Pts',(2.67931053117118,6.47911426354369,70.1487433713582));
#143515=CARTESIAN_POINT('Ctrl Pts',(2.50157428460959,6.55261359968949,70.1574824832599));
#143516=CARTESIAN_POINT('Ctrl Pts',(2.32079838006797,6.61880101813621,70.1662215951617));
#143517=CARTESIAN_POINT('Ctrl Pts',(2.13758879099239,6.67745016627782,70.1749607070634));
#143518=CARTESIAN_POINT('Ctrl Pts',(1.95200545800082,6.73685919854604,70.1838130467378));
#143519=CARTESIAN_POINT('Ctrl Pts',(1.76392520167813,6.78853315221968,70.1926653864122));
#143520=CARTESIAN_POINT('Ctrl Pts',(1.57399524889274,6.83228845402206,70.2015177260866));
#143521=CARTESIAN_POINT('Ctrl Pts',(1.38659074028235,6.87546195411048,70.2102523587363));
#143522=CARTESIAN_POINT('Ctrl Pts',(1.19738569639967,6.91092602912153,70.2189869913858));
#143523=CARTESIAN_POINT('Ctrl Pts',(1.00701460405256,6.93855519180506,70.2277216240355));
#143524=CARTESIAN_POINT('Ctrl Pts',(0.812795379370071,6.96674284618504,
70.2366328172223));
#143525=CARTESIAN_POINT('Ctrl Pts',(0.617362747750107,6.98677540412073,
70.2455440104091));
#143526=CARTESIAN_POINT('Ctrl Pts',(0.421399684128626,6.99857477410339,
70.2544552035959));
#143527=CARTESIAN_POINT('Ctrl Pts',(0.225436620507078,7.01037414408606,
70.2633663967828));
#143528=CARTESIAN_POINT('Ctrl Pts',(0.0289434266559483,7.01394029444692,
70.2722775899696));
#143529=CARTESIAN_POINT('Ctrl Pts',(-0.167392073520737,7.00925149043908,
70.2811887831564));
#143530=CARTESIAN_POINT('Ctrl Pts',(-0.34421720681212,7.00502862502291,
70.2892144480088));
#143531=CARTESIAN_POINT('Ctrl Pts',(-0.520995680480194,6.994107460158,70.2972401128612));
#143532=CARTESIAN_POINT('Ctrl Pts',(-0.697174942038089,6.97650153462996,
70.3052657777136));
#143533=CARTESIAN_POINT('Ctrl Pts',(-0.873298288620175,6.9589011967908,
70.3132888954168));
#143534=CARTESIAN_POINT('Ctrl Pts',(-1.0488224373931,6.93462035856031,70.3213120131201));
#143535=CARTESIAN_POINT('Ctrl Pts',(-1.22319820765153,6.90372455326095,
70.3293351308233));
#143536=CARTESIAN_POINT('Ctrl Pts',(-1.39755198759958,6.87283264419297,
70.3373572367412));
#143537=CARTESIAN_POINT('Ctrl Pts',(-1.57075731675607,6.83532749421412,
70.3453793426591));
#143538=CARTESIAN_POINT('Ctrl Pts',(-1.7422735306847,6.79132604921715,70.353401448577));
#143539=CARTESIAN_POINT('Ctrl Pts',(-1.91385348061782,6.74730825313459,
70.3614265355366));
#143540=CARTESIAN_POINT('Ctrl Pts',(-2.08374270526499,6.69678942780533,
70.3694516224961));
#143541=CARTESIAN_POINT('Ctrl Pts',(-2.25141363242581,6.63993698902537,
70.3774767094557));
#143542=CARTESIAN_POINT('Ctrl Pts',(-2.41911758153682,6.58307335344204,
70.385503376916));
#143543=CARTESIAN_POINT('Ctrl Pts',(-2.58460201849845,6.51987374548574,
70.3935300443762));
#143544=CARTESIAN_POINT('Ctrl Pts',(-2.747357977816,6.4505542943402,70.4015567118365));
#143545=CARTESIAN_POINT('Ctrl Pts',(-2.91024459704388,6.38117919378367,
70.4095898230771));
#143546=CARTESIAN_POINT('Ctrl Pts',(-3.07039803027828,6.30567458973282,
70.4176229343178));
#143547=CARTESIAN_POINT('Ctrl Pts',(-3.22733204274851,6.22430353118714,
70.4256560455584));
#143548=CARTESIAN_POINT('Ctrl Pts',(-3.31980326383186,6.17635674752869,
70.4303894465199));
#143549=CARTESIAN_POINT('Ctrl Pts',(-3.41115718157247,6.12637399944037,
70.4351228474814));
#143550=CARTESIAN_POINT('Ctrl Pts',(-3.50129888771257,6.07441624038086,
70.4398562484429));
#143551=CARTESIAN_POINT('Ctrl Pts',(-3.68699360776641,5.96738163968023,
70.4496072017372));
#143552=CARTESIAN_POINT('Ctrl Pts',(-3.86765228367227,5.85190080474336,
70.4593581550316));
#143553=CARTESIAN_POINT('Ctrl Pts',(-4.04260209641249,5.72843738314222,
70.469109108326));
#143554=CARTESIAN_POINT('Ctrl Pts',(-4.21780395717759,5.60479608932122,
70.4788741096978));
#143555=CARTESIAN_POINT('Ctrl Pts',(-4.38728047141502,5.47314922690004,
70.4886391110696));
#143556=CARTESIAN_POINT('Ctrl Pts',(-4.55038851878558,5.33400327058434,
70.4984041124415));
#143557=CARTESIAN_POINT('Ctrl Pts',(-4.71322469883662,5.19508924174724,
70.5081528375793));
#143558=CARTESIAN_POINT('Ctrl Pts',(-4.86971359808391,5.04870112491487,
70.5179015627171));
#143559=CARTESIAN_POINT('Ctrl Pts',(-5.01924811638757,4.89538301960529,
70.5276502878549));
#143560=CARTESIAN_POINT('Ctrl Pts',(-5.1683722204212,4.74248571304497,70.5373722565224));
#143561=CARTESIAN_POINT('Ctrl Pts',(-5.31058001986225,4.58269641717835,
70.5470942251898));
#143562=CARTESIAN_POINT('Ctrl Pts',(-5.44530257869364,4.41659443338105,
70.5568161938572));
#143563=CARTESIAN_POINT('Ctrl Pts',(-5.57913371353883,4.25159150302954,
70.5664738347971));
#143564=CARTESIAN_POINT('Ctrl Pts',(-5.70557828430508,4.08035916550015,
70.5761314757369));
#143565=CARTESIAN_POINT('Ctrl Pts',(-5.82411204847887,3.90350424737355,
70.5857891166768));
#143566=CARTESIAN_POINT('Ctrl Pts',(-5.87621171868739,3.825770422135,70.590033982361));
#143567=CARTESIAN_POINT('Ctrl Pts',(-5.9267835374794,3.74695087419612,70.5942788480452));
#143568=CARTESIAN_POINT('Ctrl Pts',(-5.97578510504719,3.66709952698262,
70.5985237137293));
#143569=CARTESIAN_POINT('Ctrl Pts',(-6.06642467779315,3.51939625229435,
70.6063755607432));
#143570=CARTESIAN_POINT('Ctrl Pts',(-6.15165117836031,3.36822136138251,
70.614227407757));
#143571=CARTESIAN_POINT('Ctrl Pts',(-6.23118342980272,3.21402856655819,
70.6220792547708));
#143572=CARTESIAN_POINT('Ctrl Pts',(-6.31069312654178,3.05987949956354,
70.6299288750643));
#143573=CARTESIAN_POINT('Ctrl Pts',(-6.38451161166049,2.90271456978279,
70.6377784953578));
#143574=CARTESIAN_POINT('Ctrl Pts',(-6.45240311453084,2.74301305321223,
70.6456281156512));
#143575=CARTESIAN_POINT('Ctrl Pts',(-6.52028919713257,2.58332428676625,
70.6534771092529));
#143576=CARTESIAN_POINT('Ctrl Pts',(-6.58224909093422,2.42109968803214,
70.6613261028546));
#143577=CARTESIAN_POINT('Ctrl Pts',(-6.63809483719363,2.25683927095469,
70.6691750964562));
#143578=CARTESIAN_POINT('Ctrl Pts',(-6.69396885651942,2.09249569363698,
70.6770280637736));
#143579=CARTESIAN_POINT('Ctrl Pts',(-6.74372242056195,1.92611460026772,
70.6848810310909));
#143580=CARTESIAN_POINT('Ctrl Pts',(-6.78721711243595,1.75821228273398,
70.6927339984082));
#143581=CARTESIAN_POINT('Ctrl Pts',(-6.83072285050017,1.59026732365346,
70.7005889601154));
#143582=CARTESIAN_POINT('Ctrl Pts',(-6.86796646776411,1.42080074334621,
70.7084439218225));
#143583=CARTESIAN_POINT('Ctrl Pts',(-6.89886066457496,1.25033919129185,
70.7162988835297));
#143584=CARTESIAN_POINT('Ctrl Pts',(-6.92978552645864,1.0797084418979,70.724161641943));
#143585=CARTESIAN_POINT('Ctrl Pts',(-6.95434832651003,0.908081125735139,
70.7320244003562));
#143586=CARTESIAN_POINT('Ctrl Pts',(-6.97251358095588,0.73598975936209,
70.7398871587695));
#143587=CARTESIAN_POINT('Ctrl Pts',(-6.985839350963,0.609746002340369,70.7456551655182));
#143588=CARTESIAN_POINT('Ctrl Pts',(-6.99572338168467,0.483252631127725,
70.751423172267));
#143589=CARTESIAN_POINT('Ctrl Pts',(-7.00216950191017,0.356719538319783,
70.7571911790158));
#143590=CARTESIAN_POINT('Ctrl Pts',(-7.01153253248355,0.172929417276306,
70.7655692454568));
#143591=CARTESIAN_POINT('Ctrl Pts',(-7.01366137701738,-0.0113515913451885,
70.7739473118978));
#143592=CARTESIAN_POINT('Ctrl Pts',(-7.00852298676297,-0.195530321216453,
70.7823253783389));
#143593=CARTESIAN_POINT('Ctrl Pts',(-7.00338811007876,-0.379583111860833,
70.7906977159576));
#143594=CARTESIAN_POINT('Ctrl Pts',(-6.99099591495639,-0.563533435639649,
70.7990700535764));
#143595=CARTESIAN_POINT('Ctrl Pts',(-6.97136540613591,-0.746787075833213,
70.8074423911951));
#143596=CARTESIAN_POINT('Ctrl Pts',(-6.95174544159702,-0.929942283632423,
70.8158102317177));
#143597=CARTESIAN_POINT('Ctrl Pts',(-6.92489495053787,-1.11240122787188,
70.8241780722404));
#143598=CARTESIAN_POINT('Ctrl Pts',(-6.89088489724594,-1.29357330499971,
70.832545912763));
#143599=CARTESIAN_POINT('Ctrl Pts',(-6.85688812980171,-1.4746746082124,
70.8409104844329));
#143600=CARTESIAN_POINT('Ctrl Pts',(-6.81573743799092,-1.65448972419131,
70.8492750561028));
#143601=CARTESIAN_POINT('Ctrl Pts',(-6.76755522877475,-1.83243629847905,
70.8576396277727));
#143602=CARTESIAN_POINT('Ctrl Pts',(-6.71938478897124,-2.01033940596234,
70.8660021562383));
#143603=CARTESIAN_POINT('Ctrl Pts',(-6.66418634327739,-2.18637456511051,
70.8743646847039));
#143604=CARTESIAN_POINT('Ctrl Pts',(-6.60213280590181,-2.35997224045857,
70.8827272131695));
#143605=CARTESIAN_POINT('Ctrl Pts',(-6.54007431646009,-2.53358376944347,
70.8910904089911));
#143606=CARTESIAN_POINT('Ctrl Pts',(-6.47115974733332,-2.70475711448229,
70.8994536048126));
#143607=CARTESIAN_POINT('Ctrl Pts',(-6.39561129658583,-2.8729397323097,
70.9078168006341));
#143608=CARTESIAN_POINT('Ctrl Pts',(-6.32005769358556,-3.04113381985424,
70.9161805668088));
#143609=CARTESIAN_POINT('Ctrl Pts',(-6.2378694413764,-3.20633647344641,
70.9245443329835));
#143610=CARTESIAN_POINT('Ctrl Pts',(-6.14931620337863,-3.3680167448166,
70.9329080991582));
#143611=CARTESIAN_POINT('Ctrl Pts',(-6.06074511999784,-3.52972959824066,
70.9412735508118));
#143612=CARTESIAN_POINT('Ctrl Pts',(-5.96580665108144,-3.68791836565289,
70.9496390024653));
#143613=CARTESIAN_POINT('Ctrl Pts',(-5.8648157864291,-3.84207786929834,
70.9580044541189));
#143614=CARTESIAN_POINT('Ctrl Pts',(-5.76379110013426,-3.99628900065919,
70.9663727073458));
#143615=CARTESIAN_POINT('Ctrl Pts',(-5.65671015643478,-4.14646790261302,
70.9747409605727));
#143616=CARTESIAN_POINT('Ctrl Pts',(-5.5439307587409,-4.2921391292439,70.9831092137996));
#143617=CARTESIAN_POINT('Ctrl Pts',(-5.43104679845622,-4.43794541388337,
70.9914852255911));
#143618=CARTESIAN_POINT('Ctrl Pts',(-5.31245402809057,-4.57923541155135,
70.9998612373825));
#143619=CARTESIAN_POINT('Ctrl Pts',(-5.18855075560524,-4.71556652153358,
71.008237249174));
#143620=CARTESIAN_POINT('Ctrl Pts',(-5.0645867194242,-4.85196448997658,
71.0166173686652));
#143621=CARTESIAN_POINT('Ctrl Pts',(-4.93530721340399,-4.98339848230032,
71.0249974881563));
#143622=CARTESIAN_POINT('Ctrl Pts',(-4.80114721921409,-5.10946297979864,
71.0333776076475));
#143623=CARTESIAN_POINT('Ctrl Pts',(-4.66683393023635,-5.23567152195436,
71.0417673024866));
#143624=CARTESIAN_POINT('Ctrl Pts',(-4.52762925404168,-5.35649808920436,
71.0501569973259));
#143625=CARTESIAN_POINT('Ctrl Pts',(-4.38400205491484,-5.47157678781926,
71.0585466921651));
#143626=CARTESIAN_POINT('Ctrl Pts',(-4.29281562472936,-5.54463826768434,
71.0638731646395));
#143627=CARTESIAN_POINT('Ctrl Pts',(-4.19984721973291,-5.61538375356384,
71.069199637114));
#143628=CARTESIAN_POINT('Ctrl Pts',(-4.10522283754347,-5.68372870716148,
71.0745261095884));
#143629=CARTESIAN_POINT('Ctrl Pts',(-3.95632966733252,-5.79127072301,71.0829074099934));
#143630=CARTESIAN_POINT('Ctrl Pts',(-3.80303460730352,-5.89308390277214,
71.0912887103984));
#143631=CARTESIAN_POINT('Ctrl Pts',(-3.64580334336631,-5.988801594977,71.0996700108033));
#143632=CARTESIAN_POINT('Ctrl Pts',(-3.48877134704022,-6.08439797901839,
71.1080406891369));
#143633=CARTESIAN_POINT('Ctrl Pts',(-3.32781336609375,-6.17391410190532,
71.1164113674705));
#143634=CARTESIAN_POINT('Ctrl Pts',(-3.16342614885192,-6.25702497703661,
71.124782045804));
#143635=CARTESIAN_POINT('Ctrl Pts',(-2.9992254828764,-6.34004153559474,
71.1331432248549));
#143636=CARTESIAN_POINT('Ctrl Pts',(-2.83160362760783,-6.41666718709266,
71.1415044039059));
#143637=CARTESIAN_POINT('Ctrl Pts',(-2.66108454776913,-6.48662127706901,
71.1498655829568));
#143638=CARTESIAN_POINT('Ctrl Pts',(-2.49078673655147,-6.55648459336161,
71.1582159123916));
#143639=CARTESIAN_POINT('Ctrl Pts',(-2.31759950116911,-6.61969349194116,
71.1665662418264));
#143640=CARTESIAN_POINT('Ctrl Pts',(-2.14206945952485,-6.67601415464879,
71.1749165712612));
#143641=CARTESIAN_POINT('Ctrl Pts',(-1.96667447774646,-6.73229148197587,
71.183260475617));
#143642=CARTESIAN_POINT('Ctrl Pts',(-1.78894059271763,-6.78169103585769,
71.1916043799728));
#143643=CARTESIAN_POINT('Ctrl Pts',(-1.60943344468846,-6.82402744349832,
71.1999482843287));
#143644=CARTESIAN_POINT('Ctrl Pts',(-1.43007047792197,-6.86632984627186,
71.2082854868084));
#143645=CARTESIAN_POINT('Ctrl Pts',(-1.24893740668833,-6.90158034212509,
71.2166226892882));
#143646=CARTESIAN_POINT('Ctrl Pts',(-1.06661419242548,-6.92964362193443,
71.2249598917679));
#143647=CARTESIAN_POINT('Ctrl Pts',(-1.00659439669826,-6.93888189874083,
71.2277044528036));
#143648=CARTESIAN_POINT('Ctrl Pts',(-0.946445732503702,-6.94734171020637,
71.2304490138393));
#143649=CARTESIAN_POINT('Ctrl Pts',(-0.886189172522259,-6.95501943297101,
71.233193574875));
#143650=CARTESIAN_POINT('Ctrl Pts',(-0.703122413099019,-6.97834528872355,
71.2415318851769));
#143651=CARTESIAN_POINT('Ctrl Pts',(-0.519209392211515,-6.99442936365933,
71.2498701954787));
#143652=CARTESIAN_POINT('Ctrl Pts',(-0.335045536714064,-7.003240039498,
71.2582085057805));
#143653=CARTESIAN_POINT('Ctrl Pts',(-0.150765811567265,-7.01205625871498,
71.2665520622643));
#143654=CARTESIAN_POINT('Ctrl Pts',(0.033764735698275,-7.01358993542551,
71.2748956187481));
#143655=CARTESIAN_POINT('Ctrl Pts',(0.217950683141193,-7.00786158983026,
71.2832391752318));
#143656=CARTESIAN_POINT('Ctrl Pts',(0.402276758448518,-7.0021288861347,
71.2915890794569));
#143657=CARTESIAN_POINT('Ctrl Pts',(0.586257383867467,-6.98912314990522,
71.299938983682));
#143658=CARTESIAN_POINT('Ctrl Pts',(0.769301819284021,-6.96891679340099,
71.3082888879071));
#143659=CARTESIAN_POINT('Ctrl Pts',(0.952620807809685,-6.94868012885713,
71.3166513163707));
#143660=CARTESIAN_POINT('Ctrl Pts',(1.13500047431318,-6.92122129742962,
71.3250137448343));
#143661=CARTESIAN_POINT('Ctrl Pts',(1.31585833880889,-6.88666417031404,
71.3333761732979));
#143662=CARTESIAN_POINT('Ctrl Pts',(1.49687086143248,-6.8520774921441,71.3417457527778));
#143663=CARTESIAN_POINT('Ctrl Pts',(1.67635866712909,-6.81038048101128,
71.3501153322576));
#143664=CARTESIAN_POINT('Ctrl Pts',(1.85375346567542,-6.76174715964716,
71.3584849117375));
#143665=CARTESIAN_POINT('Ctrl Pts',(2.03142187408473,-6.71303882731031,
71.366867400274));
#143666=CARTESIAN_POINT('Ctrl Pts',(2.20699051269871,-6.65737290495638,
71.3752498888104));
#143667=CARTESIAN_POINT('Ctrl Pts',(2.37990879088698,-6.59497238125823,
71.3836323773469));
#143668=CARTESIAN_POINT('Ctrl Pts',(2.43649048495389,-6.57455390740749,
71.3863752649517));
#143669=CARTESIAN_POINT('Ctrl Pts',(2.49278858440483,-6.55341473034262,
71.3891181525565));
#143670=CARTESIAN_POINT('Ctrl Pts',(2.54878435310448,-6.53156373955501,
71.3918610401613));
#143671=CARTESIAN_POINT('Ctrl Pts',(2.72006238382453,-6.46472664171179,
71.4002508952942));
#143672=CARTESIAN_POINT('Ctrl Pts',(2.8888558835757,-6.3910913488721,71.408640750427));
#143673=CARTESIAN_POINT('Ctrl Pts',(3.05460822287005,-6.31086326640617,
71.4170306055598));
#143674=CARTESIAN_POINT('Ctrl Pts',(3.22020760822928,-6.23070921729006,
71.4254127186519));
#143675=CARTESIAN_POINT('Ctrl Pts',(3.38277113310771,-6.14397464898929,
71.433794831744));
#143676=CARTESIAN_POINT('Ctrl Pts',(3.54176177336686,-6.05091316275628,
71.4421769448361));
#143677=CARTESIAN_POINT('Ctrl Pts',(3.70062907058682,-5.95792387251245,
71.450552555185));
#143678=CARTESIAN_POINT('Ctrl Pts',(3.85592872663196,-5.85861761554745,
71.4589281655339));
#143679=CARTESIAN_POINT('Ctrl Pts',(4.00714757241335,-5.75329426462803,
71.4673037758828));
#143680=CARTESIAN_POINT('Ctrl Pts',(4.15827129929455,-5.64803716366082,
71.4756741178484));
#143681=CARTESIAN_POINT('Ctrl Pts',(4.30531906500941,-5.53677070276705,
71.484044459814));
#143682=CARTESIAN_POINT('Ctrl Pts',(4.44780561295396,-5.4198387237883,71.4924148017796));
#143683=CARTESIAN_POINT('Ctrl Pts',(4.59022342167176,-5.30296315584578,
71.5007811056739));
#143684=CARTESIAN_POINT('Ctrl Pts',(4.72808414701667,-5.18042772841354,
71.5091474095682));
#143685=CARTESIAN_POINT('Ctrl Pts',(4.86093427647319,-5.05261759114106,
71.5175137134626));
#143686=CARTESIAN_POINT('Ctrl Pts',(4.99374725147239,-4.92484319878136,
71.5258776775362));
#143687=CARTESIAN_POINT('Ctrl Pts',(5.12155218716623,-4.79179726470219,
71.5342416416099));
#143688=CARTESIAN_POINT('Ctrl Pts',(5.24393081960761,-4.65390332104884,
71.5426056056835));
#143689=CARTESIAN_POINT('Ctrl Pts',(5.36629062001084,-4.51603059698226,
71.550968282682));
#143690=CARTESIAN_POINT('Ctrl Pts',(5.48322556392833,-4.37331159651445,
71.5593309596806));
#143691=CARTESIAN_POINT('Ctrl Pts',(5.59435596157596,-4.22620490957071,
71.5676936366791));
#143692=CARTESIAN_POINT('Ctrl Pts',(5.70548407125212,-4.07910125128437,
71.5760561415055));
#143693=CARTESIAN_POINT('Ctrl Pts',(5.8108076751712,-3.92761034912387,71.5844186463318));
#143694=CARTESIAN_POINT('Ctrl Pts',(5.90998865498239,-3.77222224431163,
71.5927811511581));
#143695=CARTESIAN_POINT('Ctrl Pts',(6.00918081295636,-3.61681662652934,
71.6011445984781));
#143696=CARTESIAN_POINT('Ctrl Pts',(6.1022287902082,-3.45751320769643,71.609508045798));
#143697=CARTESIAN_POINT('Ctrl Pts',(6.18883869360879,-3.29482961425787,
71.6178714931179));
#143698=CARTESIAN_POINT('Ctrl Pts',(6.27549959535505,-3.13205022814655,
71.6262398650708));
#143699=CARTESIAN_POINT('Ctrl Pts',(6.35571469263457,-2.96588698021059,
71.6346082370236));
#143700=CARTESIAN_POINT('Ctrl Pts',(6.42923635906474,-2.79688154947254,
71.6429766089764));
#143701=CARTESIAN_POINT('Ctrl Pts',(6.50278005450727,-2.62782548029141,
71.6513474883121));
#143702=CARTESIAN_POINT('Ctrl Pts',(6.56962619384954,-2.45592583379929,
71.6597183676478));
#143703=CARTESIAN_POINT('Ctrl Pts',(6.6295756786435,-2.28174338689489,71.6680892469836));
#143704=CARTESIAN_POINT('Ctrl Pts',(6.68957595798786,-2.1074133570862,71.6764672188748));
#143705=CARTESIAN_POINT('Ctrl Pts',(6.74266780455232,-1.93079697476473,
71.6848451907661));
#143706=CARTESIAN_POINT('Ctrl Pts',(6.7887019480829,-1.75247037709501,71.6932231626574));
#143707=CARTESIAN_POINT('Ctrl Pts',(6.81795702115392,-1.63914237215731,
71.6985474320164));
#143708=CARTESIAN_POINT('Ctrl Pts',(6.84436271219509,-1.52512392652085,
71.7038717013753));
#143709=CARTESIAN_POINT('Ctrl Pts',(6.86789146169496,-1.41056493394581,
71.7091959707343));
#143710=CARTESIAN_POINT('Ctrl Pts',(6.90680224734189,-1.22111243439664,
71.7180010074727));
#143711=CARTESIAN_POINT('Ctrl Pts',(6.93790954719751,-1.02985490893788,
71.726806044211));
#143712=CARTESIAN_POINT('Ctrl Pts',(6.96105872276573,-0.83742941237284,
71.7356110809493));
#143713=CARTESIAN_POINT('Ctrl Pts',(6.9841432039996,-0.645541681801989,
71.744391510505));
#143714=CARTESIAN_POINT('Ctrl Pts',(6.99931389611826,-0.452492746218981,
71.7531719400608));
#143715=CARTESIAN_POINT('Ctrl Pts',(7.00646718374247,-0.258928881432433,
71.7619523696164));
#143716=CARTESIAN_POINT('Ctrl Pts',(7.00961240899781,-0.173820888013127,
71.7658130320478));
#143717=CARTESIAN_POINT('Ctrl Pts',(7.01120830977235,-0.088613512133081,
71.7696736944791));
#143718=CARTESIAN_POINT('Ctrl Pts',(7.01124919374686,-0.00336239259829206,
71.7735343569104));
#143719=CARTESIAN_POINT('Ctrl Pts',(7.01124919374723,-0.0033623918231733,
71.7735343569455));
#143720=CARTESIAN_POINT('Ctrl Pts',(7.01133243824314,0.170218777619445,
71.7813951135351));
#143721=CARTESIAN_POINT('Ctrl Pts',(7.00496446246303,0.343967021436137,
71.7892558701247));
#143722=CARTESIAN_POINT('Ctrl Pts',(6.99213931214681,0.517314606435117,
71.7971166267143));
#143723=CARTESIAN_POINT('Ctrl Pts',(6.97984637489561,0.683468681241118,
71.8046511807055));
#143724=CARTESIAN_POINT('Ctrl Pts',(6.96162145167992,0.849254241414303,
71.8121857346967));
#143725=CARTESIAN_POINT('Ctrl Pts',(6.93751249916818,1.01417300614109,71.8197202886879));
#143726=CARTESIAN_POINT('Ctrl Pts',(6.91340523989911,1.17908018813785,71.8272543135052));
#143727=CARTESIAN_POINT('Ctrl Pts',(6.88341483877573,1.34312029690996,71.8347883383225));
#143728=CARTESIAN_POINT('Ctrl Pts',(6.84764077591688,1.50580289762654,71.8423223631399));
#143729=CARTESIAN_POINT('Ctrl Pts',(6.81185484725353,1.66853945810565,71.849858886898));
#143730=CARTESIAN_POINT('Ctrl Pts',(6.77028152667085,1.82991722015094,71.8573954106561));
#143731=CARTESIAN_POINT('Ctrl Pts',(6.72307070525294,1.98945893515542,71.8649319344142));
#143732=CARTESIAN_POINT('Ctrl Pts',(6.71694946583844,2.01014472296447,71.8659091016164));
#143733=CARTESIAN_POINT('Ctrl Pts',(6.71073352178202,2.03079966839776,71.8668862688185));
#143734=CARTESIAN_POINT('Ctrl Pts',(6.70442326004344,2.05142275328333,71.8678634360207));
#143735=CARTESIAN_POINT('Ctrl Pts',(6.66385193369962,2.18401723854725,71.8741460548872));
#143736=CARTESIAN_POINT('Ctrl Pts',(6.61938366189032,2.31528604824613,71.8804286737536));
#143737=CARTESIAN_POINT('Ctrl Pts',(6.57110895151816,2.44502632087631,71.8867112926201));
#143738=CARTESIAN_POINT('',(7.01124849188977,-0.00459863821984105,71.2264656430896));
#143739=CARTESIAN_POINT('Ctrl Pts',(6.57110895151817,2.44502632087629,71.3398522865014));
#143740=CARTESIAN_POINT('Ctrl Pts',(6.63771924680903,2.2660084085079,71.3311805125692));
#143741=CARTESIAN_POINT('Ctrl Pts',(6.69700989700479,2.08426710051935,71.3225087386371));
#143742=CARTESIAN_POINT('Ctrl Pts',(6.7487830778943,1.90040877971757,71.313836964705));
#143743=CARTESIAN_POINT('Ctrl Pts',(6.80055978789537,1.71653792623928,71.3051645996627));
#143744=CARTESIAN_POINT('Ctrl Pts',(6.84481792613578,1.53055004459431,71.2964922346203));
#143745=CARTESIAN_POINT('Ctrl Pts',(6.88140980451101,1.34306577086891,71.2878198695779));
#143746=CARTESIAN_POINT('Ctrl Pts',(6.91799949925382,1.15559268532947,71.2791480220618));
#143747=CARTESIAN_POINT('Ctrl Pts',(6.94692379517685,0.966623665171059,
71.2704761745457));
#143748=CARTESIAN_POINT('Ctrl Pts',(6.96808618426383,0.776789219268369,
71.2618043270296));
#143749=CARTESIAN_POINT('Ctrl Pts',(6.98924897510675,0.586951169466536,
71.2531323148834));
#143750=CARTESIAN_POINT('Ctrl Pts',(7.00264953276857,0.396247943319635,
71.2444603027372));
#143751=CARTESIAN_POINT('Ctrl Pts',(7.00824314361838,0.205315860142174,
71.235788290591));
#143752=CARTESIAN_POINT('Ctrl Pts',(7.01024757124657,0.136896809746581,
71.2326807414238));
#143753=CARTESIAN_POINT('Ctrl Pts',(7.01125,0.068448405292975,71.2295731922567));
#143754=CARTESIAN_POINT('Ctrl Pts',(7.01125,8.58630487052188E-16,71.2264656430895));
#143755=CARTESIAN_POINT('Ctrl Pts',(7.01124849188977,-0.00459863821984105,
71.2264656430896));
#143756=CARTESIAN_POINT('Ctrl Pts',(7.01110776524495,-0.219155519857082,
71.2167319929736));
#143757=CARTESIAN_POINT('Ctrl Pts',(7.00111426117045,-0.433432367386418,
71.2069983428576));
#143758=CARTESIAN_POINT('Ctrl Pts',(6.98136890923631,-0.646617905450055,
71.1972646927415));
#143759=CARTESIAN_POINT('Ctrl Pts',(6.96148781764589,-0.861268990025962,
71.1874641285322));
#143760=CARTESIAN_POINT('Ctrl Pts',(6.93172037097155,-1.07481368090438,
71.1776635643229));
#143761=CARTESIAN_POINT('Ctrl Pts',(6.89222048842957,-1.28643822291304,
71.1678630001136));
#143762=CARTESIAN_POINT('Ctrl Pts',(6.85264754105462,-1.49845421701776,
71.1580443073292));
#143763=CARTESIAN_POINT('Ctrl Pts',(6.80330615487526,-1.70854293642341,
71.1482256145448));
#143764=CARTESIAN_POINT('Ctrl Pts',(6.74440143903495,-1.9159007781311,71.1384069217604));
#143765=CARTESIAN_POINT('Ctrl Pts',(6.68553901871984,-2.1231097300819,71.1285952791206));
#143766=CARTESIAN_POINT('Ctrl Pts',(6.61712701506897,-2.32759170868229,
71.1187836364809));
#143767=CARTESIAN_POINT('Ctrl Pts',(6.5394198817576,-2.52855970318547,71.1089719938411));
#143768=CARTESIAN_POINT('Ctrl Pts',(6.47091931044857,-2.70571747302802,
71.1003228120008));
#143769=CARTESIAN_POINT('Ctrl Pts',(6.39519636928296,-2.88014479004352,
71.0916736301604));
#143770=CARTESIAN_POINT('Ctrl Pts',(6.31245749192088,-3.05131233655159,
71.0830244483201));
#143771=CARTESIAN_POINT('Ctrl Pts',(6.2356126311098,-3.21028652989516,71.0749914027212));
#143772=CARTESIAN_POINT('Ctrl Pts',(6.15267817287989,-3.366521933789,71.0669583571223));
#143773=CARTESIAN_POINT('Ctrl Pts',(6.06387990035083,-3.51951518204158,
71.0589253115234));
#143774=CARTESIAN_POINT('Ctrl Pts',(5.97513871077037,-3.67241008034347,
71.0508974298755));
#143775=CARTESIAN_POINT('Ctrl Pts',(5.88054139338673,-3.82206665590438,
71.0428695482276));
#143776=CARTESIAN_POINT('Ctrl Pts',(5.78036050395399,-3.96800441114029,
71.0348416665797));
#143777=CARTESIAN_POINT('Ctrl Pts',(5.68022484718038,-4.1138762740411,71.0268174095995));
#143778=CARTESIAN_POINT('Ctrl Pts',(5.57451084506208,-4.25603235827843,
71.0187931526193));
#143779=CARTESIAN_POINT('Ctrl Pts',(5.46353534834988,-4.39401957890851,
71.0107688956392));
#143780=CARTESIAN_POINT('Ctrl Pts',(5.35257326970559,-4.53199011547815,
71.0027456088734));
#143781=CARTESIAN_POINT('Ctrl Pts',(5.23635118719689,-4.66579250212281,
70.9947223221076));
#143782=CARTESIAN_POINT('Ctrl Pts',(5.11522747004122,-4.79500516081429,
70.9866990353418));
#143783=CARTESIAN_POINT('Ctrl Pts',(4.9941136778938,-4.92420723168092,70.9786764060128));
#143784=CARTESIAN_POINT('Ctrl Pts',(4.86809930481864,-5.04882005897734,
70.9706537766838));
#143785=CARTESIAN_POINT('Ctrl Pts',(4.73758074165986,-5.16845772728709,
70.9626311473548));
#143786=CARTESIAN_POINT('Ctrl Pts',(4.60701311281319,-5.2881403708429,70.9546055020883));
#143787=CARTESIAN_POINT('Ctrl Pts',(4.4719381837576,-5.40284387351634,70.9465798568218));
#143788=CARTESIAN_POINT('Ctrl Pts',(4.33278697616236,-5.51222129288165,
70.9385542115554));
#143789=CARTESIAN_POINT('Ctrl Pts',(4.25073494471767,-5.57671688446291,
70.9338218020481));
#143790=CARTESIAN_POINT('Ctrl Pts',(4.16726621785939,-5.63936136102783,
70.9290893925408));
#143791=CARTESIAN_POINT('Ctrl Pts',(4.08247411608701,-5.70009049524476,
70.9243569830336));
#143792=CARTESIAN_POINT('Ctrl Pts',(3.92605502595589,-5.81211974938641,
70.9156269341991));
#143793=CARTESIAN_POINT('Ctrl Pts',(3.76505279120063,-5.91768488094815,
70.9068968853646));
#143794=CARTESIAN_POINT('Ctrl Pts',(3.60001325395888,-6.01643840937647,
70.8981668365301));
#143795=CARTESIAN_POINT('Ctrl Pts',(3.43492599532925,-6.1152204925106,70.8894342633911));
#143796=CARTESIAN_POINT('Ctrl Pts',(3.26579933911061,-6.20718690045705,
70.8807016902521));
#143797=CARTESIAN_POINT('Ctrl Pts',(3.09320522068632,-6.29203528480403,
70.8719691171131));
#143798=CARTESIAN_POINT('Ctrl Pts',(2.91815912729324,-6.37808907589638,
70.8631124838326));
#143799=CARTESIAN_POINT('Ctrl Pts',(2.73954655925391,-6.45682092833281,
70.8542558505521));
#143800=CARTESIAN_POINT('Ctrl Pts',(2.55798720585462,-6.52796507475217,
70.8453992172716));
#143801=CARTESIAN_POINT('Ctrl Pts',(2.37885710472599,-6.59815731714677,
70.836661085165));
#143802=CARTESIAN_POINT('Ctrl Pts',(2.19685885117257,-6.66096355879762,
70.8279229530584));
#143803=CARTESIAN_POINT('Ctrl Pts',(2.01260584970456,-6.71617780111836,
70.8191848209518));
#143804=CARTESIAN_POINT('Ctrl Pts',(1.82460475939467,-6.77251521583741,
70.8102689370844));
#143805=CARTESIAN_POINT('Ctrl Pts',(1.63425648872507,-6.82094836000331,
70.801353053217));
#143806=CARTESIAN_POINT('Ctrl Pts',(1.4422278526844,-6.86131222022736,70.7924371693495));
#143807=CARTESIAN_POINT('Ctrl Pts',(1.25019921664367,-6.90167608045143,
70.7835212854821));
#143808=CARTESIAN_POINT('Ctrl Pts',(1.05649051242816,-6.93397060047979,
70.7746054016147));
#143809=CARTESIAN_POINT('Ctrl Pts',(0.861779521941969,-6.95808613183694,
70.7656895177473));
#143810=CARTESIAN_POINT('Ctrl Pts',(0.670894651622895,-6.98172778690884,
70.7569488332509));
#143811=CARTESIAN_POINT('Ctrl Pts',(0.479026245871978,-6.99751141897496,
70.7482081487545));
#143812=CARTESIAN_POINT('Ctrl Pts',(0.286818775441527,-7.00538089989076,
70.7394674642582));
#143813=CARTESIAN_POINT('Ctrl Pts',(0.0946458863275725,-7.01324896495623,
70.7307283523562));
#143814=CARTESIAN_POINT('Ctrl Pts',(-0.0978656721700958,-7.01320571128641,
70.7219892404541));
#143815=CARTESIAN_POINT('Ctrl Pts',(-0.290069043990111,-7.00524707003391,
70.7132501285521));
#143816=CARTESIAN_POINT('Ctrl Pts',(-0.484762687116275,-6.9971853131297,
70.7043977888778));
#143817=CARTESIAN_POINT('Ctrl Pts',(-0.679139816189818,-6.98100161767388,
70.6955454492035));
#143818=CARTESIAN_POINT('Ctrl Pts',(-0.872529556747008,-6.95674627502706,
70.6866931095292));
#143819=CARTESIAN_POINT('Ctrl Pts',(-1.06334784933147,-6.9328134487221,
70.6779584768794));
#143820=CARTESIAN_POINT('Ctrl Pts',(-1.25320457133843,-6.90102234370466,
70.6692238442294));
#143821=CARTESIAN_POINT('Ctrl Pts',(-1.44146079355278,-6.86147340905364,
70.6604892115796));
#143822=CARTESIAN_POINT('Ctrl Pts',(-1.63352239842513,-6.82112503824964,
70.6515780183931));
#143823=CARTESIAN_POINT('Ctrl Pts',(-1.82391782122646,-6.77270190480472,
70.6426668252066));
#143824=CARTESIAN_POINT('Ctrl Pts',(-2.0119789093691,-6.71636564153218,
70.6337556320201));
#143825=CARTESIAN_POINT('Ctrl Pts',(-2.20003999751181,-6.66002937825962,
70.6248444388336));
#143826=CARTESIAN_POINT('Ctrl Pts',(-2.38576645674874,-6.59578005923957,
70.6159332456472));
#143827=CARTESIAN_POINT('Ctrl Pts',(-2.56850496940922,-6.52383390228631,
70.6070220524607));
#143828=CARTESIAN_POINT('Ctrl Pts',(-2.73308428303562,-6.45903722118699,
70.5989963876084));
#143829=CARTESIAN_POINT('Ctrl Pts',(-2.89531542892063,-6.38796714380799,
70.5909707227561));
#143830=CARTESIAN_POINT('Ctrl Pts',(-3.05468423894261,-6.31082647225034,
70.5829450579037));
#143831=CARTESIAN_POINT('Ctrl Pts',(-3.21400246921343,-6.23371028324966,
70.5749219402006));
#143832=CARTESIAN_POINT('Ctrl Pts',(-3.37045984267261,-6.15052749538354,
70.5668988224974));
#143833=CARTESIAN_POINT('Ctrl Pts',(-3.52356324438916,-6.06152857167973,
70.5588757047943));
#143834=CARTESIAN_POINT('Ctrl Pts',(-3.67664733842679,-5.97254087151913,
70.5508535988765));
#143835=CARTESIAN_POINT('Ctrl Pts',(-3.8263779866911,-5.87773868118234,
70.5428314929587));
#143836=CARTESIAN_POINT('Ctrl Pts',(-3.97228775771086,-5.77741780836737,
70.5348093870409));
#143837=CARTESIAN_POINT('Ctrl Pts',(-4.11825174929443,-5.67705965597716,
70.5267843000814));
#143838=CARTESIAN_POINT('Ctrl Pts',(-4.26039172317582,-5.57117892974228,
70.518759213122));
#143839=CARTESIAN_POINT('Ctrl Pts',(-4.39826990370491,-5.46011432267344,
70.5107341261625));
#143840=CARTESIAN_POINT('Ctrl Pts',(-4.53617523865164,-5.34902784198606,
70.5027074587024));
#143841=CARTESIAN_POINT('Ctrl Pts',(-4.66981682820477,-5.23275568339619,
70.4946807912422));
#143842=CARTESIAN_POINT('Ctrl Pts',(-4.79879112613414,-5.11167587883233,
70.486654123782));
#143843=CARTESIAN_POINT('Ctrl Pts',(-4.92786896417546,-4.99049887182797,
70.4786210125415));
#143844=CARTESIAN_POINT('Ctrl Pts',(-5.05227176628368,-4.86450676796228,
70.470587901301));
#143845=CARTESIAN_POINT('Ctrl Pts',(-5.17163347091825,-4.73411383523655,
70.4625547900605));
#143846=CARTESIAN_POINT('Ctrl Pts',(-5.24196572334579,-4.65728158248588,
70.4578213890985));
#143847=CARTESIAN_POINT('Ctrl Pts',(-5.31054845581264,-4.57892201253535,
70.4530879881364));
#143848=CARTESIAN_POINT('Ctrl Pts',(-5.37731352235196,-4.49912500880236,
70.4483545871744));
#143849=CARTESIAN_POINT('Ctrl Pts',(-5.51485163727971,-4.33474069767678,
70.4386036338801));
#143850=CARTESIAN_POINT('Ctrl Pts',(-5.64475541595421,-4.16415819944512,
70.4288526805858));
#143851=CARTESIAN_POINT('Ctrl Pts',(-5.76655261146557,-3.98804432544318,
70.4191017272915));
#143852=CARTESIAN_POINT('Ctrl Pts',(-5.88852527868578,-3.81167672636744,
70.4093367259198));
#143853=CARTESIAN_POINT('Ctrl Pts',(-6.00236797922327,-3.62976184298234,
70.3995717245481));
#143854=CARTESIAN_POINT('Ctrl Pts',(-6.10765108553284,-3.44299648270072,
70.3898067231763));
#143855=CARTESIAN_POINT('Ctrl Pts',(-6.21275870671831,-3.25654242157788,
70.3800579980386));
#143856=CARTESIAN_POINT('Ctrl Pts',(-6.30933522913878,-3.06525407469387,
70.3703092729009));
#143857=CARTESIAN_POINT('Ctrl Pts',(-6.39699779057307,-2.8698511860205,
70.3605605477632));
#143858=CARTESIAN_POINT('Ctrl Pts',(-6.48441975226722,-2.67498460250943,
70.3508385790959));
#143859=CARTESIAN_POINT('Ctrl Pts',(-6.56297657773471,-2.47602605791691,
70.3411166104286));
#143860=CARTESIAN_POINT('Ctrl Pts',(-6.63233334959338,-2.27371522015654,
70.3313946417614));
#143861=CARTESIAN_POINT('Ctrl Pts',(-6.70123120580752,-2.07274302036933,
70.3217370008216));
#143862=CARTESIAN_POINT('Ctrl Pts',(-6.76105031225179,-1.86846277806501,
70.3120793598817));
#143863=CARTESIAN_POINT('Ctrl Pts',(-6.8115071862928,-1.66162463076999,
70.3024217189419));
#143864=CARTESIAN_POINT('Ctrl Pts',(-6.83368471955457,-1.570712144045,70.2981768532572));
#143865=CARTESIAN_POINT('Ctrl Pts',(-6.85405414701907,-1.47930581811492,
70.2939319875726));
#143866=CARTESIAN_POINT('Ctrl Pts',(-6.87259420767557,-1.38747087145073,
70.2896871218879));
#143867=CARTESIAN_POINT('Ctrl Pts',(-6.90688827743327,-1.21760119704961,
70.281835274874));
#143868=CARTESIAN_POINT('Ctrl Pts',(-6.9349053693729,-1.04633401805478,
70.2739834278602));
#143869=CARTESIAN_POINT('Ctrl Pts',(-6.95653755564075,-0.874192083846496,
70.2661315808463));
#143870=CARTESIAN_POINT('Ctrl Pts',(-6.97816360719546,-0.702098967699072,
70.2582819605528));
#143871=CARTESIAN_POINT('Ctrl Pts',(-6.99340830736989,-0.529131967912636,
70.2504323402592));
#143872=CARTESIAN_POINT('Ctrl Pts',(-7.00221515756051,-0.35582221646467,
70.2425827199657));
#143873=CARTESIAN_POINT('Ctrl Pts',(-7.01102130463679,-0.182526301583597,
70.2347337263639));
#143874=CARTESIAN_POINT('Ctrl Pts',(-7.01339060631139,-0.0088880705264088,
70.2268847327622));
#143875=CARTESIAN_POINT('Ctrl Pts',(-7.00931859181253,0.164558320881367,
70.2190357391604));
#143876=CARTESIAN_POINT('Ctrl Pts',(-7.00524451577196,0.33809252311822,
70.2111827718431));
#143877=CARTESIAN_POINT('Ctrl Pts',(-6.99472261678196,0.511434309793231,
70.2033298045257));
#143878=CARTESIAN_POINT('Ctrl Pts',(-6.97780054194339,0.684051284155319,
70.1954768372083));
#143879=CARTESIAN_POINT('Ctrl Pts',(-6.9608741694664,0.856712097428874,
70.1876218755011));
#143880=CARTESIAN_POINT('Ctrl Pts',(-6.93754443420151,1.02864735361808,
70.1797669137939));
#143881=CARTESIAN_POINT('Ctrl Pts',(-6.90791054361484,1.19933251599168,
70.1719119520867));
#143882=CARTESIAN_POINT('Ctrl Pts',(-6.87824723891469,1.3701870976564,70.1640491936734));
#143883=CARTESIAN_POINT('Ctrl Pts',(-6.84226736039791,1.53978873426941,
70.1561864352601));
#143884=CARTESIAN_POINT('Ctrl Pts',(-6.80012078706763,1.70762520588995,
70.1483236768468));
#143885=CARTESIAN_POINT('Ctrl Pts',(-6.76920266563841,1.8307476331666,70.1425556700984));
#143886=CARTESIAN_POINT('Ctrl Pts',(-6.73496700950947,1.95292040784015,
70.13678766335));
#143887=CARTESIAN_POINT('Ctrl Pts',(-6.69748962124314,2.07394776593829,
70.1310196566016));
#143888=CARTESIAN_POINT('Ctrl Pts',(-6.64305347672589,2.24974077235465,
70.1226415901605));
#143889=CARTESIAN_POINT('Ctrl Pts',(-6.58165583125923,2.42350599110936,
70.1142635237195));
#143890=CARTESIAN_POINT('Ctrl Pts',(-6.5134697150402,2.59467509213661,70.1058854572784));
#143891=CARTESIAN_POINT('Ctrl Pts',(-6.44533022367726,2.76572714976642,
70.0975131196597));
#143892=CARTESIAN_POINT('Ctrl Pts',(-6.3704116373528,2.93418632446898,70.0891407820409));
#143893=CARTESIAN_POINT('Ctrl Pts',(-6.28893622386487,3.09950120739777,
70.0807684444221));
#143894=CARTESIAN_POINT('Ctrl Pts',(-6.20750457387338,3.26472729351068,
70.0724006038995));
#143895=CARTESIAN_POINT('Ctrl Pts',(-6.11952326408433,3.42681216119099,
70.0640327633769));
#143896=CARTESIAN_POINT('Ctrl Pts',(-6.02526210732681,3.5852256693982,70.0556649228543));
#143897=CARTESIAN_POINT('Ctrl Pts',(-5.93103777319206,3.74357729420554,
70.0473003511843));
#143898=CARTESIAN_POINT('Ctrl Pts',(-5.83053865193824,3.89826013746391,
70.0389357795144));
#143899=CARTESIAN_POINT('Ctrl Pts',(-5.72408002124428,4.04876950108204,
70.0305712078444));
#143900=CARTESIAN_POINT('Ctrl Pts',(-5.61764739507809,4.19924209995032,
70.0222086793788));
#143901=CARTESIAN_POINT('Ctrl Pts',(-5.50525835252381,4.34554298435232,
70.0138461509132));
#143902=CARTESIAN_POINT('Ctrl Pts',(-5.3872711856394,4.48719686829979,70.0054836224476));
#143903=CARTESIAN_POINT('Ctrl Pts',(-5.26927460300992,4.62886205667041,
69.9971204266261));
#143904=CARTESIAN_POINT('Ctrl Pts',(-5.14567920921771,4.76587924728211,
69.9887572308046));
#143905=CARTESIAN_POINT('Ctrl Pts',(-5.01688372631032,4.89780606385988,
69.980394034983));
#143906=CARTESIAN_POINT('Ctrl Pts',(-4.88807945980912,5.02974187758216,
69.9720302688083));
#143907=CARTESIAN_POINT('Ctrl Pts',(-4.75407462659041,5.15658638960114,
69.9636665026336));
#143908=CARTESIAN_POINT('Ctrl Pts',(-4.61530508773046,5.27793382960315,
69.9553027364589));
#143909=CARTESIAN_POINT('Ctrl Pts',(-4.4765075838224,5.39930572372546,69.9469372848053));
#143910=CARTESIAN_POINT('Ctrl Pts',(-4.33294370714164,5.51517812047347,
69.9385718331517));
#143911=CARTESIAN_POINT('Ctrl Pts',(-4.18508301290906,5.62518504029513,
69.9302063814981));
#143912=CARTESIAN_POINT('Ctrl Pts',(-4.03717280042067,5.73522880121796,
69.9218381282712));
#143913=CARTESIAN_POINT('Ctrl Pts',(-3.88496316466333,5.8394029720958,69.9134698750443));
#143914=CARTESIAN_POINT('Ctrl Pts',(-3.7289536328293,5.9373842192256,69.9051016218174));
#143915=CARTESIAN_POINT('Ctrl Pts',(-3.5727994579021,6.03545630895002,69.8967256100259));
#143916=CARTESIAN_POINT('Ctrl Pts',(-3.41283862551568,6.12732382620423,
69.8883495982344));
#143917=CARTESIAN_POINT('Ctrl Pts',(-3.24959739565233,6.21270821209798,
69.8799735864429));
#143918=CARTESIAN_POINT('Ctrl Pts',(-3.08627611027292,6.29813447154954,
69.8715934669517));
#143919=CARTESIAN_POINT('Ctrl Pts',(-2.91967151344542,6.37707111279513,
69.8632133474606));
#143920=CARTESIAN_POINT('Ctrl Pts',(-2.75033154337589,6.44928701206665,
69.8548332279694));
#143921=CARTESIAN_POINT('Ctrl Pts',(-2.58079808093965,6.52158542715094,
69.8464435331302));
#143922=CARTESIAN_POINT('Ctrl Pts',(-2.4085233048815,6.58714763243901,69.8380538382909));
#143923=CARTESIAN_POINT('Ctrl Pts',(-2.23407333606647,6.64579136684088,
69.8296641434517));
#143924=CARTESIAN_POINT('Ctrl Pts',(-2.12331806130904,6.68302326181112,
69.8243376709773));
#143925=CARTESIAN_POINT('Ctrl Pts',(-2.0116863307701,6.71746748972255,69.8190111985029));
#143926=CARTESIAN_POINT('Ctrl Pts',(-1.89932553437109,6.74908801816853,
69.8136847260286));
#143927=CARTESIAN_POINT('Ctrl Pts',(-1.72252379684623,6.79884348938155,
69.8053034256237));
#143928=CARTESIAN_POINT('Ctrl Pts',(-1.54355969267545,6.84170545877321,
69.7969221252188));
#143929=CARTESIAN_POINT('Ctrl Pts',(-1.36299661902977,6.87748986033519,
69.788540824814));
#143930=CARTESIAN_POINT('Ctrl Pts',(-1.18266238264729,6.91322891040668,
69.7801701464804));
#143931=CARTESIAN_POINT('Ctrl Pts',(-1.00073353410874,6.94190820531124,
69.7717994681469));
#143932=CARTESIAN_POINT('Ctrl Pts',(-0.817788303417419,6.96339348689227,
69.7634287898134));
#143933=CARTESIAN_POINT('Ctrl Pts',(-0.635050684152917,6.98485438636753,
69.7550676107626));
#143934=CARTESIAN_POINT('Ctrl Pts',(-0.451299305063117,6.99913750622476,
69.7467064317118));
#143935=CARTESIAN_POINT('Ctrl Pts',(-0.267122700122726,7.00615957751314,
69.738345252661));
#143936=CARTESIAN_POINT('Ctrl Pts',(-0.083185086052544,7.01317253683572,
69.7299949232263));
#143937=CARTESIAN_POINT('Ctrl Pts',(0.101176327415832,7.01294322847672,
69.7216445937916));
#143938=CARTESIAN_POINT('Ctrl Pts',(0.285367848509045,7.00544015416143,
69.7132942643569));
#143939=CARTESIAN_POINT('Ctrl Pts',(0.469417645245128,6.99794285301299,
69.7049503600011));
#143940=CARTESIAN_POINT('Ctrl Pts',(0.653297484122077,6.98318295244684,
69.6966064556454));
#143941=CARTESIAN_POINT('Ctrl Pts',(0.836412478332128,6.96118098662794,
69.6882625512897));
#143942=CARTESIAN_POINT('Ctrl Pts',(1.01938039343656,6.93919669292523,69.67992534881));
#143943=CARTESIAN_POINT('Ctrl Pts',(1.20158436469483,6.90998197386602,69.6715881463303));
#143944=CARTESIAN_POINT('Ctrl Pts',(1.38243328120704,6.87360929828799,69.6632509438506));
#143945=CARTESIAN_POINT('Ctrl Pts',(1.44196774626208,6.8616356142598,69.6605063828145));
#143946=CARTESIAN_POINT('Ctrl Pts',(1.50135540542364,6.84888664744526,69.6577618217784));
#143947=CARTESIAN_POINT('Ctrl Pts',(1.56057531963105,6.83536621069116,69.6550172607423));
#143948=CARTESIAN_POINT('Ctrl Pts',(1.74049262305989,6.79428947907926,69.6466789504403));
#143949=CARTESIAN_POINT('Ctrl Pts',(1.91871320861347,6.74612185920721,69.6383406401384));
#143950=CARTESIAN_POINT('Ctrl Pts',(2.09466711578936,6.69103850209597,69.6300023298365));
#143951=CARTESIAN_POINT('Ctrl Pts',(2.27073172719304,6.63592048840557,69.6216587733527));
#143952=CARTESIAN_POINT('Ctrl Pts',(2.44452650296482,6.57387815645998,69.6133152168689));
#143953=CARTESIAN_POINT('Ctrl Pts',(2.61549942395125,6.50513561163875,69.604971660385));
#143954=CARTESIAN_POINT('Ctrl Pts',(2.78660242039094,6.43634076778897,69.5966217561598));
#143955=CARTESIAN_POINT('Ctrl Pts',(2.95487897611539,6.36083566531887,69.5882718519346));
#143956=CARTESIAN_POINT('Ctrl Pts',(3.1197993199902,6.27889152362809,69.5799219477093));
#143957=CARTESIAN_POINT('Ctrl Pts',(3.28496703217679,6.19682447178861,69.5715595192457));
#143958=CARTESIAN_POINT('Ctrl Pts',(3.44676817917903,6.10829922676386,69.563197090782));
#143959=CARTESIAN_POINT('Ctrl Pts',(3.6046984487669,6.0136324842775,69.5548346623183));
#143960=CARTESIAN_POINT('Ctrl Pts',(3.76276377026411,5.91888478882146,69.5464650828383));
#143961=CARTESIAN_POINT('Ctrl Pts',(3.91695133627263,5.8179852961546,69.5380955033583));
#143962=CARTESIAN_POINT('Ctrl Pts',(4.06678741139398,5.7112929108064,69.5297259238783));
#143963=CARTESIAN_POINT('Ctrl Pts',(4.2168545904053,5.60443596545312,69.5213434353418));
#143964=CARTESIAN_POINT('Ctrl Pts',(4.36255660796857,5.49176847300213,69.5129609468052));
#143965=CARTESIAN_POINT('Ctrl Pts',(4.50345319324468,5.37368922610476,69.5045784582686));
#143966=CARTESIAN_POINT('Ctrl Pts',(4.54955686467315,5.33505176167785,69.5018355706643));
#143967=CARTESIAN_POINT('Ctrl Pts',(4.59514631446448,5.29583514689353,69.49909268306));
#143968=CARTESIAN_POINT('Ctrl Pts',(4.64020700827323,5.25605417427104,69.4963497954557));
#143969=CARTESIAN_POINT('Ctrl Pts',(4.77570749191783,5.13643016108832,69.4881017511947));
#143970=CARTESIAN_POINT('Ctrl Pts',(4.9067250793169,5.01143441045634,69.4798537069337));
#143971=CARTESIAN_POINT('Ctrl Pts',(5.03281608802424,4.88143306689997,69.4716056626726));
#143972=CARTESIAN_POINT('Ctrl Pts',(5.15879061092155,4.75155182161201,69.463365238147));
#143973=CARTESIAN_POINT('Ctrl Pts',(5.2798473828122,4.61667444192376,69.4551248136213));
#143974=CARTESIAN_POINT('Ctrl Pts',(5.39557698681743,4.47720622060523,69.4468843890957));
#143975=CARTESIAN_POINT('Ctrl Pts',(5.51121869203085,4.33784392800091,69.4386502233261));
#143976=CARTESIAN_POINT('Ctrl Pts',(5.62154107133063,4.19389800584841,69.4304160575564));
#143977=CARTESIAN_POINT('Ctrl Pts',(5.72617252610861,4.04580953132238,69.4221818917868));
#143978=CARTESIAN_POINT('Ctrl Pts',(5.83073393570096,3.89782019414189,69.4139532383526));
#143979=CARTESIAN_POINT('Ctrl Pts',(5.9296118174176,3.74569411481522,69.4057245849184));
#143980=CARTESIAN_POINT('Ctrl Pts',(6.0224756756318,3.58990435790751,69.3974959314841));
#143981=CARTESIAN_POINT('Ctrl Pts',(6.11530333231547,3.43417533321306,69.3892704858625));
#143982=CARTESIAN_POINT('Ctrl Pts',(6.20212146096078,3.27478577326012,69.3810450402407));
#143983=CARTESIAN_POINT('Ctrl Pts',(6.28264339172886,3.11223690853792,69.3728195946191));
#143984=CARTESIAN_POINT('Ctrl Pts',(6.36314952543434,2.94971993319751,69.3645957626929));
#143985=CARTESIAN_POINT('Ctrl Pts',(6.43736176921313,2.78404519728397,69.3563719307667));
#143986=CARTESIAN_POINT('Ctrl Pts',(6.50503971704048,2.6157379154315,69.3481480988406));
#143987=CARTESIAN_POINT('Ctrl Pts',(6.52780435145871,2.55912488468372,69.3453818724208));
#143988=CARTESIAN_POINT('Ctrl Pts',(6.54983007321618,2.5022141828206,69.342615646001));
#143989=CARTESIAN_POINT('Ctrl Pts',(6.57110895151815,2.44502632087633,69.3398494195812));
#143990=CARTESIAN_POINT('Origin',(0.,0.,50.));
#143991=CARTESIAN_POINT('',(6.57110895151817,2.44502632087627,67.3401074818243));
#143992=CARTESIAN_POINT('',(6.57110895151815,2.44502632087632,67.8869083240903));
#143993=CARTESIAN_POINT('',(6.57110895151814,2.44502632087636,50.));
#143994=CARTESIAN_POINT('',(7.01124997488654,-0.000593425248588222,69.773534356871));
#143995=CARTESIAN_POINT('Ctrl Pts',(6.57110895151815,2.44502632087632,67.8869083240903));
#143996=CARTESIAN_POINT('Ctrl Pts',(6.53460574947235,2.543130179994,67.8916644840135));
#143997=CARTESIAN_POINT('Ctrl Pts',(6.49590744269728,2.64041041299079,67.8964206439368));
#143998=CARTESIAN_POINT('Ctrl Pts',(6.45505378653798,2.73676947794323,67.90117680386));
#143999=CARTESIAN_POINT('Ctrl Pts',(6.37997453672858,2.91385439491506,67.9099174883563));
#144000=CARTESIAN_POINT('Ctrl Pts',(6.29760020324618,3.0878574907195,67.9186581728526));
#144001=CARTESIAN_POINT('Ctrl Pts',(6.20820478069396,3.25819274498436,67.9273988573489));
#144002=CARTESIAN_POINT('Ctrl Pts',(6.11882544186321,3.42849735310753,67.9361379692509));
#144003=CARTESIAN_POINT('Ctrl Pts',(6.02242766387985,3.59513519522477,67.9448770811528));
#144004=CARTESIAN_POINT('Ctrl Pts',(5.91933170363533,3.75754424389623,67.9536161930548));
#144005=CARTESIAN_POINT('Ctrl Pts',(5.81489998684652,3.92205753553803,67.9624685327291));
#144006=CARTESIAN_POINT('Ctrl Pts',(5.70359544243341,4.08223143696591,67.9713208724034));
#144007=CARTESIAN_POINT('Ctrl Pts',(5.58579740979659,4.23751033735727,67.9801732120777));
#144008=CARTESIAN_POINT('Ctrl Pts',(5.46956570385057,4.39072453869758,67.9889078447276));
#144009=CARTESIAN_POINT('Ctrl Pts',(5.34701230226013,4.53917289001124,67.9976424773774));
#144010=CARTESIAN_POINT('Ctrl Pts',(5.21854397657135,4.68235254194842,68.0063771100272));
#144011=CARTESIAN_POINT('Ctrl Pts',(5.08747881167492,4.82842640560585,68.0152883032138));
#144012=CARTESIAN_POINT('Ctrl Pts',(4.95025722690546,4.96901606934448,68.0241994964003));
#144013=CARTESIAN_POINT('Ctrl Pts',(4.80735358883626,5.10362400989759,68.0331106895868));
#144014=CARTESIAN_POINT('Ctrl Pts',(4.66444995076705,5.23823195045071,68.0420218827733));
#144015=CARTESIAN_POINT('Ctrl Pts',(4.51586447081349,5.3668579501655,68.0509330759599));
#144016=CARTESIAN_POINT('Ctrl Pts',(4.3621113449029,5.48904465068098,68.0598442691464));
#144017=CARTESIAN_POINT('Ctrl Pts',(4.22363706511551,5.59908934247682,68.0678699339987));
#144018=CARTESIAN_POINT('Ctrl Pts',(4.08090719246255,5.7039610929444,68.075895598851));
#144019=CARTESIAN_POINT('Ctrl Pts',(3.93435465838549,5.80331629196104,68.0839212637033));
#144020=CARTESIAN_POINT('Ctrl Pts',(3.78784863648837,5.90263995807431,68.0919443814064));
#144021=CARTESIAN_POINT('Ctrl Pts',(3.63752267162726,5.99645035299509,68.0999674991095));
#144022=CARTESIAN_POINT('Ctrl Pts',(3.48384041783224,6.0844459489405,68.1079906168126));
#144023=CARTESIAN_POINT('Ctrl Pts',(3.33017754471416,6.17243044787129,68.1160127227304));
#144024=CARTESIAN_POINT('Ctrl Pts',(3.17315954406012,6.25460142688896,68.1240348286482));
#144025=CARTESIAN_POINT('Ctrl Pts',(3.01327646962929,6.330702289642,68.132056934566));
#144026=CARTESIAN_POINT('Ctrl Pts',(2.85333398210773,6.4068314317328,68.1400820215254));
#144027=CARTESIAN_POINT('Ctrl Pts',(2.69052462394261,6.47688579103166,68.1481071084848));
#144028=CARTESIAN_POINT('Ctrl Pts',(2.5253607311898,6.54065591052339,68.1561321954443));
#144029=CARTESIAN_POINT('Ctrl Pts',(2.36016431023493,6.604438589221,68.1641588629044));
#144030=CARTESIAN_POINT('Ctrl Pts',(2.19261277603009,6.6619344386964,68.1721855303646));
#144031=CARTESIAN_POINT('Ctrl Pts',(2.02323538748915,6.71298332556485,68.1802121978247));
#144032=CARTESIAN_POINT('Ctrl Pts',(1.85372202337752,6.76407319429979,68.1882453090652));
#144033=CARTESIAN_POINT('Ctrl Pts',(1.68238023097071,6.80870566659897,68.1962784203057));
#144034=CARTESIAN_POINT('Ctrl Pts',(1.5097518764689,6.84677119772515,68.2043115315462));
#144035=CARTESIAN_POINT('Ctrl Pts',(1.40803297891685,6.8692007914733,68.2090449325084));
#144036=CARTESIAN_POINT('Ctrl Pts',(1.30586757527244,6.88935131737869,68.2137783334706));
#144037=CARTESIAN_POINT('Ctrl Pts',(1.20336758864791,6.90720877121082,68.2185117344328));
#144038=CARTESIAN_POINT('Ctrl Pts',(0.992214426209671,6.94399568186245,
68.2282626877271));
#144039=CARTESIAN_POINT('Ctrl Pts',(0.779516735548898,6.97107099913281,
68.2380136410215));
#144040=CARTESIAN_POINT('Ctrl Pts',(0.566088162918322,6.98835966120117,
68.2477645943159));
#144041=CARTESIAN_POINT('Ctrl Pts',(0.352352106390719,7.00567323083052,
68.2575295956877));
#144042=CARTESIAN_POINT('Ctrl Pts',(0.137883100145668,7.01317193896387,
68.2672945970595));
#144043=CARTESIAN_POINT('Ctrl Pts',(-0.076500574440827,7.01083263418906,
68.2770595984314));
#144044=CARTESIAN_POINT('Ctrl Pts',(-0.290526915861115,7.0084972285506,
68.2868083235692));
#144045=CARTESIAN_POINT('Ctrl Pts',(-0.504468171976303,6.99635658321835,
68.296557048707));
#144046=CARTESIAN_POINT('Ctrl Pts',(-0.717509613025243,6.97443951280075,
68.3063057738448));
#144047=CARTESIAN_POINT('Ctrl Pts',(-0.9299663379256,6.95258259624307,68.3160277425122));
#144048=CARTESIAN_POINT('Ctrl Pts',(-1.14152813827517,6.92100282537907,
68.3257497111796));
#144049=CARTESIAN_POINT('Ctrl Pts',(-1.35138703438341,6.8797804940129,68.3354716798469));
#144050=CARTESIAN_POINT('Ctrl Pts',(-1.55985734898668,6.83883092004701,
68.3451293207868));
#144051=CARTESIAN_POINT('Ctrl Pts',(-1.76664716884618,6.78836594907956,
68.3547869617267));
#144052=CARTESIAN_POINT('Ctrl Pts',(-1.97096519591468,6.72851564306668,
68.3644446026666));
#144053=CARTESIAN_POINT('Ctrl Pts',(-2.06077000302823,6.7022093730606,68.3686894683508));
#144054=CARTESIAN_POINT('Ctrl Pts',(-2.15009729759262,6.67409061705496,
68.3729343340351));
#144055=CARTESIAN_POINT('Ctrl Pts',(-2.2388799771677,6.64417361380161,68.3771791997193));
#144056=CARTESIAN_POINT('Ctrl Pts',(-2.40310378761465,6.58883529449278,
68.3850310467332));
#144057=CARTESIAN_POINT('Ctrl Pts',(-2.56539553606999,6.52736341128697,
68.392882893747));
#144058=CARTESIAN_POINT('Ctrl Pts',(-2.7252486497801,6.45992618838418,68.4007347407609));
#144059=CARTESIAN_POINT('Ctrl Pts',(-2.88505643043961,6.39250809013256,
68.4085843610544));
#144060=CARTESIAN_POINT('Ctrl Pts',(-3.04242660089788,6.31912816543598,
68.416433981348));
#144061=CARTESIAN_POINT('Ctrl Pts',(-3.19687107404595,6.24000335724496,
68.4242836016415));
#144062=CARTESIAN_POINT('Ctrl Pts',(-3.35130321677823,6.16088486615784,
68.4321325952432));
#144063=CARTESIAN_POINT('Ctrl Pts',(-3.50280978803219,6.07602257923392,
68.439981588845));
#144064=CARTESIAN_POINT('Ctrl Pts',(-3.65092612509082,5.98567999408833,
68.4478305824467));
#144065=CARTESIAN_POINT('Ctrl Pts',(-3.79911744911363,5.89529167113739,
68.4556835497641));
#144066=CARTESIAN_POINT('Ctrl Pts',(-3.9439147834452,5.79941770524224,68.4635365170815));
#144067=CARTESIAN_POINT('Ctrl Pts',(-4.08488107546139,5.69836583257318,
68.4713894843988));
#144068=CARTESIAN_POINT('Ctrl Pts',(-4.22588316817927,5.59728829612382,
68.4792444461061));
#144069=CARTESIAN_POINT('Ctrl Pts',(-4.36305197862399,5.49103046672035,
68.4870994078133));
#144070=CARTESIAN_POINT('Ctrl Pts',(-4.49598306686708,5.37994078266151,
68.4949543695205));
#144071=CARTESIAN_POINT('Ctrl Pts',(-4.62904610032678,5.2687408328054,68.5028171279338));
#144072=CARTESIAN_POINT('Ctrl Pts',(-4.7578627272447,5.15269970462525,68.510679886347));
#144073=CARTESIAN_POINT('Ctrl Pts',(-4.88206453376931,5.03220353827346,
68.5185426447603));
#144074=CARTESIAN_POINT('Ctrl Pts',(-4.97317719685091,4.94380927965001,
68.5243106515088));
#144075=CARTESIAN_POINT('Ctrl Pts',(-5.061807165531,4.85301833476021,68.5300786582572));
#144076=CARTESIAN_POINT('Ctrl Pts',(-5.14782290711444,4.75999431506886,
68.5358466650056));
#144077=CARTESIAN_POINT('Ctrl Pts',(-5.27276131814438,4.62487633556995,
68.5442247314466));
#144078=CARTESIAN_POINT('Ctrl Pts',(-5.3924597185564,4.48474669896059,68.5526027978877));
#144079=CARTESIAN_POINT('Ctrl Pts',(-5.50651270748239,4.34003967318675,
68.5609808643287));
#144080=CARTESIAN_POINT('Ctrl Pts',(-5.6204877083297,4.19543159635777,68.5693532019474));
#144081=CARTESIAN_POINT('Ctrl Pts',(-5.72882479108253,4.04625262793844,
68.5777255395661));
#144082=CARTESIAN_POINT('Ctrl Pts',(-5.83115784931043,3.89297119163826,
68.5860978771849));
#144083=CARTESIAN_POINT('Ctrl Pts',(-5.93343594061958,3.7397720885391,68.5944657177075));
#144084=CARTESIAN_POINT('Ctrl Pts',(-6.02971625560652,3.5824751840913,68.60283355823));
#144085=CARTESIAN_POINT('Ctrl Pts',(-6.11967489796486,3.42157941683643,
68.6112013987526));
#144086=CARTESIAN_POINT('Ctrl Pts',(-6.20959839845501,3.2607465026627,68.6195659704225));
#144087=CARTESIAN_POINT('Ctrl Pts',(-6.29320499072813,3.09631781569016,
68.6279305420924));
#144088=CARTESIAN_POINT('Ctrl Pts',(-6.37021556185153,2.92881891861627,
68.6362951137623));
#144089=CARTESIAN_POINT('Ctrl Pts',(-6.44720732169097,2.76136093630604,
68.6446576422279));
#144090=CARTESIAN_POINT('Ctrl Pts',(-6.51760613671815,2.59083453803991,
68.6530201706935));
#144091=CARTESIAN_POINT('Ctrl Pts',(-6.58117988695038,2.41778780253763,
68.661382699159));
#144092=CARTESIAN_POINT('Ctrl Pts',(-6.6447587105668,2.24472725736442,68.6697458949806));
#144093=CARTESIAN_POINT('Ctrl Pts',(-6.70151126222094,2.06914627954993,
68.6781090908021));
#144094=CARTESIAN_POINT('Ctrl Pts',(-6.75125414920358,1.89161147579558,
68.6864722866236));
#144095=CARTESIAN_POINT('Ctrl Pts',(-6.80100042855138,1.71406456452352,
68.6948360527983));
#144096=CARTESIAN_POINT('Ctrl Pts',(-6.84373600107298,1.53456387818423,
68.7031998189729));
#144097=CARTESIAN_POINT('Ctrl Pts',(-6.87932775394974,1.35368985230621,
68.7115635851476));
#144098=CARTESIAN_POINT('Ctrl Pts',(-6.91492667933058,1.17277937641989,
68.7199290368012));
#144099=CARTESIAN_POINT('Ctrl Pts',(-6.94337885093542,0.99049533173565,
68.7282944884548));
#144100=CARTESIAN_POINT('Ctrl Pts',(-6.96460246864185,0.807427406203142,
68.7366599401083));
#144101=CARTESIAN_POINT('Ctrl Pts',(-6.98583319409612,0.624298171582286,
68.7450281933352));
#144102=CARTESIAN_POINT('Ctrl Pts',(-6.99983050060367,0.440384859106724,
68.753396446562));
#144103=CARTESIAN_POINT('Ctrl Pts',(-7.00656450931252,0.256281757724323,
68.7617646997889));
#144104=CARTESIAN_POINT('Ctrl Pts',(-7.01330476140815,0.0720079665017409,
68.7701407115804));
#144105=CARTESIAN_POINT('Ctrl Pts',(-7.01276824690758,-0.11245563634756,
68.7785167233719));
#144106=CARTESIAN_POINT('Ctrl Pts',(-7.00497722994805,-0.296514030712585,
68.7868927351633));
#144107=CARTESIAN_POINT('Ctrl Pts',(-6.99718239217753,-0.480662689588405,
68.7952728546545));
#144108=CARTESIAN_POINT('Ctrl Pts',(-6.98212597764238,-0.664405415692843,
68.8036529741456));
#144109=CARTESIAN_POINT('Ctrl Pts',(-6.95988216650146,-0.847152165147994,
68.8120330936368));
#144110=CARTESIAN_POINT('Ctrl Pts',(-6.93761293898861,-1.03010772591359,
68.820422788476));
#144111=CARTESIAN_POINT('Ctrl Pts',(-6.90813995078051,-1.21206471037406,
68.8288124833152));
#144112=CARTESIAN_POINT('Ctrl Pts',(-6.87158878422862,-1.39244179158893,
68.8372021781544));
#144113=CARTESIAN_POINT('Ctrl Pts',(-6.84838307933848,-1.50696008773349,
68.8425286506291));
#144114=CARTESIAN_POINT('Ctrl Pts',(-6.82232535479691,-1.62084179431044,
68.8478551231038));
#144115=CARTESIAN_POINT('Ctrl Pts',(-6.7934581919395,-1.73394127838003,
68.8531815955785));
#144116=CARTESIAN_POINT('Ctrl Pts',(-6.74803519108956,-1.91190535425393,
68.8615628959834));
#144117=CARTESIAN_POINT('Ctrl Pts',(-6.69556204792654,-2.08829092126212,
68.8699441963883));
#144118=CARTESIAN_POINT('Ctrl Pts',(-6.63616141893687,-2.26251810695821,
68.8783254967933));
#144119=CARTESIAN_POINT('Ctrl Pts',(-6.57683607154881,-2.4365244852015,
68.8866961751268));
#144120=CARTESIAN_POINT('Ctrl Pts',(-6.51060083998907,-2.60837762595666,
68.8950668534604));
#144121=CARTESIAN_POINT('Ctrl Pts',(-6.43762892445178,-2.7775097467987,
68.903437531794));
#144122=CARTESIAN_POINT('Ctrl Pts',(-6.36473981951007,-2.94644993172191,
68.9117987108449));
#144123=CARTESIAN_POINT('Ctrl Pts',(-6.28512939688618,-3.11267495222198,
68.9201598898957));
#144124=CARTESIAN_POINT('Ctrl Pts',(-6.19902015630381,-3.2756336279015,
68.9285210689466));
#144125=CARTESIAN_POINT('Ctrl Pts',(-6.11302265261846,-3.43838084547686,
68.9368713983813));
#144126=CARTESIAN_POINT('Ctrl Pts',(-6.02054330380782,-3.59786988397885,
68.9452217278161));
#144127=CARTESIAN_POINT('Ctrl Pts',(-5.92185200977182,-3.75357101129864,
68.9535720572508));
#144128=CARTESIAN_POINT('Ctrl Pts',(-5.82323665278288,-3.90915233591497,
68.9619159616066));
#144129=CARTESIAN_POINT('Ctrl Pts',(-5.71841905034829,-4.06095128199274,
68.9702598659623));
#144130=CARTESIAN_POINT('Ctrl Pts',(-5.60771474562165,-4.20846312734679,
68.9786037703181));
#144131=CARTESIAN_POINT('Ctrl Pts',(-5.49709935928305,-4.35585649026659,
68.9869409727978));
#144132=CARTESIAN_POINT('Ctrl Pts',(-5.38060689654618,-4.49896935858342,
68.9952781752776));
#144133=CARTESIAN_POINT('Ctrl Pts',(-5.25859597100946,-4.63732627450162,
69.0036153777573));
#144134=CARTESIAN_POINT('Ctrl Pts',(-5.21843064780921,-4.68287260750744,
69.0063599387932));
#144135=CARTESIAN_POINT('Ctrl Pts',(-5.17766763597248,-4.72790378649475,
69.0091044998292));
#144136=CARTESIAN_POINT('Ctrl Pts',(-5.1363207172274,-4.77240359276964,
69.0118490608651));
#144137=CARTESIAN_POINT('Ctrl Pts',(-5.01070374824256,-4.90759941761767,
69.020187371167));
#144138=CARTESIAN_POINT('Ctrl Pts',(-4.87979739535122,-5.0377770788816,
69.028525681469));
#144139=CARTESIAN_POINT('Ctrl Pts',(-4.7440385786251,-5.16253082576916,
69.0368639917709));
#144140=CARTESIAN_POINT('Ctrl Pts',(-4.60819434705807,-5.2873630634811,
69.0452075482548));
#144141=CARTESIAN_POINT('Ctrl Pts',(-4.46749180331283,-5.40676435837665,
69.0535511047386));
#144142=CARTESIAN_POINT('Ctrl Pts',(-4.32240126739949,-5.52036899546428,
69.0618946612225));
#144143=CARTESIAN_POINT('Ctrl Pts',(-4.17720034723872,-5.63406006246472,
69.0702445654477));
#144144=CARTESIAN_POINT('Ctrl Pts',(-4.02760503364756,-5.74194547323626,
69.078594469673));
#144145=CARTESIAN_POINT('Ctrl Pts',(-3.87411529769811,-5.84370235575371,
69.0869443738982));
#144146=CARTESIAN_POINT('Ctrl Pts',(-3.72039533850314,-5.94561186606483,
69.0953068023619));
#144147=CARTESIAN_POINT('Ctrl Pts',(-3.56276955743051,-6.04137429773488,
69.1036692308256));
#144148=CARTESIAN_POINT('Ctrl Pts',(-3.40176455165533,-6.13071158166825,
69.1120316592893));
#144149=CARTESIAN_POINT('Ctrl Pts',(-3.24062186465198,-6.22012526115785,
69.1204012387693));
#144150=CARTESIAN_POINT('Ctrl Pts',(-3.0760944791062,-6.30310268301348,
69.1287708182493));
#144151=CARTESIAN_POINT('Ctrl Pts',(-2.9087302278244,-6.37941337618442,
69.1371403977293));
#144152=CARTESIAN_POINT('Ctrl Pts',(-2.7411078375766,-6.4558417693019,69.1455228862659));
#144153=CARTESIAN_POINT('Ctrl Pts',(-2.57064014066444,-6.52558276217499,
69.1539053748025));
#144154=CARTESIAN_POINT('Ctrl Pts',(-2.39789275105042,-6.58845482013498,
69.1622878633391));
#144155=CARTESIAN_POINT('Ctrl Pts',(-2.34136697454129,-6.60902758771692,
69.1650307509432));
#144156=CARTESIAN_POINT('Ctrl Pts',(-2.28459721093394,-6.62886529793762,
69.1677736385473));
#144157=CARTESIAN_POINT('Ctrl Pts',(-2.22760354135047,-6.64796277253888,
69.1705165261514));
#144158=CARTESIAN_POINT('Ctrl Pts',(-2.05327316391249,-6.70637750490621,
69.1789063812842));
#144159=CARTESIAN_POINT('Ctrl Pts',(-1.87649502487395,-6.75798071670235,
69.1872962364169));
#144160=CARTESIAN_POINT('Ctrl Pts',(-1.6978281097713,-6.80257350362129,
69.1956860915497));
#144161=CARTESIAN_POINT('Ctrl Pts',(-1.51932606599329,-6.84712514094158,
69.2040682046418));
#144162=CARTESIAN_POINT('Ctrl Pts',(-1.33893903809474,-6.88467917035178,
69.2124503177338));
#144163=CARTESIAN_POINT('Ctrl Pts',(-1.15724183614579,-6.91508625363227,
69.2208324308259));
#144164=CARTESIAN_POINT('Ctrl Pts',(-0.975685592715808,-6.94546974746075,
69.2292080411748));
#144165=CARTESIAN_POINT('Ctrl Pts',(-0.792821524716646,-6.96871729517089,
69.2375836515236));
#144166=CARTESIAN_POINT('Ctrl Pts',(-0.609235770882665,-6.98473036974063,
69.2459592618725));
#144167=CARTESIAN_POINT('Ctrl Pts',(-0.425765495213908,-7.00073337184867,
69.2543296038381));
#144168=CARTESIAN_POINT('Ctrl Pts',(-0.241574765487565,-7.00951094579591,
69.2626999458037));
#144169=CARTESIAN_POINT('Ctrl Pts',(-0.0572564586363296,-7.01101620740135,
69.2710702877692));
#144170=CARTESIAN_POINT('Ctrl Pts',(0.126972928256298,-7.01252074282934,
69.2794365916636));
#144171=CARTESIAN_POINT('Ctrl Pts',(0.311329441413336,-7.00675995946025,
69.2878028955579));
#144172=CARTESIAN_POINT('Ctrl Pts',(0.495218112664075,-6.99373902740083,
69.2961691994522));
#144173=CARTESIAN_POINT('Ctrl Pts',(0.679055355407793,-6.98072173693113,
69.3045331635258));
#144174=CARTESIAN_POINT('Ctrl Pts',(0.86242468949627,-6.96044836823186,
69.3128971275994));
#144175=CARTESIAN_POINT('Ctrl Pts',(1.04473362047737,-6.93297614482729,
69.321261091673));
#144176=CARTESIAN_POINT('Ctrl Pts',(1.22701449714345,-6.90550814894139,
69.3296237686716));
#144177=CARTESIAN_POINT('Ctrl Pts',(1.40823497115293,-6.87084355600873,
69.3379864456701));
#144178=CARTESIAN_POINT('Ctrl Pts',(1.58780970526545,-6.82909122082616,
69.3463491226686));
#144179=CARTESIAN_POINT('Ctrl Pts',(1.76738074226206,-6.78733974524793,
69.3547116274949));
#144180=CARTESIAN_POINT('Ctrl Pts',(1.94530578690506,-6.7385008932111,69.3630741323212));
#144181=CARTESIAN_POINT('Ctrl Pts',(2.12101127108758,-6.68273430194703,
69.3714366371475));
#144182=CARTESIAN_POINT('Ctrl Pts',(2.29673655810607,-6.62696142552537,
69.3798000844674));
#144183=CARTESIAN_POINT('Ctrl Pts',(2.47024147285186,-6.56425935313681,
69.3881635317874));
#144184=CARTESIAN_POINT('Ctrl Pts',(2.64096873085647,-6.49483723623144,
69.3965269791074));
#144185=CARTESIAN_POINT('Ctrl Pts',(2.81179651786845,-6.42537424163269,
69.4048953510602));
#144186=CARTESIAN_POINT('Ctrl Pts',(2.97984307476608,-6.34918341862338,
69.413263723013));
#144187=CARTESIAN_POINT('Ctrl Pts',(3.14457123150028,-6.26652202840785,
69.4216320949658));
#144188=CARTESIAN_POINT('Ctrl Pts',(3.30934874509559,-6.18383587067936,
69.4300029743015));
#144189=CARTESIAN_POINT('Ctrl Pts',(3.47080558452627,-6.09467543208481,
69.4383738536373));
#144190=CARTESIAN_POINT('Ctrl Pts',(3.62842960467726,-5.99934372797572,
69.446744732973));
#144191=CARTESIAN_POINT('Ctrl Pts',(3.78618717795604,-5.90393125034462,
69.4551227048643));
#144192=CARTESIAN_POINT('Ctrl Pts',(3.94010516419902,-5.80233723385321,
69.4635006767556));
#144193=CARTESIAN_POINT('Ctrl Pts',(4.08969983616813,-5.69490841125179,
69.4718786486469));
#144194=CARTESIAN_POINT('Ctrl Pts',(4.18476846836167,-5.62663651969011,
69.477202918006));
#144195=CARTESIAN_POINT('Ctrl Pts',(4.2780916519057,-5.55600897634522,69.4825271873652));
#144196=CARTESIAN_POINT('Ctrl Pts',(4.36955219335629,-5.48312321510608,
69.4878514567244));
#144197=CARTESIAN_POINT('Ctrl Pts',(4.50462026549706,-5.37548620464293,
69.4957142879136));
#144198=CARTESIAN_POINT('Ctrl Pts',(4.63590515167311,-5.26269828661825,
69.5035771191028));
#144199=CARTESIAN_POINT('Ctrl Pts',(4.76297282760539,-5.14506719159164,
69.5114399502921));
#144200=CARTESIAN_POINT('Ctrl Pts',(4.88994286880163,-5.02752648053427,
69.5192967399334));
#144201=CARTESIAN_POINT('Ctrl Pts',(5.0127018657146,-4.90515025023536,69.5271535295747));
#144202=CARTESIAN_POINT('Ctrl Pts',(5.13084717804576,-4.77828774751373,
69.5350103192161));
#144203=CARTESIAN_POINT('Ctrl Pts',(5.24892586201304,-4.65149678923875,
69.542862678));
#144204=CARTESIAN_POINT('Ctrl Pts',(5.36239577814006,-4.52022486952671,
69.5507150367839));
#144205=CARTESIAN_POINT('Ctrl Pts',(5.47088981512386,-4.38485931282567,
69.5585673955677));
#144206=CARTESIAN_POINT('Ctrl Pts',(5.57935823539993,-4.24952571751164,
69.5664179003181));
#144207=CARTESIAN_POINT('Ctrl Pts',(5.68285287002074,-4.11010070088217,
69.5742684050685));
#144208=CARTESIAN_POINT('Ctrl Pts',(5.78104577593687,-3.96700596155621,
69.5821189098188));
#144209=CARTESIAN_POINT('Ctrl Pts',(5.87922288570915,-3.82393424166394,
69.5899681516704));
#144210=CARTESIAN_POINT('Ctrl Pts',(5.97209975122079,-3.67719429056144,
69.597817393522));
#144211=CARTESIAN_POINT('Ctrl Pts',(6.05939107001222,-3.52723778942619,
69.6056666353736));
#144212=CARTESIAN_POINT('Ctrl Pts',(6.14671179895765,-3.37723076501036,
69.6135185217884));
#144213=CARTESIAN_POINT('Ctrl Pts',(6.2284430301337,-3.22400535592021,69.6213704082032));
#144214=CARTESIAN_POINT('Ctrl Pts',(6.30434475481217,-3.06803907650673,
69.629222294618));
#144215=CARTESIAN_POINT('Ctrl Pts',(6.36007844651651,-2.9535149788011,69.6349878370822));
#144216=CARTESIAN_POINT('Ctrl Pts',(6.41266993518779,-2.83751361474837,
69.6407533795464));
#144217=CARTESIAN_POINT('Ctrl Pts',(6.4620406373389,-2.72023112324682,69.6465189220106));
#144218=CARTESIAN_POINT('Ctrl Pts',(6.54286855733576,-2.52822048886078,
69.6559580586793));
#144219=CARTESIAN_POINT('Ctrl Pts',(6.61503119340741,-2.33285131357872,
69.665397195348));
#144220=CARTESIAN_POINT('Ctrl Pts',(6.67832305966802,-2.13486010623796,
69.6748363320168));
#144221=CARTESIAN_POINT('Ctrl Pts',(6.74199387910535,-1.93568344804203,
69.6843319844914));
#144222=CARTESIAN_POINT('Ctrl Pts',(6.79668738743301,-1.73385338414025,
69.6938276369659));
#144223=CARTESIAN_POINT('Ctrl Pts',(6.84224674383686,-1.53012615785559,
69.7033232894405));
#144224=CARTESIAN_POINT('Ctrl Pts',(6.88791457833146,-1.32591385139671,
69.7128415513269));
#144225=CARTESIAN_POINT('Ctrl Pts',(6.9244047295736,-1.11979545018396,69.7223598132133));
#144226=CARTESIAN_POINT('Ctrl Pts',(6.95161148449768,-0.912537303949778,
69.7318780750997));
#144227=CARTESIAN_POINT('Ctrl Pts',(6.97886808837653,-0.704899413715052,
69.7414137766039));
#144228=CARTESIAN_POINT('Ctrl Pts',(6.99680725098884,-0.49611770472743,
69.7509494781081));
#144229=CARTESIAN_POINT('Ctrl Pts',(7.00537487861924,-0.286965803730128,
69.7604851796122));
#144230=CARTESIAN_POINT('Ctrl Pts',(7.00928301589988,-0.191560823861168,
69.7648349053651));
#144231=CARTESIAN_POINT('Ctrl Pts',(7.01124189309494,-0.0960788486770531,
69.7691846311181));
#144232=CARTESIAN_POINT('Ctrl Pts',(7.01124997488654,-0.00059342524868163,
69.773534356871));
#144233=CARTESIAN_POINT('Ctrl Pts',(7.01124997488661,-0.000593424381606831,
69.7735343569105));
#144234=CARTESIAN_POINT('Ctrl Pts',(7.01126957801824,0.231015623752868,
69.784085033706));
#144235=CARTESIAN_POINT('Ctrl Pts',(6.99981027861164,0.462672585231173,
69.7946357105016));
#144236=CARTESIAN_POINT('Ctrl Pts',(6.97687299454425,0.693447748932259,
69.8051863872972));
#144237=CARTESIAN_POINT('Ctrl Pts',(6.95940918677021,0.869153516278404,
69.8132193780777));
#144238=CARTESIAN_POINT('Ctrl Pts',(6.9352853685406,1.04438262091616,69.8212523688583));
#144239=CARTESIAN_POINT('Ctrl Pts',(6.90454037206146,1.21858475826403,69.8292853596388));
#144240=CARTESIAN_POINT('Ctrl Pts',(6.8738143646981,1.39267930267211,69.8373133889814));
#144241=CARTESIAN_POINT('Ctrl Pts',(6.83647538110482,1.56574778262201,69.845341418324));
#144242=CARTESIAN_POINT('Ctrl Pts',(6.79261404458961,1.73724523419812,69.8533694476666));
#144243=CARTESIAN_POINT('Ctrl Pts',(6.74877309020606,1.90866299181328,69.8613937464263));
#144244=CARTESIAN_POINT('Ctrl Pts',(6.69841590921792,2.07851082043406,69.869418045186));
#144245=CARTESIAN_POINT('Ctrl Pts',(6.64168414458086,2.24625427904394,69.8774423439457));
#144246=CARTESIAN_POINT('Ctrl Pts',(6.61915969795449,2.31285415663549,69.8806282643958));
#144247=CARTESIAN_POINT('Ctrl Pts',(6.5956309472628,2.37912244721619,69.8838141848459));
#144248=CARTESIAN_POINT('Ctrl Pts',(6.57110895151813,2.44502632087638,69.887000105296));
#144249=CARTESIAN_POINT('',(7.01124999898235,-0.000119457234741844,69.2264656431203));
#144250=CARTESIAN_POINT('Ctrl Pts',(6.57110895151815,2.44502632087633,69.3398494195812));
#144251=CARTESIAN_POINT('Ctrl Pts',(6.63437020280986,2.27500910220762,69.3316255394411));
#144252=CARTESIAN_POINT('Ctrl Pts',(6.69102680977921,2.10254104764004,69.323401659301));
#144253=CARTESIAN_POINT('Ctrl Pts',(6.74090331182414,1.92817247753887,69.3151777791609));
#144254=CARTESIAN_POINT('Ctrl Pts',(6.79080539628015,1.75371447116496,69.3069496808685));
#144255=CARTESIAN_POINT('Ctrl Pts',(6.8339203313287,1.57735433361791,69.2987215825761));
#144256=CARTESIAN_POINT('Ctrl Pts',(6.8701229150204,1.39965627745229,69.2904934842837));
#144257=CARTESIAN_POINT('Ctrl Pts',(6.90633538304412,1.22190970467799,69.2822631394871));
#144258=CARTESIAN_POINT('Ctrl Pts',(6.93563167566411,1.04282482491902,69.2740327946906));
#144259=CARTESIAN_POINT('Ctrl Pts',(6.95793805352408,0.86297427877169,69.265802449894));
#144260=CARTESIAN_POINT('Ctrl Pts',(6.98026350914649,0.682969913567984,
69.2575650660091));
#144261=CARTESIAN_POINT('Ctrl Pts',(6.99558707148393,0.502198917429808,
69.2493276821243));
#144262=CARTESIAN_POINT('Ctrl Pts',(7.00388696177219,0.321238212573748,
69.2410902982394));
#144263=CARTESIAN_POINT('Ctrl Pts',(7.00879883811094,0.214145639834064,
69.2362154131997));
#144264=CARTESIAN_POINT('Ctrl Pts',(7.01125182384951,0.106986653807984,
69.23134052816));
#144265=CARTESIAN_POINT('Ctrl Pts',(7.01124999898235,-0.000119457234834394,
69.2264656431203));
#144266=CARTESIAN_POINT('Ctrl Pts',(7.01124999898234,-0.000119457912646379,
69.2264656430895));
#144267=CARTESIAN_POINT('Ctrl Pts',(7.0112440780319,-0.347633178973828,
69.2106487170207));
#144268=CARTESIAN_POINT('Ctrl Pts',(6.98539996000994,-0.694636108609602,
69.1948317909518));
#144269=CARTESIAN_POINT('Ctrl Pts',(6.93395267227689,-1.03823258527373,
69.1790148648829));
#144270=CARTESIAN_POINT('Ctrl Pts',(6.90837745387949,-1.20903954747671,
69.1711520336937));
#144271=CARTESIAN_POINT('Ctrl Pts',(6.87644938733158,-1.37914961289592,
69.1632892025045));
#144272=CARTESIAN_POINT('Ctrl Pts',(6.83821763069403,-1.54803300926221,
69.1554263713153));
#144273=CARTESIAN_POINT('Ctrl Pts',(6.8000152501149,-1.71678664103078,69.1475695816739));
#144274=CARTESIAN_POINT('Ctrl Pts',(6.75551889518727,-1.88431510865091,
69.1397127920326));
#144275=CARTESIAN_POINT('Ctrl Pts',(6.70482937411485,-2.05009502865275,
69.1318560023913));
#144276=CARTESIAN_POINT('Ctrl Pts',(6.6541684395327,-2.2157814566276,69.1240036436074));
#144277=CARTESIAN_POINT('Ctrl Pts',(6.59732139762873,-2.37972093508718,
69.1161512848235));
#144278=CARTESIAN_POINT('Ctrl Pts',(6.53443980464629,-2.5414017789311,69.1082989260396));
#144279=CARTESIAN_POINT('Ctrl Pts',(6.47157305874174,-2.70304444804109,
69.1004484212893));
#144280=CARTESIAN_POINT('Ctrl Pts',(6.40267472777406,-2.86242918585216,
69.0925979165389));
#144281=CARTESIAN_POINT('Ctrl Pts',(6.32794573150476,-3.01906100992191,
69.0847474117886));
#144282=CARTESIAN_POINT('Ctrl Pts',(6.25322875677584,-3.17566763686751,
69.076898169937));
#144283=CARTESIAN_POINT('Ctrl Pts',(6.17268315097053,-3.32952188861905,
69.0690489280854));
#144284=CARTESIAN_POINT('Ctrl Pts',(6.08655713355269,-3.48015068962522,
69.0611996862339));
#144285=CARTESIAN_POINT('Ctrl Pts',(6.00040209859372,-3.63083024042291,
69.0533477998191));
#144286=CARTESIAN_POINT('Ctrl Pts',(5.9086630860813,-3.77828183832323,69.0454959134044));
#144287=CARTESIAN_POINT('Ctrl Pts',(5.81163335102251,-3.92205868846744,
69.0376440269896));
#144288=CARTESIAN_POINT('Ctrl Pts',(5.74038562426792,-4.02763223998237,
69.0318784845252));
#144289=CARTESIAN_POINT('Ctrl Pts',(5.66628620282106,-4.13122498531178,
69.0261129420608));
#144290=CARTESIAN_POINT('Ctrl Pts',(5.58946555198211,-4.23267071784534,
69.0203473995965));
#144291=CARTESIAN_POINT('Ctrl Pts',(5.46081733378235,-4.402557494277,69.0106920952363));
#144292=CARTESIAN_POINT('Ctrl Pts',(5.32460260861429,-4.5663359541943,69.0010367908762));
#144293=CARTESIAN_POINT('Ctrl Pts',(5.18138853131843,-4.72343513240331,
68.991381486516));
#144294=CARTESIAN_POINT('Ctrl Pts',(5.03738107490166,-4.88140461058741,
68.9816726935811));
#144295=CARTESIAN_POINT('Ctrl Pts',(4.88629657357506,-5.03262060014217,
68.9719639006461));
#144296=CARTESIAN_POINT('Ctrl Pts',(4.72874223922069,-5.17654550810771,
68.9622551077112));
#144297=CARTESIAN_POINT('Ctrl Pts',(4.57042974003007,-5.32116299495232,
68.9524995952402));
#144298=CARTESIAN_POINT('Ctrl Pts',(4.40558503934989,-5.45841904930235,
68.9427440827692));
#144299=CARTESIAN_POINT('Ctrl Pts',(4.23485403427872,-5.58781154575325,
68.9329885702982));
#144300=CARTESIAN_POINT('Ctrl Pts',(4.06395397924646,-5.71733216068197,
68.923223398369));
#144301=CARTESIAN_POINT('Ctrl Pts',(3.88715599910566,-5.83897362941886,
68.9134582264398));
#144302=CARTESIAN_POINT('Ctrl Pts',(3.70513707572406,-5.95227568351761,
68.9036930545106));
#144303=CARTESIAN_POINT('Ctrl Pts',(3.52336633101492,-6.06542325283614,
68.8939411971718));
#144304=CARTESIAN_POINT('Ctrl Pts',(3.33638890290019,-6.17025411324706,
68.8841893398329));
#144305=CARTESIAN_POINT('Ctrl Pts',(3.14490751207708,-6.26635326988362,
68.8744374824941));
#144306=CARTESIAN_POINT('Ctrl Pts',(3.0614077579646,-6.30825946199491,68.8701849664327));
#144307=CARTESIAN_POINT('Ctrl Pts',(2.97705189743213,-6.34850579991736,
68.8659324503714));
#144308=CARTESIAN_POINT('Ctrl Pts',(2.89189988375889,-6.38706048388579,
68.86167993431));
#144309=CARTESIAN_POINT('Ctrl Pts',(2.73104687373215,-6.45989066956701,
68.8536468887113));
#144310=CARTESIAN_POINT('Ctrl Pts',(2.56727285395838,-6.52671653460162,
68.8456138431125));
#144311=CARTESIAN_POINT('Ctrl Pts',(2.40107367693294,-6.58729624052538,
68.8375807975138));
#144312=CARTESIAN_POINT('Ctrl Pts',(2.23498133913767,-6.64783700348166,
68.8295529158661));
#144313=CARTESIAN_POINT('Ctrl Pts',(2.06646729025432,-6.7021394748109,68.8215250342184));
#144314=CARTESIAN_POINT('Ctrl Pts',(1.89604864416291,-6.75000934084302,
68.8134971525706));
#144315=CARTESIAN_POINT('Ctrl Pts',(1.72570694377035,-6.79785759315868,
68.8054728955906));
#144316=CARTESIAN_POINT('Ctrl Pts',(1.55346271059627,-6.83927892421513,
68.7974486386106));
#144317=CARTESIAN_POINT('Ctrl Pts',(1.37984950630213,-6.87412844675293,
68.7894243816306));
#144318=CARTESIAN_POINT('Ctrl Pts',(1.20625729361261,-6.90897375562851,
68.781401094865));
#144319=CARTESIAN_POINT('Ctrl Pts',(1.03129679716905,-6.93724875903058,
68.7733778080994));
#144320=CARTESIAN_POINT('Ctrl Pts',(0.855513271464657,-6.95885936090448,
68.7653545213337));
#144321=CARTESIAN_POINT('Ctrl Pts',(0.679744149652203,-6.98046819198232,
68.7573318920049));
#144322=CARTESIAN_POINT('Ctrl Pts',(0.503152497308208,-6.99541366853733,
68.7493092626761));
#144323=CARTESIAN_POINT('Ctrl Pts',(0.326289914393268,-7.00365343619066,
68.7412866333472));
#144324=CARTESIAN_POINT('Ctrl Pts',(0.149360843738384,-7.01189630141003,
68.7332609880809));
#144325=CARTESIAN_POINT('Ctrl Pts',(-0.0278389943924678,-7.01342840779972,
68.7252353428146));
#144326=CARTESIAN_POINT('Ctrl Pts',(-0.204756378946018,-7.0082595120173,
68.7172096975483));
#144327=CARTESIAN_POINT('Ctrl Pts',(-0.309077649702985,-7.0052116160867,
68.7124772880401));
#144328=CARTESIAN_POINT('Ctrl Pts',(-0.41330071978238,-6.9998347698926,
68.7077448785319));
#144329=CARTESIAN_POINT('Ctrl Pts',(-0.517312787693255,-6.9921394467065,
68.7030124690237));
#144330=CARTESIAN_POINT('Ctrl Pts',(-0.709187652006125,-6.9779436026873,
68.694282420189));
#144331=CARTESIAN_POINT('Ctrl Pts',(-0.900440130699388,-6.95584821871191,
68.6855523713543));
#144332=CARTESIAN_POINT('Ctrl Pts',(-1.09042849719825,-6.92593620061562,
68.6768223225197));
#144333=CARTESIAN_POINT('Ctrl Pts',(-1.28047179907019,-6.89601553342201,
68.6680897493805));
#144334=CARTESIAN_POINT('Ctrl Pts',(-1.46924998854195,-6.85827376325209,
68.6593571762413));
#144335=CARTESIAN_POINT('Ctrl Pts',(-1.65613021921969,-6.81284516626405,
68.6506246031021));
#144336=CARTESIAN_POINT('Ctrl Pts',(-1.84566538189065,-6.76677118353823,
68.6417679698217));
#144337=CARTESIAN_POINT('Ctrl Pts',(-2.03324796605526,-6.71279037058421,
68.6329113365413));
#144338=CARTESIAN_POINT('Ctrl Pts',(-2.21823189569369,-6.65109568563159,
68.6240547032609));
#144339=CARTESIAN_POINT('Ctrl Pts',(-2.4007407524607,-6.59022647152575,
68.6153165711541));
#144340=CARTESIAN_POINT('Ctrl Pts',(-2.58071980633433,-6.52184863553274,
68.6065784390473));
#144341=CARTESIAN_POINT('Ctrl Pts',(-2.75756609906633,-6.44619700069584,
68.5978403069405));
#144342=CARTESIAN_POINT('Ctrl Pts',(-2.93800981278901,-6.36900645444081,
68.5889244230733));
#144343=CARTESIAN_POINT('Ctrl Pts',(-3.11519167258863,-6.28424312418007,
68.5800085392061));
#144344=CARTESIAN_POINT('Ctrl Pts',(-3.28849396901101,-6.19220752060832,
68.5710926553389));
#144345=CARTESIAN_POINT('Ctrl Pts',(-3.46179626543339,-6.10017191703656,
68.5621767714717));
#144346=CARTESIAN_POINT('Ctrl Pts',(-3.63121873424672,-6.00086418736691,
68.5532608876044));
#144347=CARTESIAN_POINT('Ctrl Pts',(-3.7961707162443,-5.89463437845209,
68.5443450037372));
#144348=CARTESIAN_POINT('Ctrl Pts',(-3.95788135011537,-5.79049201212472,
68.5356043192409));
#144349=CARTESIAN_POINT('Ctrl Pts',(-4.11531273401089,-5.67968602162188,
68.5268636347445));
#144350=CARTESIAN_POINT('Ctrl Pts',(-4.2679340745156,-5.56258620590177,
68.5181229502482));
#144351=CARTESIAN_POINT('Ctrl Pts',(-4.42052795590595,-5.44550745838367,
68.5093838383461));
#144352=CARTESIAN_POINT('Ctrl Pts',(-4.56831330504335,-5.3221373136714,
68.5006447264441));
#144353=CARTESIAN_POINT('Ctrl Pts',(-4.71079085001859,-5.19288707078068,
68.4919056145421));
#144354=CARTESIAN_POINT('Ctrl Pts',(-4.85511439664656,-5.06196220497283,
68.4830532748678));
#144355=CARTESIAN_POINT('Ctrl Pts',(-4.99399141363427,-4.92500398339401,
68.4742009351935));
#144356=CARTESIAN_POINT('Ctrl Pts',(-5.1269390145189,-4.782480831525,68.4653485955192));
#144357=CARTESIAN_POINT('Ctrl Pts',(-5.25811884924494,-4.64185276917254,
68.4566139628694));
#144358=CARTESIAN_POINT('Ctrl Pts',(-5.38352579063847,-4.49580706297155,
68.4478793302195));
#144359=CARTESIAN_POINT('Ctrl Pts',(-5.5027336149339,-4.34483018374441,
68.4391446975696));
#144360=CARTESIAN_POINT('Ctrl Pts',(-5.62435108806826,-4.19080148083132,
68.4302335043831));
#144361=CARTESIAN_POINT('Ctrl Pts',(-5.73951596195329,-4.03164034016135,
68.4213223111966));
#144362=CARTESIAN_POINT('Ctrl Pts',(-5.84781877346933,-3.86789893290397,
68.4124111180101));
#144363=CARTESIAN_POINT('Ctrl Pts',(-5.95612158498537,-3.70415752564659,
68.4034999248236));
#144364=CARTESIAN_POINT('Ctrl Pts',(-6.05756215566655,-3.53583609719769,
68.3945887316371));
#144365=CARTESIAN_POINT('Ctrl Pts',(-6.15177738397906,-3.36351922552314,
68.3856775384507));
#144366=CARTESIAN_POINT('Ctrl Pts',(-6.23663020117123,-3.20832592744157,
68.3776518735984));
#144367=CARTESIAN_POINT('Ctrl Pts',(-6.31566086756942,-3.04982023554966,
68.3696262087461));
#144368=CARTESIAN_POINT('Ctrl Pts',(-6.38860452752145,-2.88848727769959,
68.3616005438938));
#144369=CARTESIAN_POINT('Ctrl Pts',(-6.46152503694502,-2.72720552297309,
68.3535774261907));
#144370=CARTESIAN_POINT('Ctrl Pts',(-6.52836223524753,-2.56309862235754,
68.3455543084876));
#144371=CARTESIAN_POINT('Ctrl Pts',(-6.58889796677334,-2.39667481022148,
68.3375311907845));
#144372=CARTESIAN_POINT('Ctrl Pts',(-6.64942606421354,-2.23027198558481,
68.3295090848668));
#144373=CARTESIAN_POINT('Ctrl Pts',(-6.70365415305433,-2.06155317601521,
68.3214869789491));
#144374=CARTESIAN_POINT('Ctrl Pts',(-6.75141284885911,-1.89104497745563,
68.3134648730313));
#144375=CARTESIAN_POINT('Ctrl Pts',(-6.79918929195661,-1.72047341747335,
68.3054397860719));
#144376=CARTESIAN_POINT('Ctrl Pts',(-6.84049143763795,-1.54811149266162,
68.2974146991125));
#144377=CARTESIAN_POINT('Ctrl Pts',(-6.8752001470764,-1.37449972722464,
68.2893896121531));
#144378=CARTESIAN_POINT('Ctrl Pts',(-6.9099156922215,-1.20085376981924,
68.281362944693));
#144379=CARTESIAN_POINT('Ctrl Pts',(-6.9380351509861,-1.0259578425942,68.2733362772328));
#144380=CARTESIAN_POINT('Ctrl Pts',(-6.95949086974734,-0.850360744862719,
68.2653096097727));
#144381=CARTESIAN_POINT('Ctrl Pts',(-6.98096381308399,-0.674622678399933,
68.2572764985322));
#144382=CARTESIAN_POINT('Ctrl Pts',(-6.9957622966471,-0.498182682104386,
68.2492433872918));
#144383=CARTESIAN_POINT('Ctrl Pts',(-7.00387066355044,-0.321593362427602,
68.2412102760513));
#144384=CARTESIAN_POINT('Ctrl Pts',(-7.00864840788313,-0.217540520300971,
68.236476875089));
#144385=CARTESIAN_POINT('Ctrl Pts',(-7.01110433567618,-0.113435852704417,
68.2317434741267));
#144386=CARTESIAN_POINT('Ctrl Pts',(-7.01124370937301,-0.00939203265251101,
68.2270100731644));
#144387=CARTESIAN_POINT('Ctrl Pts',(-7.01153082352607,0.204941474686562,
68.21725911987));
#144388=CARTESIAN_POINT('Ctrl Pts',(-7.00198517742497,0.419142924397046,
68.2075081665757));
#144389=CARTESIAN_POINT('Ctrl Pts',(-6.98267138124,0.632397773645563,68.1977572132813));
#144390=CARTESIAN_POINT('Ctrl Pts',(-6.96332975990841,0.845959856510448,
68.1879922119095));
#144391=CARTESIAN_POINT('Ctrl Pts',(-6.93419184213086,1.05857257252489,
68.1782272105376));
#144392=CARTESIAN_POINT('Ctrl Pts',(-6.89537417949339,1.26942565252004,
68.1684622091658));
#144393=CARTESIAN_POINT('Ctrl Pts',(-6.85662121785671,1.47992728411851,
68.158713484028));
#144394=CARTESIAN_POINT('Ctrl Pts',(-6.80822076379539,1.68867510418824,
68.1489647588902));
#144395=CARTESIAN_POINT('Ctrl Pts',(-6.75033997079495,1.89487119382507,
68.1392160337524));
#144396=CARTESIAN_POINT('Ctrl Pts',(-6.69261803812816,2.10050135514788,
68.1294940650851));
#144397=CARTESIAN_POINT('Ctrl Pts',(-6.62546772170094,2.30359372895432,
68.1197720964178));
#144398=CARTESIAN_POINT('Ctrl Pts',(-6.54910575244425,2.50336581541763,
68.1100501277504));
#144399=CARTESIAN_POINT('Ctrl Pts',(-6.47324905039368,2.70181606216193,
68.1003924868106));
#144400=CARTESIAN_POINT('Ctrl Pts',(-6.38830218448537,2.89698976137551,
68.0907348458707));
#144401=CARTESIAN_POINT('Ctrl Pts',(-6.294528085565,3.08812932736527,68.0810772049308));
#144402=CARTESIAN_POINT('Ctrl Pts',(-6.25331114065465,3.17214174713031,
68.0768323392465));
#144403=CARTESIAN_POINT('Ctrl Pts',(-6.21038951750221,3.2553749391852,68.0725874735622));
#144404=CARTESIAN_POINT('Ctrl Pts',(-6.1657886753124,3.33776520652508,68.0683426078779));
#144405=CARTESIAN_POINT('Ctrl Pts',(-6.08328924762513,3.49016479291883,
68.060490760864));
#144406=CARTESIAN_POINT('Ctrl Pts',(-5.995074925503,3.63961591340362,68.0526389138501));
#144407=CARTESIAN_POINT('Ctrl Pts',(-5.90139775178321,3.78564804726325,
68.0447870668363));
#144408=CARTESIAN_POINT('Ctrl Pts',(-5.80774714415255,3.93163876759031,
68.0369374465428));
#144409=CARTESIAN_POINT('Ctrl Pts',(-5.70863697235295,4.07421210922336,
68.0290878262492));
#144410=CARTESIAN_POINT('Ctrl Pts',(-5.60436413782013,4.21292406449672,
68.0212382059557));
#144411=CARTESIAN_POINT('Ctrl Pts',(-5.50009962813947,4.35162494539464,
68.0133892123539));
#144412=CARTESIAN_POINT('Ctrl Pts',(-5.39067350606146,4.48646474916962,
68.0055402187522));
#144413=CARTESIAN_POINT('Ctrl Pts',(-5.2764245580144,4.61703047922392,67.9976912251504));
#144414=CARTESIAN_POINT('Ctrl Pts',(-5.16211776907036,4.74766231088414,
67.989838257833));
#144415=CARTESIAN_POINT('Ctrl Pts',(-5.04298352713535,4.8740154579152,67.9819852905157));
#144416=CARTESIAN_POINT('Ctrl Pts',(-4.91939950847617,4.99571166486863,
67.9741323231983));
#144417=CARTESIAN_POINT('Ctrl Pts',(-4.79578410362873,5.11743877856957,
67.9662773614911));
#144418=CARTESIAN_POINT('Ctrl Pts',(-4.66771695223548,5.23450633856139,
67.9584223997839));
#144419=CARTESIAN_POINT('Ctrl Pts',(-4.53561028362952,5.34657515775605,
67.9505674380766));
#144420=CARTESIAN_POINT('Ctrl Pts',(-4.40337248811236,5.45875521462144,
67.9427046796633));
#144421=CARTESIAN_POINT('Ctrl Pts',(-4.26708746699851,5.565926385278,67.93484192125));
#144422=CARTESIAN_POINT('Ctrl Pts',(-4.12719846490059,5.66779140352062,
67.9269791628367));
#144423=CARTESIAN_POINT('Ctrl Pts',(-4.02457790024451,5.74251811923086,
67.9212111560883));
#144424=CARTESIAN_POINT('Ctrl Pts',(-3.9200185028237,5.81439022392368,67.9154431493399));
#144425=CARTESIAN_POINT('Ctrl Pts',(-3.81370389557039,5.88330597193544,
67.9096751425916));
#144426=CARTESIAN_POINT('Ctrl Pts',(-3.65928125321348,5.98340653368255,
67.9012970761505));
#144427=CARTESIAN_POINT('Ctrl Pts',(-3.5008126218529,6.07749008693282,67.8929190097095));
#144428=CARTESIAN_POINT('Ctrl Pts',(-3.33879497014616,6.16523111568631,
67.8845409432685));
#144429=CARTESIAN_POINT('Ctrl Pts',(-3.17688810418469,6.25291214816682,
67.8761686056498));
#144430=CARTESIAN_POINT('Ctrl Pts',(-3.01143734429132,6.33425914669018,
67.867796268031));
#144431=CARTESIAN_POINT('Ctrl Pts',(-2.84296662347438,6.40899113280013,
67.8594239304123));
#144432=CARTESIAN_POINT('Ctrl Pts',(-2.67458639459219,6.48368297756102,
67.8510560898897));
#144433=CARTESIAN_POINT('Ctrl Pts',(-2.50318973898364,6.55176676159969,
67.8426882493671));
#144434=CARTESIAN_POINT('Ctrl Pts',(-2.32932346968877,6.61300829698989,
67.8343204088445));
#144435=CARTESIAN_POINT('Ctrl Pts',(-2.15552512033324,6.6742259086979,67.8259558371746));
#144436=CARTESIAN_POINT('Ctrl Pts',(-1.97925939070828,6.72860649283184,
67.8175912655047));
#144437=CARTESIAN_POINT('Ctrl Pts',(-1.80109170179253,6.77596452501296,
67.8092266938348));
#144438=CARTESIAN_POINT('Ctrl Pts',(-1.62296753369368,6.82331098910191,
67.8008641653693));
#144439=CARTESIAN_POINT('Ctrl Pts',(-1.44294265029347,6.86363823819778,
67.7925016369037));
#144440=CARTESIAN_POINT('Ctrl Pts',(-1.26159665607423,6.89681088909087,
67.7841391084381));
#144441=CARTESIAN_POINT('Ctrl Pts',(-1.08023618987751,6.92998618726524,
67.7757759126166));
#144442=CARTESIAN_POINT('Ctrl Pts',(-0.897554724448007,6.95600568145761,
67.7674127167951));
#144443=CARTESIAN_POINT('Ctrl Pts',(-0.714141822617488,6.97478515939298,
67.7590495209736));
#144444=CARTESIAN_POINT('Ctrl Pts',(-0.530716412394702,6.99356591805111,
67.7506857547989));
#144445=CARTESIAN_POINT('Ctrl Pts',(-0.346559793393782,7.00510564218792,
67.7423219886242));
#144446=CARTESIAN_POINT('Ctrl Pts',(-0.162266591864389,7.00937202006462,
67.7339582224495));
#144447=CARTESIAN_POINT('Ctrl Pts',(0.0220637487109107,7.01363925770827,
67.725592770796));
#144448=CARTESIAN_POINT('Ctrl Pts',(0.206530398000816,7.01063021878269,
67.7172273191424));
#144449=CARTESIAN_POINT('Ctrl Pts',(0.390538351783021,7.0003647303756,67.7088618674888));
#144450=CARTESIAN_POINT('Ctrl Pts',(0.574607929467187,6.99009580407662,
67.700493614262));
#144451=CARTESIAN_POINT('Ctrl Pts',(0.758218177186079,6.97256560077398,
67.6921253610351));
#144452=CARTESIAN_POINT('Ctrl Pts',(0.940778399858321,6.94784589386236,
67.6837571078082));
#144453=CARTESIAN_POINT('Ctrl Pts',(1.12350788190187,6.9231032682558,67.6753810960168));
#144454=CARTESIAN_POINT('Ctrl Pts',(1.30518506736229,6.89115786315449,67.6670050842253));
#144455=CARTESIAN_POINT('Ctrl Pts',(1.48522742135716,6.85213295765259,67.6586290724339));
#144456=CARTESIAN_POINT('Ctrl Pts',(1.6653580703472,6.8130889138548,67.6502489529427));
#144457=CARTESIAN_POINT('Ctrl Pts',(1.84385196931342,6.76695852206363,67.6418688334516));
#144458=CARTESIAN_POINT('Ctrl Pts',(2.02014032892689,6.71391537137185,67.6334887139604));
#144459=CARTESIAN_POINT('Ctrl Pts',(2.19663012032212,6.66081161216129,67.6250990191212));
#144460=CARTESIAN_POINT('Ctrl Pts',(2.37090902365704,6.60077941180021,67.616709324282));
#144461=CARTESIAN_POINT('Ctrl Pts',(2.54242559369602,6.53404152596381,67.6083196294428));
#144462=CARTESIAN_POINT('Ctrl Pts',(2.65131850419885,6.49167079392387,67.6029931569681));
#144463=CARTESIAN_POINT('Ctrl Pts',(2.75909838700588,6.44659813077486,67.5976666844934));
#144464=CARTESIAN_POINT('Ctrl Pts',(2.86562898909334,6.39889029905717,67.5923402120187));
#144465=CARTESIAN_POINT('Ctrl Pts',(3.03325681081882,6.32382116630678,67.5839589116137));
#144466=CARTESIAN_POINT('Ctrl Pts',(3.19812844818391,6.24207373701859,67.5755776112088));
#144467=CARTESIAN_POINT('Ctrl Pts',(3.35969339088097,6.15386763602945,67.5671963108038));
#144468=CARTESIAN_POINT('Ctrl Pts',(3.52105357366497,6.06577332336066,67.5588256324701));
#144469=CARTESIAN_POINT('Ctrl Pts',(3.67911512826064,5.97123680741788,67.5504549541365));
#144470=CARTESIAN_POINT('Ctrl Pts',(3.8333480660444,5.87052545919475,67.5420842758028));
#144471=CARTESIAN_POINT('Ctrl Pts',(3.98740597592415,5.76992840106064,67.5337230967519));
#144472=CARTESIAN_POINT('Ctrl Pts',(4.13764365602719,5.66317065516584,67.525361917701));
#144473=CARTESIAN_POINT('Ctrl Pts',(4.28355587359808,5.55056534420265,67.51700073865));
#144474=CARTESIAN_POINT('Ctrl Pts',(4.42927875285473,5.43810615191344,67.5086504092152));
#144475=CARTESIAN_POINT('Ctrl Pts',(4.57068710673427,5.3198147286725,67.5003000797804));
#144476=CARTESIAN_POINT('Ctrl Pts',(4.70730491031947,5.19604725188121,67.4919497503456));
#144477=CARTESIAN_POINT('Ctrl Pts',(4.843817594677,5.07237500675979,67.4836058459898));
#144478=CARTESIAN_POINT('Ctrl Pts',(4.9755468325591,4.94323532386597,67.475261941634));
#144479=CARTESIAN_POINT('Ctrl Pts',(5.10204901725726,4.80902509746043,67.4669180372781));
#144480=CARTESIAN_POINT('Ctrl Pts',(5.22844959461181,4.67492266954565,67.4585808347983));
#144481=CARTESIAN_POINT('Ctrl Pts',(5.34963126781095,4.53575805826245,67.4502436323185));
#144482=CARTESIAN_POINT('Ctrl Pts',(5.46518660247705,4.3919656149161,67.4419064298387));
#144483=CARTESIAN_POINT('Ctrl Pts',(5.50322678079105,4.3446299362916,67.4391618688032));
#144484=CARTESIAN_POINT('Ctrl Pts',(5.5406575368392,4.29679303928106,67.4364173077677));
#144485=CARTESIAN_POINT('Ctrl Pts',(5.57746523610609,4.24847126652965,67.4336727467322));
#144486=CARTESIAN_POINT('Ctrl Pts',(5.68930934225374,4.10164042438266,67.4253331063335));
#144487=CARTESIAN_POINT('Ctrl Pts',(5.79530587865598,3.95045074942612,67.4169934659349));
#144488=CARTESIAN_POINT('Ctrl Pts',(5.89512928401661,3.79540212457519,67.4086538255363));
#144489=CARTESIAN_POINT('Ctrl Pts',(5.9950015738718,3.64027757090143,67.4003101011345));
#144490=CARTESIAN_POINT('Ctrl Pts',(6.08869453208299,3.4812905776173,67.3919663767327));
#144491=CARTESIAN_POINT('Ctrl Pts',(6.17592787990105,3.31896691528567,67.3836226523309));
#144492=CARTESIAN_POINT('Ctrl Pts',(6.26326419102146,3.15645165901962,67.3752690796607));
#144493=CARTESIAN_POINT('Ctrl Pts',(6.34412550537733,2.99059215515047,67.3669155069906));
#144494=CARTESIAN_POINT('Ctrl Pts',(6.41827853250221,2.82193678910802,67.3585619343204));
#144495=CARTESIAN_POINT('Ctrl Pts',(6.47288405162372,2.69774072898136,67.3524104501551));
#144496=CARTESIAN_POINT('Ctrl Pts',(6.52385286119279,2.57202901017231,67.3462589659897));
#144497=CARTESIAN_POINT('Ctrl Pts',(6.57110895151817,2.44502632087627,67.3401074818243));
#144498=CARTESIAN_POINT('Origin',(0.,0.,50.));
#144499=CARTESIAN_POINT('',(6.57110895151811,2.44502632087645,65.3396321383564));
#144500=CARTESIAN_POINT('',(6.57110895151813,2.4450263208764,65.8869025478802));
#144501=CARTESIAN_POINT('',(6.57110895151814,2.44502632087636,50.));
#144502=CARTESIAN_POINT('',(7.01124987764386,0.00130986217660699,67.7735343569348));
#144503=CARTESIAN_POINT('Ctrl Pts',(6.57110895151813,2.44502632087639,65.8869025478802));
#144504=CARTESIAN_POINT('Ctrl Pts',(6.50935958509336,2.61098028668847,65.89492465128));
#144505=CARTESIAN_POINT('Ctrl Pts',(6.44131154789099,2.77461454209502,65.9029467546797));
#144506=CARTESIAN_POINT('Ctrl Pts',(6.36717722856169,2.93541831815935,65.9109688580794));
#144507=CARTESIAN_POINT('Ctrl Pts',(6.29301524881048,3.0962820920807,65.9189939546242));
#144508=CARTESIAN_POINT('Ctrl Pts',(6.21276260144777,3.25431294251536,65.9270190511689));
#144509=CARTESIAN_POINT('Ctrl Pts',(6.12667896086201,3.40902206989494,65.9350441477136));
#144510=CARTESIAN_POINT('Ctrl Pts',(6.04057820932657,3.56376194899547,65.9430708394165));
#144511=CARTESIAN_POINT('Ctrl Pts',(5.94864434153738,3.71517847367931,65.9510975311194));
#144512=CARTESIAN_POINT('Ctrl Pts',(5.85118159661041,3.8628099210274,65.9591242228222));
#144513=CARTESIAN_POINT('Ctrl Pts',(5.75364074662331,4.01055967781855,65.9671573469854));
#144514=CARTESIAN_POINT('Ctrl Pts',(5.65056238001352,4.15451799840591,65.9751904711486));
#144515=CARTESIAN_POINT('Ctrl Pts',(5.5422927899449,4.29425397397788,65.9832235953118));
#144516=CARTESIAN_POINT('Ctrl Pts',(5.47964922627976,4.37510363339291,65.9878714703488));
#144517=CARTESIAN_POINT('Ctrl Pts',(5.41526857342077,4.45454041626961,65.9925193453858));
#144518=CARTESIAN_POINT('Ctrl Pts',(5.34922373629437,4.53248629138191,65.9971672204228));
#144519=CARTESIAN_POINT('Ctrl Pts',(5.21066576797148,4.69601189859992,66.0069181737171));
#144520=CARTESIAN_POINT('Ctrl Pts',(5.06469993486289,4.85307034626018,66.0166691270113));
#144521=CARTESIAN_POINT('Ctrl Pts',(4.91190287584107,5.00308271976431,66.0264200803056));
#144522=CARTESIAN_POINT('Ctrl Pts',(4.75888568398996,5.15331121423581,66.0361850816774));
#144523=CARTESIAN_POINT('Ctrl Pts',(4.59901760757246,5.29647330211476,66.0459500830492));
#144524=CARTESIAN_POINT('Ctrl Pts',(4.43291210196411,5.43202695674093,66.055715084421));
#144525=CARTESIAN_POINT('Ctrl Pts',(4.26708345981833,5.56735467151011,66.0654638095587));
#144526=CARTESIAN_POINT('Ctrl Pts',(4.0950381962377,5.69509927458982,66.0752125346964));
#144527=CARTESIAN_POINT('Ctrl Pts',(3.91742033283823,5.81476091497885,66.0849612598342));
#144528=CARTESIAN_POINT('Ctrl Pts',(3.74028996160147,5.93409413056448,66.0946832285015));
#144529=CARTESIAN_POINT('Ctrl Pts',(3.55761755688491,6.04538864907153,66.1044051971689));
#144530=CARTESIAN_POINT('Ctrl Pts',(3.37007493883061,6.14818847053064,66.1141271658362));
#144531=CARTESIAN_POINT('Ctrl Pts',(3.18377324129821,6.25030809242007,66.123784806776));
#144532=CARTESIAN_POINT('Ctrl Pts',(2.99266559430891,6.34404501232882,66.1334424477159));
#144533=CARTESIAN_POINT('Ctrl Pts',(2.79744289471133,6.42899213044542,66.1431000886557));
#144534=CARTESIAN_POINT('Ctrl Pts',(2.71163579714709,6.46632931340138,66.1473449543402));
#144535=CARTESIAN_POINT('Ctrl Pts',(2.62503412976144,6.50196891497991,66.1515898200247));
#144536=CARTESIAN_POINT('Ctrl Pts',(2.53769853712627,6.53587887717996,66.1558346857093));
#144537=CARTESIAN_POINT('Ctrl Pts',(2.37615144395389,6.59860308454738,66.1636865327232));
#144538=CARTESIAN_POINT('Ctrl Pts',(2.21215820691028,6.65538003626358,66.1715383797372));
#144539=CARTESIAN_POINT('Ctrl Pts',(2.04621555630563,6.70601434979324,66.1793902267511));
#144540=CARTESIAN_POINT('Ctrl Pts',(1.88031996569481,6.75663430384103,66.1872398470447));
#144541=CARTESIAN_POINT('Ctrl Pts',(1.71247642570905,6.80111497362372,66.1950894673383));
#144542=CARTESIAN_POINT('Ctrl Pts',(1.5431986859047,6.83931022679349,66.202939087632));
#144543=CARTESIAN_POINT('Ctrl Pts',(1.3739344607627,6.87750243056084,66.2107880812338));
#144544=CARTESIAN_POINT('Ctrl Pts',(1.20323663601939,6.90941013345104,66.2186370748357));
#144545=CARTESIAN_POINT('Ctrl Pts',(1.03163080196702,6.93493795580991,66.2264860684375));
#144546=CARTESIAN_POINT('Ctrl Pts',(0.859938088906338,6.96047870215765,
66.234339035755));
#144547=CARTESIAN_POINT('Ctrl Pts',(0.687336825839987,6.97963305817717,
66.2421920030724));
#144548=CARTESIAN_POINT('Ctrl Pts',(0.514359746088131,6.99235730023174,
66.2500449703899));
#144549=CARTESIAN_POINT('Ctrl Pts',(0.341338735969675,7.0050847738163,66.2578999320972));
#144550=CARTESIAN_POINT('Ctrl Pts',(0.167942100275611,7.01137886621324,
66.2657548938045));
#144551=CARTESIAN_POINT('Ctrl Pts',(-0.00529639140698661,7.0112479995175,
66.2736098555118));
#144552=CARTESIAN_POINT('Ctrl Pts',(-0.178706836773275,7.01111700292562,
66.2814726139252));
#144553=CARTESIAN_POINT('Ctrl Pts',(-0.351958443592178,7.004548324577,66.2893353723386));
#144554=CARTESIAN_POINT('Ctrl Pts',(-0.524520949046105,6.99160241550618,
66.297198130752));
#144555=CARTESIAN_POINT('Ctrl Pts',(-0.651110326916408,6.98210548237502,
66.3029661374999));
#144556=CARTESIAN_POINT('Ctrl Pts',(-0.777328949270345,6.96917774512625,
66.3087341442478));
#144557=CARTESIAN_POINT('Ctrl Pts',(-0.902971002041689,6.95286055749516,
66.3145021509957));
#144558=CARTESIAN_POINT('Ctrl Pts',(-1.08546688179807,6.92915973881061,
66.3228802174367));
#144559=CARTESIAN_POINT('Ctrl Pts',(-1.26715024106887,6.89825376719719,
66.3312582838777));
#144560=CARTESIAN_POINT('Ctrl Pts',(-1.44743158371718,6.86021635030252,
66.3396363503187));
#144561=CARTESIAN_POINT('Ctrl Pts',(-1.62758965212568,6.82220494294152,
66.3480086879374));
#144562=CARTESIAN_POINT('Ctrl Pts',(-1.80634729462278,6.77707188004004,
66.3563810255562));
#144563=CARTESIAN_POINT('Ctrl Pts',(-1.98312330321772,6.72494226939792,
66.3647533631749));
#144564=CARTESIAN_POINT('Ctrl Pts',(-2.15980435879701,6.67284065952228,
66.3731212036975));
#144565=CARTESIAN_POINT('Ctrl Pts',(-2.33450558821077,6.61375008798852,
66.3814890442201));
#144566=CARTESIAN_POINT('Ctrl Pts',(-2.50665864296525,6.54784613519191,
66.3898568847427));
#144567=CARTESIAN_POINT('Ctrl Pts',(-2.67874444703872,6.48196792742615,
66.3982214564126));
#144568=CARTESIAN_POINT('Ctrl Pts',(-2.84828375495011,6.40928176337826,
66.4065860280825));
#144569=CARTESIAN_POINT('Ctrl Pts',(-3.01472554613026,6.33001235733467,
66.4149505997524));
#144570=CARTESIAN_POINT('Ctrl Pts',(-3.18112668076413,6.25076231433838,
66.423313128218));
#144571=CARTESIAN_POINT('Ctrl Pts',(-3.3444315112613,6.16493237784235,66.4316756566835));
#144572=CARTESIAN_POINT('Ctrl Pts',(-3.50411067349051,6.07279465735751,
66.440038185149));
#144573=CARTESIAN_POINT('Ctrl Pts',(-3.66380257861672,5.98064958399416,
66.4484013809706));
#144574=CARTESIAN_POINT('Ctrl Pts',(-3.81986794971852,5.88219587998925,
66.456764576792));
#144575=CARTESIAN_POINT('Ctrl Pts',(-3.9718029657698,5.77775109913903,66.4651277726135));
#144576=CARTESIAN_POINT('Ctrl Pts',(-4.12374834348467,5.67329919536407,
66.4734915387882));
#144577=CARTESIAN_POINT('Ctrl Pts',(-4.27156253337539,5.56285558612425,
66.4818553049629));
#144578=CARTESIAN_POINT('Ctrl Pts',(-4.41477146026289,5.44678065614435,
66.4902190711376));
#144579=CARTESIAN_POINT('Ctrl Pts',(-4.55800924683019,5.3306823345688,66.4985845227911));
#144580=CARTESIAN_POINT('Ctrl Pts',(-4.69663966440762,5.20895063640654,
66.5069499744447));
#144581=CARTESIAN_POINT('Ctrl Pts',(-4.83022210864495,5.08198592517311,
66.5153154260982));
#144582=CARTESIAN_POINT('Ctrl Pts',(-4.96384928938052,4.95497869370722,
66.523683679325));
#144583=CARTESIAN_POINT('Ctrl Pts',(-5.09242488754069,4.82273518100134,
66.5320519325519));
#144584=CARTESIAN_POINT('Ctrl Pts',(-5.21554521691631,4.68569254783126,
66.5404201857787));
#144585=CARTESIAN_POINT('Ctrl Pts',(-5.33877969640249,4.54852285658876,
66.5487961975702));
#144586=CARTESIAN_POINT('Ctrl Pts',(-5.45654858012949,4.40654539834418,
66.5571722093616));
#144587=CARTESIAN_POINT('Ctrl Pts',(-5.56848774956643,4.26023130186948,
66.5655482211531));
#144588=CARTESIAN_POINT('Ctrl Pts',(-5.68048181535481,4.11384545115451,
66.5739283406442));
#144589=CARTESIAN_POINT('Ctrl Pts',(-5.78664027107147,3.96311898601142,
66.5823084601353));
#144590=CARTESIAN_POINT('Ctrl Pts',(-5.88664204816884,3.8085524755779,66.5906885796264));
#144591=CARTESIAN_POINT('Ctrl Pts',(-5.98675808996436,3.65380935332637,
66.5990782744656));
#144592=CARTESIAN_POINT('Ctrl Pts',(-6.08070322303536,3.49521769780813,
66.6074679693048));
#144593=CARTESIAN_POINT('Ctrl Pts',(-6.16820143086034,3.33330431716525,
66.615857664144));
#144594=CARTESIAN_POINT('Ctrl Pts',(-6.22375253307756,3.2305083058867,66.6211841366189));
#144595=CARTESIAN_POINT('Ctrl Pts',(-6.27670596914462,3.12637386532603,
66.6265106090938));
#144596=CARTESIAN_POINT('Ctrl Pts',(-6.32700113053064,3.02104009519306,
66.6318370815687));
#144597=CARTESIAN_POINT('Ctrl Pts',(-6.40614147312554,2.85529551011944,
66.6402183819735));
#144598=CARTESIAN_POINT('Ctrl Pts',(-6.47885731027143,2.68624609122133,
66.6485996823783));
#144599=CARTESIAN_POINT('Ctrl Pts',(-6.54487131078168,2.51441565533761,
66.6569809827832));
#144600=CARTESIAN_POINT('Ctrl Pts',(-6.61080164821007,2.34280298937716,
66.6653516611167));
#144601=CARTESIAN_POINT('Ctrl Pts',(-6.67004695930758,2.1684166338342,66.6737223394502));
#144602=CARTESIAN_POINT('Ctrl Pts',(-6.72237646680039,1.99180350464306,
66.6820930177837));
#144603=CARTESIAN_POINT('Ctrl Pts',(-6.77464658928657,1.81539080103108,
66.6904541968345));
#144604=CARTESIAN_POINT('Ctrl Pts',(-6.82001645807766,1.63675667261268,
66.6988153758852));
#144605=CARTESIAN_POINT('Ctrl Pts',(-6.8583037852352,1.45646687292523,66.707176554936));
#144606=CARTESIAN_POINT('Ctrl Pts',(-6.89654143006947,1.27641102051942,
66.7155268843706));
#144607=CARTESIAN_POINT('Ctrl Pts',(-6.92771479682103,1.0947041011038,66.7238772138053));
#144608=CARTESIAN_POINT('Ctrl Pts',(-6.95169173340486,0.911925767927725,
66.73222754324));
#144609=CARTESIAN_POINT('Ctrl Pts',(-6.97565022117037,0.729288071744552,
66.7405714475957));
#144610=CARTESIAN_POINT('Ctrl Pts',(-6.992423271009,0.545580928145699,66.7489153519514));
#144611=CARTESIAN_POINT('Ctrl Pts',(-7.00192979954241,0.361394029806848,
66.7572592563071));
#144612=CARTESIAN_POINT('Ctrl Pts',(-7.01142869237278,0.177355071534034,
66.7655964587868));
#144613=CARTESIAN_POINT('Ctrl Pts',(-7.01367268715592,-0.00716254670140126,
66.7739336612664));
#144614=CARTESIAN_POINT('Ctrl Pts',(-7.00863251950259,-0.191564007764597,
66.7822708637461));
#144615=CARTESIAN_POINT('Ctrl Pts',(-7.00697332413204,-0.252267950879734,
66.7850154247824));
#144616=CARTESIAN_POINT('Ctrl Pts',(-7.00452516988018,-0.312959274449869,
66.7877599858186));
#144617=CARTESIAN_POINT('Ctrl Pts',(-7.00128824767291,-0.373616695956113,
66.7905045468549));
#144618=CARTESIAN_POINT('Ctrl Pts',(-6.99145408423809,-0.557901321421504,
66.7988428571569));
#144619=CARTESIAN_POINT('Ctrl Pts',(-6.97434365674271,-0.74172169567443,
66.8071811674588));
#144620=CARTESIAN_POINT('Ctrl Pts',(-6.95003248498663,-0.92448635475627,
66.8155194777608));
#144621=CARTESIAN_POINT('Ctrl Pts',(-6.92570601746616,-1.10736600316041,
66.8238630342447));
#144622=CARTESIAN_POINT('Ctrl Pts',(-6.89416981231439,-1.28918828673419,
66.8322065907285));
#144623=CARTESIAN_POINT('Ctrl Pts',(-6.85555068412153,-1.46937108313076,
66.8405501472124));
#144624=CARTESIAN_POINT('Ctrl Pts',(-6.8169021746639,-1.64969096181517,
66.8489000514378));
#144625=CARTESIAN_POINT('Ctrl Pts',(-6.77116006214231,-1.8283685453243,
66.8572499556632));
#144626=CARTESIAN_POINT('Ctrl Pts',(-6.71850137597255,-2.00483561010748,
66.8655998598885));
#144627=CARTESIAN_POINT('Ctrl Pts',(-6.66576370567079,-2.18156736242755,
66.8739622883523));
#144628=CARTESIAN_POINT('Ctrl Pts',(-6.60608882428118,-2.3560816561386,
66.882324716816));
#144629=CARTESIAN_POINT('Ctrl Pts',(-6.53970290913463,-2.52782760938242,
66.8906871452797));
#144630=CARTESIAN_POINT('Ctrl Pts',(-6.47326022498118,-2.69972042882796,
66.8990567247597));
#144631=CARTESIAN_POINT('Ctrl Pts',(-6.40009518637036,-2.86883988441289,
66.9074263042397));
#144632=CARTESIAN_POINT('Ctrl Pts',(-6.32048077042347,-3.03465803562892,
66.9157958837197));
#144633=CARTESIAN_POINT('Ctrl Pts',(-6.2407435589398,-3.20073194114075,
66.9241783722564));
#144634=CARTESIAN_POINT('Ctrl Pts',(-6.15453724534981,-3.36349407824554,
66.932560860793));
#144635=CARTESIAN_POINT('Ctrl Pts',(-6.06217981160715,-3.52244268856751,
66.9409433493296));
#144636=CARTESIAN_POINT('Ctrl Pts',(-6.03195894592561,-3.57445327838308,
66.9436862369336));
#144637=CARTESIAN_POINT('Ctrl Pts',(-6.00107981223195,-3.62605579681705,
66.9464291245375));
#144638=CARTESIAN_POINT('Ctrl Pts',(-5.96955451152231,-3.67723340250027,
66.9491720121414));
#144639=CARTESIAN_POINT('Ctrl Pts',(-5.87312595003348,-3.83377379340497,
66.9575618672742));
#144640=CARTESIAN_POINT('Ctrl Pts',(-5.7704540065582,-3.98665241824442,
66.965951722407));
#144641=CARTESIAN_POINT('Ctrl Pts',(-5.66184044539661,-4.13535842864572,
66.9743415775398));
#144642=CARTESIAN_POINT('Ctrl Pts',(-5.55332711130674,-4.28392721522512,
66.9827236906319));
#144643=CARTESIAN_POINT('Ctrl Pts',(-5.43888328252094,-4.42833079901718,
66.991105803724));
#144644=CARTESIAN_POINT('Ctrl Pts',(-5.31885462928421,-4.56808625083217,
66.9994879168161));
#144645=CARTESIAN_POINT('Ctrl Pts',(-5.1989190928432,-4.70773328203671,
67.007863527165));
#144646=CARTESIAN_POINT('Ctrl Pts',(-5.07340758332469,-4.84273912197751,
67.0162391375138));
#144647=CARTESIAN_POINT('Ctrl Pts',(-4.94270702263624,-4.97265259704339,
67.0246147478627));
#144648=CARTESIAN_POINT('Ctrl Pts',(-4.81208867454096,-5.10248435460465,
67.0329850898283));
#144649=CARTESIAN_POINT('Ctrl Pts',(-4.67628801592457,-5.22722990298623,
67.0413554317939));
#144650=CARTESIAN_POINT('Ctrl Pts',(-4.5357302285449,-5.34647340368996,
67.0497257737595));
#144651=CARTESIAN_POINT('Ctrl Pts',(-4.39524024990849,-5.46565937821832,
67.0580920776538));
#144652=CARTESIAN_POINT('Ctrl Pts',(-4.2499979692602,-5.57934838595602,
67.066458381548));
#144653=CARTESIAN_POINT('Ctrl Pts',(-4.10046352380986,-5.68716321661378,
67.0748246854423));
#144654=CARTESIAN_POINT('Ctrl Pts',(-3.95097089895209,-5.79494789448573,
67.0831886495159));
#144655=CARTESIAN_POINT('Ctrl Pts',(-3.7971887683768,-5.89686147787002,
67.0915526135896));
#144656=CARTESIAN_POINT('Ctrl Pts',(-3.63960871915088,-5.99256830866207,
67.0999165776632));
#144657=CARTESIAN_POINT('Ctrl Pts',(-3.48205291887605,-6.0882604117632,
67.1082792546617));
#144658=CARTESIAN_POINT('Ctrl Pts',(-3.32070064602507,-6.1777474960226,
67.1166419316602));
#144659=CARTESIAN_POINT('Ctrl Pts',(-3.15607107101373,-6.26073813197855,
67.1250046086588));
#144660=CARTESIAN_POINT('Ctrl Pts',(-2.99144488542432,-6.34372705930905,
67.1333671134851));
#144661=CARTESIAN_POINT('Ctrl Pts',(-2.82354182586683,-6.42021965745362,
67.1417296183114));
#144662=CARTESIAN_POINT('Ctrl Pts',(-2.6529045611805,-6.48997102857692,
67.1500921231377));
#144663=CARTESIAN_POINT('Ctrl Pts',(-2.48224806486999,-6.55973026100858,
67.1584555704577));
#144664=CARTESIAN_POINT('Ctrl Pts',(-2.30885705345781,-6.62274662780782,
67.1668190177777));
#144665=CARTESIAN_POINT('Ctrl Pts',(-2.13329341539538,-6.67882368133272,
67.1751824650977));
#144666=CARTESIAN_POINT('Ctrl Pts',(-1.9576264005297,-6.73493375460244,
67.1835508370505));
#144667=CARTESIAN_POINT('Ctrl Pts',(-1.77978451577,-6.78409624865235,67.1919192090033));
#144668=CARTESIAN_POINT('Ctrl Pts',(-1.60034502805046,-6.82616454194405,
67.2002875809561));
#144669=CARTESIAN_POINT('Ctrl Pts',(-1.42085177557134,-6.86824543999573,
67.2086584602918));
#144670=CARTESIAN_POINT('Ctrl Pts',(-1.23976028690113,-6.90322782899852,
67.2170293396275));
#144671=CARTESIAN_POINT('Ctrl Pts',(-1.05765792792164,-6.93101625088302,
67.2254002189633));
#144672=CARTESIAN_POINT('Ctrl Pts',(-0.875401275582062,-6.95882821759697,
67.2337781908546));
#144673=CARTESIAN_POINT('Ctrl Pts',(-0.692132367456765,-6.9794339932566,
67.2421561627458));
#144674=CARTESIAN_POINT('Ctrl Pts',(-0.508444758336789,-6.99278989318425,
67.2505341346371));
#144675=CARTESIAN_POINT('Ctrl Pts',(-0.391709786965803,-7.00127767634588,
67.2558584039962));
#144676=CARTESIAN_POINT('Ctrl Pts',(-0.274805793216936,-7.00683849559469,
67.2611826733552));
#144677=CARTESIAN_POINT('Ctrl Pts',(-0.157885183101471,-7.00947207936925,
67.2665069427143));
#144678=CARTESIAN_POINT('Ctrl Pts',(0.0147820803068757,-7.01336133125443,
67.2743697739035));
#144679=CARTESIAN_POINT('Ctrl Pts',(0.187844607511428,-7.01087185981264,
67.2822326050927));
#144680=CARTESIAN_POINT('Ctrl Pts',(0.360771993992302,-7.00196187727774,
67.2900954362819));
#144681=CARTESIAN_POINT('Ctrl Pts',(0.533566508602851,-6.99305874088831,
67.2979522259233));
#144682=CARTESIAN_POINT('Ctrl Pts',(0.706225710680853,-6.97774492350471,
67.3058090155646));
#144683=CARTESIAN_POINT('Ctrl Pts',(0.878216694423301,-6.95603062098897,
67.3136658052059));
#144684=CARTESIAN_POINT('Ctrl Pts',(1.05011068339125,-6.93432856431211,
67.3215181639898));
#144685=CARTESIAN_POINT('Ctrl Pts',(1.22133682656196,-6.906233250375,67.3293705227736));
#144686=CARTESIAN_POINT('Ctrl Pts',(1.39136510248672,-6.87180687403845,
67.3372228815574));
#144687=CARTESIAN_POINT('Ctrl Pts',(1.56135323275291,-6.83738862617079,
67.3450733863078));
#144688=CARTESIAN_POINT('Ctrl Pts',(1.73014368366044,-6.79664235836967,
67.3529238910581));
#144689=CARTESIAN_POINT('Ctrl Pts',(1.8972144850932,-6.74968175250156,67.3607743958085));
#144690=CARTESIAN_POINT('Ctrl Pts',(2.06425841009959,-6.70272870111488,
67.3686236376601));
#144691=CARTESIAN_POINT('Ctrl Pts',(2.22958286985326,-6.64956340788821,
67.3764728795116));
#144692=CARTESIAN_POINT('Ctrl Pts',(2.39267942526589,-6.59034989438416,
67.3843221213632));
#144693=CARTESIAN_POINT('Ctrl Pts',(2.55583093110067,-6.5311164306883,67.392174007778));
#144694=CARTESIAN_POINT('Ctrl Pts',(2.71675267432883,-6.46583080672162,
67.4000258941928));
#144695=CARTESIAN_POINT('Ctrl Pts',(2.87495444240738,-6.39470589758295,
67.4078777806076));
#144696=CARTESIAN_POINT('Ctrl Pts',(2.99112003161824,-6.3424797620725,67.413643323072));
#144697=CARTESIAN_POINT('Ctrl Pts',(3.10581943797929,-6.28710623659363,
67.4194088655363));
#144698=CARTESIAN_POINT('Ctrl Pts',(3.21886666312054,-6.2286855730203,67.4251744080006));
#144699=CARTESIAN_POINT('Ctrl Pts',(3.4081819569637,-6.13085101691265,67.4348297123607));
#144700=CARTESIAN_POINT('Ctrl Pts',(3.59276685959877,-6.02452017000506,
67.4444850167208));
#144701=CARTESIAN_POINT('Ctrl Pts',(3.77196215332629,-5.91015465756812,
67.4541403210809));
#144702=CARTESIAN_POINT('Ctrl Pts',(3.95215015535748,-5.79515558165141,
67.4638491140155));
#144703=CARTESIAN_POINT('Ctrl Pts',(4.12688865790131,-5.67203264405174,
67.4735579069501));
#144704=CARTESIAN_POINT('Ctrl Pts',(4.29554450564503,-5.54129262559945,
67.4832666998846));
#144705=CARTESIAN_POINT('Ctrl Pts',(4.4650119396528,-5.40992347507401,67.4930222123554));
#144706=CARTESIAN_POINT('Ctrl Pts',(4.62833801801298,-5.27086380470448,
67.5027777248262));
#144707=CARTESIAN_POINT('Ctrl Pts',(4.78491794614872,-5.1246645559611,67.5125332372969));
#144708=CARTESIAN_POINT('Ctrl Pts',(4.94165291250443,-4.97832054746749,
67.522298409226));
#144709=CARTESIAN_POINT('Ctrl Pts',(5.09162834726075,-4.82482285475868,
67.5320635811551));
#144710=CARTESIAN_POINT('Ctrl Pts',(5.234275407092,-4.66476017874573,67.5418287530842));
#144711=CARTESIAN_POINT('Ctrl Pts',(5.37672797089282,-4.50491574456084,
67.5515806104229));
#144712=CARTESIAN_POINT('Ctrl Pts',(5.51187210511577,-4.33852424567191,
67.5613324677615));
#144713=CARTESIAN_POINT('Ctrl Pts',(5.63917919487846,-4.16620745649445,
67.5710843251002));
#144714=CARTESIAN_POINT('Ctrl Pts',(5.69469430602751,-4.09106485664502,
67.5753368411625));
#144715=CARTESIAN_POINT('Ctrl Pts',(5.74871962059691,-4.01479596185866,
67.5795893572248));
#144716=CARTESIAN_POINT('Ctrl Pts',(5.80121359253968,-3.93745443354369,
67.5838418732872));
#144717=CARTESIAN_POINT('Ctrl Pts',(5.90037523334362,-3.79135550892132,
67.5918749188861));
#144718=CARTESIAN_POINT('Ctrl Pts',(5.99411776632083,-3.64135563124401,
67.5999079644851));
#144719=CARTESIAN_POINT('Ctrl Pts',(6.08211843569535,-3.48790222005646,
67.607941010084));
#144720=CARTESIAN_POINT('Ctrl Pts',(6.17006253485096,-3.33454745463064,
67.6159688917319));
#144721=CARTESIAN_POINT('Ctrl Pts',(6.25227193601276,-3.17774389145165,
67.6239967733799));
#144722=CARTESIAN_POINT('Ctrl Pts',(6.32846709274347,-3.01796799495339,
67.6320246550278));
#144723=CARTESIAN_POINT('Ctrl Pts',(6.40462784661007,-2.85826423884688,
67.640048912008));
#144724=CARTESIAN_POINT('Ctrl Pts',(6.47477960543809,-2.69559115175709,
67.6480731689882));
#144725=CARTESIAN_POINT('Ctrl Pts',(6.53868872578647,-2.53044982360309,
67.6560974259685));
#144726=CARTESIAN_POINT('Ctrl Pts',(6.60259011887134,-2.36532846271748,
67.6641207127343));
#144727=CARTESIAN_POINT('Ctrl Pts',(6.66025023749395,-2.19773979408075,
67.6721439995002));
#144728=CARTESIAN_POINT('Ctrl Pts',(6.71148349589809,-2.02820508006157,
67.680167286266));
#144729=CARTESIAN_POINT('Ctrl Pts',(6.76271255619354,-1.85868425790052,
67.6881899155951));
#144730=CARTESIAN_POINT('Ctrl Pts',(6.80751570303843,-1.68721806011946,
67.6962125449241));
#144731=CARTESIAN_POINT('Ctrl Pts',(6.84575725567681,-1.5143428141766,67.7042351742532));
#144732=CARTESIAN_POINT('Ctrl Pts',(6.88401318441651,-1.34140257944856,
67.7122608195197));
#144733=CARTESIAN_POINT('Ctrl Pts',(6.91570251502456,-1.16705259719756,
67.7202864647862));
#144734=CARTESIAN_POINT('Ctrl Pts',(6.94074064033649,-0.991839667527716,
67.7283121100528));
#144735=CARTESIAN_POINT('Ctrl Pts',(6.95550464476575,-0.888523447264298,
67.7330445195597));
#144736=CARTESIAN_POINT('Ctrl Pts',(6.96795700030494,-0.784907340178289,
67.7377769290667));
#144737=CARTESIAN_POINT('Ctrl Pts',(6.97808881553933,-0.681104283458026,
67.7425093385737));
#144738=CARTESIAN_POINT('Ctrl Pts',(6.99876795306016,-0.46924119324748,
67.752168234313));
#144739=CARTESIAN_POINT('Ctrl Pts',(7.00978401744958,-0.256539865705297,
67.7618271300524));
#144740=CARTESIAN_POINT('Ctrl Pts',(7.01111315913122,-0.0438044787334321,
67.7714860257919));
#144741=CARTESIAN_POINT('Ctrl Pts',(7.01120711473929,-0.0287664410901019,
67.7721688028314));
#144742=CARTESIAN_POINT('Ctrl Pts',(7.01125268710357,-0.0137282329925991,
67.772851579871));
#144743=CARTESIAN_POINT('Ctrl Pts',(7.01124987764396,0.00130986164159499,
67.7735343569105));
#144744=CARTESIAN_POINT('Ctrl Pts',(7.01124987764386,0.00130986217660248,
67.7735343569348));
#144745=CARTESIAN_POINT('Ctrl Pts',(7.01121431270823,0.191676951975715,
67.7821776246599));
#144746=CARTESIAN_POINT('Ctrl Pts',(7.00342123474153,0.382030764535196,
67.7908208923851));
#144747=CARTESIAN_POINT('Ctrl Pts',(6.98789966165083,0.571738472730573,
67.7994641601102));
#144748=CARTESIAN_POINT('Ctrl Pts',(6.97237406338665,0.761495377384949,
67.8081096692739));
#144749=CARTESIAN_POINT('Ctrl Pts',(6.94911598735449,0.950605554743249,
67.8167551784376));
#144750=CARTESIAN_POINT('Ctrl Pts',(6.91820640209675,1.13844048614214,67.8254006876012));
#144751=CARTESIAN_POINT('Ctrl Pts',(6.88729488458905,1.32628715966041,67.8340467372214));
#144752=CARTESIAN_POINT('Ctrl Pts',(6.84873095327239,1.51285814355938,67.8426927868415));
#144753=CARTESIAN_POINT('Ctrl Pts',(6.80264692888082,1.69753389465082,67.8513388364616));
#144754=CARTESIAN_POINT('Ctrl Pts',(6.7565525050491,1.88225132014994,67.8599868371716));
#144755=CARTESIAN_POINT('Ctrl Pts',(6.70293466818401,2.06507237817528,67.8686348378817));
#144756=CARTESIAN_POINT('Ctrl Pts',(6.64197623980495,2.24539043205553,67.8772828385918));
#144757=CARTESIAN_POINT('Ctrl Pts',(6.61936005031205,2.31229024204057,67.8804913337579));
#144758=CARTESIAN_POINT('Ctrl Pts',(6.59573393242823,2.37884567034198,67.8836998289241));
#144759=CARTESIAN_POINT('Ctrl Pts',(6.57110895151815,2.44502632087632,67.8869083240903));
#144760=CARTESIAN_POINT('',(7.0112494081677,0.00288079295883046,67.2264656430621));
#144761=CARTESIAN_POINT('Ctrl Pts',(6.57110895151817,2.44502632087627,67.3401074818243));
#144762=CARTESIAN_POINT('Ctrl Pts',(6.6353893413515,2.27227012539716,67.3317398873517));
#144763=CARTESIAN_POINT('Ctrl Pts',(6.69279811250386,2.09712499354561,67.3233722928791));
#144764=CARTESIAN_POINT('Ctrl Pts',(6.74318804242022,1.92016707269471,67.3150046984065));
#144765=CARTESIAN_POINT('Ctrl Pts',(6.79366014580145,1.74292057741006,67.3066234584648));
#144766=CARTESIAN_POINT('Ctrl Pts',(6.83709045258875,1.56385570257469,67.2982422185232));
#144767=CARTESIAN_POINT('Ctrl Pts',(6.8733827515476,1.38355921927034,67.2898609785815));
#144768=CARTESIAN_POINT('Ctrl Pts',(6.89482537839213,1.27703441032229,67.2849090795362));
#144769=CARTESIAN_POINT('Ctrl Pts',(6.91377724198473,1.1700797930562,67.279957180491));
#144770=CARTESIAN_POINT('Ctrl Pts',(6.93022702928659,1.06281695745107,67.2750052814458));
#144771=CARTESIAN_POINT('Ctrl Pts',(6.97711648270191,0.757068582654123,
67.26089009349));
#144772=CARTESIAN_POINT('Ctrl Pts',(7.0037476227958,0.448352346246154,67.2467749055342));
#144773=CARTESIAN_POINT('Ctrl Pts',(7.00987641219841,0.13877769346808,67.2326597175784));
#144774=CARTESIAN_POINT('Ctrl Pts',(7.01077289755884,0.0934948282978932,
67.2305950260821));
#144775=CARTESIAN_POINT('Ctrl Pts',(7.01123078995113,0.048193640652253,
67.2285303345859));
#144776=CARTESIAN_POINT('Ctrl Pts',(7.01124940816745,0.00288079356271242,
67.2264656430896));
#144777=CARTESIAN_POINT('Ctrl Pts',(7.0112494081677,0.00288079295891919,
67.2264656430621));
#144778=CARTESIAN_POINT('Ctrl Pts',(7.01132401095931,-0.178686846915374,
67.2181924669956));
#144779=CARTESIAN_POINT('Ctrl Pts',(7.00434137349408,-0.360424500685907,
67.2099192909291));
#144780=CARTESIAN_POINT('Ctrl Pts',(6.99028831897533,-0.541752508159516,
67.2016461148625));
#144781=CARTESIAN_POINT('Ctrl Pts',(6.97624724392217,-0.722925943356717,
67.1933799912292));
#144782=CARTESIAN_POINT('Ctrl Pts',(6.95514778939696,-0.903690088920113,
67.1851138675959));
#144783=CARTESIAN_POINT('Ctrl Pts',(6.92702882887233,-1.08346581232248,
67.1768477439626));
#144784=CARTESIAN_POINT('Ctrl Pts',(6.89892893047013,-1.26311966397767,
67.1685872240165));
#144785=CARTESIAN_POINT('Ctrl Pts',(6.86381906325825,-1.44178609232468,
67.1603267040704));
#144786=CARTESIAN_POINT('Ctrl Pts',(6.821789904695,-1.61889130540051,67.1520661841243));
#144787=CARTESIAN_POINT('Ctrl Pts',(6.77978178839405,-1.79590784921733,
67.1438097998791));
#144788=CARTESIAN_POINT('Ctrl Pts',(6.7308613651662,-1.97136440397714,67.1355534156339));
#144789=CARTESIAN_POINT('Ctrl Pts',(6.67517041976566,-2.14469728157275,
67.1272970313887));
#144790=CARTESIAN_POINT('Ctrl Pts',(6.61949475681673,-2.31798259396192,
67.1190429128222));
#144791=CARTESIAN_POINT('Ctrl Pts',(6.5570523783293,-2.4891450653505,67.1107887942558));
#144792=CARTESIAN_POINT('Ctrl Pts',(6.48803506528663,-2.65763570756247,
67.1025346756894));
#144793=CARTESIAN_POINT('Ctrl Pts',(6.41902577227563,-2.82610677062502,
67.0942815162778));
#144794=CARTESIAN_POINT('Ctrl Pts',(6.34344319710818,-2.99190630719308,
67.0860283568662));
#144795=CARTESIAN_POINT('Ctrl Pts',(6.26152754535116,-3.15450461424748,
67.0777751974547));
#144796=CARTESIAN_POINT('Ctrl Pts',(6.17960845368729,-3.31710974933804,
67.0695216914659));
#144797=CARTESIAN_POINT('Ctrl Pts',(6.09135590981829,-3.47651308214818,
67.0612681854771));
#144798=CARTESIAN_POINT('Ctrl Pts',(5.99705654282694,-3.63220860973549,
67.0530146794883));
#144799=CARTESIAN_POINT('Ctrl Pts',(5.90270291679597,-3.78799372318184,
67.0447564245035));
#144800=CARTESIAN_POINT('Ctrl Pts',(5.80229569107786,-3.94006647478785,
67.0364981695188));
#144801=CARTESIAN_POINT('Ctrl Pts',(5.69616588633061,-4.087948233271,67.0282399145341));
#144802=CARTESIAN_POINT('Ctrl Pts',(5.59000606981233,-4.23587181029405,
67.0199793242501));
#144803=CARTESIAN_POINT('Ctrl Pts',(5.47812065295235,-4.37960175772584,
67.0117187339661));
#144804=CARTESIAN_POINT('Ctrl Pts',(5.36088184160279,-4.51869145249745,
67.0034581436821));
#144805=CARTESIAN_POINT('Ctrl Pts',(5.24353078727498,-4.65791431001103,
66.9951896448118));
#144806=CARTESIAN_POINT('Ctrl Pts',(5.12081632178934,-4.79248777969411,
66.9869211459415));
#144807=CARTESIAN_POINT('Ctrl Pts',(4.99314929103177,-4.92200027630728,
66.9786526470712));
#144808=CARTESIAN_POINT('Ctrl Pts',(4.88515921543913,-5.03155138136907,
66.9716585483385));
#144809=CARTESIAN_POINT('Ctrl Pts',(4.77362630084601,-5.13748190703201,
66.9646644496056));
#144810=CARTESIAN_POINT('Ctrl Pts',(4.65881814937934,-5.23956486871894,
66.9576703508729));
#144811=CARTESIAN_POINT('Ctrl Pts',(4.5297497520606,-5.35432748870857,66.9498075196836));
#144812=CARTESIAN_POINT('Ctrl Pts',(4.3962500321622,-5.46448492412578,66.9419446884944));
#144813=CARTESIAN_POINT('Ctrl Pts',(4.2586961446527,-5.56966190266701,66.9340818573052));
#144814=CARTESIAN_POINT('Ctrl Pts',(4.12124794914882,-5.67475806658345,
66.9262250676638));
#144815=CARTESIAN_POINT('Ctrl Pts',(3.97975208176395,-5.7748811537224,66.9183682780225));
#144816=CARTESIAN_POINT('Ctrl Pts',(3.83462126203656,-5.86969388803515,
66.9105114883811));
#144817=CARTESIAN_POINT('Ctrl Pts',(3.68957228922128,-5.964453152454,66.9026591295972));
#144818=CARTESIAN_POINT('Ctrl Pts',(3.54089276006501,-6.05390781348886,
66.8948067708133));
#144819=CARTESIAN_POINT('Ctrl Pts',(3.38902686433104,-6.13776209015489,
66.8869544120294));
#144820=CARTESIAN_POINT('Ctrl Pts',(3.23719682590718,-6.2215965678477,66.879103907279));
#144821=CARTESIAN_POINT('Ctrl Pts',(3.08218224765762,-6.29983310143366,
66.8712534025286));
#144822=CARTESIAN_POINT('Ctrl Pts',(2.92445452040377,-6.37222036032888,
66.8634028977782));
#144823=CARTESIAN_POINT('Ctrl Pts',(2.76675216656987,-6.4445959743957,66.8555536559266));
#144824=CARTESIAN_POINT('Ctrl Pts',(2.60633788060554,-6.51112403054878,
66.847704414075));
#144825=CARTESIAN_POINT('Ctrl Pts',(2.44370533555261,-6.57160032225726,
66.8398551722234));
#144826=CARTESIAN_POINT('Ctrl Pts',(2.28101799641227,-6.63209698961203,
66.8320032858086));
#144827=CARTESIAN_POINT('Ctrl Pts',(2.11611126326507,-6.68653768673339,
66.8241513993938));
#144828=CARTESIAN_POINT('Ctrl Pts',(1.94949655074439,-6.7347672388239,66.816299512979));
#144829=CARTESIAN_POINT('Ctrl Pts',(1.82715344114728,-6.77018159862419,
66.8105339705149));
#144830=CARTESIAN_POINT('Ctrl Pts',(1.70388980937451,-6.80224806435733,
66.8047684280507));
#144831=CARTESIAN_POINT('Ctrl Pts',(1.57991231257096,-6.83092260584811,
66.7990028855866));
#144832=CARTESIAN_POINT('Ctrl Pts',(1.37229256596841,-6.87894261909045,
66.7893475812265));
#144833=CARTESIAN_POINT('Ctrl Pts',(1.16277658245736,-6.91742492590395,
66.7796922768665));
#144834=CARTESIAN_POINT('Ctrl Pts',(0.952165633350585,-6.94629449196952,
66.7700369725065));
#144835=CARTESIAN_POINT('Ctrl Pts',(0.740387939095827,-6.97532399001524,
66.7603281795716));
#144836=CARTESIAN_POINT('Ctrl Pts',(0.52750316800487,-6.99463399454545,
66.7506193866367));
#144837=CARTESIAN_POINT('Ctrl Pts',(0.314321967060732,-7.00420075836802,
66.7409105937018));
#144838=CARTESIAN_POINT('Ctrl Pts',(0.100114920075997,-7.01381355827043,
66.731155081231));
#144839=CARTESIAN_POINT('Ctrl Pts',(-0.11439137222014,-7.01358914327683,
66.7213995687601));
#144840=CARTESIAN_POINT('Ctrl Pts',(-0.328379282896417,-7.00355578324785,
66.7116440562892));
#144841=CARTESIAN_POINT('Ctrl Pts',(-0.542579074524512,-6.99351248864889,
66.7018788843602));
#144842=CARTESIAN_POINT('Ctrl Pts',(-0.756259420085494,-6.97364083502745,
66.6921137124312));
#144843=CARTESIAN_POINT('Ctrl Pts',(-0.968605641946421,-6.94402114576918,
66.6823485405021));
#144844=CARTESIAN_POINT('Ctrl Pts',(-1.18066233455172,-6.91444184228519,
66.6725966831635));
#144845=CARTESIAN_POINT('Ctrl Pts',(-1.39138850150225,-6.8751410728307,
66.6628448258248));
#144846=CARTESIAN_POINT('Ctrl Pts',(-1.59997870808713,-6.82625041264733,
66.6530929684862));
#144847=CARTESIAN_POINT('Ctrl Pts',(-1.69093914496475,-6.8049305439808,
66.6488404524241));
#144848=CARTESIAN_POINT('Ctrl Pts',(-1.78149348873842,-6.78178773194605,
66.644587936362));
#144849=CARTESIAN_POINT('Ctrl Pts',(-1.87157533319683,-6.75683597067956,
66.6403354203));
#144850=CARTESIAN_POINT('Ctrl Pts',(-2.04174084311913,-6.70970184276623,
66.6323023747012));
#144851=CARTESIAN_POINT('Ctrl Pts',(-2.21030233969986,-6.65608610196948,
66.6242693291025));
#144852=CARTESIAN_POINT('Ctrl Pts',(-2.37672416113031,-6.59612074058681,
66.6162362835037));
#144853=CARTESIAN_POINT('Ctrl Pts',(-2.54303900020586,-6.5361939272474,
66.608208401856));
#144854=CARTESIAN_POINT('Ctrl Pts',(-2.70721655860214,-6.46992574194944,
66.6001805202082));
#144855=CARTESIAN_POINT('Ctrl Pts',(-2.86873529756915,-6.39749828878295,
66.5921526385605));
#144856=CARTESIAN_POINT('Ctrl Pts',(-3.03018110923428,-6.32510353732511,
66.5841283815804));
#144857=CARTESIAN_POINT('Ctrl Pts',(-3.18897015798354,-6.24655520490433,
66.5761041246003));
#144858=CARTESIAN_POINT('Ctrl Pts',(-3.34459994239156,-6.16208388354576,
66.5680798676202));
#144859=CARTESIAN_POINT('Ctrl Pts',(-3.50021090957254,-6.07762277563083,
66.5600565808546));
#144860=CARTESIAN_POINT('Ctrl Pts',(-3.65266304760336,-5.98724027321399,
66.552033294089));
#144861=CARTESIAN_POINT('Ctrl Pts',(-3.80147741768659,-5.89121345779619,
66.5440100073233));
#144862=CARTESIAN_POINT('Ctrl Pts',(-3.95027959375968,-5.79519451091931,
66.5359873779945));
#144863=CARTESIAN_POINT('Ctrl Pts',(-4.0954442897418,-5.69353237446911,
66.5279647486656));
#144864=CARTESIAN_POINT('Ctrl Pts',(-4.23652084418538,-5.586547923296,66.5199421193367));
#144865=CARTESIAN_POINT('Ctrl Pts',(-4.37765043336989,-5.4795232535857,
66.5119164740704));
#144866=CARTESIAN_POINT('Ctrl Pts',(-4.51468852043737,-5.36717249623786,
66.5038908288041));
#144867=CARTESIAN_POINT('Ctrl Pts',(-4.64721658537029,-5.24985757627379,
66.4958651835377));
#144868=CARTESIAN_POINT('Ctrl Pts',(-4.72536320832142,-5.18068155064017,
66.4911327740297));
#144869=CARTESIAN_POINT('Ctrl Pts',(-4.80194233615778,-5.10978023901075,
66.4864003645217));
#144870=CARTESIAN_POINT('Ctrl Pts',(-4.87687406826176,-5.0372339517652,
66.4816679550137));
#144871=CARTESIAN_POINT('Ctrl Pts',(-5.01510337395312,-4.90340516341523,
66.472937906179));
#144872=CARTESIAN_POINT('Ctrl Pts',(-5.14779378229524,-4.76390974365538,
66.4642078573442));
#144873=CARTESIAN_POINT('Ctrl Pts',(-5.2745056821904,-4.6192224855533,66.4554778085094));
#144874=CARTESIAN_POINT('Ctrl Pts',(-5.40125422098924,-4.47449339095032,
66.4467452353702));
#144875=CARTESIAN_POINT('Ctrl Pts',(-5.52202062029474,-4.32456966756031,
66.4380126622309));
#144876=CARTESIAN_POINT('Ctrl Pts',(-5.63640499890855,-4.16995986201052,
66.4292800890917));
#144877=CARTESIAN_POINT('Ctrl Pts',(-5.75241439021074,-4.01315357737142,
66.4204234558113));
#144878=CARTESIAN_POINT('Ctrl Pts',(-5.86185887282661,-3.85152728225305,
66.4115668225309));
#144879=CARTESIAN_POINT('Ctrl Pts',(-5.96436600367793,-3.68564305605834,
66.4027101892506));
#144880=CARTESIAN_POINT('Ctrl Pts',(-6.06550159582862,-3.52197834995123,
66.3939720571437));
#144881=CARTESIAN_POINT('Ctrl Pts',(-6.1598841996382,-3.35416919529334,
66.3852339250369));
#144882=CARTESIAN_POINT('Ctrl Pts',(-6.2472013001056,-3.18278219148891,
66.37649579293));
#144883=CARTESIAN_POINT('Ctrl Pts',(-6.33629461179553,-3.00790881997501,
66.3675799090629));
#144884=CARTESIAN_POINT('Ctrl Pts',(-6.41803174922114,-2.82931074057956,
66.3586640251958));
#144885=CARTESIAN_POINT('Ctrl Pts',(-6.49213095549625,-2.64761443929954,
66.3497481413286));
#144886=CARTESIAN_POINT('Ctrl Pts',(-6.56623016177137,-2.46591813801946,
66.3408322574615));
#144887=CARTESIAN_POINT('Ctrl Pts',(-6.63269132833057,-2.28112389717326,
66.3319163735943));
#144888=CARTESIAN_POINT('Ctrl Pts',(-6.69128520431793,-2.09387890695139,
66.3230004897271));
#144889=CARTESIAN_POINT('Ctrl Pts',(-6.74872769583538,-1.9103133281045,
66.314259805231));
#144890=CARTESIAN_POINT('Ctrl Pts',(-6.79861531624834,-1.72437292503407,
66.3055191207349));
#144891=CARTESIAN_POINT('Ctrl Pts',(-6.84077743512908,-1.53668169948391,
66.2967784362388));
#144892=CARTESIAN_POINT('Ctrl Pts',(-6.88293196834461,-1.34902424270155,
66.288039324337));
#144893=CARTESIAN_POINT('Ctrl Pts',(-6.91736371586907,-1.15961685956442,
66.2793002124351));
#144894=CARTESIAN_POINT('Ctrl Pts',(-6.9439528378881,-0.96909522116552,
66.2705611005333));
#144895=CARTESIAN_POINT('Ctrl Pts',(-6.97088646025153,-0.776105100731107,
66.2617087608589));
#144896=CARTESIAN_POINT('Ctrl Pts',(-6.98977275376875,-0.581971929368133,
66.2528564211845));
#144897=CARTESIAN_POINT('Ctrl Pts',(-7.00054105897644,-0.387364742955533,
66.2440040815102));
#144898=CARTESIAN_POINT('Ctrl Pts',(-7.01116618111459,-0.195345192551464,
66.2352694488605));
#144899=CARTESIAN_POINT('Ctrl Pts',(-7.01388785773911,-0.00286443578903975,
66.2265348162108));
#144900=CARTESIAN_POINT('Ctrl Pts',(-7.00869049695713,0.189430938241047,
66.2178001835612));
#144901=CARTESIAN_POINT('Ctrl Pts',(-7.00338807751408,0.385613341740791,
66.2088889903744));
#144902=CARTESIAN_POINT('Ctrl Pts',(-6.98984304867728,0.581602497237557,
66.1999777971877));
#144903=CARTESIAN_POINT('Ctrl Pts',(-6.968094780042,0.776712108088613,66.191066604001));
#144904=CARTESIAN_POINT('Ctrl Pts',(-6.94634651140671,0.971821718939736,
66.1821554108142));
#144905=CARTESIAN_POINT('Ctrl Pts',(-6.91639502316282,1.16605148238852,
66.1732442176275));
#144906=CARTESIAN_POINT('Ctrl Pts',(-6.87833604413355,1.35871992201237,
66.1643330244408));
#144907=CARTESIAN_POINT('Ctrl Pts',(-6.84405908436909,1.53224240005331,
66.1563073595883));
#144908=CARTESIAN_POINT('Ctrl Pts',(-6.80318963512189,1.70457808618064,
66.1482816947359));
#144909=CARTESIAN_POINT('Ctrl Pts',(-6.7558351447834,1.87518480662827,66.1402560298835));
#144910=CARTESIAN_POINT('Ctrl Pts',(-6.70849568359854,2.04573738068782,
66.1322329121802));
#144911=CARTESIAN_POINT('Ctrl Pts',(-6.65467537691532,2.21456172874354,
66.1242097944769));
#144912=CARTESIAN_POINT('Ctrl Pts',(-6.59453233375239,2.38112785494484,
66.1161866767736));
#144913=CARTESIAN_POINT('Ctrl Pts',(-6.53439687515367,2.54767297569959,
66.1081645708557));
#144914=CARTESIAN_POINT('Ctrl Pts',(-6.46794039332366,2.71196009736767,
66.1001424649378));
#144915=CARTESIAN_POINT('Ctrl Pts',(-6.39537020826617,2.8734763722226,66.0921203590199));
#144916=CARTESIAN_POINT('Ctrl Pts',(-6.32277305588252,3.03505266707143,
66.0840952720603));
#144917=CARTESIAN_POINT('Ctrl Pts',(-6.24405780942596,3.19385572226692,
66.0760701851007));
#144918=CARTESIAN_POINT('Ctrl Pts',(-6.15947929163983,3.34939418676873,
66.0680450981411));
#144919=CARTESIAN_POINT('Ctrl Pts',(-6.07488411653789,3.50496328379273,
66.0600184306808));
#144920=CARTESIAN_POINT('Ctrl Pts',(-5.9844235525224,3.65726619144901,66.0519917632205));
#144921=CARTESIAN_POINT('Ctrl Pts',(-5.8883972550324,3.8058381901267,66.0439650957602));
#144922=CARTESIAN_POINT('Ctrl Pts',(-5.79229386796916,3.9545294618814,66.0359319845196));
#144923=CARTESIAN_POINT('Ctrl Pts',(-5.69061603016253,4.09948353981285,
66.0278988732789));
#144924=CARTESIAN_POINT('Ctrl Pts',(-5.5837057600017,4.24026609403512,66.0198657620383));
#144925=CARTESIAN_POINT('Ctrl Pts',(-5.52071034510035,4.32322028918178,
66.0151323610769));
#144926=CARTESIAN_POINT('Ctrl Pts',(-5.4558990038931,4.40472675176677,66.0103989601156));
#144927=CARTESIAN_POINT('Ctrl Pts',(-5.38934796350171,4.48470234138231,
66.0056655591543));
#144928=CARTESIAN_POINT('Ctrl Pts',(-5.25225074908404,4.64945454500257,
65.9959146058604));
#144929=CARTESIAN_POINT('Ctrl Pts',(-5.10768840989514,4.80780577013776,
65.9861636525664));
#144930=CARTESIAN_POINT('Ctrl Pts',(-4.95623241002525,4.9591719934194,65.9764126992725));
#144931=CARTESIAN_POINT('Ctrl Pts',(-4.80455820937429,5.11075628814208,
65.9666476979011));
#144932=CARTESIAN_POINT('Ctrl Pts',(-4.64597050922282,5.25533542432872,
65.9568826965296));
#144933=CARTESIAN_POINT('Ctrl Pts',(-4.48107791698386,5.3923619374463,65.9471176951582));
#144934=CARTESIAN_POINT('Ctrl Pts',(-4.31646016653066,5.5291600557582,65.9373689700207));
#144935=CARTESIAN_POINT('Ctrl Pts',(-4.1455585562666,5.65843068638659,65.9276202448833));
#144936=CARTESIAN_POINT('Ctrl Pts',(-3.96901263396953,5.77966826676846,
65.9178715197458));
#144937=CARTESIAN_POINT('Ctrl Pts',(-3.79295126177409,5.90057309700163,
65.9081495510788));
#144938=CARTESIAN_POINT('Ctrl Pts',(-3.61127653660829,6.01348886882795,
65.8984275824118));
#144939=CARTESIAN_POINT('Ctrl Pts',(-3.42465619391963,6.11795362159177,
65.8887056137449));
#144940=CARTESIAN_POINT('Ctrl Pts',(-3.23927066929506,6.22172715837178,
65.8790479728053));
#144941=CARTESIAN_POINT('Ctrl Pts',(-3.04900478516365,6.31716109481636,
65.8693903318656));
#144942=CARTESIAN_POINT('Ctrl Pts',(-2.85454578810235,6.40384219872157,
65.8597326909261));
#144943=CARTESIAN_POINT('Ctrl Pts',(-2.7690743640634,6.44194152814324,65.85548782524));
#144944=CARTESIAN_POINT('Ctrl Pts',(-2.68279329434385,6.47835041454282,
65.851242959554));
#144945=CARTESIAN_POINT('Ctrl Pts',(-2.5957629358197,6.51303626149315,65.846998093868));
#144946=CARTESIAN_POINT('Ctrl Pts',(-2.43478044279259,6.57719564460395,
65.839146246854));
#144947=CARTESIAN_POINT('Ctrl Pts',(-2.27129897621767,6.63542977659541,
65.8312943998401));
#144948=CARTESIAN_POINT('Ctrl Pts',(-2.10581350796261,6.68753886210631,
65.8234425528261));
#144949=CARTESIAN_POINT('Ctrl Pts',(-1.94037497004867,6.73963316990179,
65.8155929325325));
#144950=CARTESIAN_POINT('Ctrl Pts',(-1.77293392443038,6.7856057719751,65.8077433122389));
#144951=CARTESIAN_POINT('Ctrl Pts',(-1.60400279984087,6.8253059697425,65.7998936919453));
#144952=CARTESIAN_POINT('Ctrl Pts',(-1.43508516224169,6.86500299795673,
65.7920446983435));
#144953=CARTESIAN_POINT('Ctrl Pts',(-1.26467805401425,6.89842853222309,
65.7841957047417));
#144954=CARTESIAN_POINT('Ctrl Pts',(-1.09330619582332,6.92548251926711,
65.7763467111399));
#144955=CARTESIAN_POINT('Ctrl Pts',(-0.921847577077617,6.95255020295276,
65.7684937438224));
#144956=CARTESIAN_POINT('Ctrl Pts',(-0.749423609760433,6.97323983468869,
65.760640776505));
#144957=CARTESIAN_POINT('Ctrl Pts',(-0.576566616985063,6.98750295160427,
65.7527878091875));
#144958=CARTESIAN_POINT('Ctrl Pts',(-0.403665724341947,7.00176969087227,
65.7449328474802));
#144959=CARTESIAN_POINT('Ctrl Pts',(-0.230331968266925,7.00960664652595,
65.7370778857729));
#144960=CARTESIAN_POINT('Ctrl Pts',(-0.0570991721608681,7.01101749013926,
65.7292229240656));
#144961=CARTESIAN_POINT('Ctrl Pts',(0.116305571975743,7.01242973413278,
65.7213601656523));
#144962=CARTESIAN_POINT('Ctrl Pts',(0.289608774858064,7.00740313774478,
65.7134974072389));
#144963=CARTESIAN_POINT('Ctrl Pts',(0.462279656693552,6.99599343063637,
65.7056346488255));
#144964=CARTESIAN_POINT('Ctrl Pts',(0.588948537924436,6.98762343322146,
65.6998666420775));
#144965=CARTESIAN_POINT('Ctrl Pts',(0.715277210151469,6.97581946807508,
65.6940986353295));
#144966=CARTESIAN_POINT('Ctrl Pts',(0.841059499438371,6.96062105568925,
65.6883306285815));
#144967=CARTESIAN_POINT('Ctrl Pts',(1.02375907362194,6.93854526515546,65.6799525621405));
#144968=CARTESIAN_POINT('Ctrl Pts',(1.20571028047177,6.90925737613356,65.6715744956995));
#144969=CARTESIAN_POINT('Ctrl Pts',(1.38632299124672,6.8728258472364,65.6631964292585));
#144970=CARTESIAN_POINT('Ctrl Pts',(1.56681220119583,6.83641922978588,65.6548240916397));
#144971=CARTESIAN_POINT('Ctrl Pts',(1.74596441859612,6.79287877596949,65.646451754021));
#144972=CARTESIAN_POINT('Ctrl Pts',(1.92319734509794,6.74232441627576,65.6380794164023));
#144973=CARTESIAN_POINT('Ctrl Pts',(2.10033507315695,6.69179721122206,65.6297115758797));
#144974=CARTESIAN_POINT('Ctrl Pts',(2.27555525047154,6.63426370216071,65.6213437353571));
#144975=CARTESIAN_POINT('Ctrl Pts',(2.44828798850789,6.56989440461778,65.6129758948345));
#144976=CARTESIAN_POINT('Ctrl Pts',(2.62095324941255,6.50555025260092,65.6046113231646));
#144977=CARTESIAN_POINT('Ctrl Pts',(2.79113270119106,6.4343757518059,65.5962467514946));
#144978=CARTESIAN_POINT('Ctrl Pts',(2.95827334528979,6.35659070391102,65.5878821798247));
#144979=CARTESIAN_POINT('Ctrl Pts',(3.12537316213467,6.27882465648077,65.5795196513592));
#144980=CARTESIAN_POINT('Ctrl Pts',(3.28943535404691,6.19445142110524,65.5711571228936));
#144981=CARTESIAN_POINT('Ctrl Pts',(3.44992815626778,6.10373838553806,65.5627945944281));
#144982=CARTESIAN_POINT('Ctrl Pts',(3.61043376631636,6.01301811078685,65.5544313986066));
#144983=CARTESIAN_POINT('Ctrl Pts',(3.76736912848605,5.91595718152013,65.5460682027851));
#144984=CARTESIAN_POINT('Ctrl Pts',(3.92022761568842,5.81286865529352,65.5377050069636));
#144985=CARTESIAN_POINT('Ctrl Pts',(4.07309652753306,5.70977309863617,65.5293412407889));
#144986=CARTESIAN_POINT('Ctrl Pts',(4.22188773726402,5.60064930901317,65.5209774746142));
#144987=CARTESIAN_POINT('Ctrl Pts',(4.36612398129579,5.4858534379305,65.5126137084395));
#144988=CARTESIAN_POINT('Ctrl Pts',(4.51038929203538,5.37103443300884,65.5042482567859));
#144989=CARTESIAN_POINT('Ctrl Pts',(4.65009754946804,5.25054127212033,65.4958828051323));
#144990=CARTESIAN_POINT('Ctrl Pts',(4.78480460372754,5.12477038184617,65.4875173534787));
#144991=CARTESIAN_POINT('Ctrl Pts',(4.91955677111448,4.99895737114831,65.4791491002518));
#144992=CARTESIAN_POINT('Ctrl Pts',(5.04930415532039,4.8678633309057,65.4707808470249));
#144993=CARTESIAN_POINT('Ctrl Pts',(5.17363919568747,4.73192181204913,65.462412593798));
#144994=CARTESIAN_POINT('Ctrl Pts',(5.29808951237505,4.59585425601068,65.4540365820066));
#144995=CARTESIAN_POINT('Ctrl Pts',(5.41711723560646,4.45493048325975,65.4456605702151));
#144996=CARTESIAN_POINT('Ctrl Pts',(5.53035406854319,4.30961836350364,65.4372845584236));
#144997=CARTESIAN_POINT('Ctrl Pts',(5.6436464342218,4.16423498088871,65.4289044389325));
#144998=CARTESIAN_POINT('Ctrl Pts',(5.75114204944297,4.01445922275958,65.4205243194413));
#144999=CARTESIAN_POINT('Ctrl Pts',(5.85251540364741,3.86078878113913,65.4121441999502));
#145000=CARTESIAN_POINT('Ctrl Pts',(5.95400458975026,3.70694275157331,65.403754505111));
#145001=CARTESIAN_POINT('Ctrl Pts',(6.04935736083194,3.54919342423773,65.3953648102718));
#145002=CARTESIAN_POINT('Ctrl Pts',(6.13829302306579,3.38806513005312,65.3869751154326));
#145003=CARTESIAN_POINT('Ctrl Pts',(6.19475674027863,3.2857675566241,65.381648642958));
#145004=CARTESIAN_POINT('Ctrl Pts',(6.24863480532168,3.18210848944696,65.3763221704833));
#145005=CARTESIAN_POINT('Ctrl Pts',(6.29986537417107,3.07722648334834,65.3709956980087));
#145006=CARTESIAN_POINT('Ctrl Pts',(6.38141373562198,2.91027624377222,65.3625170667466));
#145007=CARTESIAN_POINT('Ctrl Pts',(6.45641141732215,2.73989902163659,65.3540384354846));
#145008=CARTESIAN_POINT('Ctrl Pts',(6.52457226502016,2.56662878520243,65.3455598042225));
#145009=CARTESIAN_POINT('Ctrl Pts',(6.54045669722058,2.52624930906705,65.3435839156005));
#145010=CARTESIAN_POINT('Ctrl Pts',(6.55597001641838,2.48571283255154,65.3416080269784));
#145011=CARTESIAN_POINT('Ctrl Pts',(6.57110895151811,2.44502632087645,65.3396321383564));
#145012=CARTESIAN_POINT('Origin',(0.,0.,50.));
#145013=CARTESIAN_POINT('',(6.57110895151814,2.44502632087636,63.3399907370491));
#145014=CARTESIAN_POINT('',(6.57110895151817,2.44502632087628,63.8871110093167));
#145015=CARTESIAN_POINT('',(6.57110895151814,2.44502632087636,50.));
#145016=CARTESIAN_POINT('',(7.01124989960866,-0.00118648116582599,65.7735343569499));
#145017=CARTESIAN_POINT('Ctrl Pts',(6.57110895151817,2.44502632087628,63.8871110093167));
#145018=CARTESIAN_POINT('Ctrl Pts',(6.49699556480479,2.64420910050587,63.8967749832153));
#145019=CARTESIAN_POINT('Ctrl Pts',(6.41376271381867,2.84017939726017,63.9064389571139));
#145020=CARTESIAN_POINT('Ctrl Pts',(6.32167067777122,3.03217849149875,63.9161029310125));
#145021=CARTESIAN_POINT('Ctrl Pts',(6.26326411714714,3.15394805180726,63.9222320112414));
#145022=CARTESIAN_POINT('Ctrl Pts',(6.2012950942145,3.27412045456893,63.9283610914703));
#145023=CARTESIAN_POINT('Ctrl Pts',(6.13584066416528,3.39250437088529,63.9344901716992));
#145024=CARTESIAN_POINT('Ctrl Pts',(6.05198825043598,3.54416373332095,63.9423420187132));
#145025=CARTESIAN_POINT('Ctrl Pts',(5.96244740792769,3.69282388792006,63.9501938657272));
#145026=CARTESIAN_POINT('Ctrl Pts',(5.86747435681217,3.83801657560928,63.9580457127412));
#145027=CARTESIAN_POINT('Ctrl Pts',(5.77252823928607,3.9831680878262,63.9658953330348));
#145028=CARTESIAN_POINT('Ctrl Pts',(5.67215318614176,4.12485377025659,63.9737449533285));
#145029=CARTESIAN_POINT('Ctrl Pts',(5.56665003842499,4.26263227503887,63.9815945736221));
#145030=CARTESIAN_POINT('Ctrl Pts',(5.46115531378514,4.40039977996978,63.989443567224));
#145031=CARTESIAN_POINT('Ctrl Pts',(5.3505335421151,4.53426042582434,63.9972925608259));
#145032=CARTESIAN_POINT('Ctrl Pts',(5.23512717181703,4.6638042473289,64.0051415544278));
#145033=CARTESIAN_POINT('Ctrl Pts',(5.11966237465312,4.79341365307686,64.0129945217452));
#145034=CARTESIAN_POINT('Ctrl Pts',(4.99940839305648,4.91870158257157,64.0208474890627));
#145035=CARTESIAN_POINT('Ctrl Pts',(4.87474625455506,5.03929315640611,64.0287004563802));
#145036=CARTESIAN_POINT('Ctrl Pts',(4.75005245605922,5.15991535644842,64.0365554180875));
#145037=CARTESIAN_POINT('Ctrl Pts',(4.62094855417452,5.27583856977249,64.0444103797949));
#145038=CARTESIAN_POINT('Ctrl Pts',(4.48784978044503,5.38672729128359,64.0522653415022));
#145039=CARTESIAN_POINT('Ctrl Pts',(4.35461889505698,5.49772607911991,64.0601280999156));
#145040=CARTESIAN_POINT('Ctrl Pts',(4.21738552003268,5.60368016153394,64.067990858329));
#145041=CARTESIAN_POINT('Ctrl Pts',(4.07659552790009,5.70429622866879,64.0758536167424));
#145042=CARTESIAN_POINT('Ctrl Pts',(3.97331400989568,5.77810673175863,64.0816216234902));
#145043=CARTESIAN_POINT('Ctrl Pts',(3.86811914000701,5.8490454825764,64.0873896302379));
#145044=CARTESIAN_POINT('Ctrl Pts',(3.76119543936221,5.91701237360722,64.0931576369857));
#145045=CARTESIAN_POINT('Ctrl Pts',(3.60588808496837,6.01573471457292,64.1015357034267));
#145046=CARTESIAN_POINT('Ctrl Pts',(3.44658844908732,6.10840427875473,64.1099137698677));
#145047=CARTESIAN_POINT('Ctrl Pts',(3.28379637756845,6.19469998572718,64.1182918363087));
#145048=CARTESIAN_POINT('Ctrl Pts',(3.12111562133356,6.28093668472069,64.1266641739275));
#145049=CARTESIAN_POINT('Ctrl Pts',(2.95494748011205,6.36080806232983,64.1350365115462));
#145050=CARTESIAN_POINT('Ctrl Pts',(2.78581836668239,6.43403781387358,64.143408849165));
#145051=CARTESIAN_POINT('Ctrl Pts',(2.61678009883506,6.50722823097462,64.1517766896876));
#145052=CARTESIAN_POINT('Ctrl Pts',(2.4447843309715,6.57378400487815,64.1601445302101));
#145053=CARTESIAN_POINT('Ctrl Pts',(2.27037993859189,6.63347582319703,64.1685123707327));
#145054=CARTESIAN_POINT('Ctrl Pts',(2.09604367636636,6.69314432322258,64.1768769424027));
#145055=CARTESIAN_POINT('Ctrl Pts',(1.9193009764892,6.74595410840701,64.1852415140726));
#145056=CARTESIAN_POINT('Ctrl Pts',(1.74071888858968,6.79172469358168,64.1936060857425));
#145057=CARTESIAN_POINT('Ctrl Pts',(1.56218042273221,6.83748409842793,64.2019686142081));
#145058=CARTESIAN_POINT('Ctrl Pts',(1.38180378309591,6.8762076511627,64.2103311426736));
#145059=CARTESIAN_POINT('Ctrl Pts',(1.20016975602968,6.90776513202437,64.2186936711392));
#145060=CARTESIAN_POINT('Ctrl Pts',(1.01852123399991,6.93932513127173,64.2270568669607));
#145061=CARTESIAN_POINT('Ctrl Pts',(0.835615446852659,6.96371785390755,
64.2354200627822));
#145062=CARTESIAN_POINT('Ctrl Pts',(0.652042683505307,6.98086433770111,
64.2437832586038));
#145063=CARTESIAN_POINT('Ctrl Pts',(0.468457400863388,6.99801199085052,
64.2521470247785));
#145064=CARTESIAN_POINT('Ctrl Pts',(0.284205378697097,7.00791238895935,
64.2605107909532));
#145065=CARTESIAN_POINT('Ctrl Pts',(0.0998815072616129,7.01053851333884,
64.2688745571279));
#145066=CARTESIAN_POINT('Ctrl Pts',(-0.0844795094002239,7.01316516693891,
64.2772400087814));
#145067=CARTESIAN_POINT('Ctrl Pts',(-0.268912075450465,7.00851461905334,
64.285605460435));
#145068=CARTESIAN_POINT('Ctrl Pts',(-0.452821386676459,6.99661199111888,
64.2939709120886));
#145069=CARTESIAN_POINT('Ctrl Pts',(-0.636792288769149,6.98470537701773,
64.3023391653154));
#145070=CARTESIAN_POINT('Ctrl Pts',(-0.820239258643475,6.96554186118294,
64.3107074185423));
#145071=CARTESIAN_POINT('Ctrl Pts',(-1.00257226334398,6.93919847095278,
64.3190756717692));
#145072=CARTESIAN_POINT('Ctrl Pts',(-1.18507431675252,6.91283065664157,
64.3274516835606));
#145073=CARTESIAN_POINT('Ctrl Pts',(-1.36646001539432,6.87926971279002,
64.3358276953521));
#145074=CARTESIAN_POINT('Ctrl Pts',(-1.54614794455558,6.838644097776,64.3442037071436));
#145075=CARTESIAN_POINT('Ctrl Pts',(-1.7259239948975,6.79799855945842,64.3525838266348));
#145076=CARTESIAN_POINT('Ctrl Pts',(-1.90400029633763,6.75028151973062,
64.3609639461259));
#145077=CARTESIAN_POINT('Ctrl Pts',(-2.07980962689622,6.6956716226507,64.3693440656171));
#145078=CARTESIAN_POINT('Ctrl Pts',(-2.25581984188537,6.64099932684573,
64.3777337604563));
#145079=CARTESIAN_POINT('Ctrl Pts',(-2.42955759793582,6.57941853965959,
64.3861234552955));
#145080=CARTESIAN_POINT('Ctrl Pts',(-2.60047345402352,6.51115691543515,
64.3945131501347));
#145081=CARTESIAN_POINT('Ctrl Pts',(-2.70898498160349,6.46781878818801,
64.3998396226093));
#145082=CARTESIAN_POINT('Ctrl Pts',(-2.81635948020824,6.42178874201956,
64.405166095084));
#145083=CARTESIAN_POINT('Ctrl Pts',(-2.92246129635095,6.37313474938595,
64.4104925675586));
#145084=CARTESIAN_POINT('Ctrl Pts',(-3.08941441566581,6.29657681538813,
64.4188738679634));
#145085=CARTESIAN_POINT('Ctrl Pts',(-3.25355202745307,6.21336537748386,
64.4272551683682));
#145086=CARTESIAN_POINT('Ctrl Pts',(-3.41432559771735,6.1237249509814,64.435636468773));
#145087=CARTESIAN_POINT('Ctrl Pts',(-3.57489541101686,6.03419813059712,
64.4440071471065));
#145088=CARTESIAN_POINT('Ctrl Pts',(-3.73210939551151,5.9382587176033,64.45237782544));
#145089=CARTESIAN_POINT('Ctrl Pts',(-3.88543996298573,5.83617878894517,
64.4607485037735));
#145090=CARTESIAN_POINT('Ctrl Pts',(-4.03859652659142,5.73421470347981,
64.4691096828242));
#145091=CARTESIAN_POINT('Ctrl Pts',(-4.18787818575637,5.62612417167076,
64.4774708618749));
#145092=CARTESIAN_POINT('Ctrl Pts',(-4.33278251431195,5.51222480003969,
64.4858320409257));
#145093=CARTESIAN_POINT('Ctrl Pts',(-4.47749881240839,5.39847322627882,
64.4941823703603));
#145094=CARTESIAN_POINT('Ctrl Pts',(-4.61784885308061,5.27892804887209,
64.502532699795));
#145095=CARTESIAN_POINT('Ctrl Pts',(-4.75335979999926,5.15394966741537,
64.5108830292296));
#145096=CARTESIAN_POINT('Ctrl Pts',(-4.88876647935039,5.0290674493471,64.5192269335852));
#145097=CARTESIAN_POINT('Ctrl Pts',(-5.01934124516012,4.89876057944643,
64.5275708379409));
#145098=CARTESIAN_POINT('Ctrl Pts',(-5.14464404037652,4.76342988405606,
64.5359147422965));
#145099=CARTESIAN_POINT('Ctrl Pts',(-5.26984619160639,4.62820788712418,
64.5442519447762));
#145100=CARTESIAN_POINT('Ctrl Pts',(-5.38978459534836,4.48797035199404,
64.5525891472558));
#145101=CARTESIAN_POINT('Ctrl Pts',(-5.50405569879128,4.3431552386604,64.5609263497354));
#145102=CARTESIAN_POINT('Ctrl Pts',(-5.54167311528961,4.29548290270325,
64.5636709107719));
#145103=CARTESIAN_POINT('Ctrl Pts',(-5.5786766731508,4.24731479165283,64.5664154718084));
#145104=CARTESIAN_POINT('Ctrl Pts',(-5.61505288383781,4.19866736884511,
64.5691600328449));
#145105=CARTESIAN_POINT('Ctrl Pts',(-5.72556823703457,4.05087058044496,
64.5774983431469));
#145106=CARTESIAN_POINT('Ctrl Pts',(-5.83019934000538,3.89876854557725,
64.5858366534489));
#145107=CARTESIAN_POINT('Ctrl Pts',(-5.92862524299052,3.74286378200912,
64.5941749637509));
#145108=CARTESIAN_POINT('Ctrl Pts',(-6.02711307221399,3.58686092845398,
64.6025185202348));
#145109=CARTESIAN_POINT('Ctrl Pts',(-6.11938773932444,3.42705085102124,
64.6108620767187));
#145110=CARTESIAN_POINT('Ctrl Pts',(-6.20517366433518,3.26396175803901,
64.6192056332026));
#145111=CARTESIAN_POINT('Ctrl Pts',(-6.29102485490372,3.10074858758575,
64.6275555374279));
#145112=CARTESIAN_POINT('Ctrl Pts',(-6.3703773040939,2.93425171520219,64.6359054416531));
#145113=CARTESIAN_POINT('Ctrl Pts',(-6.44300289214442,2.76502084880361,
64.6442553458784));
#145114=CARTESIAN_POINT('Ctrl Pts',(-6.5157374132027,2.59553614862856,64.6526177743421));
#145115=CARTESIAN_POINT('Ctrl Pts',(-6.58172478121225,2.4233095611296,64.6609802028059));
#145116=CARTESIAN_POINT('Ctrl Pts',(-6.64078572321868,2.24890896676476,
64.6693426312696));
#145117=CARTESIAN_POINT('Ctrl Pts',(-6.69989717038178,2.07435923611729,
64.6777122107497));
#145118=CARTESIAN_POINT('Ctrl Pts',(-6.75207028099807,1.89763210276973,
64.6860817902297));
#145119=CARTESIAN_POINT('Ctrl Pts',(-6.79717641354589,1.71930781584782,
64.6944513697098));
#145120=CARTESIAN_POINT('Ctrl Pts',(-6.84235211680747,1.54070848544023,
64.7028338582464));
#145121=CARTESIAN_POINT('Ctrl Pts',(-6.88043899302143,1.36050739876751,
64.711216346783));
#145122=CARTESIAN_POINT('Ctrl Pts',(-6.91135973018643,1.17929353532417,
64.7195988353197));
#145123=CARTESIAN_POINT('Ctrl Pts',(-6.92147750205127,1.11999738985123,
64.7223417229236));
#145124=CARTESIAN_POINT('Ctrl Pts',(-6.93082840628621,1.06059283281779,
64.7250846105275));
#145125=CARTESIAN_POINT('Ctrl Pts',(-6.9394109443965,1.00110054804204,64.7278274981314));
#145126=CARTESIAN_POINT('Ctrl Pts',(-6.96566293201509,0.819127487944456,
64.7362173532642));
#145127=CARTESIAN_POINT('Ctrl Pts',(-6.98477516963699,0.635966017425455,
64.744607208397));
#145128=CARTESIAN_POINT('Ctrl Pts',(-6.99665206940565,0.452201705195453,
64.7529970635297));
#145129=CARTESIAN_POINT('Ctrl Pts',(-7.0085180093377,0.268606968096569,
64.7613791766218));
#145130=CARTESIAN_POINT('Ctrl Pts',(-7.01316190024731,0.0844108247160268,
64.7697612897139));
#145131=CARTESIAN_POINT('Ctrl Pts',(-7.0105397529384,-0.0997944636261545,
64.778143402806));
#145132=CARTESIAN_POINT('Ctrl Pts',(-7.00791963986005,-0.283856847705757,
64.7865190131549));
#145133=CARTESIAN_POINT('Ctrl Pts',(-6.99804473149794,-0.467928035088668,
64.7948946235037));
#145134=CARTESIAN_POINT('Ctrl Pts',(-6.98092305719585,-0.651413718009799,
64.8032702338526));
#145135=CARTESIAN_POINT('Ctrl Pts',(-6.96381215268117,-0.834783985711531,
64.8116405758181));
#145136=CARTESIAN_POINT('Ctrl Pts',(-6.93946360157776,-1.01756915682932,
64.8200109177837));
#145137=CARTESIAN_POINT('Ctrl Pts',(-6.90793744792476,-1.19917754234256,
64.8283812597493));
#145138=CARTESIAN_POINT('Ctrl Pts',(-6.87642650331046,-1.38069831523444,
64.8367475636436));
#145139=CARTESIAN_POINT('Ctrl Pts',(-6.83774491738015,-1.5610431113291,
64.8451138675379));
#145140=CARTESIAN_POINT('Ctrl Pts',(-6.79200432150243,-1.73962750587371,
64.8534801714322));
#145141=CARTESIAN_POINT('Ctrl Pts',(-6.74627651798734,-1.91816195536857,
64.8618441355058));
#145142=CARTESIAN_POINT('Ctrl Pts',(-6.69349372114037,-2.09493666656742,
64.8702080995794));
#145143=CARTESIAN_POINT('Ctrl Pts',(-6.63381833132686,-2.26937896999415,
64.878572063653));
#145144=CARTESIAN_POINT('Ctrl Pts',(-6.57415212456416,-2.44379442964924,
64.8869347406516));
#145145=CARTESIAN_POINT('Ctrl Pts',(-6.507595545918,-2.61587788626935,64.8952974176501));
#145146=CARTESIAN_POINT('Ctrl Pts',(-6.43436051072568,-2.78507295784401,
64.9036600946486));
#145147=CARTESIAN_POINT('Ctrl Pts',(-6.36112698330889,-2.95426454600137,
64.9120225994749));
#145148=CARTESIAN_POINT('Ctrl Pts',(-6.28121540443332,-3.12056756624219,
64.9203851043012));
#145149=CARTESIAN_POINT('Ctrl Pts',(-6.19488554340462,-3.28344630938537,
64.9287476091275));
#145150=CARTESIAN_POINT('Ctrl Pts',(-6.10854595259397,-3.44634340973008,
64.9371110564475));
#145151=CARTESIAN_POINT('Ctrl Pts',(-6.01578679181504,-3.60581517341989,
64.9454745037674));
#145152=CARTESIAN_POINT('Ctrl Pts',(-5.91691362818464,-3.76135077852397,
64.9538379510874));
#145153=CARTESIAN_POINT('Ctrl Pts',(-5.81798224525687,-3.91697796736334,
64.9622063230402));
#145154=CARTESIAN_POINT('Ctrl Pts',(-5.71292984131665,-4.06866408809416,
64.970574694993));
#145155=CARTESIAN_POINT('Ctrl Pts',(-5.60210571352749,-4.2159267233863,
64.9789430669458));
#145156=CARTESIAN_POINT('Ctrl Pts',(-5.49124837993321,-4.36323348241272,
64.9873139462815));
#145157=CARTESIAN_POINT('Ctrl Pts',(-5.37461607608116,-4.50611385372882,
64.9956848256173));
#145158=CARTESIAN_POINT('Ctrl Pts',(-5.25259863229461,-4.644118233908,65.004055704953));
#145159=CARTESIAN_POINT('Ctrl Pts',(-5.13047780444739,-4.78223954370618,
65.0124336768443));
#145160=CARTESIAN_POINT('Ctrl Pts',(-5.00296294133329,-4.91547636429601,
65.0208116487355));
#145161=CARTESIAN_POINT('Ctrl Pts',(-4.87048179501422,-5.04341487951716,
65.0291896206268));
#145162=CARTESIAN_POINT('Ctrl Pts',(-4.78628894772784,-5.12472084774993,
65.034513889986));
#145163=CARTESIAN_POINT('Ctrl Pts',(-4.700091096312,-5.20388774030555,65.0398381593451));
#145164=CARTESIAN_POINT('Ctrl Pts',(-4.61200508624651,-5.28081770627773,
65.0451624287043));
#145165=CARTESIAN_POINT('Ctrl Pts',(-4.48192049048981,-5.39442716046491,
65.0530252598936));
#145166=CARTESIAN_POINT('Ctrl Pts',(-4.34744573065318,-5.50339217667704,
65.0608880910829));
#145167=CARTESIAN_POINT('Ctrl Pts',(-4.20896128643903,-5.60734085389478,
65.0687509222722));
#145168=CARTESIAN_POINT('Ctrl Pts',(-4.07058324924061,-5.71120966027509,
65.0766077119136));
#145169=CARTESIAN_POINT('Ctrl Pts',(-3.92820195745968,-5.81006956527485,
65.084464501555));
#145170=CARTESIAN_POINT('Ctrl Pts',(-3.78223311581931,-5.90358697912547,
65.0923212911965));
#145171=CARTESIAN_POINT('Ctrl Pts',(-3.63634659369579,-5.99705165358157,
65.1001736499804));
#145172=CARTESIAN_POINT('Ctrl Pts',(-3.48687686637413,-6.08517962522453,
65.1080260087644));
#145173=CARTESIAN_POINT('Ctrl Pts',(-3.33427073827808,-6.16767907777006,
65.1158783675484));
#145174=CARTESIAN_POINT('Ctrl Pts',(-3.18170064226957,-6.2501590512322,
65.1237288722988));
#145175=CARTESIAN_POINT('Ctrl Pts',(-3.02599595044965,-6.32701296201912,
65.1315793770493));
#145176=CARTESIAN_POINT('Ctrl Pts',(-2.86763027164455,-6.39799368455829,
65.1394298817997));
#145177=CARTESIAN_POINT('Ctrl Pts',(-2.70929006888577,-6.4689629885364,
65.1472791236514));
#145178=CARTESIAN_POINT('Ctrl Pts',(-2.54829008068934,-6.53406083180514,
65.1551283655031));
#145179=CARTESIAN_POINT('Ctrl Pts',(-2.38512577784746,-6.59308740927553,
65.1629776073547));
#145180=CARTESIAN_POINT('Ctrl Pts',(-2.22190650175832,-6.65213387395521,
65.1708294937696));
#145181=CARTESIAN_POINT('Ctrl Pts',(-2.05652181357907,-6.70510485711426,
65.1786813801845));
#145182=CARTESIAN_POINT('Ctrl Pts',(-1.88948448864171,-6.75184974134366,
65.1865332665994));
#145183=CARTESIAN_POINT('Ctrl Pts',(-1.76683106001611,-6.78617392801027,
65.1922988090632));
#145184=CARTESIAN_POINT('Ctrl Pts',(-1.64328693965486,-6.81714216116263,
65.198064351527));
#145185=CARTESIAN_POINT('Ctrl Pts',(-1.51905916835793,-6.84471225147761,
65.2038298939908));
#145186=CARTESIAN_POINT('Ctrl Pts',(-1.31102029789007,-6.89088268815167,
65.2134851983505));
#145187=CARTESIAN_POINT('Ctrl Pts',(-1.1011701447253,-6.9274989208654,65.2231405027102));
#145188=CARTESIAN_POINT('Ctrl Pts',(-0.890310616200778,-6.95449304904248,
65.2327958070699));
#145189=CARTESIAN_POINT('Ctrl Pts',(-0.678282965444561,-6.98163671962568,
65.2425046000045));
#145190=CARTESIAN_POINT('Ctrl Pts',(-0.46523477859497,-6.9990514293502,
65.2522133929391));
#145191=CARTESIAN_POINT('Ctrl Pts',(-0.251976881867445,-7.00672064617281,
65.2619221858737));
#145192=CARTESIAN_POINT('Ctrl Pts',(-0.0376927700335318,-7.01442676791796,
65.2716776983442));
#145193=CARTESIAN_POINT('Ctrl Pts',(0.176803030718485,-7.01229340123862,
65.2814332108148));
#145194=CARTESIAN_POINT('Ctrl Pts',(0.390693177417793,-7.0003560912013,
65.2911887232853));
#145195=CARTESIAN_POINT('Ctrl Pts',(0.604795108269136,-6.9884069613905,
65.3009538952141));
#145196=CARTESIAN_POINT('Ctrl Pts',(0.818290147891335,-6.96663448447612,
65.3107190671429));
#145197=CARTESIAN_POINT('Ctrl Pts',(1.03036436573623,-6.93512623074166,
65.3204842390716));
#145198=CARTESIAN_POINT('Ctrl Pts',(1.24214942519621,-6.90366093779636,
65.33023609641));
#145199=CARTESIAN_POINT('Ctrl Pts',(1.45251749723369,-6.86248640462504,
65.3399879537484));
#145200=CARTESIAN_POINT('Ctrl Pts',(1.66066434996332,-6.81174136908184,
65.3497398110867));
#145201=CARTESIAN_POINT('Ctrl Pts',(1.75143145248323,-6.78961285845041,
65.3539923271502));
#145202=CARTESIAN_POINT('Ctrl Pts',(1.84177625502004,-6.76566509059098,
65.3582448432137));
#145203=CARTESIAN_POINT('Ctrl Pts',(1.93163247853033,-6.73991265005614,
65.3624973592771));
#145204=CARTESIAN_POINT('Ctrl Pts',(2.10137178816044,-6.69126603096945,
65.370530404876));
#145205=CARTESIAN_POINT('Ctrl Pts',(2.26944946600706,-6.63615233030069,
65.3785634504749));
#145206=CARTESIAN_POINT('Ctrl Pts',(2.4353310461155,-6.5747083021474,65.3865964960738));
#145207=CARTESIAN_POINT('Ctrl Pts',(2.60110599115723,-6.51330377258123,
65.3946243777217));
#145208=CARTESIAN_POINT('Ctrl Pts',(2.76468730624415,-6.44557714252209,
65.4026522593695));
#145209=CARTESIAN_POINT('Ctrl Pts',(2.925555093882,-6.37171515019002,65.4106801410174));
#145210=CARTESIAN_POINT('Ctrl Pts',(3.08635024812813,-6.29788650727552,
65.4187043979976));
#145211=CARTESIAN_POINT('Ctrl Pts',(3.24443398196679,-6.21792817046698,
65.4267286549777));
#145212=CARTESIAN_POINT('Ctrl Pts',(3.39930586598422,-6.13207519458016,
65.4347529119579));
#145213=CARTESIAN_POINT('Ctrl Pts',(3.55415902441318,-6.04623259919271,
65.4427761987237));
#145214=CARTESIAN_POINT('Ctrl Pts',(3.70580078238414,-5.95449695522676,
65.4507994854895));
#145215=CARTESIAN_POINT('Ctrl Pts',(3.853754685903,-5.85714959544151,65.4588227722552));
#145216=CARTESIAN_POINT('Ctrl Pts',(4.00169646591944,-5.75981021240392,
65.4668454015842));
#145217=CARTESIAN_POINT('Ctrl Pts',(4.14595068932674,-5.65686023436843,
65.4748680309132));
#145218=CARTESIAN_POINT('Ctrl Pts',(4.28606956809203,-5.54862453406026,
65.4828906602422));
#145219=CARTESIAN_POINT('Ctrl Pts',(4.42624112158021,-5.44034814483443,
65.4909163055087));
#145220=CARTESIAN_POINT('Ctrl Pts',(4.56227393640459,-5.32678229047758,
65.4989419507751));
#145221=CARTESIAN_POINT('Ctrl Pts',(4.69375273000823,-5.2082926062233,65.5069675960416));
#145222=CARTESIAN_POINT('Ctrl Pts',(4.77128063863112,-5.13842386798926,
65.5117000055489));
#145223=CARTESIAN_POINT('Ctrl Pts',(4.84722576033643,-5.06684386172466,
65.5164324150562));
#145224=CARTESIAN_POINT('Ctrl Pts',(4.92150891237859,-4.99363360569016,
65.5211648245635));
#145225=CARTESIAN_POINT('Ctrl Pts',(5.058541758735,-4.85857996982404,65.529894873398));
#145226=CARTESIAN_POINT('Ctrl Pts',(5.18998549790365,-4.71790921937674,
65.5386249222326));
#145227=CARTESIAN_POINT('Ctrl Pts',(5.31540476153175,-4.57210004085493,
65.5473549710671));
#145228=CARTESIAN_POINT('Ctrl Pts',(5.44086029029623,-4.42624870142743,
65.5560875442061));
#145229=CARTESIAN_POINT('Ctrl Pts',(5.56028768778448,-4.27525617590496,
65.5648201173452));
#145230=CARTESIAN_POINT('Ctrl Pts',(5.67329161435357,-4.11963454944798,
65.5735526904842));
#145231=CARTESIAN_POINT('Ctrl Pts',(5.78790094209027,-3.9618020693649,65.5824093237647));
#145232=CARTESIAN_POINT('Ctrl Pts',(5.89590272628379,-3.79920819291018,
65.5912659570452));
#145233=CARTESIAN_POINT('Ctrl Pts',(5.99692954073015,-3.63241829171946,
65.6001225903256));
#145234=CARTESIAN_POINT('Ctrl Pts',(6.09660462300902,-3.46786002849424,
65.6088607224323));
#145235=CARTESIAN_POINT('Ctrl Pts',(6.18949010158144,-3.2992175778555,65.6175988545389));
#145236=CARTESIAN_POINT('Ctrl Pts',(6.27527851617244,-3.12706029794192,
65.6263369866456));
#145237=CARTESIAN_POINT('Ctrl Pts',(6.36281204534399,-2.95140098129346,
65.635252870513));
#145238=CARTESIAN_POINT('Ctrl Pts',(6.44295654417856,-2.77208256922448,
65.6441687543804));
#145239=CARTESIAN_POINT('Ctrl Pts',(6.51543584224807,-2.58973403036861,
65.6530846382478));
#145240=CARTESIAN_POINT('Ctrl Pts',(6.58791514031757,-2.40738549151275,
65.6620005221152));
#145241=CARTESIAN_POINT('Ctrl Pts',(6.65272913157334,-2.22200710914342,
65.6709164059825));
#145242=CARTESIAN_POINT('Ctrl Pts',(6.70965433379166,-2.03424808799978,
65.6798322898499));
#145243=CARTESIAN_POINT('Ctrl Pts',(6.76495279891978,-1.85185460886237,
65.6884933867616));
#145244=CARTESIAN_POINT('Ctrl Pts',(6.81281612486858,-1.66718451891293,
65.6971544836732));
#145245=CARTESIAN_POINT('Ctrl Pts',(6.85308001335165,-1.48085140817713,
65.7058155805848));
#145246=CARTESIAN_POINT('Ctrl Pts',(6.89333506400459,-1.29455919712691,
65.7144747764058));
#145247=CARTESIAN_POINT('Ctrl Pts',(6.92599394708081,-1.10660497444136,
65.7231339722267));
#145248=CARTESIAN_POINT('Ctrl Pts',(6.95094321879162,-0.917613715914716,
65.7317931680476));
#145249=CARTESIAN_POINT('Ctrl Pts',(6.97588795116692,-0.728656842950113,
65.7404507883919));
#145250=CARTESIAN_POINT('Ctrl Pts',(6.9931258345822,-0.538663595112505,
65.7491084087362));
#145251=CARTESIAN_POINT('Ctrl Pts',(7.00259503583784,-0.34826617199953,
65.7577660290805));
#145252=CARTESIAN_POINT('Ctrl Pts',(7.00834386225704,-0.232674401734254,
65.7630221383572));
#145253=CARTESIAN_POINT('Ctrl Pts',(7.01123031221653,-0.116933788902505,
65.7682782476338));
#145254=CARTESIAN_POINT('Ctrl Pts',(7.01124989960851,-0.00118648203415713,
65.7735343569105));
#145255=CARTESIAN_POINT('Ctrl Pts',(7.01124989960866,-0.00118648116572791,
65.77353435695));
#145256=CARTESIAN_POINT('Ctrl Pts',(7.0112840123165,0.200395074739239,65.7826882173262));
#145257=CARTESIAN_POINT('Ctrl Pts',(7.00262022694374,0.401968333003894,
65.7918420777024));
#145258=CARTESIAN_POINT('Ctrl Pts',(6.98528696966447,0.60282046575725,65.8009959380786));
#145259=CARTESIAN_POINT('Ctrl Pts',(6.96796416523818,0.803551474259107,
65.8101442782024));
#145260=CARTESIAN_POINT('Ctrl Pts',(6.94198235287763,1.00356203563452,65.8192926183262));
#145261=CARTESIAN_POINT('Ctrl Pts',(6.90742184975187,1.20214389823782,65.8284409584499));
#145262=CARTESIAN_POINT('Ctrl Pts',(6.89475517763354,1.27492557427682,65.8317938906788));
#145263=CARTESIAN_POINT('Ctrl Pts',(6.88093665414608,1.34751538295692,65.8351468229076));
#145264=CARTESIAN_POINT('Ctrl Pts',(6.86597197759889,1.41987864457733,65.8384997551364));
#145265=CARTESIAN_POINT('Ctrl Pts',(6.82996706766942,1.59398415956331,65.8465668872604));
#145266=CARTESIAN_POINT('Ctrl Pts',(6.7873122578682,1.76683134930017,65.8546340193843));
#145267=CARTESIAN_POINT('Ctrl Pts',(6.73812170080834,1.93787061167553,65.8627011515083));
#145268=CARTESIAN_POINT('Ctrl Pts',(6.68893114374847,2.10890987405096,65.8707682836323));
#145269=CARTESIAN_POINT('Ctrl Pts',(6.63320492220022,2.27814084184561,65.8788354157562));
#145270=CARTESIAN_POINT('Ctrl Pts',(6.57110895151813,2.44502632087639,65.8869025478802));
#145271=CARTESIAN_POINT('',(7.01124984252467,0.00148600060135456,65.226465643127));
#145272=CARTESIAN_POINT('Ctrl Pts',(6.57110895151811,2.44502632087645,65.3396321383564));
#145273=CARTESIAN_POINT('Ctrl Pts',(6.6359526070107,2.27075632573637,65.3311689379889));
#145274=CARTESIAN_POINT('Ctrl Pts',(6.69392407376079,2.09373197228993,65.3227057376215));
#145275=CARTESIAN_POINT('Ctrl Pts',(6.74479490719116,1.91451514029745,65.314242537254));
#145276=CARTESIAN_POINT('Ctrl Pts',(6.79557866611771,1.73560506987483,65.3057938231633));
#145277=CARTESIAN_POINT('Ctrl Pts',(6.8392859518127,1.55451030828681,65.2973451090727));
#145278=CARTESIAN_POINT('Ctrl Pts',(6.87573731344327,1.37181010312068,65.288896394982));
#145279=CARTESIAN_POINT('Ctrl Pts',(6.91215146763154,1.18929638776006,65.2804563048501));
#145280=CARTESIAN_POINT('Ctrl Pts',(6.94132439855923,1.00518080182279,65.2720162147183));
#145281=CARTESIAN_POINT('Ctrl Pts',(6.96312671381785,0.820056662564405,
65.2635761245864));
#145282=CARTESIAN_POINT('Ctrl Pts',(6.98490210623169,0.635161126021161,
65.2551464567989));
#145283=CARTESIAN_POINT('Ctrl Pts',(6.99932500152693,0.44925983156964,65.2467167890113));
#145284=CARTESIAN_POINT('Ctrl Pts',(7.00631723022827,0.262955189921164,
65.2382871212238));
#145285=CARTESIAN_POINT('Ctrl Pts',(7.0095857844396,0.17586610186922,65.2343466285248));
#145286=CARTESIAN_POINT('Ctrl Pts',(7.01123136026748,0.0886890089352705,
65.2304061358259));
#145287=CARTESIAN_POINT('Ctrl Pts',(7.01124984252467,0.00148600060139123,
65.2264656431269));
#145288=CARTESIAN_POINT('Ctrl Pts',(7.01124984252485,0.00148599977491322,
65.2264656430896));
#145289=CARTESIAN_POINT('Ctrl Pts',(7.01127194560764,-0.102800850311695,
65.2217531729671));
#145290=CARTESIAN_POINT('Ctrl Pts',(7.00896671320105,-0.207099752355944,
65.2170407028447));
#145291=CARTESIAN_POINT('Ctrl Pts',(7.00433593370117,-0.311295182041935,
65.2123282327223));
#145292=CARTESIAN_POINT('Ctrl Pts',(6.99614216792538,-0.495660027264679,
65.2039899224206));
#145293=CARTESIAN_POINT('Ctrl Pts',(6.98066829470659,-0.679625393476375,
65.195651612119));
#145294=CARTESIAN_POINT('Ctrl Pts',(6.95798456722586,-0.862599168065245,
65.1873133018173));
#145295=CARTESIAN_POINT('Ctrl Pts',(6.93528656791354,-1.04568806354407,
65.1789697453337));
#145296=CARTESIAN_POINT('Ctrl Pts',(6.90536970664401,-1.22778379784101,
65.17062618885));
#145297=CARTESIAN_POINT('Ctrl Pts',(6.86835561249141,-1.40830314309731,
65.1622826323664));
#145298=CARTESIAN_POINT('Ctrl Pts',(6.8313133581775,-1.58895982668374,65.1539327281414));
#145299=CARTESIAN_POINT('Ctrl Pts',(6.78716316639149,-1.76803740838765,
65.1455828239164));
#145300=CARTESIAN_POINT('Ctrl Pts',(6.73607700273446,-1.94496611171812,
65.1372329196913));
#145301=CARTESIAN_POINT('Ctrl Pts',(6.68491421361207,-2.12216019501178,
65.1288704912278));
#145302=CARTESIAN_POINT('Ctrl Pts',(6.62679475423575,-2.29719864398295,
65.1205080627642));
#145303=CARTESIAN_POINT('Ctrl Pts',(6.56193989050479,-2.46952858576328,
65.1121456343007));
#145304=CARTESIAN_POINT('Ctrl Pts',(6.49702956702429,-2.64200589313594,
65.1037760548208));
#145305=CARTESIAN_POINT('Ctrl Pts',(6.42537247423215,-2.81176977086986,
65.095406475341));
#145306=CARTESIAN_POINT('Ctrl Pts',(6.34723688012722,-2.97828987005176,
65.0870368958611));
#145307=CARTESIAN_POINT('Ctrl Pts',(6.26898077138835,-3.14506680619798,
65.0786544073246));
#145308=CARTESIAN_POINT('Ctrl Pts',(6.18422634422477,-3.30858967570553,
65.0702719187882));
#145309=CARTESIAN_POINT('Ctrl Pts',(6.09328710268872,-3.46835391024436,
65.0618894302517));
#145310=CARTESIAN_POINT('Ctrl Pts',(6.06353029271894,-3.52063138569762,
65.0591465426463));
#145311=CARTESIAN_POINT('Ctrl Pts',(6.03311160924494,-3.57250666406741,
65.0564036550409));
#145312=CARTESIAN_POINT('Ctrl Pts',(6.00204300290693,-3.62396279696081,
65.0536607674355));
#145313=CARTESIAN_POINT('Ctrl Pts',(5.90701136331527,-3.78135513772773,
65.0452709123027));
#145314=CARTESIAN_POINT('Ctrl Pts',(5.80570400173806,-3.93514141930128,
65.0368810571698));
#145315=CARTESIAN_POINT('Ctrl Pts',(5.69841812432148,-4.08480812804034,
65.028491202037));
#145316=CARTESIAN_POINT('Ctrl Pts',(5.59123124880834,-4.23433672643904,
65.0201090889448));
#145317=CARTESIAN_POINT('Ctrl Pts',(5.47807704596437,-4.37975306437344,
65.0117269758526));
#145318=CARTESIAN_POINT('Ctrl Pts',(5.35929687460376,-4.52057115554688,
65.0033448627605));
#145319=CARTESIAN_POINT('Ctrl Pts',(5.24060885148161,-4.66128000172684,
64.9949692524116));
#145320=CARTESIAN_POINT('Ctrl Pts',(5.11630377263338,-4.79739746281312,
64.9865936420627));
#145321=CARTESIAN_POINT('Ctrl Pts',(4.98676452950537,-4.92846893971821,
64.9782180317138));
#145322=CARTESIAN_POINT('Ctrl Pts',(4.85730676848496,-5.0594579707179,64.9698476897481));
#145323=CARTESIAN_POINT('Ctrl Pts',(4.72262163834821,-5.18540711300072,
64.9614773477826));
#145324=CARTESIAN_POINT('Ctrl Pts',(4.58313060333516,-5.30589676070621,
64.953107005817));
#145325=CARTESIAN_POINT('Ctrl Pts',(4.44370686243555,-5.42632828106309,
64.9447407019226));
#145326=CARTESIAN_POINT('Ctrl Pts',(4.29948208843632,-5.54130534457375,
64.9363743980283));
#145327=CARTESIAN_POINT('Ctrl Pts',(4.15091304341011,-5.65044666097715,
64.928008094134));
#145328=CARTESIAN_POINT('Ctrl Pts',(4.00238554898131,-5.75955745361366,
64.9196441300604));
#145329=CARTESIAN_POINT('Ctrl Pts',(3.84951646993777,-5.86283555794911,
64.9112801659868));
#145330=CARTESIAN_POINT('Ctrl Pts',(3.69279438675011,-5.95994095437923,
64.9029162019131));
#145331=CARTESIAN_POINT('Ctrl Pts',(3.53609642048622,-6.05703140790282,
64.8945535249146));
#145332=CARTESIAN_POINT('Ctrl Pts',(3.3755469115246,-6.14795087433382,64.886190847916));
#145333=CARTESIAN_POINT('Ctrl Pts',(3.21166241619738,-6.23240331548635,
64.8778281709175));
#145334=CARTESIAN_POINT('Ctrl Pts',(3.04778129495275,-6.31685401791727,
64.8694656660912));
#145335=CARTESIAN_POINT('Ctrl Pts',(2.88056561657793,-6.39483781037193,
64.8611031612649));
#145336=CARTESIAN_POINT('Ctrl Pts',(2.71055584899794,-6.46610497532812,
64.8527406564386));
#145337=CARTESIAN_POINT('Ctrl Pts',(2.54052692051615,-6.53738017242957,
64.8443772091186));
#145338=CARTESIAN_POINT('Ctrl Pts',(2.3677035782861,-6.60193710624488,64.8360137617986));
#145339=CARTESIAN_POINT('Ctrl Pts',(2.19264594025775,-6.65957433648512,
64.8276503144786));
#145340=CARTESIAN_POINT('Ctrl Pts',(2.01748522337276,-6.71724550514621,
64.8192819425258));
#145341=CARTESIAN_POINT('Ctrl Pts',(1.8400878939732,-6.76798872457742,64.810913570573));
#145342=CARTESIAN_POINT('Ctrl Pts',(1.66102989130136,-6.81165224176216,
64.8025451986202));
#145343=CARTESIAN_POINT('Ctrl Pts',(1.48191823817219,-6.8553288416778,64.7941743192844));
#145344=CARTESIAN_POINT('Ctrl Pts',(1.30114524022368,-6.89192143686218,
64.7858034399486));
#145345=CARTESIAN_POINT('Ctrl Pts',(1.11929739056601,-6.9213293458679,64.7774325606129));
#145346=CARTESIAN_POINT('Ctrl Pts',(0.937295463191772,-6.95076217187691,
64.7690545887216));
#145347=CARTESIAN_POINT('Ctrl Pts',(0.754217189902066,-6.97299810058511,
64.7606766168303));
#145348=CARTESIAN_POINT('Ctrl Pts',(0.570655713219298,-6.98798816680954,
64.752298644939));
#145349=CARTESIAN_POINT('Ctrl Pts',(0.454000900049228,-6.99751447595904,
64.7469743755804));
#145350=CARTESIAN_POINT('Ctrl Pts',(0.337151023200128,-7.0041154412878,
64.7416501062217));
#145351=CARTESIAN_POINT('Ctrl Pts',(0.220258480231267,-7.00778943493497,
64.7363258368631));
#145352=CARTESIAN_POINT('Ctrl Pts',(0.0476326661061011,-7.01321515438915,
64.7284630056738));
#145353=CARTESIAN_POINT('Ctrl Pts',(-0.125445162475985,-7.01226592069183,
64.7206001744845));
#145354=CARTESIAN_POINT('Ctrl Pts',(-0.298444993881777,-7.00489522749105,
64.7127373432952));
#145355=CARTESIAN_POINT('Ctrl Pts',(-0.471311897752816,-6.99753019769508,
64.7048805536537));
#145356=CARTESIAN_POINT('Ctrl Pts',(-0.644100545164281,-6.98375353657632,
64.6970237640123));
#145357=CARTESIAN_POINT('Ctrl Pts',(-0.816277960679824,-6.96357069709272,
64.6891669743709));
#145358=CARTESIAN_POINT('Ctrl Pts',(-0.988358276283166,-6.94339923977522,
64.6813146155869));
#145359=CARTESIAN_POINT('Ctrl Pts',(-1.15982766819099,-6.91682883499378,
64.6734622568029));
#145360=CARTESIAN_POINT('Ctrl Pts',(-1.33015558245117,-6.88391695831479,
64.6656098980189));
#145361=CARTESIAN_POINT('Ctrl Pts',(-1.50044328030389,-6.85101285251381,
64.6577593932684));
#145362=CARTESIAN_POINT('Ctrl Pts',(-1.66958966131295,-6.81177031883289,
64.6499088885179));
#145363=CARTESIAN_POINT('Ctrl Pts',(-1.83707176434058,-6.76629838945657,
64.6420583837674));
#145364=CARTESIAN_POINT('Ctrl Pts',(-2.00452692477618,-6.72083377508061,
64.6342091419158));
#145365=CARTESIAN_POINT('Ctrl Pts',(-2.1703179727901,-6.6691418627927,64.6263599000641));
#145366=CARTESIAN_POINT('Ctrl Pts',(-2.33393502974738,-6.61138214289706,
64.6185106582124));
#145367=CARTESIAN_POINT('Ctrl Pts',(-2.4976072124939,-6.55360296262116,
64.6106587717975));
#145368=CARTESIAN_POINT('Ctrl Pts',(-2.65910358105503,-6.48975201836282,
64.6028068853825));
#145369=CARTESIAN_POINT('Ctrl Pts',(-2.81793204785603,-6.42003781423178,
64.5949549989676));
#145370=CARTESIAN_POINT('Ctrl Pts',(-2.93455781412435,-6.36884754185601,
64.5891894565039));
#145371=CARTESIAN_POINT('Ctrl Pts',(-3.04974546524054,-6.31449695611502,
64.5834239140402));
#145372=CARTESIAN_POINT('Ctrl Pts',(-3.16330811802645,-6.25708464965338,
64.5776583715764));
#145373=CARTESIAN_POINT('Ctrl Pts',(-3.35348657624183,-6.16093874554134,
64.5680030672169));
#145374=CARTESIAN_POINT('Ctrl Pts',(-3.53901044179996,-6.05625478980657,
64.5583477628573));
#145375=CARTESIAN_POINT('Ctrl Pts',(-3.71921641495434,-5.9434885228487,
64.5486924584977));
#145376=CARTESIAN_POINT('Ctrl Pts',(-3.90042069539488,-5.83009755192588,
64.5389836655633));
#145377=CARTESIAN_POINT('Ctrl Pts',(-4.07624798900836,-5.70853454417221,
64.5292748726288));
#145378=CARTESIAN_POINT('Ctrl Pts',(-4.246060655549,-5.57930062569663,64.5195660796944));
#145379=CARTESIAN_POINT('Ctrl Pts',(-4.41669047506078,-5.44944482263136,
64.5098105672239));
#145380=CARTESIAN_POINT('Ctrl Pts',(-4.58124762253423,-5.31184415036341,
64.5000550547534));
#145381=CARTESIAN_POINT('Ctrl Pts',(-4.73912242433671,-5.16704414628412,
64.4902995422829));
#145382=CARTESIAN_POINT('Ctrl Pts',(-4.89715354648244,-5.02210076792291,
64.4805343703541));
#145383=CARTESIAN_POINT('Ctrl Pts',(-5.04848906764465,-4.86994383338251,
64.4707691984254));
#145384=CARTESIAN_POINT('Ctrl Pts',(-5.19255492798473,-4.7111569579416,
64.4610040264967));
#145385=CARTESIAN_POINT('Ctrl Pts',(-5.3364243577922,-4.55258658480346,
64.4512521691583));
#145386=CARTESIAN_POINT('Ctrl Pts',(-5.47304391187152,-4.38740436615538,
64.44150031182));
#145387=CARTESIAN_POINT('Ctrl Pts',(-5.60187946290261,-4.21622734747665,
64.4317484544817));
#145388=CARTESIAN_POINT('Ctrl Pts',(-5.65806109388263,-4.14158177008204,
64.4274959384178));
#145389=CARTESIAN_POINT('Ctrl Pts',(-5.7127630105389,-4.06579668417115,
64.423243422354));
#145390=CARTESIAN_POINT('Ctrl Pts',(-5.76594319091945,-3.98892537929573,
64.4189909062902));
#145391=CARTESIAN_POINT('Ctrl Pts',(-5.86640108632526,-3.8437147115315,
64.4109578606913));
#145392=CARTESIAN_POINT('Ctrl Pts',(-5.96147480433731,-3.69455501880349,
64.4029248150925));
#145393=CARTESIAN_POINT('Ctrl Pts',(-6.05083762023003,-3.54189083063114,
64.3948917694936));
#145394=CARTESIAN_POINT('Ctrl Pts',(-6.14014299026379,-3.38932478087729,
64.3868638878458));
#145395=CARTESIAN_POINT('Ctrl Pts',(-6.22374458135831,-3.23325903501766,
64.378836006198));
#145396=CARTESIAN_POINT('Ctrl Pts',(-6.30135861793588,-3.0741675508445,
64.3708081245502));
#145397=CARTESIAN_POINT('Ctrl Pts',(-6.37893761101054,-2.91514789804532,
64.3627838675701));
#145398=CARTESIAN_POINT('Ctrl Pts',(-6.45053427203421,-2.75310555586578,
64.35475961059));
#145399=CARTESIAN_POINT('Ctrl Pts',(-6.5159105074575,-2.58853951511369,
64.3467353536099));
#145400=CARTESIAN_POINT('Ctrl Pts',(-6.58127883822837,-2.42399337207126,
64.3387120668441));
#145401=CARTESIAN_POINT('Ctrl Pts',(-6.64042809905632,-2.25692447587121,
64.3306887800784));
#145402=CARTESIAN_POINT('Ctrl Pts',(-6.69316807265263,-2.08785241665293,
64.3226654933127));
#145403=CARTESIAN_POINT('Ctrl Pts',(-6.74590372467866,-1.9187942113814,
64.3146428639837));
#145404=CARTESIAN_POINT('Ctrl Pts',(-6.79223103024297,-1.74773352125313,
64.3066202346547));
#145405=CARTESIAN_POINT('Ctrl Pts',(-6.83200954101177,-1.57520544502113,
64.2985976053257));
#145406=CARTESIAN_POINT('Ctrl Pts',(-6.87180300566862,-1.40261251051544,
64.2905719600593));
#145407=CARTESIAN_POINT('Ctrl Pts',(-6.90504267802685,-1.22855144604104,
64.2825463147929));
#145408=CARTESIAN_POINT('Ctrl Pts',(-6.93163908812218,-1.05356827710248,
64.2745206695265));
#145409=CARTESIAN_POINT('Ctrl Pts',(-6.94732195221921,-0.950387537751055,
64.2697882600188));
#145410=CARTESIAN_POINT('Ctrl Pts',(-6.96069592775564,-0.846886351344504,
64.2650558505112));
#145411=CARTESIAN_POINT('Ctrl Pts',(-6.97175111860442,-0.743177571471341,
64.2603234410035));
#145412=CARTESIAN_POINT('Ctrl Pts',(-6.99214503333888,-0.551862193665758,
64.2515933921688));
#145413=CARTESIAN_POINT('Ctrl Pts',(-7.00465564836291,-0.359744518498557,
64.2428633433341));
#145414=CARTESIAN_POINT('Ctrl Pts',(-7.00924961118251,-0.167470745618054,
64.2341332944993));
#145415=CARTESIAN_POINT('Ctrl Pts',(-7.01384490235223,0.0248586234652346,
64.22540072136));
#145416=CARTESIAN_POINT('Ctrl Pts',(-7.01051896558698,0.21734390649135,
64.2166681482206));
#145417=CARTESIAN_POINT('Ctrl Pts',(-6.99929057855394,0.409338441226893,
64.2079355750813));
#145418=CARTESIAN_POINT('Ctrl Pts',(-6.98790267435951,0.604060564804206,
64.199078941801));
#145419=CARTESIAN_POINT('Ctrl Pts',(-6.9683860917018,0.798277600745668,
64.1902223085207));
#145420=CARTESIAN_POINT('Ctrl Pts',(-6.94081497261681,0.991319362465166,
64.1813656752403));
#145421=CARTESIAN_POINT('Ctrl Pts',(-6.91361275330025,1.18177823805019,
64.1726275431335));
#145422=CARTESIAN_POINT('Ctrl Pts',(-6.87857025954122,1.3710928225916,64.1638894110266));
#145423=CARTESIAN_POINT('Ctrl Pts',(-6.83581054283176,1.55862785327678,
64.1551512789198));
#145424=CARTESIAN_POINT('Ctrl Pts',(-6.79218100465246,1.74997773608423,
64.1462353950527));
#145425=CARTESIAN_POINT('Ctrl Pts',(-6.74051697392506,1.93947460024544,
64.1373195111856));
#145426=CARTESIAN_POINT('Ctrl Pts',(-6.68100348636698,2.12645690707625,
64.1284036273185));
#145427=CARTESIAN_POINT('Ctrl Pts',(-6.62148999880889,2.31343921390706,
64.1194877434514));
#145428=CARTESIAN_POINT('Ctrl Pts',(-6.55412715193585,2.49790667708451,
64.1105718595843));
#145429=CARTESIAN_POINT('Ctrl Pts',(-6.47915356094306,2.67921550014532,
64.1016559757172));
#145430=CARTESIAN_POINT('Ctrl Pts',(-6.40565321995918,2.85696155901605,
64.0929152912211));
#145431=CARTESIAN_POINT('Ctrl Pts',(-6.32483065806716,3.03169084005782,
64.0841746067251));
#145432=CARTESIAN_POINT('Ctrl Pts',(-6.23695464383602,3.20281490773855,
64.075433922229));
#145433=CARTESIAN_POINT('Ctrl Pts',(-6.14909443995983,3.37390818735642,
64.0666948103273));
#145434=CARTESIAN_POINT('Ctrl Pts',(-6.05418344312836,3.54139730552184,
64.0579556984256));
#145435=CARTESIAN_POINT('Ctrl Pts',(-5.95253689588775,3.70471740698194,
64.0492165865238));
#145436=CARTESIAN_POINT('Ctrl Pts',(-5.84957337132991,3.87015355541964,
64.0403642468494));
#145437=CARTESIAN_POINT('Ctrl Pts',(-5.73969867367886,4.03131164898845,
64.031511907175));
#145438=CARTESIAN_POINT('Ctrl Pts',(-5.62328718275385,4.18763272300429,
64.0226595675006));
#145439=CARTESIAN_POINT('Ctrl Pts',(-5.50842358207695,4.34187524047797,
64.013924934851));
#145440=CARTESIAN_POINT('Ctrl Pts',(-5.38719612325943,4.49140835545715,
64.0051903022014));
#145441=CARTESIAN_POINT('Ctrl Pts',(-5.26000708672101,4.63572561851376,
63.9964556695518));
#145442=CARTESIAN_POINT('Ctrl Pts',(-5.13024707032258,4.78296008879882,
63.987544476365));
#145443=CARTESIAN_POINT('Ctrl Pts',(-4.99428207218218,4.9247653643007,63.9786332831781));
#145444=CARTESIAN_POINT('Ctrl Pts',(-4.85258201246857,5.06063971991353,
63.9697220899913));
#145445=CARTESIAN_POINT('Ctrl Pts',(-4.71088195275502,5.19651407552631,
63.9608108968044));
#145446=CARTESIAN_POINT('Ctrl Pts',(-4.56344704093831,5.32645729172441,
63.9518997036176));
#145447=CARTESIAN_POINT('Ctrl Pts',(-4.41078738240452,5.4500074522629,63.9429885104308));
#145448=CARTESIAN_POINT('Ctrl Pts',(-4.27329790931198,5.56128011352838,
63.9349628455783));
#145449=CARTESIAN_POINT('Ctrl Pts',(-4.13150697620337,5.66741791020393,
63.9269371807258));
#145450=CARTESIAN_POINT('Ctrl Pts',(-3.98584443947909,5.76807339297738,
63.9189115158734));
#145451=CARTESIAN_POINT('Ctrl Pts',(-3.8402281324701,5.86869693017022,63.91088839817));
#145452=CARTESIAN_POINT('Ctrl Pts',(-3.6907429693899,5.96384140939698,63.9028652804667));
#145453=CARTESIAN_POINT('Ctrl Pts',(-3.53784990251516,6.05320118860867,
63.8948421627633));
#145454=CARTESIAN_POINT('Ctrl Pts',(-3.384976116794,6.1425496987703,63.8868200568453));
#145455=CARTESIAN_POINT('Ctrl Pts',(-3.22869560001304,6.2261147775928,63.8787979509273));
#145456=CARTESIAN_POINT('Ctrl Pts',(-3.06949610299193,6.3036354777396,63.8707758450093));
#145457=CARTESIAN_POINT('Ctrl Pts',(-2.91023744690084,6.38118498484001,
63.8627507580497));
#145458=CARTESIAN_POINT('Ctrl Pts',(-2.74805797224509,6.45268546291316,
63.8547256710901));
#145459=CARTESIAN_POINT('Ctrl Pts',(-2.58346813076676,6.51792290379478,
63.8467005841305));
#145460=CARTESIAN_POINT('Ctrl Pts',(-2.41884587414272,6.58317319286394,
63.8386739166702));
#145461=CARTESIAN_POINT('Ctrl Pts',(-2.25181264901268,6.6421578605787,63.8306472492099));
#145462=CARTESIAN_POINT('Ctrl Pts',(-2.08289626825347,6.69471206985004,
63.8226205817495));
#145463=CARTESIAN_POINT('Ctrl Pts',(-1.9138442820195,6.74730846945523,63.8145874705089));
#145464=CARTESIAN_POINT('Ctrl Pts',(-1.74290647344521,6.7934640001079,63.8065543592682));
#145465=CARTESIAN_POINT('Ctrl Pts',(-1.57062371239913,6.83306429916693,
63.7985212480275));
#145466=CARTESIAN_POINT('Ctrl Pts',(-1.46910845109101,6.85639823392887,
63.7937878470665));
#145467=CARTESIAN_POINT('Ctrl Pts',(-1.3671264192136,6.87745716470111,63.7890544461054));
#145468=CARTESIAN_POINT('Ctrl Pts',(-1.26478941081879,6.89622609176792,
63.7843210451443));
#145469=CARTESIAN_POINT('Ctrl Pts',(-1.05397198856531,6.9348906656572,63.7745700918503));
#145470=CARTESIAN_POINT('Ctrl Pts',(-0.841523672655311,6.96385777599663,
63.7648191385563));
#145471=CARTESIAN_POINT('Ctrl Pts',(-0.628257409121949,6.9830451230379,
63.7550681852622));
#145472=CARTESIAN_POINT('Ctrl Pts',(-0.414683895533134,7.0022601130516,
63.745303183891));
#145473=CARTESIAN_POINT('Ctrl Pts',(-0.200290115638335,7.01166715299209,
63.7355381825197));
#145474=CARTESIAN_POINT('Ctrl Pts',(0.0141058876221566,7.01123581021452,
63.7257731811485));
#145475=CARTESIAN_POINT('Ctrl Pts',(0.228144537171048,7.01080518639597,
63.7160244560111));
#145476=CARTESIAN_POINT('Ctrl Pts',(0.442185364769944,7.00056895396792,
63.7062757308736));
#145477=CARTESIAN_POINT('Ctrl Pts',(0.655413416490399,6.98054867585524,
63.6965270057362));
#145478=CARTESIAN_POINT('Ctrl Pts',(0.868056239884947,6.96058334564342,
63.6868050370694));
#145479=CARTESIAN_POINT('Ctrl Pts',(1.07989070097927,6.93088758192718,63.6770830684026));
#145480=CARTESIAN_POINT('Ctrl Pts',(1.29010813751828,6.8915344848596,63.6673610997357));
#145481=CARTESIAN_POINT('Ctrl Pts',(1.49893462018888,6.85244177695623,63.6577034587962));
#145482=CARTESIAN_POINT('Ctrl Pts',(1.70616535524532,6.80381909359534,63.6480458178566));
#145483=CARTESIAN_POINT('Ctrl Pts',(1.91100791851239,6.74578944956652,63.638388176917));
#145484=CARTESIAN_POINT('Ctrl Pts',(2.00104327739133,6.72028342317033,63.6341433112307));
#145485=CARTESIAN_POINT('Ctrl Pts',(2.09061727252663,6.69296073300884,63.6298984455443));
#145486=CARTESIAN_POINT('Ctrl Pts',(2.17966267742007,6.66383502010381,63.625653579858));
#145487=CARTESIAN_POINT('Ctrl Pts',(2.34437245817196,6.60996037275317,63.617801732844));
#145488=CARTESIAN_POINT('Ctrl Pts',(2.50720483800169,6.54993521035113,63.60994988583));
#145489=CARTESIAN_POINT('Ctrl Pts',(2.66765176713443,6.48392324228199,63.6020980388161));
#145490=CARTESIAN_POINT('Ctrl Pts',(2.82805319481588,6.41792999467305,63.5942484185224));
#145491=CARTESIAN_POINT('Ctrl Pts',(2.98607016503819,6.3459534636276,63.5863987982287));
#145492=CARTESIAN_POINT('Ctrl Pts',(3.14121267937534,6.26820623986094,63.5785491779351));
#145493=CARTESIAN_POINT('Ctrl Pts',(3.2963428075658,6.19046522321631,63.5707001843333));
#145494=CARTESIAN_POINT('Ctrl Pts',(3.44859859601861,6.10695460258495,63.5628511907314));
#145495=CARTESIAN_POINT('Ctrl Pts',(3.5975130554672,6.01793372996439,63.5550021971296));
#145496=CARTESIAN_POINT('Ctrl Pts',(3.7465029059468,5.9288677886823,63.5471492298121));
#145497=CARTESIAN_POINT('Ctrl Pts',(3.89214771963935,5.83428621747869,63.5392962624946));
#145498=CARTESIAN_POINT('Ctrl Pts',(4.03400772258457,5.73449285086554,63.5314432951772));
#145499=CARTESIAN_POINT('Ctrl Pts',(4.17590375320397,5.63467414009039,63.5235883334698));
#145500=CARTESIAN_POINT('Ctrl Pts',(4.31401275444233,5.52964122788591,63.5157333717625));
#145501=CARTESIAN_POINT('Ctrl Pts',(4.44792720152231,5.41973893951156,63.5078784100552));
#145502=CARTESIAN_POINT('Ctrl Pts',(4.58197456988463,5.30972756392952,63.5000156516418));
#145503=CARTESIAN_POINT('Ctrl Pts',(4.71181878306663,5.19483741159344,63.4921528932284));
#145504=CARTESIAN_POINT('Ctrl Pts',(4.8370880054203,5.07545132873118,63.484290134815));
#145505=CARTESIAN_POINT('Ctrl Pts',(4.92898370942698,4.98787141143711,63.4785221280672));
#145506=CARTESIAN_POINT('Ctrl Pts',(5.01841814622961,4.89787280848837,63.4727541213193));
#145507=CARTESIAN_POINT('Ctrl Pts',(5.10525833231068,4.80561795431892,63.4669861145715));
#145508=CARTESIAN_POINT('Ctrl Pts',(5.23025327460224,4.67282931471073,63.4586838330689));
#145509=CARTESIAN_POINT('Ctrl Pts',(5.35016368603412,4.53505539088394,63.4503815515662));
#145510=CARTESIAN_POINT('Ctrl Pts',(5.46458333403442,4.39271619250473,63.4420792700636));
#145511=CARTESIAN_POINT('Ctrl Pts',(5.58182955935114,4.24686070337994,63.4335718923124));
#145512=CARTESIAN_POINT('Ctrl Pts',(5.69330995865957,4.09621169834653,63.4250645145612));
#145513=CARTESIAN_POINT('Ctrl Pts',(5.79862868272004,3.94126019978845,63.41655713681));
#145514=CARTESIAN_POINT('Ctrl Pts',(5.90126312236804,3.7902579884628,63.4082665887032));
#145515=CARTESIAN_POINT('Ctrl Pts',(5.9980459315389,3.63517021859697,63.3999760405964));
#145516=CARTESIAN_POINT('Ctrl Pts',(6.08865238761097,3.4764836638965,63.3916854924896));
#145517=CARTESIAN_POINT('Ctrl Pts',(6.18281340341766,3.3115717157504,63.3830696999162));
#145518=CARTESIAN_POINT('Ctrl Pts',(6.27030342472347,3.14277320211189,63.3744539073428));
#145519=CARTESIAN_POINT('Ctrl Pts',(6.35080850537203,2.97066623682201,63.3658381147693));
#145520=CARTESIAN_POINT('Ctrl Pts',(6.43131358602062,2.79855927153207,63.3572223221959));
#145521=CARTESIAN_POINT('Ctrl Pts',(6.50483353961304,2.62314422035117,63.3486065296225));
#145522=CARTESIAN_POINT('Ctrl Pts',(6.57110895151814,2.44502632087636,63.3399907370491));
#145523=CARTESIAN_POINT('Origin',(0.,0.,50.));
#145524=CARTESIAN_POINT('',(6.57110895151815,2.44502632087632,61.3398717892601));
#145525=CARTESIAN_POINT('',(6.57110895151817,2.44502632087627,61.8868156729052));
#145526=CARTESIAN_POINT('',(6.57110895151814,2.44502632087636,50.));
#145527=CARTESIAN_POINT('',(7.01124948002266,0.00270025590217394,63.773534356882));
#145528=CARTESIAN_POINT('Ctrl Pts',(6.57110895151817,2.44502632087627,61.8868156729052));
#145529=CARTESIAN_POINT('Ctrl Pts',(6.50691218988431,2.61755776212454,61.8951901719231));
#145530=CARTESIAN_POINT('Ctrl Pts',(6.43587838748572,2.78766143545089,61.903564670941));
#145531=CARTESIAN_POINT('Ctrl Pts',(6.35821510578084,2.95478040319757,61.9119391699589));
#145532=CARTESIAN_POINT('Ctrl Pts',(6.28059813039113,3.12179972715606,61.9203086757267));
#145533=CARTESIAN_POINT('Ctrl Pts',(6.1963596950319,3.28583759643497,61.9286781814945));
#145534=CARTESIAN_POINT('Ctrl Pts',(6.10575546037758,3.44635703614257,61.9370476872623));
#145535=CARTESIAN_POINT('Ctrl Pts',(6.01519196982608,3.60680429135921,61.9454134293207));
#145536=CARTESIAN_POINT('Ctrl Pts',(5.91826854952778,3.76373598624047,61.9537791713792));
#145537=CARTESIAN_POINT('Ctrl Pts',(5.81528699583377,3.91663933986609,61.9621449134376));
#145538=CARTESIAN_POINT('Ctrl Pts',(5.71233667388179,4.0694963217103,61.9705081183747));
#145539=CARTESIAN_POINT('Ctrl Pts',(5.60333206608359,4.21832712642698,61.9788713233118));
#145540=CARTESIAN_POINT('Ctrl Pts',(5.48861876500483,4.36264720266685,61.9872345282489));
#145541=CARTESIAN_POINT('Ctrl Pts',(5.37322158177889,4.5078276666969,61.9956475918031));
#145542=CARTESIAN_POINT('Ctrl Pts',(5.25204759730724,4.64844315984357,62.0040606553572));
#145543=CARTESIAN_POINT('Ctrl Pts',(5.12549076997958,4.78403291474402,62.0124737189114));
#145544=CARTESIAN_POINT('Ctrl Pts',(4.99968093332064,4.91882236290619,62.0208371250895));
#145545=CARTESIAN_POINT('Ctrl Pts',(4.86855187424113,5.04864501876509,62.0292005312675));
#145546=CARTESIAN_POINT('Ctrl Pts',(4.73252882630589,5.17308394197154,62.0375639374456));
#145547=CARTESIAN_POINT('Ctrl Pts',(4.59648557025939,5.29754135230678,62.0459285861237));
#145548=CARTESIAN_POINT('Ctrl Pts',(4.45554711813616,5.41661321313302,62.0542932348018));
#145549=CARTESIAN_POINT('Ctrl Pts',(4.31017345618164,5.52992145876659,62.0626578834799));
#145550=CARTESIAN_POINT('Ctrl Pts',(4.16475881112236,5.64326164776349,62.0710248902831));
#145551=CARTESIAN_POINT('Ctrl Pts',(4.01490672227784,5.75083477951493,62.0793918970863));
#145552=CARTESIAN_POINT('Ctrl Pts',(3.86110828640053,5.85230461982193,62.0877589038894));
#145553=CARTESIAN_POINT('Ctrl Pts',(3.70580092859063,5.95476998434649,62.0962079996943));
#145554=CARTESIAN_POINT('Ctrl Pts',(3.54646965994457,6.0510114686339,62.1046570954993));
#145555=CARTESIAN_POINT('Ctrl Pts',(3.38364764720855,6.1407292044219,62.1131061913042));
#145556=CARTESIAN_POINT('Ctrl Pts',(3.22218795096895,6.22969628033639,62.1214845943176));
#145557=CARTESIAN_POINT('Ctrl Pts',(3.05729601733866,6.312248251256,62.1298629973311));
#145558=CARTESIAN_POINT('Ctrl Pts',(2.88951408629364,6.38814017595189,62.1382414003445));
#145559=CARTESIAN_POINT('Ctrl Pts',(2.71960866470156,6.46499260803786,62.1467258425452));
#145560=CARTESIAN_POINT('Ctrl Pts',(2.54673991877884,6.53501513325592,62.1552102847459));
#145561=CARTESIAN_POINT('Ctrl Pts',(2.37148933148852,6.59800461602871,62.1636947269465));
#145562=CARTESIAN_POINT('Ctrl Pts',(2.19623874419813,6.66099409880152,62.1721791691472));
#145563=CARTESIAN_POINT('Ctrl Pts',(2.0186066570039,6.71695046741193,62.1806636113479));
#145564=CARTESIAN_POINT('Ctrl Pts',(1.83918801382947,6.76572346554942,62.1891480535485));
#145565=CARTESIAN_POINT('Ctrl Pts',(1.66195048764615,6.81390355085988,62.1975293539535));
#145566=CARTESIAN_POINT('Ctrl Pts',(1.48261202793872,6.85517116373265,62.2059106543584));
#145567=CARTESIAN_POINT('Ctrl Pts',(1.30173764763051,6.88934725930123,62.2142919547633));
#145568=CARTESIAN_POINT('Ctrl Pts',(1.12109249912092,6.92348004167176,62.222662633097));
#145569=CARTESIAN_POINT('Ctrl Pts',(0.938915628636189,6.95053915747266,
62.2310333114306));
#145570=CARTESIAN_POINT('Ctrl Pts',(0.755786438088463,6.97039549971891,
62.2394039897642));
#145571=CARTESIAN_POINT('Ctrl Pts',(0.572865067730339,6.99022930842586,
62.2477651688151));
#145572=CARTESIAN_POINT('Ctrl Pts',(0.388993855063862,7.00287659997775,
62.256126347866));
#145573=CARTESIAN_POINT('Ctrl Pts',(0.204762051795161,7.00825934627455,
62.2644875269168));
#145574=CARTESIAN_POINT('Ctrl Pts',(0.0207693110235397,7.01363510782308,
62.2728378563516));
#145575=CARTESIAN_POINT('Ctrl Pts',(-0.163582761091555,7.01176511695458,
62.2811881857864));
#145576=CARTESIAN_POINT('Ctrl Pts',(-0.347700215973515,7.00262316009594,
62.2895385152211));
#145577=CARTESIAN_POINT('Ctrl Pts',(-0.531676003487666,6.99348823742623,
62.2978824195769));
#145578=CARTESIAN_POINT('Ctrl Pts',(-0.715417207661931,6.97709251544554,
62.3062263239327));
#145579=CARTESIAN_POINT('Ctrl Pts',(-0.898329147986046,6.95346182159496,
62.3145702282885));
#145580=CARTESIAN_POINT('Ctrl Pts',(-1.08109417229915,6.92985010806502,
62.3229074307683));
#145581=CARTESIAN_POINT('Ctrl Pts',(-1.26303093713436,6.89901505408378,
62.331244633248));
#145582=CARTESIAN_POINT('Ctrl Pts',(-1.44354899992312,6.86103438610542,
62.3395818357278));
#145583=CARTESIAN_POINT('Ctrl Pts',(-1.50297454974923,6.84853135985692,
62.3423263967635));
#145584=CARTESIAN_POINT('Ctrl Pts',(-1.56224640000419,6.83525438799622,
62.3450709577992));
#145585=CARTESIAN_POINT('Ctrl Pts',(-1.62134364638829,6.82120746956258,
62.3478155188349));
#145586=CARTESIAN_POINT('Ctrl Pts',(-1.80088827007231,6.77853122255614,
62.3561538291368));
#145587=CARTESIAN_POINT('Ctrl Pts',(-1.97867313897258,6.72877946772584,
62.3644921394386));
#145588=CARTESIAN_POINT('Ctrl Pts',(-2.1541298738823,6.6721324214188,62.3728304497405));
#145589=CARTESIAN_POINT('Ctrl Pts',(-2.32969700021576,6.61544973471245,
62.3811740062242));
#145590=CARTESIAN_POINT('Ctrl Pts',(-2.50293275906428,6.55186320395057,
62.3895175627079));
#145591=CARTESIAN_POINT('Ctrl Pts',(-2.67328714752016,6.4816018382344,62.3978611191917));
#145592=CARTESIAN_POINT('Ctrl Pts',(-2.84377114085238,6.41128701797739,
62.4062110234168));
#145593=CARTESIAN_POINT('Ctrl Pts',(-3.01136908864337,6.3342873582309,62.414560927642));
#145594=CARTESIAN_POINT('Ctrl Pts',(-3.17555365440632,6.25087878225827,
62.4229108318672));
#145595=CARTESIAN_POINT('Ctrl Pts',(-3.3399844848681,6.167345099594,62.4312732603307));
#145596=CARTESIAN_POINT('Ctrl Pts',(-3.50099140991984,6.07738343963517,
62.4396356887943));
#145597=CARTESIAN_POINT('Ctrl Pts',(-3.65807295567938,5.9813149736013,62.4479981172579));
#145598=CARTESIAN_POINT('Ctrl Pts',(-3.81528882757404,5.88516435593284,
62.4563676967378));
#145599=CARTESIAN_POINT('Ctrl Pts',(-3.96857235071375,5.78289669405816,
62.4647372762177));
#145600=CARTESIAN_POINT('Ctrl Pts',(-4.11745300246685,5.67487509421809,
62.4731068556977));
#145601=CARTESIAN_POINT('Ctrl Pts',(-4.26656328448577,5.56668688422153,
62.4814893442342));
#145602=CARTESIAN_POINT('Ctrl Pts',(-4.41125686798621,5.45272720420105,
62.4898718327707));
#145603=CARTESIAN_POINT('Ctrl Pts',(-4.55109704854791,5.33339874912785,
62.4982543213072));
#145604=CARTESIAN_POINT('Ctrl Pts',(-4.59685504705112,5.29435252330993,
62.5009972089119));
#145605=CARTESIAN_POINT('Ctrl Pts',(-4.64209369023455,5.25473174629258,
62.5037400965166));
#145606=CARTESIAN_POINT('Ctrl Pts',(-4.68679857597168,5.21455133935508,
62.5064829841214));
#145607=CARTESIAN_POINT('Ctrl Pts',(-4.82354042219802,5.09164882129327,
62.5148728392542));
#145608=CARTESIAN_POINT('Ctrl Pts',(-4.95556165108419,4.96325958096101,
62.523262694387));
#145609=CARTESIAN_POINT('Ctrl Pts',(-5.08241371095019,4.82977198563717,
62.5316525495197));
#145610=CARTESIAN_POINT('Ctrl Pts',(-5.20914871351373,4.69640757079486,
62.5400346626118));
#145611=CARTESIAN_POINT('Ctrl Pts',(-5.33072383076614,4.5579544168971,62.5484167757039));
#145612=CARTESIAN_POINT('Ctrl Pts',(-5.44672584142539,4.41483908776401,
62.556798888796));
#145613=CARTESIAN_POINT('Ctrl Pts',(-5.56263785911027,4.27183478579391,
62.5651744991449));
#145614=CARTESIAN_POINT('Ctrl Pts',(-5.67298518379294,4.12417577396186,
62.5735501094938));
#145615=CARTESIAN_POINT('Ctrl Pts',(-5.77739322365019,3.97232351424464,
62.5819257198426));
#145616=CARTESIAN_POINT('Ctrl Pts',(-5.88173558929987,3.82056677185385,
62.5902960618082));
#145617=CARTESIAN_POINT('Ctrl Pts',(-5.98014593340554,3.66462231092458,
62.5986664037738));
#145618=CARTESIAN_POINT('Ctrl Pts',(-6.07229127951136,3.50498290712956,
62.6070367457394));
#145619=CARTESIAN_POINT('Ctrl Pts',(-6.16439217229915,3.34542051754617,
62.6154030496337));
#145620=CARTESIAN_POINT('Ctrl Pts',(-6.25023393020028,3.18216702395701,
62.623769353528));
#145621=CARTESIAN_POINT('Ctrl Pts',(-6.32952784024959,3.01574267503137,
62.6321356574223));
#145622=CARTESIAN_POINT('Ctrl Pts',(-6.40879957401472,2.84936487033156,
62.640499621496));
#145623=CARTESIAN_POINT('Ctrl Pts',(-6.48152696887035,2.6798182743762,62.6488635855696));
#145624=CARTESIAN_POINT('Ctrl Pts',(-6.5474678242823,2.50764663628831,62.6572275496432));
#145625=CARTESIAN_POINT('Ctrl Pts',(-6.61339853249239,2.33550149255439,
62.6655902266417));
#145626=CARTESIAN_POINT('Ctrl Pts',(-6.67254466594148,2.1607324189128,62.6739529036403));
#145627=CARTESIAN_POINT('Ctrl Pts',(-6.72471247731919,1.98390238164271,
62.6823155806388));
#145628=CARTESIAN_POINT('Ctrl Pts',(-6.77687921465701,1.8070759849799,62.6906780854651));
#145629=CARTESIAN_POINT('Ctrl Pts',(-6.82206782379463,1.62818902462807,
62.6990405902914));
#145630=CARTESIAN_POINT('Ctrl Pts',(-6.86013454488729,1.44781925271909,
62.7074030951177));
#145631=CARTESIAN_POINT('Ctrl Pts',(-6.89820555627872,1.26742915228726,
62.7157665424377));
#145632=CARTESIAN_POINT('Ctrl Pts',(-6.92915301199316,1.08555622877291,
62.7241299897576));
#145633=CARTESIAN_POINT('Ctrl Pts',(-6.95288426097044,0.902788466945334,
62.7324934370776));
#145634=CARTESIAN_POINT('Ctrl Pts',(-6.97662948357404,0.719913086323296,
62.7408618090304));
#145635=CARTESIAN_POINT('Ctrl Pts',(-6.99314996540047,0.536142140642771,
62.7492301809832));
#145636=CARTESIAN_POINT('Ctrl Pts',(-7.00240482998677,0.352069821879175,
62.757598552936));
#145637=CARTESIAN_POINT('Ctrl Pts',(-7.01166246757238,0.167942350238086,
62.7659694322718));
#145638=CARTESIAN_POINT('Ctrl Pts',(-7.01365013587316,-0.0164863459675034,
62.7743403116075));
#145639=CARTESIAN_POINT('Ctrl Pts',(-7.00837910332975,-0.200621301239111,
62.7827111909433));
#145640=CARTESIAN_POINT('Ctrl Pts',(-7.00310360469747,-0.384912272067153,
62.7910891628346));
#145641=CARTESIAN_POINT('Ctrl Pts',(-6.99055713077681,-0.568908676021576,
62.7994671347259));
#145642=CARTESIAN_POINT('Ctrl Pts',(-6.97080299477925,-0.752018730136862,
62.8078451066172));
#145643=CARTESIAN_POINT('Ctrl Pts',(-6.95824908049424,-0.868386660598136,
62.8131693759762));
#145644=CARTESIAN_POINT('Ctrl Pts',(-6.94278524829728,-0.984396730672524,
62.8184936453352));
#145645=CARTESIAN_POINT('Ctrl Pts',(-6.92443852335641,-1.09989894933928,
62.8238179146942));
#145646=CARTESIAN_POINT('Ctrl Pts',(-6.8973442515681,-1.27047154552732,
62.8316807458835));
#145647=CARTESIAN_POINT('Ctrl Pts',(-6.86390358510918,-1.44029073648694,
62.8395435770729));
#145648=CARTESIAN_POINT('Ctrl Pts',(-6.82417039470791,-1.60882720840124,
62.8474064082622));
#145649=CARTESIAN_POINT('Ctrl Pts',(-6.78446773401874,-1.7772341822834,
62.8552631979036));
#145650=CARTESIAN_POINT('Ctrl Pts',(-6.73848225135099,-1.94436002842866,
62.8631199875451));
#145651=CARTESIAN_POINT('Ctrl Pts',(-6.68631940867443,-2.10968228121764,
62.8709767771865));
#145652=CARTESIAN_POINT('Ctrl Pts',(-6.63418598337189,-2.27491130008196,
62.8788291359706));
#145653=CARTESIAN_POINT('Ctrl Pts',(-6.57588224238199,-2.43833838644849,
62.8866814947546));
#145654=CARTESIAN_POINT('Ctrl Pts',(-6.51156428959697,-2.59945322422727,
62.8945338535386));
#145655=CARTESIAN_POINT('Ctrl Pts',(-6.44726152303103,-2.76053002091305,
62.9023843582891));
#145656=CARTESIAN_POINT('Ctrl Pts',(-6.3769475043088,-2.91929529869549,
62.9102348630396));
#145657=CARTESIAN_POINT('Ctrl Pts',(-6.30082755024359,-3.07525588278299,
62.91808536779));
#145658=CARTESIAN_POINT('Ctrl Pts',(-6.22471984147991,-3.23119137772794,
62.9259346096417));
#145659=CARTESIAN_POINT('Ctrl Pts',(-6.14280822672519,-3.38432273560712,
62.9337838514934));
#145660=CARTESIAN_POINT('Ctrl Pts',(-6.05534512566555,-3.5341791085878,
62.9416330933451));
#145661=CARTESIAN_POINT('Ctrl Pts',(-5.9678525565752,-3.68408597111377,
62.94948497976));
#145662=CARTESIAN_POINT('Ctrl Pts',(-5.87480495764768,-3.83071531495389,
62.957336866175));
#145663=CARTESIAN_POINT('Ctrl Pts',(-5.77649954844859,-3.9736229727131,
62.9651887525899));
#145664=CARTESIAN_POINT('Ctrl Pts',(-5.70431511006091,-4.07855828706345,
62.9709542950535));
#145665=CARTESIAN_POINT('Ctrl Pts',(-5.6292967177402,-4.1814874955188,62.9767198375172));
#145666=CARTESIAN_POINT('Ctrl Pts',(-5.55157631074634,-4.28224555910332,
62.9824853799808));
#145667=CARTESIAN_POINT('Ctrl Pts',(-5.4214213098565,-4.45098072613015,
62.9921406843405));
#145668=CARTESIAN_POINT('Ctrl Pts',(-5.28375446150655,-4.61354048174883,
63.0017959887003));
#145669=CARTESIAN_POINT('Ctrl Pts',(-5.13914797928086,-4.76935893066914,
63.01145129306));
#145670=CARTESIAN_POINT('Ctrl Pts',(-4.99374040427196,-4.92604058456477,
63.0211600859945));
#145671=CARTESIAN_POINT('Ctrl Pts',(-4.84131616607317,-5.07590603636646,
63.030868878929));
#145672=CARTESIAN_POINT('Ctrl Pts',(-4.68248723673392,-5.21842311817698,
63.0405776718636));
#145673=CARTESIAN_POINT('Ctrl Pts',(-4.52289400910047,-5.36162600428635,
63.0503331843341));
#145674=CARTESIAN_POINT('Ctrl Pts',(-4.35683435041004,-5.49740961724818,
63.0600886968046));
#145675=CARTESIAN_POINT('Ctrl Pts',(-4.18495860075941,-5.6252775995883,
63.0698442092751));
#145676=CARTESIAN_POINT('Ctrl Pts',(-4.01291266767407,-5.75327219090302,
63.0796093812038));
#145677=CARTESIAN_POINT('Ctrl Pts',(-3.83503916209638,-5.87333546050407,
63.0893745531325));
#145678=CARTESIAN_POINT('Ctrl Pts',(-3.65201913516281,-5.98501318285137,
63.0991397250612));
#145679=CARTESIAN_POINT('Ctrl Pts',(-3.46924865188348,-6.09653863515807,
63.1088915823995));
#145680=CARTESIAN_POINT('Ctrl Pts',(-3.28134570445317,-6.19970137194527,
63.1186434397378));
#145681=CARTESIAN_POINT('Ctrl Pts',(-3.08901667891444,-6.29409266851771,
63.1283952970762));
#145682=CARTESIAN_POINT('Ctrl Pts',(-3.00514729462933,-6.3352541099758,
63.1326478131398));
#145683=CARTESIAN_POINT('Ctrl Pts',(-2.92043660940189,-6.37474814420639,
63.1369003292034));
#145684=CARTESIAN_POINT('Ctrl Pts',(-2.83494485713366,-6.41254350624707,
63.141152845267));
#145685=CARTESIAN_POINT('Ctrl Pts',(-2.6734500775664,-6.4839393251358,63.1491858908659));
#145686=CARTESIAN_POINT('Ctrl Pts',(-2.50908783830633,-6.54930506614085,
63.1572189364648));
#145687=CARTESIAN_POINT('Ctrl Pts',(-2.34235612441156,-6.60840331312577,
63.1652519820637));
#145688=CARTESIAN_POINT('Ctrl Pts',(-2.17573159208224,-6.66746356948204,
63.1732798637116));
#145689=CARTESIAN_POINT('Ctrl Pts',(-2.00674096113006,-6.72026422965895,
63.1813077453595));
#145690=CARTESIAN_POINT('Ctrl Pts',(-1.83590305421743,-6.76661558964414,
63.1893356270073));
#145691=CARTESIAN_POINT('Ctrl Pts',(-1.66514228230398,-6.81294602153334,
63.1973598839875));
#145692=CARTESIAN_POINT('Ctrl Pts',(-1.49253624819078,-6.85283285541565,
63.2053841409677));
#145693=CARTESIAN_POINT('Ctrl Pts',(-1.31861978180878,-6.88613595810616,
63.2134083979479));
#145694=CARTESIAN_POINT('Ctrl Pts',(-1.14472434369888,-6.91943503411236,
63.2214316847137));
#145695=CARTESIAN_POINT('Ctrl Pts',(-0.969519147282888,-6.94615188802948,
63.2294549714794));
#145696=CARTESIAN_POINT('Ctrl Pts',(-0.793550262853192,-6.96619727992437,
63.2374782582452));
#145697=CARTESIAN_POINT('Ctrl Pts',(-0.617595797503796,-6.98624102927821,
63.2455008875742));
#145698=CARTESIAN_POINT('Ctrl Pts',(-0.4408781335326,-6.99961436801203,
63.2535235169032));
#145699=CARTESIAN_POINT('Ctrl Pts',(-0.263949225982252,-7.0062798522899,
63.2615461462322));
#145700=CARTESIAN_POINT('Ctrl Pts',(-0.0869538057588191,-7.01294784231532,
63.2695717914987));
#145701=CARTESIAN_POINT('Ctrl Pts',(0.0902526500143067,-7.01290292960822,
63.2775974367652));
#145702=CARTESIAN_POINT('Ctrl Pts',(0.267117029018896,-7.00615979373209,
63.2856230820317));
#145703=CARTESIAN_POINT('Ctrl Pts',(0.371407044452844,-7.00218362991351,
63.290355491539));
#145704=CARTESIAN_POINT('Ctrl Pts',(0.475578137019581,-6.99587948197759,
63.2950879010463));
#145705=CARTESIAN_POINT('Ctrl Pts',(0.579517602900145,-6.98725882663788,
63.2998203105537));
#145706=CARTESIAN_POINT('Ctrl Pts',(0.771258535625853,-6.97135598856246,
63.3085503593882));
#145707=CARTESIAN_POINT('Ctrl Pts',(0.962306806828307,-6.94755946216096,
63.3172804082228));
#145708=CARTESIAN_POINT('Ctrl Pts',(1.15202145315067,-6.91595786091707,
63.3260104570573));
#145709=CARTESIAN_POINT('Ctrl Pts',(1.3417909556994,-6.88434712203081,63.3347430301963));
#145710=CARTESIAN_POINT('Ctrl Pts',(1.53022579343208,-6.84492684852486,
63.3434756033354));
#145711=CARTESIAN_POINT('Ctrl Pts',(1.71669433998222,-6.79783694314397,
63.3522081764744));
#145712=CARTESIAN_POINT('Ctrl Pts',(1.90581196989943,-6.75007805048663,
63.3610648097549));
#145713=CARTESIAN_POINT('Ctrl Pts',(2.09290673320342,-6.69443001733442,
63.3699214430354));
#145714=CARTESIAN_POINT('Ctrl Pts',(2.27733429665622,-6.63109154391442,
63.3787780763158));
#145715=CARTESIAN_POINT('Ctrl Pts',(2.45929423137669,-6.56860053512469,
63.3875162084224));
#145716=CARTESIAN_POINT('Ctrl Pts',(2.63865764173921,-6.49862371531824,
63.3962543405291));
#145717=CARTESIAN_POINT('Ctrl Pts',(2.81482368313845,-6.42140126415901,
63.4049924726357));
#145718=CARTESIAN_POINT('Ctrl Pts',(2.99457330780912,-6.34260794791162,
63.4139083565031));
#145719=CARTESIAN_POINT('Ctrl Pts',(3.17099381508166,-6.25627117582712,
63.4228242403704));
#145720=CARTESIAN_POINT('Ctrl Pts',(3.34347019430442,-6.16269694389542,
63.4317401242378));
#145721=CARTESIAN_POINT('Ctrl Pts',(3.51594657352718,-6.06912271196373,
63.4406560081052));
#145722=CARTESIAN_POINT('Ctrl Pts',(3.68447856178892,-5.9683111697436,63.4495718919725));
#145723=CARTESIAN_POINT('Ctrl Pts',(3.84847863845254,-5.86061760669253,
63.4584877758399));
#145724=CARTESIAN_POINT('Ctrl Pts',(4.00925607216609,-5.75504024937012,
63.4672284603362));
#145725=CARTESIAN_POINT('Ctrl Pts',(4.16569512362393,-5.64283761417378,
63.4759691448325));
#145726=CARTESIAN_POINT('Ctrl Pts',(4.3172683113901,-5.52438420911932,63.4847098293288));
#145727=CARTESIAN_POINT('Ctrl Pts',(4.46881422862211,-5.40595211579999,
63.4934489412307));
#145728=CARTESIAN_POINT('Ctrl Pts',(4.61549581484821,-5.28127166710137,
63.5021880531327));
#145729=CARTESIAN_POINT('Ctrl Pts',(4.75681747821264,-5.15075858893336,
63.5109271650346));
#145730=CARTESIAN_POINT('Ctrl Pts',(4.89997016712154,-5.01855452599823,
63.519779504709));
#145731=CARTESIAN_POINT('Ctrl Pts',(5.03762284929539,-4.8803658166327,63.5286318443833));
#145732=CARTESIAN_POINT('Ctrl Pts',(5.16929682606274,-4.73666516513018,
63.5374841840576));
#145733=CARTESIAN_POINT('Ctrl Pts',(5.2992199716851,-4.594875260021,63.5462188167074));
#145734=CARTESIAN_POINT('Ctrl Pts',(5.42332223922286,-4.44771930043756,
63.5549534493572));
#145735=CARTESIAN_POINT('Ctrl Pts',(5.54118175104932,-4.29568753104064,
63.5636880820071));
#145736=CARTESIAN_POINT('Ctrl Pts',(5.66142365713336,-4.14058261456575,
63.5725992751936));
#145737=CARTESIAN_POINT('Ctrl Pts',(5.77516754427281,-3.98040288733585,
63.5815104683802));
#145738=CARTESIAN_POINT('Ctrl Pts',(5.88200887951174,-3.81570414259872,
63.5904216615667));
#145739=CARTESIAN_POINT('Ctrl Pts',(5.98885021475063,-3.65100539786166,
63.5993328547533));
#145740=CARTESIAN_POINT('Ctrl Pts',(6.08878882181403,-3.48178788259178,
63.6082440479399));
#145741=CARTESIAN_POINT('Ctrl Pts',(6.18146681589444,-3.30863938296332,
63.6171552411264));
#145742=CARTESIAN_POINT('Ctrl Pts',(6.26488837546854,-3.15278450047213,
63.6251764077546));
#145743=CARTESIAN_POINT('Ctrl Pts',(6.34246548234576,-2.99367208680069,
63.6331975743829));
#145744=CARTESIAN_POINT('Ctrl Pts',(6.41393773392161,-2.8317890648628,63.6412187410111));
#145745=CARTESIAN_POINT('Ctrl Pts',(6.48538716206193,-2.66995773748654,
63.6492373462176));
#145746=CARTESIAN_POINT('Ctrl Pts',(6.55073546808279,-2.50535789862939,
63.6572559514241));
#145747=CARTESIAN_POINT('Ctrl Pts',(6.60976914815376,-2.33849917053966,
63.6652745566305));
#145748=CARTESIAN_POINT('Ctrl Pts',(6.66879529367676,-2.17166173885381,
63.6732921384117));
#145749=CARTESIAN_POINT('Ctrl Pts',(6.72150829684188,-2.00256633831411,
63.6813097201928));
#145750=CARTESIAN_POINT('Ctrl Pts',(6.76774358430884,-1.83174052189346,
63.6893273019739));
#145751=CARTESIAN_POINT('Ctrl Pts',(6.81399538839174,-1.66085368142483,
63.697347747873));
#145752=CARTESIAN_POINT('Ctrl Pts',(6.85376475567758,-1.48823554410405,
63.7053681937721));
#145753=CARTESIAN_POINT('Ctrl Pts',(6.88693748412361,-1.31442711942242,
63.7133886396712));
#145754=CARTESIAN_POINT('Ctrl Pts',(6.92011674764756,-1.14058445421699,
63.7214106656104));
#145755=CARTESIAN_POINT('Ctrl Pts',(6.9466967234212,-0.965551396643878,
63.7294326915495));
#145756=CARTESIAN_POINT('Ctrl Pts',(6.96661476310131,-0.789876765729247,
63.7374547174887));
#145757=CARTESIAN_POINT('Ctrl Pts',(6.98654811079227,-0.614067120064253,
63.7454829087565));
#145758=CARTESIAN_POINT('Ctrl Pts',(6.99980926583188,-0.437615281936497,
63.7535111000242));
#145759=CARTESIAN_POINT('Ctrl Pts',(7.00638760501589,-0.261073343678946,
63.761539291292));
#145760=CARTESIAN_POINT('Ctrl Pts',(7.00966387681666,-0.173148510710257,
63.7655376464887));
#145761=CARTESIAN_POINT('Ctrl Pts',(7.01128333372664,-0.0852013256471142,
63.7695360016853));
#145762=CARTESIAN_POINT('Ctrl Pts',(7.01124948002266,0.00270025590207967,
63.773534356882));
#145763=CARTESIAN_POINT('Ctrl Pts',(7.01124948002242,0.00270025652918008,
63.7735343569105));
#145764=CARTESIAN_POINT('Ctrl Pts',(7.01124302160633,0.0194696138023747,
63.7742971400779));
#145765=CARTESIAN_POINT('Ctrl Pts',(7.01117640060358,0.0362375540536934,
63.7750599232454));
#145766=CARTESIAN_POINT('Ctrl Pts',(7.01104964859508,0.0530036549197061,
63.7758227064129));
#145767=CARTESIAN_POINT('Ctrl Pts',(7.00942846247404,0.267445779739449,
63.7855788712198));
#145768=CARTESIAN_POINT('Ctrl Pts',(6.99796556449339,0.481668111792948,
63.7953350360268));
#145769=CARTESIAN_POINT('Ctrl Pts',(6.97673294021471,0.694855411882936,
63.8050912008337));
#145770=CARTESIAN_POINT('Ctrl Pts',(6.95548118222794,0.908234824992813,
63.8148561573758));
#145771=CARTESIAN_POINT('Ctrl Pts',(6.9244421066821,1.12057730384373,63.8246211139179));
#145772=CARTESIAN_POINT('Ctrl Pts',(6.88373949701866,1.33107366425954,63.83438607046));
#145773=CARTESIAN_POINT('Ctrl Pts',(6.84311081382055,1.54118770884795,63.8441332913157));
#145774=CARTESIAN_POINT('Ctrl Pts',(6.79285368022903,1.74946229878537,63.8538805121713));
#145775=CARTESIAN_POINT('Ctrl Pts',(6.73314228653791,1.95510140702088,63.863627733027));
#145776=CARTESIAN_POINT('Ctrl Pts',(6.68518950162099,2.12024523164395,63.8714554917902));
#145777=CARTESIAN_POINT('Ctrl Pts',(6.63114033388791,2.28368950797833,63.8792832505535));
#145778=CARTESIAN_POINT('Ctrl Pts',(6.57110895151817,2.44502632087628,63.8871110093167));
#145779=CARTESIAN_POINT('',(7.01124858877574,-0.00444847055471408,63.2264656430603));
#145780=CARTESIAN_POINT('Ctrl Pts',(6.57110895151814,2.44502632087636,63.3399907370491));
#145781=CARTESIAN_POINT('Ctrl Pts',(6.63484048754942,2.27374519259836,63.331705647918));
#145782=CARTESIAN_POINT('Ctrl Pts',(6.69187315219911,2.09996518305276,63.3234205587869));
#145783=CARTESIAN_POINT('Ctrl Pts',(6.7420259826953,1.92424328273777,63.3151354696559));
#145784=CARTESIAN_POINT('Ctrl Pts',(6.79219731414985,1.74845656008818,63.306847324225));
#145785=CARTESIAN_POINT('Ctrl Pts',(6.83548364555182,1.5707268398795,63.298559178794));
#145786=CARTESIAN_POINT('Ctrl Pts',(6.87175418446422,1.39162530546065,63.2902710333631));
#145787=CARTESIAN_POINT('Ctrl Pts',(6.90803158763612,1.21248987578013,63.281981319387));
#145788=CARTESIAN_POINT('Ctrl Pts',(6.93729048961663,1.03198244662936,63.2736916054108));
#145789=CARTESIAN_POINT('Ctrl Pts',(6.95945146872979,0.850683147179211,
63.2654018914347));
#145790=CARTESIAN_POINT('Ctrl Pts',(6.98162775056118,0.669258655963964,
63.2571064532007));
#145791=CARTESIAN_POINT('Ctrl Pts',(6.99669628152373,0.487041538204856,
63.2488110149668));
#145792=CARTESIAN_POINT('Ctrl Pts',(7.00462955623186,0.304616714024459,
63.2405155767329));
#145793=CARTESIAN_POINT('Ctrl Pts',(7.00910840272075,0.201626106321506,
63.2358322655185));
#145794=CARTESIAN_POINT('Ctrl Pts',(7.01131395111323,0.0985693323568585,
63.231148954304));
#145795=CARTESIAN_POINT('Ctrl Pts',(7.01124858877614,-0.00444846991103996,
63.2264656430896));
#145796=CARTESIAN_POINT('Ctrl Pts',(7.01124858877573,-0.00444847055461616,
63.2264656430603));
#145797=CARTESIAN_POINT('Ctrl Pts',(7.01109817222254,-0.241520478426499,
63.2156880690037));
#145798=CARTESIAN_POINT('Ctrl Pts',(6.99891979679981,-0.478179014153952,
63.204910494947));
#145799=CARTESIAN_POINT('Ctrl Pts',(6.97486124731762,-0.713398306114453,
63.1941329208903));
#145800=CARTESIAN_POINT('Ctrl Pts',(6.95038805171756,-0.952671573412448,
63.1831695966808));
#145801=CARTESIAN_POINT('Ctrl Pts',(6.91362159641276,-1.19045596327219,
63.1722062724713));
#145802=CARTESIAN_POINT('Ctrl Pts',(6.86476735118868,-1.42569133284663,
63.1612429482619));
#145803=CARTESIAN_POINT('Ctrl Pts',(6.84754912786283,-1.50859784606554,
63.1573790268408));
#145804=CARTESIAN_POINT('Ctrl Pts',(6.82882987787831,-1.59118788006927,
63.1535151054197));
#145805=CARTESIAN_POINT('Ctrl Pts',(6.80862007451927,-1.67341544254653,
63.1496511839986));
#145806=CARTESIAN_POINT('Ctrl Pts',(6.76478263203099,-1.85177670499975,
63.1412698835937));
#145807=CARTESIAN_POINT('Ctrl Pts',(6.71388127875477,-2.0286222625827,63.1328885831888));
#145808=CARTESIAN_POINT('Ctrl Pts',(6.65603350584824,-2.20337117425222,
63.1245072827839));
#145809=CARTESIAN_POINT('Ctrl Pts',(6.59825904652563,-2.37789861725739,
63.1161366044503));
#145810=CARTESIAN_POINT('Ctrl Pts',(6.53355581430722,-2.5503344013266,63.1077659261167));
#145811=CARTESIAN_POINT('Ctrl Pts',(6.46209194964979,-2.72010922515463,
63.0993952477831));
#145812=CARTESIAN_POINT('Ctrl Pts',(6.39070918420901,-2.88969138370652,
63.0910340687323));
#145813=CARTESIAN_POINT('Ctrl Pts',(6.31258120412595,-3.05661830052571,
63.0826728896814));
#145814=CARTESIAN_POINT('Ctrl Pts',(6.22792559518153,-3.22033683694466,
63.0743117106306));
#145815=CARTESIAN_POINT('Ctrl Pts',(6.14337983687574,-3.38384292925029,
63.0659613811959));
#145816=CARTESIAN_POINT('Ctrl Pts',(6.05232349453927,-3.54414865553281,
63.0576110517611));
#145817=CARTESIAN_POINT('Ctrl Pts',(5.95502174312746,-3.70072190273455,
63.0492607223264));
#145818=CARTESIAN_POINT('Ctrl Pts',(5.85779485959307,-3.85717467618828,
63.0409168179707));
#145819=CARTESIAN_POINT('Ctrl Pts',(5.75433231561575,-4.00990041666434,
63.0325729136149));
#145820=CARTESIAN_POINT('Ctrl Pts',(5.64494515016839,-4.15839161384427,
63.0242290092592));
#145821=CARTESIAN_POINT('Ctrl Pts',(5.53564584517409,-4.30676354196915,
63.0158918067795));
#145822=CARTESIAN_POINT('Ctrl Pts',(5.42043160301229,-4.45090744699308,
63.0075546042997));
#145823=CARTESIAN_POINT('Ctrl Pts',(5.29965679182837,-4.59034469853055,
62.99921740182));
#145824=CARTESIAN_POINT('Ctrl Pts',(5.25989839064931,-4.63624667205952,
62.996472840784));
#145825=CARTESIAN_POINT('Ctrl Pts',(5.21953773998056,-4.68163883099359,
62.993728279748));
#145826=CARTESIAN_POINT('Ctrl Pts',(5.17858847666912,-4.72650483463307,
62.9909837187121));
#145827=CARTESIAN_POINT('Ctrl Pts',(5.05417963326997,-4.86281321161849,
62.9826454084102));
#145828=CARTESIAN_POINT('Ctrl Pts',(4.92443695716898,-4.99415069566876,
62.9743070981084));
#145829=CARTESIAN_POINT('Ctrl Pts',(4.78979374022895,-5.12010766376681,
62.9659687878066));
#145830=CARTESIAN_POINT('Ctrl Pts',(4.65506581034569,-5.24614387971507,
62.9576252313229));
#145831=CARTESIAN_POINT('Ctrl Pts',(4.5154314289632,-5.36679260359573,62.9492816748391));
#145832=CARTESIAN_POINT('Ctrl Pts',(4.37135764285154,-5.48168394937025,
62.9409381183554));
#145833=CARTESIAN_POINT('Ctrl Pts',(4.22717424603034,-5.5966627039807,62.9325882141302));
#145834=CARTESIAN_POINT('Ctrl Pts',(4.07854496339126,-5.70587513938718,
62.924238309905));
#145835=CARTESIAN_POINT('Ctrl Pts',(3.92596687286556,-5.8089939469466,62.9158884056798));
#145836=CARTESIAN_POINT('Ctrl Pts',(3.7731599264961,-5.91226742508571,62.9075259772162));
#145837=CARTESIAN_POINT('Ctrl Pts',(3.61639260808626,-6.00942882717345,
62.8991635487527));
#145838=CARTESIAN_POINT('Ctrl Pts',(3.45618901933156,-6.10019540876782,
62.8908011202891));
#145839=CARTESIAN_POINT('Ctrl Pts',(3.29584843466955,-6.19103960816273,
62.8824315408092));
#145840=CARTESIAN_POINT('Ctrl Pts',(3.13206600716901,-6.27547792632041,
62.8740619613293));
#145841=CARTESIAN_POINT('Ctrl Pts',(2.96538749690621,-6.35327502597616,
62.8656923818495));
#145842=CARTESIAN_POINT('Ctrl Pts',(2.79845190534932,-6.43119211817938,
62.857309893313));
#145843=CARTESIAN_POINT('Ctrl Pts',(2.6286116064732,-6.50244739625811,62.8489274047765));
#145844=CARTESIAN_POINT('Ctrl Pts',(2.45643057630671,-6.56685429915157,
62.84054491624));
#145845=CARTESIAN_POINT('Ctrl Pts',(2.40009012187456,-6.58792929315107,
62.8378020286353));
#145846=CARTESIAN_POINT('Ctrl Pts',(2.34349914849372,-6.60827143021681,
62.8350591410305));
#145847=CARTESIAN_POINT('Ctrl Pts',(2.28667769040812,-6.62787535358729,
62.8323162534258));
#145848=CARTESIAN_POINT('Ctrl Pts',(2.11287406792426,-6.68783919491554,
62.823926398293));
#145849=CARTESIAN_POINT('Ctrl Pts',(1.93656216285547,-6.74101356882585,
62.8155365431602));
#145850=CARTESIAN_POINT('Ctrl Pts',(1.75829916848905,-6.78719460429644,
62.8071466880274));
#145851=CARTESIAN_POINT('Ctrl Pts',(1.58020067271463,-6.83333302455495,
62.7987645749353));
#145852=CARTESIAN_POINT('Ctrl Pts',(1.40015499349829,-6.87249088908758,
62.7903824618432));
#145853=CARTESIAN_POINT('Ctrl Pts',(1.21873558913893,-6.90451375016852,
62.7820003487511));
#145854=CARTESIAN_POINT('Ctrl Pts',(1.0374569277867,-6.93651176829631,62.7736247384022));
#145855=CARTESIAN_POINT('Ctrl Pts',(0.854806988572278,-6.96138576163942,
62.7652491280533));
#145856=CARTESIAN_POINT('Ctrl Pts',(0.671371010195393,-6.97903199084008,
62.7568735177045));
#145857=CARTESIAN_POINT('Ctrl Pts',(0.488050415772942,-6.99666712030052,
62.7485031757389));
#145858=CARTESIAN_POINT('Ctrl Pts',(0.303945094410669,-7.00708351927796,
62.7401328337733));
#145859=CARTESIAN_POINT('Ctrl Pts',(0.119647482326063,-7.01022902924527,
62.7317624918077));
#145860=CARTESIAN_POINT('Ctrl Pts',(-0.064561219784228,-7.01337302173654,
62.7233961879134));
#145861=CARTESIAN_POINT('Ctrl Pts',(-0.248961699536415,-7.00925311447306,
62.7150298840191));
#145862=CARTESIAN_POINT('Ctrl Pts',(-0.432958966309935,-6.99786918254349,
62.7066635801247));
#145863=CARTESIAN_POINT('Ctrl Pts',(-0.616904774204914,-6.98648843438061,
62.6982996160511));
#145864=CARTESIAN_POINT('Ctrl Pts',(-0.800447266150583,-6.96784773125722,
62.6899356519775));
#145865=CARTESIAN_POINT('Ctrl Pts',(-0.982993461906868,-6.94199902163263,
62.6815716879039));
#145866=CARTESIAN_POINT('Ctrl Pts',(-1.1655115668371,-6.9161542896949,62.6732090109053));
#145867=CARTESIAN_POINT('Ctrl Pts',(-1.34703335593707,-6.88310380882911,
62.6648463339068));
#145868=CARTESIAN_POINT('Ctrl Pts',(-1.52697254641174,-6.84295122041688,
62.6564836569083));
#145869=CARTESIAN_POINT('Ctrl Pts',(-1.7069080322674,-6.80279945867305,
62.648121152082));
#145870=CARTESIAN_POINT('Ctrl Pts',(-1.8852606637958,-6.75554595291287,
62.6397586472557));
#145871=CARTESIAN_POINT('Ctrl Pts',(-2.06145547494011,-6.70134522967885,
62.6313961424294));
#145872=CARTESIAN_POINT('Ctrl Pts',(-2.23767014406945,-6.64713839776805,
62.6230326951094));
#145873=CARTESIAN_POINT('Ctrl Pts',(-2.41172619399862,-6.58598288447688,
62.6146692477894));
#145874=CARTESIAN_POINT('Ctrl Pts',(-2.58306450102135,-6.51808287351912,
62.6063058004694));
#145875=CARTESIAN_POINT('Ctrl Pts',(-2.75450369685442,-6.4501428811267,
62.5979374285166));
#145876=CARTESIAN_POINT('Ctrl Pts',(-2.92322164582076,-6.37545057568158,
62.5895690565638));
#145877=CARTESIAN_POINT('Ctrl Pts',(-3.08867890969278,-6.29425842775136,
62.581200684611));
#145878=CARTESIAN_POINT('Ctrl Pts',(-3.25418574888546,-6.21304195253158,
62.5728298052752));
#145879=CARTESIAN_POINT('Ctrl Pts',(-3.41642966212173,-6.12532190107686,
62.5644589259395));
#145880=CARTESIAN_POINT('Ctrl Pts',(-3.57489582793616,-6.03139671899508,
62.5560880466037));
#145881=CARTESIAN_POINT('Ctrl Pts',(-3.73349626041912,-5.9373919551223,
62.5477100747124));
#145882=CARTESIAN_POINT('Ctrl Pts',(-3.88831226941796,-5.83717172745508,
62.5393321028211));
#145883=CARTESIAN_POINT('Ctrl Pts',(-4.03885706116365,-5.73107845016874,
62.5309541309298));
#145884=CARTESIAN_POINT('Ctrl Pts',(-4.13452950220826,-5.66365530853291,
62.5256298615709));
#145885=CARTESIAN_POINT('Ctrl Pts',(-4.22847752742665,-5.59386107508764,
62.5203055922119));
#145886=CARTESIAN_POINT('Ctrl Pts',(-4.32058308092017,-5.52179213692134,
62.514981322853));
#145887=CARTESIAN_POINT('Ctrl Pts',(-4.45660370082002,-5.41536140312642,
62.5071184916636));
#145888=CARTESIAN_POINT('Ctrl Pts',(-4.58888712415343,-5.30374629795428,
62.4992556604743));
#145889=CARTESIAN_POINT('Ctrl Pts',(-4.71699660523524,-5.18725067725662,
62.491392829285));
#145890=CARTESIAN_POINT('Ctrl Pts',(-4.84500765109107,-5.07084456806625,
62.4835360396435));
#145891=CARTESIAN_POINT('Ctrl Pts',(-4.96885085226277,-4.94956565568039,
62.4756792500021));
#145892=CARTESIAN_POINT('Ctrl Pts',(-5.08812047633635,-4.82375958986212,
62.4678224603606));
#145893=CARTESIAN_POINT('Ctrl Pts',(-5.2073228379878,-4.69802447270971,
62.4599701015766));
#145894=CARTESIAN_POINT('Ctrl Pts',(-5.32195649182377,-4.56776755665584,
62.4521177427926));
#145895=CARTESIAN_POINT('Ctrl Pts',(-5.43165089415382,-4.43337288376897,
62.4442653840086));
#145896=CARTESIAN_POINT('Ctrl Pts',(-5.54131939635566,-4.29900994303236,
62.4364148792581));
#145897=CARTESIAN_POINT('Ctrl Pts',(-5.64605072073865,-4.16051147967919,
62.4285643745076));
#145898=CARTESIAN_POINT('Ctrl Pts',(-5.74551318440802,-4.01829625715845,
62.4207138697572));
#145899=CARTESIAN_POINT('Ctrl Pts',(-5.84495964770179,-3.87610391258475,
62.4128646279055));
#145900=CARTESIAN_POINT('Ctrl Pts',(-5.93913872139395,-3.73019631348123,
62.4050153860538));
#145901=CARTESIAN_POINT('Ctrl Pts',(-6.0277610946666,-3.58102258414042,
62.3971661442021));
#145902=CARTESIAN_POINT('Ctrl Pts',(-6.11641332655142,-3.4317985952504,
62.3893142577872));
#145903=CARTESIAN_POINT('Ctrl Pts',(-6.19950492345108,-3.27930660639255,
62.3814623713722));
#145904=CARTESIAN_POINT('Ctrl Pts',(-6.2767916365877,-3.12402197709343,
62.3736104849573));
#145905=CARTESIAN_POINT('Ctrl Pts',(-6.33354230807208,-3.00999840659495,
62.3678449424937));
#145906=CARTESIAN_POINT('Ctrl Pts',(-6.38716404762343,-2.89446966477233,
62.36207940003));
#145907=CARTESIAN_POINT('Ctrl Pts',(-6.43757652936332,-2.777631183417,62.3563138575664));
#145908=CARTESIAN_POINT('Ctrl Pts',(-6.52200013005579,-2.58196683690949,
62.3466585532067));
#145909=CARTESIAN_POINT('Ctrl Pts',(-6.59737977147073,-2.38272892650724,
62.337003248847));
#145910=CARTESIAN_POINT('Ctrl Pts',(-6.66349814332101,-2.18069233420431,
62.3273479444873));
#145911=CARTESIAN_POINT('Ctrl Pts',(-6.72998279854747,-1.97753649708229,
62.3176391515528));
#145912=CARTESIAN_POINT('Ctrl Pts',(-6.78710332592351,-1.77155094568032,
62.3079303586183));
#145913=CARTESIAN_POINT('Ctrl Pts',(-6.83469119427755,-1.56352897042712,
62.2982215656837));
#145914=CARTESIAN_POINT('Ctrl Pts',(-6.88250805949484,-1.3545059757657,
62.2884660532132));
#145915=CARTESIAN_POINT('Ctrl Pts',(-6.92070031476327,-1.14342695873469,
62.2787105407428));
#145916=CARTESIAN_POINT('Ctrl Pts',(-6.94914935517109,-0.931101391914558,
62.2689550282723));
#145917=CARTESIAN_POINT('Ctrl Pts',(-6.97762656450572,-0.718565590117578,
62.2591898563436));
#145918=CARTESIAN_POINT('Ctrl Pts',(-6.99634126819928,-0.504780809182639,
62.2494246844149));
#145919=CARTESIAN_POINT('Ctrl Pts',(-7.0052266015776,-0.290562941631536,
62.2396595124862));
#145920=CARTESIAN_POINT('Ctrl Pts',(-7.01409982000545,-0.0766371552824991,
62.2299076551478));
#145921=CARTESIAN_POINT('Ctrl Pts',(-7.0131704526151,0.137720499562426,
62.2201557978095));
#145922=CARTESIAN_POINT('Ctrl Pts',(-7.00242371330003,0.351694045888468,
62.2104039404712));
#145923=CARTESIAN_POINT('Ctrl Pts',(-6.99773735664163,0.445002008810862,
62.2061514244075));
#145924=CARTESIAN_POINT('Ctrl Pts',(-6.99118480248129,0.538236889438612,
62.2018989083438));
#145925=CARTESIAN_POINT('Ctrl Pts',(-6.9827679269484,0.631330848985552,
62.1976463922802));
#145926=CARTESIAN_POINT('Ctrl Pts',(-6.9668683644438,0.807186274533022,
62.1896133466813));
#145927=CARTESIAN_POINT('Ctrl Pts',(-6.94430472223171,0.982624320127165,
62.1815803010824));
#145928=CARTESIAN_POINT('Ctrl Pts',(-6.9151109345152,1.15709434613102,62.1735472554835));
#145929=CARTESIAN_POINT('Ctrl Pts',(-6.8859359136895,1.33145221608439,62.1655193738356));
#145930=CARTESIAN_POINT('Ctrl Pts',(-6.85013929144247,1.50484294507663,
62.1574914921877));
#145931=CARTESIAN_POINT('Ctrl Pts',(-6.80780683282828,1.67672081438639,
62.1494636105398));
#145932=CARTESIAN_POINT('Ctrl Pts',(-6.76549348773645,1.8485210791439,62.1414393535596));
#145933=CARTESIAN_POINT('Ctrl Pts',(-6.71665026952844,2.01880948909778,
62.1334150965794));
#145934=CARTESIAN_POINT('Ctrl Pts',(-6.66141405653127,2.18705037206455,
62.1253908395993));
#145935=CARTESIAN_POINT('Ctrl Pts',(-6.60618452215485,2.35527091299494,
62.1173675528335));
#145936=CARTESIAN_POINT('Ctrl Pts',(-6.54456363958376,2.52144406956844,
62.1093442660677));
#145937=CARTESIAN_POINT('Ctrl Pts',(-6.47673824463895,2.68504902616902,
62.1013209793019));
#145938=CARTESIAN_POINT('Ctrl Pts',(-6.40891840738025,2.84864057680276,
62.0932983499729));
#145939=CARTESIAN_POINT('Ctrl Pts',(-6.33489521456378,3.00966400948752,
62.0852757206439));
#145940=CARTESIAN_POINT('Ctrl Pts',(-6.25490365125662,3.16761848649686,
62.0772530913149));
#145941=CARTESIAN_POINT('Ctrl Pts',(-6.17488201681645,3.32563234314437,
62.0692274460484));
#145942=CARTESIAN_POINT('Ctrl Pts',(-6.08888769815882,3.48057461350168,
62.0612018007819));
#145943=CARTESIAN_POINT('Ctrl Pts',(-5.99720182272748,3.63196873058871,
62.0531761555154));
#145944=CARTESIAN_POINT('Ctrl Pts',(-5.94313824351753,3.72123992751572,
62.0484437460081));
#145945=CARTESIAN_POINT('Ctrl Pts',(-5.8870965657202,3.80927792588718,62.0437113365009));
#145946=CARTESIAN_POINT('Ctrl Pts',(-5.82914149318423,3.89598973496311,
62.0389789269936));
#145947=CARTESIAN_POINT('Ctrl Pts',(-5.72222965204512,4.05595017934109,
62.030248878159));
#145948=CARTESIAN_POINT('Ctrl Pts',(-5.60875089324011,4.21147602252567,
62.0215188293245));
#145949=CARTESIAN_POINT('Ctrl Pts',(-5.48909361084644,4.36204973537268,
62.0127887804899));
#145950=CARTESIAN_POINT('Ctrl Pts',(-5.36940172940039,4.51266698679647,
62.0040562073509));
#145951=CARTESIAN_POINT('Ctrl Pts',(-5.24352792879278,4.65832903523479,
61.9953236342118));
#145952=CARTESIAN_POINT('Ctrl Pts',(-5.11190092573161,4.79855139474449,
61.9865910610728));
#145953=CARTESIAN_POINT('Ctrl Pts',(-4.9784039509733,4.94076583671062,61.9777344277923));
#145954=CARTESIAN_POINT('Ctrl Pts',(-4.8389892594256,5.07738464152953,61.9688777945119));
#145955=CARTESIAN_POINT('Ctrl Pts',(-4.69414314874617,5.20794073138121,
61.9600211612314));
#145956=CARTESIAN_POINT('Ctrl Pts',(-4.55123506955074,5.3367499892926,61.9512830291248));
#145957=CARTESIAN_POINT('Ctrl Pts',(-4.40304023448336,5.45965759339595,
61.9425448970182));
#145958=CARTESIAN_POINT('Ctrl Pts',(-4.25006011984992,5.57625461579376,
61.9338067649115));
#145959=CARTESIAN_POINT('Ctrl Pts',(-4.09396807186477,5.69522346386043,
61.9248908810442));
#145960=CARTESIAN_POINT('Ctrl Pts',(-3.93289420718763,5.8076220569043,61.9159749971768));
#145961=CARTESIAN_POINT('Ctrl Pts',(-3.76740442871578,5.913061003659,61.9070591133094));
#145962=CARTESIAN_POINT('Ctrl Pts',(-3.60191465024387,6.01849995041373,
61.898143229442));
#145963=CARTESIAN_POINT('Ctrl Pts',(-3.43200921629051,6.1169790935122,61.8892273455747));
#145964=CARTESIAN_POINT('Ctrl Pts',(-3.25828380186393,6.20815699133093,
61.8803114617073));
#145965=CARTESIAN_POINT('Ctrl Pts',(-3.08797213573309,6.29754322041591,
61.8715707772111));
#145966=CARTESIAN_POINT('Ctrl Pts',(-2.91397113395657,6.37992197706101,
61.8628300927148));
#145967=CARTESIAN_POINT('Ctrl Pts',(-2.73686415547664,6.45501364498691,
61.8540894082186));
#145968=CARTESIAN_POINT('Ctrl Pts',(-2.55978904148388,6.53009180267447,
61.8453502963167));
#145969=CARTESIAN_POINT('Ctrl Pts',(-2.37960931877037,6.59788538310797,
61.8366111844148));
#145970=CARTESIAN_POINT('Ctrl Pts',(-2.1969289224011,6.65816264989205,61.8278720725129));
#145971=CARTESIAN_POINT('Ctrl Pts',(-2.0118816385748,6.71922089542115,61.8190197328385));
#145972=CARTESIAN_POINT('Ctrl Pts',(-1.82426869333963,6.77256658958781,
61.8101673931642));
#145973=CARTESIAN_POINT('Ctrl Pts',(-1.63473565425623,6.81801040650449,
61.8013150534898));
#145974=CARTESIAN_POINT('Ctrl Pts',(-1.44772278169457,6.86284997000673,
61.7925804208401));
#145975=CARTESIAN_POINT('Ctrl Pts',(-1.25884083650483,6.89999643726584,
61.7838457881903));
#145976=CARTESIAN_POINT('Ctrl Pts',(-1.06872316361794,6.92931867949847,
61.7751111555405));
#145977=CARTESIAN_POINT('Ctrl Pts',(-0.874762480986496,6.95923363707903,
61.7661999623539));
#145978=CARTESIAN_POINT('Ctrl Pts',(-0.679515864638774,6.98100461965456,
61.7572887691673));
#145979=CARTESIAN_POINT('Ctrl Pts',(-0.483665567503547,6.99454746079484,
61.7483775759807));
#145980=CARTESIAN_POINT('Ctrl Pts',(-0.287815270368321,7.00809030193511,
61.739466382794));
#145981=CARTESIAN_POINT('Ctrl Pts',(-0.0913615939237434,7.01340496728704,
61.7305551896074));
#145982=CARTESIAN_POINT('Ctrl Pts',(0.105007858588381,7.01046360179801,
61.7216439964208));
#145983=CARTESIAN_POINT('Ctrl Pts',(0.281863570289811,7.00781452741153,
61.7136183315683));
#145984=CARTESIAN_POINT('Ctrl Pts',(0.458732234539534,6.99846700358813,
61.7055926667158));
#145985=CARTESIAN_POINT('Ctrl Pts',(0.635061200245588,6.98242965123478,
61.6975670018633));
#145986=CARTESIAN_POINT('Ctrl Pts',(0.81133420346308,6.96639738874369,61.68954388416));
#145987=CARTESIAN_POINT('Ctrl Pts',(0.98706748452383,6.94367955795302,61.6815207664567));
#145988=CARTESIAN_POINT('Ctrl Pts',(1.16171130126777,6.91433680225419,61.6734976487534));
#145989=CARTESIAN_POINT('Ctrl Pts',(1.33633309389806,6.88499774693364,61.6654755428354));
#145990=CARTESIAN_POINT('Ctrl Pts',(1.50986533457572,6.84903549215138,61.6574534369174));
#145991=CARTESIAN_POINT('Ctrl Pts',(1.68176633953544,6.80656216762218,61.6494313309995));
#145992=CARTESIAN_POINT('Ctrl Pts',(1.85373122348923,6.76407305986213,61.6414062440398));
#145993=CARTESIAN_POINT('Ctrl Pts',(2.02406330386218,6.71506813398563,61.6333811570802));
#145994=CARTESIAN_POINT('Ctrl Pts',(2.19223353945854,6.65971010412414,61.6253560701206));
#145995=CARTESIAN_POINT('Ctrl Pts',(2.36043689534125,6.60434117177568,61.6173294026603));
#145996=CARTESIAN_POINT('Ctrl Pts',(2.52647721282525,6.54261676580371,61.6093027351999));
#145997=CARTESIAN_POINT('Ctrl Pts',(2.68984362316753,6.47474847738544,61.6012760677396));
#145998=CARTESIAN_POINT('Ctrl Pts',(2.85334118348836,6.40682570454437,61.5932429564989));
#145999=CARTESIAN_POINT('Ctrl Pts',(3.01416021447469,6.33274934743334,61.5852098452582));
#146000=CARTESIAN_POINT('Ctrl Pts',(3.17181215965281,6.25277811747535,61.5771767340175));
#146001=CARTESIAN_POINT('Ctrl Pts',(3.26470641275866,6.205656163677,61.5724433330564));
#146002=CARTESIAN_POINT('Ctrl Pts',(3.35650152547001,6.15648838283058,61.5677099320953));
#146003=CARTESIAN_POINT('Ctrl Pts',(3.44710205084303,6.10533488136186,61.5629765311343));
#146004=CARTESIAN_POINT('Ctrl Pts',(3.63374195280158,5.99995707632539,61.5532255778405));
#146005=CARTESIAN_POINT('Ctrl Pts',(3.8154211757974,5.88608855414379,61.5434746245467));
#146006=CARTESIAN_POINT('Ctrl Pts',(3.9914628013073,5.76418695639551,61.5337236712529));
#146007=CARTESIAN_POINT('Ctrl Pts',(4.16775804780412,5.64210973652695,61.5239586698816));
#146008=CARTESIAN_POINT('Ctrl Pts',(4.33839941862934,5.51197631337505,61.5141936685103));
#146009=CARTESIAN_POINT('Ctrl Pts',(4.5027393116297,5.37428741825411,61.5044286671391));
#146010=CARTESIAN_POINT('Ctrl Pts',(4.66680528407829,5.23682802199335,61.4946799420018));
#146011=CARTESIAN_POINT('Ctrl Pts',(4.8245907413907,5.09183834721426,61.4849312168646));
#146012=CARTESIAN_POINT('Ctrl Pts',(4.97548376535131,4.93985706910894,61.4751824917274));
#146013=CARTESIAN_POINT('Ctrl Pts',(5.12596264647027,4.78829292068092,61.4654605230606));
#146014=CARTESIAN_POINT('Ctrl Pts',(5.26958683091385,4.62977550544657,61.4557385543938));
#146015=CARTESIAN_POINT('Ctrl Pts',(5.40578224980526,4.46487903869639,61.4460165857269));
#146016=CARTESIAN_POINT('Ctrl Pts',(5.54107649918223,4.30107364879802,61.4363589447875));
#146017=CARTESIAN_POINT('Ctrl Pts',(5.66903991448771,4.13097336299275,61.4267013038482));
#146018=CARTESIAN_POINT('Ctrl Pts',(5.78914287362294,3.95518031842806,61.4170436629088));
#146019=CARTESIAN_POINT('Ctrl Pts',(5.8419322590775,3.8779132231244,61.4127987972218));
#146020=CARTESIAN_POINT('Ctrl Pts',(5.89320351581207,3.79954685127154,61.4085539315349));
#146021=CARTESIAN_POINT('Ctrl Pts',(5.94291376581599,3.7201347468304,61.404309065848));
#146022=CARTESIAN_POINT('Ctrl Pts',(6.03486251755945,3.57324665280332,61.3964573632072));
#146023=CARTESIAN_POINT('Ctrl Pts',(6.12142950456126,3.42283903687358,61.3886056605664));
#146024=CARTESIAN_POINT('Ctrl Pts',(6.20232953860754,3.26936306595281,61.3807539579256));
#146025=CARTESIAN_POINT('Ctrl Pts',(6.28321295025175,3.11591862949711,61.3729038685617));
#146026=CARTESIAN_POINT('Ctrl Pts',(6.35843154219062,2.95940742648086,61.3650537791978));
#146027=CARTESIAN_POINT('Ctrl Pts',(6.42774524540919,2.80030670152746,61.3572036898339));
#146028=CARTESIAN_POINT('Ctrl Pts',(6.47875690302238,2.68321597732042,61.3514263896426));
#146029=CARTESIAN_POINT('Ctrl Pts',(6.52657123496308,2.56472326869091,61.3456490894513));
#146030=CARTESIAN_POINT('Ctrl Pts',(6.57110895151815,2.44502632087632,61.3398717892601));
#146031=CARTESIAN_POINT('Origin',(0.,0.,50.));
#146032=CARTESIAN_POINT('',(6.57110895151816,2.4450263208763,59.3399667921338));
#146033=CARTESIAN_POINT('',(6.57110895151811,2.44502632087644,59.8868036378692));
#146034=CARTESIAN_POINT('',(6.57110895151814,2.44502632087636,50.));
#146035=CARTESIAN_POINT('',(7.01124996031773,0.000745952195652544,61.7735343568788));
#146036=CARTESIAN_POINT('Ctrl Pts',(6.57110895151811,2.44502632087643,59.8868036378692));
#146037=CARTESIAN_POINT('Ctrl Pts',(6.50640911017929,2.61890980955436,59.8952320262474));
#146038=CARTESIAN_POINT('Ctrl Pts',(6.43483843042466,2.79012927483976,59.9036604146256));
#146039=CARTESIAN_POINT('Ctrl Pts',(6.35665295223755,2.95813958550128,59.9120888030038));
#146040=CARTESIAN_POINT('Ctrl Pts',(6.27841693811276,3.12625849124703,59.9205226391521));
#146041=CARTESIAN_POINT('Ctrl Pts',(6.1935577387562,3.29116381664877,59.9289564753004));
#146042=CARTESIAN_POINT('Ctrl Pts',(6.102377161576,3.45233537484058,59.9373903114487));
#146043=CARTESIAN_POINT('Ctrl Pts',(6.01109044809208,3.61369454045911,59.9458339647777));
#146044=CARTESIAN_POINT('Ctrl Pts',(5.91346782168328,3.77131098065186,59.9542776181066));
#146045=CARTESIAN_POINT('Ctrl Pts',(5.80985483003942,3.9246927798705,59.9627212714355));
#146046=CARTESIAN_POINT('Ctrl Pts',(5.78906647449476,3.95546648233435,59.9644153608032));
#146047=CARTESIAN_POINT('Ctrl Pts',(5.76803711304307,3.98606982641891,59.9661094501708));
#146048=CARTESIAN_POINT('Ctrl Pts',(5.74676973213664,4.01649899891662,59.9678035395385));
#146049=CARTESIAN_POINT('Ctrl Pts',(5.64155196050998,4.16704361636331,59.9761848399435));
#146050=CARTESIAN_POINT('Ctrl Pts',(5.53029242921032,4.31362675215176,59.9845661403485));
#146051=CARTESIAN_POINT('Ctrl Pts',(5.41331025385377,4.45574894468053,59.9929474407534));
#146052=CARTESIAN_POINT('Ctrl Pts',(5.29647633627894,4.59769101813617,60.0013181190871));
#146053=CARTESIAN_POINT('Ctrl Pts',(5.17393443489199,4.73518316442958,60.0096887974208));
#146054=CARTESIAN_POINT('Ctrl Pts',(5.04604670722158,4.86775504632662,60.0180594757544));
#146055=CARTESIAN_POINT('Ctrl Pts',(4.918304110165,5.000176481899,60.0264206548054));
#146056=CARTESIAN_POINT('Ctrl Pts',(4.78522800431385,5.12768854753524,60.0347818338563));
#146057=CARTESIAN_POINT('Ctrl Pts',(4.64722083486221,5.24985381458594,60.0431430129072));
#146058=CARTESIAN_POINT('Ctrl Pts',(4.50939274599253,5.37186055779179,60.051493342342));
#146059=CARTESIAN_POINT('Ctrl Pts',(4.36664660046041,5.48853412504243,60.0598436717768));
#146060=CARTESIAN_POINT('Ctrl Pts',(4.21942164594463,5.59947386244761,60.0681940012116));
#146061=CARTESIAN_POINT('Ctrl Pts',(4.07230997222455,5.71032823836112,60.0765379055674));
#146062=CARTESIAN_POINT('Ctrl Pts',(3.92072661768556,5.81545738007573,60.0848818099233));
#146063=CARTESIAN_POINT('Ctrl Pts',(3.76514473326157,5.91450012258793,60.0932257142791));
#146064=CARTESIAN_POINT('Ctrl Pts',(3.60968781317767,6.01346331335153,60.1015629167589));
#146065=CARTESIAN_POINT('Ctrl Pts',(3.45023904397216,6.10634967915229,60.1099001192387));
#146066=CARTESIAN_POINT('Ctrl Pts',(3.28730157291819,6.19284061890742,60.1182373217184));
#146067=CARTESIAN_POINT('Ctrl Pts',(3.23366345685152,6.22131295885042,60.120981882754));
#146068=CARTESIAN_POINT('Ctrl Pts',(3.17964750749847,6.2490925814078,60.1237264437895));
#146069=CARTESIAN_POINT('Ctrl Pts',(3.125272337548,6.27616916427985,60.126471004825));
#146070=CARTESIAN_POINT('Ctrl Pts',(2.96007395649831,6.35843111691184,60.1348093151269));
#146071=CARTESIAN_POINT('Ctrl Pts',(2.79169365377402,6.43413296875797,60.1431476254287));
#146072=CARTESIAN_POINT('Ctrl Pts',(2.62068329858579,6.50304894730261,60.1514859357305));
#146073=CARTESIAN_POINT('Ctrl Pts',(2.4495653494853,6.57200828544228,60.1598294922142));
#146074=CARTESIAN_POINT('Ctrl Pts',(2.27581435123775,6.63417311187902,60.1681730486979));
#146075=CARTESIAN_POINT('Ctrl Pts',(2.09999932366907,6.68936689105101,60.1765166051816));
#146076=CARTESIAN_POINT('Ctrl Pts',(1.92405053679387,6.74460266140958,60.1848665094067));
#146077=CARTESIAN_POINT('Ctrl Pts',(1.74603490060753,6.79285670764081,60.1932164136319));
#146078=CARTESIAN_POINT('Ctrl Pts',(1.56653408797299,6.83400303729217,60.201566317857));
#146079=CARTESIAN_POINT('Ctrl Pts',(1.38676403740216,6.87521108339328,60.2099287463205));
#146080=CARTESIAN_POINT('Ctrl Pts',(1.20550467847311,6.90929003551477,60.2182911747841));
#146081=CARTESIAN_POINT('Ctrl Pts',(1.02334681551833,6.9361652126855,60.2266536032477));
#146082=CARTESIAN_POINT('Ctrl Pts',(0.841033182758529,6.9630633717964,60.2350231827276));
#146083=CARTESIAN_POINT('Ctrl Pts',(0.657819837930774,6.98274542983082,
60.2433927622075));
#146084=CARTESIAN_POINT('Ctrl Pts',(0.474300687196313,6.99518873373872,
60.2517623416874));
#146085=CARTESIAN_POINT('Ctrl Pts',(0.290498480531814,7.00765122992681,
60.2601448302239));
#146086=CARTESIAN_POINT('Ctrl Pts',(0.106389852311009,7.01285265196089,
60.2685273187603));
#146087=CARTESIAN_POINT('Ctrl Pts',(-0.077431893973664,7.01082240998128,
60.2769098072968));
#146088=CARTESIAN_POINT('Ctrl Pts',(-0.137581381466362,7.01015808153794,
60.2796526949017));
#146089=CARTESIAN_POINT('Ctrl Pts',(-0.197700200067954,7.00871986780067,
60.2823955825065));
#146090=CARTESIAN_POINT('Ctrl Pts',(-0.257767731965874,7.00650999848407,
60.2851384701114));
#146091=CARTESIAN_POINT('Ctrl Pts',(-0.441500339135086,6.99975052230428,
60.2935283252442));
#146092=CARTESIAN_POINT('Ctrl Pts',(-0.62512358458665,6.98575389272276,
60.301918180377));
#146093=CARTESIAN_POINT('Ctrl Pts',(-0.80804424770065,6.96453092865973,
60.3103080355098));
#146094=CARTESIAN_POINT('Ctrl Pts',(-0.990796114190584,6.94332754885046,
60.3186901486019));
#146095=CARTESIAN_POINT('Ctrl Pts',(-1.17284636583484,6.91491116563024,
60.3270722616939));
#146096=CARTESIAN_POINT('Ctrl Pts',(-1.35360443769803,6.8793445609843,60.335454374786));
#146097=CARTESIAN_POINT('Ctrl Pts',(-1.53422227960854,6.84380554848533,
60.3438299851349));
#146098=CARTESIAN_POINT('Ctrl Pts',(-1.71354961894826,6.80112743693797,
60.3522055954838));
#146099=CARTESIAN_POINT('Ctrl Pts',(-1.89100319271688,6.75142455246554,
60.3605812058327));
#146100=CARTESIAN_POINT('Ctrl Pts',(-2.06834514555234,6.70175293184556,
60.3689515477982));
#146101=CARTESIAN_POINT('Ctrl Pts',(-2.24381536716304,6.64506543719745,
60.3773218897638));
#146102=CARTESIAN_POINT('Ctrl Pts',(-2.41684248557271,6.58152709957429,
60.3856922317294));
#146103=CARTESIAN_POINT('Ctrl Pts',(-2.58978613118775,6.51801941450234,
60.3940585356237));
#146104=CARTESIAN_POINT('Ctrl Pts',(-2.7602887159284,6.44766759032323,60.4024248395181));
#146105=CARTESIAN_POINT('Ctrl Pts',(-2.92779525274036,6.37068611065802,
60.4107911434124));
#146106=CARTESIAN_POINT('Ctrl Pts',(-3.095254942669,6.29372616055497,60.419155107486));
#146107=CARTESIAN_POINT('Ctrl Pts',(-3.25971995648313,6.21014038788013,
60.4275190715596));
#146108=CARTESIAN_POINT('Ctrl Pts',(-3.42065596391864,6.12019111948376,
60.4358830356332));
#146109=CARTESIAN_POINT('Ctrl Pts',(-3.58156720597674,6.03025569278518,
60.4442457126318));
#146110=CARTESIAN_POINT('Ctrl Pts',(-3.7389502375947,5.93395888306578,60.4526083896303));
#146111=CARTESIAN_POINT('Ctrl Pts',(-3.89229561965895,5.83160881504271,
60.4609710666288));
#146112=CARTESIAN_POINT('Ctrl Pts',(-4.04563784462231,5.72926085422029,
60.4693335714551));
#146113=CARTESIAN_POINT('Ctrl Pts',(-4.19494231265859,5.62086006638129,
60.4776960762814));
#146114=CARTESIAN_POINT('Ctrl Pts',(-4.33972849283295,5.50675795464027,
60.4860585811077));
#146115=CARTESIAN_POINT('Ctrl Pts',(-4.48453099109167,5.39264298305391,
60.4944220284277));
#146116=CARTESIAN_POINT('Ctrl Pts',(-4.62481392844133,5.27282561030957,
60.5027854757477));
#146117=CARTESIAN_POINT('Ctrl Pts',(-4.76012946021177,5.14769794029564,
60.5111489230676));
#146118=CARTESIAN_POINT('Ctrl Pts',(-4.89552466957032,5.02249659159293,
60.5195172950204));
#146119=CARTESIAN_POINT('Ctrl Pts',(-5.02594638640059,4.8919789200875,60.5278856669733));
#146120=CARTESIAN_POINT('Ctrl Pts',(-5.15098254250197,4.75657496622727,
60.5362540389261));
#146121=CARTESIAN_POINT('Ctrl Pts',(-5.27605616270253,4.62113044180477,
60.5446249182618));
#146122=CARTESIAN_POINT('Ctrl Pts',(-5.39574078546182,4.4807969608252,60.5529957975974));
#146123=CARTESIAN_POINT('Ctrl Pts',(-5.50966388458844,4.33603856548369,
60.5613666769331));
#146124=CARTESIAN_POINT('Ctrl Pts',(-5.62368350952584,4.19115751791814,
60.5697446488244));
#146125=CARTESIAN_POINT('Ctrl Pts',(-5.73193165718387,4.0418443262551,60.5781226207157));
#146126=CARTESIAN_POINT('Ctrl Pts',(-5.83407780103488,3.88859393276954,
60.586500592607));
#146127=CARTESIAN_POINT('Ctrl Pts',(-5.89899250723227,3.79120205978547,
60.5918248619661));
#146128=CARTESIAN_POINT('Ctrl Pts',(-5.96144366641336,3.69222065152036,
60.5971491313251));
#146129=CARTESIAN_POINT('Ctrl Pts',(-6.02135593370052,3.59178218746482,
60.6024734006842));
#146130=CARTESIAN_POINT('Ctrl Pts',(-6.1098338096449,3.44345560319192,60.6103362318735));
#146131=CARTESIAN_POINT('Ctrl Pts',(-6.19295614891969,3.29164153103617,
60.6181990630628));
#146132=CARTESIAN_POINT('Ctrl Pts',(-6.27042519721603,3.13678089904576,
60.6260618942521));
#146133=CARTESIAN_POINT('Ctrl Pts',(-6.34783472077468,2.98203925700939,
60.6339186838935));
#146134=CARTESIAN_POINT('Ctrl Pts',(-6.41959942216613,2.82425604909458,
60.6417754735349));
#146135=CARTESIAN_POINT('Ctrl Pts',(-6.485465547011,2.66389999831701,60.6496322631763));
#146136=CARTESIAN_POINT('Ctrl Pts',(-6.5512945264794,2.50363438076118,60.6574846219603));
#146137=CARTESIAN_POINT('Ctrl Pts',(-6.61123140219648,2.34079915821796,
60.6653369807442));
#146138=CARTESIAN_POINT('Ctrl Pts',(-6.66506908723143,2.17588617003095,
60.6731893395282));
#146139=CARTESIAN_POINT('Ctrl Pts',(-6.71889406056072,2.01101211972483,
60.6810398442786));
#146140=CARTESIAN_POINT('Ctrl Pts',(-6.7666225831489,1.84406163967337,60.6888903490291));
#146141=CARTESIAN_POINT('Ctrl Pts',(-6.80809633639751,1.67554493727587,
60.6967408537795));
#146142=CARTESIAN_POINT('Ctrl Pts',(-6.84956341782639,1.5070553439045,60.7045900956312));
#146143=CARTESIAN_POINT('Ctrl Pts',(-6.88477764469766,1.33700040095018,
60.7124393374828));
#146144=CARTESIAN_POINT('Ctrl Pts',(-6.91363116893276,1.16590335039466,
60.7202885793345));
#146145=CARTESIAN_POINT('Ctrl Pts',(-6.94249441448492,0.994748653893899,
60.7281404657493));
#146146=CARTESIAN_POINT('Ctrl Pts',(-6.9649926132986,0.822551525024216,
60.7359923521642));
#146147=CARTESIAN_POINT('Ctrl Pts',(-6.98106940870049,0.649843422222746,
60.7438442385791));
#146148=CARTESIAN_POINT('Ctrl Pts',(-6.99287439946007,0.523026011992201,
60.7496097810429));
#146149=CARTESIAN_POINT('Ctrl Pts',(-7.00121818321514,0.39593328043947,
60.7553753235068));
#146150=CARTESIAN_POINT('Ctrl Pts',(-7.00609632877495,0.268776476698001,
60.7611408659707));
#146151=CARTESIAN_POINT('Ctrl Pts',(-7.0142655479574,0.0558324823935959,
60.7707961703308));
#146152=CARTESIAN_POINT('Ctrl Pts',(-7.01271064726126,-0.157182581790572,
60.780451474691));
#146153=CARTESIAN_POINT('Ctrl Pts',(-7.00150842649691,-0.369467611831974,
60.7901067790512));
#146154=CARTESIAN_POINT('Ctrl Pts',(-6.99024414753111,-0.582928661114273,
60.7998155719861));
#146155=CARTESIAN_POINT('Ctrl Pts',(-6.9692254208665,-0.79565152111639,
60.8095243649211));
#146156=CARTESIAN_POINT('Ctrl Pts',(-6.93858118164358,-1.00683551200857,
60.819233157856));
#146157=CARTESIAN_POINT('Ctrl Pts',(-6.90778947973966,-1.2190357381956,
60.8289886703269));
#146158=CARTESIAN_POINT('Ctrl Pts',(-6.86727943477904,-1.4296822099299,
60.8387441827978));
#146159=CARTESIAN_POINT('Ctrl Pts',(-6.81723238419103,-1.63797716175688,
60.8484996952686));
#146160=CARTESIAN_POINT('Ctrl Pts',(-6.7671357793234,-1.84647835763151,
60.8582648671977));
#146161=CARTESIAN_POINT('Ctrl Pts',(-6.70748330029079,-2.05262334166574,
60.8680300391268));
#146162=CARTESIAN_POINT('Ctrl Pts',(-6.6385068576747,-2.25562702216169,
60.8777952110558));
#146163=CARTESIAN_POINT('Ctrl Pts',(-6.56962446287299,-2.45835391174557,
60.8875470683946));
#146164=CARTESIAN_POINT('Ctrl Pts',(-6.49144352547867,-2.65794802224537,
60.8972989257333));
#146165=CARTESIAN_POINT('Ctrl Pts',(-6.40424455972472,-2.85364296675958,
60.907050783072));
#146166=CARTESIAN_POINT('Ctrl Pts',(-6.36621949541621,-2.93898013544801,
60.9113032991337));
#146167=CARTESIAN_POINT('Ctrl Pts',(-6.32648020592294,-3.02357604429839,
60.9155558151954));
#146168=CARTESIAN_POINT('Ctrl Pts',(-6.28505290906144,-3.1073680974095,
60.9198083312571));
#146169=CARTESIAN_POINT('Ctrl Pts',(-6.20679632874754,-3.2656521282474,
60.9278413768558));
#146170=CARTESIAN_POINT('Ctrl Pts',(-6.12247476553096,-3.42114328480263,
60.9358744224545));
#146171=CARTESIAN_POINT('Ctrl Pts',(-6.03231847320822,-3.57334023013354,
60.9439074680532));
#146172=CARTESIAN_POINT('Ctrl Pts',(-5.94222013682133,-3.72543933740822,
60.9519353497009));
#146173=CARTESIAN_POINT('Ctrl Pts',(-5.84629472340964,-3.87424813461167,
60.9599632313486));
#146174=CARTESIAN_POINT('Ctrl Pts',(-5.74481905403682,-4.0192885687489,
60.9679911129963));
#146175=CARTESIAN_POINT('Ctrl Pts',(-5.6433892019298,-4.16426351569925,
60.9760153699762));
#146176=CARTESIAN_POINT('Ctrl Pts',(-5.53641429329042,-4.30547318763866,
60.9840396269562));
#146177=CARTESIAN_POINT('Ctrl Pts',(-5.4242151984711,-4.44246733732226,
60.9920638839361));
#146178=CARTESIAN_POINT('Ctrl Pts',(-5.31202966966456,-4.57944492301854,
61.0000871707017));
#146179=CARTESIAN_POINT('Ctrl Pts',(-5.19462143899718,-4.71220771337947,
61.0081104574673));
#146180=CARTESIAN_POINT('Ctrl Pts',(-5.07235261325369,-4.84033733631433,
61.0161337442329));
#146181=CARTESIAN_POINT('Ctrl Pts',(-4.95009380634964,-4.9684564601697,
61.0241563735617));
#146182=CARTESIAN_POINT('Ctrl Pts',(-4.82297545373627,-5.09194291034018,
61.0321790028905));
#146183=CARTESIAN_POINT('Ctrl Pts',(-4.69139736494629,-5.21041431430122,
61.0402016322193));
#146184=CARTESIAN_POINT('Ctrl Pts',(-4.55976981216225,-5.32893025507591,
61.0482272774856));
#146185=CARTESIAN_POINT('Ctrl Pts',(-4.42367944863565,-5.44242714022515,
61.0562529227519));
#146186=CARTESIAN_POINT('Ctrl Pts',(-4.28356036651973,-5.55056187686268,
61.0642785680182));
#146187=CARTESIAN_POINT('Ctrl Pts',(-4.20093761725585,-5.61432470699975,
61.0690109775266));
#146188=CARTESIAN_POINT('Ctrl Pts',(-4.1169147023471,-5.67622388779455,
61.073743387035));
#146189=CARTESIAN_POINT('Ctrl Pts',(-4.03158551017731,-5.73619602494792,
61.0784757965434));
#146190=CARTESIAN_POINT('Ctrl Pts',(-3.8741756297881,-5.84682881890682,
61.0872058453782));
#146191=CARTESIAN_POINT('Ctrl Pts',(-3.71224031257441,-5.95095695938307,
61.095935894213));
#146192=CARTESIAN_POINT('Ctrl Pts',(-3.54632847140008,-6.04823783720822,
61.1046659430478));
#146193=CARTESIAN_POINT('Ctrl Pts',(-3.3803686566086,-6.14554684392132,
61.1133985161871));
#146194=CARTESIAN_POINT('Ctrl Pts',(-3.2104302590754,-6.23600449744522,
61.1221310893265));
#146195=CARTESIAN_POINT('Ctrl Pts',(-3.03708788223122,-6.31931355117819,
61.1308636624658));
#146196=CARTESIAN_POINT('Ctrl Pts',(-2.86128290022261,-6.40380614300324,
61.1397202957462));
#146197=CARTESIAN_POINT('Ctrl Pts',(-2.68197674508946,-6.48094534691311,
61.1485769290265));
#146198=CARTESIAN_POINT('Ctrl Pts',(-2.49979144672779,-6.5504709208855,
61.1574335623069));
#146199=CARTESIAN_POINT('Ctrl Pts',(-2.32004377573059,-6.61906624722997,
61.1661716944138));
#146200=CARTESIAN_POINT('Ctrl Pts',(-2.13749379628574,-6.68025034070188,
61.1749098265207));
#146201=CARTESIAN_POINT('Ctrl Pts',(-1.95275672186057,-6.73382266975663,
61.1836479586276));
#146202=CARTESIAN_POINT('Ctrl Pts',(-1.76426171155767,-6.78848477127875,
61.1925638424947));
#146203=CARTESIAN_POINT('Ctrl Pts',(-1.57348995649215,-6.83522202694157,
61.2014797263617));
#146204=CARTESIAN_POINT('Ctrl Pts',(-1.3811097137541,-6.87387536409223,
61.2103956102288));
#146205=CARTESIAN_POINT('Ctrl Pts',(-1.18872947101606,-6.91252870124289,
61.2193114940959));
#146206=CARTESIAN_POINT('Ctrl Pts',(-0.994741038290665,-6.94309806627461,
61.228227377963));
#146207=CARTESIAN_POINT('Ctrl Pts',(-0.799823146438977,-6.96547984685337,
61.23714326183));
#146208=CARTESIAN_POINT('Ctrl Pts',(-0.608735440416435,-6.98742181978806,
61.2458839463261));
#146209=CARTESIAN_POINT('Ctrl Pts',(-0.416734168987128,-7.0014973280946,
61.2546246308223));
#146210=CARTESIAN_POINT('Ctrl Pts',(-0.224464276884863,-7.00765598120388,
61.2633653153184));
#146211=CARTESIAN_POINT('Ctrl Pts',(-0.0322289773305222,-7.01381352626916,
61.2721044272201));
#146212=CARTESIAN_POINT('Ctrl Pts',(0.160274572823184,-7.01205705195798,
61.2808435391219));
#146213=CARTESIAN_POINT('Ctrl Pts',(0.352399506920261,-7.00238824616447,
61.2895826510236));
#146214=CARTESIAN_POINT('Ctrl Pts',(0.547013696058328,-6.99259416707588,
61.298434990698));
#146215=CARTESIAN_POINT('Ctrl Pts',(0.741239103930971,-6.97468128782271,
61.3072873303724));
#146216=CARTESIAN_POINT('Ctrl Pts',(0.934405330199851,-6.94870586810192,
61.3161396700468));
#146217=CARTESIAN_POINT('Ctrl Pts',(1.12500308049431,-6.92307583609599,
61.3248743026965));
#146218=CARTESIAN_POINT('Ctrl Pts',(1.31456936493636,-6.88959639389009,
61.3336089353461));
#146219=CARTESIAN_POINT('Ctrl Pts',(1.50246617354109,-6.84837367262219,
61.3423435679958));
#146220=CARTESIAN_POINT('Ctrl Pts',(1.69416109968256,-6.8063176815307,61.3512547611826));
#146221=CARTESIAN_POINT('Ctrl Pts',(1.8841180498202,-6.7562020754472,61.3601659543693));
#146222=CARTESIAN_POINT('Ctrl Pts',(2.07167033624739,-6.69819442688943,
61.3690771475561));
#146223=CARTESIAN_POINT('Ctrl Pts',(2.25922262267458,-6.64018677833167,
61.3779883407428));
#146224=CARTESIAN_POINT('Ctrl Pts',(2.44436995181516,-6.57428716399544,
61.3868995339296));
#146225=CARTESIAN_POINT('Ctrl Pts',(2.62646095606154,-6.50071760721724,
61.3958107271163));
#146226=CARTESIAN_POINT('Ctrl Pts',(2.79045710585923,-6.43445884773662,
61.4038363919688));
#146227=CARTESIAN_POINT('Ctrl Pts',(2.95204935192849,-6.36194783750196,
61.4118620568212));
#146228=CARTESIAN_POINT('Ctrl Pts',(3.11072535130985,-6.28339194633108,
61.4198877216737));
#146229=CARTESIAN_POINT('Ctrl Pts',(3.26935099082007,-6.20486098687369,
61.4279108393769));
#146230=CARTESIAN_POINT('Ctrl Pts',(3.42506189819082,-6.12028912847259,
61.4359339570802));
#146231=CARTESIAN_POINT('Ctrl Pts',(3.57736720696945,-6.02993121262586,
61.4439570747834));
#146232=CARTESIAN_POINT('Ctrl Pts',(3.72965330871607,-5.93958469170289,
61.4519791807013));
#146233=CARTESIAN_POINT('Ctrl Pts',(3.87853435246432,-5.84345375424984,
61.4600012866192));
#146234=CARTESIAN_POINT('Ctrl Pts',(4.02354555774109,-5.74183835607395,
61.4680233925371));
#146235=CARTESIAN_POINT('Ctrl Pts',(4.1686106496721,-5.64018519727249,61.4760484794967));
#146236=CARTESIAN_POINT('Ctrl Pts',(4.30980272816781,-5.53304371448372,
61.4840735664563));
#146237=CARTESIAN_POINT('Ctrl Pts',(4.44668704905208,-5.4207564832127,61.4920986534159));
#146238=CARTESIAN_POINT('Ctrl Pts',(4.58359832861805,-5.30844713753364,
61.5001253208762));
#146239=CARTESIAN_POINT('Ctrl Pts',(4.7161998826159,-5.19099026374683,61.5081519883365));
#146240=CARTESIAN_POINT('Ctrl Pts',(4.84409154502365,-5.06876747009866,
61.5161786557968));
#146241=CARTESIAN_POINT('Ctrl Pts',(4.97208587840775,-4.94644655642203,
61.5242117670375));
#146242=CARTESIAN_POINT('Ctrl Pts',(5.09536250989122,-4.81935234121083,
61.5322448782781));
#146243=CARTESIAN_POINT('Ctrl Pts',(5.21355907913378,-4.68790233376099,
61.5402779895188));
#146244=CARTESIAN_POINT('Ctrl Pts',(5.283204791451,-4.61044721419521,61.5450113904802));
#146245=CARTESIAN_POINT('Ctrl Pts',(5.35108746100097,-4.53148040745293,
61.5497447914415));
#146246=CARTESIAN_POINT('Ctrl Pts',(5.41713974441693,-4.45109239984506,
61.5544781924029));
#146247=CARTESIAN_POINT('Ctrl Pts',(5.5532095039421,-4.28549060232616,61.5642291456968));
#146248=CARTESIAN_POINT('Ctrl Pts',(5.68159006986931,-4.11375880356511,
61.5739800989907));
#146249=CARTESIAN_POINT('Ctrl Pts',(5.80181514815839,-3.93656799116945,
61.5837310522846));
#146250=CARTESIAN_POINT('Ctrl Pts',(5.92221343322642,-3.75912190216833,
61.593496053656));
#146251=CARTESIAN_POINT('Ctrl Pts',(6.03443270648752,-3.57620109972098,
61.6032610550274));
#146252=CARTESIAN_POINT('Ctrl Pts',(6.13804955852324,-3.38850618704064,
61.6130260563988));
#146253=CARTESIAN_POINT('Ctrl Pts',(6.24149370273561,-3.2011241228901,61.6227747815362));
#146254=CARTESIAN_POINT('Ctrl Pts',(6.33636406414719,-3.00898388541046,
61.6325235066736));
#146255=CARTESIAN_POINT('Ctrl Pts',(6.42228420093148,-2.81280859728597,
61.6422722318109));
#146256=CARTESIAN_POINT('Ctrl Pts',(6.50796852025351,-2.61717173426571,
61.6519942004776));
#146257=CARTESIAN_POINT('Ctrl Pts',(6.58475163872778,-2.41752196590726,
61.6617161691443));
#146258=CARTESIAN_POINT('Ctrl Pts',(6.65230523477775,-2.2146019113711,61.6714381378109));
#146259=CARTESIAN_POINT('Ctrl Pts',(6.71941184632809,-2.01302452583181,
61.6810957787504));
#146260=CARTESIAN_POINT('Ctrl Pts',(6.77741062828986,-1.80822002349115,
61.6907534196898));
#146261=CARTESIAN_POINT('Ctrl Pts',(6.82602478497098,-1.60094103497345,
61.7004110606292));
#146262=CARTESIAN_POINT('Ctrl Pts',(6.84739238052307,-1.50983478330803,
61.7046559263159));
#146263=CARTESIAN_POINT('Ctrl Pts',(6.86694754704264,-1.41825080290872,
61.7089007920025));
#146264=CARTESIAN_POINT('Ctrl Pts',(6.88466960476102,-1.32625449887257,
61.7131456576892));
#146265=CARTESIAN_POINT('Ctrl Pts',(6.91599476258385,-1.16364365599851,
61.720648798108));
#146266=CARTESIAN_POINT('Ctrl Pts',(6.941587348978,-0.999751854661091,61.7281519385268));
#146267=CARTESIAN_POINT('Ctrl Pts',(6.9613427933109,-0.835064713970333,
61.7356550789455));
#146268=CARTESIAN_POINT('Ctrl Pts',(6.98109422577986,-0.670411017346532,
61.7431566956538));
#146269=CARTESIAN_POINT('Ctrl Pts',(6.99501081379055,-0.504962703708429,
61.750658312362));
#146270=CARTESIAN_POINT('Ctrl Pts',(7.00303936527326,-0.33921410780379,
61.7581599290703));
#146271=CARTESIAN_POINT('Ctrl Pts',(7.00852415564041,-0.225981190988831,
61.7632847383398));
#146272=CARTESIAN_POINT('Ctrl Pts',(7.01126202048759,-0.112608316252692,
61.7684095476093));
#146273=CARTESIAN_POINT('Ctrl Pts',(7.01124996031773,0.000745952195671065,
61.7735343568789));
#146274=CARTESIAN_POINT('Ctrl Pts',(7.01124996031765,0.000745952895824991,
61.7735343569105));
#146275=CARTESIAN_POINT('Ctrl Pts',(7.01123049451363,0.183706054626861,
61.7818060844611));
#146276=CARTESIAN_POINT('Ctrl Pts',(7.00404513626102,0.366557650708819,
61.7900778120117));
#146277=CARTESIAN_POINT('Ctrl Pts',(6.98974513960821,0.548716179662563,
61.7983495395624));
#146278=CARTESIAN_POINT('Ctrl Pts',(6.97543598949126,0.730991308752774,
61.8066265618668));
#146279=CARTESIAN_POINT('Ctrl Pts',(6.95400315525616,0.912572151228788,
61.8149035841712));
#146280=CARTESIAN_POINT('Ctrl Pts',(6.9255494732271,1.0928819956353,61.8231806064756));
#146281=CARTESIAN_POINT('Ctrl Pts',(6.89705104070401,1.27347542213181,61.8314706464568));
#146282=CARTESIAN_POINT('Ctrl Pts',(6.86150975109376,1.45279352336208,61.839760686438));
#146283=CARTESIAN_POINT('Ctrl Pts',(6.81907938419261,1.63027081019669,61.8480507264193));
#146284=CARTESIAN_POINT('Ctrl Pts',(6.7785388798998,1.7998431998382,61.8559715252714));
#146285=CARTESIAN_POINT('Ctrl Pts',(6.73170975517686,1.96773496389655,61.8638923241236));
#146286=CARTESIAN_POINT('Ctrl Pts',(6.67876767326888,2.13346875510251,61.8718131229757));
#146287=CARTESIAN_POINT('Ctrl Pts',(6.64534233145582,2.23810590614353,61.8768139729522));
#146288=CARTESIAN_POINT('Ctrl Pts',(6.60944418485232,2.34199880220716,61.8818148229287));
#146289=CARTESIAN_POINT('Ctrl Pts',(6.57110895151817,2.44502632087627,61.8868156729052));
#146290=CARTESIAN_POINT('',(7.01124977383073,-0.00178085893519804,61.2264656430588));
#146291=CARTESIAN_POINT('Ctrl Pts',(6.57110895151815,2.44502632087632,61.3398717892601));
#146292=CARTESIAN_POINT('Ctrl Pts',(6.63164596423562,2.2823306055912,61.3320191079328));
#146293=CARTESIAN_POINT('Ctrl Pts',(6.68612743998776,2.11740963806755,61.3241664266055));
#146294=CARTESIAN_POINT('Ctrl Pts',(6.7343971179006,1.95077472326052,61.3163137452782));
#146295=CARTESIAN_POINT('Ctrl Pts',(6.78267671899837,1.78410555197722,61.3084594496122));
#146296=CARTESIAN_POINT('Ctrl Pts',(6.82474188414918,1.61572210142618,61.3006051539462));
#146297=CARTESIAN_POINT('Ctrl Pts',(6.86048707053804,1.4461478892148,61.2927508582802));
#146298=CARTESIAN_POINT('Ctrl Pts',(6.89626942910293,1.27639733319035,61.2848883947658));
#146299=CARTESIAN_POINT('Ctrl Pts',(6.92571861128505,1.10545391742226,61.2770259312515));
#146300=CARTESIAN_POINT('Ctrl Pts',(6.94878064777434,0.933849062545336,
61.2691634677372));
#146301=CARTESIAN_POINT('Ctrl Pts',(6.97177862027636,0.762720908468189,
61.2613228453453));
#146302=CARTESIAN_POINT('Ctrl Pts',(6.98842491556832,0.59093536336877,61.2534822229534));
#146303=CARTESIAN_POINT('Ctrl Pts',(6.99871765569726,0.419019973666483,
61.2456416005615));
#146304=CARTESIAN_POINT('Ctrl Pts',(7.00710870499223,0.27886774097779,61.2392496147375));
#146305=CARTESIAN_POINT('Ctrl Pts',(7.01128541614006,0.138543129239347,
61.2328576289136));
#146306=CARTESIAN_POINT('Ctrl Pts',(7.0112497738309,-0.00178085825863861,
61.2264656430896));
#146307=CARTESIAN_POINT('Ctrl Pts',(7.01124977383073,-0.00178085893530164,
61.2264656430588));
#146308=CARTESIAN_POINT('Ctrl Pts',(7.01120349318839,-0.183987959526845,
61.2181658133235));
#146309=CARTESIAN_POINT('Ctrl Pts',(7.00405009571344,-0.366345146885556,
61.2098659835883));
#146310=CARTESIAN_POINT('Ctrl Pts',(6.98978022374334,-0.548269081990379,
61.201566153853));
#146311=CARTESIAN_POINT('Ctrl Pts',(6.97552151841008,-0.730050655725633,
61.1932728190033));
#146312=CARTESIAN_POINT('Ctrl Pts',(6.9541574639881,-0.911399316733849,
61.1849794841536));
#146313=CARTESIAN_POINT('Ctrl Pts',(6.92573074867032,-1.09173264099891,
61.1766861493038));
#146314=CARTESIAN_POINT('Ctrl Pts',(6.89732149485793,-1.27195519301059,
61.1683979087504));
#146315=CARTESIAN_POINT('Ctrl Pts',(6.86185828029754,-1.45116331791928,
61.1601096681969));
#146316=CARTESIAN_POINT('Ctrl Pts',(6.81943556082566,-1.62878027807512,
61.1518214276435));
#146317=CARTESIAN_POINT('Ctrl Pts',(6.77703176659377,-1.80631800135883,
61.143536884565));
#146318=CARTESIAN_POINT('Ctrl Pts',(6.72767473546444,-1.98226564625203,
61.1352523414865));
#146319=CARTESIAN_POINT('Ctrl Pts',(6.6715099690144,-2.15605688604023,61.126967798408));
#146320=CARTESIAN_POINT('Ctrl Pts',(6.61535405140371,-2.32982074476984,
61.1186845605711));
#146321=CARTESIAN_POINT('Ctrl Pts',(6.55239263567478,-2.50142855213749,
61.1104013227342));
#146322=CARTESIAN_POINT('Ctrl Pts',(6.48282118364402,-2.67032883057432,
61.1021180848974));
#146323=CARTESIAN_POINT('Ctrl Pts',(6.41325469007457,-2.83921707123599,
61.0938354374192));
#146324=CARTESIAN_POINT('Ctrl Pts',(6.33707922764114,-3.00539785430112,
61.0855527899411));
#146325=CARTESIAN_POINT('Ctrl Pts',(6.25453861104882,-3.16833920617719,
61.0772701424629));
#146326=CARTESIAN_POINT('Ctrl Pts',(6.17199128110482,-3.33129381071169,
61.0689868213246));
#146327=CARTESIAN_POINT('Ctrl Pts',(6.08307791799497,-3.49100815671002,
61.0607035001863));
#146328=CARTESIAN_POINT('Ctrl Pts',(5.98808868764945,-3.64697414733703,
61.052420179048));
#146329=CARTESIAN_POINT('Ctrl Pts',(5.89307723454667,-3.80297662625159,
61.0441349200243));
#146330=CARTESIAN_POINT('Ctrl Pts',(5.79198725699891,-3.95522871267261,
61.0358496610007));
#146331=CARTESIAN_POINT('Ctrl Pts',(5.68515286692431,-4.10325035090503,
61.0275644019771));
#146332=CARTESIAN_POINT('Ctrl Pts',(5.57822405302862,-4.2514028156314,61.0192718201633));
#146333=CARTESIAN_POINT('Ctrl Pts',(5.46554087860769,-4.39531708486661,
61.0109792383496));
#146334=CARTESIAN_POINT('Ctrl Pts',(5.34747918397504,-4.53454440263337,
61.0026866565358));
#146335=CARTESIAN_POINT('Ctrl Pts',(5.22936597961448,-4.67383246458374,
60.99439045671));
#146336=CARTESIAN_POINT('Ctrl Pts',(5.10586980112438,-4.80842924463886,
60.9860942568842));
#146337=CARTESIAN_POINT('Ctrl Pts',(4.9774044478282,-4.93792178200911,60.9777980570584));
#146338=CARTESIAN_POINT('Ctrl Pts',(4.84877759344969,-5.06757711179307,
60.9694914276093));
#146339=CARTESIAN_POINT('Ctrl Pts',(4.71516932244074,-5.19211513814238,
60.9611847981601));
#146340=CARTESIAN_POINT('Ctrl Pts',(4.57702879684953,-5.31116126240864,
60.9528781687109));
#146341=CARTESIAN_POINT('Ctrl Pts',(4.44081952894491,-5.42854307606393,
60.9446876691368));
#146342=CARTESIAN_POINT('Ctrl Pts',(4.30020418609226,-5.54058539599169,
60.9364971695627));
#146343=CARTESIAN_POINT('Ctrl Pts',(4.15564160387625,-5.6469699328607,60.9283066699885));
#146344=CARTESIAN_POINT('Ctrl Pts',(4.00771138083155,-5.7558327383412,60.9199253695837));
#146345=CARTESIAN_POINT('Ctrl Pts',(3.85532845952543,-5.85900610843106,
60.9115440691789));
#146346=CARTESIAN_POINT('Ctrl Pts',(3.69895524447717,-5.95611926188981,
60.903162768774));
#146347=CARTESIAN_POINT('Ctrl Pts',(3.54278020958773,-6.05310933864281,
60.8947920904405));
#146348=CARTESIAN_POINT('Ctrl Pts',(3.3826252353439,-6.14405433361975,60.8864214121071));
#146349=CARTESIAN_POINT('Ctrl Pts',(3.21898415823916,-6.22862485236551,
60.8780507337736));
#146350=CARTESIAN_POINT('Ctrl Pts',(3.0555287856611,-6.31309939809258,60.8696895547228));
#146351=CARTESIAN_POINT('Ctrl Pts',(2.8885954845283,-6.39121373610326,60.8613283756721));
#146352=CARTESIAN_POINT('Ctrl Pts',(2.71870570118038,-6.46268256011924,
60.8529671966213));
#146353=CARTESIAN_POINT('Ctrl Pts',(2.54903636986627,-6.53405864490571,
60.8446168671866));
#146354=CARTESIAN_POINT('Ctrl Pts',(2.37641850900181,-6.59880628940873,
60.836266537752));
#146355=CARTESIAN_POINT('Ctrl Pts',(2.20139663402076,-6.65668682019983,
60.8279162083173));
#146356=CARTESIAN_POINT('Ctrl Pts',(2.02650942790268,-6.7145228153849,60.8195723039616));
#146357=CARTESIAN_POINT('Ctrl Pts',(1.84922220363346,-6.76550212413633,
60.8112283996059));
#146358=CARTESIAN_POINT('Ctrl Pts',(1.67009892937172,-6.80943434718417,
60.8028844952502));
#146359=CARTESIAN_POINT('Ctrl Pts',(1.49111952804158,-6.85333128359632,
60.7945472927706));
#146360=CARTESIAN_POINT('Ctrl Pts',(1.31030733514935,-6.89019234507178,
60.786210090291));
#146361=CARTESIAN_POINT('Ctrl Pts',(1.12824108500719,-6.91987706658159,
60.7778728878113));
#146362=CARTESIAN_POINT('Ctrl Pts',(1.06830588043472,-6.92964911304807,
60.7751283267749));
#146363=CARTESIAN_POINT('Ctrl Pts',(1.00823488468427,-6.93864387184233,
60.7723837657386));
#146364=CARTESIAN_POINT('Ctrl Pts',(0.948049037360293,-6.94685753310518,
60.7696392047022));
#146365=CARTESIAN_POINT('Ctrl Pts',(0.765197111634181,-6.97181163520646,
60.7613008944002));
#146366=CARTESIAN_POINT('Ctrl Pts',(0.581434511015953,-6.98953177441674,
60.7529625840983));
#146367=CARTESIAN_POINT('Ctrl Pts',(0.397356357399926,-6.99998103481244,
60.7446242737963));
#146368=CARTESIAN_POINT('Ctrl Pts',(0.213162388055935,-7.01043686952822,
60.7362807173124));
#146369=CARTESIAN_POINT('Ctrl Pts',(0.0286527968346948,-7.01361268227103,
60.7279371608286));
#146370=CARTESIAN_POINT('Ctrl Pts',(-0.15557683528507,-7.00952369357738,
60.7195936043447));
#146371=CARTESIAN_POINT('Ctrl Pts',(-0.33994662850615,-7.00543159399895,
60.7112437001194));
#146372=CARTESIAN_POINT('Ctrl Pts',(-0.524035710577234,-6.99406367562674,
60.7028937958941));
#146373=CARTESIAN_POINT('Ctrl Pts',(-0.707252720357442,-6.97548709066593,
60.6945438916689));
#146374=CARTESIAN_POINT('Ctrl Pts',(-0.89074454209414,-6.95688264220235,
60.6861814632051));
#146375=CARTESIAN_POINT('Ctrl Pts',(-1.07336135139443,-6.93104795352176,
60.6778190347414));
#146376=CARTESIAN_POINT('Ctrl Pts',(-1.2545195889691,-6.89810170723749,
60.6694566062777));
#146377=CARTESIAN_POINT('Ctrl Pts',(-1.43583274153234,-6.86512728742143,
60.6610870267977));
#146378=CARTESIAN_POINT('Ctrl Pts',(-1.61568451468976,-6.82502924726269,
60.6527174473177));
#146379=CARTESIAN_POINT('Ctrl Pts',(-1.79350509203785,-6.77797654520391,
60.6443478678377));
#146380=CARTESIAN_POINT('Ctrl Pts',(-1.97159993596103,-6.73085127008505,
60.635965379301));
#146381=CARTESIAN_POINT('Ctrl Pts',(-2.1476570110733,-6.67674999394005,
60.6275828907644));
#146382=CARTESIAN_POINT('Ctrl Pts',(-2.3211237640995,-6.61589079672818,
60.6192004022278));
#146383=CARTESIAN_POINT('Ctrl Pts',(-2.37788492810306,-6.59597667016615,
60.6164575146238));
#146384=CARTESIAN_POINT('Ctrl Pts',(-2.43436892249107,-6.57533934513027,
60.6137146270197));
#146385=CARTESIAN_POINT('Ctrl Pts',(-2.49055693275975,-6.553987544021,60.6109717394157));
#146386=CARTESIAN_POINT('Ctrl Pts',(-2.6624229857697,-6.48867735126354,
60.6025818842829));
#146387=CARTESIAN_POINT('Ctrl Pts',(-2.83186510552412,-6.41654712207527,
60.5941920291502));
#146388=CARTESIAN_POINT('Ctrl Pts',(-2.99832485660896,-6.33779730006734,
60.5858021740174));
#146389=CARTESIAN_POINT('Ctrl Pts',(-3.16463100096917,-6.25912014729113,
60.5774200609253));
#146390=CARTESIAN_POINT('Ctrl Pts',(-3.32795996722733,-6.17383571881712,
60.5690379478332));
#146391=CARTESIAN_POINT('Ctrl Pts',(-3.48777249563173,-6.08219282670443,
60.5606558347412));
#146392=CARTESIAN_POINT('Ctrl Pts',(-3.64746104338542,-5.99062103005285,
60.5522802243923));
#146393=CARTESIAN_POINT('Ctrl Pts',(-3.80363830796317,-5.89270076724273,
60.5439046140434));
#146394=CARTESIAN_POINT('Ctrl Pts',(-3.95578847193313,-5.78872733230897,
60.5355290036946));
#146395=CARTESIAN_POINT('Ctrl Pts',(-4.10784293119036,-5.6848192982099,
60.527158661729));
#146396=CARTESIAN_POINT('Ctrl Pts',(-4.25587506991755,-5.57486586886242,
60.5187883197634));
#146397=CARTESIAN_POINT('Ctrl Pts',(-4.39939659076748,-5.45920655403727,
60.5104179777979));
#146398=CARTESIAN_POINT('Ctrl Pts',(-4.54284887309268,-5.343603036282,60.5020516739036));
#146399=CARTESIAN_POINT('Ctrl Pts',(-4.68179462141666,-5.22229932821359,
60.4936853700093));
#146400=CARTESIAN_POINT('Ctrl Pts',(-4.81577691361216,-5.09567652827573,
60.485319066115));
#146401=CARTESIAN_POINT('Ctrl Pts',(-4.94972173471596,-4.96908914118586,
60.4769551020414));
#146402=CARTESIAN_POINT('Ctrl Pts',(-5.07870562797895,-4.83718585297373,
60.4685911379677));
#146403=CARTESIAN_POINT('Ctrl Pts',(-5.20230657686822,-4.70038645674733,
60.4602271738941));
#146404=CARTESIAN_POINT('Ctrl Pts',(-5.32588850562545,-4.56360811167468,
60.4518644968956));
#146405=CARTESIAN_POINT('Ctrl Pts',(-5.4440889212943,-4.42193540456727,
60.4435018198971));
#146406=CARTESIAN_POINT('Ctrl Pts',(-5.55652406798683,-4.2758235282087,
60.4351391428986));
#146407=CARTESIAN_POINT('Ctrl Pts',(-5.66895689984519,-4.12971466002662,
60.4267766380723));
#146408=CARTESIAN_POINT('Ctrl Pts',(-5.77562449929959,-3.97916706553816,
60.418414133246));
#146409=CARTESIAN_POINT('Ctrl Pts',(-5.87618440035397,-3.82466775753616,
60.4100516284197));
#146410=CARTESIAN_POINT('Ctrl Pts',(-5.97675563498276,-3.67015103673457,
60.4016881810997));
#146411=CARTESIAN_POINT('Ctrl Pts',(-6.07121761998422,-3.51168199019138,
60.3933247337797));
#146412=CARTESIAN_POINT('Ctrl Pts',(-6.15927186734285,-3.34977560840408,
60.3849612864598));
#146413=CARTESIAN_POINT('Ctrl Pts',(-6.247377963517,-3.18777389158897,60.376592914507));
#146414=CARTESIAN_POINT('Ctrl Pts',(-6.3290686245528,-3.02233108365956,
60.3682245425542));
#146415=CARTESIAN_POINT('Ctrl Pts',(-6.40409141329752,-2.85398663848115,
60.3598561706014));
#146416=CARTESIAN_POINT('Ctrl Pts',(-6.47913668083047,-2.68559175290729,
60.3514852912657));
#146417=CARTESIAN_POINT('Ctrl Pts',(-6.5475099633949,-2.51429379891878,
60.3431144119299));
#146418=CARTESIAN_POINT('Ctrl Pts',(-6.6090071798928,-2.34065175936649,
60.3347435325942));
#146419=CARTESIAN_POINT('Ctrl Pts',(-6.67055650231725,-2.16686259479172,
60.3263655607029));
#146420=CARTESIAN_POINT('Ctrl Pts',(-6.72521801252132,-1.9907256878751,
60.3179875888116));
#146421=CARTESIAN_POINT('Ctrl Pts',(-6.77283731893193,-1.81281582456216,
60.3096096169203));
#146422=CARTESIAN_POINT('Ctrl Pts',(-6.80309977592204,-1.69975265769871,
60.3042853475612));
#146423=CARTESIAN_POINT('Ctrl Pts',(-6.83051910817107,-1.58597371990945,
60.2989610782021));
#146424=CARTESIAN_POINT('Ctrl Pts',(-6.85506642330611,-1.47162865375785,
60.293636808843));
#146425=CARTESIAN_POINT('Ctrl Pts',(-6.89131766869568,-1.30276492958497,
60.2857739776537));
#146426=CARTESIAN_POINT('Ctrl Pts',(-6.92137795629609,-1.13231489320908,
60.2779111464644));
#146427=CARTESIAN_POINT('Ctrl Pts',(-6.94510661887924,-0.960791660507012,
60.2700483152751));
#146428=CARTESIAN_POINT('Ctrl Pts',(-6.96881704911733,-0.789400220768501,
60.2621915256337));
#146429=CARTESIAN_POINT('Ctrl Pts',(-6.9862054772162,-0.616937599792321,
60.2543347359923));
#146430=CARTESIAN_POINT('Ctrl Pts',(-6.99718182459544,-0.443929134041922,
60.2464779463509));
#146431=CARTESIAN_POINT('Ctrl Pts',(-7.00815198183436,-0.27101823687632,
60.2386255875669));
#146432=CARTESIAN_POINT('Ctrl Pts',(-7.01271722755956,-0.0975624866027649,
60.2307732287829));
#146433=CARTESIAN_POINT('Ctrl Pts',(-7.01083909849225,0.0759058466283117,
60.2229208699989));
#146434=CARTESIAN_POINT('Ctrl Pts',(-7.00896141287313,0.249333221961846,
60.2150703652485));
#146435=CARTESIAN_POINT('Ctrl Pts',(-7.00064337606927,0.422772793345405,
60.207219860498));
#146436=CARTESIAN_POINT('Ctrl Pts',(-6.98589860770976,0.595690528125873,
60.1993693557476));
#146437=CARTESIAN_POINT('Ctrl Pts',(-6.97115621131877,0.768580445892675,
60.1915201138959));
#146438=CARTESIAN_POINT('Ctrl Pts',(-6.94998917689306,0.940948314276102,
60.1836708720442));
#146439=CARTESIAN_POINT('Ctrl Pts',(-6.9224631093025,1.11226393578411,60.1758216301926));
#146440=CARTESIAN_POINT('Ctrl Pts',(-6.89492776764099,1.28363727687826,
60.1679697437777));
#146441=CARTESIAN_POINT('Ctrl Pts',(-6.86102917391458,1.45395728593272,
60.1601178573628));
#146442=CARTESIAN_POINT('Ctrl Pts',(-6.82088434045903,1.62270249170353,
60.1522659709479));
#146443=CARTESIAN_POINT('Ctrl Pts',(-6.79140648892611,1.74660999596832,
60.1465004284841));
#146444=CARTESIAN_POINT('Ctrl Pts',(-6.75856187735721,1.8696685699544,60.1407348860203));
#146445=CARTESIAN_POINT('Ctrl Pts',(-6.72241403827011,1.99167669579403,
60.1349693435565));
#146446=CARTESIAN_POINT('Ctrl Pts',(-6.66187881707922,2.19599842210773,
60.1253140391967));
#146447=CARTESIAN_POINT('Ctrl Pts',(-6.5921100323113,2.39726976123393,60.115658734837));
#146448=CARTESIAN_POINT('Ctrl Pts',(-6.513437275972,2.59475652315945,60.1060034304772));
#146449=CARTESIAN_POINT('Ctrl Pts',(-6.43432868732159,2.79333732469751,
60.0962946375426));
#146450=CARTESIAN_POINT('Ctrl Pts',(-6.34621726946916,2.98809147761485,
60.0865858446081));
#146451=CARTESIAN_POINT('Ctrl Pts',(-6.24948186149068,3.17830190910162,
60.0768770516735));
#146452=CARTESIAN_POINT('Ctrl Pts',(-6.15228095451501,3.36942764933584,
60.0671215392029));
#146453=CARTESIAN_POINT('Ctrl Pts',(-6.04637289996954,3.5559658056905,60.0573660267324));
#146454=CARTESIAN_POINT('Ctrl Pts',(-5.93218523847481,3.73721886687434,
60.0476105142618));
#146455=CARTESIAN_POINT('Ctrl Pts',(-5.81788451362779,3.91865139647398,
60.037845342333));
#146456=CARTESIAN_POINT('Ctrl Pts',(-5.6952878136832,4.09478833711091,60.0280801704043));
#146457=CARTESIAN_POINT('Ctrl Pts',(-5.56486651922017,4.26496039674021,
60.0183149984755));
#146458=CARTESIAN_POINT('Ctrl Pts',(-5.43462305123304,4.4349004306272,60.0085631411371));
#146459=CARTESIAN_POINT('Ctrl Pts',(-5.29657633465462,4.59889180831757,
59.9988112837987));
#146460=CARTESIAN_POINT('Ctrl Pts',(-5.15123779084723,4.75629853821723,
59.9890594264603));
#146461=CARTESIAN_POINT('Ctrl Pts',(-5.08785965981767,4.82493927240359,
59.9848069103969));
#146462=CARTESIAN_POINT('Ctrl Pts',(-5.0230954581525,4.89232827086292,59.9805543943335));
#146463=CARTESIAN_POINT('Ctrl Pts',(-4.95699008884031,4.95841464801392,
59.9763018782701));
#146464=CARTESIAN_POINT('Ctrl Pts',(-4.8321163815815,5.08325247888928,59.9682688326712));
#146465=CARTESIAN_POINT('Ctrl Pts',(-4.70239330495944,5.20350034449769,
59.9602357870723));
#146466=CARTESIAN_POINT('Ctrl Pts',(-4.56819969400882,5.31875719676672,
59.9522027414734));
#146467=CARTESIAN_POINT('Ctrl Pts',(-4.4340923478782,5.43393995749335,59.9441748598256));
#146468=CARTESIAN_POINT('Ctrl Pts',(-4.29552046477135,5.5441378534666,59.9361469781777));
#146469=CARTESIAN_POINT('Ctrl Pts',(-4.15289952347646,5.64898682158217,
59.9281190965298));
#146470=CARTESIAN_POINT('Ctrl Pts',(-4.01034297694249,5.75378844935505,
59.9200948395496));
#146471=CARTESIAN_POINT('Ctrl Pts',(-3.86374130708915,5.85324574132342,
59.9120705825695));
#146472=CARTESIAN_POINT('Ctrl Pts',(-3.71354280164434,5.94703509514241,
59.9040463255893));
#146473=CARTESIAN_POINT('Ctrl Pts',(-3.56336245672864,6.04081310887327,
59.8960230388235));
#146474=CARTESIAN_POINT('Ctrl Pts',(-3.40958644912039,6.12892434889666,
59.8879997520578));
#146475=CARTESIAN_POINT('Ctrl Pts',(-3.25269190640852,6.21108862635887,
59.879976465292));
#146476=CARTESIAN_POINT('Ctrl Pts',(-3.09581021980487,6.29324617119148,
59.871953835963));
#146477=CARTESIAN_POINT('Ctrl Pts',(-2.93581083376654,6.36945755758264,
59.863931206634));
#146478=CARTESIAN_POINT('Ctrl Pts',(-2.77319504625346,6.439488783897,59.855908577305));
#146479=CARTESIAN_POINT('Ctrl Pts',(-2.61051812678136,6.50954633696673,
59.8478829320385));
#146480=CARTESIAN_POINT('Ctrl Pts',(-2.44522317905844,6.57341894644921,
59.8398572867721));
#146481=CARTESIAN_POINT('Ctrl Pts',(-2.27783138019637,6.63092080829599,
59.8318316415056));
#146482=CARTESIAN_POINT('Ctrl Pts',(-2.17912697524418,6.66482741002804,
59.8270992319982));
#146483=CARTESIAN_POINT('Ctrl Pts',(-2.07969383546348,6.69651983059121,
59.8223668224909));
#146484=CARTESIAN_POINT('Ctrl Pts',(-1.97964121801694,6.72596812439878,
59.8176344129836));
#146485=CARTESIAN_POINT('Ctrl Pts',(-1.79507049670079,6.78029246861194,
59.8089043641491));
#146486=CARTESIAN_POINT('Ctrl Pts',(-1.60829873307994,6.82700461812528,
59.8001743153145));
#146487=CARTESIAN_POINT('Ctrl Pts',(-1.41995570843133,6.86595604039185,
59.79144426648));
#146488=CARTESIAN_POINT('Ctrl Pts',(-1.23155822416242,6.90491872551071,
59.7827116933409));
#146489=CARTESIAN_POINT('Ctrl Pts',(-1.04158884025968,6.93611614870944,
59.7739791202019));
#146490=CARTESIAN_POINT('Ctrl Pts',(-0.850687128395915,6.95945098208771,
59.7652465470628));
#146491=CARTESIAN_POINT('Ctrl Pts',(-0.657073352975061,6.98311732402396,
59.7563899137824));
#146492=CARTESIAN_POINT('Ctrl Pts',(-0.462500844984582,6.99869593704891,
59.7475332805019));
#146493=CARTESIAN_POINT('Ctrl Pts',(-0.267642234641472,7.00613975001471,
59.7386766472214));
#146494=CARTESIAN_POINT('Ctrl Pts',(-0.0753908197555502,7.01348396525006,
59.7299385151148));
#146495=CARTESIAN_POINT('Ctrl Pts',(0.117138810529907,7.01290972725822,
59.7212003830082));
#146496=CARTESIAN_POINT('Ctrl Pts',(0.309299626698119,7.00442433776141,
59.7124622509015));
#146497=CARTESIAN_POINT('Ctrl Pts',(0.505369393085973,6.99576633781364,
59.7035463670341));
#146498=CARTESIAN_POINT('Ctrl Pts',(0.701054883652899,6.97887188955907,
59.6946304831668));
#146499=CARTESIAN_POINT('Ctrl Pts',(0.895672117836021,6.9538045715875,59.6857145992994));
#146500=CARTESIAN_POINT('Ctrl Pts',(1.09028935201921,6.92873725361591,59.676798715432));
#146501=CARTESIAN_POINT('Ctrl Pts',(1.28383803066124,6.89549711059299,59.6678828315646));
#146502=CARTESIAN_POINT('Ctrl Pts',(1.4756420337927,6.85420361169729,59.6589669476973));
#146503=CARTESIAN_POINT('Ctrl Pts',(1.66367703979367,6.81372154048978,59.6502262632009));
#146504=CARTESIAN_POINT('Ctrl Pts',(1.850055271653,6.76549537689206,59.6414855787046));
#146505=CARTESIAN_POINT('Ctrl Pts',(2.03414967566964,6.70968416987514,59.6327448942083));
#146506=CARTESIAN_POINT('Ctrl Pts',(2.21821095804526,6.65388300422137,59.6240057823063));
#146507=CARTESIAN_POINT('Ctrl Pts',(2.39998897124958,6.59049959991576,59.6152666704043));
#146508=CARTESIAN_POINT('Ctrl Pts',(2.57887153829044,6.51974295133601,59.6065275585022));
#146509=CARTESIAN_POINT('Ctrl Pts',(2.76007178644062,6.44806954853875,59.5976752188279));
#146510=CARTESIAN_POINT('Ctrl Pts',(2.93830076275092,6.36883059152284,59.5888228791536));
#146511=CARTESIAN_POINT('Ctrl Pts',(3.11294149548016,6.28229431085633,59.5799705394793));
#146512=CARTESIAN_POINT('Ctrl Pts',(3.28526008042121,6.19690867832102,59.5712359068295));
#146513=CARTESIAN_POINT('Ctrl Pts',(3.45408500730464,6.10441871501682,59.5625012741796));
#146514=CARTESIAN_POINT('Ctrl Pts',(3.61884597440103,6.00512950535303,59.5537666415298));
#146515=CARTESIAN_POINT('Ctrl Pts',(3.78693739464137,5.90383327869782,59.5448554483432));
#146516=CARTESIAN_POINT('Ctrl Pts',(3.95079854883831,5.79546013155386,59.5359442551567));
#146517=CARTESIAN_POINT('Ctrl Pts',(4.10985167052522,5.68038254070807,59.5270330619702));
#146518=CARTESIAN_POINT('Ctrl Pts',(4.26890479221214,5.56530494986227,59.5181218687837));
#146519=CARTESIAN_POINT('Ctrl Pts',(4.42314962790079,5.44352308208674,59.5092106755972));
#146520=CARTESIAN_POINT('Ctrl Pts',(4.57204038025183,5.3154560786302,59.5002994824107));
#146521=CARTESIAN_POINT('Ctrl Pts',(4.70613547312816,5.20011542481706,59.4922738175583));
#146522=CARTESIAN_POINT('Ctrl Pts',(4.83594899628315,5.07962330972136,59.484248152706));
#146523=CARTESIAN_POINT('Ctrl Pts',(4.96106213967889,4.95434042116049,59.4762224878536));
#146524=CARTESIAN_POINT('Ctrl Pts',(5.08613557523176,4.82909729431546,59.4681993701504));
#146525=CARTESIAN_POINT('Ctrl Pts',(5.206511342309,4.69906668019786,59.4601762524472));
#146526=CARTESIAN_POINT('Ctrl Pts',(5.32180619378596,4.56464734654074,59.452153134744));
#146527=CARTESIAN_POINT('Ctrl Pts',(5.43708650557331,4.43024496433778,59.4441310288262));
#146528=CARTESIAN_POINT('Ctrl Pts',(5.5472869399191,4.29145524356305,59.4361089229083));
#146529=CARTESIAN_POINT('Ctrl Pts',(5.65206342293754,4.14871132107207,59.4280868169905));
#146530=CARTESIAN_POINT('Ctrl Pts',(5.75687884125086,4.0059143544575,59.420061730031));
#146531=CARTESIAN_POINT('Ctrl Pts',(5.85626606225826,3.85916054474957,59.4120366430715));
#146532=CARTESIAN_POINT('Ctrl Pts',(5.94992312727897,3.7089137684733,59.404011556112));
#146533=CARTESIAN_POINT('Ctrl Pts',(6.04359863759,3.55863740184624,59.3959848886518));
#146534=CARTESIAN_POINT('Ctrl Pts',(6.13154155727149,3.40486701393061,59.3879582211916));
#146535=CARTESIAN_POINT('Ctrl Pts',(6.21349519490292,3.24809236713157,59.3799315537313));
#146536=CARTESIAN_POINT('Ctrl Pts',(6.2955146246258,3.09119186219863,59.3718984424908));
#146537=CARTESIAN_POINT('Ctrl Pts',(6.37153500761923,2.93128261050024,59.3638653312502));
#146538=CARTESIAN_POINT('Ctrl Pts',(6.44134697279782,2.76887625915793,59.3558322200097));
#146539=CARTESIAN_POINT('Ctrl Pts',(6.48248271874028,2.67318053721156,59.3510988190479));
#146540=CARTESIAN_POINT('Ctrl Pts',(6.521463823452,2.57661819015167,59.3463654180861));
#146541=CARTESIAN_POINT('Ctrl Pts',(6.55825550999446,2.47929651879869,59.3416320171243));
#146542=CARTESIAN_POINT('Ctrl Pts',(6.56256998608823,2.46788383120762,59.3410769421275));
#146543=CARTESIAN_POINT('Ctrl Pts',(6.56685448137081,2.45646038464508,59.3405218671306));
#146544=CARTESIAN_POINT('Ctrl Pts',(6.57110895151816,2.4450263208763,59.3399667921338));
#146545=CARTESIAN_POINT('Origin',(0.,0.,50.));
#146546=CARTESIAN_POINT('',(6.57110895151816,2.4450263208763,57.3398522865015));
#146547=CARTESIAN_POINT('',(6.57110895151813,2.44502632087639,57.8870048219557));
#146548=CARTESIAN_POINT('',(6.57110895151814,2.44502632087636,50.));
#146549=CARTESIAN_POINT('',(7.01124999602994,-0.000235945344234768,59.7735343568684));
#146550=CARTESIAN_POINT('Ctrl Pts',(6.57110895151813,2.44502632087639,57.8870048219557));
#146551=CARTESIAN_POINT('Ctrl Pts',(6.52450546921719,2.57027509922486,57.8930453782421));
#146552=CARTESIAN_POINT('Ctrl Pts',(6.47430760150655,2.69422367287727,57.8990859345286));
#146553=CARTESIAN_POINT('Ctrl Pts',(6.42059905730801,2.816653032909,57.905126490815));
#146554=CARTESIAN_POINT('Ctrl Pts',(6.34646043726219,2.98565302986097,57.9134648011168));
#146555=CARTESIAN_POINT('Ctrl Pts',(6.26567581471899,3.15165466081322,57.9218031114186));
#146556=CARTESIAN_POINT('Ctrl Pts',(6.17852427623118,3.31413100684357,57.9301414217204));
#146557=CARTESIAN_POINT('Ctrl Pts',(6.09131790495256,3.47670957747773,57.9384849782041));
#146558=CARTESIAN_POINT('Ctrl Pts',(5.99773678244466,3.63575815039843,57.9468285346878));
#146559=CARTESIAN_POINT('Ctrl Pts',(5.8981047085228,3.79077662356954,57.9551720911715));
#146560=CARTESIAN_POINT('Ctrl Pts',(5.79839683495317,3.94591303411963,57.9635219953967));
#146561=CARTESIAN_POINT('Ctrl Pts',(5.69262900436559,4.09701295376717,57.9718718996218));
#146562=CARTESIAN_POINT('Ctrl Pts',(5.58116711335293,4.24360698172295,57.9802218038469));
#146563=CARTESIAN_POINT('Ctrl Pts',(5.46953803775208,4.3904208898725,57.9885842323105));
#146564=CARTESIAN_POINT('Ctrl Pts',(5.35219803326782,4.5327151396672,57.9969466607741));
#146565=CARTESIAN_POINT('Ctrl Pts',(5.22955288163711,4.6700538777043,58.0053090892377));
#146566=CARTESIAN_POINT('Ctrl Pts',(5.10680285168271,4.80751005908451,58.0136786687175));
#146567=CARTESIAN_POINT('Ctrl Pts',(4.97873885001579,4.9400020384957,58.0220482481974));
#146568=CARTESIAN_POINT('Ctrl Pts',(4.84580237287856,5.06713192304133,58.0304178276773));
#146569=CARTESIAN_POINT('Ctrl Pts',(4.71266085742252,5.19445788994418,58.0388003162137));
#146570=CARTESIAN_POINT('Ctrl Pts',(4.57463209395561,5.31640501878296,58.0471828047502));
#146571=CARTESIAN_POINT('Ctrl Pts',(4.43219047145647,5.43261577761859,58.0555652932867));
#146572=CARTESIAN_POINT('Ctrl Pts',(4.38558123852113,5.47064184214335,58.0583081808916));
#146573=CARTESIAN_POINT('Ctrl Pts',(4.33849974627091,5.50805405801524,58.0610510684965));
#146574=CARTESIAN_POINT('Ctrl Pts',(4.29096325386765,5.54484092796697,58.0637939561013));
#146575=CARTESIAN_POINT('Ctrl Pts',(4.14556018154534,5.65736340578731,58.0721838112342));
#146576=CARTESIAN_POINT('Ctrl Pts',(3.99560443078813,5.76425903116473,58.080573666367));
#146577=CARTESIAN_POINT('Ctrl Pts',(3.84155841605354,5.86515605065613,58.0889635214998));
#146578=CARTESIAN_POINT('Ctrl Pts',(3.68765455282126,5.96595996379276,58.097345634592));
#146579=CARTESIAN_POINT('Ctrl Pts',(3.52966822361311,6.06077612667109,58.1057277476842));
#146580=CARTESIAN_POINT('Ctrl Pts',(3.36809309514126,6.14927438523943,58.1141098607763));
#146581=CARTESIAN_POINT('Ctrl Pts',(3.20664331472488,6.23770398791544,58.1224854711252));
#146582=CARTESIAN_POINT('Ctrl Pts',(3.0416105730649,6.31982530074116,58.1308610814741));
#146583=CARTESIAN_POINT('Ctrl Pts',(2.87351595327708,6.39535242412505,58.139236691823));
#146584=CARTESIAN_POINT('Ctrl Pts',(2.70552706750145,6.47083203982669,58.1476070337886));
#146585=CARTESIAN_POINT('Ctrl Pts',(2.53448044288038,6.53972560213424,58.1559773757542));
#146586=CARTESIAN_POINT('Ctrl Pts',(2.36092051770871,6.60179376166524,58.1643477177198));
#146587=CARTESIAN_POINT('Ctrl Pts',(2.1874443223696,6.66383197789798,58.1727140216142));
#146588=CARTESIAN_POINT('Ctrl Pts',(2.01145755333925,6.71905124714059,58.1810803255087));
#146589=CARTESIAN_POINT('Ctrl Pts',(1.83352375125979,6.76726068775736,58.1894466294031));
#146590=CARTESIAN_POINT('Ctrl Pts',(1.65563971227895,6.81545664554445,58.1978105934767));
#146591=CARTESIAN_POINT('Ctrl Pts',(1.47581004259518,6.85664659655504,58.2061745575504));
#146592=CARTESIAN_POINT('Ctrl Pts',(1.29461307413814,6.89068962809751,58.214538521624));
#146593=CARTESIAN_POINT('Ctrl Pts',(1.11344398888363,6.92472742098311,58.2229011986226));
#146594=CARTESIAN_POINT('Ctrl Pts',(0.930908347273212,6.95162042649785,
58.2312638756212));
#146595=CARTESIAN_POINT('Ctrl Pts',(0.747594710914991,6.97127884327631,
58.2396265526197));
#146596=CARTESIAN_POINT('Ctrl Pts',(0.564284848649643,6.99093685532389,
58.247989057446));
#146597=CARTESIAN_POINT('Ctrl Pts',(0.380197350393221,7.00336054099226,
58.2563515622724));
#146598=CARTESIAN_POINT('Ctrl Pts',(0.195926373013485,7.0085119261408,58.2647140670987));
#146599=CARTESIAN_POINT('Ctrl Pts',(0.0116346274260749,7.01366389187472,
58.2730775144187));
#146600=CARTESIAN_POINT('Ctrl Pts',(-0.172840309989962,7.01154191434983,
58.2814409617387));
#146601=CARTESIAN_POINT('Ctrl Pts',(-0.356903367522352,7.00216013446931,
58.2898044090588));
#146602=CARTESIAN_POINT('Ctrl Pts',(-0.541074806555653,6.99277283033314,
58.2981727810116));
#146603=CARTESIAN_POINT('Ctrl Pts',(-0.724833552456556,6.97611719760979,
58.3065411529645));
#146604=CARTESIAN_POINT('Ctrl Pts',(-0.907587698260507,6.95225942643586,
58.3149095249173));
#146605=CARTESIAN_POINT('Ctrl Pts',(-1.09039660198301,6.92839450685012,
58.3232804042531));
#146606=CARTESIAN_POINT('Ctrl Pts',(-1.27219998014171,6.89732319371543,
58.3316512835889));
#146607=CARTESIAN_POINT('Ctrl Pts',(-1.45241450268126,6.85916311767705,
58.3400221629247));
#146608=CARTESIAN_POINT('Ctrl Pts',(-1.6327817190366,6.82097070901897,58.348400134816));
#146609=CARTESIAN_POINT('Ctrl Pts',(-1.81155706911948,6.77567760933404,
58.3567781067074));
#146610=CARTESIAN_POINT('Ctrl Pts',(-1.98816967395938,6.72345208282533,
58.3651560785987));
#146611=CARTESIAN_POINT('Ctrl Pts',(-2.10040842248689,6.69026233545797,
58.3704803479572));
#146612=CARTESIAN_POINT('Ctrl Pts',(-2.21177399738411,6.65427379297141,
58.3758046173158));
#146613=CARTESIAN_POINT('Ctrl Pts',(-2.32212367178652,6.61553990354746,
58.3811288866743));
#146614=CARTESIAN_POINT('Ctrl Pts',(-2.48508703881145,6.55833805793548,
58.3889917178636));
#146615=CARTESIAN_POINT('Ctrl Pts',(-2.64617268895316,6.49502732338538,
58.3968545490528));
#146616=CARTESIAN_POINT('Ctrl Pts',(-2.80486951165799,6.42575548749495,
58.4047173802421));
#146617=CARTESIAN_POINT('Ctrl Pts',(-2.96344439680265,6.35653687786648,
58.4125741698835));
#146618=CARTESIAN_POINT('Ctrl Pts',(-3.11963375748957,6.28136642706461,
58.4204309595249));
#146619=CARTESIAN_POINT('Ctrl Pts',(-3.27294245944308,6.20044145361237,
58.4282877491663));
#146620=CARTESIAN_POINT('Ctrl Pts',(-3.4261647025459,6.11956211801439,58.4361401079502));
#146621=CARTESIAN_POINT('Ctrl Pts',(-3.5765091823989,6.03293489279628,58.4439924667342));
#146622=CARTESIAN_POINT('Ctrl Pts',(-3.72350178664023,5.94080474408872,
58.4518448255181));
#146623=CARTESIAN_POINT('Ctrl Pts',(-3.87045968421232,5.84869634838441,
58.4596953302685));
#146624=CARTESIAN_POINT('Ctrl Pts',(-4.01406695406378,5.75108781031801,
58.467545835019));
#146625=CARTESIAN_POINT('Ctrl Pts',(-4.1538751609237,5.64826944381738,58.4753963397694));
#146626=CARTESIAN_POINT('Ctrl Pts',(-4.29366087704949,5.54546761755139,
58.483245581621));
#146627=CARTESIAN_POINT('Ctrl Pts',(-4.42964844122439,5.43745785971971,
58.4910948234726));
#146628=CARTESIAN_POINT('Ctrl Pts',(-4.56141981924342,5.32457282747765,
58.4989440653242));
#146629=CARTESIAN_POINT('Ctrl Pts',(-4.69323559361908,5.21164976205854,
58.5067959517391));
#146630=CARTESIAN_POINT('Ctrl Pts',(-4.82083205444636,5.09384838971931,
58.5146478381539));
#146631=CARTESIAN_POINT('Ctrl Pts',(-4.94382543927954,4.97154066547106,
58.5224997245688));
#146632=CARTESIAN_POINT('Ctrl Pts',(-5.03413795089466,4.88173162588922,
58.5282652670327));
#146633=CARTESIAN_POINT('Ctrl Pts',(-5.12196929038337,4.78949368930705,
58.5340308094967));
#146634=CARTESIAN_POINT('Ctrl Pts',(-5.20718071382556,4.6949862168129,58.5397963519606));
#146635=CARTESIAN_POINT('Ctrl Pts',(-5.34988059565328,4.53671864408659,
58.5494516563206));
#146636=CARTESIAN_POINT('Ctrl Pts',(-5.48515969510916,4.37216652306128,
58.5591069606805));
#146637=CARTESIAN_POINT('Ctrl Pts',(-5.61256373454069,4.20199415613809,
58.5687622650405));
#146638=CARTESIAN_POINT('Ctrl Pts',(-5.7406735684508,4.03087906622498,58.5784710579754));
#146639=CARTESIAN_POINT('Ctrl Pts',(-5.86082086347158,3.8540813582749,58.5881798509102));
#146640=CARTESIAN_POINT('Ctrl Pts',(-5.97259164395314,3.67229841067977,
58.5978886438451));
#146641=CARTESIAN_POINT('Ctrl Pts',(-6.0849002749202,3.48964070810666,58.6076441563158));
#146642=CARTESIAN_POINT('Ctrl Pts',(-6.18875157816082,3.30194972107997,
58.6173996687866));
#146643=CARTESIAN_POINT('Ctrl Pts',(-6.28377368039477,3.10995416301881,
58.6271551812574));
#146644=CARTESIAN_POINT('Ctrl Pts',(-6.37888986912822,2.91776849981838,
58.6369203531863));
#146645=CARTESIAN_POINT('Ctrl Pts',(-6.46515936333439,2.72126977955496,
58.6466855251152));
#146646=CARTESIAN_POINT('Ctrl Pts',(-6.54225724023705,2.5212093854073,58.6564506970442));
#146647=CARTESIAN_POINT('Ctrl Pts',(-6.61924999593386,2.32142176906782,
58.6662025543827));
#146648=CARTESIAN_POINT('Ctrl Pts',(-6.68709611430525,2.11808222018858,
58.6759544117213));
#146649=CARTESIAN_POINT('Ctrl Pts',(-6.74551997479243,1.91195889918595,
58.6857062690598));
#146650=CARTESIAN_POINT('Ctrl Pts',(-6.7709970092206,1.82207420307306,58.6899587851223));
#146651=CARTESIAN_POINT('Ctrl Pts',(-6.79468293256122,1.7316603990258,58.6942113011848));
#146652=CARTESIAN_POINT('Ctrl Pts',(-6.81655777172355,1.64078234609448,
58.6984638172473));
#146653=CARTESIAN_POINT('Ctrl Pts',(-6.85787956284092,1.46911279037727,
58.706496862846));
#146654=CARTESIAN_POINT('Ctrl Pts',(-6.89275525666476,1.2957019724591,58.7145299084448));
#146655=CARTESIAN_POINT('Ctrl Pts',(-6.9210404522921,1.12108234320073,58.7225629540435));
#146656=CARTESIAN_POINT('Ctrl Pts',(-6.94930746510654,0.946574966163909,
58.7305908356913));
#146657=CARTESIAN_POINT('Ctrl Pts',(-6.97099235446236,0.77086068490809,
58.738618717339));
#146658=CARTESIAN_POINT('Ctrl Pts',(-6.98600139184709,0.59448390693991,
58.7466465989868));
#146659=CARTESIAN_POINT('Ctrl Pts',(-7.0010036525035,0.418186764825464,
58.7546708559668));
#146660=CARTESIAN_POINT('Ctrl Pts',(-7.00933603181592,0.241228086079722,
58.7626951129468));
#146661=CARTESIAN_POINT('Ctrl Pts',(-7.01095643732032,0.0641591497509032,
58.7707193699269));
#146662=CARTESIAN_POINT('Ctrl Pts',(-7.01257664690119,-0.112888377140101,
58.7787426566925));
#146663=CARTESIAN_POINT('Ctrl Pts',(-7.00748648807325,-0.290045768790848,
58.7867659434582));
#146664=CARTESIAN_POINT('Ctrl Pts',(-6.9956959518272,-0.466759801277448,
58.7947892302238));
#146665=CARTESIAN_POINT('Ctrl Pts',(-6.98390638171043,-0.643459353625247,
58.8028118595527));
#146666=CARTESIAN_POINT('Ctrl Pts',(-6.96541755622063,-0.819715253609423,
58.8108344888815));
#146667=CARTESIAN_POINT('Ctrl Pts',(-6.94029147899009,-0.994977763147284,
58.8188571182104));
#146668=CARTESIAN_POINT('Ctrl Pts',(-6.91515595614323,-1.17030615891187,
58.8268827634767));
#146669=CARTESIAN_POINT('Ctrl Pts',(-6.88337825213684,-1.3446400555356,
58.8349084087431));
#146670=CARTESIAN_POINT('Ctrl Pts',(-6.84507185867646,-1.51743791044498,
58.8429340540095));
#146671=CARTESIAN_POINT('Ctrl Pts',(-6.82248407481442,-1.6193300554874,
58.8476664635175));
#146672=CARTESIAN_POINT('Ctrl Pts',(-6.79762723465024,-1.72068831271401,
58.8523988730255));
#146673=CARTESIAN_POINT('Ctrl Pts',(-6.77053281198699,-1.82140385535652,
58.8571312825335));
#146674=CARTESIAN_POINT('Ctrl Pts',(-6.72055073993723,-2.00719749899507,
58.8658613313682));
#146675=CARTESIAN_POINT('Ctrl Pts',(-6.66292661929621,-2.19089610356262,
58.874591380203));
#146676=CARTESIAN_POINT('Ctrl Pts',(-6.5978624126179,-2.37188493537608,
58.8833214290377));
#146677=CARTESIAN_POINT('Ctrl Pts',(-6.53277939254295,-2.55292610033632,
58.8920540021769));
#146678=CARTESIAN_POINT('Ctrl Pts',(-6.46025208497314,-2.73125567077547,
58.9007865753162));
#146679=CARTESIAN_POINT('Ctrl Pts',(-6.38053124060429,-2.90627728377262,
58.9095191484554));
#146680=CARTESIAN_POINT('Ctrl Pts',(-6.29967783438381,-3.08378535816713,
58.9183757817358));
#146681=CARTESIAN_POINT('Ctrl Pts',(-6.21142506240127,-3.2578905053806,
58.9272324150162));
#146682=CARTESIAN_POINT('Ctrl Pts',(-6.11608379788457,-3.42799439027456,
58.9360890482966));
#146683=CARTESIAN_POINT('Ctrl Pts',(-6.0220181932462,-3.59582229632339,
58.9448271804034));
#146684=CARTESIAN_POINT('Ctrl Pts',(-5.92105276120039,-3.75975511738309,
58.9535653125102));
#146685=CARTESIAN_POINT('Ctrl Pts',(-5.81353139610945,-3.91924473195406,
58.9623034446171));
#146686=CARTESIAN_POINT('Ctrl Pts',(-5.70382282307937,-4.08197869662147,
58.9712193284842));
#146687=CARTESIAN_POINT('Ctrl Pts',(-5.58728889986215,-4.24008650268444,
58.9801352123514));
#146688=CARTESIAN_POINT('Ctrl Pts',(-5.46434081004124,-4.3930178777485,
58.9890510962186));
#146689=CARTESIAN_POINT('Ctrl Pts',(-5.34139272022036,-4.5459492528125,
58.9979669800857));
#146690=CARTESIAN_POINT('Ctrl Pts',(-5.2120306580182,-4.69370396499874,
59.0068828639529));
#146691=CARTESIAN_POINT('Ctrl Pts',(-5.07670938084766,-4.83576761485841,
59.01579874782));
#146692=CARTESIAN_POINT('Ctrl Pts',(-4.94404720096971,-4.97503967809833,
59.0245394323161));
#146693=CARTESIAN_POINT('Ctrl Pts',(-4.80564374230496,-5.10885705661865,
59.0332801168122));
#146694=CARTESIAN_POINT('Ctrl Pts',(-4.66196191854767,-5.23676786123954,
59.0420208013083));
#146695=CARTESIAN_POINT('Ctrl Pts',(-4.51830594553702,-5.36465565258208,
59.0507599132101));
#146696=CARTESIAN_POINT('Ctrl Pts',(-4.36937370841492,-5.48663881031182,
59.0594990251118));
#146697=CARTESIAN_POINT('Ctrl Pts',(-4.21566296181306,-5.60230420049621,
59.0682381370136));
#146698=CARTESIAN_POINT('Ctrl Pts',(-4.05996067125789,-5.71946820228404,
59.077090476688));
#146699=CARTESIAN_POINT('Ctrl Pts',(-3.89935539732758,-5.83014939441803,
59.0859428163624));
#146700=CARTESIAN_POINT('Ctrl Pts',(-3.7343979268174,-5.93396146656531,
59.0947951560368));
#146701=CARTESIAN_POINT('Ctrl Pts',(-3.57163384853754,-6.0363931793281,
59.1035297886865));
#146702=CARTESIAN_POINT('Ctrl Pts',(-3.40463283991887,-6.13213717322749,
59.1122644213361));
#146703=CARTESIAN_POINT('Ctrl Pts',(-3.23395276927096,-6.22086618153973,
59.1209990539858));
#146704=CARTESIAN_POINT('Ctrl Pts',(-3.05982259761068,-6.31138874454317,
59.1299102471725));
#146705=CARTESIAN_POINT('Ctrl Pts',(-2.8818632914545,-6.39460954862002,
59.1388214403593));
#146706=CARTESIAN_POINT('Ctrl Pts',(-2.70069410209234,-6.47023012955673,
59.1477326335461));
#146707=CARTESIAN_POINT('Ctrl Pts',(-2.51952491273025,-6.5458507104934,
59.1566438267328));
#146708=CARTESIAN_POINT('Ctrl Pts',(-2.33514611471098,-6.61387093909174,
59.1655550199196));
#146709=CARTESIAN_POINT('Ctrl Pts',(-2.14820008150133,-6.67404397440845,
59.1744662131063));
#146710=CARTESIAN_POINT('Ctrl Pts',(-1.97983135953765,-6.72823745944264,
59.1824918779587));
#146711=CARTESIAN_POINT('Ctrl Pts',(-1.80930274092148,-6.7760902631983,
59.1905175428111));
#146712=CARTESIAN_POINT('Ctrl Pts',(-1.63714046594313,-6.81743336287723,
59.1985432076635));
#146713=CARTESIAN_POINT('Ctrl Pts',(-1.46503283104772,-6.85876334127046,
59.2065663253668));
#146714=CARTESIAN_POINT('Ctrl Pts',(-1.2912929280533,-6.89358764334637,
59.21458944307));
#146715=CARTESIAN_POINT('Ctrl Pts',(-1.11646092110653,-6.92178745514061,
59.2226125607733));
#146716=CARTESIAN_POINT('Ctrl Pts',(-0.941650962006826,-6.94998371069164,
59.2306346666911));
#146717=CARTESIAN_POINT('Ctrl Pts',(-0.76574953516945,-6.9715570822227,
59.2386567726089));
#146718=CARTESIAN_POINT('Ctrl Pts',(-0.589305679076254,-6.98644010774504,
59.2466788785268));
#146719=CARTESIAN_POINT('Ctrl Pts',(-0.41279625584923,-7.00132866385001,
59.2547039654863));
#146720=CARTESIAN_POINT('Ctrl Pts',(-0.23574436605913,-7.00952187356466,
59.2627290524459));
#146721=CARTESIAN_POINT('Ctrl Pts',(-0.0587032911843279,-7.01100424233962,
59.2707541394054));
#146722=CARTESIAN_POINT('Ctrl Pts',(0.11837265104363,-7.01248690305969,
59.2787808068656));
#146723=CARTESIAN_POINT('Ctrl Pts',(0.295437407489505,-7.00725609560233,
59.2868074743259));
#146724=CARTESIAN_POINT('Ctrl Pts',(0.47193923904547,-6.99534844858705,
59.2948341417861));
#146725=CARTESIAN_POINT('Ctrl Pts',(0.648582765650722,-6.98343124215465,
59.3028672530267));
#146726=CARTESIAN_POINT('Ctrl Pts',(0.824662099738474,-6.96482652455851,
59.3109003642673));
#146727=CARTESIAN_POINT('Ctrl Pts',(0.999631529102146,-6.93962271081973,
59.3189334755079));
#146728=CARTESIAN_POINT('Ctrl Pts',(1.1027298729944,-6.92477170818637,59.3236668764696));
#146729=CARTESIAN_POINT('Ctrl Pts',(1.20544302502316,-6.90763047736603,
59.3284002774312));
#146730=CARTESIAN_POINT('Ctrl Pts',(1.30766130588673,-6.88822534994222,
59.3331336783929));
#146731=CARTESIAN_POINT('Ctrl Pts',(1.51823414571167,-6.84825018352115,
59.3428846316872));
#146732=CARTESIAN_POINT('Ctrl Pts',(1.72683044093882,-6.79864205883776,
59.3526355849815));
#146733=CARTESIAN_POINT('Ctrl Pts',(1.93266228093756,-6.73961742759492,
59.3623865382758));
#146734=CARTESIAN_POINT('Ctrl Pts',(2.138790660315,-6.68050776029802,59.3721515396476));
#146735=CARTESIAN_POINT('Ctrl Pts',(2.34214658072248,-6.61195446061038,
59.3819165410193));
#146736=CARTESIAN_POINT('Ctrl Pts',(2.54195608502505,-6.5342241945241,59.3916815423911));
#146737=CARTESIAN_POINT('Ctrl Pts',(2.74143254828437,-6.45662348868572,
59.4014302675289));
#146738=CARTESIAN_POINT('Ctrl Pts',(2.93737437407866,-6.36987640088767,
59.4111789926666));
#146739=CARTESIAN_POINT('Ctrl Pts',(3.12902924003106,-6.27429697874835,
59.4209277178044));
#146740=CARTESIAN_POINT('Ctrl Pts',(3.32015808768823,-6.17897988506306,
59.4306496864717));
#146741=CARTESIAN_POINT('Ctrl Pts',(3.50702342874798,-6.0748788687175,59.4403716551389));
#146742=CARTESIAN_POINT('Ctrl Pts',(3.68889739736921,-5.96235377633554,
59.4500936238061));
#146743=CARTESIAN_POINT('Ctrl Pts',(3.86956795344513,-5.85057323309858,
59.459751264746));
#146744=CARTESIAN_POINT('Ctrl Pts',(4.04531291709129,-5.73047972517395,
59.4694089056859));
#146745=CARTESIAN_POINT('Ctrl Pts',(4.21543757068625,-5.6024737973637,59.4790665466259));
#146746=CARTESIAN_POINT('Ctrl Pts',(4.2902132129599,-5.54621078512777,59.4833114123103));
#146747=CARTESIAN_POINT('Ctrl Pts',(4.36390331477806,-5.48841979198442,
59.4875562779948));
#146748=CARTESIAN_POINT('Ctrl Pts',(4.43645009465427,-5.42913778791275,
59.4918011436793));
#146749=CARTESIAN_POINT('Ctrl Pts',(4.57064190642679,-5.31948220367514,
59.4996529906931));
#146750=CARTESIAN_POINT('Ctrl Pts',(4.70086432802666,-5.20476723100868,
59.5075048377069));
#146751=CARTESIAN_POINT('Ctrl Pts',(4.82670255273915,-5.08532880253395,
59.5153566847208));
#146752=CARTESIAN_POINT('Ctrl Pts',(4.95250509074879,-4.96592424583161,
59.5232063050143));
#146753=CARTESIAN_POINT('Ctrl Pts',(5.07392562864606,-4.84179916023225,
59.5310559253078));
#146754=CARTESIAN_POINT('Ctrl Pts',(5.19058382646348,-4.71332855877413,
59.5389055456013));
#146755=CARTESIAN_POINT('Ctrl Pts',(5.30723271061473,-4.58486821405163,
59.5467545392029));
#146756=CARTESIAN_POINT('Ctrl Pts',(5.41911975569858,-4.45206332703062,
59.5546035328045));
#146757=CARTESIAN_POINT('Ctrl Pts',(5.52590294794162,-4.31532422564402,
59.5624525264062));
#146758=CARTESIAN_POINT('Ctrl Pts',(5.63274020138915,-4.17851589725299,
59.5703054937235));
#146759=CARTESIAN_POINT('Ctrl Pts',(5.73446820407984,-4.0377696758671,59.5781584610409));
#146760=CARTESIAN_POINT('Ctrl Pts',(5.83078636956512,-3.89352756186387,
59.5860114283582));
#146761=CARTESIAN_POINT('Ctrl Pts',(5.92712899662768,-3.74924881521091,
59.5938663900654));
#146762=CARTESIAN_POINT('Ctrl Pts',(6.01805884938787,-3.60147273208194,
59.6017213517725));
#146763=CARTESIAN_POINT('Ctrl Pts',(6.10332020436586,-3.45066791295244,
59.6095763134797));
#146764=CARTESIAN_POINT('Ctrl Pts',(6.18866618836593,-3.29971340743369,
59.617439071893));
#146765=CARTESIAN_POINT('Ctrl Pts',(6.26833226190828,-3.14572450028115,
59.6253018303062));
#146766=CARTESIAN_POINT('Ctrl Pts',(6.3421097017522,-2.98919238147038,59.6331645887195));
#146767=CARTESIAN_POINT('Ctrl Pts',(6.39623177298422,-2.87436266520077,
59.6389325954682));
#146768=CARTESIAN_POINT('Ctrl Pts',(6.44718587697957,-2.75816478953243,
59.6447006022169));
#146769=CARTESIAN_POINT('Ctrl Pts',(6.49490656785004,-2.64079821974311,
59.6504686089657));
#146770=CARTESIAN_POINT('Ctrl Pts',(6.57394014154451,-2.44641923499858,
59.6600214083516));
#146771=CARTESIAN_POINT('Ctrl Pts',(6.64423617990191,-2.2485090433388,59.6695742077376));
#146772=CARTESIAN_POINT('Ctrl Pts',(6.70553042679575,-2.04780083450916,
59.6791270071235));
#146773=CARTESIAN_POINT('Ctrl Pts',(6.76670447562403,-1.84748621463226,
59.6886610734625));
#146774=CARTESIAN_POINT('Ctrl Pts',(6.81891197121808,-1.64438463374801,
59.6981951398015));
#146775=CARTESIAN_POINT('Ctrl Pts',(6.86193910720774,-1.43924224905782,
59.7077292061405));
#146776=CARTESIAN_POINT('Ctrl Pts',(6.90486689029431,-1.23457355361042,
59.717241257601));
#146777=CARTESIAN_POINT('Ctrl Pts',(6.93865661190477,-1.0278735591232,59.7267533090615));
#146778=CARTESIAN_POINT('Ctrl Pts',(6.96314526809213,-0.819899102296261,
59.736265360522));
#146779=CARTESIAN_POINT('Ctrl Pts',(6.98751355114625,-0.612946936639984,
59.7457306558262));
#146780=CARTESIAN_POINT('Ctrl Pts',(7.00267193531367,-0.404732904770793,
59.7551959511303));
#146781=CARTESIAN_POINT('Ctrl Pts',(7.00850939139864,-0.196017022671853,
59.7646612464345));
#146782=CARTESIAN_POINT('Ctrl Pts',(7.01033347227623,-0.130797748411864,
59.7676189499124));
#146783=CARTESIAN_POINT('Ctrl Pts',(7.01124779874313,-0.0655295714675496,
59.7705766533904));
#146784=CARTESIAN_POINT('Ctrl Pts',(7.01124999602994,-0.000235945344329035,
59.7735343568684));
#146785=CARTESIAN_POINT('Ctrl Pts',(7.01124999602997,-0.000235944414836881,
59.7735343569105));
#146786=CARTESIAN_POINT('Ctrl Pts',(7.01125624018264,0.185313331802434,
59.7819394612398));
#146787=CARTESIAN_POINT('Ctrl Pts',(7.0038924388928,0.370844036264387,59.790344565569));
#146788=CARTESIAN_POINT('Ctrl Pts',(6.98918905231667,0.555754400321562,
59.7987496698983));
#146789=CARTESIAN_POINT('Ctrl Pts',(6.97447793728878,0.740761957690168,
59.8071591921515));
#146790=CARTESIAN_POINT('Ctrl Pts',(6.95241955274104,0.925148202345302,
59.8155687144047));
#146791=CARTESIAN_POINT('Ctrl Pts',(6.92309629813099,1.10831593388573,59.8239782366579));
#146792=CARTESIAN_POINT('Ctrl Pts',(6.89376518002966,1.29153278473029,59.8323900140566));
#146793=CARTESIAN_POINT('Ctrl Pts',(6.85716536206296,1.47353015410552,59.8408017914553));
#146794=CARTESIAN_POINT('Ctrl Pts',(6.81343045669716,1.65372064577168,59.849213568854));
#146795=CARTESIAN_POINT('Ctrl Pts',(6.76966412479619,1.83404061668966,59.8576313906928));
#146796=CARTESIAN_POINT('Ctrl Pts',(6.71875254183586,2.01255080428954,59.8660492125316));
#146797=CARTESIAN_POINT('Ctrl Pts',(6.66087961695624,2.18867752099686,59.8744670343705));
#146798=CARTESIAN_POINT('Ctrl Pts',(6.63260803866194,2.27471741394277,59.8785792355367));
#146799=CARTESIAN_POINT('Ctrl Pts',(6.60267593100112,2.3601887632264,59.882691436703));
#146800=CARTESIAN_POINT('Ctrl Pts',(6.57110895151811,2.44502632087643,59.8868036378692));
#146801=CARTESIAN_POINT('',(7.01125,-8.5868812060852E-16,59.2264656430896));
#146802=CARTESIAN_POINT('Ctrl Pts',(6.57110895151816,2.4450263208763,59.3399667921338));
#146803=CARTESIAN_POINT('Ctrl Pts',(6.64787822596452,2.23870573356451,59.3299508081697));
#146804=CARTESIAN_POINT('Ctrl Pts',(6.71486704351225,2.02892736619064,59.3199348242056));
#146805=CARTESIAN_POINT('Ctrl Pts',(6.77184227450777,1.81652932034951,59.3099188402415));
#146806=CARTESIAN_POINT('Ctrl Pts',(6.82887754402312,1.60390745682371,59.2998923017813));
#146807=CARTESIAN_POINT('Ctrl Pts',(6.87587814593312,1.38866035124284,59.2898657633211));
#146808=CARTESIAN_POINT('Ctrl Pts',(6.91266147369141,1.17163898562759,59.2798392248609));
#146809=CARTESIAN_POINT('Ctrl Pts',(6.94931701083637,0.95537158369946,59.2698475200489));
#146810=CARTESIAN_POINT('Ctrl Pts',(6.97582616014358,0.737342184747944,
59.259855815237));
#146811=CARTESIAN_POINT('Ctrl Pts',(6.99205864969101,0.518403705408438,
59.249864110425));
#146812=CARTESIAN_POINT('Ctrl Pts',(7.00472967309146,0.347501109915278,
59.2420646213132));
#146813=CARTESIAN_POINT('Ctrl Pts',(7.01113979294834,0.176044788858334,
59.2342651322014));
#146814=CARTESIAN_POINT('Ctrl Pts',(7.01124859079596,0.00444528533067366,
59.2264656430896));
#146815=CARTESIAN_POINT('Ctrl Pts',(7.01125,-8.58630487052188E-16,59.2264656430896));
#146816=CARTESIAN_POINT('Ctrl Pts',(7.01125,-0.191009525814462,59.2177938341508));
#146817=CARTESIAN_POINT('Ctrl Pts',(7.00344006572041,-0.382018909628726,
59.209122025212));
#146818=CARTESIAN_POINT('Ctrl Pts',(6.98784625534317,-0.572390840411034,
59.2004502162733));
#146819=CARTESIAN_POINT('Ctrl Pts',(6.97225246786074,-0.762762491689531,
59.1917784200664));
#146820=CARTESIAN_POINT('Ctrl Pts',(6.94887485033525,-0.952496408757991,
59.1831066238596));
#146821=CARTESIAN_POINT('Ctrl Pts',(6.91779140296513,-1.14095953809139,
59.1744348276527));
#146822=CARTESIAN_POINT('Ctrl Pts',(6.88670800059787,-1.32942239456645,
59.165763044001));
#146823=CARTESIAN_POINT('Ctrl Pts',(6.84791883692705,-1.51661418677696,
59.1570912603492));
#146824=CARTESIAN_POINT('Ctrl Pts',(6.80155333291305,-1.70191034488875,
59.1484194766975));
#146825=CARTESIAN_POINT('Ctrl Pts',(6.75518789508205,-1.88720623850532,
59.139747705424));
#146826=CARTESIAN_POINT('Ctrl Pts',(6.70124620748597,-2.07060622793696,
59.1310759341505));
#146827=CARTESIAN_POINT('Ctrl Pts',(6.63990824732571,-2.25149839653418,
59.122404162877));
#146828=CARTESIAN_POINT('Ctrl Pts',(6.57857037346951,-2.43239031061157,
59.113732403805));
#146829=CARTESIAN_POINT('Ctrl Pts',(6.50983633907179,-2.61077414196406,
59.1050606447329));
#146830=CARTESIAN_POINT('Ctrl Pts',(6.43393547556233,-2.78605471209748,
59.0963888856608));
#146831=CARTESIAN_POINT('Ctrl Pts',(6.35803471730007,-2.96133503917979,
59.0877171386133));
#146832=CARTESIAN_POINT('Ctrl Pts',(6.27496726266193,-3.1335118530473,59.0790453915658));
#146833=CARTESIAN_POINT('Ctrl Pts',(6.18501026583403,-3.30201068654051,
59.0703736445184));
#146834=CARTESIAN_POINT('Ctrl Pts',(6.09151188668825,-3.47714289832064,
59.0613605124454));
#146835=CARTESIAN_POINT('Ctrl Pts',(5.99057066119165,-3.64830137931007,
59.0523473803724));
#146836=CARTESIAN_POINT('Ctrl Pts',(5.88255038916588,-3.81486926138032,
59.0433342482994));
#146837=CARTESIAN_POINT('Ctrl Pts',(5.77621793389049,-3.97883452029324,
59.034461946415));
#146838=CARTESIAN_POINT('Ctrl Pts',(5.66302622906376,-4.13835132493741,
59.0255896445306));
#146839=CARTESIAN_POINT('Ctrl Pts',(5.54337059052903,-4.29286257158994,
59.0167173426463));
#146840=CARTESIAN_POINT('Ctrl Pts',(5.42558457134642,-4.44495958001353,
59.0079836704789));
#146841=CARTESIAN_POINT('Ctrl Pts',(5.30153533574937,-4.59220608124103,
58.9992499983114));
#146842=CARTESIAN_POINT('Ctrl Pts',(5.17164269972312,-4.73410375349976,
58.990516326144));
#146843=CARTESIAN_POINT('Ctrl Pts',(5.04265587431577,-4.87501189762002,
58.98184355853));
#146844=CARTESIAN_POINT('Ctrl Pts',(4.9079071016412,-5.01064538261968,58.973170790916));
#146845=CARTESIAN_POINT('Ctrl Pts',(4.7678460760923,-5.14055156157307,58.964498023302));
#146846=CARTESIAN_POINT('Ctrl Pts',(4.62778576967364,-5.27045707353532,
58.9558253002176));
#146847=CARTESIAN_POINT('Ctrl Pts',(4.48241347329788,-5.39463514506495,
58.9471525771331));
#146848=CARTESIAN_POINT('Ctrl Pts',(4.3322143300549,-5.51267136341058,58.9384798540486));
#146849=CARTESIAN_POINT('Ctrl Pts',(4.18201594573482,-5.63070698534541,
58.9298071747855));
#146850=CARTESIAN_POINT('Ctrl Pts',(4.02699098676462,-5.74260064062568,
58.9211344955223));
#146851=CARTESIAN_POINT('Ctrl Pts',(3.86765680431923,-5.84797891638668,
58.9124618162592));
#146852=CARTESIAN_POINT('Ctrl Pts',(3.70832341394854,-5.9533566682961,58.9037891801093));
#146853=CARTESIAN_POINT('Ctrl Pts',(3.54468107996522,-6.0522189487593,58.8951165439594));
#146854=CARTESIAN_POINT('Ctrl Pts',(3.37727590612859,-6.14423583665075,
58.8864439078095));
#146855=CARTESIAN_POINT('Ctrl Pts',(3.20987155082483,-6.23625227462273,
58.8777713140647));
#146856=CARTESIAN_POINT('Ctrl Pts',(3.0387046414804,-6.32142325013736,58.8690987203199));
#146857=CARTESIAN_POINT('Ctrl Pts',(2.86434638712907,-6.3994645351811,58.8604261265751));
#146858=CARTESIAN_POINT('Ctrl Pts',(2.68998897107704,-6.47750544500914,
58.8517535745274));
#146859=CARTESIAN_POINT('Ctrl Pts',(2.51244050005463,-6.5484166168872,58.8430810224797));
#146860=CARTESIAN_POINT('Ctrl Pts',(2.33229347360944,-6.61196141212718,
58.834408470432));
#146861=CARTESIAN_POINT('Ctrl Pts',(2.15214729859244,-6.67550590703564,
58.8257359593733));
#146862=CARTESIAN_POINT('Ctrl Pts',(1.96940286066631,-6.73168400046421,
58.8170634483147));
#146863=CARTESIAN_POINT('Ctrl Pts',(1.78466999315554,-6.78030822146237,
58.808390937256));
#146864=CARTESIAN_POINT('Ctrl Pts',(1.59993798367062,-6.82893221661638,
58.7997184664784));
#146865=CARTESIAN_POINT('Ctrl Pts',(1.41321783783503,-6.8700023372309,58.7910459957009));
#146866=CARTESIAN_POINT('Ctrl Pts',(1.22513265045738,-6.90338153018383,
58.7823735249233));
#146867=CARTESIAN_POINT('Ctrl Pts',(1.03704832132596,-6.93676057082511,
58.7737010937188));
#146868=CARTESIAN_POINT('Ctrl Pts',(0.847599242850215,-6.96244870438833,
58.7650286625143));
#146869=CARTESIAN_POINT('Ctrl Pts',(0.657417610664734,-6.9803602090213,
58.7563562313098));
#146870=CARTESIAN_POINT('Ctrl Pts',(0.467236830771745,-6.99827163338448,
58.7476838389706));
#146871=CARTESIAN_POINT('Ctrl Pts',(0.276323786584655,-7.00840647191863,
58.7390114466313));
#146872=CARTESIAN_POINT('Ctrl Pts',(0.0853155533185971,-7.01073090475322,
58.730339054292));
#146873=CARTESIAN_POINT('Ctrl Pts',(-0.105691839537741,-7.01305532736064,
58.7216667001101));
#146874=CARTESIAN_POINT('Ctrl Pts',(-0.296794136564428,-7.00756940957899,
58.7129943459281));
#146875=CARTESIAN_POINT('Ctrl Pts',(-0.487353636617199,-6.99429145770864,
58.7043219917462));
#146876=CARTESIAN_POINT('Ctrl Pts',(-0.677912313784896,-6.9810135631759,
58.6956496750137));
#146877=CARTESIAN_POINT('Ctrl Pts',(-0.867927915270903,-6.95994372163458,
58.6869773582812));
#146878=CARTESIAN_POINT('Ctrl Pts',(-1.05676637166362,-6.93115224174314,
58.6783050415487));
#146879=CARTESIAN_POINT('Ctrl Pts',(-1.24560402801224,-6.90236088383137,
58.6696327615579));
#146880=CARTESIAN_POINT('Ctrl Pts',(-1.43326426841345,-6.86584799585127,
58.660960481567));
#146881=CARTESIAN_POINT('Ctrl Pts',(-1.61912088843955,-6.82173541784777,
58.6522882015762));
#146882=CARTESIAN_POINT('Ctrl Pts',(-1.80497673622004,-6.77762302313473,
58.6436159576192));
#146883=CARTESIAN_POINT('Ctrl Pts',(-1.98902870222715,-6.7259110671892,
58.6349437136622));
#146884=CARTESIAN_POINT('Ctrl Pts',(-2.17066262760132,-6.66677210647214,
58.6262714697052));
#146885=CARTESIAN_POINT('Ctrl Pts',(-2.35229581309554,-6.60763338665573,
58.6175992610743));
#146886=CARTESIAN_POINT('Ctrl Pts',(-2.53151070755663,-6.54106781055513,
58.6089270524435));
#146887=CARTESIAN_POINT('Ctrl Pts',(-2.70770929770725,-6.46729749753402,
58.6002548438126));
#146888=CARTESIAN_POINT('Ctrl Pts',(-2.88390718449518,-6.39352747899475,
58.5915826698001));
#146889=CARTESIAN_POINT('Ctrl Pts',(-3.05708852904383,-6.31255289079089,
58.5829104957876));
#146890=CARTESIAN_POINT('Ctrl Pts',(-3.22667545573784,-6.22464393084769,
58.574238321775));
#146891=CARTESIAN_POINT('Ctrl Pts',(-3.39626171929845,-6.13673531465368,
58.5655661816732));
#146892=CARTESIAN_POINT('Ctrl Pts',(-3.56225334094293,-6.04189251170778,
58.5568940415714));
#146893=CARTESIAN_POINT('Ctrl Pts',(-3.72409644022107,-5.94043199325039,
58.5482219014696));
#146894=CARTESIAN_POINT('Ctrl Pts',(-3.88593891985092,-5.83897186325464,
58.5395497945707));
#146895=CARTESIAN_POINT('Ctrl Pts',(-4.04363266823074,-5.7308942193264,
58.5308776876719));
#146896=CARTESIAN_POINT('Ctrl Pts',(-4.19665149725939,-5.61655969193336,
58.5222055807731));
#146897=CARTESIAN_POINT('Ctrl Pts',(-4.34966975290894,-5.50222559296491,
58.5135335063696));
#146898=CARTESIAN_POINT('Ctrl Pts',(-4.49801289671901,-5.38163482746632,
58.5048614319662));
#146899=CARTESIAN_POINT('Ctrl Pts',(-4.64118594513082,-5.2551897763278,
58.4961893575627));
#146900=CARTESIAN_POINT('Ctrl Pts',(-4.78435846873758,-5.12874518867735,
58.487517314947));
#146901=CARTESIAN_POINT('Ctrl Pts',(-4.92236072197075,-4.99644654635288,
58.4788452723313));
#146902=CARTESIAN_POINT('Ctrl Pts',(-5.05473222958088,-4.85873529323592,
58.4701732297156));
#146903=CARTESIAN_POINT('Ctrl Pts',(-5.18710326277798,-4.72102453366937,
58.4615012181801));
#146904=CARTESIAN_POINT('Ctrl Pts',(-5.31384339390117,-4.57790140690284,
58.4528292066446));
#146905=CARTESIAN_POINT('Ctrl Pts',(-5.43452972930759,-4.429843471701,58.4441571951091));
#146906=CARTESIAN_POINT('Ctrl Pts',(-5.55521564202563,-4.28178605505306,
58.4354852139461));
#146907=CARTESIAN_POINT('Ctrl Pts',(-5.66984762199996,-4.1287940847122,
58.4268132327832));
#146908=CARTESIAN_POINT('Ctrl Pts',(-5.77804317951767,-3.97137804522931,
58.4181412516203));
#146909=CARTESIAN_POINT('Ctrl Pts',(-5.88623836692049,-3.81396254423451,
58.4094693001225));
#146910=CARTESIAN_POINT('Ctrl Pts',(-5.98799701504623,-3.65212323845021,
58.4007973486246));
#146911=CARTESIAN_POINT('Ctrl Pts',(-6.08297959063289,-3.48640012942344,
58.3921253971268));
#146912=CARTESIAN_POINT('Ctrl Pts',(-6.17796184905169,-3.32067757378284,
58.3834534745865));
#146913=CARTESIAN_POINT('Ctrl Pts',(-6.26616793897866,-3.15107148726879,
58.3747815520462));
#146914=CARTESIAN_POINT('Ctrl Pts',(-6.3473035492945,-2.97814778270211,
58.3661096295059));
#146915=CARTESIAN_POINT('Ctrl Pts',(-6.42843889529885,-2.80522464146048,
58.3574377352158));
#146916=CARTESIAN_POINT('Ctrl Pts',(-6.50250368714336,-2.62898416091372,
58.3487658409256));
#146917=CARTESIAN_POINT('Ctrl Pts',(-6.56925079960199,-2.45001438657584,
58.3400939466354));
#146918=CARTESIAN_POINT('Ctrl Pts',(-6.63599770006635,-2.2710451806606,
58.3314220798879));
#146919=CARTESIAN_POINT('Ctrl Pts',(-6.69542686840867,-2.08934696440751,
58.3227502131403));
#146920=CARTESIAN_POINT('Ctrl Pts',(-6.7473400140094,-1.90552598981166,
58.3140783463928));
#146921=CARTESIAN_POINT('Ctrl Pts',(-6.79925299896442,-1.7217055840515,
58.3054065064804));
#146922=CARTESIAN_POINT('Ctrl Pts',(-6.84364993053273,-1.53576270641015,
58.2967346665681));
#146923=CARTESIAN_POINT('Ctrl Pts',(-6.88038267538378,-1.34831776773087,
58.2880628266557));
#146924=CARTESIAN_POINT('Ctrl Pts',(-6.91711530956105,-1.1608733938131,
58.2793910128711));
#146925=CARTESIAN_POINT('Ctrl Pts',(-6.94618374861435,-0.971927246615138,
58.2707191990866));
#146926=CARTESIAN_POINT('Ctrl Pts',(-6.96749100433714,-0.782109753794825,
58.262047385302));
#146927=CARTESIAN_POINT('Ctrl Pts',(-6.9887981976002,-0.592292817402312,
58.2533755969378));
#146928=CARTESIAN_POINT('Ctrl Pts',(-7.00234422137977,-0.401604822724534,
58.2447038085736));
#146929=CARTESIAN_POINT('Ctrl Pts',(-7.00808387899861,-0.210682005448528,
58.2360320202095));
#146930=CARTESIAN_POINT('Ctrl Pts',(-7.01382352026048,-0.0197597322676766,
58.2273602565583));
#146931=CARTESIAN_POINT('Ctrl Pts',(-7.01175683134594,0.171397078306313,
58.2186884929072));
#146932=CARTESIAN_POINT('Ctrl Pts',(-7.00189070777957,0.362150630000985,
58.210016729256));
#146933=CARTESIAN_POINT('Ctrl Pts',(-6.9915780829724,0.561536923516253,
58.2009525163107));
#146934=CARTESIAN_POINT('Ctrl Pts',(-6.97274368607516,0.760482277946813,
58.1918883033653));
#146935=CARTESIAN_POINT('Ctrl Pts',(-6.94545616842791,0.958261537862561,
58.1828240904199));
#146936=CARTESIAN_POINT('Ctrl Pts',(-6.91902138570714,1.14986019590593,
58.1740431341291));
#146937=CARTESIAN_POINT('Ctrl Pts',(-6.88465388689258,1.34036422799789,
58.1652621778383));
#146938=CARTESIAN_POINT('Ctrl Pts',(-6.84247124235198,1.52912192453256,
58.1564812215475));
#146939=CARTESIAN_POINT('Ctrl Pts',(-6.80080846652261,1.71555332736278,
58.147808483802));
#146940=CARTESIAN_POINT('Ctrl Pts',(-6.75152215882473,1.90028091508853,
58.1391357460565));
#146941=CARTESIAN_POINT('Ctrl Pts',(-6.69477680033874,2.08268820425579,
58.130463008311));
#146942=CARTESIAN_POINT('Ctrl Pts',(-6.63803201373068,2.26509365512815,
58.1217903579691));
#146943=CARTESIAN_POINT('Ctrl Pts',(-6.57382841116582,2.44517858291869,
58.1131177076272));
#146944=CARTESIAN_POINT('Ctrl Pts',(-6.50238025225844,2.62234201002453,
58.1044450572853));
#146945=CARTESIAN_POINT('Ctrl Pts',(-6.43093279007603,2.79950370952556,
58.0957724915145));
#146946=CARTESIAN_POINT('Ctrl Pts',(-6.35224101918865,2.97374370184446,
58.0870999257437));
#146947=CARTESIAN_POINT('Ctrl Pts',(-6.26656754386312,3.14448052636702,
58.078427359973));
#146948=CARTESIAN_POINT('Ctrl Pts',(-6.18089487601068,3.31521574169382,
58.0697548759412));
#146949=CARTESIAN_POINT('Ctrl Pts',(-6.08824076282076,3.48244760135704,
58.0610823919094));
#146950=CARTESIAN_POINT('Ctrl Pts',(-5.98891439681757,3.64561804226544,
58.0524099078776));
#146951=CARTESIAN_POINT('Ctrl Pts',(-5.88958893454135,3.80878699855768,
58.0437375027529));
#146952=CARTESIAN_POINT('Ctrl Pts',(-5.78359148865815,3.96789436736601,
58.0350650976283));
#146953=CARTESIAN_POINT('Ctrl Pts',(-5.67127577279106,4.12240920718131,
58.0263926925036));
#146954=CARTESIAN_POINT('Ctrl Pts',(-5.55896104217282,4.27692269157125,
58.0177203634545));
#146955=CARTESIAN_POINT('Ctrl Pts',(-5.44032831951742,4.42684349779038,
58.0090480344054));
#146956=CARTESIAN_POINT('Ctrl Pts',(-5.31577347544553,4.57167134866995,
58.0003757053562));
#146957=CARTESIAN_POINT('Ctrl Pts',(-5.19121968333082,4.71649797637192,
57.9917034495513));
#146958=CARTESIAN_POINT('Ctrl Pts',(-5.06074405512004,4.8562315194283,57.9830311937463));
#146959=CARTESIAN_POINT('Ctrl Pts',(-4.92478197318643,4.99040570285402,
57.9743589379414));
#146960=CARTESIAN_POINT('Ctrl Pts',(-4.78882099517689,5.12457879687227,
57.9656867525496));
#146961=CARTESIAN_POINT('Ctrl Pts',(-4.64737385477618,5.25319242205562,
57.9570145671577));
#146962=CARTESIAN_POINT('Ctrl Pts',(-4.50091253739251,5.37581741628591,
57.9483423817659));
#146963=CARTESIAN_POINT('Ctrl Pts',(-4.3544523613803,5.49844145490095,57.9396702639563));
#146964=CARTESIAN_POINT('Ctrl Pts',(-4.20297830437536,5.61507677360282,
57.9309981461467));
#146965=CARTESIAN_POINT('Ctrl Pts',(-4.04699580205666,5.72533418593498,
57.9223260283371));
#146966=CARTESIAN_POINT('Ctrl Pts',(-3.89101446440432,5.83559077501392,
57.9136539752791));
#146967=CARTESIAN_POINT('Ctrl Pts',(-3.73052498074915,5.93946938906479,
57.9049819222212));
#146968=CARTESIAN_POINT('Ctrl Pts',(-3.56606286128093,6.03662341312533,
57.8963098691632));
#146969=CARTESIAN_POINT('Ctrl Pts',(-3.40160191612509,6.13377674347491,
57.8876378780265));
#146970=CARTESIAN_POINT('Ctrl Pts',(-3.2331686364694,6.2242054354536,57.8789658868898));
#146971=CARTESIAN_POINT('Ctrl Pts',(-3.06132503079386,6.30760775717189,
57.8702938957531));
#146972=CARTESIAN_POINT('Ctrl Pts',(-2.8894825960632,6.39100951058552,57.8616219637075));
#146973=CARTESIAN_POINT('Ctrl Pts',(-2.7142301373335,6.46738486553392,57.8529500316619));
#146974=CARTESIAN_POINT('Ctrl Pts',(-2.5361524085633,6.53647898512942,57.8442780996162));
#146975=CARTESIAN_POINT('Ctrl Pts',(-2.35807583511184,6.60557265646151,
57.8356062238317));
#146976=CARTESIAN_POINT('Ctrl Pts',(-2.17717429308117,6.66738508423481,
57.8269343480472));
#146977=CARTESIAN_POINT('Ctrl Pts',(-1.99405137754989,6.72171002544675,
57.8182624722626));
#146978=CARTESIAN_POINT('Ctrl Pts',(-1.81092959032083,6.77603463193842,
57.8095906499094));
#146979=CARTESIAN_POINT('Ctrl Pts',(-1.62558672925683,6.82287176341404,
57.8009188275561));
#146980=CARTESIAN_POINT('Ctrl Pts',(-1.43864120070387,6.86206514528515,
57.7922470052029));
#146981=CARTESIAN_POINT('Ctrl Pts',(-1.25169676301303,6.90125829845556,
57.7835752334514));
#146982=CARTESIAN_POINT('Ctrl Pts',(-1.06314995450122,6.93280773300277,
57.7749034616998));
#146983=CARTESIAN_POINT('Ctrl Pts',(-0.873629864321623,6.95660818378219,
57.7662316899483));
#146984=CARTESIAN_POINT('Ctrl Pts',(-0.679495509708901,6.98098810649739,
57.7573487857098));
#146985=CARTESIAN_POINT('Ctrl Pts',(-0.48434018208405,6.99723686027501,
57.7484658814713));
#146986=CARTESIAN_POINT('Ctrl Pts',(-0.288847078968885,7.00529756166511,
57.7395829772329));
#146987=CARTESIAN_POINT('Ctrl Pts',(-0.0979805523943737,7.0131674969803,
57.7309102974765));
#146988=CARTESIAN_POINT('Ctrl Pts',(0.0932076478891657,7.01323255451603,
57.7222376177202));
#146989=CARTESIAN_POINT('Ctrl Pts',(0.284079486226396,7.00549251716147,
57.7135649379638));
#146990=CARTESIAN_POINT('Ctrl Pts',(0.474947621918049,6.99775262995276,
57.7048924264453));
#146991=CARTESIAN_POINT('Ctrl Pts',(0.665499124053657,6.98220796234689,
57.6962199149268));
#146992=CARTESIAN_POINT('Ctrl Pts',(0.855098106421533,6.95891038819256,
57.6875474034082));
#146993=CARTESIAN_POINT('Ctrl Pts',(1.04469365841792,6.93561323555597,57.6788750487995));
#146994=CARTESIAN_POINT('Ctrl Pts',(1.23333644315622,6.90456349171623,57.6702026941907));
#146995=CARTESIAN_POINT('Ctrl Pts',(1.42039696672986,6.86586476850547,57.661530339582));
#146996=CARTESIAN_POINT('Ctrl Pts',(1.60745435009459,6.82716669493512,57.6528581305571));
#146997=CARTESIAN_POINT('Ctrl Pts',(1.79292924726445,6.78081995649295,57.6441859215323));
#146998=CARTESIAN_POINT('Ctrl Pts',(1.97620275621391,6.72697920532185,57.6355137125075));
#146999=CARTESIAN_POINT('Ctrl Pts',(2.15947342778787,6.67313928769417,57.6268416377427));
#147000=CARTESIAN_POINT('Ctrl Pts',(2.3405425068073,6.61180566956694,57.618169562978));
#147001=CARTESIAN_POINT('Ctrl Pts',(2.51880581149286,6.54318300573122,57.6094974882132));
#147002=CARTESIAN_POINT('Ctrl Pts',(2.69706658906144,6.47456131471208,57.6008255363865));
#147003=CARTESIAN_POINT('Ctrl Pts',(2.87252140682272,6.39865088679973,57.5921535845598));
#147004=CARTESIAN_POINT('Ctrl Pts',(3.04458483295129,6.31570500874312,57.5834816327332));
#147005=CARTESIAN_POINT('Ctrl Pts',(3.21664604443053,6.23276019829303,57.5748097925242));
#147006=CARTESIAN_POINT('Ctrl Pts',(3.38531569579111,6.14278024223614,57.5661379523153));
#147007=CARTESIAN_POINT('Ctrl Pts',(3.55003100942567,6.04606536473236,57.5574661121063));
#147008=CARTESIAN_POINT('Ctrl Pts',(3.72225670716351,5.9449406611928,57.5483988693728));
#147009=CARTESIAN_POINT('Ctrl Pts',(3.89015872998899,5.8364526481946,57.5393316266393));
#147010=CARTESIAN_POINT('Ctrl Pts',(4.05312466660087,5.72099702844632,57.5302643839057));
#147011=CARTESIAN_POINT('Ctrl Pts',(4.20899688868252,5.61056705531127,57.5215918275273));
#147012=CARTESIAN_POINT('Ctrl Pts',(4.36035338104125,5.49376336253442,57.5129192711489));
#147013=CARTESIAN_POINT('Ctrl Pts',(4.50668904925292,5.37097573778208,57.5042467147704));
#147014=CARTESIAN_POINT('Ctrl Pts',(4.65301950884331,5.2481924834901,57.49557446708));
#147015=CARTESIAN_POINT('Ctrl Pts',(4.7943292842724,5.11942590603737,57.4869022193895));
#147016=CARTESIAN_POINT('Ctrl Pts',(4.930146841728,4.98510568408529,57.4782299716991));
#147017=CARTESIAN_POINT('Ctrl Pts',(5.06596027420137,4.85078954163911,57.4695579873978));
#147018=CARTESIAN_POINT('Ctrl Pts',(5.19628162053707,4.71092029195257,57.4608860030965));
#147019=CARTESIAN_POINT('Ctrl Pts',(5.32067604038424,4.56596463365422,57.4522140187951));
#147020=CARTESIAN_POINT('Ctrl Pts',(5.44506733164634,4.4210126210669,57.4435422525988));
#147021=CARTESIAN_POINT('Ctrl Pts',(5.56353180975929,4.27097467138257,57.4348704864024));
#147022=CARTESIAN_POINT('Ctrl Pts',(5.67567421678466,4.11635138774934,57.4261987202061));
#147023=CARTESIAN_POINT('Ctrl Pts',(5.78782406006403,3.9617178509207,57.4175263789778));
#147024=CARTESIAN_POINT('Ctrl Pts',(5.89365082654566,3.80249860161938,57.4088540377496));
#147025=CARTESIAN_POINT('Ctrl Pts',(5.99280137736245,3.63922494687849,57.4001816965214));
#147026=CARTESIAN_POINT('Ctrl Pts',(6.09194609291145,3.47596090121682,57.391509865683));
#147027=CARTESIAN_POINT('Ctrl Pts',(6.18441523160766,3.30864317036249,57.3828380348447));
#147028=CARTESIAN_POINT('Ctrl Pts',(6.26990026463242,3.13783001994409,57.3741662040063));
#147029=CARTESIAN_POINT('Ctrl Pts',(6.35538670852655,2.96701405037675,57.3654942300455));
#147030=CARTESIAN_POINT('Ctrl Pts',(6.43388868897279,2.79270279979035,57.3568222560848));
#147031=CARTESIAN_POINT('Ctrl Pts',(6.50514427077518,2.6154778872896,57.3481502821241));
#147032=CARTESIAN_POINT('Ctrl Pts',(6.52787183386361,2.55895052090203,57.3453842835832));
#147033=CARTESIAN_POINT('Ctrl Pts',(6.5498625512979,2.50212689663814,57.3426182850423));
#147034=CARTESIAN_POINT('Ctrl Pts',(6.57110895151816,2.4450263208763,57.3398522865015));
#147035=CARTESIAN_POINT('Origin',(0.,0.,50.));
#147036=CARTESIAN_POINT('',(6.57110895151813,2.44502632087638,55.3399173263397));
#147037=CARTESIAN_POINT('',(6.57110895151812,2.44502632087641,55.886985753209));
#147038=CARTESIAN_POINT('',(6.57110895151814,2.44502632087636,50.));
#147039=CARTESIAN_POINT('',(7.01124831048998,-0.00486735569172974,57.7735343569399));
#147040=CARTESIAN_POINT('Ctrl Pts',(6.57110895151812,2.44502632087642,55.886985753209));
#147041=CARTESIAN_POINT('Ctrl Pts',(6.50692229192473,2.61753061247478,55.8953627491612));
#147042=CARTESIAN_POINT('Ctrl Pts',(6.43589784857362,2.78761567826404,55.9037397451133));
#147043=CARTESIAN_POINT('Ctrl Pts',(6.35824132120199,2.954723991147,55.9121167410655));
#147044=CARTESIAN_POINT('Ctrl Pts',(6.28063626007775,3.1217215543214,55.92048818523));
#147045=CARTESIAN_POINT('Ctrl Pts',(6.19640801680893,3.28574600083383,55.9288596293946));
#147046=CARTESIAN_POINT('Ctrl Pts',(6.10581046081725,3.44625959252559,55.9372310735591));
#147047=CARTESIAN_POINT('Ctrl Pts',(6.01525966353638,3.6066903408279,55.9455981971001));
#147048=CARTESIAN_POINT('Ctrl Pts',(5.91834626998841,3.76361356190755,55.9539653206411));
#147049=CARTESIAN_POINT('Ctrl Pts',(5.8153703705518,3.91651554520192,55.962332444182));
#147050=CARTESIAN_POINT('Ctrl Pts',(5.7124277728145,4.06936808104401,55.9706968618527));
#147051=CARTESIAN_POINT('Ctrl Pts',(5.60342676106945,4.21820169925229,55.9790612795233));
#147052=CARTESIAN_POINT('Ctrl Pts',(5.48871137006098,4.36253069429469,55.9874256971939));
#147053=CARTESIAN_POINT('Ctrl Pts',(5.37401714775546,4.50683305596561,55.9957885713587));
#147054=CARTESIAN_POINT('Ctrl Pts',(5.25361085293471,4.64663219454363,56.0041514455235));
#147055=CARTESIAN_POINT('Ctrl Pts',(5.12787778651435,4.78147424640902,56.0125143196883));
#147056=CARTESIAN_POINT('Ctrl Pts',(5.00215116167431,4.91630939002082,56.0208767654048));
#147057=CARTESIAN_POINT('Ctrl Pts',(4.87109853372871,5.04618771315425,56.0292392111212));
#147058=CARTESIAN_POINT('Ctrl Pts',(4.73514344505988,5.17069077756604,56.0376016568377));
#147059=CARTESIAN_POINT('Ctrl Pts',(4.59917720012601,5.2952040585074,56.0459647887636));
#147060=CARTESIAN_POINT('Ctrl Pts',(4.45830793515744,5.41434097976978,56.0543279206894));
#147061=CARTESIAN_POINT('Ctrl Pts',(4.3129940934042,5.52772181940811,56.0626910526153));
#147062=CARTESIAN_POINT('Ctrl Pts',(4.16759669615451,5.64116785305844,56.0710589933442));
#147063=CARTESIAN_POINT('Ctrl Pts',(4.01774987339592,5.74885098721903,56.079426934073));
#147064=CARTESIAN_POINT('Ctrl Pts',(3.86394387481114,5.85043282969812,56.0877948748019));
#147065=CARTESIAN_POINT('Ctrl Pts',(3.71009612548348,5.9520422466374,56.096165087014));
#147066=CARTESIAN_POINT('Ctrl Pts',(3.55228733458885,6.04754689257731,56.1045352992261));
#147067=CARTESIAN_POINT('Ctrl Pts',(3.39103505703203,6.13665281765881,56.1129055114382));
#147068=CARTESIAN_POINT('Ctrl Pts',(3.22963973294287,6.22583778840581,56.1212831488466));
#147069=CARTESIAN_POINT('Ctrl Pts',(3.06479510755026,6.30861253885692,56.1296607862551));
#147070=CARTESIAN_POINT('Ctrl Pts',(2.89704270074082,6.38472945022609,56.1380384236636));
#147071=CARTESIAN_POINT('Ctrl Pts',(2.75189695517394,6.4505886892144,56.1452870733305));
#147072=CARTESIAN_POINT('Ctrl Pts',(2.60457481242047,6.51146432822324,56.1525357229974));
#147073=CARTESIAN_POINT('Ctrl Pts',(2.45543802521295,6.56722549230939,56.1597843726644));
#147074=CARTESIAN_POINT('Ctrl Pts',(2.29366480687932,6.62771132642955,56.1676472038755));
#147075=CARTESIAN_POINT('Ctrl Pts',(2.12941952631151,6.68230366807814,56.1755100350867));
#147076=CARTESIAN_POINT('Ctrl Pts',(1.96318930483182,6.7307885359662,56.1833728662979));
#147077=CARTESIAN_POINT('Ctrl Pts',(1.79708680933532,6.77923614963317,56.1912296559611));
#147078=CARTESIAN_POINT('Ctrl Pts',(1.62900276959128,6.82158551575422,56.1990864456244));
#147079=CARTESIAN_POINT('Ctrl Pts',(1.45944377323308,6.85767091914385,56.2069432352877));
#147080=CARTESIAN_POINT('Ctrl Pts',(1.28998040012236,6.89373597207415,56.2147955940935));
#147081=CARTESIAN_POINT('Ctrl Pts',(1.11904409680735,6.92354401026403,56.2226479528993));
#147082=CARTESIAN_POINT('Ctrl Pts',(0.947155836532505,6.94697937119598,
56.2305003117051));
#147083=CARTESIAN_POINT('Ctrl Pts',(0.775308161083144,6.97040919876553,
56.2383508164773));
#147084=CARTESIAN_POINT('Ctrl Pts',(0.602509352318679,6.9874692839556,56.2462013212495));
#147085=CARTESIAN_POINT('Ctrl Pts',(0.429289721358449,6.99809523353577,
56.2540518260217));
#147086=CARTESIAN_POINT('Ctrl Pts',(0.256097955977921,7.00871947373551,
56.2619010678951));
#147087=CARTESIAN_POINT('Ctrl Pts',(0.0824858841641347,7.01291161844657,
56.2697503097685));
#147088=CARTESIAN_POINT('Ctrl Pts',(-0.0910123971688293,7.01065926329768,
56.2775995516419));
#147089=CARTESIAN_POINT('Ctrl Pts',(-0.264569133466189,7.00840614928629,
56.2854514380784));
#147090=CARTESIAN_POINT('Ctrl Pts',(-0.438011620873844,6.99970420337629,
56.2933033245149));
#147091=CARTESIAN_POINT('Ctrl Pts',(-0.610806899742382,6.98459315162502,
56.3011552109514));
#147092=CARTESIAN_POINT('Ctrl Pts',(-0.737688319046612,6.97349729468995,
56.3069207532845));
#147093=CARTESIAN_POINT('Ctrl Pts',(-0.864220788215814,6.95894687722375,
56.3126862956176));
#147094=CARTESIAN_POINT('Ctrl Pts',(-0.990195679420402,6.94097536942447,
56.3184518379507));
#147095=CARTESIAN_POINT('Ctrl Pts',(-1.20116038014341,6.91087926274668,
56.328107142283));
#147096=CARTESIAN_POINT('Ctrl Pts',(-1.41045364027579,6.87120349826754,
56.3377624466153));
#147097=CARTESIAN_POINT('Ctrl Pts',(-1.61730105857216,6.822167093266,56.3474177509476));
#147098=CARTESIAN_POINT('Ctrl Pts',(-1.8252943727057,6.77285903579315,56.357126543852));
#147099=CARTESIAN_POINT('Ctrl Pts',(-2.03081463764949,6.714086402269,56.3668353367563));
#147100=CARTESIAN_POINT('Ctrl Pts',(-2.23309720570835,6.64611942657951,
56.3765441296607));
#147101=CARTESIAN_POINT('Ctrl Pts',(-2.43635317461807,6.5778253880462,56.3862996420989));
#147102=CARTESIAN_POINT('Ctrl Pts',(-2.63634017815743,6.50024834306042,
56.396055154537));
#147103=CARTESIAN_POINT('Ctrl Pts',(-2.83230581991641,6.41370955882535,
56.4058106669752));
#147104=CARTESIAN_POINT('Ctrl Pts',(-3.02846549780603,6.32708508788166,
56.4155758388714));
#147105=CARTESIAN_POINT('Ctrl Pts',(-3.22059581891455,6.23148115437375,
56.4253410107675));
#147106=CARTESIAN_POINT('Ctrl Pts',(-3.40796591218387,6.12726651157698,
56.4351061826637));
#147107=CARTESIAN_POINT('Ctrl Pts',(-3.59508053060769,6.023193963067,56.4448580399709));
#147108=CARTESIAN_POINT('Ctrl Pts',(-3.77744786015144,5.91053418880033,
56.454609897278));
#147109=CARTESIAN_POINT('Ctrl Pts',(-3.95436413596618,5.78970041044305,
56.4643617545852));
#147110=CARTESIAN_POINT('Ctrl Pts',(-4.03151244816047,5.73700812979566,
56.4686142708025));
#147111=CARTESIAN_POINT('Ctrl Pts',(-4.10762450529992,5.68276207628728,
56.4728667870198));
#147112=CARTESIAN_POINT('Ctrl Pts',(-4.18264341832615,5.62699925338834,
56.4771193032371));
#147113=CARTESIAN_POINT('Ctrl Pts',(-4.3243548941933,5.52166272406854,56.4851523488385));
#147114=CARTESIAN_POINT('Ctrl Pts',(-4.4622325460807,5.41085938963786,56.4931853944399));
#147115=CARTESIAN_POINT('Ctrl Pts',(-4.59582437413559,5.29490555955451,
56.5012184400412));
#147116=CARTESIAN_POINT('Ctrl Pts',(-4.72933032421962,5.17902626905778,
56.5092463216916));
#147117=CARTESIAN_POINT('Ctrl Pts',(-4.85855565887089,5.05800331269003,
56.5172742033419));
#147118=CARTESIAN_POINT('Ctrl Pts',(-4.98307962490636,4.93219464481513,
56.5253020849923));
#147119=CARTESIAN_POINT('Ctrl Pts',(-5.10754736714371,4.80644278079391,
56.5333263419749));
#147120=CARTESIAN_POINT('Ctrl Pts',(-5.22731770999815,4.67590976764803,
56.5413505989576));
#147121=CARTESIAN_POINT('Ctrl Pts',(-5.34200514475477,4.54099191762258,
56.5493748559402));
#147122=CARTESIAN_POINT('Ctrl Pts',(-5.45667871263212,4.40609038053971,
56.5573981427085));
#147123=CARTESIAN_POINT('Ctrl Pts',(-5.56627035338833,4.26680533672825,
56.5654214294767));
#147124=CARTESIAN_POINT('Ctrl Pts',(-5.67043330268262,4.12356796019272,
56.573444716245));
#147125=CARTESIAN_POINT('Ctrl Pts',(-5.77458771675235,3.9803423206825,56.5814673455764));
#147126=CARTESIAN_POINT('Ctrl Pts',(-5.87331411303707,3.83316529243472,
56.5894899749079));
#147127=CARTESIAN_POINT('Ctrl Pts',(-5.96630789651182,3.68249869606504,
56.5975126042393));
#147128=CARTESIAN_POINT('Ctrl Pts',(-6.05933663902847,3.53177545978182,
56.6055382495082));
#147129=CARTESIAN_POINT('Ctrl Pts',(-6.14662827354817,3.37756034850298,
56.6135638947772));
#147130=CARTESIAN_POINT('Ctrl Pts',(-6.22792298894739,3.2203418772299,56.6215895400461));
#147131=CARTESIAN_POINT('Ctrl Pts',(-6.2758593068327,3.12763628647436,56.6263219495386));
#147132=CARTESIAN_POINT('Ctrl Pts',(-6.32171136420164,3.0338868994117,56.631054359031));
#147133=CARTESIAN_POINT('Ctrl Pts',(-6.36543360472109,2.93919743916387,
56.6357867685235));
#147134=CARTESIAN_POINT('Ctrl Pts',(-6.44608962056194,2.76452032941438,
56.6445168173604));
#147135=CARTESIAN_POINT('Ctrl Pts',(-6.51953573015837,2.58655576663999,
56.6532468661973));
#147136=CARTESIAN_POINT('Ctrl Pts',(-6.58553315998018,2.40590514387029,
56.6619769150341));
#147137=CARTESIAN_POINT('Ctrl Pts',(-6.65154967304157,2.22520228574651,
56.6707094881756));
#147138=CARTESIAN_POINT('Ctrl Pts',(-6.71011311323383,2.04181207464561,
56.679442061317));
#147139=CARTESIAN_POINT('Ctrl Pts',(-6.76103393689184,1.85635305550881,
56.6881746344584));
#147140=CARTESIAN_POINT('Ctrl Pts',(-6.81267817211495,1.66825929502929,
56.6970312677377));
#147141=CARTESIAN_POINT('Ctrl Pts',(-6.85646090792406,1.47803777657233,
56.705887901017));
#147142=CARTESIAN_POINT('Ctrl Pts',(-6.89223750002692,1.28634707825015,
56.7147445342963));
#147143=CARTESIAN_POINT('Ctrl Pts',(-6.92753540368285,1.09722118885126,
56.7234826664054));
#147144=CARTESIAN_POINT('Ctrl Pts',(-6.95504004827874,0.906665467779782,
56.7322207985145));
#147145=CARTESIAN_POINT('Ctrl Pts',(-6.97466431412637,0.715321094161304,
56.7409589306236));
#147146=CARTESIAN_POINT('Ctrl Pts',(-6.99468777829888,0.520084378581257,
56.749874814488));
#147147=CARTESIAN_POINT('Ctrl Pts',(-7.00650678903345,0.324026875386856,
56.7587906983524));
#147148=CARTESIAN_POINT('Ctrl Pts',(-7.01008451422468,0.127834525568464,
56.7677065822168));
#147149=CARTESIAN_POINT('Ctrl Pts',(-7.01366223941591,-0.0683578242499944,
56.7766224660812));
#147150=CARTESIAN_POINT('Ctrl Pts',(-7.00899867963198,-0.2646847182196,
56.7855383499456));
#147151=CARTESIAN_POINT('Ctrl Pts',(-6.99611344218485,-0.460459842527483,
56.79445423381));
#147152=CARTESIAN_POINT('Ctrl Pts',(-6.98348140291007,-0.652387936164065,
56.8031949183031));
#147153=CARTESIAN_POINT('Ctrl Pts',(-6.96294646113462,-0.843806128364029,
56.8119356027962));
#147154=CARTESIAN_POINT('Ctrl Pts',(-6.93457453531067,-1.0340708760626,
56.8206762872894));
#147155=CARTESIAN_POINT('Ctrl Pts',(-6.90620771406765,-1.22430139197131,
56.8294153991881));
#147156=CARTESIAN_POINT('Ctrl Pts',(-6.87000676502785,-1.41337860711619,
56.8381545110868));
#147157=CARTESIAN_POINT('Ctrl Pts',(-6.82608918743713,-1.60066641360838,
56.8468936229856));
#147158=CARTESIAN_POINT('Ctrl Pts',(-6.78160259439649,-1.79038080328941,
56.8557459626615));
#147159=CARTESIAN_POINT('Ctrl Pts',(-6.72919806200088,-1.9782588097309,
56.8645983023374));
#147160=CARTESIAN_POINT('Ctrl Pts',(-6.66905099348429,-2.16365094430831,
56.8734506420133));
#147161=CARTESIAN_POINT('Ctrl Pts',(-6.60970368333869,-2.34657797268516,
56.8821852746598));
#147162=CARTESIAN_POINT('Ctrl Pts',(-6.54281855888771,-2.5270845635597,
56.8909199073064));
#147163=CARTESIAN_POINT('Ctrl Pts',(-6.46861428828942,-2.70456202588107,
56.899654539953));
#147164=CARTESIAN_POINT('Ctrl Pts',(-6.39291006378181,-2.88562699079874,
56.9085657331435));
#147165=CARTESIAN_POINT('Ctrl Pts',(-6.30958773748115,-3.06353878594618,
56.9174769263341));
#147166=CARTESIAN_POINT('Ctrl Pts',(-6.21893156124203,-3.23767150882972,
56.9263881195247));
#147167=CARTESIAN_POINT('Ctrl Pts',(-6.12827538500291,-3.41180423171327,
56.9352993127153));
#147168=CARTESIAN_POINT('Ctrl Pts',(-6.03028548685395,-3.58215760723677,
56.9442105059059));
#147169=CARTESIAN_POINT('Ctrl Pts',(-5.92529694580897,-3.74813055622226,
56.9531216990964));
#147170=CARTESIAN_POINT('Ctrl Pts',(-5.83074138788335,-3.89761034359408,
56.9611473639502));
#147171=CARTESIAN_POINT('Ctrl Pts',(-5.73046512865698,-4.04360545461279,
56.9691730288041));
#147172=CARTESIAN_POINT('Ctrl Pts',(-5.62476393444491,-4.18564896333506,
56.9771986936579));
#147173=CARTESIAN_POINT('Ctrl Pts',(-5.51909628719897,-4.32764739093205,
56.9852218113625));
#147174=CARTESIAN_POINT('Ctrl Pts',(-5.40800735137135,-4.46569641937993,
56.9932449290672));
#147175=CARTESIAN_POINT('Ctrl Pts',(-5.29183575164625,-4.59935875314142,
57.0012680467719));
#147176=CARTESIAN_POINT('Ctrl Pts',(-5.17567880217664,-4.73300423091277,
57.0092901526912));
#147177=CARTESIAN_POINT('Ctrl Pts',(-5.05444070639232,-4.86226383970237,
57.0173122586105));
#147178=CARTESIAN_POINT('Ctrl Pts',(-4.92849980263377,-4.98673402719044,
57.0253343645298));
#147179=CARTESIAN_POINT('Ctrl Pts',(-4.80251209880957,-5.11125046822101,
57.0333594514908));
#147180=CARTESIAN_POINT('Ctrl Pts',(-4.67181835475729,-5.23097367248907,
57.0413845384518));
#147181=CARTESIAN_POINT('Ctrl Pts',(-4.53683346077818,-5.34553727062711,
57.0494096254128));
#147182=CARTESIAN_POINT('Ctrl Pts',(-4.40182198219965,-5.46012343149254,
57.0574362928745));
#147183=CARTESIAN_POINT('Ctrl Pts',(-4.26251795525101,-5.56954773139381,
57.0654629603362));
#147184=CARTESIAN_POINT('Ctrl Pts',(-4.11936847988045,-5.67348481001469,
57.0734896277979));
#147185=CARTESIAN_POINT('Ctrl Pts',(-3.97610408461541,-5.77750532895611,
57.08152273904));
#147186=CARTESIAN_POINT('Ctrl Pts',(-3.82898837722223,-5.87602962067472,
57.089555850282));
#147187=CARTESIAN_POINT('Ctrl Pts',(-3.67849700825313,-5.96877594844813,
57.0975889615241));
#147188=CARTESIAN_POINT('Ctrl Pts',(-3.58982202693959,-6.02342545385527,
57.102322362477));
#147189=CARTESIAN_POINT('Ctrl Pts',(-3.49997551423724,-6.07606970813474,
57.1070557634299));
#147190=CARTESIAN_POINT('Ctrl Pts',(-3.40905855337498,-6.12665866049031,
57.1117891643827));
#147191=CARTESIAN_POINT('Ctrl Pts',(-3.22176678416488,-6.23087347694808,
57.1215401176751));
#147192=CARTESIAN_POINT('Ctrl Pts',(-3.02982105839677,-6.32642565514109,
57.1312910709674));
#147193=CARTESIAN_POINT('Ctrl Pts',(-2.83396501958068,-6.41297659673674,
57.1410420242597));
#147194=CARTESIAN_POINT('Ctrl Pts',(-2.6378268134008,-6.49965223119951,
57.1508070256294));
#147195=CARTESIAN_POINT('Ctrl Pts',(-2.43776706077307,-6.57730067369326,
57.160572026999));
#147196=CARTESIAN_POINT('Ctrl Pts',(-2.23455086245205,-6.64563082074342,
57.1703370283687));
#147197=CARTESIAN_POINT('Ctrl Pts',(-2.03167338342854,-6.71384707559601,
57.1800857535044));
#147198=CARTESIAN_POINT('Ctrl Pts',(-1.82565000952821,-6.77277606441918,
57.18983447864));
#147199=CARTESIAN_POINT('Ctrl Pts',(-1.61725958615924,-6.82217692481484,
57.1995832037756));
#147200=CARTESIAN_POINT('Ctrl Pts',(-1.40944111369837,-6.87144219900405,
57.2093051724409));
#147201=CARTESIAN_POINT('Ctrl Pts',(-1.19926860009142,-6.91123154178717,
57.2190271411061));
#147202=CARTESIAN_POINT('Ctrl Pts',(-0.987531454857761,-6.94135492452061,
57.2287491097713));
#147203=CARTESIAN_POINT('Ctrl Pts',(-0.777195319008167,-6.97127898869877,
57.2384067507093));
#147204=CARTESIAN_POINT('Ctrl Pts',(-0.565315230750769,-6.99166454913837,
57.2480643916473));
#147205=CARTESIAN_POINT('Ctrl Pts',(-0.352681222158356,-7.00237406299013,
57.2577220325852));
#147206=CARTESIAN_POINT('Ctrl Pts',(-0.259221254615671,-7.00708126304533,
57.2619668982799));
#147207=CARTESIAN_POINT('Ctrl Pts',(-0.165615844256471,-7.00991978170583,
57.2662117639746));
#147208=CARTESIAN_POINT('Ctrl Pts',(-0.0719330421756044,-7.01088098600621,
57.2704566296693));
#147209=CARTESIAN_POINT('Ctrl Pts',(0.101354661770682,-7.01265895253301,
57.2783084766835));
#147210=CARTESIAN_POINT('Ctrl Pts',(0.274836025498248,-7.00800916941368,
57.2861603236976));
#147211=CARTESIAN_POINT('Ctrl Pts',(0.44797733170565,-6.99692381499026,
57.2940121707118));
#147212=CARTESIAN_POINT('Ctrl Pts',(0.621069536438241,-6.98584160428375,
57.3018617910056));
#147213=CARTESIAN_POINT('Ctrl Pts',(0.793821495172513,-6.96832747701064,
57.3097114112994));
#147214=CARTESIAN_POINT('Ctrl Pts',(0.965700916892863,-6.94442569991301,
57.3175610315932));
#147215=CARTESIAN_POINT('Ctrl Pts',(1.13756661623999,-6.92052583106654,
57.3254100251952));
#147216=CARTESIAN_POINT('Ctrl Pts',(1.30855953952385,-6.89023938089365,
57.3332590187973));
#147217=CARTESIAN_POINT('Ctrl Pts',(1.47815419782025,-6.85366228595825,
57.3411080123993));
#147218=CARTESIAN_POINT('Ctrl Pts',(1.64783471692615,-6.81706667311071,
57.348960979717));
#147219=CARTESIAN_POINT('Ctrl Pts',(1.81611518324735,-6.77417413269953,
57.3568139470346));
#147220=CARTESIAN_POINT('Ctrl Pts',(1.98248162466146,-6.72513146119685,
57.3646669143523));
#147221=CARTESIAN_POINT('Ctrl Pts',(2.14889031756157,-6.67607633450351,
57.3725218760598));
#147222=CARTESIAN_POINT('Ctrl Pts',(2.31338365545163,-6.62086808638544,
57.3803768377673));
#147223=CARTESIAN_POINT('Ctrl Pts',(2.47546507066133,-6.55970267972838,
57.3882317994748));
#147224=CARTESIAN_POINT('Ctrl Pts',(2.63770736522403,-6.49847656129239,
57.3960945578884));
#147225=CARTESIAN_POINT('Ctrl Pts',(2.79753260411244,-6.43128162237353,
57.403957316302));
#147226=CARTESIAN_POINT('Ctrl Pts',(2.95446583461559,-6.35836128216927,
57.4118200747156));
#147227=CARTESIAN_POINT('Ctrl Pts',(3.06958980062205,-6.30486796695527,
57.4175880814622));
#147228=CARTESIAN_POINT('Ctrl Pts',(3.18315789980236,-6.24829452918601,
57.4233560882089));
#147229=CARTESIAN_POINT('Ctrl Pts',(3.29499208989736,-6.18875219167918,
57.4291240949556));
#147230=CARTESIAN_POINT('Ctrl Pts',(3.45743196144031,-6.10226656820607,
57.4375021613966));
#147231=CARTESIAN_POINT('Ctrl Pts',(3.61657259156186,-6.00932420993033,
57.4458802278377));
#147232=CARTESIAN_POINT('Ctrl Pts',(3.77188826441528,-5.91020181408946,
57.4542582942787));
#147233=CARTESIAN_POINT('Ctrl Pts',(3.92709773425678,-5.81114719696528,
57.4626306318974));
#147234=CARTESIAN_POINT('Ctrl Pts',(4.07848718506613,-5.70592114362543,
57.4710029695161));
#147235=CARTESIAN_POINT('Ctrl Pts',(4.22555676910864,-5.59484553437717,
57.4793753071348));
#147236=CARTESIAN_POINT('Ctrl Pts',(4.37254735656861,-5.48382958799933,
57.4877431476573));
#147237=CARTESIAN_POINT('Ctrl Pts',(4.51522244211506,-5.36697054826797,
57.4961109881799));
#147238=CARTESIAN_POINT('Ctrl Pts',(4.65311199744705,-5.24463299971641,
57.5044788287024));
#147239=CARTESIAN_POINT('Ctrl Pts',(4.79094768695342,-5.12234324168127,
57.5128434003724));
#147240=CARTESIAN_POINT('Ctrl Pts',(4.92400132865464,-4.99457946042438,
57.5212079720423));
#147241=CARTESIAN_POINT('Ctrl Pts',(5.05183642380995,-4.86174611734993,
57.5295725437122));
#147242=CARTESIAN_POINT('Ctrl Pts',(5.17964029283286,-4.72894522132418,
57.5379350721777));
#147243=CARTESIAN_POINT('Ctrl Pts',(5.30222793002041,-4.5910774699408,57.5462976006433));
#147244=CARTESIAN_POINT('Ctrl Pts',(5.41919980444543,-4.44858404911031,
57.5546601291088));
#147245=CARTESIAN_POINT('Ctrl Pts',(5.53618101359193,-4.3060792568591,57.5630233249303));
#147246=CARTESIAN_POINT('Ctrl Pts',(5.64754535141674,-4.15894830787069,
57.5713865207518));
#147247=CARTESIAN_POINT('Ctrl Pts',(5.75293320475518,-4.00766591722979,
57.5797497165733));
#147248=CARTESIAN_POINT('Ctrl Pts',(5.8583282453339,-3.85637320943319,57.588113482748));
#147249=CARTESIAN_POINT('Ctrl Pts',(5.95774580056145,-3.70092876512131,
57.5964772489227));
#147250=CARTESIAN_POINT('Ctrl Pts',(6.05086918737543,-3.54183690191554,
57.6048410150973));
#147251=CARTESIAN_POINT('Ctrl Pts',(6.14401134055583,-3.38271297827572,
57.6132064667509));
#147252=CARTESIAN_POINT('Ctrl Pts',(6.23085663000172,-3.21994045382377,
57.6215719184044));
#147253=CARTESIAN_POINT('Ctrl Pts',(6.31113378383685,-3.05404926695905,
57.629937370058));
#147254=CARTESIAN_POINT('Ctrl Pts',(6.39143782233269,-2.88810252346259,
57.6383056232848));
#147255=CARTESIAN_POINT('Ctrl Pts',(6.46516919588372,-2.71903533075755,
57.6466738765116));
#147256=CARTESIAN_POINT('Ctrl Pts',(6.53210414895704,-2.5473990558368,57.6550421297385));
#147257=CARTESIAN_POINT('Ctrl Pts',(6.59910116028132,-2.37560364960222,
57.6634181415299));
#147258=CARTESIAN_POINT('Ctrl Pts',(6.65928903976748,-2.20123470802503,
57.6717941533214));
#147259=CARTESIAN_POINT('Ctrl Pts',(6.71249303090066,-2.02486144528707,
57.6801701651128));
#147260=CARTESIAN_POINT('Ctrl Pts',(6.76572311392852,-1.8484016869217,57.6885502846039));
#147261=CARTESIAN_POINT('Ctrl Pts',(6.81196238989097,-1.66993596367686,
57.6969304040951));
#147262=CARTESIAN_POINT('Ctrl Pts',(6.85108676488036,-1.49004587264327,
57.7053105235862));
#147263=CARTESIAN_POINT('Ctrl Pts',(6.8902558444242,-1.30995023439335,57.7137002184254));
#147264=CARTESIAN_POINT('Ctrl Pts',(6.92229371470968,-1.12842729894076,
57.7220899132646));
#147265=CARTESIAN_POINT('Ctrl Pts',(6.94712769003129,-0.946067344801934,
57.7304796081038));
#147266=CARTESIAN_POINT('Ctrl Pts',(6.96289435241049,-0.83029015685037,
57.7358060805787));
#147267=CARTESIAN_POINT('Ctrl Pts',(6.97575834093414,-0.714175705115564,
57.7411325530537));
#147268=CARTESIAN_POINT('Ctrl Pts',(6.98571194797933,-0.597875524134276,
57.7464590255286));
#147269=CARTESIAN_POINT('Ctrl Pts',(7.00257721922354,-0.400817905816182,
57.7554841359893));
#147270=CARTESIAN_POINT('Ctrl Pts',(7.01111079365633,-0.202955311594732,
57.7645092464499));
#147271=CARTESIAN_POINT('Ctrl Pts',(7.01124831048953,-0.00486735633776691,
57.7735343569105));
#147272=CARTESIAN_POINT('Ctrl Pts',(7.01124831048998,-0.00486735569163166,
57.7735343569399));
#147273=CARTESIAN_POINT('Ctrl Pts',(7.01137216007327,0.173533450955664,
57.7816624987251));
#147274=CARTESIAN_POINT('Ctrl Pts',(7.00468277305869,0.352181946036952,
57.7897906405102));
#147275=CARTESIAN_POINT('Ctrl Pts',(6.9911500422492,0.530516398671202,57.7979187822954));
#147276=CARTESIAN_POINT('Ctrl Pts',(6.97763572442698,0.708608204787677,
57.8060358647183));
#147277=CARTESIAN_POINT('Ctrl Pts',(6.9572966460282,0.886386467559613,57.8141529471413));
#147278=CARTESIAN_POINT('Ctrl Pts',(6.93015469145915,1.06328853795513,57.8222700295642));
#147279=CARTESIAN_POINT('Ctrl Pts',(6.90303402361234,1.24005186870217,57.8303807459726));
#147280=CARTESIAN_POINT('Ctrl Pts',(6.86912115405176,1.41594002501076,57.838491462381));
#147281=CARTESIAN_POINT('Ctrl Pts',(6.82848988511768,1.59039380385664,57.8466021787894));
#147282=CARTESIAN_POINT('Ctrl Pts',(6.78788803830109,1.76472125636045,57.8547070220252));
#147283=CARTESIAN_POINT('Ctrl Pts',(6.74057756546112,1.93761605511888,57.8628118652611));
#147284=CARTESIAN_POINT('Ctrl Pts',(6.68668361174142,2.10852764719099,57.870916708497));
#147285=CARTESIAN_POINT('Ctrl Pts',(6.65102377983819,2.22161414804974,57.8762794129832));
#147286=CARTESIAN_POINT('Ctrl Pts',(6.61248274091082,2.33383255763744,57.8816421174695));
#147287=CARTESIAN_POINT('Ctrl Pts',(6.57110895151813,2.44502632087639,57.8870048219557));
#147288=CARTESIAN_POINT('',(7.01124998181045,-0.000505037546988676,57.2264656430896));
#147289=CARTESIAN_POINT('Ctrl Pts',(6.57110895151816,2.4450263208763,57.3398522865015));
#147290=CARTESIAN_POINT('Ctrl Pts',(6.63771924680899,2.266008408508,57.3311805125693));
#147291=CARTESIAN_POINT('Ctrl Pts',(6.69700989700473,2.08426710051955,57.3225087386372));
#147292=CARTESIAN_POINT('Ctrl Pts',(6.74878307789422,1.90040877971785,57.3138369647051));
#147293=CARTESIAN_POINT('Ctrl Pts',(6.80055978789531,1.71653792623954,57.3051645996628));
#147294=CARTESIAN_POINT('Ctrl Pts',(6.84481792613573,1.53055004459453,57.2964922346204));
#147295=CARTESIAN_POINT('Ctrl Pts',(6.88140980451098,1.3430657708691,57.2878198695781));
#147296=CARTESIAN_POINT('Ctrl Pts',(6.91799949925383,1.15559268532943,57.2791480220619));
#147297=CARTESIAN_POINT('Ctrl Pts',(6.94692379517689,0.966623665170781,
57.2704761745458));
#147298=CARTESIAN_POINT('Ctrl Pts',(6.96808618426389,0.776789219267855,
57.2618043270297));
#147299=CARTESIAN_POINT('Ctrl Pts',(6.98924897510677,0.586951169466182,
57.2531323148835));
#147300=CARTESIAN_POINT('Ctrl Pts',(7.00264953276857,0.396247943319445,
57.2444603027373));
#147301=CARTESIAN_POINT('Ctrl Pts',(7.00824314361839,0.205315860142146,
57.2357882905911));
#147302=CARTESIAN_POINT('Ctrl Pts',(7.01024757124657,0.136896809746564,
57.2326807414239));
#147303=CARTESIAN_POINT('Ctrl Pts',(7.01125,0.0684484052929644,57.2295731922568));
#147304=CARTESIAN_POINT('Ctrl Pts',(7.01125,8.58630487052188E-16,57.2264656430896));
#147305=CARTESIAN_POINT('Ctrl Pts',(7.01124998181045,-0.000505037546988675,
57.2264656430896));
#147306=CARTESIAN_POINT('Ctrl Pts',(7.01123724491756,-0.177326623645792,
57.2184554091803));
#147307=CARTESIAN_POINT('Ctrl Pts',(7.00453108466972,-0.354163812240794,
57.2104451752711));
#147308=CARTESIAN_POINT('Ctrl Pts',(6.99115392040837,-0.530465289777442,
57.2024349413618));
#147309=CARTESIAN_POINT('Ctrl Pts',(6.97777149517461,-0.706836103175747,
57.194421557187));
#147310=CARTESIAN_POINT('Ctrl Pts',(6.957712851468,-0.882670417579134,57.1864081730122));
#147311=CARTESIAN_POINT('Ctrl Pts',(6.93105236669831,-1.05742122760315,
57.1783947888374));
#147312=CARTESIAN_POINT('Ctrl Pts',(6.90438587943545,-1.23221138201846,
57.1703796004837));
#147313=CARTESIAN_POINT('Ctrl Pts',(6.8711146549574,-1.40591718416178,57.16236441213));
#147314=CARTESIAN_POINT('Ctrl Pts',(6.83136423261756,-1.57800167421124,
57.1543492237764));
#147315=CARTESIAN_POINT('Ctrl Pts',(6.79158278043253,-1.75022049629471,
57.1463277786324));
#147316=CARTESIAN_POINT('Ctrl Pts',(6.74531212406688,-1.92081512357284,
57.1383063334885));
#147317=CARTESIAN_POINT('Ctrl Pts',(6.69272786200115,-2.08926310638309,
57.1302848883446));
#147318=CARTESIAN_POINT('Ctrl Pts',(6.6708820426386,-2.15924382038188,57.1269524266012));
#147319=CARTESIAN_POINT('Ctrl Pts',(6.64794711619884,-2.22885425457659,
57.1236199648578));
#147320=CARTESIAN_POINT('Ctrl Pts',(6.62393811561288,-2.29805796337492,
57.1202875031143));
#147321=CARTESIAN_POINT('Ctrl Pts',(6.55368655366752,-2.50055154981511,
57.1105365498516));
#147322=CARTESIAN_POINT('Ctrl Pts',(6.47419318465181,-2.69968513413424,
57.1007855965888));
#147323=CARTESIAN_POINT('Ctrl Pts',(6.3857870322112,-2.89471078723649,57.0910346433261));
#147324=CARTESIAN_POINT('Ctrl Pts',(6.29725351413347,-3.09001741135576,
57.0812696419871));
#147325=CARTESIAN_POINT('Ctrl Pts',(6.19978154373158,-3.28120423083926,
57.071504640648));
#147326=CARTESIAN_POINT('Ctrl Pts',(6.09374778772134,-3.467544442706,57.061739639309));
#147327=CARTESIAN_POINT('Ctrl Pts',(5.98789076800703,-3.65357406405831,
57.0519909142034));
#147328=CARTESIAN_POINT('Ctrl Pts',(5.87350050281105,-3.83477319006731,
57.0422421890978));
#147329=CARTESIAN_POINT('Ctrl Pts',(5.75099737952567,-4.01044333000591,
57.0324934639922));
#147330=CARTESIAN_POINT('Ctrl Pts',(5.62883047979592,-4.18563132355114,
57.0227714953556));
#147331=CARTESIAN_POINT('Ctrl Pts',(5.49859519654304,-4.35532059252179,
57.013049526719));
#147332=CARTESIAN_POINT('Ctrl Pts',(5.36075366068567,-4.51884351930283,
57.0033275580824));
#147333=CARTESIAN_POINT('Ctrl Pts',(5.22382418622545,-4.68128445763867,
56.9936699171699));
#147334=CARTESIAN_POINT('Ctrl Pts',(5.07938879163111,-4.83764033191866,
56.9840122762575));
#147335=CARTESIAN_POINT('Ctrl Pts',(4.92794503770073,-4.98728225268039,
56.974354635345));
#147336=CARTESIAN_POINT('Ctrl Pts',(4.86138029135914,-5.0530550312801,56.970109769506));
#147337=CARTESIAN_POINT('Ctrl Pts',(4.79346217679016,-5.11753107602661,
56.9658649036669));
#147338=CARTESIAN_POINT('Ctrl Pts',(4.72423569398403,-5.18065861355361,
56.9616200378279));
#147339=CARTESIAN_POINT('Ctrl Pts',(4.59618553305735,-5.29742738486149,
56.9537681907924));
#147340=CARTESIAN_POINT('Ctrl Pts',(4.46370883211363,-5.40953147895155,
56.9459163437568));
#147341=CARTESIAN_POINT('Ctrl Pts',(4.32719841650096,-5.51660950464428,
56.9380644967213));
#147342=CARTESIAN_POINT('Ctrl Pts',(4.19072671413717,-5.62365716387566,
56.930214876406));
#147343=CARTESIAN_POINT('Ctrl Pts',(4.05022387242283,-5.7256813547798,56.9223652560908));
#147344=CARTESIAN_POINT('Ctrl Pts',(3.90611635385955,-5.82236048288072,
56.9145156357755));
#147345=CARTESIAN_POINT('Ctrl Pts',(3.76202034043703,-5.91903189239077,
56.9066666421519));
#147346=CARTESIAN_POINT('Ctrl Pts',(3.61432054026825,-6.01035887671013,
56.8988176485283));
#147347=CARTESIAN_POINT('Ctrl Pts',(3.46347276498308,-6.09606290721483,
56.8909686549048));
#147348=CARTESIAN_POINT('Ctrl Pts',(3.31254861988543,-6.18181032716113,
56.8831156875655));
#147349=CARTESIAN_POINT('Ctrl Pts',(3.15847364742723,-6.26192891668545,
56.8752627202263));
#147350=CARTESIAN_POINT('Ctrl Pts',(3.00172895266888,-6.33618574989791,
56.867409752887));
#147351=CARTESIAN_POINT('Ctrl Pts',(2.8449444500238,-6.41046144185141,56.8595547911578));
#147352=CARTESIAN_POINT('Ctrl Pts',(2.68548922490902,-6.47887226125682,
56.8516998294287));
#147353=CARTESIAN_POINT('Ctrl Pts',(2.52386415672786,-6.54123354428539,
56.8438448676995));
#147354=CARTESIAN_POINT('Ctrl Pts',(2.36207866215702,-6.60365672609986,
56.8359821092643));
#147355=CARTESIAN_POINT('Ctrl Pts',(2.1981193835196,-6.66001825472769,56.8281193508291));
#147356=CARTESIAN_POINT('Ctrl Pts',(2.03250269519127,-6.71018325804447,
56.8202565923939));
#147357=CARTESIAN_POINT('Ctrl Pts',(1.91100867218322,-6.74698358371626,
56.8144885857764));
#147358=CARTESIAN_POINT('Ctrl Pts',(1.78862303317405,-6.7804503082767,56.808720579159));
#147359=CARTESIAN_POINT('Ctrl Pts',(1.66555265432867,-6.81054776931773,
56.8029525725415));
#147360=CARTESIAN_POINT('Ctrl Pts',(1.48679214367329,-6.85426452354895,
56.7945745061208));
#147361=CARTESIAN_POINT('Ctrl Pts',(1.30619072169333,-6.8909680429163,56.7861964397));
#147362=CARTESIAN_POINT('Ctrl Pts',(1.12432479047456,-6.92051445544508,
56.7778183732792));
#147363=CARTESIAN_POINT('Ctrl Pts',(0.942583217022785,-6.95004066448738,
56.7694460356809));
#147364=CARTESIAN_POINT('Ctrl Pts',(0.759579181637139,-6.97241947122276,
56.7610736980826));
#147365=CARTESIAN_POINT('Ctrl Pts',(0.575899895042257,-6.98755793345503,
56.7527013604843));
#147366=CARTESIAN_POINT('Ctrl Pts',(0.392319269475441,-7.00268826425194,
56.7443335199822));
#147367=CARTESIAN_POINT('Ctrl Pts',(0.208064442775255,-7.01058597802294,
56.7359656794802));
#147368=CARTESIAN_POINT('Ctrl Pts',(0.0237288361009822,-7.01120984601355,
56.7275978389782));
#147369=CARTESIAN_POINT('Ctrl Pts',(-0.160534760840535,-7.01183347029341,
56.7192332673289));
#147370=CARTESIAN_POINT('Ctrl Pts',(-0.344878746602167,-7.00518891401741,
56.7108686956796));
#147371=CARTESIAN_POINT('Ctrl Pts',(-0.528708140090684,-6.99128702494053,
56.7025041240303));
#147372=CARTESIAN_POINT('Ctrl Pts',(-0.712492629783648,-6.97738853166219,
56.6941415955854));
#147373=CARTESIAN_POINT('Ctrl Pts',(-0.89576245044932,-6.9562362660491,
56.6857790671405));
#147374=CARTESIAN_POINT('Ctrl Pts',(-1.07792572532216,-6.92789309192836,
56.6774165386956));
#147375=CARTESIAN_POINT('Ctrl Pts',(-1.26010353739538,-6.89954765593348,
56.6690533428946));
#147376=CARTESIAN_POINT('Ctrl Pts',(-1.44117430156223,-6.86401020950662,
56.6606901470937));
#147377=CARTESIAN_POINT('Ctrl Pts',(-1.62055357410303,-6.82139521476083,
56.6523269512928));
#147378=CARTESIAN_POINT('Ctrl Pts',(-1.79994507995217,-6.77877731375746,
56.6439631851387));
#147379=CARTESIAN_POINT('Ctrl Pts',(-1.97764454418465,-6.72908097776443,
56.6355994189845));
#147380=CARTESIAN_POINT('Ctrl Pts',(-2.15307981856414,-6.67247134556544,
56.6272356528303));
#147381=CARTESIAN_POINT('Ctrl Pts',(-2.32855044692903,-6.6158503053066,
56.6188702011972));
#147382=CARTESIAN_POINT('Ctrl Pts',(-2.50175566270643,-6.55231329178988,
56.610504749564));
#147383=CARTESIAN_POINT('Ctrl Pts',(-2.67214011610176,-6.48207480382784,
56.6021392979309));
#147384=CARTESIAN_POINT('Ctrl Pts',(-2.84258163091896,-6.41181279313286,
56.5937710447243));
#147385=CARTESIAN_POINT('Ctrl Pts',(-3.01020019581222,-6.33484495803051,
56.5854027915176));
#147386=CARTESIAN_POINT('Ctrl Pts',(-3.17446162221211,-6.25143343334971,
56.577034538311));
#147387=CARTESIAN_POINT('Ctrl Pts',(-3.33887534239639,-6.16794457428167,
56.5686585265394));
#147388=CARTESIAN_POINT('Ctrl Pts',(-3.49992541083501,-6.07800023637808,
56.5602825147678));
#147389=CARTESIAN_POINT('Ctrl Pts',(-3.65710229183514,-5.98190850728713,
56.5519065029962));
#147390=CARTESIAN_POINT('Ctrl Pts',(-3.81435625432398,-5.88576965362237,
56.5435263835248));
#147391=CARTESIAN_POINT('Ctrl Pts',(-3.96773296456334,-5.78347757372875,
56.5351462640533));
#147392=CARTESIAN_POINT('Ctrl Pts',(-4.11675242066685,-5.67538334118795,
56.5267661445818));
#147393=CARTESIAN_POINT('Ctrl Pts',(-4.26594215038535,-5.56716559728684,
56.5183764497617));
#147394=CARTESIAN_POINT('Ctrl Pts',(-4.41076441511358,-5.45313265159622,
56.5099867549417));
#147395=CARTESIAN_POINT('Ctrl Pts',(-4.55077176871854,-5.33367629984557,
56.5015970601216));
#147396=CARTESIAN_POINT('Ctrl Pts',(-4.63966002571034,-5.25783551991287,
56.496270587404));
#147397=CARTESIAN_POINT('Ctrl Pts',(-4.72660820663073,-5.17980947826596,
56.4909441146863));
#147398=CARTESIAN_POINT('Ctrl Pts',(-4.81150961224631,-5.09970605170155,
56.4856176419687));
#147399=CARTESIAN_POINT('Ctrl Pts',(-4.94510349810382,-4.97366187201275,
56.4772363415284));
#147400=CARTESIAN_POINT('Ctrl Pts',(-5.0738972911768,-4.84221812688308,
56.4688550410881));
#147401=CARTESIAN_POINT('Ctrl Pts',(-5.19744339804855,-4.70576334791514,
56.4604737406478));
#147402=CARTESIAN_POINT('Ctrl Pts',(-5.32083292830701,-4.5694815054136,
56.4521030622795));
#147403=CARTESIAN_POINT('Ctrl Pts',(-5.43898780833956,-4.42820152638251,
56.4437323839112));
#147404=CARTESIAN_POINT('Ctrl Pts',(-5.55149553377463,-4.28235027770737,
56.4353617055429));
#147405=CARTESIAN_POINT('Ctrl Pts',(-5.66387558224888,-4.13666454516981,
56.4270005264581));
#147406=CARTESIAN_POINT('Ctrl Pts',(-5.77062105016662,-3.98641814031486,
56.4186393473732));
#147407=CARTESIAN_POINT('Ctrl Pts',(-5.87135786437864,-3.83207298872284,
56.4102781682883));
#147408=CARTESIAN_POINT('Ctrl Pts',(-5.97196396067764,-3.67792811819247,
56.4019278388208));
#147409=CARTESIAN_POINT('Ctrl Pts',(-6.06657677685428,-3.51969538253832,
56.3935775093532));
#147410=CARTESIAN_POINT('Ctrl Pts',(-6.15486398766265,-3.35786775437531,
56.3852271798856));
#147411=CARTESIAN_POINT('Ctrl Pts',(-6.24308326673597,-3.1961646429057,
56.3768832754977));
#147412=CARTESIAN_POINT('Ctrl Pts',(-6.32498648358142,-3.03087243757995,
56.3685393711099));
#147413=CARTESIAN_POINT('Ctrl Pts',(-6.40028532324032,-2.86251189405645,
56.360195466722));
#147414=CARTESIAN_POINT('Ctrl Pts',(-6.47552368239123,-2.69428657879464,
56.3518582642114));
#147415=CARTESIAN_POINT('Ctrl Pts',(-6.54416811039554,-2.52299813867956,
56.3435210617007));
#147416=CARTESIAN_POINT('Ctrl Pts',(-6.60597677508422,-2.34919079888117,
56.3351838591901));
#147417=CARTESIAN_POINT('Ctrl Pts',(-6.62632384476534,-2.29197438639628,
56.3324392983541));
#147418=CARTESIAN_POINT('Ctrl Pts',(-6.64593050863622,-2.2344851838378,
56.3296947375181));
#147419=CARTESIAN_POINT('Ctrl Pts',(-6.66478926863333,-2.17674311006374,
56.3269501766821));
#147420=CARTESIAN_POINT('Ctrl Pts',(-6.72208447980906,-2.00131565295013,
56.3186118663845));
#147421=CARTESIAN_POINT('Ctrl Pts',(-6.77242574454439,-1.82369680889926,
56.3102735560869));
#147422=CARTESIAN_POINT('Ctrl Pts',(-6.81567017129344,-1.64446546897187,
56.3019352457894));
#147423=CARTESIAN_POINT('Ctrl Pts',(-6.85894180596994,-1.46512136276081,
56.2935916893096));
#147424=CARTESIAN_POINT('Ctrl Pts',(-6.89510761963376,-1.28416305558202,
56.2852481328298));
#147425=CARTESIAN_POINT('Ctrl Pts',(-6.92407593220963,-1.10217922657585,
56.2769045763501));
#147426=CARTESIAN_POINT('Ctrl Pts',(-6.95306628375251,-0.920056945059139,
56.2685546721286));
#147427=CARTESIAN_POINT('Ctrl Pts',(-6.97484816026935,-0.736907908656635,
56.2602047679072));
#147428=CARTESIAN_POINT('Ctrl Pts',(-6.98938172955969,-0.55332594462682,
56.2518548636857));
#147429=CARTESIAN_POINT('Ctrl Pts',(-7.0039370981293,-0.369468621225876,
56.2434924352253));
#147430=CARTESIAN_POINT('Ctrl Pts',(-7.01122240806667,-0.185177399485568,
56.235130006765));
#147431=CARTESIAN_POINT('Ctrl Pts',(-7.01124992172658,-0.00104765881511994,
56.2267675783046));
#147432=CARTESIAN_POINT('Ctrl Pts',(-7.01127745891443,0.183239537890237,
56.2183979988277));
#147433=CARTESIAN_POINT('Ctrl Pts',(-7.00403482928812,0.367364651384708,
56.2100284193507));
#147434=CARTESIAN_POINT('Ctrl Pts',(-6.98958621935857,0.550736819772151,
56.2016588398738));
#147435=CARTESIAN_POINT('Ctrl Pts',(-6.97511532420791,0.734391817396487,
56.1932763513398));
#147436=CARTESIAN_POINT('Ctrl Pts',(-6.95341627750075,0.917291224500392,
56.1848938628059));
#147437=CARTESIAN_POINT('Ctrl Pts',(-6.92460468464367,1.09885236674949,
56.1765113742719));
#147438=CARTESIAN_POINT('Ctrl Pts',(-6.91517705927983,1.15826214802212,
56.1737684866465));
#147439=CARTESIAN_POINT('Ctrl Pts',(-6.90498829125462,1.21752874795626,
56.1710255990212));
#147440=CARTESIAN_POINT('Ctrl Pts',(-6.89404359273626,1.27663209420416,
56.1682827113958));
#147441=CARTESIAN_POINT('Ctrl Pts',(-6.86056630663616,1.45741547791228,
56.1598928563787));
#147442=CARTESIAN_POINT('Ctrl Pts',(-6.81994515962662,1.63703541942779,
56.1515030013616));
#147443=CARTESIAN_POINT('Ctrl Pts',(-6.77227735248947,1.81490661563019,
56.1431131463445));
#147444=CARTESIAN_POINT('Ctrl Pts',(-6.72465353254082,1.99261367477013,
56.1347310333688));
#147445=CARTESIAN_POINT('Ctrl Pts',(-6.66999609999171,2.16857488955242,
56.126348920393));
#147446=CARTESIAN_POINT('Ctrl Pts',(-6.6084532761143,2.34221516089241,56.1179668074173));
#147447=CARTESIAN_POINT('Ctrl Pts',(-6.54695819642816,2.51572072417377,
56.1095911971852));
#147448=CARTESIAN_POINT('Ctrl Pts',(-6.47858848436843,2.68690862505205,
56.1012155869531));
#147449=CARTESIAN_POINT('Ctrl Pts',(-6.40354228977823,2.85521850398911,
56.0928399767209));
#147450=CARTESIAN_POINT('Ctrl Pts',(-6.32854330036063,3.02342251350895,
56.0844696348722));
#147451=CARTESIAN_POINT('Ctrl Pts',(-6.2468763355756,3.18875181124019,56.0760992930235));
#147452=CARTESIAN_POINT('Ctrl Pts',(-6.15878797446274,3.35066519487,56.0677289511748));
#147453=CARTESIAN_POINT('Ctrl Pts',(-6.07074210947161,3.5125004672627,56.0593626473972));
#147454=CARTESIAN_POINT('Ctrl Pts',(-5.97628118258174,3.67092282354423,
56.0509963436196));
#147455=CARTESIAN_POINT('Ctrl Pts',(-5.87569830779665,3.82541448189024,
56.042630039842));
#147456=CARTESIAN_POINT('Ctrl Pts',(-5.77514356321215,3.97986293326541,
56.0342660758843));
#147457=CARTESIAN_POINT('Ctrl Pts',(-5.66847046265733,4.13038260273449,
56.0259021119265));
#147458=CARTESIAN_POINT('Ctrl Pts',(-5.55601644007937,4.27648312051711,
56.0175381479687));
#147459=CARTESIAN_POINT('Ctrl Pts',(-5.4435797222972,4.42256115587032,56.0091754710853));
#147460=CARTESIAN_POINT('Ctrl Pts',(-5.32536405655652,4.56422113502112,
56.0008127942018));
#147461=CARTESIAN_POINT('Ctrl Pts',(-5.20174855583322,4.7010039911052,55.9924501173184));
#147462=CARTESIAN_POINT('Ctrl Pts',(-5.07813560011289,4.83778403109605,
55.9840876126062));
#147463=CARTESIAN_POINT('Ctrl Pts',(-4.9491232517426,4.96968690467919,55.9757251078941));
#147464=CARTESIAN_POINT('Ctrl Pts',(-4.8151293233923,5.09628846922028,55.9673626031819));
#147465=CARTESIAN_POINT('Ctrl Pts',(-4.68112029327568,5.22290430237241,
55.9589991559749));
#147466=CARTESIAN_POINT('Ctrl Pts',(-4.54212880305775,5.34421740996469,
55.9506357087678));
#147467=CARTESIAN_POINT('Ctrl Pts',(-4.39860806628166,5.45984190629564,
55.9422722615608));
#147468=CARTESIAN_POINT('Ctrl Pts',(-4.25500282041639,5.57553448561647,
55.9339038897183));
#147469=CARTESIAN_POINT('Ctrl Pts',(-4.10686325439232,5.68553155319408,
55.9255355178758));
#147470=CARTESIAN_POINT('Ctrl Pts',(-3.95467489630229,5.78948814896934,
55.9171671460333));
#147471=CARTESIAN_POINT('Ctrl Pts',(-3.80244093857533,5.89347589287633,
55.9087962668064));
#147472=CARTESIAN_POINT('Ctrl Pts',(-3.64615604426595,5.99141937507047,
55.9004253875795));
#147473=CARTESIAN_POINT('Ctrl Pts',(-3.48633361420345,6.08301771269615,
55.8920545083526));
#147474=CARTESIAN_POINT('Ctrl Pts',(-3.32637576825999,6.17469366063961,
55.8836765365669));
#147475=CARTESIAN_POINT('Ctrl Pts',(-3.16287468543343,6.26001356257396,
55.8752985647811));
#147476=CARTESIAN_POINT('Ctrl Pts',(-2.99636821242039,6.3387225919815,55.8669205929954));
#147477=CARTESIAN_POINT('Ctrl Pts',(-2.8905519644874,6.3887428345561,55.8615963222712));
#147478=CARTESIAN_POINT('Ctrl Pts',(-2.78352237841438,6.43609408750066,
55.856272051547));
#147479=CARTESIAN_POINT('Ctrl Pts',(-2.6754215039807,6.48072112797161,55.8509477808228));
#147480=CARTESIAN_POINT('Ctrl Pts',(-2.51577917410116,6.54662591138558,
55.8430849491133));
#147481=CARTESIAN_POINT('Ctrl Pts',(-2.35346751901651,6.60672388344153,
55.8352221174038));
#147482=CARTESIAN_POINT('Ctrl Pts',(-2.18896617001708,6.66078476375125,
55.8273592856943));
#147483=CARTESIAN_POINT('Ctrl Pts',(-2.02459121863661,6.71480410539522,
55.8195024955353));
#147484=CARTESIAN_POINT('Ctrl Pts',(-1.85803027908938,6.76279546176815,
55.8116457053763));
#147485=CARTESIAN_POINT('Ctrl Pts',(-1.68978406494728,6.80457613495141,
55.8037889152173));
#147486=CARTESIAN_POINT('Ctrl Pts',(-1.52163273375822,6.84633324579972,
55.7959365559185));
#147487=CARTESIAN_POINT('Ctrl Pts',(-1.35179838744811,6.88188654919576,
55.7880841966197));
#147488=CARTESIAN_POINT('Ctrl Pts',(-1.18079780428295,6.9111028865081,55.7802318373209));
#147489=CARTESIAN_POINT('Ctrl Pts',(-1.00983759645948,6.94031232548372,
55.7723813320607));
#147490=CARTESIAN_POINT('Ctrl Pts',(-0.837712073892817,6.96318770382964,
55.7645308268005));
#147491=CARTESIAN_POINT('Ctrl Pts',(-0.66494907568763,6.9796467882868,55.7566803215403));
#147492=CARTESIAN_POINT('Ctrl Pts',(-0.49221386965655,6.99610322499099,
55.7488310791814));
#147493=CARTESIAN_POINT('Ctrl Pts',(-0.318841772228494,7.00614538938612,
55.7409818368225));
#147494=CARTESIAN_POINT('Ctrl Pts',(-0.14536615867979,7.00974287990727,
55.7331325944636));
#147495=CARTESIAN_POINT('Ctrl Pts',(0.028167902071642,7.01334158249077,
55.7252807075471));
#147496=CARTESIAN_POINT('Ctrl Pts',(0.201805166826835,7.01049126617955,
55.7174288206305));
#147497=CARTESIAN_POINT('Ctrl Pts',(0.375011639626966,7.00121366854664,
55.709576933714));
#147498=CARTESIAN_POINT('Ctrl Pts',(0.502194920866248,6.99440124814517,
55.7038113943215));
#147499=CARTESIAN_POINT('Ctrl Pts',(0.629145902603533,6.98412447108672,
55.698045854929));
#147500=CARTESIAN_POINT('Ctrl Pts',(0.755654947645477,6.9704097557173,55.6922803155365));
#147501=CARTESIAN_POINT('Ctrl Pts',(0.967514223858894,6.94744230962937,
55.6826250137968));
#147502=CARTESIAN_POINT('Ctrl Pts',(1.17802593747764,6.91484431154008,55.6729697120572));
#147503=CARTESIAN_POINT('Ctrl Pts',(1.38640874482444,6.87280854925949,55.6633144103175));
#147504=CARTESIAN_POINT('Ctrl Pts',(1.59594594977885,6.83053991755926,55.6536056202053));
#147505=CARTESIAN_POINT('Ctrl Pts',(1.80333056029977,6.77872872847641,55.6438968300932));
#147506=CARTESIAN_POINT('Ctrl Pts',(2.00778925425767,6.71761928610035,55.634188039981));
#147507=CARTESIAN_POINT('Ctrl Pts',(2.21323181874091,6.65621578051764,55.6244325304447));
#147508=CARTESIAN_POINT('Ctrl Pts',(2.41572020486721,6.58542435393008,55.6146770209085));
#147509=CARTESIAN_POINT('Ctrl Pts',(2.61449161453801,6.50554072771898,55.6049215113722));
#147510=CARTESIAN_POINT('Ctrl Pts',(2.81345983918247,6.42557800414768,55.5951563423464));
#147511=CARTESIAN_POINT('Ctrl Pts',(3.00870369433969,6.3365050981482,55.5853911733206));
#147512=CARTESIAN_POINT('Ctrl Pts',(3.19948029428995,6.23866591579885,55.5756260042948));
#147513=CARTESIAN_POINT('Ctrl Pts',(3.38999677842398,6.14096013303196,55.5658741496635));
#147514=CARTESIAN_POINT('Ctrl Pts',(3.57605814715117,6.03451197991433,55.5561222950322));
#147515=CARTESIAN_POINT('Ctrl Pts',(3.75694710651464,5.91971071939764,55.5463704404009));
#147516=CARTESIAN_POINT('Ctrl Pts',(3.83582807475557,5.86964887694633,55.5421179103506));
#147517=CARTESIAN_POINT('Ctrl Pts',(3.91372574775415,5.81799920250456,55.5378653803003));
#147518=CARTESIAN_POINT('Ctrl Pts',(3.99058202083765,5.76479676115883,55.53361285025));
#147519=CARTESIAN_POINT('Ctrl Pts',(4.13576384025537,5.66429712824473,55.5255798033032));
#147520=CARTESIAN_POINT('Ctrl Pts',(4.27729829741059,5.55820455855653,55.5175467563565));
#147521=CARTESIAN_POINT('Ctrl Pts',(4.4147229865368,5.44681994512794,55.5095137094097));
#147522=CARTESIAN_POINT('Ctrl Pts',(4.55205933369662,5.33550693408638,55.5014858264198));
#147523=CARTESIAN_POINT('Ctrl Pts',(4.68529088804447,5.21890888078641,55.4934579434299));
#147524=CARTESIAN_POINT('Ctrl Pts',(4.81398506889093,5.09736935281281,55.48543006044));
#147525=CARTESIAN_POINT('Ctrl Pts',(4.9426211429497,4.97588470122523,55.4774058021244));
#147526=CARTESIAN_POINT('Ctrl Pts',(5.06672365669603,4.84946326856371,55.4693815438088));
#147527=CARTESIAN_POINT('Ctrl Pts',(5.18589396084689,4.7184881465732,55.4613572854932));
#147528=CARTESIAN_POINT('Ctrl Pts',(5.3050498559007,4.58752886102161,55.4533339974052));
#147529=CARTESIAN_POINT('Ctrl Pts',(5.41927447695573,4.45201724861941,55.4453107093172));
#147530=CARTESIAN_POINT('Ctrl Pts',(5.52820672190483,4.31237254911798,55.4372874212292));
#147531=CARTESIAN_POINT('Ctrl Pts',(5.63713004073727,4.17273929237051,55.4292647905847));
#147532=CARTESIAN_POINT('Ctrl Pts',(5.74076162494552,4.02897391469021,55.4212421599403));
#147533=CARTESIAN_POINT('Ctrl Pts',(5.83878148468279,3.88152770653842,55.4132195292959));
#147534=CARTESIAN_POINT('Ctrl Pts',(5.93683819271826,3.73402606939643,55.4051938827291));
#147535=CARTESIAN_POINT('Ctrl Pts',(6.02927876143492,3.58284114470238,55.3971682361623));
#147536=CARTESIAN_POINT('Ctrl Pts',(6.11582705957431,3.42845241178563,55.3891425895955));
#147537=CARTESIAN_POINT('Ctrl Pts',(6.16686111599986,3.3374155748226,55.3844101880516));
#147538=CARTESIAN_POINT('Ctrl Pts',(6.21584728934764,3.24526527880537,55.3796777865076));
#147539=CARTESIAN_POINT('Ctrl Pts',(6.26273655294488,3.15210365167582,55.3749453849637));
#147540=CARTESIAN_POINT('Ctrl Pts',(6.34919419481366,2.98032585061109,55.3662194582488));
#147541=CARTESIAN_POINT('Ctrl Pts',(6.42856377990602,2.80502227980312,55.3574935315339));
#147542=CARTESIAN_POINT('Ctrl Pts',(6.50058655335303,2.62678530239259,55.348767604819));
#147543=CARTESIAN_POINT('Ctrl Pts',(6.52493627278427,2.5665263011836,55.3458175119926));
#147544=CARTESIAN_POINT('Ctrl Pts',(6.54844665376745,2.50593217957409,55.3428674191661));
#147545=CARTESIAN_POINT('Ctrl Pts',(6.57110895151813,2.44502632087638,55.3399173263397));
#147546=CARTESIAN_POINT('Origin',(0.,0.,50.));
#147547=CARTESIAN_POINT('',(6.57110895151814,2.44502632087635,53.3398059204455));
#147548=CARTESIAN_POINT('',(6.57110895151814,2.44502632087637,53.8869540129975));
#147549=CARTESIAN_POINT('',(6.57110895151814,2.44502632087636,50.));
#147550=CARTESIAN_POINT('',(7.01124705281182,0.00642860308702523,55.773534356869));
#147551=CARTESIAN_POINT('Ctrl Pts',(6.57110895151814,2.44502632087636,53.8869540129975));
#147552=CARTESIAN_POINT('Ctrl Pts',(6.50353113000907,2.62664449980998,53.8957638417488));
#147553=CARTESIAN_POINT('Ctrl Pts',(6.42844709549375,2.80538575922644,53.9045736705001));
#147554=CARTESIAN_POINT('Ctrl Pts',(6.34612790280083,2.98065214404377,53.9133834992514));
#147555=CARTESIAN_POINT('Ctrl Pts',(6.26808555048096,3.1468126772838,53.9217356190523));
#147556=CARTESIAN_POINT('Ctrl Pts',(6.18354076655633,3.30985002457295,53.9300877388533));
#147557=CARTESIAN_POINT('Ctrl Pts',(6.09276264047734,3.46927513600516,53.9384398586542));
#147558=CARTESIAN_POINT('Ctrl Pts',(6.00730213029333,3.61936141722321,53.9463027266175));
#147559=CARTESIAN_POINT('Ctrl Pts',(5.91616768828528,3.76650633753764,53.9541655945807));
#147560=CARTESIAN_POINT('Ctrl Pts',(5.81959624471386,3.91023351105946,53.9620284625439));
#147561=CARTESIAN_POINT('Ctrl Pts',(5.72309900317295,4.05385024978065,53.9698852889616));
#147562=CARTESIAN_POINT('Ctrl Pts',(5.62117327908481,4.19405414961448,53.9777421153793));
#147563=CARTESIAN_POINT('Ctrl Pts',(5.51410187190258,4.33039341270288,53.9855989417971));
#147564=CARTESIAN_POINT('Ctrl Pts',(5.40709084775426,4.46665578711892,53.9934513373492));
#147565=CARTESIAN_POINT('Ctrl Pts',(5.29494014783479,4.59905756132789,54.0013037329013));
#147566=CARTESIAN_POINT('Ctrl Pts',(5.17797568436643,4.7271761522721,54.0091561284534));
#147567=CARTESIAN_POINT('Ctrl Pts',(5.06103883857755,4.85526449182134,54.0170066698958));
#147568=CARTESIAN_POINT('Ctrl Pts',(4.93929074204122,4.97907137395758,54.0248572113383));
#147569=CARTESIAN_POINT('Ctrl Pts',(4.81309732348821,5.09820759847328,54.0327077527807));
#147570=CARTESIAN_POINT('Ctrl Pts',(4.68692420563802,5.21732465757514,54.0405570313086));
#147571=CARTESIAN_POINT('Ctrl Pts',(4.55630746885099,5.33177229508453,54.0484063098365));
#147572=CARTESIAN_POINT('Ctrl Pts',(4.42164925644293,5.44119880315889,54.0562555883643));
#147573=CARTESIAN_POINT('Ctrl Pts',(4.28694567770733,5.55066217700413,54.0641075113127));
#147574=CARTESIAN_POINT('Ctrl Pts',(4.14819820004141,5.6551008016911,54.0719594342611));
#147575=CARTESIAN_POINT('Ctrl Pts',(4.0058414920635,5.75420372449243,54.0798113572095));
#147576=CARTESIAN_POINT('Ctrl Pts',(3.90131521226575,5.82697064910488,54.0855766794532));
#147577=CARTESIAN_POINT('Ctrl Pts',(3.79484377077415,5.89686176940799,54.091342001697));
#147578=CARTESIAN_POINT('Ctrl Pts',(3.68660877623829,5.96376913482261,54.0971073239407));
#147579=CARTESIAN_POINT('Ctrl Pts',(3.50534659890811,6.07581953761967,54.1067625640726));
#147580=CARTESIAN_POINT('Ctrl Pts',(3.31923040315571,6.17944381964446,54.1164178042044));
#147581=CARTESIAN_POINT('Ctrl Pts',(3.12899509086528,6.27431400902449,54.1260730443363));
#147582=CARTESIAN_POINT('Ctrl Pts',(2.93770603920344,6.36970969733803,54.1357817661617));
#147583=CARTESIAN_POINT('Ctrl Pts',(2.74225217857912,6.45625407208534,54.145490487987));
#147584=CARTESIAN_POINT('Ctrl Pts',(2.54339373412106,6.53366473548603,54.1551992098124));
#147585=CARTESIAN_POINT('Ctrl Pts',(2.34357847294275,6.61144786391968,54.1649546456076));
#147586=CARTESIAN_POINT('Ctrl Pts',(2.14032583552511,6.68000918165012,54.1747100814028));
#147587=CARTESIAN_POINT('Ctrl Pts',(1.93441933500118,6.73911332438279,54.184465517198));
#147588=CARTESIAN_POINT('Ctrl Pts',(1.72830896972415,6.79827598518766,54.1942306116951));
#147589=CARTESIAN_POINT('Ctrl Pts',(1.51953952560415,6.84796274221861,54.2039957061922));
#147590=CARTESIAN_POINT('Ctrl Pts',(1.30890841130126,6.88798848237458,54.2137608006893));
#147591=CARTESIAN_POINT('Ctrl Pts',(1.098564428644,6.92795965957256,54.2235125834416));
#147592=CARTESIAN_POINT('Ctrl Pts',(0.886363885309897,6.95829613468245,
54.2332643661938));
#147593=CARTESIAN_POINT('Ctrl Pts',(0.673111867682699,6.97886430417476,
54.2430161489461));
#147594=CARTESIAN_POINT('Ctrl Pts',(0.580109871664257,6.98783435209513,
54.2472690290397));
#147595=CARTESIAN_POINT('Ctrl Pts',(0.486908028073329,6.99494717353388,
54.2515219091334));
#147596=CARTESIAN_POINT('Ctrl Pts',(0.393573741917043,7.00019473101809,
54.255774789227));
#147597=CARTESIAN_POINT('Ctrl Pts',(0.217279127273066,7.01010658830655,
54.2638078485465));
#147598=CARTESIAN_POINT('Ctrl Pts',(0.040425745098178,7.01336470575221,
54.2718409078661));
#147599=CARTESIAN_POINT('Ctrl Pts',(-0.136436700210057,7.00992236685513,
54.2798739671856));
#147600=CARTESIAN_POINT('Ctrl Pts',(-0.313185452402696,7.00648224080902,
54.2879018625849));
#147601=CARTESIAN_POINT('Ctrl Pts',(-0.489942891161812,6.99635023926621,
54.2959297579843));
#147602=CARTESIAN_POINT('Ctrl Pts',(-0.666156623046019,6.97953164016555,
54.3039576533837));
#147603=CARTESIAN_POINT('Ctrl Pts',(-0.842290793328995,6.96272063476749,
54.3119819241381));
#147604=CARTESIAN_POINT('Ctrl Pts',(-1.0178813813776,6.93922907782464,54.3200061948925));
#147605=CARTESIAN_POINT('Ctrl Pts',(-1.19237848016099,6.90911427916408,
54.328030465647));
#147606=CARTESIAN_POINT('Ctrl Pts',(-1.3668544805284,6.87900312167895,54.3360537661881));
#147607=CARTESIAN_POINT('Ctrl Pts',(-1.54023689264898,6.84227037227052,
54.3440770667293));
#147608=CARTESIAN_POINT('Ctrl Pts',(-1.71198322303292,6.79902493057305,
54.3521003672704));
#147609=CARTESIAN_POINT('Ctrl Pts',(-1.88371548052415,6.75578303240666,
54.3601230103824));
#147610=CARTESIAN_POINT('Ctrl Pts',(-2.05381156874999,6.70602959835288,
54.3681456534944));
#147611=CARTESIAN_POINT('Ctrl Pts',(-2.22174173798897,6.64992407567017,
54.3761682966063));
#147612=CARTESIAN_POINT('Ctrl Pts',(-2.38973503612754,6.59379746160213,
54.3841939556185));
#147613=CARTESIAN_POINT('Ctrl Pts',(-2.55556044177969,6.53131410776282,
54.3922196146307));
#147614=CARTESIAN_POINT('Ctrl Pts',(-2.71870548857921,6.46268264955578,
54.4002452736429));
#147615=CARTESIAN_POINT('Ctrl Pts',(-2.81490390688788,6.42221413484906,
54.4049776005998));
#147616=CARTESIAN_POINT('Ctrl Pts',(-2.91017076440804,6.37960892477289,
54.4097099275567));
#147617=CARTESIAN_POINT('Ctrl Pts',(-3.00440463526238,6.33491746987393,
54.4144422545136));
#147618=CARTESIAN_POINT('Ctrl Pts',(-3.17824421839563,6.25247212597776,
54.4231722975224));
#147619=CARTESIAN_POINT('Ctrl Pts',(-3.34865412282789,6.16288344747847,
54.4319023405312));
#147620=CARTESIAN_POINT('Ctrl Pts',(-3.51506571933231,6.06646021591462,
54.4406323835399));
#147621=CARTESIAN_POINT('Ctrl Pts',(-3.68152543207951,5.9700091045412,54.449364950753));
#147622=CARTESIAN_POINT('Ctrl Pts',(-3.84398429229108,5.86671963295671,
54.4580975179661));
#147623=CARTESIAN_POINT('Ctrl Pts',(-4.00190048133327,5.75694529242762,
54.4668300851791));
#147624=CARTESIAN_POINT('Ctrl Pts',(-4.16206028373926,5.64561131967269,
54.4756867213975));
#147625=CARTESIAN_POINT('Ctrl Pts',(-4.31754711202974,5.52760696979519,
54.4845433576159));
#147626=CARTESIAN_POINT('Ctrl Pts',(-4.46782797217122,5.40334523916291,
54.4933999938343));
#147627=CARTESIAN_POINT('Ctrl Pts',(-4.6160979330381,5.28074624737677,54.5021381199289));
#147628=CARTESIAN_POINT('Ctrl Pts',(-4.7593001826618,5.15205648890996,54.5108762460234));
#147629=CARTESIAN_POINT('Ctrl Pts',(-4.89695704387536,5.0177124541906,54.519614372118));
#147630=CARTESIAN_POINT('Ctrl Pts',(-5.03741434505067,4.88063537441898,
54.5285302633983));
#147631=CARTESIAN_POINT('Ctrl Pts',(-5.17209799958015,4.73767170116489,
54.5374461546786));
#147632=CARTESIAN_POINT('Ctrl Pts',(-5.30054026203266,4.58932451381145,
54.546362045959));
#147633=CARTESIAN_POINT('Ctrl Pts',(-5.42898252448522,4.44097732645797,
54.5552779372393));
#147634=CARTESIAN_POINT('Ctrl Pts',(-5.55118320150893,4.28724685761481,
54.5641938285196));
#147635=CARTESIAN_POINT('Ctrl Pts',(-5.66671764406679,4.12867263232654,
54.5731097197999));
#147636=CARTESIAN_POINT('Ctrl Pts',(-5.7799817066632,3.97321456647546,54.581850403926));
#147637=CARTESIAN_POINT('Ctrl Pts',(-5.88685113118549,3.81308483500101,
54.590591088052));
#147638=CARTESIAN_POINT('Ctrl Pts',(-5.98696423013525,3.64881979132719,
54.599331772178));
#147639=CARTESIAN_POINT('Ctrl Pts',(-6.0870593168541,3.48458430202668,54.6080708836905));
#147640=CARTESIAN_POINT('Ctrl Pts',(-6.18040036318854,3.31621522010431,
54.6168099952029));
#147641=CARTESIAN_POINT('Ctrl Pts',(-6.26667004960582,3.14427623657232,
54.6255491067154));
#147642=CARTESIAN_POINT('Ctrl Pts',(-6.35405748974329,2.97010952454761,
54.6344014465796));
#147643=CARTESIAN_POINT('Ctrl Pts',(-6.43418890444417,2.7922800038065,54.6432537864439));
#147644=CARTESIAN_POINT('Ctrl Pts',(-6.50678286093266,2.61139873691724,
54.6521061263081));
#147645=CARTESIAN_POINT('Ctrl Pts',(-6.57841155134463,2.43292260895761,
54.6608407585314));
#147646=CARTESIAN_POINT('Ctrl Pts',(-6.6427018948626,2.25147565357265,54.6695753907547));
#147647=CARTESIAN_POINT('Ctrl Pts',(-6.69943181608028,2.06766532693067,
54.6783100229779));
#147648=CARTESIAN_POINT('Ctrl Pts',(-6.75730847336472,1.88013946664295,
54.6872212166627));
#147649=CARTESIAN_POINT('Ctrl Pts',(-6.807315694583,1.69015394239007,54.6961324103474));
#147650=CARTESIAN_POINT('Ctrl Pts',(-6.84927073344378,1.49837144343133,
54.7050436040322));
#147651=CARTESIAN_POINT('Ctrl Pts',(-6.89122577230458,1.30658894447253,
54.7139547977169));
#147652=CARTESIAN_POINT('Ctrl Pts',(-6.92512855086331,1.1130097640552,54.7228659914017));
#147653=CARTESIAN_POINT('Ctrl Pts',(-6.95085125227764,0.918310095343839,
54.7317771850864));
#147654=CARTESIAN_POINT('Ctrl Pts',(-6.97401782472743,0.742958218085718,
54.7398028512397));
#147655=CARTESIAN_POINT('Ctrl Pts',(-6.99055942297077,0.566616825996988,
54.747828517393));
#147656=CARTESIAN_POINT('Ctrl Pts',(-7.00040399381127,0.389833920960158,
54.7558541835463));
#147657=CARTESIAN_POINT('Ctrl Pts',(-7.01024544024081,0.213107122223639,
54.7638773025617));
#147658=CARTESIAN_POINT('Ctrl Pts',(-7.01339407050618,0.0359394550822815,
54.7719004215771));
#147659=CARTESIAN_POINT('Ctrl Pts',(-7.00982972206353,-0.141116371037569,
54.7799235405925));
#147660=CARTESIAN_POINT('Ctrl Pts',(-7.00626582311167,-0.318149869103393,
54.787945647833));
#147661=CARTESIAN_POINT('Ctrl Pts',(-6.99599063966237,-0.495071187861098,
54.7959677550735));
#147662=CARTESIAN_POINT('Ctrl Pts',(-6.97903612023533,-0.671328082945003,
54.8039898623141));
#147663=CARTESIAN_POINT('Ctrl Pts',(-6.9620753004268,-0.847650475944406,
54.8120149506085));
#147664=CARTESIAN_POINT('Ctrl Pts',(-6.93843021838755,-1.0233075865209,
54.8200400389029));
#147665=CARTESIAN_POINT('Ctrl Pts',(-6.90818470985104,-1.19775230205596,
54.8280651271973));
#147666=CARTESIAN_POINT('Ctrl Pts',(-6.87793324458435,-1.3722313737699,
54.8360917960003));
#147667=CARTESIAN_POINT('Ctrl Pts',(-6.8410788344518,-1.5454972150915,54.8441184648033));
#147668=CARTESIAN_POINT('Ctrl Pts',(-6.79775631958861,-1.71701356488324,
54.8521451336063));
#147669=CARTESIAN_POINT('Ctrl Pts',(-6.75439902553422,-1.88866760751076,
54.8601782461961));
#147670=CARTESIAN_POINT('Ctrl Pts',(-6.70456335463898,-2.05856900043394,
54.8682113587859));
#147671=CARTESIAN_POINT('Ctrl Pts',(-6.64843401704203,-2.2261966857262,
54.8762444713757));
#147672=CARTESIAN_POINT('Ctrl Pts',(-6.61536063351217,-2.32496882456212,
54.8809778643747));
#147673=CARTESIAN_POINT('Ctrl Pts',(-6.58010302925627,-2.42295187452145,
54.8857112573737));
#147674=CARTESIAN_POINT('Ctrl Pts',(-6.54270675095957,-2.52004264516458,
54.8904446503727));
#147675=CARTESIAN_POINT('Ctrl Pts',(-6.46566914564606,-2.72005293520058,
54.9001956009555));
#147676=CARTESIAN_POINT('Ctrl Pts',(-6.37950825511883,-2.91639359711574,
54.9099465515383));
#147677=CARTESIAN_POINT('Ctrl Pts',(-6.28457812809835,-3.10832821856507,
54.9196975021211));
#147678=CARTESIAN_POINT('Ctrl Pts',(-6.1895112379634,-3.30053935472502,
54.9294625006191));
#147679=CARTESIAN_POINT('Ctrl Pts',(-6.08564985756998,-3.48833171860857,
54.939227499117));
#147680=CARTESIAN_POINT('Ctrl Pts',(-5.9733949394707,-3.67099161802446,
54.948992497615));
#147681=CARTESIAN_POINT('Ctrl Pts',(-5.86132712748513,-3.85334706054448,
54.9587412198468));
#147682=CARTESIAN_POINT('Ctrl Pts',(-5.74089375861056,-4.03058710381781,
54.9684899420787));
#147683=CARTESIAN_POINT('Ctrl Pts',(-5.61253852683564,-4.2020278256201,
54.9782386643105));
#147684=CARTESIAN_POINT('Ctrl Pts',(-5.48453557941323,-4.37299801043815,
54.987960630155));
#147685=CARTESIAN_POINT('Ctrl Pts',(-5.34865419813391,-4.53820061719486,
54.9976825959995));
#147686=CARTESIAN_POINT('Ctrl Pts',(-5.20537875608043,-4.69698398637323,
55.007404561844));
#147687=CARTESIAN_POINT('Ctrl Pts',(-5.06305132705065,-4.85471673096605,
55.0170622001939));
#147688=CARTESIAN_POINT('Ctrl Pts',(-4.91342737247014,-5.00611485176101,
55.0267198385437));
#147689=CARTESIAN_POINT('Ctrl Pts',(-4.75702536968583,-5.15056658967394,
55.0363774768935));
#147690=CARTESIAN_POINT('Ctrl Pts',(-4.68828106127532,-5.21405832663855,
55.0406223564821));
#147691=CARTESIAN_POINT('Ctrl Pts',(-4.61822785765543,-5.27620843656793,
55.0448672360707));
#147692=CARTESIAN_POINT('Ctrl Pts',(-4.54691247897004,-5.33696669195963,
55.0491121156593));
#147693=CARTESIAN_POINT('Ctrl Pts',(-4.41499884814111,-5.44935257869675,
55.0569639631751));
#147694=CARTESIAN_POINT('Ctrl Pts',(-4.27881843737147,-5.55692722135325,
55.0648158106908));
#147695=CARTESIAN_POINT('Ctrl Pts',(-4.13877603120052,-5.65934267614712,
55.0726676582066));
#147696=CARTESIAN_POINT('Ctrl Pts',(-3.99877333985031,-5.76172908679973,
55.080517279006));
#147697=CARTESIAN_POINT('Ctrl Pts',(-3.85491113930223,-5.85895899499041,
55.0883668998054));
#147698=CARTESIAN_POINT('Ctrl Pts',(-3.70762649059494,-5.95072536492306,
55.0962165206048));
#147699=CARTESIAN_POINT('Ctrl Pts',(-3.5603536006087,-6.0424844085311,55.1040655147163));
#147700=CARTESIAN_POINT('Ctrl Pts',(-3.40965913056299,-6.12878058113111,
55.1119145088278));
#147701=CARTESIAN_POINT('Ctrl Pts',(-3.25600802220571,-6.20935087765477,
55.1197635029393));
#147702=CARTESIAN_POINT('Ctrl Pts',(-3.10227912470417,-6.28996196460608,
55.1276164707712));
#147703=CARTESIAN_POINT('Ctrl Pts',(-2.94559093636288,-6.36484120605821,
55.1354694386031));
#147704=CARTESIAN_POINT('Ctrl Pts',(-2.78643214072944,-6.433772026394,55.143322406435));
#147705=CARTESIAN_POINT('Ctrl Pts',(-2.62723292404789,-6.50272035286883,
55.1511773686599));
#147706=CARTESIAN_POINT('Ctrl Pts',(-2.46556220551837,-6.56571711004186,
55.1590323308847));
#147707=CARTESIAN_POINT('Ctrl Pts',(-2.30192680489228,-6.62259462351565,
55.1668872931096));
#147708=CARTESIAN_POINT('Ctrl Pts',(-2.13812898240354,-6.67952859269308,
55.1747500520435));
#147709=CARTESIAN_POINT('Ctrl Pts',(-1.97236294751005,-6.73033107539278,
55.1826128109774));
#147710=CARTESIAN_POINT('Ctrl Pts',(-1.80514932766534,-6.77488468295434,
55.1904755699112));
#147711=CARTESIAN_POINT('Ctrl Pts',(-1.68248388892909,-6.80756855059561,
55.1962435735893));
#147712=CARTESIAN_POINT('Ctrl Pts',(-1.55903971638853,-6.83689065907245,
55.2020115772675));
#147713=CARTESIAN_POINT('Ctrl Pts',(-1.43502477046539,-6.86282234001805,
55.2077795809456));
#147714=CARTESIAN_POINT('Ctrl Pts',(-1.25489218013704,-6.90048829088814,
55.2161576472814));
#147715=CARTESIAN_POINT('Ctrl Pts',(-1.07315613852357,-6.93108293641786,
55.2245357136171));
#147716=CARTESIAN_POINT('Ctrl Pts',(-0.890397569983565,-6.95448191671151,
55.2329137799528));
#147717=CARTESIAN_POINT('Ctrl Pts',(-0.707763969636188,-6.97786489705342,
55.2412861174638));
#147718=CARTESIAN_POINT('Ctrl Pts',(-0.524109561367762,-6.99406198019323,
55.2496584549748));
#147719=CARTESIAN_POINT('Ctrl Pts',(-0.340024355208382,-7.00300007142404,
55.2580307924858));
#147720=CARTESIAN_POINT('Ctrl Pts',(-0.156038028158063,-7.01193336166885,
55.2663986328985));
#147721=CARTESIAN_POINT('Ctrl Pts',(0.0283783077945347,-7.01361541849126,
55.2747664733111));
#147722=CARTESIAN_POINT('Ctrl Pts',(0.212630178955949,-7.0080250405872,
55.2831343137238));
#147723=CARTESIAN_POINT('Ctrl Pts',(0.396810073053705,-7.00243684653605,
55.2914988852818));
#147724=CARTESIAN_POINT('Ctrl Pts',(0.580825302401443,-6.98958189295206,
55.2998634568399));
#147725=CARTESIAN_POINT('Ctrl Pts',(0.764081589738954,-6.96949107802873,
55.3082280283979));
#147726=CARTESIAN_POINT('Ctrl Pts',(0.947293113236532,-6.94940517066975,
55.31659055675));
#147727=CARTESIAN_POINT('Ctrl Pts',(1.12974573803573,-6.92208696300415,
55.324953085102));
#147728=CARTESIAN_POINT('Ctrl Pts',(1.31085004288317,-6.88761923508938,
55.3333156134541));
#147729=CARTESIAN_POINT('Ctrl Pts',(1.49196880038271,-6.85314875654932,
55.3416788091603));
#147730=CARTESIAN_POINT('Ctrl Pts',(1.67173869895743,-6.8115276733912,55.3500420048665));
#147731=CARTESIAN_POINT('Ctrl Pts',(1.84957948553568,-6.76289008406802,
55.3584052005727));
#147732=CARTESIAN_POINT('Ctrl Pts',(2.02743240047959,-6.71424917776409,
55.3667689666312));
#147733=CARTESIAN_POINT('Ctrl Pts',(2.20335562386006,-6.65859089766998,
55.3751327326897));
#147734=CARTESIAN_POINT('Ctrl Pts',(2.37678289939389,-6.59609957563171,
55.3834964987482));
#147735=CARTESIAN_POINT('Ctrl Pts',(2.55024512424107,-6.53359566025258,
55.3918619502848));
#147736=CARTESIAN_POINT('Ctrl Pts',(2.72121008895998,-6.46425606861821,
55.4002274018214));
#147737=CARTESIAN_POINT('Ctrl Pts',(2.88912999007159,-6.3883138982809,55.408592853358));
#147738=CARTESIAN_POINT('Ctrl Pts',(3.05710612721923,-6.312346295064,55.4169611064675));
#147739=CARTESIAN_POINT('Ctrl Pts',(3.22203486782568,-6.22977183939668,
55.425329359577));
#147740=CARTESIAN_POINT('Ctrl Pts',(3.38339116340422,-6.14087052443693,
55.4336976126864));
#147741=CARTESIAN_POINT('Ctrl Pts',(3.5448970592932,-6.05188678527259,55.4420736243606));
#147742=CARTESIAN_POINT('Ctrl Pts',(3.70282360319209,-5.95656462381894,
55.4504496360348));
#147743=CARTESIAN_POINT('Ctrl Pts',(3.85667193453369,-5.85522912889668,
55.458825647709));
#147744=CARTESIAN_POINT('Ctrl Pts',(4.01059571499958,-5.75384393779452,
55.4672057670829));
#147745=CARTESIAN_POINT('Ctrl Pts',(4.16043702371027,-5.64643971852223,
55.4755858864567));
#147746=CARTESIAN_POINT('Ctrl Pts',(4.30572796616131,-5.53338352582905,
55.4839660058306));
#147747=CARTESIAN_POINT('Ctrl Pts',(4.4511849219402,-5.42019815209771,55.4923557005537));
#147748=CARTESIAN_POINT('Ctrl Pts',(4.59208086652548,-5.30134810742315,
55.5007453952768));
#147749=CARTESIAN_POINT('Ctrl Pts',(4.72798181539348,-5.17724004811527,
55.5091350899998));
#147750=CARTESIAN_POINT('Ctrl Pts',(4.81426300592747,-5.09844596167848,
55.5144615638394));
#147751=CARTESIAN_POINT('Ctrl Pts',(4.8985315577186,-5.01753325389086,55.519788037679));
#147752=CARTESIAN_POINT('Ctrl Pts',(4.98068446859895,-4.9346133371073,55.5251145115186));
#147753=CARTESIAN_POINT('Ctrl Pts',(5.10995352083697,-4.80413738757123,
55.533495811921));
#147754=CARTESIAN_POINT('Ctrl Pts',(5.23424319083462,-4.66842675091216,
55.5418771123234));
#147755=CARTESIAN_POINT('Ctrl Pts',(5.35311923683061,-4.52788482613837,
55.5502584127257));
#147756=CARTESIAN_POINT('Ctrl Pts',(5.47184462483593,-4.38752101768579,
55.5586290910564));
#147757=CARTESIAN_POINT('Ctrl Pts',(5.58516985216965,-4.24233837165848,
55.5669997693871));
#147758=CARTESIAN_POINT('Ctrl Pts',(5.69269703844291,-4.09277741772055,
55.5753704477178));
#147759=CARTESIAN_POINT('Ctrl Pts',(5.80010219981773,-3.9433861897919,55.5837316267655));
#147760=CARTESIAN_POINT('Ctrl Pts',(5.90172224425848,-3.78962682138928,
55.5920928058132));
#147761=CARTESIAN_POINT('Ctrl Pts',(5.99719888257382,-3.63197358544295,
55.6004539848609));
#147762=CARTESIAN_POINT('Ctrl Pts',(6.09255162868244,-3.47452492317708,
55.608804314292));
#147763=CARTESIAN_POINT('Ctrl Pts',(6.18177670032624,-3.31319275055744,
55.6171546437231));
#147764=CARTESIAN_POINT('Ctrl Pts',(6.26455857907563,-3.14848096259607,
55.6255049731542));
#147765=CARTESIAN_POINT('Ctrl Pts',(6.34727676211866,-2.98389591050782,
55.633848877506));
#147766=CARTESIAN_POINT('Ctrl Pts',(6.42356148545388,-2.81593671673851,
55.6421927818578));
#147767=CARTESIAN_POINT('Ctrl Pts',(6.49314215248363,-2.64513355998147,
55.6505366862096));
#147768=CARTESIAN_POINT('Ctrl Pts',(6.56266693188494,-2.47446759339189,
55.6588738886851));
#147769=CARTESIAN_POINT('Ctrl Pts',(6.6254982708226,-2.30096252206304,55.6672110911606));
#147770=CARTESIAN_POINT('Ctrl Pts',(6.68141282022042,-2.12517041394196,
55.675548293636));
#147771=CARTESIAN_POINT('Ctrl Pts',(6.69981958138623,-2.06730062184191,
55.6782928546923));
#147772=CARTESIAN_POINT('Ctrl Pts',(6.71747716175574,-2.00918315349665,
55.6810374157486));
#147773=CARTESIAN_POINT('Ctrl Pts',(6.73437873898325,-1.95083816920585,
55.6837819768049));
#147774=CARTESIAN_POINT('Ctrl Pts',(6.78297200599455,-1.78309208478724,
55.6916727899783));
#147775=CARTESIAN_POINT('Ctrl Pts',(6.82529219203744,-1.61353383431378,
55.6995636031516));
#147776=CARTESIAN_POINT('Ctrl Pts',(6.86121524485502,-1.44268913015557,
55.7074544163249));
#147777=CARTESIAN_POINT('Ctrl Pts',(6.89714304061904,-1.27182186924851,
55.715346271328));
#147778=CARTESIAN_POINT('Ctrl Pts',(6.92667195235105,-1.09966818756756,
55.723238126331));
#147779=CARTESIAN_POINT('Ctrl Pts',(6.94972928813047,-0.926762852191188,
55.7311299813341));
#147780=CARTESIAN_POINT('Ctrl Pts',(6.97280535063941,-0.753717086390481,
55.7390282459517));
#147781=CARTESIAN_POINT('Ctrl Pts',(6.98939929757199,-0.579918822786608,
55.7469265105693));
#147782=CARTESIAN_POINT('Ctrl Pts',(6.99949039413753,-0.405907359968376,
55.7548247751868));
#147783=CARTESIAN_POINT('Ctrl Pts',(7.00745839743096,-0.268506642432263,
55.7610613024142));
#147784=CARTESIAN_POINT('Ctrl Pts',(7.0113730362753,-0.13097312713087,55.7672978296416));
#147785=CARTESIAN_POINT('Ctrl Pts',(7.01124705281182,0.00642860308711848,
55.773534356869));
#147786=CARTESIAN_POINT('Ctrl Pts',(7.01124705281098,0.00642860400140193,
55.7735343569105));
#147787=CARTESIAN_POINT('Ctrl Pts',(7.01105339139811,0.217642113168657,
55.7831211270235));
#147788=CARTESIAN_POINT('Ctrl Pts',(7.00131167594713,0.428520891988302,
55.7927078971364));
#147789=CARTESIAN_POINT('Ctrl Pts',(6.98213567539767,0.638285181434724,
55.8022946672493));
#147790=CARTESIAN_POINT('Ctrl Pts',(6.9628194060205,0.84958385709994,55.8119515627777));
#147791=CARTESIAN_POINT('Ctrl Pts',(6.93393038498918,1.0597516130558,55.8216084583061));
#147792=CARTESIAN_POINT('Ctrl Pts',(6.89563491151376,1.2680085684303,55.8312653538345));
#147793=CARTESIAN_POINT('Ctrl Pts',(6.88085100385837,1.34840584041663,55.8349933832535));
#147794=CARTESIAN_POINT('Ctrl Pts',(6.86466574189174,1.42851852440994,55.8387214126724));
#147795=CARTESIAN_POINT('Ctrl Pts',(6.84709064213326,1.50830245670791,55.8424494420914));
#147796=CARTESIAN_POINT('Ctrl Pts',(6.80754063442373,1.68784369293669,55.8508387880574));
#147797=CARTESIAN_POINT('Ctrl Pts',(6.76089090729276,1.86598150139765,55.8592281340235));
#147798=CARTESIAN_POINT('Ctrl Pts',(6.70725831382453,2.04213429385331,55.8676174799895));
#147799=CARTESIAN_POINT('Ctrl Pts',(6.6659849047502,2.1776941426776,55.8740735710627));
#147800=CARTESIAN_POINT('Ctrl Pts',(6.62057715257561,2.31207849286783,55.8805296621359));
#147801=CARTESIAN_POINT('Ctrl Pts',(6.57110895151812,2.44502632087642,55.886985753209));
#147802=CARTESIAN_POINT('',(7.01124999682065,-0.000211145429389691,55.2264656430482));
#147803=CARTESIAN_POINT('Ctrl Pts',(6.57110895151813,2.44502632087638,55.3399173263397));
#147804=CARTESIAN_POINT('Ctrl Pts',(6.63816763466189,2.26480334768358,55.331187878767));
#147805=CARTESIAN_POINT('Ctrl Pts',(6.69779687952727,2.08184970904798,55.3224584311943));
#147806=CARTESIAN_POINT('Ctrl Pts',(6.74980327540723,1.89678209233477,55.3137289836216));
#147807=CARTESIAN_POINT('Ctrl Pts',(6.80183255142163,1.71163305540624,55.3049956955417));
#147808=CARTESIAN_POINT('Ctrl Pts',(6.84623220132626,1.52436844594368,55.2962624074619));
#147809=CARTESIAN_POINT('Ctrl Pts',(6.88285906775861,1.33561881383617,55.287529119382));
#147810=CARTESIAN_POINT('Ctrl Pts',(6.91949072354235,1.14684450071162,55.2787946893321));
#147811=CARTESIAN_POINT('Ctrl Pts',(6.94834751786577,0.956585047407869,
55.2700602592821));
#147812=CARTESIAN_POINT('Ctrl Pts',(6.96933759544937,0.765480269605941,
55.2613258292322));
#147813=CARTESIAN_POINT('Ctrl Pts',(6.99033260036295,0.574330630783553,
55.2525893488126));
#147814=CARTESIAN_POINT('Ctrl Pts',(7.00345716960281,0.382335543913326,
55.243852868393));
#147815=CARTESIAN_POINT('Ctrl Pts',(7.00867129074538,0.190140213477998,
55.2351163879733));
#147816=CARTESIAN_POINT('Ctrl Pts',(7.01039227485,0.126703806916737,55.2322328063454));
#147817=CARTESIAN_POINT('Ctrl Pts',(7.01125190782734,0.0632456077901646,
55.2293492247175));
#147818=CARTESIAN_POINT('Ctrl Pts',(7.01124999682068,-0.000211144518860344,
55.2264656430896));
#147819=CARTESIAN_POINT('Ctrl Pts',(7.01124999682065,-0.000211145429297141,
55.2264656430482));
#147820=CARTESIAN_POINT('Ctrl Pts',(7.0112477462756,-0.0749422636437259,
55.2230697352579));
#147821=CARTESIAN_POINT('Ctrl Pts',(7.01005060799595,-0.149671035804848,
55.2196738274676));
#147822=CARTESIAN_POINT('Ctrl Pts',(7.00765927269795,-0.224361494625235,
55.2162779196773));
#147823=CARTESIAN_POINT('Ctrl Pts',(7.00150424893689,-0.41660619955968,
55.2075372411295));
#147824=CARTESIAN_POINT('Ctrl Pts',(6.98743363633494,-0.608607698602225,
55.1987965625817));
#147825=CARTESIAN_POINT('Ctrl Pts',(6.96549162193804,-0.79972059321427,
55.1900558840339));
#147826=CARTESIAN_POINT('Ctrl Pts',(6.94355355540339,-0.990799102315082,
55.1813167781309));
#147827=CARTESIAN_POINT('Ctrl Pts',(6.91374694663639,-1.18098905436653,
55.1725776722279));
#147828=CARTESIAN_POINT('Ctrl Pts',(6.87616778480095,-1.36965074298726,
55.1638385663249));
#147829=CARTESIAN_POINT('Ctrl Pts',(6.83810169186425,-1.56075701097914,
55.1549862236637));
#147830=CARTESIAN_POINT('Ctrl Pts',(6.7920602499044,-1.75029485064277,55.1461338810025));
#147831=CARTESIAN_POINT('Ctrl Pts',(6.73819686859386,-1.93760922855254,
55.1372815383414));
#147832=CARTESIAN_POINT('Ctrl Pts',(6.6850497474794,-2.12243275219755,55.1285469116597));
#147833=CARTESIAN_POINT('Ctrl Pts',(6.62428751394606,-2.30509131460187,
55.119812284978));
#147834=CARTESIAN_POINT('Ctrl Pts',(6.55610819284299,-2.48496920025924,
55.1110776582963));
#147835=CARTESIAN_POINT('Ctrl Pts',(6.48655059951523,-2.66848338926529,
55.1021664576454));
#147836=CARTESIAN_POINT('Ctrl Pts',(6.40927292840654,-2.84910299986734,
55.0932552569945));
#147837=CARTESIAN_POINT('Ctrl Pts',(6.32453817181363,-3.02619290128245,
55.0843440563435));
#147838=CARTESIAN_POINT('Ctrl Pts',(6.23980341522072,-3.20328280269756,
55.0754328556926));
#147839=CARTESIAN_POINT('Ctrl Pts',(6.14761169182779,-3.37684271566718,
55.0665216550417));
#147840=CARTESIAN_POINT('Ctrl Pts',(6.04827762928387,-3.54626060542712,
55.0576104543908));
#147841=CARTESIAN_POINT('Ctrl Pts',(5.95881457135179,-3.69884313450292,
55.0495847757901));
#147842=CARTESIAN_POINT('Ctrl Pts',(5.86351657780664,-3.84813579674568,
55.0415590971894));
#147843=CARTESIAN_POINT('Ctrl Pts',(5.76266350826657,-3.99366196028068,
55.0335334185887));
#147844=CARTESIAN_POINT('Ctrl Pts',(5.66184244664213,-4.1391419379218,55.0255102871117));
#147845=CARTESIAN_POINT('Ctrl Pts',(5.55547002759096,-4.28085749581419,
55.0174871556348));
#147846=CARTESIAN_POINT('Ctrl Pts',(5.44386994354426,-4.41836017095432,
55.0094640241578));
#147847=CARTESIAN_POINT('Ctrl Pts',(5.33228393297764,-4.55584550613296,
55.0014419044487));
#147848=CARTESIAN_POINT('Ctrl Pts',(5.21547180194833,-4.6891187326226,54.9934197847396));
#147849=CARTESIAN_POINT('Ctrl Pts',(5.09379807142342,-4.81776377275423,
54.9853976650305));
#147850=CARTESIAN_POINT('Ctrl Pts',(4.9720791267729,-4.94645661755971,54.9773725642907));
#147851=CARTESIAN_POINT('Ctrl Pts',(4.84549522359992,-5.07051757167975,
54.9693474635509));
#147852=CARTESIAN_POINT('Ctrl Pts',(4.7144486674688,-5.18956648712604,54.9613223628111));
#147853=CARTESIAN_POINT('Ctrl Pts',(4.58337630236738,-5.3086388486667,54.9532956815675));
#147854=CARTESIAN_POINT('Ctrl Pts',(4.44783981064288,-5.42269696511521,
54.9452690003238));
#147855=CARTESIAN_POINT('Ctrl Pts',(4.30827507160288,-5.53140058845002,
54.9372423190802));
#147856=CARTESIAN_POINT('Ctrl Pts',(4.16859829159107,-5.6401914778069,54.9292091941089));
#147857=CARTESIAN_POINT('Ctrl Pts',(4.02488710034641,-5.74361907094462,
54.9211760691376));
#147858=CARTESIAN_POINT('Ctrl Pts',(3.87760738209954,-5.84138575620436,
54.9131429441663));
#147859=CARTESIAN_POINT('Ctrl Pts',(3.79082648474781,-5.89899233488972,
54.9084096258123));
#147860=CARTESIAN_POINT('Ctrl Pts',(3.70280716923416,-5.95463436232717,
54.9036763074583));
#147861=CARTESIAN_POINT('Ctrl Pts',(3.61364876866986,-6.00825841148588,
54.8989429891043));
#147862=CARTESIAN_POINT('Ctrl Pts',(3.42997789160466,-6.11872670250984,
54.889192110578));
#147863=CARTESIAN_POINT('Ctrl Pts',(3.24136375540439,-6.2206942963535,54.8794412320516));
#147864=CARTESIAN_POINT('Ctrl Pts',(3.04853815308218,-6.31379772337555,
54.8696903535253));
#147865=CARTESIAN_POINT('Ctrl Pts',(2.85543479600782,-6.40703526080092,
54.8599254293908));
#147866=CARTESIAN_POINT('Ctrl Pts',(2.65810787306583,-6.49138307414728,
54.8501605052563));
#147867=CARTESIAN_POINT('Ctrl Pts',(2.45731222308588,-6.56652443845089,
54.8403955811218));
#147868=CARTESIAN_POINT('Ctrl Pts',(2.25685122170069,-6.64154057119707,
54.8306469313346));
#147869=CARTESIAN_POINT('Ctrl Pts',(2.05293308272549,-6.70738090720442,
54.8208982815474));
#147870=CARTESIAN_POINT('Ctrl Pts',(1.84632807593882,-6.76377847053702,
54.8111496317601));
#147871=CARTESIAN_POINT('Ctrl Pts',(1.64029004573899,-6.82002126463889,
54.8014277347427));
#147872=CARTESIAN_POINT('Ctrl Pts',(1.43157990615793,-6.86687300734899,
54.7917058377253));
#147873=CARTESIAN_POINT('Ctrl Pts',(1.22098019931334,-6.904117171325,54.7819839407078));
#147874=CARTESIAN_POINT('Ctrl Pts',(1.01177380921548,-6.94111492984223,
54.7723263632573));
#147875=CARTESIAN_POINT('Ctrl Pts',(0.800702812731656,-6.96863177940732,
54.7626687858067));
#147876=CARTESIAN_POINT('Ctrl Pts',(0.588552144967729,-6.98650362736282,
54.7530112083561));
#147877=CARTESIAN_POINT('Ctrl Pts',(0.49529604656456,-6.99435964228444,
54.7487659801767));
#147878=CARTESIAN_POINT('Ctrl Pts',(0.401831556430714,-7.00035262339382,
54.7445207519973));
#147879=CARTESIAN_POINT('Ctrl Pts',(0.308226413662711,-7.0044716460573,
54.7402755238179));
#147880=CARTESIAN_POINT('Ctrl Pts',(0.135096336517516,-7.0120901025908,
54.7324236402519));
#147881=CARTESIAN_POINT('Ctrl Pts',(-0.0384439618467919,-7.01329093163461,
54.7245717566859));
#147882=CARTESIAN_POINT('Ctrl Pts',(-0.211861327003002,-7.00804832607628,
54.7167198731199));
#147883=CARTESIAN_POINT('Ctrl Pts',(-0.385229514743517,-7.00280720720754,
54.7088702161783));
#147884=CARTESIAN_POINT('Ctrl Pts',(-0.558474457710154,-6.99112629990335,
54.7010205592367));
#147885=CARTESIAN_POINT('Ctrl Pts',(-0.731062671239445,-6.97303190392961,
54.6931709022951));
#147886=CARTESIAN_POINT('Ctrl Pts',(-0.903637107778184,-6.95493895235534,
54.6853218719585));
#147887=CARTESIAN_POINT('Ctrl Pts',(-1.07555453993769,-6.93043357180747,
54.677472841622));
#147888=CARTESIAN_POINT('Ctrl Pts',(-1.24628653963422,-6.89959393179241,
54.6696238112855));
#147889=CARTESIAN_POINT('Ctrl Pts',(-1.41710497670054,-6.86873867843378,
54.6617708071799));
#147890=CARTESIAN_POINT('Ctrl Pts',(-1.58673640628852,-6.83154282599992,
54.6539178030743));
#147891=CARTESIAN_POINT('Ctrl Pts',(-1.75466219618514,-6.7881357632106,
54.6460647989688));
#147892=CARTESIAN_POINT('Ctrl Pts',(-1.922630634798,-6.74471767617357,54.6382098004075));
#147893=CARTESIAN_POINT('Ctrl Pts',(-2.08889220514317,-6.69508534519298,
54.6303548018463));
#147894=CARTESIAN_POINT('Ctrl Pts',(-2.25294401222274,-6.63941788414389,
54.622499803285));
#147895=CARTESIAN_POINT('Ctrl Pts',(-2.4171586526295,-6.58369516909875,
54.6146370080675));
#147896=CARTESIAN_POINT('Ctrl Pts',(-2.57915879281569,-6.52192549566605,
54.60677421285));
#147897=CARTESIAN_POINT('Ctrl Pts',(-2.73846154073518,-6.4543361356854,
54.5989114176325));
#147898=CARTESIAN_POINT('Ctrl Pts',(-2.85531873874926,-6.40475567755736,
54.5931436312654));
#147899=CARTESIAN_POINT('Ctrl Pts',(-2.97072489308552,-6.35204464108381,
54.5873758448984));
#147900=CARTESIAN_POINT('Ctrl Pts',(-3.08449833512118,-6.29630817091529,
54.5816080585314));
#147901=CARTESIAN_POINT('Ctrl Pts',(-3.24976105988727,-6.21534761664107,
54.5732300040942));
#147902=CARTESIAN_POINT('Ctrl Pts',(-3.41194408556617,-6.12782279722444,
54.564851949657));
#147903=CARTESIAN_POINT('Ctrl Pts',(-3.57051266870268,-6.03399252942309,
54.5564738952198));
#147904=CARTESIAN_POINT('Ctrl Pts',(-3.72897282251262,-5.94022642283544,
54.5481015697031));
#147905=CARTESIAN_POINT('Ctrl Pts',(-3.88382317933206,-5.84016363092992,
54.5397292441864));
#147906=CARTESIAN_POINT('Ctrl Pts',(-4.03455332592352,-5.73410899990395,
54.5313569186696));
#147907=CARTESIAN_POINT('Ctrl Pts',(-4.18520250831488,-5.62811133577254,
54.5229890903199));
#147908=CARTESIAN_POINT('Ctrl Pts',(-4.33173562505888,-5.51612843863671,
54.5146212619701));
#147909=CARTESIAN_POINT('Ctrl Pts',(-4.47367062579133,-5.39850883989568,
54.5062534336204));
#147910=CARTESIAN_POINT('Ctrl Pts',(-4.61555017954625,-5.28093518930849,
54.4978888741669));
#147911=CARTESIAN_POINT('Ctrl Pts',(-4.75283494655109,-5.15772943761216,
54.4895243147134));
#147912=CARTESIAN_POINT('Ctrl Pts',(-4.88507504265928,-5.02928110072279,
54.4811597552599));
#147913=CARTESIAN_POINT('Ctrl Pts',(-5.017282836326,-4.90086414005748,54.472797239027));
#147914=CARTESIAN_POINT('Ctrl Pts',(-5.14444818127107,-4.76720737716857,
54.4644347227941));
#147915=CARTESIAN_POINT('Ctrl Pts',(-5.26615690214589,-4.62873827781192,
54.4560722065612));
#147916=CARTESIAN_POINT('Ctrl Pts',(-5.38787533644869,-4.49025812740145,
54.4477090229259));
#147917=CARTESIAN_POINT('Ctrl Pts',(-5.50413605511812,-4.34696511608873,
54.4393458392906));
#147918=CARTESIAN_POINT('Ctrl Pts',(-5.61456364759881,-4.19932156539149,
54.4309826556552));
#147919=CARTESIAN_POINT('Ctrl Pts',(-5.724998771629,-4.05166794488572,54.4226189016214));
#147920=CARTESIAN_POINT('Ctrl Pts',(-5.82959977905141,-3.8996634565157,
54.4142551475876));
#147921=CARTESIAN_POINT('Ctrl Pts',(-5.92803316711366,-3.74380145468485,
54.4058913935538));
#147922=CARTESIAN_POINT('Ctrl Pts',(-6.02648639246817,-3.58790804196648,
54.3975259539716));
#147923=CARTESIAN_POINT('Ctrl Pts',(-6.11876934441629,-3.42815584362014,
54.3891605143895));
#147924=CARTESIAN_POINT('Ctrl Pts',(-6.2045930419162,-3.26506535106191,
54.3807950748073));
#147925=CARTESIAN_POINT('Ctrl Pts',(-6.2904454826061,-3.10192023791346,
54.3724268335582));
#147926=CARTESIAN_POINT('Ctrl Pts',(-6.36983420218175,-2.93543489201752,
54.364058592309));
#147927=CARTESIAN_POINT('Ctrl Pts',(-6.44251698659686,-2.76615282294941,
54.3556903510599));
#147928=CARTESIAN_POINT('Ctrl Pts',(-6.51526716039136,-2.59671380043394,
54.3473143510191));
#147929=CARTESIAN_POINT('Ctrl Pts',(-6.58129884465704,-2.42447317550418,
54.3389383509783));
#147930=CARTESIAN_POINT('Ctrl Pts',(-6.64041819490054,-2.24999394651049,
54.3305623509374));
#147931=CARTESIAN_POINT('Ctrl Pts',(-6.69956653892374,-2.07542914803224,
54.3221822430723));
#147932=CARTESIAN_POINT('Ctrl Pts',(-6.75179568935851,-1.89862386941246,
54.3138021352073));
#147933=CARTESIAN_POINT('Ctrl Pts',(-6.79696201811788,-1.72015519263901,
54.3054220273422));
#147934=CARTESIAN_POINT('Ctrl Pts',(-6.84217995684615,-1.54148258601093,
54.2970323438238));
#147935=CARTESIAN_POINT('Ctrl Pts',(-6.880318873142,-1.36114310361073,54.2886426603054));
#147936=CARTESIAN_POINT('Ctrl Pts',(-6.91128622526463,-1.17972423683137,
54.280252976787));
#147937=CARTESIAN_POINT('Ctrl Pts',(-6.93094742005016,-1.06454126402203,
54.2749263605109));
#147938=CARTESIAN_POINT('Ctrl Pts',(-6.9477188042965,-0.948923346076843,
54.2695997442348));
#147939=CARTESIAN_POINT('Ctrl Pts',(-6.96158756580647,-0.833021684056731,
54.2642731279587));
#147940=CARTESIAN_POINT('Ctrl Pts',(-6.98340956402631,-0.650654580803841,
54.2558918885228));
#147941=CARTESIAN_POINT('Ctrl Pts',(-6.99808673708094,-0.467216904398952,
54.2475106490869));
#147942=CARTESIAN_POINT('Ctrl Pts',(-7.00552433630664,-0.283293727278623,
54.2391294096509));
#147943=CARTESIAN_POINT('Ctrl Pts',(-7.01295250963259,-0.0996036416945087,
54.2307587920192));
#147944=CARTESIAN_POINT('Ctrl Pts',(-7.01315938068839,0.0845703936586706,
54.2223881743875));
#147945=CARTESIAN_POINT('Ctrl Pts',(-7.00610170299844,0.268636352235332,
54.2140175567558));
#147946=CARTESIAN_POINT('Ctrl Pts',(-6.99905203428671,0.452493434703441,
54.2056564380126));
#147947=CARTESIAN_POINT('Ctrl Pts',(-6.98475425997115,0.636242359411314,
54.1972953192695));
#147948=CARTESIAN_POINT('Ctrl Pts',(-6.96321710275037,0.819288802843555,
54.1889342005264));
#147949=CARTESIAN_POINT('Ctrl Pts',(-6.94170789054723,1.00209773878867,
54.1805839305508));
#147950=CARTESIAN_POINT('Ctrl Pts',(-6.91297806944858,1.18420568763883,
54.1722336605751));
#147951=CARTESIAN_POINT('Ctrl Pts',(-6.87708830778799,1.36502123404209,
54.1638833905995));
#147952=CARTESIAN_POINT('Ctrl Pts',(-6.84122615889285,1.54569766508087,
54.1555395451314));
#147953=CARTESIAN_POINT('Ctrl Pts',(-6.7982151107814,1.72508335519677,54.1471956996634));
#147954=CARTESIAN_POINT('Ctrl Pts',(-6.74816742335769,1.90259375296833,
54.1388518541954));
#147955=CARTESIAN_POINT('Ctrl Pts',(-6.6981599286592,2.07996159417015,54.1305147095741));
#147956=CARTESIAN_POINT('Ctrl Pts',(-6.64112715350645,2.25545683213024,
54.1221775649529));
#147957=CARTESIAN_POINT('Ctrl Pts',(-6.57723208423473,2.42850667543109,
54.1138404203317));
#147958=CARTESIAN_POINT('Ctrl Pts',(-6.55619528906484,2.48548155861368,
54.1110955011119));
#147959=CARTESIAN_POINT('Ctrl Pts',(-6.53441503618932,2.54219146814402,
54.108350581892));
#147960=CARTESIAN_POINT('Ctrl Pts',(-6.51189833282458,2.59861629823575,
54.1056056626722));
#147961=CARTESIAN_POINT('Ctrl Pts',(-6.44349740817105,2.77002285314629,
54.0972671856893));
#147962=CARTESIAN_POINT('Ctrl Pts',(-6.36835293155707,2.93865662908672,
54.0889287087064));
#147963=CARTESIAN_POINT('Ctrl Pts',(-6.28672608723384,3.10398158283737,
54.0805902317235));
#147964=CARTESIAN_POINT('Ctrl Pts',(-6.20504785834692,3.26941060958855,
54.0722465056218));
#147965=CARTESIAN_POINT('Ctrl Pts',(-6.1168792673513,3.43152636572703,54.0639027795201));
#147966=CARTESIAN_POINT('Ctrl Pts',(-6.02252708990521,3.58981810317152,
54.0555590534185));
#147967=CARTESIAN_POINT('Ctrl Pts',(-5.9281031021205,3.74823031460582,54.0472089770044));
#147968=CARTESIAN_POINT('Ctrl Pts',(-5.82748630799288,3.90281242090337,
54.0388589005904));
#147969=CARTESIAN_POINT('Ctrl Pts',(-5.72102659059777,4.05308293921717,
54.0305088241764));
#147970=CARTESIAN_POINT('Ctrl Pts',(-5.61440715990367,4.20357889679388,
54.0221462207871));
#147971=CARTESIAN_POINT('Ctrl Pts',(-5.50192747889674,4.34975007302886,
54.0137836173978));
#147972=CARTESIAN_POINT('Ctrl Pts',(-5.38397842384047,4.49114716905607,
54.0054210140085));
#147973=CARTESIAN_POINT('Ctrl Pts',(-5.26592848664575,4.63266520239312,
53.9970512580624));
#147974=CARTESIAN_POINT('Ctrl Pts',(-5.14240006074251,4.76940076577675,
53.9886815021163));
#147975=CARTESIAN_POINT('Ctrl Pts',(-5.01382099609593,4.90094129546637,
53.9803117461702));
#147976=CARTESIAN_POINT('Ctrl Pts',(-4.88504360187024,5.03268472271138,
53.9719290801117));
#147977=CARTESIAN_POINT('Ctrl Pts',(-4.75120023883623,5.15921687887051,
53.9635464140532));
#147978=CARTESIAN_POINT('Ctrl Pts',(-4.61275299158931,5.2801644293605,53.9551637479947));
#147979=CARTESIAN_POINT('Ctrl Pts',(-4.56746887668824,5.31972464368259,
53.9524218977917));
#147980=CARTESIAN_POINT('Ctrl Pts',(-4.52169245438644,5.35868772824994,
53.9496800475887));
#147981=CARTESIAN_POINT('Ctrl Pts',(-4.47544056682393,5.39704162438337,
53.9469381973857));
#147982=CARTESIAN_POINT('Ctrl Pts',(-4.33391683922757,5.51439870178506,
53.9385485535963));
#147983=CARTESIAN_POINT('Ctrl Pts',(-4.18765352090479,5.62628592099622,
53.9301589098068));
#147984=CARTESIAN_POINT('Ctrl Pts',(-4.0371002004268,5.73231615790807,53.9217692660174));
#147985=CARTESIAN_POINT('Ctrl Pts',(-3.88668583235713,5.83824853476125,
53.9133873654062));
#147986=CARTESIAN_POINT('Ctrl Pts',(-3.73198962274071,5.93833451712331,
53.9050054647951));
#147987=CARTESIAN_POINT('Ctrl Pts',(-3.57349379823855,6.03222750204687,
53.896623564184));
#147988=CARTESIAN_POINT('Ctrl Pts',(-3.41512094837784,6.12604763674746,
53.8882481669696));
#147989=CARTESIAN_POINT('Ctrl Pts',(-3.25295464300533,6.21368418686658,
53.8798727697552));
#147990=CARTESIAN_POINT('Ctrl Pts',(-3.08750600255809,6.29483385377786,
53.8714973725407));
#147991=CARTESIAN_POINT('Ctrl Pts',(-2.92216143775945,6.37593247340223,
53.8631272438791));
#147992=CARTESIAN_POINT('Ctrl Pts',(-2.75353894922176,6.4505522017272,53.8547571152175));
#147993=CARTESIAN_POINT('Ctrl Pts',(-2.58217456944514,6.51843547604875,
53.8463869865559));
#147994=CARTESIAN_POINT('Ctrl Pts',(-2.41089285598169,6.58628600342474,
53.838020895651));
#147995=CARTESIAN_POINT('Ctrl Pts',(-2.23687219403378,6.64740643630317,
53.8296548047461));
#147996=CARTESIAN_POINT('Ctrl Pts',(-2.06066934216875,6.70158700792177,
53.8212887138412));
#147997=CARTESIAN_POINT('Ctrl Pts',(-1.88451573485769,6.75575243734457,
53.812924961062));
#147998=CARTESIAN_POINT('Ctrl Pts',(-1.70618146716293,6.80298177499312,
53.8045612082828));
#147999=CARTESIAN_POINT('Ctrl Pts',(-1.52623976564818,6.84311469582779,
53.7961974555036));
#148000=CARTESIAN_POINT('Ctrl Pts',(-1.34632572539831,6.88324144729013,
53.7878349884296));
#148001=CARTESIAN_POINT('Ctrl Pts',(-1.16480506470539,6.91627388541577,
53.7794725213556));
#148002=CARTESIAN_POINT('Ctrl Pts',(-0.982262957190229,6.94210242256854,
53.7711100542816));
#148003=CARTESIAN_POINT('Ctrl Pts',(-0.799724568665301,6.96793043350804,
53.7627477575789));
#148004=CARTESIAN_POINT('Ctrl Pts',(-0.616165100303348,6.98655479047963,
53.7543854608762));
#148005=CARTESIAN_POINT('Ctrl Pts',(-0.432177064832101,6.99791751502782,
53.7460231641734));
#148006=CARTESIAN_POINT('Ctrl Pts',(-0.248168243395415,7.00928152327469,
53.737659922744));
#148007=CARTESIAN_POINT('Ctrl Pts',(-0.0637310863896442,7.01338224377359,
53.7292966813146));
#148008=CARTESIAN_POINT('Ctrl Pts',(0.120539222708804,7.01021375268178,
53.7209334398852));
#148009=CARTESIAN_POINT('Ctrl Pts',(0.304918144002506,7.00704339402501,
53.7125652690126));
#148010=CARTESIAN_POINT('Ctrl Pts',(0.489129691880897,6.99659526681974,
53.7041970981401));
#148011=CARTESIAN_POINT('Ctrl Pts',(0.672580091473121,6.97891557357259,
53.6958289272675));
#148012=CARTESIAN_POINT('Ctrl Pts',(0.856085518248708,6.96123057718233,
53.6874582463057));
#148013=CARTESIAN_POINT('Ctrl Pts',(1.0388290147668,6.93630972631325,53.6790875653439));
#148014=CARTESIAN_POINT('Ctrl Pts',(1.22022364519409,6.90425092375771,53.6707168843821));
#148015=CARTESIAN_POINT('Ctrl Pts',(1.40177210295799,6.87216493450872,53.6623391048665));
#148016=CARTESIAN_POINT('Ctrl Pts',(1.58196908598455,6.83292896081518,53.6539613253508));
#148017=CARTESIAN_POINT('Ctrl Pts',(1.76023839636499,6.78669192983315,53.6455835458351));
#148018=CARTESIAN_POINT('Ctrl Pts',(1.87358558721402,6.75729350133288,53.6402567861611));
#148019=CARTESIAN_POINT('Ctrl Pts',(1.98615374499486,6.72506579399611,53.634930026487));
#148020=CARTESIAN_POINT('Ctrl Pts',(2.09779821810326,6.6900574884393,53.629603266813));
#148021=CARTESIAN_POINT('Ctrl Pts',(2.26260797048975,6.63837817096261,53.6217398955375));
#148022=CARTESIAN_POINT('Ctrl Pts',(2.42574672627303,6.58052935195627,53.6138765242621));
#148023=CARTESIAN_POINT('Ctrl Pts',(2.58669862915145,6.51664152493031,53.6060131529867));
#148024=CARTESIAN_POINT('Ctrl Pts',(2.74752679726607,6.45280281285761,53.5981558268239));
#148025=CARTESIAN_POINT('Ctrl Pts',(2.90617110371796,6.38293446500579,53.5902985006611));
#148026=CARTESIAN_POINT('Ctrl Pts',(3.06212998960766,6.30721701618435,53.5824411744984));
#148027=CARTESIAN_POINT('Ctrl Pts',(3.21800085446169,6.23154230124258,53.5745882829017));
#148028=CARTESIAN_POINT('Ctrl Pts',(3.37118897178812,6.15002521807402,53.566735391305));
#148029=CARTESIAN_POINT('Ctrl Pts',(3.52121218575977,6.06289463089677,53.5588824997083));
#148030=CARTESIAN_POINT('Ctrl Pts',(3.67119985365704,5.97578468819348,53.5510314687535));
#148031=CARTESIAN_POINT('Ctrl Pts',(3.81802377709204,5.88306407266356,53.5431804377986));
#148032=CARTESIAN_POINT('Ctrl Pts',(3.96122593330704,5.78500783645068,53.5353294068438));
#148033=CARTESIAN_POINT('Ctrl Pts',(4.10440499417583,5.68696741454384,53.5274796420869));
#148034=CARTESIAN_POINT('Ctrl Pts',(4.24396313754947,5.58359330299941,53.51962987733));
#148035=CARTESIAN_POINT('Ctrl Pts',(4.37947129523831,5.4752038990967,53.5117801125732));
#148036=CARTESIAN_POINT('Ctrl Pts',(4.51502498564773,5.36677807477085,53.5039277101807));
#148037=CARTESIAN_POINT('Ctrl Pts',(4.64652567396897,5.25333383046175,53.4960753077881));
#148038=CARTESIAN_POINT('Ctrl Pts',(4.77357721788263,5.13522999557098,53.4882229053956));
#148039=CARTESIAN_POINT('Ctrl Pts',(4.86681209160202,5.0485612641835,53.4824605374392));
#148040=CARTESIAN_POINT('Ctrl Pts',(4.9576517174774,4.95938413182107,53.4766981694828));
#148041=CARTESIAN_POINT('Ctrl Pts',(5.04595229654346,4.86785291309298,53.4709358015264));
#148042=CARTESIAN_POINT('Ctrl Pts',(5.19375898840963,4.71463844059719,53.4612901507962));
#148043=CARTESIAN_POINT('Ctrl Pts',(5.33437537846057,4.55490577118934,53.4516445000659));
#148044=CARTESIAN_POINT('Ctrl Pts',(5.46732638077762,4.38930163107449,53.4419988493356));
#148045=CARTESIAN_POINT('Ctrl Pts',(5.60132159491213,4.22239681780098,53.432277440602));
#148046=CARTESIAN_POINT('Ctrl Pts',(5.72753053363526,4.04952800389971,53.4225560318684));
#148047=CARTESIAN_POINT('Ctrl Pts',(5.84551417401756,3.87138096857695,53.4128346231348));
#148048=CARTESIAN_POINT('Ctrl Pts',(5.96383325771917,3.69272743733103,53.4030855751318));
#148049=CARTESIAN_POINT('Ctrl Pts',(6.07388021664457,3.50876568583934,53.3933365271289));
#148050=CARTESIAN_POINT('Ctrl Pts',(6.17525959117132,3.32021016565919,53.3835874791259));
#148051=CARTESIAN_POINT('Ctrl Pts',(6.27678527771802,3.13138251972213,53.3738243611712));
#148052=CARTESIAN_POINT('Ctrl Pts',(6.36961833797077,2.93794787726775,53.3640612432166));
#148053=CARTESIAN_POINT('Ctrl Pts',(6.45340892105336,2.74064588375968,53.3542981252619));
#148054=CARTESIAN_POINT('Ctrl Pts',(6.49486802245064,2.64302198553866,53.3494673903231));
#148055=CARTESIAN_POINT('Ctrl Pts',(6.53411406089336,2.5444516133034,53.3446366553843));
#148056=CARTESIAN_POINT('Ctrl Pts',(6.57110895151815,2.44502632087634,53.3398059204455));
#148057=CARTESIAN_POINT('Origin',(0.,0.,50.));
#148058=CARTESIAN_POINT('',(6.57110895151816,2.4450263208763,51.3398522865015));
#148059=CARTESIAN_POINT('',(6.57110895151813,2.44502632087638,51.8867297377812));
#148060=CARTESIAN_POINT('',(6.57110895151814,2.44502632087636,50.));
#148061=CARTESIAN_POINT('',(7.01124961176728,-0.00233323662125234,53.7735343569105));
#148062=CARTESIAN_POINT('Ctrl Pts',(6.57110895151814,2.44502632087637,51.8867297377812));
#148063=CARTESIAN_POINT('Ctrl Pts',(6.49738188562511,2.64317084738811,51.8963190332494));
#148064=CARTESIAN_POINT('Ctrl Pts',(6.41477564156754,2.83774523706095,51.9059083287176));
#148065=CARTESIAN_POINT('Ctrl Pts',(6.32365121254535,3.02804588878268,51.9154976241858));
#148066=CARTESIAN_POINT('Ctrl Pts',(6.22946919857259,3.22473187992474,51.9254086784384));
#148067=CARTESIAN_POINT('Ctrl Pts',(6.1261876257228,3.41685231034913,51.935319732691));
#148068=CARTESIAN_POINT('Ctrl Pts',(6.01425257633941,3.60366376213081,51.9452307869436));
#148069=CARTESIAN_POINT('Ctrl Pts',(5.90515769409783,3.78573518163498,51.9548903645517));
#148070=CARTESIAN_POINT('Ctrl Pts',(5.78784316266017,3.96276371850206,51.9645499421597));
#148071=CARTESIAN_POINT('Ctrl Pts',(5.6627647591983,4.13409262650002,51.9742095197677));
#148072=CARTESIAN_POINT('Ctrl Pts',(5.53280193451934,4.31211207843014,51.9842463123426));
#148073=CARTESIAN_POINT('Ctrl Pts',(5.39445678623906,4.48397777650178,51.9942831049175));
#148074=CARTESIAN_POINT('Ctrl Pts',(5.24828784053023,4.64898927783691,52.0043198974924));
#148075=CARTESIAN_POINT('Ctrl Pts',(5.1021188948214,4.81400077917204,52.0143566900673));
#148076=CARTESIAN_POINT('Ctrl Pts',(4.94812618434371,4.97215800313843,52.0243934826422));
#148077=CARTESIAN_POINT('Ctrl Pts',(4.7869157045588,5.12279851252695,52.0344302752171));
#148078=CARTESIAN_POINT('Ctrl Pts',(4.65746671048288,5.24376001846283,52.0424896315585));
#148079=CARTESIAN_POINT('Ctrl Pts',(4.52330104608478,5.35993212343665,52.0505489879));
#148080=CARTESIAN_POINT('Ctrl Pts',(4.38481438060566,5.47092582751163,52.0586083442415));
#148081=CARTESIAN_POINT('Ctrl Pts',(4.24641501525139,5.58184956265357,52.0666626200735));
#148082=CARTESIAN_POINT('Ctrl Pts',(4.10370035448013,5.68760116891075,52.0747168959055));
#148083=CARTESIAN_POINT('Ctrl Pts',(3.95710130850763,5.78782997303024,52.0827711717375));
#148084=CARTESIAN_POINT('Ctrl Pts',(3.81056701941027,5.88801450329985,52.0908218897719));
#148085=CARTESIAN_POINT('Ctrl Pts',(3.66015206190331,5.98268088453343,52.0988726078063));
#148086=CARTESIAN_POINT('Ctrl Pts',(3.50631865348546,6.07152007842516,52.1069233258408));
#148087=CARTESIAN_POINT('Ctrl Pts',(3.35250310584948,6.16034895766886,52.1149731091489));
#148088=CARTESIAN_POINT('Ctrl Pts',(3.19527020929626,6.2433518090098,52.1230228924571));
#148089=CARTESIAN_POINT('Ctrl Pts',(3.03510944213073,6.32026401638325,52.1310726757653));
#148090=CARTESIAN_POINT('Ctrl Pts',(2.87496110514854,6.39717025454928,52.1391218343245));
#148091=CARTESIAN_POINT('Ctrl Pts',(2.71188568012388,6.46798663639252,52.1471709928837));
#148092=CARTESIAN_POINT('Ctrl Pts',(2.54639517432985,6.53249555519555,52.1552201514429));
#148093=CARTESIAN_POINT('Ctrl Pts',(2.38084358045904,6.59702828639657,52.1632722812155));
#148094=CARTESIAN_POINT('Ctrl Pts',(2.21287546535397,6.65524877389044,52.1713244109881));
#148095=CARTESIAN_POINT('Ctrl Pts',(2.04302102858217,6.70698826890812,52.1793765407607));
#148096=CARTESIAN_POINT('Ctrl Pts',(1.94654110256793,6.73637709587191,52.1839502740084));
#148097=CARTESIAN_POINT('Ctrl Pts',(1.84945286413414,6.7636757918757,52.188524007256));
#148098=CARTESIAN_POINT('Ctrl Pts',(1.751855358782,6.78886068235362,52.1930977405036));
#148099=CARTESIAN_POINT('Ctrl Pts',(1.56596748980799,6.83682876928772,52.2018090443796));
#148100=CARTESIAN_POINT('Ctrl Pts',(1.37813987116082,6.87714975211457,52.2105203482555));
#148101=CARTESIAN_POINT('Ctrl Pts',(1.18900391786138,6.90969581427506,52.2192316521315));
#148102=CARTESIAN_POINT('Ctrl Pts',(0.999821277320133,6.94224991026438,
52.2279451063482));
#148103=CARTESIAN_POINT('Ctrl Pts',(0.80932993070789,6.96702520816864,52.2366585605649));
#148104=CARTESIAN_POINT('Ctrl Pts',(0.618169440027649,6.98394538251237,
52.2453720147816));
#148105=CARTESIAN_POINT('Ctrl Pts',(0.423660139694004,7.00116196979676,
52.2542381140323));
#148106=CARTESIAN_POINT('Ctrl Pts',(0.22845832857096,7.01024563163166,52.263104213283));
#148107=CARTESIAN_POINT('Ctrl Pts',(0.0332415144088999,7.01117119775433,
52.2719703125337));
#148108=CARTESIAN_POINT('Ctrl Pts',(-0.158727631150627,7.01208136596135,
52.2806889134642));
#148109=CARTESIAN_POINT('Ctrl Pts',(-0.350711002208583,7.00510277572953,
52.2894075143947));
#148110=CARTESIAN_POINT('Ctrl Pts',(-0.542065010767642,6.99026409276513,
52.2981261153252));
#148111=CARTESIAN_POINT('Ctrl Pts',(-0.738274912213163,6.97504885612623,
52.307065963736));
#148112=CARTESIAN_POINT('Ctrl Pts',(-0.933822781115421,6.95156933986731,
52.3160058121468));
#148113=CARTESIAN_POINT('Ctrl Pts',(-1.12802008593984,6.91991309542369,
52.3249456605575));
#148114=CARTESIAN_POINT('Ctrl Pts',(-1.32221739076425,6.88825685098008,
52.3338855089683));
#148115=CARTESIAN_POINT('Ctrl Pts',(-1.51506382311917,6.848423935652,52.3428253573791));
#148116=CARTESIAN_POINT('Ctrl Pts',(-1.70588084663852,6.80055858732001,
52.3517652057899));
#148117=CARTESIAN_POINT('Ctrl Pts',(-1.89259041650315,6.75372357001568,
52.3605126184717));
#148118=CARTESIAN_POINT('Ctrl Pts',(-2.07737841994065,6.69919308793782,
52.3692600311535));
#148119=CARTESIAN_POINT('Ctrl Pts',(-2.25962264990725,6.63714788463585,
52.3780074438353));
#148120=CARTESIAN_POINT('Ctrl Pts',(-2.44183590375321,6.57511322718054,
52.386753369716));
#148121=CARTESIAN_POINT('Ctrl Pts',(-2.6215059896338,6.5055664873029,52.3954992955967));
#148122=CARTESIAN_POINT('Ctrl Pts',(-2.79802728278639,6.42873781447673,
52.4042452214775));
#148123=CARTESIAN_POINT('Ctrl Pts',(-2.97662802191316,6.35100408894243,
52.4130941756107));
#148124=CARTESIAN_POINT('Ctrl Pts',(-3.15200504087013,6.26581586515213,
52.421943129744));
#148125=CARTESIAN_POINT('Ctrl Pts',(-3.32355202203126,6.17346163180366,
52.4307920838772));
#148126=CARTESIAN_POINT('Ctrl Pts',(-3.49301548090057,6.08222908595224,
52.4395335631189));
#148127=CARTESIAN_POINT('Ctrl Pts',(-3.65874117300866,5.98400376189612,
52.4482750423606));
#148128=CARTESIAN_POINT('Ctrl Pts',(-3.82016857284352,5.87911036106303,
52.4570165216023));
#148129=CARTESIAN_POINT('Ctrl Pts',(-3.98457305329781,5.77228249240697,
52.4659192131813));
#148130=CARTESIAN_POINT('Ctrl Pts',(-4.1445189012361,5.65853833707336,52.4748219047603));
#148131=CARTESIAN_POINT('Ctrl Pts',(-4.29944325999532,5.53826816040726,
52.4837245963393));
#148132=CARTESIAN_POINT('Ctrl Pts',(-4.45436761875454,5.41799798374116,
52.4926272879184));
#148133=CARTESIAN_POINT('Ctrl Pts',(-4.60427024354619,5.29120195842042,
52.5015299794974));
#148134=CARTESIAN_POINT('Ctrl Pts',(-4.74862154391487,5.15831561608706,
52.5104326710764));
#148135=CARTESIAN_POINT('Ctrl Pts',(-4.87874294222263,5.03852898003835,
52.5184577506843));
#148136=CARTESIAN_POINT('Ctrl Pts',(-5.00441227347482,4.91373879624791,
52.5264828302922));
#148137=CARTESIAN_POINT('Ctrl Pts',(-5.12522316360501,4.78431960530928,
52.5345079099001));
#148138=CARTESIAN_POINT('Ctrl Pts',(-5.24599570916076,4.6549414911626,52.5425304424011));
#148139=CARTESIAN_POINT('Ctrl Pts',(-5.36191263375501,4.52093756261607,
52.550552974902));
#148140=CARTESIAN_POINT('Ctrl Pts',(-5.47260438858179,4.38271922082345,
52.5585755074029));
#148141=CARTESIAN_POINT('Ctrl Pts',(-5.58328218852011,4.24451830419088,
52.5665970285047));
#148142=CARTESIAN_POINT('Ctrl Pts',(-5.68873590216296,4.1021043190771,52.5746185496065));
#148143=CARTESIAN_POINT('Ctrl Pts',(-5.78863628977454,3.95592169629345,
52.5826400707083));
#148144=CARTESIAN_POINT('Ctrl Pts',(-5.88857383065286,3.80968470773498,
52.5906645750389));
#148145=CARTESIAN_POINT('Ctrl Pts',(-5.98295371015508,3.65967658290397,
52.5986890793694));
#148146=CARTESIAN_POINT('Ctrl Pts',(-6.0714898159291,3.50637105531763,52.6067135837));
#148147=CARTESIAN_POINT('Ctrl Pts',(-6.16004336901296,3.35303531667765,
52.6147396693743));
#148148=CARTESIAN_POINT('Ctrl Pts',(-6.24275067848505,3.1964012026647,52.6227657550486));
#148149=CARTESIAN_POINT('Ctrl Pts',(-6.31937174657498,3.03696679123923,
52.6307918407229));
#148150=CARTESIAN_POINT('Ctrl Pts',(-6.3960543660021,2.8774043027527,52.6388243739229));
#148151=CARTESIAN_POINT('Ctrl Pts',(-6.46664082868963,2.7150373583768,52.6468569071229));
#148152=CARTESIAN_POINT('Ctrl Pts',(-6.53093916853663,2.55038431209378,
52.6548894403228));
#148153=CARTESIAN_POINT('Ctrl Pts',(-6.5688568109,2.45328607693165,52.6596263390029));
#148154=CARTESIAN_POINT('Ctrl Pts',(-6.60458860855919,2.35539315621848,
52.6643632376829));
#148155=CARTESIAN_POINT('Ctrl Pts',(-6.63810335611066,2.25681421390695,
52.6691001363629));
#148156=CARTESIAN_POINT('Ctrl Pts',(-6.7070829409835,2.05392041297912,52.6788495550041));
#148157=CARTESIAN_POINT('Ctrl Pts',(-6.76670966664594,1.84799973121889,
52.6885989736453));
#148158=CARTESIAN_POINT('Ctrl Pts',(-6.81678354254027,1.63984410742365,
52.6983483922864));
#148159=CARTESIAN_POINT('Ctrl Pts',(-6.86692900026164,1.43139092008672,
52.7081117479594));
#148160=CARTESIAN_POINT('Ctrl Pts',(-6.90749428319051,1.22069643805856,
52.7178751036323));
#148161=CARTESIAN_POINT('Ctrl Pts',(-6.93832997257971,1.00856519576182,
52.7276384593053));
#148162=CARTESIAN_POINT('Ctrl Pts',(-6.9691141134063,0.796788576982175,
52.7373854934053));
#148163=CARTESIAN_POINT('Ctrl Pts',(-6.99020116242303,0.583580036267177,
52.7471325275054));
#148164=CARTESIAN_POINT('Ctrl Pts',(-7.00149359135956,0.369748634413932,
52.7568795616055));
#148165=CARTESIAN_POINT('Ctrl Pts',(-7.01275505981469,0.156503494664312,
52.7665998722372));
#148166=CARTESIAN_POINT('Ctrl Pts',(-7.01427551555764,-0.0573610567043534,
52.7763201828688));
#148167=CARTESIAN_POINT('Ctrl Pts',(-7.00600933329113,-0.271034655233487,
52.7860404935005));
#148168=CARTESIAN_POINT('Ctrl Pts',(-6.99779775869817,-0.483296693052025,
52.7956965902626));
#148169=CARTESIAN_POINT('Ctrl Pts',(-6.97992839641362,-0.695370244413059,
52.8053526870247));
#148170=CARTESIAN_POINT('Ctrl Pts',(-6.9524073705954,-0.90645370305976,
52.8150087837868));
#148171=CARTESIAN_POINT('Ctrl Pts',(-6.94028598709886,-0.999423477112943,
52.8192617230742));
#148172=CARTESIAN_POINT('Ctrl Pts',(-6.9262929634038,-1.09220109507887,
52.8235146623617));
#148173=CARTESIAN_POINT('Ctrl Pts',(-6.91043201460631,-1.18471766003728,
52.8277676016491));
#148174=CARTESIAN_POINT('Ctrl Pts',(-6.88114734309575,-1.35553450388971,
52.8356199648071));
#148175=CARTESIAN_POINT('Ctrl Pts',(-6.84550330118022,-1.52539042967983,
52.843472327965));
#148176=CARTESIAN_POINT('Ctrl Pts',(-6.80358783046252,-1.69375889538101,
52.8513246911229));
#148177=CARTESIAN_POINT('Ctrl Pts',(-6.76168421922834,-1.86207972322893,
52.8591748325482));
#148178=CARTESIAN_POINT('Ctrl Pts',(-6.71351280089283,-2.02891355839185,
52.8670249739734));
#148179=CARTESIAN_POINT('Ctrl Pts',(-6.65921250695034,-2.19374459538394,
52.8748751153986));
#148180=CARTESIAN_POINT('Ctrl Pts',(-6.60491651439462,-2.35856257531884,
52.8827246349765));
#148181=CARTESIAN_POINT('Ctrl Pts',(-6.54449273278661,-2.52137771088187,
52.8905741545544));
#148182=CARTESIAN_POINT('Ctrl Pts',(-6.47812970861941,-2.68169014630748,
52.8984236741323));
#148183=CARTESIAN_POINT('Ctrl Pts',(-6.41173303607269,-2.84208386575736,
52.9062771736917));
#148184=CARTESIAN_POINT('Ctrl Pts',(-6.33939125012485,-2.99997199676093,
52.9141306732512));
#148185=CARTESIAN_POINT('Ctrl Pts',(-6.26134087109187,-3.15487512565783,
52.9219841728107));
#148186=CARTESIAN_POINT('Ctrl Pts',(-6.18327063117989,-3.30981767156125,
52.9298396707897));
#148187=CARTESIAN_POINT('Ctrl Pts',(-6.09948908840324,-3.46177336806262,
52.9376951687687));
#148188=CARTESIAN_POINT('Ctrl Pts',(-6.01027801610609,-3.61028873244396,
52.9455506667477));
#148189=CARTESIAN_POINT('Ctrl Pts',(-5.92097835337921,-3.75895157896641,
52.9534139655739));
#148190=CARTESIAN_POINT('Ctrl Pts',(-5.82623860074293,-3.904166950647,52.9612772644001));
#148191=CARTESIAN_POINT('Ctrl Pts',(-5.72638334820141,-4.04551113111083,
52.9691405632263));
#148192=CARTESIAN_POINT('Ctrl Pts',(-5.65317628529437,-4.14913504720336,
52.9749053977961));
#148193=CARTESIAN_POINT('Ctrl Pts',(-5.57722062337591,-4.25067889836404,
52.9806702323659));
#148194=CARTESIAN_POINT('Ctrl Pts',(-5.49865742519521,-4.34998771065454,
52.9864350669357));
#148195=CARTESIAN_POINT('Ctrl Pts',(-5.38448370215646,-4.49431046090313,
52.9948129415739));
#148196=CARTESIAN_POINT('Ctrl Pts',(-5.26454865711783,-4.63423138252872,
53.0031908162122));
#148197=CARTESIAN_POINT('Ctrl Pts',(-5.13921861863479,-4.76928281320972,
53.0115686908504));
#148198=CARTESIAN_POINT('Ctrl Pts',(-5.01397434899191,-4.90424182227565,
53.0199408321417));
#148199=CARTESIAN_POINT('Ctrl Pts',(-4.88334266962664,-5.03433774401859,
53.028312973433));
#148200=CARTESIAN_POINT('Ctrl Pts',(-4.74772973120227,-5.15913645506281,
53.0366851147243));
#148201=CARTESIAN_POINT('Ctrl Pts',(-4.61218970251025,-5.28386807043957,
53.0450527548921));
#148202=CARTESIAN_POINT('Ctrl Pts',(-4.47167399595628,-5.40330793152722,
53.0534203950599));
#148203=CARTESIAN_POINT('Ctrl Pts',(-4.32662543794832,-5.51705889783664,
53.0617880352277));
#148204=CARTESIAN_POINT('Ctrl Pts',(-4.18163360499046,-5.63076537884163,
53.07015240301));
#148205=CARTESIAN_POINT('Ctrl Pts',(-4.03211271387152,-5.7387871990518,
53.0785167707922));
#148206=CARTESIAN_POINT('Ctrl Pts',(-3.87853882063992,-5.84076734507454,
53.0868811385745));
#148207=CARTESIAN_POINT('Ctrl Pts',(-3.72500249747157,-5.94272254284302,
53.0952434601116));
#148208=CARTESIAN_POINT('Ctrl Pts',(-3.56741542335055,-6.0386388326411,
53.1036057816488));
#148209=CARTESIAN_POINT('Ctrl Pts',(-3.40628316674059,-6.12820214667236,
53.1119681031859));
#148210=CARTESIAN_POINT('Ctrl Pts',(-3.24513811494998,-6.21777257274193,
53.1203310887578));
#148211=CARTESIAN_POINT('Ctrl Pts',(-3.08044760260133,-6.30098885019583,
53.1286940743297));
#148212=CARTESIAN_POINT('Ctrl Pts',(-2.91274303831639,-6.3775821872587,
53.1370570599016));
#148213=CARTESIAN_POINT('Ctrl Pts',(-2.74502707181406,-6.45418073189527,
53.145420614072));
#148214=CARTESIAN_POINT('Ctrl Pts',(-2.57429694378769,-6.5241553014348,
53.1537841682425));
#148215=CARTESIAN_POINT('Ctrl Pts',(-2.40110550043158,-6.58728464075276,
53.162147722413));
#148216=CARTESIAN_POINT('Ctrl Pts',(-2.22787918181044,-6.65042669231791,
53.1705129607381));
#148217=CARTESIAN_POINT('Ctrl Pts',(-2.05219086849353,-6.7067206524817,
53.1788781990632));
#148218=CARTESIAN_POINT('Ctrl Pts',(-1.87461048231744,-6.75599453093959,
53.1872434373883));
#148219=CARTESIAN_POINT('Ctrl Pts',(-1.69697064230528,-6.80528490627056,
53.1956114763915));
#148220=CARTESIAN_POINT('Ctrl Pts',(-1.51743778300031,-6.84755042541538,
53.2039795153948));
#148221=CARTESIAN_POINT('Ctrl Pts',(-1.3365944002167,-6.8826696834738,53.212347554398));
#148222=CARTESIAN_POINT('Ctrl Pts',(-1.15558334281819,-6.91782150345393,
53.2207233520911));
#148223=CARTESIAN_POINT('Ctrl Pts',(-0.973259656936354,-6.94581375911681,
53.2290991497842));
#148224=CARTESIAN_POINT('Ctrl Pts',(-0.790214623164005,-6.96657644843131,
53.2374749474773));
#148225=CARTESIAN_POINT('Ctrl Pts',(-0.607079819284237,-6.9873493203157,
53.2458548528822));
#148226=CARTESIAN_POINT('Ctrl Pts',(-0.423223289275351,-7.00088552477128,
53.2542347582872));
#148227=CARTESIAN_POINT('Ctrl Pts',(-0.239239424257183,-7.00716712091135,
53.2626146636922));
#148228=CARTESIAN_POINT('Ctrl Pts',(-0.0550452854087596,-7.01345589624228,
53.2710041464305));
#148229=CARTESIAN_POINT('Ctrl Pts',(0.129276150356669,-7.01247349094504,
53.2793936291688));
#148230=CARTESIAN_POINT('Ctrl Pts',(0.313131156556268,-7.00425409599721,
53.2877831119071));
#148231=CARTESIAN_POINT('Ctrl Pts',(0.429915033188503,-6.99903317313294,
53.2931120737743));
#148232=CARTESIAN_POINT('Ctrl Pts',(0.546510788298153,-6.99089336650238,
53.2984410356414));
#148233=CARTESIAN_POINT('Ctrl Pts',(0.662767741419831,-6.97985425946941,
53.3037699975085));
#148234=CARTESIAN_POINT('Ctrl Pts',(0.845618554035697,-6.96249177372269,
53.3121514747591));
#148235=CARTESIAN_POINT('Ctrl Pts',(1.02799978744619,-6.93791956892268,
53.3205329520096));
#148236=CARTESIAN_POINT('Ctrl Pts',(1.20931955548607,-6.90616918234842,
53.3289144292601));
#148237=CARTESIAN_POINT('Ctrl Pts',(1.39040950741343,-6.87445903821706,
53.3372852832977));
#148238=CARTESIAN_POINT('Ctrl Pts',(1.57044035504783,-6.83558889990403,
53.3456561373352));
#148239=CARTESIAN_POINT('Ctrl Pts',(1.74882434320985,-6.78964210979464,
53.3540269913727));
#148240=CARTESIAN_POINT('Ctrl Pts',(1.92700586840388,-6.74374746855574,
53.362388344625));
#148241=CARTESIAN_POINT('Ctrl Pts',(2.10354394422297,-6.69079226518622,
53.3707496978774));
#148242=CARTESIAN_POINT('Ctrl Pts',(2.27785959632453,-6.63091111552042,
53.3791110511297));
#148243=CARTESIAN_POINT('Ctrl Pts',(2.45194899597982,-6.57110768840239,
53.3874615517902));
#148244=CARTESIAN_POINT('Ctrl Pts',(2.62382141714329,-6.50439635146568,
53.3958120524506));
#148245=CARTESIAN_POINT('Ctrl Pts',(2.7929117479289,-6.43096186668688,53.4041625531111));
#148246=CARTESIAN_POINT('Ctrl Pts',(2.96187193696155,-6.35758390135854,
53.4125066267406));
#148247=CARTESIAN_POINT('Ctrl Pts',(3.12805400352092,-6.27749323003578,
53.4208507003701));
#148248=CARTESIAN_POINT('Ctrl Pts',(3.29091048807659,-6.19092357584614,
53.4291947739996));
#148249=CARTESIAN_POINT('Ctrl Pts',(3.45363610160427,-6.10442348879511,
53.4375321423542));
#148250=CARTESIAN_POINT('Ctrl Pts',(3.61304117445129,-6.01145495582541,
53.4458695107088));
#148251=CARTESIAN_POINT('Ctrl Pts',(3.76860050051226,-5.9122987771288,53.4542068790634));
#148252=CARTESIAN_POINT('Ctrl Pts',(3.81978947701362,-5.87967004679298,
53.4569504069739));
#148253=CARTESIAN_POINT('Ctrl Pts',(3.87056221194856,-5.8463716738514,53.4596939348844));
#148254=CARTESIAN_POINT('Ctrl Pts',(3.92090057162729,-5.81241475377599,
53.4624374627949));
#148255=CARTESIAN_POINT('Ctrl Pts',(4.07389115569456,-5.70921137034,53.470775714977));
#148256=CARTESIAN_POINT('Ctrl Pts',(4.2227417677762,-5.60000642957328,53.4791139671591));
#148257=CARTESIAN_POINT('Ctrl Pts',(4.36698398876145,-5.48516885833072,
53.4874522193411));
#148258=CARTESIAN_POINT('Ctrl Pts',(4.51131694716161,-5.37025904704446,
53.4957957168074));
#148259=CARTESIAN_POINT('Ctrl Pts',(4.65103547577643,-5.24970974185834,
53.5041392142737));
#148260=CARTESIAN_POINT('Ctrl Pts',(4.7857055458016,-5.12392905799679,53.51248271174));
#148261=CARTESIAN_POINT('Ctrl Pts',(4.92047806053816,-4.99805269165838,
53.5208325561785));
#148262=CARTESIAN_POINT('Ctrl Pts',(5.05019421714145,-4.86693723213022,
53.529182400617));
#148263=CARTESIAN_POINT('Ctrl Pts',(5.17445773021242,-4.73102671317178,
53.5375322450555));
#148264=CARTESIAN_POINT('Ctrl Pts',(5.29890761930794,-4.59491234948376,
53.5458946129675));
#148265=CARTESIAN_POINT('Ctrl Pts',(5.41788830112758,-4.45398879682521,
53.5542569808795));
#148266=CARTESIAN_POINT('Ctrl Pts',(5.53104363784399,-4.30873332184362,
53.5626193487914));
#148267=CARTESIAN_POINT('Ctrl Pts',(5.64429573273144,-4.16335364013435,
53.5709888672935));
#148268=CARTESIAN_POINT('Ctrl Pts',(5.7517123531769,-4.01363491088012,53.5793583857955));
#148269=CARTESIAN_POINT('Ctrl Pts',(5.85298110386718,-3.86008274008133,
53.5877279042975));
#148270=CARTESIAN_POINT('Ctrl Pts',(5.95440604789685,-3.70629373584512,
53.5961103316489));
#148271=CARTESIAN_POINT('Ctrl Pts',(6.04966400466087,-3.54865975488553,
53.6044927590003));
#148272=CARTESIAN_POINT('Ctrl Pts',(6.13848817773367,-3.38771153646883,
53.6128751863516));
#148273=CARTESIAN_POINT('Ctrl Pts',(6.16755692568737,-3.33503935238987,
53.6156184335949));
#148274=CARTESIAN_POINT('Ctrl Pts',(6.19593699709623,-3.28201237487052,
53.6183616808381));
#148275=CARTESIAN_POINT('Ctrl Pts',(6.22362016802609,-3.22864965064946,
53.6211049280814));
#148276=CARTESIAN_POINT('Ctrl Pts',(6.31279000626182,-3.05676379629179,
53.6299411597957));
#148277=CARTESIAN_POINT('Ctrl Pts',(6.39488485271589,-2.88108616740664,
53.63877739151));
#148278=CARTESIAN_POINT('Ctrl Pts',(6.46960175896294,-2.70219903836183,
53.6476136232243));
#148279=CARTESIAN_POINT('Ctrl Pts',(6.54422323585766,-2.52354038616014,
53.6564385691946));
#148280=CARTESIAN_POINT('Ctrl Pts',(6.61148547670641,-2.34168065360165,
53.665263515165));
#148281=CARTESIAN_POINT('Ctrl Pts',(6.67113258381076,-2.15722428405542,
53.6740884611354));
#148282=CARTESIAN_POINT('Ctrl Pts',(6.73065862261849,-1.97314231352942,
53.6828954947337));
#148283=CARTESIAN_POINT('Ctrl Pts',(6.78260030170666,-1.78647447390649,
53.691702528332));
#148284=CARTESIAN_POINT('Ctrl Pts',(6.82675078815544,-1.59784236985976,
53.7005095619303));
#148285=CARTESIAN_POINT('Ctrl Pts',(6.87084338698309,-1.40945758956077,
53.7093050482441));
#148286=CARTESIAN_POINT('Ctrl Pts',(6.90716511315425,-1.2191139350955,53.718100534558));
#148287=CARTESIAN_POINT('Ctrl Pts',(6.93555892679197,-1.02744777750318,
53.7268960208719));
#148288=CARTESIAN_POINT('Ctrl Pts',(6.96389349720157,-0.836181528216391,
53.7356731555473));
#148289=CARTESIAN_POINT('Ctrl Pts',(6.98433312971832,-0.643598539623538,
53.7444502902227));
#148290=CARTESIAN_POINT('Ctrl Pts',(6.99677184506829,-0.450344657523186,
53.7532274248982));
#148291=CARTESIAN_POINT('Ctrl Pts',(7.00636465472937,-0.301306139067398,
53.7599964022356));
#148292=CARTESIAN_POINT('Ctrl Pts',(7.01119984858409,-0.151868905524662,
53.7667653795731));
#148293=CARTESIAN_POINT('Ctrl Pts',(7.01124961176728,-0.00233323662125234,
53.7735343569105));
#148294=CARTESIAN_POINT('Ctrl Pts',(7.01124961574396,-0.00232125615213359,
53.7735348992261));
#148295=CARTESIAN_POINT('Ctrl Pts',(7.01131371635395,0.191291748034507,
53.7822991096566));
#148296=CARTESIAN_POINT('Ctrl Pts',(7.00335363842858,0.384791190643915,
53.7910633200871));
#148297=CARTESIAN_POINT('Ctrl Pts',(6.98742384762321,0.577524489668229,
53.7998275305177));
#148298=CARTESIAN_POINT('Ctrl Pts',(6.97146745755452,0.770579611108935,
53.8086063752609));
#148299=CARTESIAN_POINT('Ctrl Pts',(6.94751476422251,0.962865767552298,
53.8173852200042));
#148300=CARTESIAN_POINT('Ctrl Pts',(6.9156720775946,1.15373579197248,53.8261640647475));
#148301=CARTESIAN_POINT('Ctrl Pts',(6.88380340884426,1.34476155728231,53.8349500726118));
#148302=CARTESIAN_POINT('Ctrl Pts',(6.84403193840754,1.53436862407777,53.8437360804762));
#148303=CARTESIAN_POINT('Ctrl Pts',(6.79651493802973,1.72192080527496,53.8525220883405));
#148304=CARTESIAN_POINT('Ctrl Pts',(6.74894331126548,1.90968859978627,53.8613181967553));
#148305=CARTESIAN_POINT('Ctrl Pts',(6.69360842302094,2.09539653188144,53.8701143051701));
#148306=CARTESIAN_POINT('Ctrl Pts',(6.63071768709321,2.27842259393846,53.8789104135849));
#148307=CARTESIAN_POINT('Ctrl Pts',(6.611547547197,2.33421197471973,53.8815916133891));
#148308=CARTESIAN_POINT('Ctrl Pts',(6.59167571245204,2.38975230369193,53.8842728131933));
#148309=CARTESIAN_POINT('Ctrl Pts',(6.57110895151814,2.44502632087636,53.8869540129975));
#148310=CARTESIAN_POINT('',(7.01125,-2.00130710614754E-13,53.2264656430896));
#148311=CARTESIAN_POINT('Ctrl Pts',(6.57110895151815,2.44502632087634,53.3398059204455));
#148312=CARTESIAN_POINT('Ctrl Pts',(6.64140535766679,2.25610183374145,53.3306267257104));
#148313=CARTESIAN_POINT('Ctrl Pts',(6.70357143908928,2.06408955382915,53.3214475309752));
#148314=CARTESIAN_POINT('Ctrl Pts',(6.75737442391738,1.86963029968155,53.31226833624));
#148315=CARTESIAN_POINT('Ctrl Pts',(6.80474661620868,1.69841375454496,53.3041862831817));
#148316=CARTESIAN_POINT('Ctrl Pts',(6.84565607039973,1.52521926086687,53.2961042301234));
#148317=CARTESIAN_POINT('Ctrl Pts',(6.87993901121358,1.35057978826928,53.2880221770651));
#148318=CARTESIAN_POINT('Ctrl Pts',(6.91419962127447,1.17605406994208,53.2799453883839));
#148319=CARTESIAN_POINT('Ctrl Pts',(6.94184224021634,1.00008559936461,53.2718685997028));
#148320=CARTESIAN_POINT('Ctrl Pts',(6.96275330735328,0.823221078107828,
53.2637918110216));
#148321=CARTESIAN_POINT('Ctrl Pts',(6.98365362487211,0.646447476460647,
53.2557191743234));
#148322=CARTESIAN_POINT('Ctrl Pts',(6.99782924055202,0.468779099787468,
53.2476465376252));
#148323=CARTESIAN_POINT('Ctrl Pts',(7.0052179552401,0.290771322660413,53.2395739009269));
#148324=CARTESIAN_POINT('Ctrl Pts',(7.0092171928638,0.1944223053211,53.2352044816478));
#148325=CARTESIAN_POINT('Ctrl Pts',(7.01122899283649,0.097973988105694,
53.2308350623687));
#148326=CARTESIAN_POINT('Ctrl Pts',(7.01124983631059,0.00151503620485756,
53.2264656430896));
#148327=CARTESIAN_POINT('Ctrl Pts',(7.01125,-8.58630487052188E-16,53.2264656430896));
#148328=CARTESIAN_POINT('Ctrl Pts',(7.01125,-0.191009525814462,53.2177938341508));
#148329=CARTESIAN_POINT('Ctrl Pts',(7.00344006572041,-0.382018909628726,
53.209122025212));
#148330=CARTESIAN_POINT('Ctrl Pts',(6.98784625534317,-0.572390840411034,
53.2004502162733));
#148331=CARTESIAN_POINT('Ctrl Pts',(6.97225246786074,-0.762762491689531,
53.1917784200664));
#148332=CARTESIAN_POINT('Ctrl Pts',(6.94887485033525,-0.952496408757991,
53.1831066238596));
#148333=CARTESIAN_POINT('Ctrl Pts',(6.91779140296513,-1.14095953809139,
53.1744348276527));
#148334=CARTESIAN_POINT('Ctrl Pts',(6.88670800059787,-1.32942239456645,
53.165763044001));
#148335=CARTESIAN_POINT('Ctrl Pts',(6.84791883692705,-1.51661418677696,
53.1570912603492));
#148336=CARTESIAN_POINT('Ctrl Pts',(6.80155333291305,-1.70191034488875,
53.1484194766975));
#148337=CARTESIAN_POINT('Ctrl Pts',(6.75518789508205,-1.88720623850532,
53.139747705424));
#148338=CARTESIAN_POINT('Ctrl Pts',(6.70124620748597,-2.07060622793696,
53.1310759341505));
#148339=CARTESIAN_POINT('Ctrl Pts',(6.63990824732571,-2.25149839653418,
53.122404162877));
#148340=CARTESIAN_POINT('Ctrl Pts',(6.57857037346951,-2.43239031061157,
53.113732403805));
#148341=CARTESIAN_POINT('Ctrl Pts',(6.50983633907179,-2.61077414196406,
53.1050606447329));
#148342=CARTESIAN_POINT('Ctrl Pts',(6.43393547556233,-2.78605471209748,
53.0963888856608));
#148343=CARTESIAN_POINT('Ctrl Pts',(6.35803471730007,-2.96133503917979,
53.0877171386133));
#148344=CARTESIAN_POINT('Ctrl Pts',(6.27496726266193,-3.1335118530473,53.0790453915659));
#148345=CARTESIAN_POINT('Ctrl Pts',(6.18501026583403,-3.30201068654051,
53.0703736445184));
#148346=CARTESIAN_POINT('Ctrl Pts',(6.09151188668825,-3.47714289832064,
53.0613605124454));
#148347=CARTESIAN_POINT('Ctrl Pts',(5.99057066119165,-3.64830137931007,
53.0523473803724));
#148348=CARTESIAN_POINT('Ctrl Pts',(5.88255038916588,-3.81486926138032,
53.0433342482994));
#148349=CARTESIAN_POINT('Ctrl Pts',(5.77621793389049,-3.97883452029324,
53.034461946415));
#148350=CARTESIAN_POINT('Ctrl Pts',(5.66302622906376,-4.13835132493741,
53.0255896445306));
#148351=CARTESIAN_POINT('Ctrl Pts',(5.54337059052903,-4.29286257158994,
53.0167173426463));
#148352=CARTESIAN_POINT('Ctrl Pts',(5.42558457134642,-4.44495958001353,
53.0079836704789));
#148353=CARTESIAN_POINT('Ctrl Pts',(5.30153533574937,-4.59220608124103,
52.9992499983114));
#148354=CARTESIAN_POINT('Ctrl Pts',(5.17164269972312,-4.73410375349976,
52.990516326144));
#148355=CARTESIAN_POINT('Ctrl Pts',(5.04265587431577,-4.87501189762002,
52.98184355853));
#148356=CARTESIAN_POINT('Ctrl Pts',(4.9079071016412,-5.01064538261968,52.973170790916));
#148357=CARTESIAN_POINT('Ctrl Pts',(4.7678460760923,-5.14055156157307,52.964498023302));
#148358=CARTESIAN_POINT('Ctrl Pts',(4.62778576967364,-5.27045707353532,
52.9558253002176));
#148359=CARTESIAN_POINT('Ctrl Pts',(4.48241347329788,-5.39463514506495,
52.9471525771331));
#148360=CARTESIAN_POINT('Ctrl Pts',(4.3322143300549,-5.51267136341058,52.9384798540486));
#148361=CARTESIAN_POINT('Ctrl Pts',(4.18201594573482,-5.63070698534541,
52.9298071747855));
#148362=CARTESIAN_POINT('Ctrl Pts',(4.02699098676462,-5.74260064062568,
52.9211344955224));
#148363=CARTESIAN_POINT('Ctrl Pts',(3.86765680431923,-5.84797891638668,
52.9124618162592));
#148364=CARTESIAN_POINT('Ctrl Pts',(3.70832341394854,-5.9533566682961,52.9037891801093));
#148365=CARTESIAN_POINT('Ctrl Pts',(3.54468107996522,-6.0522189487593,52.8951165439594));
#148366=CARTESIAN_POINT('Ctrl Pts',(3.37727590612859,-6.14423583665075,
52.8864439078095));
#148367=CARTESIAN_POINT('Ctrl Pts',(3.20987155082483,-6.23625227462273,
52.8777713140647));
#148368=CARTESIAN_POINT('Ctrl Pts',(3.0387046414804,-6.32142325013736,52.8690987203199));
#148369=CARTESIAN_POINT('Ctrl Pts',(2.86434638712907,-6.3994645351811,52.8604261265751));
#148370=CARTESIAN_POINT('Ctrl Pts',(2.68998897107704,-6.47750544500914,
52.8517535745274));
#148371=CARTESIAN_POINT('Ctrl Pts',(2.51244050005463,-6.5484166168872,52.8430810224797));
#148372=CARTESIAN_POINT('Ctrl Pts',(2.33229347360944,-6.61196141212718,
52.834408470432));
#148373=CARTESIAN_POINT('Ctrl Pts',(2.15214729859256,-6.6755059070356,52.8257359593734));
#148374=CARTESIAN_POINT('Ctrl Pts',(1.96940286066657,-6.73168400046413,
52.8170634483147));
#148375=CARTESIAN_POINT('Ctrl Pts',(1.78466999315593,-6.78030822146227,
52.808390937256));
#148376=CARTESIAN_POINT('Ctrl Pts',(1.59993798367095,-6.8289322166163,52.7997184664785));
#148377=CARTESIAN_POINT('Ctrl Pts',(1.41321783783529,-6.87000233723084,
52.7910459957009));
#148378=CARTESIAN_POINT('Ctrl Pts',(1.22513265045758,-6.9033815301838,52.7823735249233));
#148379=CARTESIAN_POINT('Ctrl Pts',(1.03704832132629,-6.93676057082506,
52.7737010937188));
#148380=CARTESIAN_POINT('Ctrl Pts',(0.847599242850681,-6.96244870438827,
52.7650286625143));
#148381=CARTESIAN_POINT('Ctrl Pts',(0.657417610665334,-6.98036020902124,
52.7563562313099));
#148382=CARTESIAN_POINT('Ctrl Pts',(0.467236830772413,-6.99827163338443,
52.7476838389706));
#148383=CARTESIAN_POINT('Ctrl Pts',(0.276323786585382,-7.0084064719186,
52.7390114466313));
#148384=CARTESIAN_POINT('Ctrl Pts',(0.085315553319391,-7.01073090475321,
52.7303390542921));
#148385=CARTESIAN_POINT('Ctrl Pts',(-0.10569183953708,-7.01305532736065,
52.7216667001101));
#148386=CARTESIAN_POINT('Ctrl Pts',(-0.296794136563897,-7.00756940957902,
52.7129943459281));
#148387=CARTESIAN_POINT('Ctrl Pts',(-0.487353636616802,-6.99429145770867,
52.7043219917462));
#148388=CARTESIAN_POINT('Ctrl Pts',(-0.677912313784566,-6.98101356317594,
52.6956496750137));
#148389=CARTESIAN_POINT('Ctrl Pts',(-0.867927915270643,-6.95994372163462,
52.6869773582812));
#148390=CARTESIAN_POINT('Ctrl Pts',(-1.05676637166343,-6.93115224174317,
52.6783050415487));
#148391=CARTESIAN_POINT('Ctrl Pts',(-1.24560402801217,-6.90236088383138,
52.6696327615579));
#148392=CARTESIAN_POINT('Ctrl Pts',(-1.43326426841352,-6.86584799585126,
52.660960481567));
#148393=CARTESIAN_POINT('Ctrl Pts',(-1.61912088843974,-6.82173541784773,
52.6522882015762));
#148394=CARTESIAN_POINT('Ctrl Pts',(-1.80497673622023,-6.77762302313468,
52.6436159576192));
#148395=CARTESIAN_POINT('Ctrl Pts',(-1.98902870222734,-6.72591106718914,
52.6349437136622));
#148396=CARTESIAN_POINT('Ctrl Pts',(-2.17066262760151,-6.66677210647208,
52.6262714697052));
#148397=CARTESIAN_POINT('Ctrl Pts',(-2.35229581309592,-6.6076333866556,
52.6175992610743));
#148398=CARTESIAN_POINT('Ctrl Pts',(-2.53151070755718,-6.54106781055492,
52.6089270524434));
#148399=CARTESIAN_POINT('Ctrl Pts',(-2.70770929770798,-6.46729749753371,
52.6002548438125));
#148400=CARTESIAN_POINT('Ctrl Pts',(-2.8839071844959,-6.39352747899442,
52.5915826698));
#148401=CARTESIAN_POINT('Ctrl Pts',(-3.05708852904455,-6.31255289079054,
52.5829104957875));
#148402=CARTESIAN_POINT('Ctrl Pts',(-3.22667545573855,-6.22464393084732,
52.574238321775));
#148403=CARTESIAN_POINT('Ctrl Pts',(-3.39626171929933,-6.1367353146532,
52.5655661816732));
#148404=CARTESIAN_POINT('Ctrl Pts',(-3.56225334094397,-6.04189251170717,
52.5568940415713));
#148405=CARTESIAN_POINT('Ctrl Pts',(-3.72409644022225,-5.94043199324965,
52.5482219014695));
#148406=CARTESIAN_POINT('Ctrl Pts',(-3.88593891985202,-5.83897186325391,
52.5395497945707));
#148407=CARTESIAN_POINT('Ctrl Pts',(-4.04363266823177,-5.73089421932567,
52.5308776876718));
#148408=CARTESIAN_POINT('Ctrl Pts',(-4.19665149726035,-5.61655969193264,
52.522205580773));
#148409=CARTESIAN_POINT('Ctrl Pts',(-4.34966975290987,-5.50222559296417,
52.5135335063696));
#148410=CARTESIAN_POINT('Ctrl Pts',(-4.49801289671993,-5.38163482746555,
52.5048614319661));
#148411=CARTESIAN_POINT('Ctrl Pts',(-4.64118594513171,-5.255189776327,52.4961893575627));
#148412=CARTESIAN_POINT('Ctrl Pts',(-4.78435846873845,-5.12874518867653,
52.487517314947));
#148413=CARTESIAN_POINT('Ctrl Pts',(-4.92236072197161,-4.99644654635204,
52.4788452723313));
#148414=CARTESIAN_POINT('Ctrl Pts',(-5.05473222958171,-4.85873529323506,
52.4701732297156));
#148415=CARTESIAN_POINT('Ctrl Pts',(-5.18710326277897,-4.7210245336683,
52.46150121818));
#148416=CARTESIAN_POINT('Ctrl Pts',(-5.3138433939023,-4.57790140690153,
52.4528292066445));
#148417=CARTESIAN_POINT('Ctrl Pts',(-5.43452972930885,-4.42984347169945,
52.444157195109));
#148418=CARTESIAN_POINT('Ctrl Pts',(-5.55521564202676,-4.28178605505159,
52.4354852139461));
#148419=CARTESIAN_POINT('Ctrl Pts',(-5.66984762200097,-4.1287940847108,
52.4268132327831));
#148420=CARTESIAN_POINT('Ctrl Pts',(-5.77804317951857,-3.971378045228,52.4181412516202));
#148421=CARTESIAN_POINT('Ctrl Pts',(-5.88623836692132,-3.81396254423323,
52.4094693001224));
#148422=CARTESIAN_POINT('Ctrl Pts',(-5.98799701504699,-3.65212323844896,
52.4007973486246));
#148423=CARTESIAN_POINT('Ctrl Pts',(-6.08297959063358,-3.48640012942223,
52.3921253971267));
#148424=CARTESIAN_POINT('Ctrl Pts',(-6.17796184905218,-3.3206775737819,
52.3834534745865));
#148425=CARTESIAN_POINT('Ctrl Pts',(-6.26616793897898,-3.15107148726813,
52.3747815520462));
#148426=CARTESIAN_POINT('Ctrl Pts',(-6.34730354929467,-2.97814778270175,
52.3661096295059));
#148427=CARTESIAN_POINT('Ctrl Pts',(-6.42843889529886,-2.80522464146042,
52.3574377352158));
#148428=CARTESIAN_POINT('Ctrl Pts',(-6.50250368714325,-2.62898416091396,
52.3487658409256));
#148429=CARTESIAN_POINT('Ctrl Pts',(-6.56925079960179,-2.4500143865764,
52.3400939466354));
#148430=CARTESIAN_POINT('Ctrl Pts',(-6.63599770006617,-2.2710451806611,
52.3314220798879));
#148431=CARTESIAN_POINT('Ctrl Pts',(-6.69542686840853,-2.08934696440795,
52.3227502131404));
#148432=CARTESIAN_POINT('Ctrl Pts',(-6.74734001400929,-1.90552598981205,
52.3140783463928));
#148433=CARTESIAN_POINT('Ctrl Pts',(-6.79925299896423,-1.7217055840522,
52.3054065064805));
#148434=CARTESIAN_POINT('Ctrl Pts',(-6.84364993053248,-1.53576270641118,
52.2967346665681));
#148435=CARTESIAN_POINT('Ctrl Pts',(-6.88038267538351,-1.34831776773224,
52.2880628266558));
#148436=CARTESIAN_POINT('Ctrl Pts',(-6.91711530956076,-1.1608733938148,
52.2793910128712));
#148437=CARTESIAN_POINT('Ctrl Pts',(-6.94618374861406,-0.971927246617174,
52.2707191990867));
#148438=CARTESIAN_POINT('Ctrl Pts',(-6.96749100433688,-0.782109753797198,
52.2620473853021));
#148439=CARTESIAN_POINT('Ctrl Pts',(-6.98879819760004,-0.592292817404362,
52.2533755969379));
#148440=CARTESIAN_POINT('Ctrl Pts',(-7.00234422137968,-0.401604822726262,
52.2447038085737));
#148441=CARTESIAN_POINT('Ctrl Pts',(-7.00808387899857,-0.210682005449926,
52.2360320202095));
#148442=CARTESIAN_POINT('Ctrl Pts',(-7.01382352026046,-0.0197597322696063,
52.2273602565584));
#148443=CARTESIAN_POINT('Ctrl Pts',(-7.01175683134598,0.171397078303853,
52.2186884929073));
#148444=CARTESIAN_POINT('Ctrl Pts',(-7.00189070777973,0.362150629997999,
52.2100167292562));
#148445=CARTESIAN_POINT('Ctrl Pts',(-6.99157808297264,0.561536923513271,
52.2009525163108));
#148446=CARTESIAN_POINT('Ctrl Pts',(-6.97274368607548,0.760482277943844,
52.1918883033654));
#148447=CARTESIAN_POINT('Ctrl Pts',(-6.94545616842832,0.958261537859603,
52.1828240904201));
#148448=CARTESIAN_POINT('Ctrl Pts',(-6.91902138570762,1.14986019590305,
52.1740431341293));
#148449=CARTESIAN_POINT('Ctrl Pts',(-6.88465388689313,1.34036422799509,
52.1652621778384));
#148450=CARTESIAN_POINT('Ctrl Pts',(-6.84247124235259,1.52912192452984,
52.1564812215476));
#148451=CARTESIAN_POINT('Ctrl Pts',(-6.80080846652329,1.71555332736007,
52.1478084838021));
#148452=CARTESIAN_POINT('Ctrl Pts',(-6.75152215882549,1.90028091508584,
52.1391357460566));
#148453=CARTESIAN_POINT('Ctrl Pts',(-6.69477680033957,2.08268820425313,
52.1304630083111));
#148454=CARTESIAN_POINT('Ctrl Pts',(-6.6380320137316,2.26509365512544,52.1217903579692));
#148455=CARTESIAN_POINT('Ctrl Pts',(-6.57382841116684,2.44517858291594,
52.1131177076273));
#148456=CARTESIAN_POINT('Ctrl Pts',(-6.50238025225956,2.62234201002176,
52.1044450572854));
#148457=CARTESIAN_POINT('Ctrl Pts',(-6.43093279007722,2.79950370952282,
52.0957724915146));
#148458=CARTESIAN_POINT('Ctrl Pts',(-6.35224101918992,2.97374370184175,
52.0870999257439));
#148459=CARTESIAN_POINT('Ctrl Pts',(-6.26656754386446,3.14448052636435,
52.0784273599731));
#148460=CARTESIAN_POINT('Ctrl Pts',(-6.18089487601213,3.31521574169113,
52.0697548759413));
#148461=CARTESIAN_POINT('Ctrl Pts',(-6.08824076282231,3.48244760135432,
52.0610823919095));
#148462=CARTESIAN_POINT('Ctrl Pts',(-5.98891439681922,3.64561804226272,
52.0524099078778));
#148463=CARTESIAN_POINT('Ctrl Pts',(-5.88958893454311,3.80878699855495,
52.0437375027531));
#148464=CARTESIAN_POINT('Ctrl Pts',(-5.78359148866003,3.96789436736326,
52.0350650976284));
#148465=CARTESIAN_POINT('Ctrl Pts',(-5.67127577279305,4.12240920717856,
52.0263926925038));
#148466=CARTESIAN_POINT('Ctrl Pts',(-5.55896104217497,4.27692269156845,
52.0177203634547));
#148467=CARTESIAN_POINT('Ctrl Pts',(-5.44032831951973,4.42684349778754,
52.0090480344055));
#148468=CARTESIAN_POINT('Ctrl Pts',(-5.315773475448,4.57167134866708,52.0003757053564));
#148469=CARTESIAN_POINT('Ctrl Pts',(-5.19121968333332,4.71649797636917,
51.9917034495515));
#148470=CARTESIAN_POINT('Ctrl Pts',(-5.06074405512257,4.85623151942566,
51.9830311937465));
#148471=CARTESIAN_POINT('Ctrl Pts',(-4.92478197318899,4.9904057028515,51.9743589379416));
#148472=CARTESIAN_POINT('Ctrl Pts',(-4.78882099517946,5.12457879686986,
51.9656867525497));
#148473=CARTESIAN_POINT('Ctrl Pts',(-4.64737385477877,5.25319242205333,
51.9570145671579));
#148474=CARTESIAN_POINT('Ctrl Pts',(-4.5009125373951,5.37581741628374,51.948342381766));
#148475=CARTESIAN_POINT('Ctrl Pts',(-4.35445236138306,5.49844145489876,
51.9396702639564));
#148476=CARTESIAN_POINT('Ctrl Pts',(-4.20297830437828,5.61507677360063,
51.9309981461468));
#148477=CARTESIAN_POINT('Ctrl Pts',(-4.04699580205975,5.7253341859328,51.9223260283373));
#148478=CARTESIAN_POINT('Ctrl Pts',(-3.89101446440741,5.83559077501185,
51.9136539752793));
#148479=CARTESIAN_POINT('Ctrl Pts',(-3.73052498075225,5.93946938906285,
51.9049819222214));
#148480=CARTESIAN_POINT('Ctrl Pts',(-3.56606286128402,6.0366234131235,51.8963098691634));
#148481=CARTESIAN_POINT('Ctrl Pts',(-3.40160191612828,6.13377674347314,
51.8876378780267));
#148482=CARTESIAN_POINT('Ctrl Pts',(-3.2331686364727,6.22420543545189,51.87896588689));
#148483=CARTESIAN_POINT('Ctrl Pts',(-3.06132503079727,6.30760775717023,
51.8702938957533));
#148484=CARTESIAN_POINT('Ctrl Pts',(-2.88948259606659,6.39100951058399,
51.8616219637077));
#148485=CARTESIAN_POINT('Ctrl Pts',(-2.71423013733688,6.46738486553251,
51.852950031662));
#148486=CARTESIAN_POINT('Ctrl Pts',(-2.53615240856665,6.53647898512812,
51.8442780996164));
#148487=CARTESIAN_POINT('Ctrl Pts',(-2.35807583511529,6.60557265646028,
51.8356062238319));
#148488=CARTESIAN_POINT('Ctrl Pts',(-2.17717429308471,6.66738508423366,
51.8269343480473));
#148489=CARTESIAN_POINT('Ctrl Pts',(-1.99405137755352,6.72171002544568,
51.8182624722628));
#148490=CARTESIAN_POINT('Ctrl Pts',(-1.81092959032436,6.77603463193748,
51.8095906499095));
#148491=CARTESIAN_POINT('Ctrl Pts',(-1.62558672926026,6.82287176341322,
51.8009188275563));
#148492=CARTESIAN_POINT('Ctrl Pts',(-1.43864120070719,6.86206514528446,
51.7922470052031));
#148493=CARTESIAN_POINT('Ctrl Pts',(-1.25169676301637,6.90125829845495,
51.7835752334515));
#148494=CARTESIAN_POINT('Ctrl Pts',(-1.06314995450457,6.93280773300226,
51.7749034617));
#148495=CARTESIAN_POINT('Ctrl Pts',(-0.873629864324986,6.95660818378177,
51.7662316899485));
#148496=CARTESIAN_POINT('Ctrl Pts',(-0.67949550971221,6.98098810649707,
51.75734878571));
#148497=CARTESIAN_POINT('Ctrl Pts',(-0.484340182087299,6.99723686027479,
51.7484658814715));
#148498=CARTESIAN_POINT('Ctrl Pts',(-0.288847078972072,7.00529756166498,
51.739582977233));
#148499=CARTESIAN_POINT('Ctrl Pts',(-0.0979805523976308,7.01316749698026,
51.7309102974767));
#148500=CARTESIAN_POINT('Ctrl Pts',(0.093207647885845,7.01323255451608,
51.7222376177203));
#148501=CARTESIAN_POINT('Ctrl Pts',(0.284079486223013,7.00549251716161,
51.713564937964));
#148502=CARTESIAN_POINT('Ctrl Pts',(0.474947621914736,6.99775262995299,
51.7048924264455));
#148503=CARTESIAN_POINT('Ctrl Pts',(0.665499124050418,6.9822079623472,51.6962199149269));
#148504=CARTESIAN_POINT('Ctrl Pts',(0.85509810641837,6.95891038819295,51.6875474034084));
#148505=CARTESIAN_POINT('Ctrl Pts',(1.04469365841483,6.93561323555644,51.6788750487996));
#148506=CARTESIAN_POINT('Ctrl Pts',(1.23333644315321,6.90456349171677,51.6702026941909));
#148507=CARTESIAN_POINT('Ctrl Pts',(1.42039696672693,6.86586476850607,51.6615303395821));
#148508=CARTESIAN_POINT('Ctrl Pts',(1.60745435009168,6.8271666949358,51.6528581305573));
#148509=CARTESIAN_POINT('Ctrl Pts',(1.79292924726155,6.78081995649372,51.6441859215325));
#148510=CARTESIAN_POINT('Ctrl Pts',(1.97620275621103,6.72697920532269,51.6355137125076));
#148511=CARTESIAN_POINT('Ctrl Pts',(2.15947342778489,6.67313928769513,51.6268416377429));
#148512=CARTESIAN_POINT('Ctrl Pts',(2.34054250680423,6.61180566956803,51.6181695629781));
#148513=CARTESIAN_POINT('Ctrl Pts',(2.51880581148969,6.54318300573244,51.6094974882134));
#148514=CARTESIAN_POINT('Ctrl Pts',(2.69706658905806,6.47456131471348,51.6008255363867));
#148515=CARTESIAN_POINT('Ctrl Pts',(2.87252140681914,6.39865088680132,51.59215358456));
#148516=CARTESIAN_POINT('Ctrl Pts',(3.04458483294752,6.31570500874494,51.5834816327333));
#148517=CARTESIAN_POINT('Ctrl Pts',(3.21664604442681,6.23276019829495,51.5748097925244));
#148518=CARTESIAN_POINT('Ctrl Pts',(3.38531569578744,6.14278024223816,51.5661379523155));
#148519=CARTESIAN_POINT('Ctrl Pts',(3.55003100942206,6.04606536473447,51.5574661121065));
#148520=CARTESIAN_POINT('Ctrl Pts',(3.72225670716014,5.94494066119492,51.548398869373));
#148521=CARTESIAN_POINT('Ctrl Pts',(3.89015872998584,5.8364526481967,51.5393316266394));
#148522=CARTESIAN_POINT('Ctrl Pts',(4.05312466659795,5.72099702844839,51.5302643839059));
#148523=CARTESIAN_POINT('Ctrl Pts',(4.20899688867971,5.61056705531338,51.5215918275275));
#148524=CARTESIAN_POINT('Ctrl Pts',(4.36035338103854,5.49376336253657,51.512919271149));
#148525=CARTESIAN_POINT('Ctrl Pts',(4.50668904925033,5.37097573778426,51.5042467147706));
#148526=CARTESIAN_POINT('Ctrl Pts',(4.65301950884067,5.24819248349244,51.4955744670802));
#148527=CARTESIAN_POINT('Ctrl Pts',(4.79432928426973,5.11942590603987,51.4869022193897));
#148528=CARTESIAN_POINT('Ctrl Pts',(4.93014684172531,4.98510568408795,51.4782299716993));
#148529=CARTESIAN_POINT('Ctrl Pts',(5.06596027419871,4.85078954164189,51.469557987398));
#148530=CARTESIAN_POINT('Ctrl Pts',(5.19628162053444,4.71092029195547,51.4608860030966));
#148531=CARTESIAN_POINT('Ctrl Pts',(5.32067604038165,4.56596463365724,51.4522140187953));
#148532=CARTESIAN_POINT('Ctrl Pts',(5.44506733164383,4.42101262106999,51.443542252599));
#148533=CARTESIAN_POINT('Ctrl Pts',(5.56353180975687,4.27097467138573,51.4348704864026));
#148534=CARTESIAN_POINT('Ctrl Pts',(5.67567421678232,4.11635138775256,51.4261987202062));
#148535=CARTESIAN_POINT('Ctrl Pts',(5.78782406006177,3.96171785092399,51.417526378978));
#148536=CARTESIAN_POINT('Ctrl Pts',(5.8936508265435,3.80249860162274,51.4088540377498));
#148537=CARTESIAN_POINT('Ctrl Pts',(5.99280137736038,3.6392249468819,51.4001816965216));
#148538=CARTESIAN_POINT('Ctrl Pts',(6.09194609290926,3.47596090122063,51.3915098656832));
#148539=CARTESIAN_POINT('Ctrl Pts',(6.18441523160539,3.3086431703667,51.3828380348449));
#148540=CARTESIAN_POINT('Ctrl Pts',(6.2699002646301,3.13783001994872,51.3741662040065));
#148541=CARTESIAN_POINT('Ctrl Pts',(6.35538670852435,2.96701405038144,51.3654942300458));
#148542=CARTESIAN_POINT('Ctrl Pts',(6.43388868897073,2.79270279979511,51.356822256085));
#148543=CARTESIAN_POINT('Ctrl Pts',(6.50514427077325,2.61547788729441,51.3481502821243));
#148544=CARTESIAN_POINT('Ctrl Pts',(6.52787183386237,2.55895052090526,51.3453842835833));
#148545=CARTESIAN_POINT('Ctrl Pts',(6.5498625512973,2.50212689663976,51.3426182850424));
#148546=CARTESIAN_POINT('Ctrl Pts',(6.57110895151816,2.4450263208763,51.3398522865015));
#148547=CARTESIAN_POINT('Origin',(0.,0.,50.));
#148548=CARTESIAN_POINT('',(6.57110895151812,2.44502632087642,49.3398351631816));
#148549=CARTESIAN_POINT('',(6.57110895151815,2.44502632087633,49.8869210003222));
#148550=CARTESIAN_POINT('',(6.57110895151814,2.44502632087636,50.));
#148551=CARTESIAN_POINT('',(7.01125,3.46460097481842E-12,51.7735343569105));
#148552=CARTESIAN_POINT('Ctrl Pts',(6.57110895151815,2.44502632087633,49.8869210003222));
#148553=CARTESIAN_POINT('Ctrl Pts',(6.50449838733148,2.62404495591329,49.895592809261));
#148554=CARTESIAN_POINT('Ctrl Pts',(6.43056821795871,2.80033990715968,49.9042646181997));
#148555=CARTESIAN_POINT('Ctrl Pts',(6.34956511459254,2.97332295892145,49.9129364271385));
#148556=CARTESIAN_POINT('Ctrl Pts',(6.26856213015516,3.14630575670943,49.9216082233453));
#148557=CARTESIAN_POINT('Ctrl Pts',(6.18048635294282,3.31597640754664,49.9302800195521));
#148558=CARTESIAN_POINT('Ctrl Pts',(6.08563165071566,3.48176879966316,49.938951815759));
#148559=CARTESIAN_POINT('Ctrl Pts',(5.99077708581972,3.64756095174443,49.9476235994107));
#148560=CARTESIAN_POINT('Ctrl Pts',(5.88914375658112,3.80947460983729,49.9562953830624));
#148561=CARTESIAN_POINT('Ctrl Pts',(5.78107076500233,3.96696954519888,49.9649671667142));
#148562=CARTESIAN_POINT('Ctrl Pts',(5.67299792768882,4.12446425574944,49.9736389379876));
#148563=CARTESIAN_POINT('Ctrl Pts',(5.55848560711395,4.27754002202474,49.9823107092611));
#148564=CARTESIAN_POINT('Ctrl Pts',(5.43791587524921,4.42568610457323,49.9909824805346));
#148565=CARTESIAN_POINT('Ctrl Pts',(5.31734631302949,4.573831978676,49.9996542396066));
#148566=CARTESIAN_POINT('Ctrl Pts',(5.19071953583903,4.71704796266761,50.0083259986787));
#148567=CARTESIAN_POINT('Ctrl Pts',(5.05845803451681,4.85485621574237,50.0169977577508));
#148568=CARTESIAN_POINT('Ctrl Pts',(4.9261967165929,4.99266427772752,50.0256695047983));
#148569=CARTESIAN_POINT('Ctrl Pts',(4.78830088681858,5.12506441890826,50.0343412518457));
#148570=CARTESIAN_POINT('Ctrl Pts',(4.64523063400523,5.25161488681333,50.0430129988932));
#148571=CARTESIAN_POINT('Ctrl Pts',(4.49652806262455,5.38314733060835,50.0520261309662));
#148572=CARTESIAN_POINT('Ctrl Pts',(4.34223563524025,5.50835996364214,50.0610392630393));
#148573=CARTESIAN_POINT('Ctrl Pts',(4.18290943344624,5.62680151010203,50.0700523951123));
#148574=CARTESIAN_POINT('Ctrl Pts',(4.0260727035553,5.74339240739846,50.0789246969966));
#148575=CARTESIAN_POINT('Ctrl Pts',(3.8643586282048,5.85342208902574,50.087796998881));
#148576=CARTESIAN_POINT('Ctrl Pts',(3.69833198496549,5.95650628233373,50.0966693007654));
#148577=CARTESIAN_POINT('Ctrl Pts',(3.5348995080268,6.05797978512129,50.1054029729328));
#148578=CARTESIAN_POINT('Ctrl Pts',(3.36728850947182,6.15272311279854,50.1141366451002));
#148579=CARTESIAN_POINT('Ctrl Pts',(3.19606623001071,6.24041562845658,50.1228703172676));
#148580=CARTESIAN_POINT('Ctrl Pts',(3.02603797481211,6.32749661743909,50.1315430848816));
#148581=CARTESIAN_POINT('Ctrl Pts',(2.85244891335465,6.40762471321549,50.1402158524956));
#148582=CARTESIAN_POINT('Ctrl Pts',(2.67587836095273,6.48053250588908,50.1488886201096));
#148583=CARTESIAN_POINT('Ctrl Pts',(2.49930871513574,6.55343992422444,50.1575613431941));
#148584=CARTESIAN_POINT('Ctrl Pts',(2.31975787165094,6.6191270051938,50.1662340662785));
#148585=CARTESIAN_POINT('Ctrl Pts',(2.137825035802,6.6773745348601,50.174906789363));
#148586=CARTESIAN_POINT('Ctrl Pts',(1.95589311921941,6.73562177021454,50.1835794686261));
#148587=CARTESIAN_POINT('Ctrl Pts',(1.77157950497145,6.78642944284865,50.1922521478893));
#148588=CARTESIAN_POINT('Ctrl Pts',(1.58549928668899,6.82962799678055,50.2009248271524));
#148589=CARTESIAN_POINT('Ctrl Pts',(1.39941999343982,6.87282633596582,50.2095974633023));
#148590=CARTESIAN_POINT('Ctrl Pts',(1.21157439050756,6.90841556788897,50.2182700994522));
#148591=CARTESIAN_POINT('Ctrl Pts',(1.02258935229219,6.93627692491286,50.2269427356021));
#148592=CARTESIAN_POINT('Ctrl Pts',(0.833605238125191,6.96413814570776,
50.2356153293469));
#148593=CARTESIAN_POINT('Ctrl Pts',(0.643481980916576,6.98427152577614,
50.2442879230917));
#148594=CARTESIAN_POINT('Ctrl Pts',(0.452854049808002,6.99660987708137,
50.2529605168364));
#148595=CARTESIAN_POINT('Ctrl Pts',(0.262227035221766,7.00894816906488,
50.2616330688842));
#148596=CARTESIAN_POINT('Ctrl Pts',(0.0710956351219621,7.01349148893087,
50.2703056209319));
#148597=CARTESIAN_POINT('Ctrl Pts',(-0.119902323156486,7.01022467510148,
50.2789781729796));
#148598=CARTESIAN_POINT('Ctrl Pts',(-0.310899378721912,7.00695787671203,
50.2876506840382));
#148599=CARTESIAN_POINT('Ctrl Pts',(-0.501762709652217,6.99588102335287,
50.2963231950969));
#148600=CARTESIAN_POINT('Ctrl Pts',(-0.691855389204572,6.97703107940108,
50.3049957061555));
#148601=CARTESIAN_POINT('Ctrl Pts',(-0.881947185836504,6.95818122300132,
50.3136681769331));
#148602=CARTESIAN_POINT('Ctrl Pts',(-1.07126805552919,6.93155837629142,
50.3223406477107));
#148603=CARTESIAN_POINT('Ctrl Pts',(-1.25918622472362,6.89725138109133,
50.3310131184883));
#148604=CARTESIAN_POINT('Ctrl Pts',(-1.44710353643389,6.86294454243654,
50.3396855496928));
#148605=CARTESIAN_POINT('Ctrl Pts',(-1.63361788096937,6.82095367648074,
50.3483579808972));
#148606=CARTESIAN_POINT('Ctrl Pts',(-1.81810685596554,6.77141890764344,
50.3570304121017));
#148607=CARTESIAN_POINT('Ctrl Pts',(-2.00259500418079,6.72188436079449,
50.365702804441));
#148608=CARTESIAN_POINT('Ctrl Pts',(-2.18505752664021,6.66480605238715,
50.3743751967802));
#148609=CARTESIAN_POINT('Ctrl Pts',(-2.36488554744824,6.60037445225424,
50.3830475891195));
#148610=CARTESIAN_POINT('Ctrl Pts',(-2.54471277703807,6.53594313561138,
50.3917199433015));
#148611=CARTESIAN_POINT('Ctrl Pts',(-2.7219052607291,6.46415868780939,50.4003922974834));
#148612=CARTESIAN_POINT('Ctrl Pts',(-2.89587171389858,6.38526065083815,
50.4090646516654));
#148613=CARTESIAN_POINT('Ctrl Pts',(-3.06983741583593,6.30636295456905,
50.4177369683979));
#148614=CARTESIAN_POINT('Ctrl Pts',(-3.24057685640759,6.22035184793775,
50.4264092851304));
#148615=CARTESIAN_POINT('Ctrl Pts',(-3.40752028946761,6.12751434428077,
50.4350816018628));
#148616=CARTESIAN_POINT('Ctrl Pts',(-3.57446301524526,6.03467723394461,
50.4437538818537));
#148617=CARTESIAN_POINT('Ctrl Pts',(-3.73760951742141,5.93501392252171,
50.4524261618445));
#148618=CARTESIAN_POINT('Ctrl Pts',(-3.89641539158832,5.82885697703192,
50.4610984418354));
#148619=CARTESIAN_POINT('Ctrl Pts',(-4.05522060590707,5.72270047263075,
50.4697706857923));
#148620=CARTESIAN_POINT('Ctrl Pts',(-4.20968499214109,5.61005054602573,
50.4784429297493));
#148621=CARTESIAN_POINT('Ctrl Pts',(-4.35929312155931,5.49128309621947,
50.4871151737063));
#148622=CARTESIAN_POINT('Ctrl Pts',(-4.50890064155372,5.37251613020852,
50.4957873823372));
#148623=CARTESIAN_POINT('Ctrl Pts',(-4.65365172183319,5.24763186748397,
50.5044595909681));
#148624=CARTESIAN_POINT('Ctrl Pts',(-4.79306334970965,5.11704702813743,
50.513131799599));
#148625=CARTESIAN_POINT('Ctrl Pts',(-4.93247442107221,4.98646271006935,
50.5218039736115));
#148626=CARTESIAN_POINT('Ctrl Pts',(-5.06654587536628,4.85017805510816,
50.530476147624));
#148627=CARTESIAN_POINT('Ctrl Pts',(-5.19483033978528,4.70864782112088,
50.5391483216365));
#148628=CARTESIAN_POINT('Ctrl Pts',(-5.3231143025755,4.56711814055711,50.5478204617383));
#148629=CARTESIAN_POINT('Ctrl Pts',(-5.44561113000544,4.42034313247858,
50.5564926018401));
#148630=CARTESIAN_POINT('Ctrl Pts',(-5.56191207495125,4.26881255538487,
50.565164741942));
#148631=CARTESIAN_POINT('Ctrl Pts',(-5.67821257461588,4.11728255845596,
50.5738368488408));
#148632=CARTESIAN_POINT('Ctrl Pts',(-5.78831706632212,3.96099725428024,
50.5825089557396));
#148633=CARTESIAN_POINT('Ctrl Pts',(-5.89185815647313,3.80047813130152,
50.5911810626385));
#148634=CARTESIAN_POINT('Ctrl Pts',(-5.99539885864389,3.63995960980621,
50.5998531370419));
#148635=CARTESIAN_POINT('Ctrl Pts',(-6.09237605450623,3.47520753995041,
50.6085252114454));
#148636=CARTESIAN_POINT('Ctrl Pts',(-6.18246615568055,3.30677165772973,
50.6171972858489));
#148637=CARTESIAN_POINT('Ctrl Pts',(-6.27255592662674,3.13833639291612,
50.6258693284645));
#148638=CARTESIAN_POINT('Ctrl Pts',(-6.35575851943845,2.96621759322332,
50.6345413710802));
#148639=CARTESIAN_POINT('Ctrl Pts',(-6.43179631013648,2.79098957135543,
50.6432134136959));
#148640=CARTESIAN_POINT('Ctrl Pts',(-6.50783382831893,2.61576217749586,
50.6518854252315));
#148641=CARTESIAN_POINT('Ctrl Pts',(-6.57670648270601,2.43742584432079,
50.660557436767));
#148642=CARTESIAN_POINT('Ctrl Pts',(-6.63818446599478,2.25657562645829,
50.6692294483026));
#148643=CARTESIAN_POINT('Ctrl Pts',(-6.69966223396472,2.07572604200071,
50.6779014294655));
#148644=CARTESIAN_POINT('Ctrl Pts',(-6.75374529124755,1.89236285939156,
50.6865734106284));
#148645=CARTESIAN_POINT('Ctrl Pts',(-6.80025318023398,1.70709790205998,
50.6952453917913));
#148646=CARTESIAN_POINT('Ctrl Pts',(-6.84676091012637,1.52183357848221,
50.7039173432891));
#148647=CARTESIAN_POINT('Ctrl Pts',(-6.88569345442289,1.33466776867811,
50.712589294787));
#148648=CARTESIAN_POINT('Ctrl Pts',(-6.9169209087468,1.14622497994126,50.7212612462848));
#148649=CARTESIAN_POINT('Ctrl Pts',(-6.94814825879533,0.957782820456561,
50.7299331688251));
#148650=CARTESIAN_POINT('Ctrl Pts',(-6.97167052392505,0.768063970771273,
50.7386050913653));
#148651=CARTESIAN_POINT('Ctrl Pts',(-6.98740921903153,0.57770145256284,
50.7472770139056));
#148652=CARTESIAN_POINT('Ctrl Pts',(-7.00314786286684,0.387339554488891,
50.7559489081958));
#148653=CARTESIAN_POINT('Ctrl Pts',(-7.01110296401745,0.19633427513781,
50.764620802486));
#148654=CARTESIAN_POINT('Ctrl Pts',(-7.01124797942393,0.00532292437921427,
50.7732926967761));
#148655=CARTESIAN_POINT('Ctrl Pts',(-7.01139299436982,-0.185687819711979,
50.7819645635237));
#148656=CARTESIAN_POINT('Ctrl Pts',(-7.00372797299438,-0.376704351160972,
50.7906364302712));
#148657=CARTESIAN_POINT('Ctrl Pts',(-6.98827849031203,-0.567089326598777,
50.7993082970188));
#148658=CARTESIAN_POINT('Ctrl Pts',(-6.97282905543826,-0.757473712888272,
50.8079801369311));
#148659=CARTESIAN_POINT('Ctrl Pts',(-6.94959523043372,-0.947226264001188,
50.8166519768435));
#148660=CARTESIAN_POINT('Ctrl Pts',(-6.91865453650893,-1.13571385786402,
50.8253238167558));
#148661=CARTESIAN_POINT('Ctrl Pts',(-6.88771393580689,-1.32420088382328,
50.8339956305404));
#148662=CARTESIAN_POINT('Ctrl Pts',(-6.84906655865514,-1.51142267990746,
50.8426674443249));
#148663=CARTESIAN_POINT('Ctrl Pts',(-6.80284135383523,-1.69675457183686,
50.8513392581095));
#148664=CARTESIAN_POINT('Ctrl Pts',(-6.75661628451883,-1.88208592048857,
50.8600110464737));
#148665=CARTESIAN_POINT('Ctrl Pts',(-6.70281350071472,-2.06552710051522,
50.8686828348379));
#148666=CARTESIAN_POINT('Ctrl Pts',(-6.64161251687621,-2.24646605542423,
50.877354623202));
#148667=CARTESIAN_POINT('Ctrl Pts',(-6.58041170744959,-2.42740449468945,
50.8860263868532));
#148668=CARTESIAN_POINT('Ctrl Pts',(-6.51181283117328,-2.60584045408488,
50.8946981505043));
#148669=CARTESIAN_POINT('Ctrl Pts',(-6.4360447687628,-2.78117858056274,
50.9033699141555));
#148670=CARTESIAN_POINT('Ctrl Pts',(-6.35684774728306,-2.96445180845203,
50.9124341271008));
#148671=CARTESIAN_POINT('Ctrl Pts',(-6.26981768815725,-3.14433998862126,
50.9214983400462));
#148672=CARTESIAN_POINT('Ctrl Pts',(-6.17527181578168,-3.32018742900344,
50.9305625529916));
#148673=CARTESIAN_POINT('Ctrl Pts',(-6.08368050191785,-3.49053963687367,
50.9393435092824));
#148674=CARTESIAN_POINT('Ctrl Pts',(-5.98503618716671,-3.65709956718525,
50.9481244655732));
#148675=CARTESIAN_POINT('Ctrl Pts',(-5.87967633130162,-3.81929742251524,
50.956905421864));
#148676=CARTESIAN_POINT('Ctrl Pts',(-5.77561495477753,-3.97949631379415,
50.9655781596095));
#148677=CARTESIAN_POINT('Ctrl Pts',(-5.66500279405277,-4.13543980257547,
50.974250897355));
#148678=CARTESIAN_POINT('Ctrl Pts',(-5.54820899034624,-4.28660746534379,
50.9829236351005));
#148679=CARTESIAN_POINT('Ctrl Pts',(-5.43141636368402,-4.43777360464914,
50.9915962854424));
#148680=CARTESIAN_POINT('Ctrl Pts',(-5.3084423924273,-4.58416378940542,
51.0002689357843));
#148681=CARTESIAN_POINT('Ctrl Pts',(-5.1796974640714,-4.72528948776605,
51.0089415861262));
#148682=CARTESIAN_POINT('Ctrl Pts',(-5.05095379116855,-4.86641380994285,
51.017614151897));
#148683=CARTESIAN_POINT('Ctrl Pts',(-4.91643946526993,-5.00227353854812,
51.0262867176678));
#148684=CARTESIAN_POINT('Ctrl Pts',(-4.7766033774798,-5.13241529270076,
51.0349592834386));
#148685=CARTESIAN_POINT('Ctrl Pts',(-4.63676860764581,-5.26255582026642,
51.0436317674703));
#148686=CARTESIAN_POINT('Ctrl Pts',(-4.49161238427032,-5.38697828766175,
51.0523042515021));
#148687=CARTESIAN_POINT('Ctrl Pts',(-4.34161910267662,-5.50526748939354,
51.0609767355339));
#148688=CARTESIAN_POINT('Ctrl Pts',(-4.19162718580574,-5.62355561486398,
51.0696491406585));
#148689=CARTESIAN_POINT('Ctrl Pts',(-4.03679852186387,-5.73571041041401,
51.0783215457832));
#148690=CARTESIAN_POINT('Ctrl Pts',(-3.87764977431607,-5.84135761533623,
51.0869939509079));
#148691=CARTESIAN_POINT('Ctrl Pts',(-3.7185024228429,-5.94700389350669,
51.095666279957));
#148692=CARTESIAN_POINT('Ctrl Pts',(-3.55503530028467,-6.04614253816448,
51.1043386090061));
#148693=CARTESIAN_POINT('Ctrl Pts',(-3.38779388709415,-6.13844272931397,
51.1130109380553));
#148694=CARTESIAN_POINT('Ctrl Pts',(-3.2205538863803,-6.23074214092049,
51.1216831938602));
#148695=CARTESIAN_POINT('Ctrl Pts',(-3.04953990753596,-6.31620307732955,
51.1303554496652));
#148696=CARTESIAN_POINT('Ctrl Pts',(-2.8753226048127,-6.39454036508904,
51.1390277054701));
#148697=CARTESIAN_POINT('Ctrl Pts',(-2.70110671662106,-6.47287701680052,
51.147699890862));
#148698=CARTESIAN_POINT('Ctrl Pts',(-2.52368781567611,-6.54409001910944,
51.1563720762538));
#148699=CARTESIAN_POINT('Ctrl Pts',(-2.34365791912394,-6.60794174615876,
51.1650442616456));
#148700=CARTESIAN_POINT('Ctrl Pts',(-2.16362942554312,-6.67179297561215,
51.1737163794552));
#148701=CARTESIAN_POINT('Ctrl Pts',(-1.9809902447871,-6.72828294965083,
51.1823884972648));
#148702=CARTESIAN_POINT('Ctrl Pts',(-1.79634980371192,-6.77722317363123,
51.1910606150744));
#148703=CARTESIAN_POINT('Ctrl Pts',(-1.61171074128151,-6.82616303219231,
51.1997326681323));
#148704=CARTESIAN_POINT('Ctrl Pts',(-1.42507072299637,-6.86755318072527,
51.2084047211903));
#148705=CARTESIAN_POINT('Ctrl Pts',(-1.23705251633842,-6.90125551145013,
51.2170767742482));
#148706=CARTESIAN_POINT('Ctrl Pts',(-1.04903565219108,-6.93495760152948,
51.2257487653849));
#148707=CARTESIAN_POINT('Ctrl Pts',(-0.859640898940478,-6.96097193353402,
51.2344207565216));
#148708=CARTESIAN_POINT('Ctrl Pts',(-0.669500206861603,-6.97921170588142,
51.2430927476583));
#148709=CARTESIAN_POINT('Ctrl Pts',(-0.479360810404349,-6.99745135394274,
51.251764679704));
#148710=CARTESIAN_POINT('Ctrl Pts',(-0.288475768015695,-7.00791652123613,
51.2604366117496));
#148711=CARTESIAN_POINT('Ctrl Pts',(-0.0974819939219479,-7.01057228929001,
51.2691085437952));
#148712=CARTESIAN_POINT('Ctrl Pts',(0.0935105410576831,-7.01322804011402,
51.2777804195797));
#148713=CARTESIAN_POINT('Ctrl Pts',(0.284611522344142,-7.00807448913604,
51.2864522953643));
#148714=CARTESIAN_POINT('Ctrl Pts',(0.475183323466561,-6.9951288316656,
51.2951241711488));
#148715=CARTESIAN_POINT('Ctrl Pts',(0.665753950390968,-6.98218325395913,
51.3037959935021));
#148716=CARTESIAN_POINT('Ctrl Pts',(0.855795120323774,-6.96144568508285,
51.3124678158553));
#148717=CARTESIAN_POINT('Ctrl Pts',(1.04467275076075,-6.93298531704186,
51.3211396382086));
#148718=CARTESIAN_POINT('Ctrl Pts',(1.23354927906118,-6.90452511507248,
51.3298114099601));
#148719=CARTESIAN_POINT('Ctrl Pts',(1.42126200062561,-6.86834224643157,
51.3384831817116));
#148720=CARTESIAN_POINT('Ctrl Pts',(1.60718460924404,-6.82455743578359,
51.3471549534632));
#148721=CARTESIAN_POINT('Ctrl Pts',(1.79763389405547,-6.77970659200791,
51.3560378577016));
#148722=CARTESIAN_POINT('Ctrl Pts',(1.98620448431563,-6.72687898190959,
51.3649207619401));
#148723=CARTESIAN_POINT('Ctrl Pts',(2.1722362342754,-6.66625954377723,51.3738036661786));
#148724=CARTESIAN_POINT('Ctrl Pts',(2.3538653218573,-6.60707473666721,51.382476345935));
#148725=CARTESIAN_POINT('Ctrl Pts',(2.53307410227384,-6.54046283696636,
51.3911490256913));
#148726=CARTESIAN_POINT('Ctrl Pts',(2.70926451773964,-6.46664614274022,
51.3998217054477));
#148727=CARTESIAN_POINT('Ctrl Pts',(2.8854515153589,-6.39283088045425,51.4084942169662));
#148728=CARTESIAN_POINT('Ctrl Pts',(3.05862000314123,-6.31181121311156,
51.4171667284847));
#148729=CARTESIAN_POINT('Ctrl Pts',(3.22819210343966,-6.22385751008085,
51.4258392400033));
#148730=CARTESIAN_POINT('Ctrl Pts',(3.39776113570845,-6.13590539837659,
51.434511594612));
#148731=CARTESIAN_POINT('Ctrl Pts',(3.5637336585096,-6.04101963284044,51.4431839492208));
#148732=CARTESIAN_POINT('Ctrl Pts',(3.72555582775144,-5.93951684371779,
51.4518563038295));
#148733=CARTESIAN_POINT('Ctrl Pts',(3.88737528046379,-5.83801575853546,
51.4605285128544));
#148734=CARTESIAN_POINT('Ctrl Pts',(4.04504427838822,-5.72989802299727,
51.4692007218792));
#148735=CARTESIAN_POINT('Ctrl Pts',(4.1980367036313,-5.61552440983604,51.477872930904));
#148736=CARTESIAN_POINT('Ctrl Pts',(4.35102676029984,-5.50115256736659,
51.4865450056688));
#148737=CARTESIAN_POINT('Ctrl Pts',(4.49934016166372,-5.38052521116008,
51.4952170804335));
#148738=CARTESIAN_POINT('Ctrl Pts',(4.64248202336599,-5.25404484423417,
51.5038891551983));
#148739=CARTESIAN_POINT('Ctrl Pts',(4.78562185584416,-5.12756627033376,
51.512561107025));
#148740=CARTESIAN_POINT('Ctrl Pts',(4.92359008252347,-4.99523503982289,
51.5212330588517));
#148741=CARTESIAN_POINT('Ctrl Pts',(5.05592635132112,-4.85749269608475,
51.5299050106784));
#148742=CARTESIAN_POINT('Ctrl Pts',(5.18826091680221,-4.71975212524545,
51.5385768508873));
#148743=CARTESIAN_POINT('Ctrl Pts',(5.3149634726937,-4.57660078535456,51.5472486910962));
#148744=CARTESIAN_POINT('Ctrl Pts',(5.43561126741774,-4.42851631046125,
51.5559205313051));
#148745=CARTESIAN_POINT('Ctrl Pts',(5.56176013705507,-4.27367975367746,
51.5649877740387));
#148746=CARTESIAN_POINT('Ctrl Pts',(5.68128895686456,-4.11344992041185,
51.5740550167723));
#148747=CARTESIAN_POINT('Ctrl Pts',(5.79376175353962,-3.94841123817182,
51.5831222595058));
#148748=CARTESIAN_POINT('Ctrl Pts',(5.90133874236269,-3.79055649462878,
51.5917948158842));
#148749=CARTESIAN_POINT('Ctrl Pts',(6.00246078174151,-3.62830291661796,
51.6004673722627));
#148750=CARTESIAN_POINT('Ctrl Pts',(6.09679041553231,-3.46219196342049,
51.6091399286411));
#148751=CARTESIAN_POINT('Ctrl Pts',(6.19111669178666,-3.29608692271898,
51.6178121763316));
#148752=CARTESIAN_POINT('Ctrl Pts',(6.2786509059623,-3.12612502860927,51.626484424022));
#148753=CARTESIAN_POINT('Ctrl Pts',(6.35910096686043,-2.9528734235952,51.6351566717125));
#148754=CARTESIAN_POINT('Ctrl Pts',(6.43954858436979,-2.77962708049169,
51.6438286560138));
#148755=CARTESIAN_POINT('Ctrl Pts',(6.5129123595191,-2.60309148404068,51.6525006403151));
#148756=CARTESIAN_POINT('Ctrl Pts',(6.57894750102417,-2.42385567665813,
51.6611726246164));
#148757=CARTESIAN_POINT('Ctrl Pts',(6.6449809817109,-2.24462437714989,51.6698443908127));
#148758=CARTESIAN_POINT('Ctrl Pts',(6.70368609940859,-2.06269326910016,
51.6785161570091));
#148759=CARTESIAN_POINT('Ctrl Pts',(6.75486698389381,-1.87866936750494,
51.6871879232055));
#148760=CARTESIAN_POINT('Ctrl Pts',(6.80605126222495,-1.69463326313567,
51.6958602644337));
#148761=CARTESIAN_POINT('Ctrl Pts',(6.84971023276614,-1.50850436117982,
51.7045326056619));
#148762=CARTESIAN_POINT('Ctrl Pts',(6.88569820761715,-1.3209037648966,51.7132049468901));
#148763=CARTESIAN_POINT('Ctrl Pts',(6.92168406448219,-1.13331420939665,
51.7218767777285));
#148764=CARTESIAN_POINT('Ctrl Pts',(6.9499997755378,-0.944253411829444,
51.7305486085668));
#148765=CARTESIAN_POINT('Ctrl Pts',(6.9705508637184,-0.754352184867711,
51.7392204394052));
#148766=CARTESIAN_POINT('Ctrl Pts',(6.99110229108004,-0.564447823721784,
51.7478924133659));
#148767=CARTESIAN_POINT('Ctrl Pts',(7.0038888085648,-0.373703287796009,
51.7565643873266));
#148768=CARTESIAN_POINT('Ctrl Pts',(7.00886775178455,-0.182755028643803,
51.7652363612874));
#148769=CARTESIAN_POINT('Ctrl Pts',(7.01045582731892,-0.121850486192426,
51.7680023598284));
#148770=CARTESIAN_POINT('Ctrl Pts',(7.01125000000003,-0.0609252433289545,
51.7707683583695));
#148771=CARTESIAN_POINT('Ctrl Pts',(7.01125,3.46460095547362E-12,51.7735343569105));
#148772=CARTESIAN_POINT('Ctrl Pts',(7.01124999999651,-6.99800587777282E-6,
51.7736935453439));
#148773=CARTESIAN_POINT('Ctrl Pts',(7.01125016734379,0.167656998790483,
51.7812920136671));
#148774=CARTESIAN_POINT('Ctrl Pts',(7.00523183104702,0.335486844567159,
51.7888904819904));
#148775=CARTESIAN_POINT('Ctrl Pts',(6.99318534782853,0.502976394492236,
51.7964889503137));
#148776=CARTESIAN_POINT('Ctrl Pts',(6.98114140614357,0.670430607937701,
51.8040858155332));
#148777=CARTESIAN_POINT('Ctrl Pts',(6.96307186471559,0.837544268886115,
51.8116826807527));
#148778=CARTESIAN_POINT('Ctrl Pts',(6.9390191791175,1.00381242985907,51.8192795459723));
#148779=CARTESIAN_POINT('Ctrl Pts',(6.91496982024836,1.17005759426877,51.8268753604687));
#148780=CARTESIAN_POINT('Ctrl Pts',(6.88493902506947,1.33545709566369,51.8344711749652));
#148781=CARTESIAN_POINT('Ctrl Pts',(6.8490208902499,1.49951305676892,51.8420669894617));
#148782=CARTESIAN_POINT('Ctrl Pts',(6.81309084638302,1.66362341240805,51.8496653224329));
#148783=CARTESIAN_POINT('Ctrl Pts',(6.77126965611079,1.82638894818059,51.8572636554041));
#148784=CARTESIAN_POINT('Ctrl Pts',(6.72370207982196,1.98732405618659,51.8648619883752));
#148785=CARTESIAN_POINT('Ctrl Pts',(6.7009547367353,2.06428501157083,51.8684955955604));
#148786=CARTESIAN_POINT('Ctrl Pts',(6.67689401063677,2.14082759811051,51.8721292027455));
#148787=CARTESIAN_POINT('Ctrl Pts',(6.65153969883759,2.21690013245694,51.8757628099306));
#148788=CARTESIAN_POINT('Ctrl Pts',(6.62603162985497,2.29343399656497,51.8794184525475));
#148789=CARTESIAN_POINT('Ctrl Pts',(6.59921527121467,2.36948942895206,51.8830740951643));
#148790=CARTESIAN_POINT('Ctrl Pts',(6.57110895151814,2.44502632087637,51.8867297377812));
#148791=CARTESIAN_POINT('',(7.01124899179693,-0.00375999023141351,51.2264656430896));
#148792=CARTESIAN_POINT('Ctrl Pts',(6.57110895151816,2.4450263208763,51.3398522865015));
#148793=CARTESIAN_POINT('Ctrl Pts',(6.63771924680899,2.266008408508,51.3311805125694));
#148794=CARTESIAN_POINT('Ctrl Pts',(6.69700989700473,2.08426710051955,51.3225087386372));
#148795=CARTESIAN_POINT('Ctrl Pts',(6.74878307789422,1.90040877971785,51.3138369647051));
#148796=CARTESIAN_POINT('Ctrl Pts',(6.80055978789531,1.71653792623954,51.3051645996628));
#148797=CARTESIAN_POINT('Ctrl Pts',(6.84481792613573,1.53055004459453,51.2964922346204));
#148798=CARTESIAN_POINT('Ctrl Pts',(6.88140980451098,1.3430657708691,51.2878198695781));
#148799=CARTESIAN_POINT('Ctrl Pts',(6.91799949925383,1.15559268532943,51.2791480220619));
#148800=CARTESIAN_POINT('Ctrl Pts',(6.94692379517689,0.966623665170781,
51.2704761745458));
#148801=CARTESIAN_POINT('Ctrl Pts',(6.96808618426389,0.776789219267855,
51.2618043270297));
#148802=CARTESIAN_POINT('Ctrl Pts',(6.98924897510677,0.586951169466182,
51.2531323148835));
#148803=CARTESIAN_POINT('Ctrl Pts',(7.00264953276857,0.396247943319445,
51.2444603027373));
#148804=CARTESIAN_POINT('Ctrl Pts',(7.00824314361839,0.205315860142146,
51.2357882905911));
#148805=CARTESIAN_POINT('Ctrl Pts',(7.01024757124657,0.136896809746564,
51.2326807414239));
#148806=CARTESIAN_POINT('Ctrl Pts',(7.01125,0.0684484052929644,51.2295731922568));
#148807=CARTESIAN_POINT('Ctrl Pts',(7.01125,8.58630487052188E-16,51.2264656430896));
#148808=CARTESIAN_POINT('Ctrl Pts',(7.01124899179693,-0.00375999023141351,
51.2264656430896));
#148809=CARTESIAN_POINT('Ctrl Pts',(7.01114686516534,-0.194195389987069,
51.2178782345103));
#148810=CARTESIAN_POINT('Ctrl Pts',(7.00328188214509,-0.384378067801461,
51.209290825931));
#148811=CARTESIAN_POINT('Ctrl Pts',(6.9877404724221,-0.573680793276399,
51.2007034173516));
#148812=CARTESIAN_POINT('Ctrl Pts',(6.97216474589871,-0.763401515828795,
51.1920970470184));
#148813=CARTESIAN_POINT('Ctrl Pts',(6.94887874818298,-0.952238122132306,
51.1834906766853));
#148814=CARTESIAN_POINT('Ctrl Pts',(6.9180198950668,-1.13957329468532,51.1748843063521));
#148815=CARTESIAN_POINT('Ctrl Pts',(6.88705732364092,-1.32753811110005,
51.1662490095328));
#148816=CARTESIAN_POINT('Ctrl Pts',(6.84847101251243,-1.51399111503323,
51.1576137127136));
#148817=CARTESIAN_POINT('Ctrl Pts',(6.80244897060659,-1.69832698995022,
51.1489784158944));
#148818=CARTESIAN_POINT('Ctrl Pts',(6.75634013910903,-1.88301049036709,
51.1403268344026));
#148819=CARTESIAN_POINT('Ctrl Pts',(6.70276764581104,-2.06556861579921,
51.1316752529107));
#148820=CARTESIAN_POINT('Ctrl Pts',(6.64196799252027,-2.24541482778488,
51.1230236714189));
#148821=CARTESIAN_POINT('Ctrl Pts',(6.58099956891383,-2.42576026468925,
51.1143480744918));
#148822=CARTESIAN_POINT('Ctrl Pts',(6.51276396106416,-2.60337846703591,
51.1056724775646));
#148823=CARTESIAN_POINT('Ctrl Pts',(6.43754508372162,-2.77770406227007,
51.0969968806375));
#148824=CARTESIAN_POINT('Ctrl Pts',(6.41999360611982,-2.81838097594212,
51.094972527835));
#148825=CARTESIAN_POINT('Ctrl Pts',(6.40206209931074,-2.85887873757411,
51.0929481750325));
#148826=CARTESIAN_POINT('Ctrl Pts',(6.38375451036624,-2.89919038938092,
51.09092382223));
#148827=CARTESIAN_POINT('Ctrl Pts',(6.30905780118092,-3.06366577392893,
51.0826642697005));
#148828=CARTESIAN_POINT('Ctrl Pts',(6.22790629528599,-3.22546041629001,
51.074404717171));
#148829=CARTESIAN_POINT('Ctrl Pts',(6.14051288283972,-3.38404020339289,
51.0661451646414));
#148830=CARTESIAN_POINT('Ctrl Pts',(6.05322118716208,-3.54243542025116,
51.057895225365));
#148831=CARTESIAN_POINT('Ctrl Pts',(5.95970222323858,-3.69762293679834,
51.0496452860886));
#148832=CARTESIAN_POINT('Ctrl Pts',(5.86021662995801,-3.84908919258356,
51.0413953468122));
#148833=CARTESIAN_POINT('Ctrl Pts',(5.76082890037866,-4.00040645143455,
51.0331535229781));
#148834=CARTESIAN_POINT('Ctrl Pts',(5.65548642398,-4.1480094566598,51.0249116991439));
#148835=CARTESIAN_POINT('Ctrl Pts',(5.54449549951053,-4.2914095840886,51.0166698753098));
#148836=CARTESIAN_POINT('Ctrl Pts',(5.43359376933599,-4.43469447260648,
51.008434674753));
#148837=CARTESIAN_POINT('Ctrl Pts',(5.31705284651501,-4.57378294220874,
51.0001994741961));
#148838=CARTESIAN_POINT('Ctrl Pts',(5.19522219400986,-4.7082154705756,50.9919642736392));
#148839=CARTESIAN_POINT('Ctrl Pts',(5.07346751947766,-4.84256416198687,
50.9837342088494));
#148840=CARTESIAN_POINT('Ctrl Pts',(4.94642992078197,-4.97226244427602,
50.9755041440595));
#148841=CARTESIAN_POINT('Ctrl Pts',(4.81449914552032,-5.0968838068259,50.9672740792697));
#148842=CARTESIAN_POINT('Ctrl Pts',(4.68262164753145,-5.22145484384474,
50.9590473380062));
#148843=CARTESIAN_POINT('Ctrl Pts',(4.54585516074474,-5.34095281011707,
50.9508205967427));
#148844=CARTESIAN_POINT('Ctrl Pts',(4.40462653196979,-5.45498777967172,
50.9425938554792));
#148845=CARTESIAN_POINT('Ctrl Pts',(4.26342782703677,-5.56899858723859,
50.9343688573162));
#148846=CARTESIAN_POINT('Ctrl Pts',(4.11776913183774,-5.67754848776479,
50.9261438591533));
#148847=CARTESIAN_POINT('Ctrl Pts',(3.96811085296037,-5.78028743412627,
50.9179188609904));
#148848=CARTESIAN_POINT('Ctrl Pts',(3.81845986875505,-5.88302137276667,
50.9096942637318));
#148849=CARTESIAN_POINT('Ctrl Pts',(3.66480997364422,-5.9799447266635,50.9014696664733));
#148850=CARTESIAN_POINT('Ctrl Pts',(3.50765125758459,-6.07075030104725,
50.8932450692148));
#148851=CARTESIAN_POINT('Ctrl Pts',(3.35047456404471,-6.16156626273539,
50.8850195311397));
#148852=CARTESIAN_POINT('Ctrl Pts',(3.18978854848019,-6.24626287833383,
50.8767939930645));
#148853=CARTESIAN_POINT('Ctrl Pts',(3.02610884015156,-6.32457839306753,
50.8685684549893));
#148854=CARTESIAN_POINT('Ctrl Pts',(2.86231442999977,-6.40294878896159,
50.8603371527042));
#148855=CARTESIAN_POINT('Ctrl Pts',(2.69552244617433,-6.47492899902809,
50.852105850419));
#148856=CARTESIAN_POINT('Ctrl Pts',(2.52627036974207,-6.54030462451584,
50.8438745481338));
#148857=CARTESIAN_POINT('Ctrl Pts',(2.35695843339274,-6.60570337160778,
50.835640334658));
#148858=CARTESIAN_POINT('Ctrl Pts',(2.18518499436796,-6.66449276065142,
50.8274061211821));
#148859=CARTESIAN_POINT('Ctrl Pts',(2.01150401975149,-6.71650788289745,
50.8191719077062));
#148860=CARTESIAN_POINT('Ctrl Pts',(1.83763489346561,-6.76857935404472,
50.8109287739614));
#148861=CARTESIAN_POINT('Ctrl Pts',(1.66185443491329,-6.81386180185788,
50.8026856402165));
#148862=CARTESIAN_POINT('Ctrl Pts',(1.48472933798092,-6.85224090027772,
50.7944425064716));
#148863=CARTESIAN_POINT('Ctrl Pts',(1.33536468048928,-6.88460492429011,
50.7874913015335));
#148864=CARTESIAN_POINT('Ctrl Pts',(1.18504413502541,-6.91206079366791,
50.7805400965954));
#148865=CARTESIAN_POINT('Ctrl Pts',(1.03411085615969,-6.93456857343503,
50.7735888916573));
#148866=CARTESIAN_POINT('Ctrl Pts',(0.852786367835311,-6.9616084130268,
50.7652380250484));
#148867=CARTESIAN_POINT('Ctrl Pts',(0.670243323763772,-6.98155555507229,
50.7568871584396));
#148868=CARTESIAN_POINT('Ctrl Pts',(0.487063628053379,-6.99431165910753,
50.7485362918308));
#148869=CARTESIAN_POINT('Ctrl Pts',(0.304043063887654,-7.00705668168239,
50.7401926797722));
#148870=CARTESIAN_POINT('Ctrl Pts',(0.120387279841823,-7.01262309418271,
50.7318490677136));
#148871=CARTESIAN_POINT('Ctrl Pts',(-0.0633147710334978,-7.01096411360585,
50.723505455655));
#148872=CARTESIAN_POINT('Ctrl Pts',(-0.246882989121302,-7.0093063416491,
50.7151679221831));
#148873=CARTESIAN_POINT('Ctrl Pts',(-0.430497076145864,-7.00043367259616,
50.7068303887113));
#148874=CARTESIAN_POINT('Ctrl Pts',(-0.61356573293114,-6.98435134095305,
50.6984928552395));
#148875=CARTESIAN_POINT('Ctrl Pts',(-0.796509835818056,-6.96827995119992,
50.6901609943515));
#148876=CARTESIAN_POINT('Ctrl Pts',(-0.97890891887683,-6.94500871154048,
50.6818291334635));
#148877=CARTESIAN_POINT('Ctrl Pts',(-1.16017422465034,-6.91459487829598,
50.6734972725755));
#148878=CARTESIAN_POINT('Ctrl Pts',(-1.34136576371141,-6.88419342209452,
50.6651688023748));
#148879=CARTESIAN_POINT('Ctrl Pts',(-1.52142411862375,-6.84665522173497,
50.6568403321742));
#148880=CARTESIAN_POINT('Ctrl Pts',(-1.69976754339773,-6.80208915414313,
50.6485118619736));
#148881=CARTESIAN_POINT('Ctrl Pts',(-1.87806378529055,-6.75753487703628,
50.6401855951691));
#148882=CARTESIAN_POINT('Ctrl Pts',(-2.05464568012357,-6.705956520383,50.6318593283647));
#148883=CARTESIAN_POINT('Ctrl Pts',(-2.22894313884969,-6.64751374923549,
50.6235330615602));
#148884=CARTESIAN_POINT('Ctrl Pts',(-2.28903353967636,-6.62736515057351,
50.6206625164971));
#148885=CARTESIAN_POINT('Ctrl Pts',(-2.34885253725066,-6.60640110093273,
50.6177919714339));
#148886=CARTESIAN_POINT('Ctrl Pts',(-2.408377186239,-6.58462951815085,50.6149214263707));
#148887=CARTESIAN_POINT('Ctrl Pts',(-2.58802914240775,-6.51892047992671,
50.6062578047512));
#148888=CARTESIAN_POINT('Ctrl Pts',(-2.76490399357511,-6.44588668882583,
50.5975941831317));
#148889=CARTESIAN_POINT('Ctrl Pts',(-2.9384196596914,-6.36579268167281,
50.5889305615122));
#148890=CARTESIAN_POINT('Ctrl Pts',(-3.11207603129979,-6.28563372553309,
50.5802599144801));
#148891=CARTESIAN_POINT('Ctrl Pts',(-3.28236752256699,-6.19840324020155,
50.571589267448));
#148892=CARTESIAN_POINT('Ctrl Pts',(-3.44873578605048,-6.10441217813106,
50.5629186204159));
#148893=CARTESIAN_POINT('Ctrl Pts',(-3.619288361139,-6.00805715623099,50.554029898805));
#148894=CARTESIAN_POINT('Ctrl Pts',(-3.78571750450639,-5.90459720012164,
50.545141177194));
#148895=CARTESIAN_POINT('Ctrl Pts',(-3.94745299325198,-5.7944146752339,
50.536252455583));
#148896=CARTESIAN_POINT('Ctrl Pts',(-4.1055484615931,-5.68671191926959,
50.5275637836228));
#148897=CARTESIAN_POINT('Ctrl Pts',(-4.25915907189742,-5.57258613754218,
50.5188751116625));
#148898=CARTESIAN_POINT('Ctrl Pts',(-4.40778493321005,-5.45243601934644,
50.5101864397023));
#148899=CARTESIAN_POINT('Ctrl Pts',(-4.56154378005493,-5.32813636208025,
50.501197693266));
#148900=CARTESIAN_POINT('Ctrl Pts',(-4.70996717776444,-5.19738905481171,
50.4922089468296));
#148901=CARTESIAN_POINT('Ctrl Pts',(-4.85254158261168,-5.06067848727071,
50.4832202003933));
#148902=CARTESIAN_POINT('Ctrl Pts',(-4.99511598745892,-4.9239679197297,
50.4742314539569));
#148903=CARTESIAN_POINT('Ctrl Pts',(-5.13184118669585,-4.78129434844169,
50.4652427075206));
#148904=CARTESIAN_POINT('Ctrl Pts',(-5.26224758495059,-4.63318215886033,
50.4562539610843));
#148905=CARTESIAN_POINT('Ctrl Pts',(-5.38755233669695,-4.49086428646692,
50.4476168646243));
#148906=CARTESIAN_POINT('Ctrl Pts',(-5.50714608811164,-4.34338555826818,
50.4389797681644));
#148907=CARTESIAN_POINT('Ctrl Pts',(-5.6206143895385,-4.19121944624864,
50.4303426717045));
#148908=CARTESIAN_POINT('Ctrl Pts',(-5.73398628081987,-4.03918262458434,
50.4217129138908));
#148909=CARTESIAN_POINT('Ctrl Pts',(-5.84124293139716,-3.88246659835011,
50.4130831560772));
#148910=CARTESIAN_POINT('Ctrl Pts',(-5.94201028610278,-3.72157766576875,
50.4044533982635));
#148911=CARTESIAN_POINT('Ctrl Pts',(-6.04599828610969,-3.55554653027593,
50.395547823058));
#148912=CARTESIAN_POINT('Ctrl Pts',(-6.14307510290476,-3.38507156342488,
50.3866422478526));
#148913=CARTESIAN_POINT('Ctrl Pts',(-6.23287680377116,-3.21074342037967,
50.3777366726471));
#148914=CARTESIAN_POINT('Ctrl Pts',(-6.31973521627337,-3.04212895524955,
50.3691229813996));
#148915=CARTESIAN_POINT('Ctrl Pts',(-6.39978767404947,-2.86991016399872,
50.360509290152));
#148916=CARTESIAN_POINT('Ctrl Pts',(-6.47275013472672,-2.69464881865806,
50.3518955989045));
#148917=CARTESIAN_POINT('Ctrl Pts',(-6.54942120960752,-2.51047910168861,
50.3428440817201));
#148918=CARTESIAN_POINT('Ctrl Pts',(-6.61826259867565,-2.32294975584741,
50.3337925645356));
#148919=CARTESIAN_POINT('Ctrl Pts',(-6.67900042040682,-2.13274000916791,
50.3247410473512));
#148920=CARTESIAN_POINT('Ctrl Pts',(-6.73973824213799,-1.9425302624884,
50.3156895301668));
#148921=CARTESIAN_POINT('Ctrl Pts',(-6.79237234741334,-1.74964046124067,
50.3066380129823));
#148922=CARTESIAN_POINT('Ctrl Pts',(-6.8366883706311,-1.55477287260149,
50.2975864957979));
#148923=CARTESIAN_POINT('Ctrl Pts',(-6.87773839777344,-1.37426660823085,
50.2892020560598));
#148924=CARTESIAN_POINT('Ctrl Pts',(-6.91163053864259,-1.19215520593247,
50.2808176163217));
#148925=CARTESIAN_POINT('Ctrl Pts',(-6.93826242264715,-1.00902978993809,
50.2724331765837));
#148926=CARTESIAN_POINT('Ctrl Pts',(-6.96490149311032,-0.825854958617998,
50.2640464743534));
#148927=CARTESIAN_POINT('Ctrl Pts',(-6.98427635294729,-0.641665888901126,
50.2556597721232));
#148928=CARTESIAN_POINT('Ctrl Pts',(-6.99633636889544,-0.457060144588258,
50.2472730698929));
#148929=CARTESIAN_POINT('Ctrl Pts',(-7.00840113260011,-0.272381725153531,
50.238883066007));
#148930=CARTESIAN_POINT('Ctrl Pts',(-7.01314528820371,-0.0872866274934254,
50.2304930621211));
#148931=CARTESIAN_POINT('Ctrl Pts',(-7.01057028857457,0.097625772496311,
50.2221030582351));
#148932=CARTESIAN_POINT('Ctrl Pts',(-7.00799288167434,0.282711040189968,
50.2137052108476));
#148933=CARTESIAN_POINT('Ctrl Pts',(-6.9980826523609,0.467612944374797,
50.2053073634601));
#148934=CARTESIAN_POINT('Ctrl Pts',(-6.98089314537137,0.651734190761063,
50.1969095160725));
#148935=CARTESIAN_POINT('Ctrl Pts',(-6.96369459592466,0.835952293240432,
50.1885072510379));
#148936=CARTESIAN_POINT('Ctrl Pts',(-6.9392091680795,1.01938859684581,50.1801049860033));
#148937=CARTESIAN_POINT('Ctrl Pts',(-6.90754197487244,1.20145346471486,
50.1717027209686));
#148938=CARTESIAN_POINT('Ctrl Pts',(-6.87584176519267,1.3837081548932,50.1632916956643));
#148939=CARTESIAN_POINT('Ctrl Pts',(-6.83694489388335,1.56458823472889,
50.1548806703599));
#148940=CARTESIAN_POINT('Ctrl Pts',(-6.79100728441987,1.74351559369462,
50.1464696450555));
#148941=CARTESIAN_POINT('Ctrl Pts',(-6.77726115282142,1.79705688701902,
50.1439527735408));
#148942=CARTESIAN_POINT('Ctrl Pts',(-6.76288492067004,1.85042343905972,
50.1414359020261));
#148943=CARTESIAN_POINT('Ctrl Pts',(-6.74788362291677,1.90360005622813,
50.1389190305114));
#148944=CARTESIAN_POINT('Ctrl Pts',(-6.69886596229565,2.0773579147955,50.1306949984468));
#148945=CARTESIAN_POINT('Ctrl Pts',(-6.64308337158687,2.24939632808308,
50.1224709663821));
#148946=CARTESIAN_POINT('Ctrl Pts',(-6.58067605921214,2.41915877242735,
50.1142469343175));
#148947=CARTESIAN_POINT('Ctrl Pts',(-6.51832251648744,2.58877495078333,
50.1060299880142));
#148948=CARTESIAN_POINT('Ctrl Pts',(-6.44935574289596,2.75611874316578,
50.097813041711));
#148949=CARTESIAN_POINT('Ctrl Pts',(-6.37396598305644,2.92064790917004,
50.0895960954078));
#148950=CARTESIAN_POINT('Ctrl Pts',(-6.29862732739923,3.08506554638696,
50.081384719096));
#148951=CARTESIAN_POINT('Ctrl Pts',(-6.21687450492783,3.24667204463256,
50.0731733427843));
#148952=CARTESIAN_POINT('Ctrl Pts',(-6.12894626796018,3.40494408279447,
50.0649619664726));
#148953=CARTESIAN_POINT('Ctrl Pts',(-6.04106148598651,3.56313790136841,
50.0567546483033));
#148954=CARTESIAN_POINT('Ctrl Pts',(-5.94700753964128,3.71800024127984,
50.0485473301339));
#148955=CARTESIAN_POINT('Ctrl Pts',(-5.84706972497163,3.869031169921,50.0403400119646));
#148956=CARTESIAN_POINT('Ctrl Pts',(-5.74716295158532,4.02001518745183,
50.0321352430374));
#148957=CARTESIAN_POINT('Ctrl Pts',(-5.64137614378662,4.16716987677307,
50.0239304741103));
#148958=CARTESIAN_POINT('Ctrl Pts',(-5.53003876001613,4.31002295530074,
50.0157257051831));
#148959=CARTESIAN_POINT('Ctrl Pts',(-5.41869192894773,4.45288815532384,
50.0075202400576));
#148960=CARTESIAN_POINT('Ctrl Pts',(-5.30179378764467,4.59145073660134,
49.9993147749322));
#148961=CARTESIAN_POINT('Ctrl Pts',(-5.17971542014312,4.72526980487164,
49.9911093098067));
#148962=CARTESIAN_POINT('Ctrl Pts',(-5.05762626039362,4.85910070331786,
49.9829031192831));
#148963=CARTESIAN_POINT('Ctrl Pts',(-4.93035619510045,4.98818699599834,
49.9746969287596));
#148964=CARTESIAN_POINT('Ctrl Pts',(-4.7983146184668,5.11212317777142,49.966490738236));
#148965=CARTESIAN_POINT('Ctrl Pts',(-4.66623938327661,5.23609095196477,
49.9582824558825));
#148966=CARTESIAN_POINT('Ctrl Pts',(-4.52939046556829,5.35490576114034,
49.950074173529));
#148967=CARTESIAN_POINT('Ctrl Pts',(-4.38821206241735,5.46820093428861,
49.9418658911754));
#148968=CARTESIAN_POINT('Ctrl Pts',(-4.24697416290341,5.58154385305943,
49.9336541496317));
#148969=CARTESIAN_POINT('Ctrl Pts',(-4.10140341208564,5.68936228277764,
49.925442408088));
#148970=CARTESIAN_POINT('Ctrl Pts',(-3.95197498637103,5.79133147640486,
49.9172306665443));
#148971=CARTESIAN_POINT('Ctrl Pts',(-3.80236826487776,5.89342233815975,
49.9090091268725));
#148972=CARTESIAN_POINT('Ctrl Pts',(-3.64889495842309,5.98964982288017,
49.9007875872007));
#148973=CARTESIAN_POINT('Ctrl Pts',(-3.49205803781394,6.07973331841448,
49.8925660475289));
#148974=CARTESIAN_POINT('Ctrl Pts',(-3.33512346264137,6.16987290446876,
49.8843393887126));
#148975=CARTESIAN_POINT('Ctrl Pts',(-3.17482140377513,6.25386071168839,
49.8761127298962));
#148976=CARTESIAN_POINT('Ctrl Pts',(-3.01167720518098,6.33146325696464,
49.8678860710799));
#148977=CARTESIAN_POINT('Ctrl Pts',(-2.84828125709027,6.40918555152939,
49.8596467176214));
#148978=CARTESIAN_POINT('Ctrl Pts',(-2.68203472247581,6.48050275408142,
49.851407364163));
#148979=CARTESIAN_POINT('Ctrl Pts',(-2.51348197790676,6.54522993555138,
49.8431680107045));
#148980=CARTESIAN_POINT('Ctrl Pts',(-2.36630103640591,6.60174997344102,
49.8359733737826));
#148981=CARTESIAN_POINT('Ctrl Pts',(-2.21736203517322,6.65324594581425,
49.8287787368606));
#148982=CARTESIAN_POINT('Ctrl Pts',(-2.0670347233137,6.69962640862276,49.8215840999386));
#148983=CARTESIAN_POINT('Ctrl Pts',(-1.90024344144612,6.7510864976096,49.8136015005032));
#148984=CARTESIAN_POINT('Ctrl Pts',(-1.73121745408192,6.79641013066064,
49.8056189010677));
#148985=CARTESIAN_POINT('Ctrl Pts',(-1.56045933555508,6.83539268985909,
49.7976363016322));
#148986=CARTESIAN_POINT('Ctrl Pts',(-1.38991509841071,6.87432642184084,
49.7896637007222));
#148987=CARTESIAN_POINT('Ctrl Pts',(-1.2176434041049,6.90693480175379,49.7816910998123));
#148988=CARTESIAN_POINT('Ctrl Pts',(-1.0441653504234,6.93306175390608,49.7737184989023));
#148989=CARTESIAN_POINT('Ctrl Pts',(-0.870866908181658,6.95916165537735,
49.7657541524677));
#148990=CARTESIAN_POINT('Ctrl Pts',(-0.696364955962511,6.97879342840225,
49.7577898060332));
#148991=CARTESIAN_POINT('Ctrl Pts',(-0.521194181197202,6.99185119893052,
49.7498254595986));
#148992=CARTESIAN_POINT('Ctrl Pts',(-0.346166793694386,7.00489828092943,
49.7418676324355));
#148993=CARTESIAN_POINT('Ctrl Pts',(-0.170472041520858,7.01138204324479,
49.7339098052724));
#148994=CARTESIAN_POINT('Ctrl Pts',(0.00534687895631584,7.01124796119674,
49.7259519781093));
#148995=CARTESIAN_POINT('Ctrl Pts',(0.181059950969795,7.01111395987026,
49.7179989418059));
#148996=CARTESIAN_POINT('Ctrl Pts',(0.356896672224531,7.00437004559262,
49.7100459055025));
#148997=CARTESIAN_POINT('Ctrl Pts',(0.53231051110847,6.99101366629071,49.7020928691991));
#148998=CARTESIAN_POINT('Ctrl Pts',(0.714130602427552,6.97716950142996,
49.6938493817061));
#148999=CARTESIAN_POINT('Ctrl Pts',(0.895495928886207,6.95622072434907,
49.685605894213));
#149000=CARTESIAN_POINT('Ctrl Pts',(1.0757993490757,6.9282236051551,49.67736240672));
#149001=CARTESIAN_POINT('Ctrl Pts',(1.24968766269844,6.90122260962314,49.6694122184372));
#149002=CARTESIAN_POINT('Ctrl Pts',(1.4225879440712,6.86766627608292,49.6614620301544));
#149003=CARTESIAN_POINT('Ctrl Pts',(1.59396264879154,6.82765769768502,49.6535118418716));
#149004=CARTESIAN_POINT('Ctrl Pts',(1.76535290166246,6.7876454894667,49.6455609322996));
#149005=CARTESIAN_POINT('Ctrl Pts',(1.93521694017008,6.74117995505776,49.6376100227276));
#149006=CARTESIAN_POINT('Ctrl Pts',(2.10302955462439,6.6884148536762,49.6296591131556));
#149007=CARTESIAN_POINT('Ctrl Pts',(2.27089027670589,6.63563462587619,49.6217059242592));
#149008=CARTESIAN_POINT('Ctrl Pts',(2.43669804965809,6.57655134781931,49.6137527353627));
#149009=CARTESIAN_POINT('Ctrl Pts',(2.5999450286778,6.51136793695101,49.6057995464663));
#149010=CARTESIAN_POINT('Ctrl Pts',(2.76327080887429,6.44615306130759,49.5978425184749));
#149011=CARTESIAN_POINT('Ctrl Pts',(2.92403299011285,6.37483232927915,49.5898854904836));
#149012=CARTESIAN_POINT('Ctrl Pts',(3.08174593827678,6.29765579675601,49.5819284624923));
#149013=CARTESIAN_POINT('Ctrl Pts',(3.23965263439011,6.22038445404074,49.5739616594135));
#149014=CARTESIAN_POINT('Ctrl Pts',(3.39450228635389,6.13724311373323,49.5659948563347));
#149015=CARTESIAN_POINT('Ctrl Pts',(3.54583533107336,6.04852695847608,49.558028053256));
#149016=CARTESIAN_POINT('Ctrl Pts',(3.69727876073859,5.95974609211764,49.550055439053));
#149017=CARTESIAN_POINT('Ctrl Pts',(3.84520016447192,5.86538251282993,49.54208282485));
#149018=CARTESIAN_POINT('Ctrl Pts',(3.98917137484191,5.76577300148401,49.534110210647));
#149019=CARTESIAN_POINT('Ctrl Pts',(4.1333501474075,5.66601988386553,49.5261261023869));
#149020=CARTESIAN_POINT('Ctrl Pts',(4.27356706678711,5.5610059623044,49.5181419941268));
#149021=CARTESIAN_POINT('Ctrl Pts',(4.40942872327172,5.45110675889643,49.5101578858667));
#149022=CARTESIAN_POINT('Ctrl Pts',(4.4429439673612,5.42399610293387,49.5081883136997));
#149023=CARTESIAN_POINT('Ctrl Pts',(4.47619435967196,5.39658832312724,49.5062187415327));
#149024=CARTESIAN_POINT('Ctrl Pts',(4.50917436348155,5.36888937511482,49.5042491693657));
#149025=CARTESIAN_POINT('Ctrl Pts',(4.64638763713034,5.25364792895385,49.496054766288));
#149026=CARTESIAN_POINT('Ctrl Pts',(4.77937035689912,5.13298339543888,49.4878603632103));
#149027=CARTESIAN_POINT('Ctrl Pts',(4.90766902805733,5.00723589154205,49.4796659601326));
#149028=CARTESIAN_POINT('Ctrl Pts',(5.03582349476579,4.88162972464771,49.4714807673559));
#149029=CARTESIAN_POINT('Ctrl Pts',(5.15930414786905,4.75095220810401,49.4632955745792));
#149030=CARTESIAN_POINT('Ctrl Pts',(5.27768968001487,4.61558427546985,49.4551103818026));
#149031=CARTESIAN_POINT('Ctrl Pts',(5.39596273489216,4.48034495496451,49.4469329657205));
#149032=CARTESIAN_POINT('Ctrl Pts',(5.50915008003478,4.34042435702449,49.4387555496384));
#149033=CARTESIAN_POINT('Ctrl Pts',(5.61686638443958,4.19624100616882,49.4305781335563));
#149034=CARTESIAN_POINT('Ctrl Pts',(5.72448335994765,4.05219061172347,49.4224082581499));
#149035=CARTESIAN_POINT('Ctrl Pts',(5.82663914104444,3.90388558009215,49.4142383827435));
#149036=CARTESIAN_POINT('Ctrl Pts',(5.92298797670736,3.75177824375056,49.4060685073371));
#149037=CARTESIAN_POINT('Ctrl Pts',(6.0192848778625,3.59975289718694,49.3979030357043));
#149038=CARTESIAN_POINT('Ctrl Pts',(6.10978087998942,3.44392962425402,49.3897375640715));
#149039=CARTESIAN_POINT('Ctrl Pts',(6.19417266954185,3.28479093739628,49.3815720924387));
#149040=CARTESIAN_POINT('Ctrl Pts',(6.27853476099334,3.12570825263085,49.3734094942963));
#149041=CARTESIAN_POINT('Ctrl Pts',(6.35679675379812,2.96331278812909,49.365246896154));
#149042=CARTESIAN_POINT('Ctrl Pts',(6.42870047017853,2.79811308335213,49.3570842980116));
#149043=CARTESIAN_POINT('Ctrl Pts',(6.47934924960681,2.68174686711097,49.3513345864016));
#149044=CARTESIAN_POINT('Ctrl Pts',(6.52684414272043,2.56398981785157,49.3455848747916));
#149045=CARTESIAN_POINT('Ctrl Pts',(6.57110895151812,2.44502632087643,49.3398351631816));
#149046=CARTESIAN_POINT('Origin',(0.,0.,50.));
#149047=CARTESIAN_POINT('',(6.57110895151816,2.44502632087632,47.3397953554189));
#149048=CARTESIAN_POINT('',(6.57110895151812,2.44502632087642,47.8869530982584));
#149049=CARTESIAN_POINT('',(6.57110895151814,2.44502632087636,50.));
#149050=CARTESIAN_POINT('',(7.01124999999811,5.14667476088492E-6,49.7734178143132));
#149051=CARTESIAN_POINT('Ctrl Pts',(6.57110895151812,2.44502632087642,47.8869530982584));
#149052=CARTESIAN_POINT('Ctrl Pts',(6.51463505187432,2.59680225241057,47.8943274580956));
#149053=CARTESIAN_POINT('Ctrl Pts',(6.45289207376814,2.74664578379087,47.9017018179328));
#149054=CARTESIAN_POINT('Ctrl Pts',(6.38600797641393,2.89422333064981,47.90907617777));
#149055=CARTESIAN_POINT('Ctrl Pts',(6.31139718170492,3.0588495794581,47.9173024508257));
#149056=CARTESIAN_POINT('Ctrl Pts',(6.23035139912944,3.22073266371939,47.9255287238814));
#149057=CARTESIAN_POINT('Ctrl Pts',(6.14309824714195,3.37934468328721,47.9337549969371));
#149058=CARTESIAN_POINT('Ctrl Pts',(6.05590682677823,3.53784448481712,47.9419754499029));
#149059=CARTESIAN_POINT('Ctrl Pts',(5.96251695279652,3.69307752994855,47.9501959028687));
#149060=CARTESIAN_POINT('Ctrl Pts',(5.86320334614051,3.84453808464772,47.9584163558345));
#149061=CARTESIAN_POINT('Ctrl Pts',(5.76394352395888,3.99591661406759,47.9666323569154));
#149062=CARTESIAN_POINT('Ctrl Pts',(5.65876655127818,4.14352643512401,47.9748483579963));
#149063=CARTESIAN_POINT('Ctrl Pts',(5.54799198093946,4.2868883286052,47.9830643590772));
#149064=CARTESIAN_POINT('Ctrl Pts',(5.43725477539619,4.43020186543008,47.9912775888615));
#149065=CARTESIAN_POINT('Ctrl Pts',(5.32092394576607,4.56927005576485,47.9994908186457));
#149066=CARTESIAN_POINT('Ctrl Pts',(5.19936123939148,4.70364425364137,48.0077040484299));
#149067=CARTESIAN_POINT('Ctrl Pts',(5.07782294310237,4.83799146885393,48.0159156289778));
#149068=CARTESIAN_POINT('Ctrl Pts',(4.95105509758945,4.96764631462191,48.0241272095256));
#149069=CARTESIAN_POINT('Ctrl Pts',(4.81945855553145,5.09219459506554,48.0323387900734));
#149070=CARTESIAN_POINT('Ctrl Pts',(4.68784883333586,5.21675534972352,48.0405511930574));
#149071=CARTESIAN_POINT('Ctrl Pts',(4.55140969910055,5.33620827810491,48.0487635960415));
#149072=CARTESIAN_POINT('Ctrl Pts',(4.41057787328124,5.45017700503589,48.0569759990255));
#149073=CARTESIAN_POINT('Ctrl Pts',(4.34902759899551,5.49998681444358,48.0605652137025));
#149074=CARTESIAN_POINT('Ctrl Pts',(4.28663870993172,5.54874959094404,48.0641544283794));
#149075=CARTESIAN_POINT('Ctrl Pts',(4.22344961252298,5.59643636012949,48.0677436430564));
#149076=CARTESIAN_POINT('Ctrl Pts',(4.07564924571124,5.70797651921876,48.0761388768478));
#149077=CARTESIAN_POINT('Ctrl Pts',(3.9234191645242,5.813664558907,48.0845341106393));
#149078=CARTESIAN_POINT('Ctrl Pts',(3.76725238731245,5.91315787145825,48.0929293444308));
#149079=CARTESIAN_POINT('Ctrl Pts',(3.61107845045146,6.01265574539721,48.1013249631116));
#149080=CARTESIAN_POINT('Ctrl Pts',(3.45096773100342,6.10595815233807,48.1097205817925));
#149081=CARTESIAN_POINT('Ctrl Pts',(3.28744105561792,6.1927665762838,48.1181162004733));
#149082=CARTESIAN_POINT('Ctrl Pts',(3.12388684239997,6.27958961873644,48.1265132329732));
#149083=CARTESIAN_POINT('Ctrl Pts',(2.95691581233362,6.35991634618527,48.1349102654732));
#149084=CARTESIAN_POINT('Ctrl Pts',(2.78707257109982,6.43349462158189,48.1433072979731));
#149085=CARTESIAN_POINT('Ctrl Pts',(2.61712751558886,6.50711700423217,48.1517093641605));
#149086=CARTESIAN_POINT('Ctrl Pts',(2.44430710591814,6.57398272280881,48.1601114303479));
#149087=CARTESIAN_POINT('Ctrl Pts',(2.26917603244139,6.6338877512582,48.1685134965354));
#149088=CARTESIAN_POINT('Ctrl Pts',(2.09398709362871,6.69381257302311,48.1769183388628));
#149089=CARTESIAN_POINT('Ctrl Pts',(1.91648627641171,6.74677201820913,48.1853231811902));
#149090=CARTESIAN_POINT('Ctrl Pts',(1.73725332938764,6.792611974199,48.1937280235177));
#149091=CARTESIAN_POINT('Ctrl Pts',(1.55788446949918,6.83848669076065,48.2021392392614));
#149092=CARTESIAN_POINT('Ctrl Pts',(1.37678117094426,6.87723105851779,48.2105504550052));
#149093=CARTESIAN_POINT('Ctrl Pts',(1.19453427722378,6.90874188423894,48.218961670749));
#149094=CARTESIAN_POINT('Ctrl Pts',(1.14073163628928,6.91804446058038,48.2214448166137));
#149095=CARTESIAN_POINT('Ctrl Pts',(1.08682937379787,6.92671694796164,48.2239279624783));
#149096=CARTESIAN_POINT('Ctrl Pts',(1.03284279133955,6.9347575538643,48.2264111083429));
#149097=CARTESIAN_POINT('Ctrl Pts',(0.836866110723315,6.96394575550984,
48.2354251755774));
#149098=CARTESIAN_POINT('Ctrl Pts',(0.639662547652286,6.9848205477569,48.2444392428119));
#149099=CARTESIAN_POINT('Ctrl Pts',(0.441915919871735,6.99730926015593,
48.2534533100463));
#149100=CARTESIAN_POINT('Ctrl Pts',(0.244216234661515,7.00979500789121,
48.2624652374542));
#149101=CARTESIAN_POINT('Ctrl Pts',(0.0459739666607946,7.01389863951236,
48.2714771648622));
#149102=CARTESIAN_POINT('Ctrl Pts',(-0.152123700502803,7.00959948515215,
48.2804890922701));
#149103=CARTESIAN_POINT('Ctrl Pts',(-0.350051838192558,7.00530400995378,
48.2894933073847));
#149104=CARTESIAN_POINT('Ctrl Pts',(-0.547835397827325,6.99262012224001,
48.2984975224993));
#149105=CARTESIAN_POINT('Ctrl Pts',(-0.744788474997783,6.97157921062441,
48.3075017376139));
#149106=CARTESIAN_POINT('Ctrl Pts',(-0.941583074783314,6.95055522948127,
48.3164987075284));
#149107=CARTESIAN_POINT('Ctrl Pts',(-1.13754830323584,6.92118767471165,
48.3254956774428));
#149108=CARTESIAN_POINT('Ctrl Pts',(-1.33200279437177,6.88355977080797,
48.3344926473573));
#149109=CARTESIAN_POINT('Ctrl Pts',(-1.52613539751012,6.84599415382073,
48.3434747242414));
#149110=CARTESIAN_POINT('Ctrl Pts',(-1.71876203702228,6.80019553628115,
48.3524568011256));
#149111=CARTESIAN_POINT('Ctrl Pts',(-1.90921095828222,6.74629825009798,
48.3614388780097));
#149112=CARTESIAN_POINT('Ctrl Pts',(-2.07629015342896,6.69901462603489,
48.3693187765495));
#149113=CARTESIAN_POINT('Ctrl Pts',(-2.24169328504685,6.64549871121803,
48.3771986750894));
#149114=CARTESIAN_POINT('Ctrl Pts',(-2.40497280154338,6.58587369954333,
48.3850785736292));
#149115=CARTESIAN_POINT('Ctrl Pts',(-2.57539384840242,6.52364080513861,
48.393303123696));
#149116=CARTESIAN_POINT('Ctrl Pts',(-2.74343544721625,6.45477517583604,
48.4015276737627));
#149117=CARTESIAN_POINT('Ctrl Pts',(-2.90856058795098,6.3794907217362,48.4097522238295));
#149118=CARTESIAN_POINT('Ctrl Pts',(-3.07367624415493,6.3042105918581,48.4179763014909));
#149119=CARTESIAN_POINT('Ctrl Pts',(-3.23587546241489,6.22251251541378,
48.4262003791523));
#149120=CARTESIAN_POINT('Ctrl Pts',(-3.39464265267125,6.13465792226145,
48.4344244568137));
#149121=CARTESIAN_POINT('Ctrl Pts',(-3.55342668942099,6.04679400702047,
48.4426494071168));
#149122=CARTESIAN_POINT('Ctrl Pts',(-3.70877767108523,5.95277244110612,
48.4508743574199));
#149123=CARTESIAN_POINT('Ctrl Pts',(-3.86020578286179,5.85289995442092,
48.459099307723));
#149124=CARTESIAN_POINT('Ctrl Pts',(-4.01172801401266,5.75296539249852,
48.4673293702023));
#149125=CARTESIAN_POINT('Ctrl Pts',(-4.15932221583622,5.64717283459909,
48.4755594326815));
#149126=CARTESIAN_POINT('Ctrl Pts',(-4.30252799035537,5.5358720590986,48.4837894951607));
#149127=CARTESIAN_POINT('Ctrl Pts',(-4.44578393186894,5.42453229337302,
48.4920224407464));
#149128=CARTESIAN_POINT('Ctrl Pts',(-4.5846481140489,5.30768068128211,48.5002553863321));
#149129=CARTESIAN_POINT('Ctrl Pts',(-4.71869403801562,5.18570661897642,
48.5084883319178));
#149130=CARTESIAN_POINT('Ctrl Pts',(-4.85286155771467,5.06362191156499,
48.5167287457728));
#149131=CARTESIAN_POINT('Ctrl Pts',(-4.982201839449,4.93640571065444,48.5249691596277));
#149132=CARTESIAN_POINT('Ctrl Pts',(-5.10632535682955,4.80448414636781,
48.5332095734826));
#149133=CARTESIAN_POINT('Ctrl Pts',(-5.15922816702545,4.74825772269336,
48.536721728627));
#149134=CARTESIAN_POINT('Ctrl Pts',(-5.2111838141935,4.69117696147659,48.5402338837714));
#149135=CARTESIAN_POINT('Ctrl Pts',(-5.26216439543281,4.63327664163702,
48.5437460389157));
#149136=CARTESIAN_POINT('Ctrl Pts',(-5.3819779525632,4.497200451246,48.5520002367065));
#149137=CARTESIAN_POINT('Ctrl Pts',(-5.49661766467963,4.35635166722079,
48.5602544344973));
#149138=CARTESIAN_POINT('Ctrl Pts',(-5.60569258271975,4.21115628189465,
48.5685086322881));
#149139=CARTESIAN_POINT('Ctrl Pts',(-5.71468122007305,4.06607574934855,
48.5767563008248));
#149140=CARTESIAN_POINT('Ctrl Pts',(-5.81811362944432,3.91665573995058,
48.5850039693615));
#149141=CARTESIAN_POINT('Ctrl Pts',(-5.91563833670354,3.76335616595392,
48.5932516378982));
#149142=CARTESIAN_POINT('Ctrl Pts',(-6.01310318906929,3.61015067816299,
48.6014942445041));
#149143=CARTESIAN_POINT('Ctrl Pts',(-6.10466738136032,3.45307065968898,
48.6097368511099));
#149144=CARTESIAN_POINT('Ctrl Pts',(-6.19002191479071,3.29260614968004,
48.6179794577158));
#149145=CARTESIAN_POINT('Ctrl Pts',(-6.27533918726352,3.13221168939264,
48.6262184660663));
#149146=CARTESIAN_POINT('Ctrl Pts',(-6.35445204293472,2.96843598493146,
48.6344574744167));
#149147=CARTESIAN_POINT('Ctrl Pts',(-6.42709658715709,2.80179514273505,
48.6426964827671));
#149148=CARTESIAN_POINT('Ctrl Pts',(-6.49972228675129,2.63519752862607,
48.650933353847));
#149149=CARTESIAN_POINT('Ctrl Pts',(-6.56588288287072,2.46573657282829,
48.6591702249268));
#149150=CARTESIAN_POINT('Ctrl Pts',(-6.62536181871064,2.29395015936946,
48.6674070960066));
#149151=CARTESIAN_POINT('Ctrl Pts',(-6.68484926816119,2.12213915699334,
48.6756451460839));
#149152=CARTESIAN_POINT('Ctrl Pts',(-6.73765302742374,1.94800235401809,
48.6838831961612));
#149153=CARTESIAN_POINT('Ctrl Pts',(-6.7836055886088,1.7720953080169,48.6921212462384));
#149154=CARTESIAN_POINT('Ctrl Pts',(-6.82956375477965,1.59616680605181,
48.7003603011379));
#149155=CARTESIAN_POINT('Ctrl Pts',(-6.86866896967914,1.41846796286247,
48.7085993560374));
#149156=CARTESIAN_POINT('Ctrl Pts',(-6.90080430639761,1.23956705639681,
48.7168384109369));
#149157=CARTESIAN_POINT('Ctrl Pts',(-6.932948728012,1.06061557332974,48.7250797950777));
#149158=CARTESIAN_POINT('Ctrl Pts',(-6.95811928290728,0.880461687592994,
48.7333211792186));
#149159=CARTESIAN_POINT('Ctrl Pts',(-6.97625058249306,0.699681622429293,
48.7415625633594));
#149160=CARTESIAN_POINT('Ctrl Pts',(-6.99438992270689,0.518821387322052,
48.7498076022799));
#149161=CARTESIAN_POINT('Ctrl Pts',(-7.0054837509383,0.337334760735345,
48.7580526412005));
#149162=CARTESIAN_POINT('Ctrl Pts',(-7.00951871315642,0.155801066780609,
48.7662976801209));
#149163=CARTESIAN_POINT('Ctrl Pts',(-7.01355852014873,-0.0259505944580573,
48.7745526188496));
#149164=CARTESIAN_POINT('Ctrl Pts',(-7.01052251805914,-0.207749092278264,
48.7828075575782));
#149165=CARTESIAN_POINT('Ctrl Pts',(-7.00044950268285,-0.389015838864519,
48.7910624963068));
#149166=CARTESIAN_POINT('Ctrl Pts',(-6.99037012363632,-0.57039710148762,
48.7993226501281));
#149167=CARTESIAN_POINT('Ctrl Pts',(-6.97324489693582,-0.751245601443899,
48.8075828039493));
#149168=CARTESIAN_POINT('Ctrl Pts',(-6.94916433108735,-0.930989614358494,
48.8158429577705));
#149169=CARTESIAN_POINT('Ctrl Pts',(-6.92504725073931,-1.11100618161099,
48.8241156368532));
#149170=CARTESIAN_POINT('Ctrl Pts',(-6.89395381022648,-1.28991457612809,
48.8323883159359));
#149171=CARTESIAN_POINT('Ctrl Pts',(-6.85602560790063,-1.46715351150136,
48.8406609950185));
#149172=CARTESIAN_POINT('Ctrl Pts',(-6.82481875155469,-1.61298351809075,
48.8474676531752));
#149173=CARTESIAN_POINT('Ctrl Pts',(-6.7889858638027,-1.7576834940798,48.8542743113319));
#149174=CARTESIAN_POINT('Ctrl Pts',(-6.7486307173724,-1.90094976341766,
48.8610809694886));
#149175=CARTESIAN_POINT('Ctrl Pts',(-6.70130433897402,-2.06896485626637,
48.8690634576727));
#149176=CARTESIAN_POINT('Ctrl Pts',(-6.64761112439817,-2.23552497683376,
48.8770459458569));
#149177=CARTESIAN_POINT('Ctrl Pts',(-6.58765216540073,-2.40009697933044,
48.8850284340411));
#149178=CARTESIAN_POINT('Ctrl Pts',(-6.52776817218238,-2.56446321994284,
48.8930009418411));
#149179=CARTESIAN_POINT('Ctrl Pts',(-6.46163414743741,-2.7268459441573,
48.9009734496411));
#149180=CARTESIAN_POINT('Ctrl Pts',(-6.38940200334982,-2.8867228135187,
48.9089459574412));
#149181=CARTESIAN_POINT('Ctrl Pts',(-6.3172444826564,-3.04643451327602,
48.9169102288029));
#149182=CARTESIAN_POINT('Ctrl Pts',(-6.23900153118579,-3.20364517460469,
48.9248745001647));
#149183=CARTESIAN_POINT('Ctrl Pts',(-6.15487459551915,-3.35784831044122,
48.9328387715265));
#149184=CARTESIAN_POINT('Ctrl Pts',(-6.07081633352349,-3.51192556869374,
48.9407965415728));
#149185=CARTESIAN_POINT('Ctrl Pts',(-5.98088382397672,-3.66299986365458,
48.9487543116191));
#149186=CARTESIAN_POINT('Ctrl Pts',(-5.88532625238966,-3.81058544917092,
48.9567120816654));
#149187=CARTESIAN_POINT('Ctrl Pts',(-5.78982599496341,-3.9580825148155,
48.964665078747));
#149188=CARTESIAN_POINT('Ctrl Pts',(-5.68870759294114,-4.10209472566131,
48.9726180758287));
#149189=CARTESIAN_POINT('Ctrl Pts',(-5.58226568439211,-4.24216175921643,
48.9805710729103));
#149190=CARTESIAN_POINT('Ctrl Pts',(-5.47193526020129,-4.38734569511109,
48.9888146073749));
#149191=CARTESIAN_POINT('Ctrl Pts',(-5.35588521613781,-4.52829039198769,
48.9970581418396));
#149192=CARTESIAN_POINT('Ctrl Pts',(-5.23449250536215,-4.66451656378317,
49.0053016763042));
#149193=CARTESIAN_POINT('Ctrl Pts',(-5.11741946947604,-4.7958952223314,
49.0132518703483));
#149194=CARTESIAN_POINT('Ctrl Pts',(-4.99537773349444,-4.92288510432967,
49.0212020643924));
#149195=CARTESIAN_POINT('Ctrl Pts',(-4.86874576639462,-5.04509080440724,
49.0291522584365));
#149196=CARTESIAN_POINT('Ctrl Pts',(-4.74210204530033,-5.16730784763263,
49.0371031904186));
#149197=CARTESIAN_POINT('Ctrl Pts',(-4.61086751207262,-5.28473956635985,
49.0450541224006));
#149198=CARTESIAN_POINT('Ctrl Pts',(-4.47545648116745,-5.39702842754013,
49.0530050543827));
#149199=CARTESIAN_POINT('Ctrl Pts',(-4.34000634767566,-5.50934971432778,
49.0609582823521));
#149200=CARTESIAN_POINT('Ctrl Pts',(-4.20037760186455,-5.616524950249,49.0689115103214));
#149201=CARTESIAN_POINT('Ctrl Pts',(-4.0570164057572,-5.71823787944476,
49.0768647382908));
#149202=CARTESIAN_POINT('Ctrl Pts',(-3.91358570704467,-5.82000011984712,
49.084821822046));
#149203=CARTESIAN_POINT('Ctrl Pts',(-3.76641925880851,-5.91629456772982,
49.0927789058011));
#149204=CARTESIAN_POINT('Ctrl Pts',(-3.61599074299558,-6.00684921644203,
49.1007359895563));
#149205=CARTESIAN_POINT('Ctrl Pts',(-3.46537696563385,-6.09751538852055,
49.1087028729272));
#149206=CARTESIAN_POINT('Ctrl Pts',(-3.31149341907474,-6.18242745899568,
49.1166697562982));
#149207=CARTESIAN_POINT('Ctrl Pts',(-3.15483752095674,-6.26135981867067,
49.1246366396692));
#149208=CARTESIAN_POINT('Ctrl Pts',(-2.99806707295894,-6.34034989524251,
49.1326093485822));
#149209=CARTESIAN_POINT('Ctrl Pts',(-2.83852057282886,-6.41335140127589,
49.1405820574953));
#149210=CARTESIAN_POINT('Ctrl Pts',(-2.67671331754712,-6.48018768078255,
49.1485547664084));
#149211=CARTESIAN_POINT('Ctrl Pts',(-2.51467237314459,-6.54712048816966,
49.1565389898567));
#149212=CARTESIAN_POINT('Ctrl Pts',(-2.35036450340084,-6.60787017223447,
49.164523213305));
#149213=CARTESIAN_POINT('Ctrl Pts',(-2.18431866091726,-6.66231030124451,
49.1725074367532));
#149214=CARTESIAN_POINT('Ctrl Pts',(-2.14335973009001,-6.67573917995051,
49.1744769245226));
#149215=CARTESIAN_POINT('Ctrl Pts',(-2.10229508780297,-6.68878438460215,
49.176446412292));
#149216=CARTESIAN_POINT('Ctrl Pts',(-2.06113274009001,-6.70144450027224,
49.1784159000614));
#149217=CARTESIAN_POINT('Ctrl Pts',(-1.88891025134105,-6.75441418615501,
49.1866561998511));
#149218=CARTESIAN_POINT('Ctrl Pts',(-1.71441685224321,-6.80081079918157,
49.1948964996408));
#149219=CARTESIAN_POINT('Ctrl Pts',(-1.53819039578885,-6.84043835355622,
49.2031367994305));
#149220=CARTESIAN_POINT('Ctrl Pts',(-1.36217376504217,-6.88001872500609,
49.2113672878288));
#149221=CARTESIAN_POINT('Ctrl Pts',(-1.18442852288641,-6.91284601743312,
49.2195977762271));
#149222=CARTESIAN_POINT('Ctrl Pts',(-1.00550902170901,-6.93877353498165,
49.2278282646254));
#149223=CARTESIAN_POINT('Ctrl Pts',(-0.826769649261018,-6.9646749497814,
49.2360504669096));
#149224=CARTESIAN_POINT('Ctrl Pts',(-0.646858714141219,-6.98369037941077,
49.2442726691937));
#149225=CARTESIAN_POINT('Ctrl Pts',(-0.466342382286715,-6.99572378992933,
49.2524948714779));
#149226=CARTESIAN_POINT('Ctrl Pts',(-0.28597460846228,-7.00774729741173,
49.2607103072043));
#149227=CARTESIAN_POINT('Ctrl Pts',(-0.105002775211771,-7.01280021177242,
49.2689257429307));
#149228=CARTESIAN_POINT('Ctrl Pts',(0.0759999335337276,-7.01083807918874,
49.2771411786572));
#149229=CARTESIAN_POINT('Ctrl Pts',(0.256886936402633,-7.00887720089718,
49.2853513626711));
#149230=CARTESIAN_POINT('Ctrl Pts',(0.43780442954631,-6.99991021597309,
49.293561546685));
#149231=CARTESIAN_POINT('Ctrl Pts',(0.618177072252241,-6.98394470695764,
49.3017717306989));
#149232=CARTESIAN_POINT('Ctrl Pts',(0.798474546826755,-6.96798585137622,
49.3099784932173));
#149233=CARTESIAN_POINT('Ctrl Pts',(0.978227278392545,-6.94503431356391,
49.3181852557357));
#149234=CARTESIAN_POINT('Ctrl Pts',(1.15686258505065,-6.91514971073005,
49.3263920182541));
#149235=CARTESIAN_POINT('Ctrl Pts',(1.33545890920995,-6.8852716294317,49.3345969898605));
#149236=CARTESIAN_POINT('Ctrl Pts',(1.51293795230025,-6.84846355431093,
49.3428019614669));
#149237=CARTESIAN_POINT('Ctrl Pts',(1.68873452703979,-6.80483668133804,
49.3510069330734));
#149238=CARTESIAN_POINT('Ctrl Pts',(1.86452200785808,-6.76121206517446,
49.3592114802382));
#149239=CARTESIAN_POINT('Ctrl Pts',(2.03862685710062,-6.71076943764895,
49.3674160274031));
#149240=CARTESIAN_POINT('Ctrl Pts',(2.21049620691852,-6.65367064722164,
49.375620574568));
#149241=CARTESIAN_POINT('Ctrl Pts',(2.38238528005077,-6.5965653042741,49.3838260632671));
#149242=CARTESIAN_POINT('Ctrl Pts',(2.55203801354117,-6.53280238624694,
49.3920315519661));
#149243=CARTESIAN_POINT('Ctrl Pts',(2.71891857186782,-6.46259300606593,
49.4002370406652));
#149244=CARTESIAN_POINT('Ctrl Pts',(2.88591860377642,-6.39233336139503,
49.4084484038599));
#149245=CARTESIAN_POINT('Ctrl Pts',(3.05014217433,-6.31561816665135,49.4166597670547));
#149246=CARTESIAN_POINT('Ctrl Pts',(3.21107437139439,-6.2327063097722,49.4248711302495));
#149247=CARTESIAN_POINT('Ctrl Pts',(3.37206445358993,-6.14976463062132,
49.4330854469603));
#149248=CARTESIAN_POINT('Ctrl Pts',(3.52976049776058,-6.06062201245151,
49.4412997636712));
#149249=CARTESIAN_POINT('Ctrl Pts',(3.68367371229846,-5.96558249828307,
49.4495140803821));
#149250=CARTESIAN_POINT('Ctrl Pts',(3.8377586158128,-5.87043696828643,49.4577375600984));
#149251=CARTESIAN_POINT('Ctrl Pts',(3.9880519661498,-5.76938158669269,49.4659610398148));
#149252=CARTESIAN_POINT('Ctrl Pts',(4.13409439688657,-5.66276346672992,
49.4741845195311));
#149253=CARTESIAN_POINT('Ctrl Pts',(4.26176121613083,-5.56956044223369,
49.4813732898988));
#149254=CARTESIAN_POINT('Ctrl Pts',(4.38617991706146,-5.47210719630128,
49.4885620602665));
#149255=CARTESIAN_POINT('Ctrl Pts',(4.50706545228633,-5.37065988229631,
49.4957508306342));
#149256=CARTESIAN_POINT('Ctrl Pts',(4.6484910384279,-5.25197532819353,49.5041610681452));
#149257=CARTESIAN_POINT('Ctrl Pts',(4.78533802794167,-5.12760708804512,
49.5125713056563));
#149258=CARTESIAN_POINT('Ctrl Pts',(4.91714286723303,-4.99793283125327,
49.5209815431673));
#149259=CARTESIAN_POINT('Ctrl Pts',(5.04883326038516,-4.86837117061592,
49.5293844780692));
#149260=CARTESIAN_POINT('Ctrl Pts',(5.17549000107735,-4.73351290448966,
49.5377874129712));
#149261=CARTESIAN_POINT('Ctrl Pts',(5.29668369780876,-4.59377495833948,
49.5461903478732));
#149262=CARTESIAN_POINT('Ctrl Pts',(5.41778724163909,-4.45414095968474,
49.5545870320461));
#149263=CARTESIAN_POINT('Ctrl Pts',(5.53343563203491,-4.30963476240791,
49.562983716219));
#149264=CARTESIAN_POINT('Ctrl Pts',(5.64323702120201,-4.16070937281554,
49.5713804003919));
#149265=CARTESIAN_POINT('Ctrl Pts',(5.75295723959736,-4.01189407644602,
49.5797708773088));
#149266=CARTESIAN_POINT('Ctrl Pts',(5.85683888789494,-3.85866636558156,
49.5881613542257));
#149267=CARTESIAN_POINT('Ctrl Pts',(5.95453086573895,-3.70151168192972,
49.5965518311426));
#149268=CARTESIAN_POINT('Ctrl Pts',(6.05217899339721,-3.54442753899393,
49.6049385418959));
#149269=CARTESIAN_POINT('Ctrl Pts',(6.1436428190526,-3.38342021257108,49.6133252526492));
#149270=CARTESIAN_POINT('Ctrl Pts',(6.2286145561511,-3.21900408098571,49.6217119634025));
#149271=CARTESIAN_POINT('Ctrl Pts',(6.31355606045063,-3.05464644837922,
49.6300956901785));
#149272=CARTESIAN_POINT('Ctrl Pts',(6.39200993482019,-2.88688271754616,
49.6384794169544));
#149273=CARTESIAN_POINT('Ctrl Pts',(6.46371414703572,-2.7162521951966,49.6468631437303));
#149274=CARTESIAN_POINT('Ctrl Pts',(6.48525334435847,-2.66499656632052,
49.6493815277938));
#149275=CARTESIAN_POINT('Ctrl Pts',(6.50618381300509,-2.6134824140297,49.6518999118572));
#149276=CARTESIAN_POINT('Ctrl Pts',(6.52649928291784,-2.56172474566901,
49.6544182959207));
#149277=CARTESIAN_POINT('Ctrl Pts',(6.59416463280609,-2.38933391473736,
49.6628063538657));
#149278=CARTESIAN_POINT('Ctrl Pts',(6.65498010262475,-2.21430015321486,
49.6711944118106));
#149279=CARTESIAN_POINT('Ctrl Pts',(6.70876036467014,-2.03719437755236,
49.6795824697556));
#149280=CARTESIAN_POINT('Ctrl Pts',(6.76258461466526,-1.85994374354111,
49.6879773884606));
#149281=CARTESIAN_POINT('Ctrl Pts',(6.80936206295708,-1.68061801858394,
49.6963723071656));
#149282=CARTESIAN_POINT('Ctrl Pts',(6.8489575222117,-1.49980246080603,49.7047672258705));
#149283=CARTESIAN_POINT('Ctrl Pts',(6.88856939771308,-1.31891193703781,
49.7131656251023));
#149284=CARTESIAN_POINT('Ctrl Pts',(6.92099328199438,-1.13653066598544,
49.7215640243341));
#149285=CARTESIAN_POINT('Ctrl Pts',(6.94614538059307,-0.953252807058868,
49.7299624235659));
#149286=CARTESIAN_POINT('Ctrl Pts',(6.97132356719064,-0.769784850572,49.7383695336982));
#149287=CARTESIAN_POINT('Ctrl Pts',(6.98921485666406,-0.585418769512334,
49.7467766438305));
#149288=CARTESIAN_POINT('Ctrl Pts',(6.99978734403713,-0.400753915461443,
49.7551837539629));
#149289=CARTESIAN_POINT('Ctrl Pts',(7.00743084934709,-0.267248266062745,
49.7612617740797));
#149290=CARTESIAN_POINT('Ctrl Pts',(7.01125009806236,-0.133586540720038,
49.7673397941964));
#149291=CARTESIAN_POINT('Ctrl Pts',(7.01124999999811,5.14667476088493E-6,
49.7734178143132));
#149292=CARTESIAN_POINT('Ctrl Pts',(7.01125,3.41650028888675E-12,49.7735343569105));
#149293=CARTESIAN_POINT('Ctrl Pts',(7.01124999999991,0.191008754743501,
49.7822061308426));
#149294=CARTESIAN_POINT('Ctrl Pts',(7.00344012881,0.38201736748625,49.7908779047747));
#149295=CARTESIAN_POINT('Ctrl Pts',(6.98784644419154,0.572388534912878,
49.7995496787068));
#149296=CARTESIAN_POINT('Ctrl Pts',(6.97225169663174,0.762772678963538,
49.8082220437492));
#149297=CARTESIAN_POINT('Ctrl Pts',(6.94887209704289,0.952519007629858,
49.8168944087915));
#149298=CARTESIAN_POINT('Ctrl Pts',(6.9177856624606,1.14099434299849,49.8255667738339));
#149299=CARTESIAN_POINT('Ctrl Pts',(6.88670108297151,1.32945843103956,49.83423862135));
#149300=CARTESIAN_POINT('Ctrl Pts',(6.84791063501112,1.51665139731078,49.8429104688661));
#149301=CARTESIAN_POINT('Ctrl Pts',(6.80154374572929,1.7019486588704,49.8515823163822));
#149302=CARTESIAN_POINT('Ctrl Pts',(6.7551759761985,1.8872494381929,49.8602543285284));
#149303=CARTESIAN_POINT('Ctrl Pts',(6.70123154646077,2.07065416525498,49.8689263406747));
#149304=CARTESIAN_POINT('Ctrl Pts',(6.63989045285515,2.25155087363867,49.8775983528209));
#149305=CARTESIAN_POINT('Ctrl Pts',(6.6179093415363,2.31637382429816,49.880705901988));
#149306=CARTESIAN_POINT('Ctrl Pts',(6.59497889661508,2.38087486019083,49.8838134511551));
#149307=CARTESIAN_POINT('Ctrl Pts',(6.57110895151815,2.44502632087633,49.8869210003222));
#149308=CARTESIAN_POINT('',(7.01124962123882,-0.00230459943256138,49.2264656431155));
#149309=CARTESIAN_POINT('Ctrl Pts',(6.57110895151812,2.44502632087643,49.3398351631816));
#149310=CARTESIAN_POINT('Ctrl Pts',(6.63393545901991,2.27617749405085,49.3316744072807));
#149311=CARTESIAN_POINT('Ctrl Pts',(6.69025281322801,2.10489771849203,49.3235136513798));
#149312=CARTESIAN_POINT('Ctrl Pts',(6.73988482605375,1.93172956027246,49.3153528954789));
#149313=CARTESIAN_POINT('Ctrl Pts',(6.78953780024269,1.75848826698436,49.3071886930007));
#149314=CARTESIAN_POINT('Ctrl Pts',(6.83249969278043,1.58335733548993,49.2990244905225));
#149315=CARTESIAN_POINT('Ctrl Pts',(6.86864450317827,1.40689347551938,49.2908602880443));
#149316=CARTESIAN_POINT('Ctrl Pts',(6.90479730607753,1.23039059507434,49.2826942802612));
#149317=CARTESIAN_POINT('Ctrl Pts',(6.9341299589928,1.05255454485122,49.2745282724782));
#149318=CARTESIAN_POINT('Ctrl Pts',(6.95656788542627,0.873950695380447,
49.2663622646952));
#149319=CARTESIAN_POINT('Ctrl Pts',(6.97902400505887,0.695202029702612,
49.2581896357208));
#149320=CARTESIAN_POINT('Ctrl Pts',(6.9945741935382,0.515684671185068,49.2500170067464));
#149321=CARTESIAN_POINT('Ctrl Pts',(7.00319582682655,0.335968411639008,
49.2418443777719));
#149322=CARTESIAN_POINT('Ctrl Pts',(7.008603707655,0.223242193525074,49.2367181328865));
#149323=CARTESIAN_POINT('Ctrl Pts',(7.01128667968011,0.11043776212266,49.231591888001));
#149324=CARTESIAN_POINT('Ctrl Pts',(7.01124962123882,-0.00230459943246711,
49.2264656431155));
#149325=CARTESIAN_POINT('Ctrl Pts',(7.01124962123863,-0.00230460000231739,
49.2264656430896));
#149326=CARTESIAN_POINT('Ctrl Pts',(7.0111543134133,-0.292258150983308,
49.2132818416574));
#149327=CARTESIAN_POINT('Ctrl Pts',(6.99306880246358,-0.581786799269796,
49.2000980402251));
#149328=CARTESIAN_POINT('Ctrl Pts',(6.95717055138536,-0.869140081595806,
49.1869142387928));
#149329=CARTESIAN_POINT('Ctrl Pts',(6.93473364888314,-1.04873984998543,
49.1786741808942));
#149330=CARTESIAN_POINT('Ctrl Pts',(6.90531789339566,-1.22763027984424,
49.1704341229955));
#149331=CARTESIAN_POINT('Ctrl Pts',(6.86898335526019,-1.40523813912747,
49.1621940650969));
#149332=CARTESIAN_POINT('Ctrl Pts',(6.83267575384516,-1.58271432828368,
49.1539601159903));
#149333=CARTESIAN_POINT('Ctrl Pts',(6.78945965786096,-1.75890950466602,
49.1457261668836));
#149334=CARTESIAN_POINT('Ctrl Pts',(6.73944670513276,-1.93325752841551,
49.137492217777));
#149335=CARTESIAN_POINT('Ctrl Pts',(6.6894626438119,-2.10750483506075,49.1292630252457));
#149336=CARTESIAN_POINT('Ctrl Pts',(6.63268964487006,-2.27990678465444,
49.1210338327145));
#149337=CARTESIAN_POINT('Ctrl Pts',(6.56929005055234,-2.44990913999153,
49.1128046401832));
#149338=CARTESIAN_POINT('Ctrl Pts',(6.50591565050843,-2.6198439383366,49.1045787178389));
#149339=CARTESIAN_POINT('Ctrl Pts',(6.43592002366576,-2.78738072007506,
49.0963527954947));
#149340=CARTESIAN_POINT('Ctrl Pts',(6.35951490614674,-2.95198182938131,
49.0881268731504));
#149341=CARTESIAN_POINT('Ctrl Pts',(6.28312779743214,-3.11654414195143,
49.0799028896688));
#149342=CARTESIAN_POINT('Ctrl Pts',(6.20033435550908,-3.27817184906863,
49.0716789061871));
#149343=CARTESIAN_POINT('Ctrl Pts',(6.11139394687428,-3.43634843818382,
49.0634549227055));
#149344=CARTESIAN_POINT('Ctrl Pts',(6.02244980194379,-3.5945316721359,49.0552305937427));
#149345=CARTESIAN_POINT('Ctrl Pts',(5.92735834133822,-3.74926319654111,
49.0470062647799));
#149346=CARTESIAN_POINT('Ctrl Pts',(5.82642447659114,-3.90005184338359,
49.0387819358171));
#149347=CARTESIAN_POINT('Ctrl Pts',(5.78332654716101,-3.96443735439881,
49.0352702150469));
#149348=CARTESIAN_POINT('Ctrl Pts',(5.73916396958308,-4.02810433437554,
49.0317584942767));
#149349=CARTESIAN_POINT('Ctrl Pts',(5.69396288521739,-4.09101616035269,
49.0282467735065));
#149350=CARTESIAN_POINT('Ctrl Pts',(5.57839100933724,-4.25187154347584,
49.0192678703967));
#149351=CARTESIAN_POINT('Ctrl Pts',(5.45607575093163,-4.40772067452792,
49.0102889672868));
#149352=CARTESIAN_POINT('Ctrl Pts',(5.32746421809379,-4.55804251487744,
49.001310064177));
#149353=CARTESIAN_POINT('Ctrl Pts',(5.1986842859189,-4.7085611812635,48.9923194044128));
#149354=CARTESIAN_POINT('Ctrl Pts',(5.06359174978242,-4.85353792162908,
48.9833287446486));
#149355=CARTESIAN_POINT('Ctrl Pts',(4.92267206018854,-4.99248699050275,
48.9743380848845));
#149356=CARTESIAN_POINT('Ctrl Pts',(4.78153217249342,-5.13165317822774,
48.9653333765071));
#149357=CARTESIAN_POINT('Ctrl Pts',(4.63454708033781,-5.26477269728677,
48.9563286681298));
#149358=CARTESIAN_POINT('Ctrl Pts',(4.48223860910744,-5.39139718565852,
48.9473239597524));
#149359=CARTESIAN_POINT('Ctrl Pts',(4.32984940165237,-5.51808879559654,
48.9383144781267));
#149360=CARTESIAN_POINT('Ctrl Pts',(4.17213135487001,-5.63827835741899,
48.929304996501));
#149361=CARTESIAN_POINT('Ctrl Pts',(4.00963852602667,-5.75155852383532,
48.9202955148753));
#149362=CARTESIAN_POINT('Ctrl Pts',(3.84706374338567,-5.86489582347964,
48.9112814892876));
#149363=CARTESIAN_POINT('Ctrl Pts',(3.67970955101394,-5.97131663517501,
48.9022674637));
#149364=CARTESIAN_POINT('Ctrl Pts',(3.50815945691212,-6.0704566374679,48.8932534381123));
#149365=CARTESIAN_POINT('Ctrl Pts',(3.35797501485197,-6.15724927962969,
48.8853620614815));
#149366=CARTESIAN_POINT('Ctrl Pts',(3.20457525062338,-6.23846235574786,
48.8774706848508));
#149367=CARTESIAN_POINT('Ctrl Pts',(3.04836791990124,-6.31387991550497,
48.86957930822));
#149368=CARTESIAN_POINT('Ctrl Pts',(2.88188031053688,-6.39426083725818,
48.8611685862406));
#149369=CARTESIAN_POINT('Ctrl Pts',(2.71211133539213,-6.46810118178353,
48.8527578642613));
#149370=CARTESIAN_POINT('Ctrl Pts',(2.53960042779602,-6.53514010788126,
48.8443471422819));
#149371=CARTESIAN_POINT('Ctrl Pts',(2.36719949029477,-6.60213629884319,
48.8359417818643));
#149372=CARTESIAN_POINT('Ctrl Pts',(2.19206040635686,-6.66233959912067,
48.8275364214467));
#149373=CARTESIAN_POINT('Ctrl Pts',(2.01474359368856,-6.7155368224879,48.8191310610291));
#149374=CARTESIAN_POINT('Ctrl Pts',(1.8375180199141,-6.76870667306548,48.8107300256148));
#149375=CARTESIAN_POINT('Ctrl Pts',(1.6581172615034,-6.81487754270127,48.8023289902005));
#149376=CARTESIAN_POINT('Ctrl Pts',(1.4771184101876,-6.8538855961261,48.7939279547861));
#149377=CARTESIAN_POINT('Ctrl Pts',(1.29619290096818,-6.89287784319419,
48.7855303235345));
#149378=CARTESIAN_POINT('Ctrl Pts',(1.11367090665178,-6.92471299539992,
48.7771326922829));
#149379=CARTESIAN_POINT('Ctrl Pts',(0.930141722771828,-6.94927787169711,
48.7687350610314));
#149380=CARTESIAN_POINT('Ctrl Pts',(0.746659319491453,-6.97383648653975,
48.7603395702907));
#149381=CARTESIAN_POINT('Ctrl Pts',(0.562170559411362,-6.99112847922829,
48.7519440795501));
#149382=CARTESIAN_POINT('Ctrl Pts',(0.377272445272298,-7.00109220511616,
48.7435485888094));
#149383=CARTESIAN_POINT('Ctrl Pts',(0.192389203732857,-7.01105512955451,
48.7351537733746));
#149384=CARTESIAN_POINT('Ctrl Pts',(0.00709699690991861,-7.0136909444913,
48.7267589579397));
#149385=CARTESIAN_POINT('Ctrl Pts',(-0.178003978355003,-7.00899002326225,
48.7183641425049));
#149386=CARTESIAN_POINT('Ctrl Pts',(-0.232776987931474,-7.00759897924896,
48.7158800426478));
#149387=CARTESIAN_POINT('Ctrl Pts',(-0.287533248423897,-7.00556586290797,
48.7133959427907));
#149388=CARTESIAN_POINT('Ctrl Pts',(-0.342257216702542,-7.00289130003565,
48.7109118429336));
#149389=CARTESIAN_POINT('Ctrl Pts',(-0.523177875600953,-6.99404903781773,
48.7026992626501));
#149390=CARTESIAN_POINT('Ctrl Pts',(-0.703804957775542,-6.97818886163649,
48.6944866823667));
#149391=CARTESIAN_POINT('Ctrl Pts',(-0.883563655581548,-6.95535346542758,
48.6862741020833));
#149392=CARTESIAN_POINT('Ctrl Pts',(-1.06330372176843,-6.93252043606049,
48.6780623730169));
#149393=CARTESIAN_POINT('Ctrl Pts',(-1.24217523938604,-6.90271367141434,
48.6698506439505));
#149394=CARTESIAN_POINT('Ctrl Pts',(-1.41960952695709,-6.86602762545219,
48.6616389148841));
#149395=CARTESIAN_POINT('Ctrl Pts',(-1.59705484946293,-6.82933929792356,
48.6534266751165));
#149396=CARTESIAN_POINT('Ctrl Pts',(-1.7730624247913,-6.78577090772626,
48.645214435349));
#149397=CARTESIAN_POINT('Ctrl Pts',(-1.94707453745135,-6.73546786111467,
48.6370021955814));
#149398=CARTESIAN_POINT('Ctrl Pts',(-2.12118466334839,-6.68513648104771,
48.6287853302267));
#149399=CARTESIAN_POINT('Ctrl Pts',(-2.29329674790264,-6.62806296212458,
48.6205684648719));
#149400=CARTESIAN_POINT('Ctrl Pts',(-2.46286823844427,-6.5644425964862,
48.6123515995171));
#149401=CARTESIAN_POINT('Ctrl Pts',(-2.63249341959451,-6.50080208703625,
48.6041321324957));
#149402=CARTESIAN_POINT('Ctrl Pts',(-2.79957608169925,-6.4306107277192,
48.5959126654742));
#149403=CARTESIAN_POINT('Ctrl Pts',(-2.96359411896677,-6.3541117758917,
48.5876931984527));
#149404=CARTESIAN_POINT('Ctrl Pts',(-3.12775415315384,-6.27754659588778,
48.5794666155127));
#149405=CARTESIAN_POINT('Ctrl Pts',(-3.28884395258761,-6.19466306970273,
48.5712400325727));
#149406=CARTESIAN_POINT('Ctrl Pts',(-3.44636568945316,-6.10575057606025,
48.5630134496326));
#149407=CARTESIAN_POINT('Ctrl Pts',(-3.51510070519197,-6.06695338037475,
48.5594237589708));
#149408=CARTESIAN_POINT('Ctrl Pts',(-3.58315670515217,-6.02700881618113,
48.555834068309));
#149409=CARTESIAN_POINT('Ctrl Pts',(-3.65049407409528,-5.98594349935708,
48.5522443776472));
#149410=CARTESIAN_POINT('Ctrl Pts',(-3.82915323051799,-5.87698921472776,
48.5427202290871));
#149411=CARTESIAN_POINT('Ctrl Pts',(-4.00285577337634,-5.76007938028789,
48.533196080527));
#149412=CARTESIAN_POINT('Ctrl Pts',(-4.17096818931078,-5.63565887241745,
48.5236719319669));
#149413=CARTESIAN_POINT('Ctrl Pts',(-4.33914537389983,-5.5111904290697,
48.5141441140391));
#149414=CARTESIAN_POINT('Ctrl Pts',(-4.50172804277483,-5.37920559321943,
48.5046162961112));
#149415=CARTESIAN_POINT('Ctrl Pts',(-4.65811393997038,-5.24019093972287,
48.4950884781833));
#149416=CARTESIAN_POINT('Ctrl Pts',(-4.81421893533291,-5.1014259856665,
48.4855777742124));
#149417=CARTESIAN_POINT('Ctrl Pts',(-4.96414932030537,-4.95565651457983,
48.4760670702415));
#149418=CARTESIAN_POINT('Ctrl Pts',(-5.10733913016107,-4.80340645500936,
48.4665563662707));
#149419=CARTESIAN_POINT('Ctrl Pts',(-5.2502234378214,-4.65148122810325,
48.4570659538341));
#149420=CARTESIAN_POINT('Ctrl Pts',(-5.38639581029265,-4.49310309591276,
48.4475755413976));
#149421=CARTESIAN_POINT('Ctrl Pts',(-5.51532812086316,-4.32883151459099,
48.438085128961));
#149422=CARTESIAN_POINT('Ctrl Pts',(-5.64362606150262,-4.16536817870633,
48.4286414110439));
#149423=CARTESIAN_POINT('Ctrl Pts',(-5.76475491902691,-3.9960693127224,
48.4191976931268));
#149424=CARTESIAN_POINT('Ctrl Pts',(-5.87822958593923,-3.82152371410787,
48.4097539752097));
#149425=CARTESIAN_POINT('Ctrl Pts',(-5.94302351683683,-3.72185833713127,
48.4043616209267));
#149426=CARTESIAN_POINT('Ctrl Pts',(-6.00532252882905,-3.62048299862126,
48.3989692666437));
#149427=CARTESIAN_POINT('Ctrl Pts',(-6.06504169686301,-3.51751272603427,
48.3935769123607));
#149428=CARTESIAN_POINT('Ctrl Pts',(-6.15236834452326,-3.36694048918445,
48.3856917351549));
#149429=CARTESIAN_POINT('Ctrl Pts',(-6.23414206732846,-3.21301399738746,
48.3778065579491));
#149430=CARTESIAN_POINT('Ctrl Pts',(-6.31009330272946,-3.05619846759808,
48.3699213807432));
#149431=CARTESIAN_POINT('Ctrl Pts',(-6.38602530597681,-2.89942264618669,
48.3620382001994));
#149432=CARTESIAN_POINT('Ctrl Pts',(-6.45613759027239,-2.739759582739,48.3541550196555));
#149433=CARTESIAN_POINT('Ctrl Pts',(-6.52020675079018,-2.5776986808877,
48.3462718391116));
#149434=CARTESIAN_POINT('Ctrl Pts',(-6.5842726076758,-2.4156461354688,48.3383890650523));
#149435=CARTESIAN_POINT('Ctrl Pts',(-6.64229582294004,-2.25119635027543,
48.330506290993));
#149436=CARTESIAN_POINT('Ctrl Pts',(-6.69410139158002,-2.08485805793737,
48.3226235169338));
#149437=CARTESIAN_POINT('Ctrl Pts',(-6.74593478824017,-1.91843041486979,
48.3147365085421));
#149438=CARTESIAN_POINT('Ctrl Pts',(-6.79154375300138,-1.75011259990219,
48.3068495001505));
#149439=CARTESIAN_POINT('Ctrl Pts',(-6.83080326259212,-1.58042821737047,
48.2989624917589));
#149440=CARTESIAN_POINT('Ctrl Pts',(-6.87007359128198,-1.41069707337455,
48.2910733098728));
#149441=CARTESIAN_POINT('Ctrl Pts',(-6.90299090701275,-1.23959898324818,
48.2831841279868));
#149442=CARTESIAN_POINT('Ctrl Pts',(-6.92948157068107,-1.0676664854211,
48.2752949461007));
#149443=CARTESIAN_POINT('Ctrl Pts',(-6.95599887859821,-0.895561058281625,
48.2673978292936));
#149444=CARTESIAN_POINT('Ctrl Pts',(-6.97607658060606,-0.722619923094152,
48.2595007124864));
#149445=CARTESIAN_POINT('Ctrl Pts',(-6.98969298956055,-0.549380081717617,
48.2516035956793));
#149446=CARTESIAN_POINT('Ctrl Pts',(-6.99928781427546,-0.427306345742015,
48.2460388794777));
#149447=CARTESIAN_POINT('Ctrl Pts',(-7.00567548191634,-0.305084359689145,
48.240474163276));
#149448=CARTESIAN_POINT('Ctrl Pts',(-7.00886393579073,-0.182901317852169,
48.2349094470743));
#149449=CARTESIAN_POINT('Ctrl Pts',(-7.0136627053592,0.0009897735821425,
48.2265342935304));
#149450=CARTESIAN_POINT('Ctrl Pts',(-7.01122326831066,0.185193758841107,
48.2181591399865));
#149451=CARTESIAN_POINT('Ctrl Pts',(-7.00152690421748,0.369117287618403,
48.2097839864426));
#149452=CARTESIAN_POINT('Ctrl Pts',(-6.99183724965269,0.552913548058271,
48.2014146281979));
#149453=CARTESIAN_POINT('Ctrl Pts',(-6.97490069659784,0.736429411317662,
48.1930452699531));
#149454=CARTESIAN_POINT('Ctrl Pts',(-6.95075058721552,0.919071725613981,
48.1846759117083));
#149455=CARTESIAN_POINT('Ctrl Pts',(-6.92661362404325,1.10161461782533,
48.1763111093577));
#149456=CARTESIAN_POINT('Ctrl Pts',(-6.89527097699532,1.28328458365763,
48.1679463070071));
#149457=CARTESIAN_POINT('Ctrl Pts',(-6.85680784497028,1.4634933343388,48.1595815046564));
#149458=CARTESIAN_POINT('Ctrl Pts',(-6.81835997906454,1.64363055968799,
48.1512200223181));
#149459=CARTESIAN_POINT('Ctrl Pts',(-6.77279733241736,1.8223074050096,48.1428585399797));
#149460=CARTESIAN_POINT('Ctrl Pts',(-6.72025633178953,1.99894507116699,
48.1344970576413));
#149461=CARTESIAN_POINT('Ctrl Pts',(-6.66772844373725,2.17553865413762,
48.1261376620651));
#149462=CARTESIAN_POINT('Ctrl Pts',(-6.60822576893657,2.35009375780528,
48.1177782664888));
#149463=CARTESIAN_POINT('Ctrl Pts',(-6.54193491543914,2.52204562303267,
48.1094188709126));
#149464=CARTESIAN_POINT('Ctrl Pts',(-6.4756391357662,2.69401026626827,48.1010588541367));
#149465=CARTESIAN_POINT('Ctrl Pts',(-6.40255428225458,2.86337097533321,
48.0926988373609));
#149466=CARTESIAN_POINT('Ctrl Pts',(-6.32291581769584,3.02958117977251,
48.0843388205851));
#149467=CARTESIAN_POINT('Ctrl Pts',(-6.24327214762705,3.19580224842039,
48.0759782573629));
#149468=CARTESIAN_POINT('Ctrl Pts',(-6.15707415439254,3.3588721048185,48.0676176941406));
#149469=CARTESIAN_POINT('Ctrl Pts',(-6.06460422482876,3.51826692544628,
48.0592571309184));
#149470=CARTESIAN_POINT('Ctrl Pts',(-5.9721158442247,3.67769355101074,48.0508948994664));
#149471=CARTESIAN_POINT('Ctrl Pts',(-5.87335319704827,3.83344339386688,
48.0425326680145));
#149472=CARTESIAN_POINT('Ctrl Pts',(-5.76864335165365,3.98501950358115,
48.0341704365625));
#149473=CARTESIAN_POINT('Ctrl Pts',(-5.66389855846263,4.13664620310389,
48.025805414145));
#149474=CARTESIAN_POINT('Ctrl Pts',(-5.55320279612925,4.28409612106476,
48.0174403917276));
#149475=CARTESIAN_POINT('Ctrl Pts',(-5.43692520276366,4.42690308252319,
48.0090753693102));
#149476=CARTESIAN_POINT('Ctrl Pts',(-5.32053966812708,4.56984261264322,
48.0007025815862));
#149477=CARTESIAN_POINT('Ctrl Pts',(-5.19856215605856,4.70813031790278,
47.9923297938623));
#149478=CARTESIAN_POINT('Ctrl Pts',(-5.07140148787643,4.841333856621,47.9839570061383));
#149479=CARTESIAN_POINT('Ctrl Pts',(-4.94417838928989,4.97460279253247,
47.9755801077367));
#149480=CARTESIAN_POINT('Ctrl Pts',(-4.81176729192242,5.10278235082226,
47.967203209335));
#149481=CARTESIAN_POINT('Ctrl Pts',(-4.67461276146979,5.22547816881899,
47.9588263109334));
#149482=CARTESIAN_POINT('Ctrl Pts',(-4.53730088598192,5.34831474467287,
47.9504398024709));
#149483=CARTESIAN_POINT('Ctrl Pts',(-4.39523495349272,5.46565479488748,
47.9420532940085));
#149484=CARTESIAN_POINT('Ctrl Pts',(-4.24889242112825,5.57714440876143,
47.9336667855461));
#149485=CARTESIAN_POINT('Ctrl Pts',(-4.15529036118381,5.64845421427322,
47.9283026958646));
#149486=CARTESIAN_POINT('Ctrl Pts',(-4.05993936491755,5.71737145869807,
47.922938606183));
#149487=CARTESIAN_POINT('Ctrl Pts',(-3.96297029502821,5.78381301592851,
47.9175745165015));
#149488=CARTESIAN_POINT('Ctrl Pts',(-3.81161611212275,5.88751832749905,
47.9092019765596));
#149489=CARTESIAN_POINT('Ctrl Pts',(-3.65601025415236,5.98540131201746,
47.9008294366177));
#149490=CARTESIAN_POINT('Ctrl Pts',(-3.49662611191066,6.07710723913973,
47.8924568966757));
#149491=CARTESIAN_POINT('Ctrl Pts',(-3.3374438431573,6.16869701295372,47.8840949612634));
#149492=CARTESIAN_POINT('Ctrl Pts',(-3.17449310946873,6.25412515821576,
47.875733025851));
#149493=CARTESIAN_POINT('Ctrl Pts',(-3.00827736862891,6.33307933282816,
47.8673710904386));
#149494=CARTESIAN_POINT('Ctrl Pts',(-2.8422497503453,6.41194414730489,47.8590186190436));
#149495=CARTESIAN_POINT('Ctrl Pts',(-2.67296478500967,6.48434945447317,
47.8506661476487));
#149496=CARTESIAN_POINT('Ctrl Pts',(-2.5009520785021,6.55002788265333,47.8423136762537));
#149497=CARTESIAN_POINT('Ctrl Pts',(-2.32916097188154,6.61562169887336,
47.8339719651494));
#149498=CARTESIAN_POINT('Ctrl Pts',(-2.15464943880652,6.67450580441283,
47.825630254045));
#149499=CARTESIAN_POINT('Ctrl Pts',(-1.97796860756911,6.72646019463218,
47.8172885429407));
#149500=CARTESIAN_POINT('Ctrl Pts',(-1.80142253261501,6.77837495870488,
47.8089531941451));
#149501=CARTESIAN_POINT('Ctrl Pts',(-1.62271077067838,6.82337044759098,
47.8006178453494));
#149502=CARTESIAN_POINT('Ctrl Pts',(-1.44240228279849,6.86127555321004,
47.7922824965538));
#149503=CARTESIAN_POINT('Ctrl Pts',(-1.26223618799388,6.89915072443931,
47.7839537303431));
#149504=CARTESIAN_POINT('Ctrl Pts',(-1.08047620279392,6.92994661192153,
47.7756249641325));
#149505=CARTESIAN_POINT('Ctrl Pts',(-0.897704377648231,6.95354250816454,
47.7672961979218));
#149506=CARTESIAN_POINT('Ctrl Pts',(-0.836338759730766,6.96146482743949,
47.7644998156862));
#149507=CARTESIAN_POINT('Ctrl Pts',(-0.774859178520908,6.96857592923775,
47.7617034334506));
#149508=CARTESIAN_POINT('Ctrl Pts',(-0.713287932486978,6.97487253560009,
47.758907051215));
#149509=CARTESIAN_POINT('Ctrl Pts',(-0.529553038553202,6.99366225282443,
47.750562360689));
#149510=CARTESIAN_POINT('Ctrl Pts',(-0.34515329223523,7.00517965295675,
47.7422176701629));
#149511=CARTESIAN_POINT('Ctrl Pts',(-0.160685625171539,7.00940844097155,
47.7338729796368));
#149512=CARTESIAN_POINT('Ctrl Pts',(0.0239015034585188,7.01363996755647,
47.7255228850754));
#149513=CARTESIAN_POINT('Ctrl Pts',(0.208556313908372,7.01057345934576,
47.7171727905139));
#149514=CARTESIAN_POINT('Ctrl Pts',(0.392683226795378,7.00024474185679,
47.7088226959525));
#149515=CARTESIAN_POINT('Ctrl Pts',(0.576953270014772,6.98990799537985,
47.7004661104779));
#149516=CARTESIAN_POINT('Ctrl Pts',(0.760694271244567,6.9722977970693,47.6921095250032));
#149517=CARTESIAN_POINT('Ctrl Pts',(0.943316662251313,6.94750172631998,
47.6837529395286));
#149518=CARTESIAN_POINT('Ctrl Pts',(1.12621645255707,6.92266799089764,47.6753836605888));
#149519=CARTESIAN_POINT('Ctrl Pts',(1.30799391308432,6.89062661468306,47.667014381649));
#149520=CARTESIAN_POINT('Ctrl Pts',(1.48806903357164,6.85151640980485,47.6586451027092));
#149521=CARTESIAN_POINT('Ctrl Pts',(1.66830008658007,6.81237233821129,47.6502685765564));
#149522=CARTESIAN_POINT('Ctrl Pts',(1.84682554268267,6.76614730615661,47.6418920504035));
#149523=CARTESIAN_POINT('Ctrl Pts',(2.02308084742507,6.71302990066944,47.6335155242507));
#149524=CARTESIAN_POINT('Ctrl Pts',(2.19960972899756,6.65983004835073,47.6251259963702));
#149525=CARTESIAN_POINT('Ctrl Pts',(2.37386110953577,6.59971655072576,47.6167364684897));
#149526=CARTESIAN_POINT('Ctrl Pts',(2.54528935663812,6.53292649992978,47.6083469406092));
#149527=CARTESIAN_POINT('Ctrl Pts',(2.60051016768242,6.51141195470758,47.605644489049));
#149528=CARTESIAN_POINT('Ctrl Pts',(2.65543822837897,6.48920499253787,47.6029420374888));
#149529=CARTESIAN_POINT('Ctrl Pts',(2.71005585341318,6.46631454801582,47.6002395859286));
#149530=CARTESIAN_POINT('Ctrl Pts',(2.87960170853735,6.39525726589795,47.59185054557));
#149531=CARTESIAN_POINT('Ctrl Pts',(3.04649674636681,6.31746679995528,47.5834615052114));
#149532=CARTESIAN_POINT('Ctrl Pts',(3.21018958197694,6.23316207155459,47.5750724648528));
#149533=CARTESIAN_POINT('Ctrl Pts',(3.37372780399423,6.14893697191042,47.5666913482355));
#149534=CARTESIAN_POINT('Ctrl Pts',(3.53406956243541,6.05821002621535,47.5583102316181));
#149535=CARTESIAN_POINT('Ctrl Pts',(3.69068428208039,5.9612478637031,47.5499291150007));
#149536=CARTESIAN_POINT('Ctrl Pts',(3.85429633078517,5.85995356587825,47.5411735416848));
#149537=CARTESIAN_POINT('Ctrl Pts',(4.01384031646739,5.75185422115874,47.5324179683689));
#149538=CARTESIAN_POINT('Ctrl Pts',(4.16873914753686,5.63730791089982,47.523662395053));
#149539=CARTESIAN_POINT('Ctrl Pts',(4.31677978741585,5.5278331721337,47.5152944773144));
#149540=CARTESIAN_POINT('Ctrl Pts',(4.46057741905618,5.41247023983569,47.5069265595758));
#149541=CARTESIAN_POINT('Ctrl Pts',(4.59965704948135,5.29157647489447,47.4985586418372));
#149542=CARTESIAN_POINT('Ctrl Pts',(4.73867542173533,5.17073595808833,47.490194409781));
#149543=CARTESIAN_POINT('Ctrl Pts',(4.87297968789883,5.04436968066918,47.4818301777247));
#149544=CARTESIAN_POINT('Ctrl Pts',(5.00212771071479,4.91287542363932,47.4734659456684));
#149545=CARTESIAN_POINT('Ctrl Pts',(5.1312361384931,4.78142148097079,47.4651042779726));
#149546=CARTESIAN_POINT('Ctrl Pts',(5.25519124492781,4.64484292801901,47.4567426102768));
#149547=CARTESIAN_POINT('Ctrl Pts',(5.3735872615183,4.50357485841506,47.448380942581));
#149548=CARTESIAN_POINT('Ctrl Pts',(5.49196282015109,4.36233119889074,47.4400207197197));
#149549=CARTESIAN_POINT('Ctrl Pts',(5.60478099394573,4.21639989101749,47.4316604968583));
#149550=CARTESIAN_POINT('Ctrl Pts',(5.7116755962774,4.06624992411795,47.423300273997));
#149551=CARTESIAN_POINT('Ctrl Pts',(5.81858358501917,3.91608115393938,47.414939004185));
#149552=CARTESIAN_POINT('Ctrl Pts',(5.91956632664644,3.76169293515637,47.406577734373));
#149553=CARTESIAN_POINT('Ctrl Pts',(6.01429994629887,3.6035847039371,47.398216464561));
#149554=CARTESIAN_POINT('Ctrl Pts',(6.10903907307722,3.4454672814514,47.3898547086854));
#149555=CARTESIAN_POINT('Ctrl Pts',(6.19752818793235,3.28362969949976,47.3814929528098));
#149556=CARTESIAN_POINT('Ctrl Pts',(6.27948847744328,3.11859760536,47.3731311969342));
#149557=CARTESIAN_POINT('Ctrl Pts',(6.36148111448179,2.95350037747987,47.3647661408979));
#149558=CARTESIAN_POINT('Ctrl Pts',(6.43693963536268,2.78520641485026,47.3564010848616));
#149559=CARTESIAN_POINT('Ctrl Pts',(6.50563230234053,2.61426374133205,47.3480360288252));
#149560=CARTESIAN_POINT('Ctrl Pts',(6.52818938709538,2.55813011682139,47.3452891376898));
#149561=CARTESIAN_POINT('Ctrl Pts',(6.5500172888635,2.50171103305673,47.3425422465544));
#149562=CARTESIAN_POINT('Ctrl Pts',(6.57110895151816,2.44502632087632,47.3397953554189));
#149563=CARTESIAN_POINT('Origin',(0.,0.,50.));
#149564=CARTESIAN_POINT('',(6.57110895151812,2.4450263208764,45.3397873838214));
#149565=CARTESIAN_POINT('',(6.57110895151812,2.4450263208764,45.8869210003222));
#149566=CARTESIAN_POINT('',(6.57110895151814,2.44502632087636,50.));
#149567=CARTESIAN_POINT('',(7.01125,3.56735040812906E-12,47.7735343569105));
#149568=CARTESIAN_POINT('Ctrl Pts',(6.57110895151812,2.4450263208764,45.8869210003222));
#149569=CARTESIAN_POINT('Ctrl Pts',(6.50449838733133,2.62404495591367,45.895592809261));
#149570=CARTESIAN_POINT('Ctrl Pts',(6.43056821795842,2.80033990716037,45.9042646181998));
#149571=CARTESIAN_POINT('Ctrl Pts',(6.34956511459209,2.97332295892242,45.9129364271385));
#149572=CARTESIAN_POINT('Ctrl Pts',(6.26856213015448,3.14630575671081,45.9216082233454));
#149573=CARTESIAN_POINT('Ctrl Pts',(6.18048635294189,3.3159764075484,45.9302800195522));
#149574=CARTESIAN_POINT('Ctrl Pts',(6.08563165071444,3.48176879966529,45.9389518157591));
#149575=CARTESIAN_POINT('Ctrl Pts',(5.99077708581834,3.6475609517467,45.9476235994108));
#149576=CARTESIAN_POINT('Ctrl Pts',(5.88914375657957,3.8094746098397,45.9562953830625));
#149577=CARTESIAN_POINT('Ctrl Pts',(5.7810707650006,3.9669695452014,45.9649671667143));
#149578=CARTESIAN_POINT('Ctrl Pts',(5.67299792768672,4.12446425575235,45.9736389379878));
#149579=CARTESIAN_POINT('Ctrl Pts',(5.55848560711145,4.27754002202802,45.9823107092613));
#149580=CARTESIAN_POINT('Ctrl Pts',(5.43791587524628,4.42568610457684,45.9909824805348));
#149581=CARTESIAN_POINT('Ctrl Pts',(5.31734631302621,4.57383197867983,45.9996542396069));
#149582=CARTESIAN_POINT('Ctrl Pts',(5.19071953583538,4.71704796267164,46.0083259986789));
#149583=CARTESIAN_POINT('Ctrl Pts',(5.05845803451277,4.85485621574658,46.016997757751));
#149584=CARTESIAN_POINT('Ctrl Pts',(4.92619671658875,4.99266427773161,46.0256695047985));
#149585=CARTESIAN_POINT('Ctrl Pts',(4.78830088681432,5.12506441891224,46.034341251846));
#149586=CARTESIAN_POINT('Ctrl Pts',(4.64523063400086,5.25161488681719,46.0430129988935));
#149587=CARTESIAN_POINT('Ctrl Pts',(4.49652806262013,5.38314733061205,46.0520261309665));
#149588=CARTESIAN_POINT('Ctrl Pts',(4.34223563523578,5.50835996364566,46.0610392630395));
#149589=CARTESIAN_POINT('Ctrl Pts',(4.18290943344173,5.62680151010538,46.0700523951125));
#149590=CARTESIAN_POINT('Ctrl Pts',(4.02607270355069,5.74339240740169,46.0789246969969));
#149591=CARTESIAN_POINT('Ctrl Pts',(3.8643586282001,5.85342208902884,46.0877969988812));
#149592=CARTESIAN_POINT('Ctrl Pts',(3.69833198496072,5.9565062823367,46.0966693007656));
#149593=CARTESIAN_POINT('Ctrl Pts',(3.53489950802194,6.05797978512413,46.105402972933));
#149594=CARTESIAN_POINT('Ctrl Pts',(3.36728850946689,6.15272311280124,46.1141366451004));
#149595=CARTESIAN_POINT('Ctrl Pts',(3.19606623000572,6.24041562845914,46.1228703172679));
#149596=CARTESIAN_POINT('Ctrl Pts',(3.02603797480699,6.32749661744154,46.1315430848818));
#149597=CARTESIAN_POINT('Ctrl Pts',(2.8524489133494,6.40762471321783,46.1402158524958));
#149598=CARTESIAN_POINT('Ctrl Pts',(2.67587836094736,6.48053250589129,46.1488886201098));
#149599=CARTESIAN_POINT('Ctrl Pts',(2.49930871513026,6.55343992422653,46.1575613431943));
#149600=CARTESIAN_POINT('Ctrl Pts',(2.31975787164533,6.61912700519576,46.1662340662788));
#149601=CARTESIAN_POINT('Ctrl Pts',(2.13782503579629,6.67737453486193,46.1749067893633));
#149602=CARTESIAN_POINT('Ctrl Pts',(1.95589311921358,6.73562177021623,46.1835794686264));
#149603=CARTESIAN_POINT('Ctrl Pts',(1.77157950496551,6.7864294428502,46.1922521478895));
#149604=CARTESIAN_POINT('Ctrl Pts',(1.58549928668296,6.82962799678195,46.2009248271527));
#149605=CARTESIAN_POINT('Ctrl Pts',(1.39941999343375,6.87282633596706,46.2095974633026));
#149606=CARTESIAN_POINT('Ctrl Pts',(1.21157439050145,6.90841556789004,46.2182700994525));
#149607=CARTESIAN_POINT('Ctrl Pts',(1.02258935228606,6.93627692491377,46.2269427356024));
#149608=CARTESIAN_POINT('Ctrl Pts',(0.833605238118976,6.96413814570851,
46.2356153293472));
#149609=CARTESIAN_POINT('Ctrl Pts',(0.643481980910279,6.98427152577672,
46.2442879230919));
#149610=CARTESIAN_POINT('Ctrl Pts',(0.452854049801629,6.99660987708178,
46.2529605168367));
#149611=CARTESIAN_POINT('Ctrl Pts',(0.262227035215384,7.00894816906512,
46.2616330688844));
#149612=CARTESIAN_POINT('Ctrl Pts',(0.0710956351155785,7.01349148893093,
46.2703056209321));
#149613=CARTESIAN_POINT('Ctrl Pts',(-0.119902323162865,7.01022467510137,
46.2789781729798));
#149614=CARTESIAN_POINT('Ctrl Pts',(-0.310899378728219,7.00695787671175,
46.2876506840385));
#149615=CARTESIAN_POINT('Ctrl Pts',(-0.501762709658449,6.99588102335243,
46.2963231950972));
#149616=CARTESIAN_POINT('Ctrl Pts',(-0.691855389210719,6.97703107940047,
46.3049957061558));
#149617=CARTESIAN_POINT('Ctrl Pts',(-0.881947185842832,6.95818122300052,
46.3136681769334));
#149618=CARTESIAN_POINT('Ctrl Pts',(-1.07126805553568,6.93155837629042,
46.322340647711));
#149619=CARTESIAN_POINT('Ctrl Pts',(-1.25918622473028,6.89725138109012,
46.3310131184886));
#149620=CARTESIAN_POINT('Ctrl Pts',(-1.44710353644051,6.86294454243514,
46.339685549693));
#149621=CARTESIAN_POINT('Ctrl Pts',(-1.63361788097595,6.82095367647916,
46.3483579808975));
#149622=CARTESIAN_POINT('Ctrl Pts',(-1.81810685597207,6.77141890764169,
46.357030412102));
#149623=CARTESIAN_POINT('Ctrl Pts',(-2.00259500418734,6.72188436079254,
46.3657028044413));
#149624=CARTESIAN_POINT('Ctrl Pts',(-2.18505752664676,6.66480605238501,
46.3743751967805));
#149625=CARTESIAN_POINT('Ctrl Pts',(-2.36488554745479,6.60037445225189,
46.3830475891198));
#149626=CARTESIAN_POINT('Ctrl Pts',(-2.54471277704449,6.53594313560888,
46.3917199433018));
#149627=CARTESIAN_POINT('Ctrl Pts',(-2.72190526073538,6.46415868780674,
46.4003922974837));
#149628=CARTESIAN_POINT('Ctrl Pts',(-2.89587171390473,6.38526065083537,
46.4090646516657));
#149629=CARTESIAN_POINT('Ctrl Pts',(-3.06983741584206,6.30636295456607,
46.4177369683982));
#149630=CARTESIAN_POINT('Ctrl Pts',(-3.2405768564137,6.22035184793457,46.4264092851306));
#149631=CARTESIAN_POINT('Ctrl Pts',(-3.40752028947368,6.12751434427739,
46.4350816018631));
#149632=CARTESIAN_POINT('Ctrl Pts',(-3.57446301525142,6.03467723394097,
46.443753881854));
#149633=CARTESIAN_POINT('Ctrl Pts',(-3.73760951742763,5.9350139225178,46.4524261618448));
#149634=CARTESIAN_POINT('Ctrl Pts',(-3.89641539159459,5.82885697702773,
46.4610984418357));
#149635=CARTESIAN_POINT('Ctrl Pts',(-4.05522060591328,5.72270047262635,
46.4697706857927));
#149636=CARTESIAN_POINT('Ctrl Pts',(-4.20968499214723,5.61005054602113,
46.4784429297497));
#149637=CARTESIAN_POINT('Ctrl Pts',(-4.35929312156537,5.49128309621466,
46.4871151737067));
#149638=CARTESIAN_POINT('Ctrl Pts',(-4.50890064155975,5.37251613020347,
46.4957873823375));
#149639=CARTESIAN_POINT('Ctrl Pts',(-4.65365172183918,5.24763186747866,
46.5044595909684));
#149640=CARTESIAN_POINT('Ctrl Pts',(-4.79306334971558,5.11704702813187,
46.5131317995993));
#149641=CARTESIAN_POINT('Ctrl Pts',(-4.93247442107824,4.9864627100634,46.5218039736118));
#149642=CARTESIAN_POINT('Ctrl Pts',(-5.06654587537236,4.85017805510181,
46.5304761476244));
#149643=CARTESIAN_POINT('Ctrl Pts',(-5.1948303397914,4.70864782111412,46.5391483216369));
#149644=CARTESIAN_POINT('Ctrl Pts',(-5.32311430258135,4.56711814055029,
46.5478204617387));
#149645=CARTESIAN_POINT('Ctrl Pts',(-5.44561113001101,4.42034313247171,
46.5564926018405));
#149646=CARTESIAN_POINT('Ctrl Pts',(-5.56191207495656,4.26881255537795,
46.5651647419424));
#149647=CARTESIAN_POINT('Ctrl Pts',(-5.67821257462083,4.11728255844911,
46.5738368488412));
#149648=CARTESIAN_POINT('Ctrl Pts',(-5.78831706632673,3.96099725427349,
46.58250895574));
#149649=CARTESIAN_POINT('Ctrl Pts',(-5.89185815647741,3.80047813129488,
46.5911810626388));
#149650=CARTESIAN_POINT('Ctrl Pts',(-5.99539885864796,3.6399596097995,46.5998531370423));
#149651=CARTESIAN_POINT('Ctrl Pts',(-6.09237605451008,3.47520753994365,
46.6085252114457));
#149652=CARTESIAN_POINT('Ctrl Pts',(-6.18246615568418,3.30677165772293,
46.6171972858492));
#149653=CARTESIAN_POINT('Ctrl Pts',(-6.27255592663025,3.13833639290911,
46.6258693284649));
#149654=CARTESIAN_POINT('Ctrl Pts',(-6.35575851944183,2.9662175932161,46.6345413710806));
#149655=CARTESIAN_POINT('Ctrl Pts',(-6.4317963101397,2.79098957134801,46.6432134136963));
#149656=CARTESIAN_POINT('Ctrl Pts',(-6.50783382832182,2.61576217748865,
46.6518854252318));
#149657=CARTESIAN_POINT('Ctrl Pts',(-6.57670648270859,2.43742584431381,
46.6605574367673));
#149658=CARTESIAN_POINT('Ctrl Pts',(-6.63818446599706,2.25657562645157,
46.6692294483029));
#149659=CARTESIAN_POINT('Ctrl Pts',(-6.69966223396684,2.07572604199386,
46.6779014294658));
#149660=CARTESIAN_POINT('Ctrl Pts',(-6.7537452912495,1.8923628593846,46.6865734106287));
#149661=CARTESIAN_POINT('Ctrl Pts',(-6.80025318023576,1.70709790205291,
46.6952453917916));
#149662=CARTESIAN_POINT('Ctrl Pts',(-6.846760910128,1.52183357847489,46.7039173432895));
#149663=CARTESIAN_POINT('Ctrl Pts',(-6.88569345442436,1.33466776867056,
46.7125892947873));
#149664=CARTESIAN_POINT('Ctrl Pts',(-6.91692090874809,1.14622497993348,
46.7212612462851));
#149665=CARTESIAN_POINT('Ctrl Pts',(-6.94814825879637,0.957782820449011,
46.7299331688254));
#149666=CARTESIAN_POINT('Ctrl Pts',(-6.97167052392585,0.768063970763964,
46.7386050913656));
#149667=CARTESIAN_POINT('Ctrl Pts',(-6.98740921903211,0.577701452555783,
46.7472770139059));
#149668=CARTESIAN_POINT('Ctrl Pts',(-7.00314786286725,0.387339554481687,
46.7559489081961));
#149669=CARTESIAN_POINT('Ctrl Pts',(-7.01110296401766,0.196334275130466,
46.7646208024863));
#149670=CARTESIAN_POINT('Ctrl Pts',(-7.01124797942393,0.00532292437173847,
46.7732926967765));
#149671=CARTESIAN_POINT('Ctrl Pts',(-7.01139299436962,-0.185687819719586,
46.781964563524));
#149672=CARTESIAN_POINT('Ctrl Pts',(-7.00372797299397,-0.376704351168703,
46.7906364302716));
#149673=CARTESIAN_POINT('Ctrl Pts',(-6.98827849031139,-0.567089326606621,
46.7993082970191));
#149674=CARTESIAN_POINT('Ctrl Pts',(-6.97282905543744,-0.757473712895766,
46.8079801369314));
#149675=CARTESIAN_POINT('Ctrl Pts',(-6.94959523043274,-0.947226264008327,
46.8166519768438));
#149676=CARTESIAN_POINT('Ctrl Pts',(-6.91865453650782,-1.1357138578708,
46.8253238167561));
#149677=CARTESIAN_POINT('Ctrl Pts',(-6.88771393580554,-1.32420088383036,
46.8339956305407));
#149678=CARTESIAN_POINT('Ctrl Pts',(-6.84906655865352,-1.51142267991482,
46.8426674443253));
#149679=CARTESIAN_POINT('Ctrl Pts',(-6.80284135383333,-1.69675457184448,
46.8513392581098));
#149680=CARTESIAN_POINT('Ctrl Pts',(-6.75661628451684,-1.88208592049568,
46.860011046474));
#149681=CARTESIAN_POINT('Ctrl Pts',(-6.70281350071267,-2.06552710052184,
46.8686828348382));
#149682=CARTESIAN_POINT('Ctrl Pts',(-6.64161251687414,-2.24646605543035,
46.8773546232023));
#149683=CARTESIAN_POINT('Ctrl Pts',(-6.58041170744734,-2.42740449469558,
46.8860263868535));
#149684=CARTESIAN_POINT('Ctrl Pts',(-6.51181283117083,-2.60584045409099,
46.8946981505046));
#149685=CARTESIAN_POINT('Ctrl Pts',(-6.43604476876016,-2.78117858056885,
46.9033699141557));
#149686=CARTESIAN_POINT('Ctrl Pts',(-6.35684774728027,-2.964451808458,46.9124341271011));
#149687=CARTESIAN_POINT('Ctrl Pts',(-6.26981768815432,-3.14433998862709,
46.9214983400465));
#149688=CARTESIAN_POINT('Ctrl Pts',(-6.17527181577862,-3.32018742900912,
46.9305625529918));
#149689=CARTESIAN_POINT('Ctrl Pts',(-6.08368050191467,-3.49053963687921,
46.9393435092827));
#149690=CARTESIAN_POINT('Ctrl Pts',(-5.98503618716342,-3.65709956719063,
46.9481244655735));
#149691=CARTESIAN_POINT('Ctrl Pts',(-5.87967633129822,-3.81929742252048,
46.9569054218643));
#149692=CARTESIAN_POINT('Ctrl Pts',(-5.77561495477403,-3.97949631379923,
46.9655781596098));
#149693=CARTESIAN_POINT('Ctrl Pts',(-5.66500279404917,-4.1354398025804,
46.9742508973553));
#149694=CARTESIAN_POINT('Ctrl Pts',(-5.54820899034255,-4.28660746534857,
46.9829236351008));
#149695=CARTESIAN_POINT('Ctrl Pts',(-5.43141636368016,-4.43777360465386,
46.9915962854427));
#149696=CARTESIAN_POINT('Ctrl Pts',(-5.30844239242327,-4.58416378941009,
47.0002689357846));
#149697=CARTESIAN_POINT('Ctrl Pts',(-5.1796974640672,-4.72528948777066,
47.0089415861265));
#149698=CARTESIAN_POINT('Ctrl Pts',(-5.05095379116422,-4.86641380994734,
47.0176141518973));
#149699=CARTESIAN_POINT('Ctrl Pts',(-4.91643946526549,-5.00227353855249,
47.0262867176681));
#149700=CARTESIAN_POINT('Ctrl Pts',(-4.77660337747524,-5.132415292705,47.0349592834388));
#149701=CARTESIAN_POINT('Ctrl Pts',(-4.63676860764104,-5.26255582027063,
47.0436317674706));
#149702=CARTESIAN_POINT('Ctrl Pts',(-4.49161238426534,-5.38697828766591,
47.0523042515024));
#149703=CARTESIAN_POINT('Ctrl Pts',(-4.34161910267142,-5.50526748939764,
47.0609767355342));
#149704=CARTESIAN_POINT('Ctrl Pts',(-4.19162718580059,-5.62355561486781,
47.0696491406588));
#149705=CARTESIAN_POINT('Ctrl Pts',(-4.03679852185878,-5.73571041041759,
47.0783215457835));
#149706=CARTESIAN_POINT('Ctrl Pts',(-3.87764977431105,-5.84135761533956,
47.0869939509081));
#149707=CARTESIAN_POINT('Ctrl Pts',(-3.71850242283774,-5.94700389350991,
47.0956662799573));
#149708=CARTESIAN_POINT('Ctrl Pts',(-3.55503530027938,-6.0461425381676,
47.1043386090064));
#149709=CARTESIAN_POINT('Ctrl Pts',(-3.38779388708872,-6.13844272931697,
47.1130109380556));
#149710=CARTESIAN_POINT('Ctrl Pts',(-3.22055388637478,-6.23074214092334,
47.1216831938605));
#149711=CARTESIAN_POINT('Ctrl Pts',(-3.04953990753037,-6.31620307733225,
47.1303554496654));
#149712=CARTESIAN_POINT('Ctrl Pts',(-2.87532260480704,-6.39454036509159,
47.1390277054704));
#149713=CARTESIAN_POINT('Ctrl Pts',(-2.70110671661545,-6.47287701680285,
47.1476998908622));
#149714=CARTESIAN_POINT('Ctrl Pts',(-2.52368781567056,-6.54409001911157,
47.1563720762541));
#149715=CARTESIAN_POINT('Ctrl Pts',(-2.34365791911847,-6.6079417461607,
47.1650442616459));
#149716=CARTESIAN_POINT('Ctrl Pts',(-2.16362942553754,-6.67179297561396,
47.1737163794555));
#149717=CARTESIAN_POINT('Ctrl Pts',(-1.98099024478141,-6.72828294965251,
47.1823884972651));
#149718=CARTESIAN_POINT('Ctrl Pts',(-1.79634980370613,-6.77722317363277,
47.1910606150747));
#149719=CARTESIAN_POINT('Ctrl Pts',(-1.61171074127587,-6.82616303219364,
47.1997326681326));
#149720=CARTESIAN_POINT('Ctrl Pts',(-1.42507072299089,-6.8675531807264,
47.2084047211905));
#149721=CARTESIAN_POINT('Ctrl Pts',(-1.23705251633311,-6.90125551145108,
47.2170767742485));
#149722=CARTESIAN_POINT('Ctrl Pts',(-1.04903565218561,-6.93495760153032,
47.2257487653852));
#149723=CARTESIAN_POINT('Ctrl Pts',(-0.85964089893486,-6.96097193353472,
47.2344207565219));
#149724=CARTESIAN_POINT('Ctrl Pts',(-0.66950020685584,-6.97921170588198,
47.2430927476586));
#149725=CARTESIAN_POINT('Ctrl Pts',(-0.479360810398374,-6.99745135394315,
47.2517646797042));
#149726=CARTESIAN_POINT('Ctrl Pts',(-0.288475768009516,-7.00791652123639,
47.2604366117498));
#149727=CARTESIAN_POINT('Ctrl Pts',(-0.0974819939155687,-7.0105722892901,
47.2691085437955));
#149728=CARTESIAN_POINT('Ctrl Pts',(0.0935105410641958,-7.01322804011393,
47.27778041958));
#149729=CARTESIAN_POINT('Ctrl Pts',(0.284611522350782,-7.00807448913577,
47.2864522953646));
#149730=CARTESIAN_POINT('Ctrl Pts',(0.475183323473319,-6.99512883166514,
47.2951241711491));
#149731=CARTESIAN_POINT('Ctrl Pts',(0.665753950397314,-6.98218325395852,
47.3037959935024));
#149732=CARTESIAN_POINT('Ctrl Pts',(0.855795120329706,-6.9614456850821,
47.3124678158556));
#149733=CARTESIAN_POINT('Ctrl Pts',(1.04467275076626,-6.93298531704103,
47.3211396382088));
#149734=CARTESIAN_POINT('Ctrl Pts',(1.23354927906719,-6.90452511507142,
47.3298114099604));
#149735=CARTESIAN_POINT('Ctrl Pts',(1.42126200063211,-6.86834224643024,
47.3384831817119));
#149736=CARTESIAN_POINT('Ctrl Pts',(1.60718460925101,-6.82455743578195,
47.3471549534635));
#149737=CARTESIAN_POINT('Ctrl Pts',(1.79763389406226,-6.77970659200611,
47.356037857702));
#149738=CARTESIAN_POINT('Ctrl Pts',(1.98620448432225,-6.72687898190764,
47.3649207619404));
#149739=CARTESIAN_POINT('Ctrl Pts',(2.17223623428182,-6.66625954377514,
47.3738036661789));
#149740=CARTESIAN_POINT('Ctrl Pts',(2.3538653218636,-6.60707473666497,47.3824763459353));
#149741=CARTESIAN_POINT('Ctrl Pts',(2.53307410228002,-6.54046283696397,
47.3911490256916));
#149742=CARTESIAN_POINT('Ctrl Pts',(2.70926451774568,-6.46664614273769,
47.3998217054479));
#149743=CARTESIAN_POINT('Ctrl Pts',(2.88545151536487,-6.39283088045156,
47.4084942169665));
#149744=CARTESIAN_POINT('Ctrl Pts',(3.05862000314713,-6.3118112131087,47.417166728485));
#149745=CARTESIAN_POINT('Ctrl Pts',(3.22819210344548,-6.22385751007784,
47.4258392400036));
#149746=CARTESIAN_POINT('Ctrl Pts',(3.39776113571412,-6.13590539837345,
47.4345115946123));
#149747=CARTESIAN_POINT('Ctrl Pts',(3.56373365851512,-6.04101963283718,
47.4431839492211));
#149748=CARTESIAN_POINT('Ctrl Pts',(3.72555582775681,-5.93951684371442,
47.4518563038298));
#149749=CARTESIAN_POINT('Ctrl Pts',(3.88737528046907,-5.83801575853195,
47.4605285128546));
#149750=CARTESIAN_POINT('Ctrl Pts',(4.0450442783934,-5.72989802299362,47.4692007218795));
#149751=CARTESIAN_POINT('Ctrl Pts',(4.19803670363638,-5.61552440983225,
47.4778729309043));
#149752=CARTESIAN_POINT('Ctrl Pts',(4.35102676030492,-5.50115256736257,
47.4865450056691));
#149753=CARTESIAN_POINT('Ctrl Pts',(4.49934016166879,-5.38052521115584,
47.4952170804338));
#149754=CARTESIAN_POINT('Ctrl Pts',(4.64248202337103,-5.25404484422971,
47.5038891551986));
#149755=CARTESIAN_POINT('Ctrl Pts',(4.78562185584888,-5.12756627032935,
47.5125611070253));
#149756=CARTESIAN_POINT('Ctrl Pts',(4.92359008252787,-4.99523503981853,
47.5212330588519));
#149757=CARTESIAN_POINT('Ctrl Pts',(5.05592635132523,-4.85749269608048,
47.5299050106786));
#149758=CARTESIAN_POINT('Ctrl Pts',(5.18826091680615,-4.71975212524111,
47.5385768508876));
#149759=CARTESIAN_POINT('Ctrl Pts',(5.31496347269748,-4.57660078535016,
47.5472486910965));
#149760=CARTESIAN_POINT('Ctrl Pts',(5.43561126742136,-4.42851631045681,
47.5559205313054));
#149761=CARTESIAN_POINT('Ctrl Pts',(5.56176013705839,-4.27367975367312,
47.5649877740389));
#149762=CARTESIAN_POINT('Ctrl Pts',(5.6812889568676,-4.11344992040764,47.5740550167725));
#149763=CARTESIAN_POINT('Ctrl Pts',(5.79376175354239,-3.94841123816776,
47.583122259506));
#149764=CARTESIAN_POINT('Ctrl Pts',(5.90133874236535,-3.79055649462464,
47.5917948158845));
#149765=CARTESIAN_POINT('Ctrl Pts',(6.00246078174406,-3.62830291661375,
47.6004673722629));
#149766=CARTESIAN_POINT('Ctrl Pts',(6.09679041553473,-3.46219196341621,
47.6091399286413));
#149767=CARTESIAN_POINT('Ctrl Pts',(6.19111669178891,-3.29608692271475,
47.6178121763318));
#149768=CARTESIAN_POINT('Ctrl Pts',(6.27865090596437,-3.1261250286051,47.6264844240222));
#149769=CARTESIAN_POINT('Ctrl Pts',(6.35910096686233,-2.9528734235911,47.6351566717127));
#149770=CARTESIAN_POINT('Ctrl Pts',(6.43954858437163,-2.77962708048742,
47.643828656014));
#149771=CARTESIAN_POINT('Ctrl Pts',(6.51291235952087,-2.60309148403624,
47.6525006403153));
#149772=CARTESIAN_POINT('Ctrl Pts',(6.57894750102587,-2.42385567665353,
47.6611726246166));
#149773=CARTESIAN_POINT('Ctrl Pts',(6.64498098171233,-2.24462437714561,
47.6698443908129));
#149774=CARTESIAN_POINT('Ctrl Pts',(6.70368609940979,-2.06269326909623,
47.6785161570093));
#149775=CARTESIAN_POINT('Ctrl Pts',(6.7548669838948,-1.87866936750137,47.6871879232056));
#149776=CARTESIAN_POINT('Ctrl Pts',(6.80605126222585,-1.69463326313208,
47.6958602644338));
#149777=CARTESIAN_POINT('Ctrl Pts',(6.84971023276694,-1.5085043611762,47.704532605662));
#149778=CARTESIAN_POINT('Ctrl Pts',(6.88569820761785,-1.32090376489296,
47.7132049468903));
#149779=CARTESIAN_POINT('Ctrl Pts',(6.92168406448285,-1.13331420939267,
47.7218767777286));
#149780=CARTESIAN_POINT('Ctrl Pts',(6.9499997755384,-0.944253411825118,
47.730548608567));
#149781=CARTESIAN_POINT('Ctrl Pts',(6.9705508637189,-0.754352184863043,
47.7392204394054));
#149782=CARTESIAN_POINT('Ctrl Pts',(6.99110229108043,-0.564447823716972,
47.7478924133661));
#149783=CARTESIAN_POINT('Ctrl Pts',(7.00388880856507,-0.373703287791058,
47.7565643873269));
#149784=CARTESIAN_POINT('Ctrl Pts',(7.00886775178468,-0.182755028638717,
47.7652363612876));
#149785=CARTESIAN_POINT('Ctrl Pts',(7.01045582731897,-0.121850486188999,
47.7680023598286));
#149786=CARTESIAN_POINT('Ctrl Pts',(7.01125000000003,-0.0609252433271906,
47.7707683583695));
#149787=CARTESIAN_POINT('Ctrl Pts',(7.01125,3.56735043106814E-12,47.7735343569105));
#149788=CARTESIAN_POINT('Ctrl Pts',(7.01124848872571,0.00460345972294059,
47.7735343569105));
#149789=CARTESIAN_POINT('Ctrl Pts',(7.01111020263014,0.215218570302498,
47.7830916938172));
#149790=CARTESIAN_POINT('Ctrl Pts',(7.00147759625489,0.425596535594836,
47.7926490307239));
#149791=CARTESIAN_POINT('Ctrl Pts',(6.9824391034497,0.634957265582918,47.8022063676305));
#149792=CARTESIAN_POINT('Ctrl Pts',(6.96334835668509,0.844892617060276,
47.8117899360619));
#149793=CARTESIAN_POINT('Ctrl Pts',(6.93480007718454,1.05380505887218,47.8213735044934));
#149794=CARTESIAN_POINT('Ctrl Pts',(6.8969345210992,1.26092060581554,47.8309570729248));
#149795=CARTESIAN_POINT('Ctrl Pts',(6.85898843994858,1.46847660563112,47.8405610218168));
#149796=CARTESIAN_POINT('Ctrl Pts',(6.81168544968352,1.67422797938378,47.8501649707087));
#149797=CARTESIAN_POINT('Ctrl Pts',(6.75521722589369,1.87740959662223,47.8597689196007));
#149798=CARTESIAN_POINT('Ctrl Pts',(6.70193906218384,2.06911287219101,47.8688303124866));
#149799=CARTESIAN_POINT('Ctrl Pts',(6.6405023909177,2.25852859407412,47.8778917053725));
#149800=CARTESIAN_POINT('Ctrl Pts',(6.57110895151812,2.44502632087642,47.8869530982584));
#149801=CARTESIAN_POINT('',(7.01124900031637,0.0037440703390971,47.2264656430477));
#149802=CARTESIAN_POINT('Ctrl Pts',(6.57110895151816,2.44502632087632,47.3397953554189));
#149803=CARTESIAN_POINT('Ctrl Pts',(6.63537926896215,2.27229719535844,47.3314250544072));
#149804=CARTESIAN_POINT('Ctrl Pts',(6.69280958576941,2.09710061241682,47.3230547533954));
#149805=CARTESIAN_POINT('Ctrl Pts',(6.74323350051052,1.92000742709311,47.3146844523836));
#149806=CARTESIAN_POINT('Ctrl Pts',(6.79369723377461,1.74277439564464,47.3063075415514));
#149807=CARTESIAN_POINT('Ctrl Pts',(6.83714342931925,1.56364208808661,47.2979306307192));
#149808=CARTESIAN_POINT('Ctrl Pts',(6.87345634102338,1.38319358390121,47.2895537198869));
#149809=CARTESIAN_POINT('Ctrl Pts',(6.88306397555093,1.3354506958238,47.2873373650432));
#149810=CARTESIAN_POINT('Ctrl Pts',(6.89217254502337,1.28761571539511,47.2851210101995));
#149811=CARTESIAN_POINT('Ctrl Pts',(6.90078051029069,1.23969952459951,47.2829046553557));
#149812=CARTESIAN_POINT('Ctrl Pts',(6.93731384930597,1.03633689611582,47.2734981533114));
#149813=CARTESIAN_POINT('Ctrl Pts',(6.96489074497273,0.831146044054557,
47.264091651267));
#149814=CARTESIAN_POINT('Ctrl Pts',(6.98334685255806,0.624894630611765,
47.2546851492227));
#149815=CARTESIAN_POINT('Ctrl Pts',(7.00180296014339,0.418643217168973,
47.2452786471783));
#149816=CARTESIAN_POINT('Ctrl Pts',(7.01113814671998,0.211331509871976,
47.235872145134));
#149817=CARTESIAN_POINT('Ctrl Pts',(7.01124900031588,0.00374407126288481,
47.2264656430896));
#149818=CARTESIAN_POINT('Ctrl Pts',(7.01124900031637,0.00374407033909243,
47.2264656430477));
#149819=CARTESIAN_POINT('Ctrl Pts',(7.01133805377372,-0.163019880989669,
47.2189089938612));
#149820=CARTESIAN_POINT('Ctrl Pts',(7.00547309213724,-0.329959880594732,
47.2113523446747));
#149821=CARTESIAN_POINT('Ctrl Pts',(6.99364288946165,-0.496573959428494,
47.2037956954882));
#149822=CARTESIAN_POINT('Ctrl Pts',(6.98181519998804,-0.66315264285587,
47.1962406516323));
#149823=CARTESIAN_POINT('Ctrl Pts',(6.96402480635603,-0.829405141217421,
47.1886856077763));
#149824=CARTESIAN_POINT('Ctrl Pts',(6.94031258484574,-0.994830531865516,
47.1811305639204));
#149825=CARTESIAN_POINT('Ctrl Pts',(6.91660374076276,-1.16023236030828,
47.1735765961598));
#149826=CARTESIAN_POINT('Ctrl Pts',(6.88697480798972,-1.32480691708793,
47.1660226283992));
#149827=CARTESIAN_POINT('Ctrl Pts',(6.85151831906088,-1.4880602427567,47.1584686606386));
#149828=CARTESIAN_POINT('Ctrl Pts',(6.81604972350294,-1.65136931132397,
47.1509121135734));
#149829=CARTESIAN_POINT('Ctrl Pts',(6.77474968933664,-1.81335585520407,
47.1433555665082));
#149830=CARTESIAN_POINT('Ctrl Pts',(6.72776143470871,-1.97353810202544,
47.135799019443));
#149831=CARTESIAN_POINT('Ctrl Pts',(6.70379677739981,-2.05523325504701,
47.1319450763184));
#149832=CARTESIAN_POINT('Ctrl Pts',(6.67835333670491,-2.13645932533242,
47.1280911331939));
#149833=CARTESIAN_POINT('Ctrl Pts',(6.65145502672404,-2.21715416468216,
47.1242371900694));
#149834=CARTESIAN_POINT('Ctrl Pts',(6.58406734638552,-2.41931697873763,
47.1145820003009));
#149835=CARTESIAN_POINT('Ctrl Pts',(6.50755438751975,-2.61811991118926,
47.1049268105323));
#149836=CARTESIAN_POINT('Ctrl Pts',(6.42227030571619,-2.81284032302157,
47.0952716207638));
#149837=CARTESIAN_POINT('Ctrl Pts',(6.33651370934528,-3.00863957898522,
47.0855629366301));
#149838=CARTESIAN_POINT('Ctrl Pts',(6.2418885974367,-3.2003109294957,47.0758542524964));
#149839=CARTESIAN_POINT('Ctrl Pts',(6.13879776728405,-3.38715050372556,
47.0661455683627));
#149840=CARTESIAN_POINT('Ctrl Pts',(6.03521067167438,-3.57488949865616,
47.0563901479231));
#149841=CARTESIAN_POINT('Ctrl Pts',(5.92307619790506,-3.757750059978,47.0466347274835));
#149842=CARTESIAN_POINT('Ctrl Pts',(5.8028451586132,-3.93504950765036,47.036879307044));
#149843=CARTESIAN_POINT('Ctrl Pts',(5.68249490884342,-4.11252474979324,
47.0271142139912));
#149844=CARTESIAN_POINT('Ctrl Pts',(5.55403206681813,-4.2844278237235,47.0173491209385));
#149845=CARTESIAN_POINT('Ctrl Pts',(5.41795030919277,-4.45010573016169,
47.0075840278858));
#149846=CARTESIAN_POINT('Ctrl Pts',(5.2820537653651,-4.61555814102444,46.997832225593));
#149847=CARTESIAN_POINT('Ctrl Pts',(5.13855905542658,-4.77480228909225,
46.9880804233002));
#149848=CARTESIAN_POINT('Ctrl Pts',(4.98799875327024,-4.92721980429883,
46.9783286210073));
#149849=CARTESIAN_POINT('Ctrl Pts',(4.92233624928531,-4.99369227782795,
46.9740756555992));
#149850=CARTESIAN_POINT('Ctrl Pts',(4.85533038262588,-5.0588667289273,46.969822690191));
#149851=CARTESIAN_POINT('Ctrl Pts',(4.7870277619448,-5.12269380003039,46.9655697247829));
#149852=CARTESIAN_POINT('Ctrl Pts',(4.65802278161931,-5.24324569056962,
46.9575370356513));
#149853=CARTESIAN_POINT('Ctrl Pts',(4.5243262391785,-5.35904729458481,46.9495043465197));
#149854=CARTESIAN_POINT('Ctrl Pts',(4.38633022244782,-5.46971057206329,
46.9414716573881));
#149855=CARTESIAN_POINT('Ctrl Pts',(4.24842295027931,-5.58030268253027,
46.9334441340395));
#149856=CARTESIAN_POINT('Ctrl Pts',(4.10622199235734,-5.68576281560668,
46.9254166106909));
#149857=CARTESIAN_POINT('Ctrl Pts',(3.96015481489761,-5.78574112837269,
46.9173890873423));
#149858=CARTESIAN_POINT('Ctrl Pts',(3.81415362062243,-5.88567427775856,
46.9093651902811));
#149859=CARTESIAN_POINT('Ctrl Pts',(3.66428998616904,-5.9801303308086,46.9013412932198));
#149860=CARTESIAN_POINT('Ctrl Pts',(3.51102280616601,-6.06880098677508,
46.8933173961586));
#149861=CARTESIAN_POINT('Ctrl Pts',(3.35777418886415,-6.15746090354163,
46.8852944708983));
#149862=CARTESIAN_POINT('Ctrl Pts',(3.20112316035059,-6.24033662872264,
46.8772715456381));
#149863=CARTESIAN_POINT('Ctrl Pts',(3.04155597700651,-6.31716422148704,
46.8692486203779));
#149864=CARTESIAN_POINT('Ctrl Pts',(2.88200189084887,-6.39398550828499,
46.8612263536349));
#149865=CARTESIAN_POINT('Ctrl Pts',(2.71953245875733,-6.46475949605074,
46.853204086892));
#149866=CARTESIAN_POINT('Ctrl Pts',(2.55465653826101,-6.5292692189877,46.8451818201491));
#149867=CARTESIAN_POINT('Ctrl Pts',(2.38971864118606,-6.59380319102001,
46.8371565378497));
#149868=CARTESIAN_POINT('Ctrl Pts',(2.22237279135252,-6.65206806339079,
46.8291312555503));
#149869=CARTESIAN_POINT('Ctrl Pts',(2.05314609058131,-6.70389571019946,
46.8211059732509));
#149870=CARTESIAN_POINT('Ctrl Pts',(1.95330961847189,-6.73447179181974,
46.8163714019994));
#149871=CARTESIAN_POINT('Ctrl Pts',(1.85281882675055,-6.76280834132154,
46.811636830748));
#149872=CARTESIAN_POINT('Ctrl Pts',(1.75178407774357,-6.78887907591998,
46.8069022594965));
#149873=CARTESIAN_POINT('Ctrl Pts',(1.56547532649853,-6.83695368445631,
46.798171678521));
#149874=CARTESIAN_POINT('Ctrl Pts',(1.37722330343465,-6.87734522639827,
46.7894410975456));
#149875=CARTESIAN_POINT('Ctrl Pts',(1.18766252571079,-6.90992650377139,
46.7807105165701));
#149876=CARTESIAN_POINT('Ctrl Pts',(0.99804667740148,-6.94251724655207,
46.7719773992144));
#149877=CARTESIAN_POINT('Ctrl Pts',(0.807121585391957,-6.96729314928906,
46.7632442818587));
#149878=CARTESIAN_POINT('Ctrl Pts',(0.615529822806346,-6.98417852003627,
46.7545111645031));
#149879=CARTESIAN_POINT('Ctrl Pts',(0.421234205747432,-7.00130218696391,
46.745654800312));
#149880=CARTESIAN_POINT('Ctrl Pts',(0.22625324723321,-7.01031089814164,
46.7367984361209));
#149881=CARTESIAN_POINT('Ctrl Pts',(0.0312606778596215,-7.01118030951421,
46.7279420719298));
#149882=CARTESIAN_POINT('Ctrl Pts',(-0.161141059103698,-7.01203816916884,
46.7192033807119));
#149883=CARTESIAN_POINT('Ctrl Pts',(-0.353553822554361,-7.00497170861606,
46.710464689494));
#149884=CARTESIAN_POINT('Ctrl Pts',(-0.545331116062804,-6.99001005266471,
46.7017259982761));
#149885=CARTESIAN_POINT('Ctrl Pts',(-0.740982045293665,-6.97474619198464,
46.6928107975984));
#149886=CARTESIAN_POINT('Ctrl Pts',(-0.935971264890385,-6.95126481781544,
46.6838955969208));
#149887=CARTESIAN_POINT('Ctrl Pts',(-1.12961752830356,-6.91965250588853,
46.6749803962431));
#149888=CARTESIAN_POINT('Ctrl Pts',(-1.32326379171673,-6.88804019396161,
46.6660651955655));
#149889=CARTESIAN_POINT('Ctrl Pts',(-1.51556680177303,-6.84829699893491,
46.6571499948878));
#149890=CARTESIAN_POINT('Ctrl Pts',(-1.70585504549666,-6.80056505933541,
46.6482347942101));
#149891=CARTESIAN_POINT('Ctrl Pts',(-1.8924107996392,-6.75376937813924,
46.6394944645229));
#149892=CARTESIAN_POINT('Ctrl Pts',(-2.07704992960731,-6.69929046862994,
46.6307541348356));
#149893=CARTESIAN_POINT('Ctrl Pts',(-2.25915114490896,-6.63730839022541,
46.6220138051484));
#149894=CARTESIAN_POINT('Ctrl Pts',(-2.44121948182397,-6.57533750268928,
46.6132750535282));
#149895=CARTESIAN_POINT('Ctrl Pts',(-2.62075056001516,-6.50586623989363,
46.604536301908));
#149896=CARTESIAN_POINT('Ctrl Pts',(-2.79713963903848,-6.42912407737008,
46.5957975502879));
#149897=CARTESIAN_POINT('Ctrl Pts',(-2.97582506732171,-6.35138283480659,
46.5869450318409));
#149898=CARTESIAN_POINT('Ctrl Pts',(-3.15128584389833,-6.26618014521787,
46.5780925133938));
#149899=CARTESIAN_POINT('Ctrl Pts',(-3.32291432147881,-6.17380490253871,
46.5692399949468));
#149900=CARTESIAN_POINT('Ctrl Pts',(-3.49225022036918,-6.08266358977518,
46.560505726661));
#149901=CARTESIAN_POINT('Ctrl Pts',(-3.65785532263737,-5.98454029265149,
46.5517714583752));
#149902=CARTESIAN_POINT('Ctrl Pts',(-3.81916997763898,-5.87975911448769,
46.5430371900894));
#149903=CARTESIAN_POINT('Ctrl Pts',(-3.98376060551057,-5.77285004349887,
46.5341255465618));
#149904=CARTESIAN_POINT('Ctrl Pts',(-4.14388440592885,-5.65900992260237,
46.5252139030341));
#149905=CARTESIAN_POINT('Ctrl Pts',(-4.2989763871825,-5.53863056945915,
46.5163022595065));
#149906=CARTESIAN_POINT('Ctrl Pts',(-4.4540683684362,-5.41825121631588,
46.5073906159788));
#149907=CARTESIAN_POINT('Ctrl Pts',(-4.60412828264362,-5.29133280628025,
46.4984789724512));
#149908=CARTESIAN_POINT('Ctrl Pts',(-4.7486246754473,-5.15831273327171,
46.4895673289236));
#149909=CARTESIAN_POINT('Ctrl Pts',(-4.87875740055003,-5.03851552409512,
46.4815415475536));
#149910=CARTESIAN_POINT('Ctrl Pts',(-5.00443717117772,-4.9137139901756,
46.4735157661836));
#149911=CARTESIAN_POINT('Ctrl Pts',(-5.12525756911808,-4.78428274798823,
46.4654899848136));
#149912=CARTESIAN_POINT('Ctrl Pts',(-5.24603963359131,-4.65489257128611,
46.457466749835));
#149913=CARTESIAN_POINT('Ctrl Pts',(-5.36196514505517,-4.52087587839287,
46.4494435148564));
#149914=CARTESIAN_POINT('Ctrl Pts',(-5.47266451228036,-4.38264414463771,
46.4414202798778));
#149915=CARTESIAN_POINT('Ctrl Pts',(-5.58334992904249,-4.24442983100647,
46.4333980559967));
#149916=CARTESIAN_POINT('Ctrl Pts',(-5.68881028482749,-4.10200182098042,
46.4253758321155));
#149917=CARTESIAN_POINT('Ctrl Pts',(-5.78871629840333,-3.95580461841832,
46.4173536082344));
#149918=CARTESIAN_POINT('Ctrl Pts',(-5.88865944579762,-3.80955307618052,
46.4093284025927));
#149919=CARTESIAN_POINT('Ctrl Pts',(-5.98304391732017,-3.65952984396228,
46.401303196951));
#149920=CARTESIAN_POINT('Ctrl Pts',(-6.07158355952368,-3.50620872770315,
46.3932779913094));
#149921=CARTESIAN_POINT('Ctrl Pts',(-6.16014064428648,-3.35285740675159,
46.3852512046796));
#149922=CARTESIAN_POINT('Ctrl Pts',(-6.24285043017741,-3.19620722929424,
46.3772244180497));
#149923=CARTESIAN_POINT('Ctrl Pts',(-6.31947287807022,-3.03675634614221,
46.3691976314199));
#149924=CARTESIAN_POINT('Ctrl Pts',(-6.39615683968545,-2.87717745327973,
46.3611644007579));
#149925=CARTESIAN_POINT('Ctrl Pts',(-6.46674355235671,-2.71479369835474,
46.3531311700958));
#149926=CARTESIAN_POINT('Ctrl Pts',(-6.53104100822,-2.5501235090577,46.3450979394338));
#149927=CARTESIAN_POINT('Ctrl Pts',(-6.56892116670468,-2.45310982811927,
46.3403652475016));
#149928=CARTESIAN_POINT('Ctrl Pts',(-6.60461934743842,-2.35530289510654,
46.3356325555694));
#149929=CARTESIAN_POINT('Ctrl Pts',(-6.63810442454595,-2.25681107125154,
46.3308998636373));
#149930=CARTESIAN_POINT('Ctrl Pts',(-6.70709429909258,-2.05388668944988,
46.3211490178614));
#149931=CARTESIAN_POINT('Ctrl Pts',(-6.76672836725575,-1.84793490421423,
46.3113981720856));
#149932=CARTESIAN_POINT('Ctrl Pts',(-6.8168066730418,-1.63974795162941,
46.3016473263097));
#149933=CARTESIAN_POINT('Ctrl Pts',(-6.86695709865057,-1.43126118047285,
46.2918824379408));
#149934=CARTESIAN_POINT('Ctrl Pts',(-6.90752422550909,-1.22053284070518,
46.282117549572));
#149935=CARTESIAN_POINT('Ctrl Pts',(-6.93835866734817,-1.00836777305433,
46.2723526612031));
#149936=CARTESIAN_POINT('Ctrl Pts',(-6.96914171415797,-0.79655634338794,
46.2626040490076));
#149937=CARTESIAN_POINT('Ctrl Pts',(-6.99022449267146,-0.583313009512905,
46.2528554368122));
#149938=CARTESIAN_POINT('Ctrl Pts',(-7.00150950686121,-0.369447138075453,
46.2431068246167));
#149939=CARTESIAN_POINT('Ctrl Pts',(-7.01276355231825,-0.15616816488158,
46.2333849649056));
#149940=CARTESIAN_POINT('Ctrl Pts',(-7.01427350758934,0.0577298954421971,
46.2236631051945));
#149941=CARTESIAN_POINT('Ctrl Pts',(-7.00599378042487,0.271436385085205,
46.2139412454834));
#149942=CARTESIAN_POINT('Ctrl Pts',(-6.99776883006673,0.483729040822207,
46.2042837034021));
#149943=CARTESIAN_POINT('Ctrl Pts',(-6.97988327480615,0.695832604492826,
46.1946261613208));
#149944=CARTESIAN_POINT('Ctrl Pts',(-6.95234327129287,0.90694520264944,
46.1849686192395));
#149945=CARTESIAN_POINT('Ctrl Pts',(-6.94023682415646,0.999749239808647,
46.1807232122766));
#149946=CARTESIAN_POINT('Ctrl Pts',(-6.92626538129789,1.09236168942198,
46.1764778053136));
#149947=CARTESIAN_POINT('Ctrl Pts',(-6.91043263731572,1.18471402778128,
46.1722323983507));
#149948=CARTESIAN_POINT('Ctrl Pts',(-6.88115006925828,1.35551914130519,
46.1643805428249));
#149949=CARTESIAN_POINT('Ctrl Pts',(-6.84550896167075,1.52536372061138,
46.1565286872992));
#149950=CARTESIAN_POINT('Ctrl Pts',(-6.80359719615246,1.69372127429703,
46.1486768317735));
#149951=CARTESIAN_POINT('Ctrl Pts',(-6.76169731632826,1.86203108371913,
46.1408272029435));
#149952=CARTESIAN_POINT('Ctrl Pts',(-6.7135304079491,2.02885433656054,46.1329775741136));
#149953=CARTESIAN_POINT('Ctrl Pts',(-6.65923534359031,2.19367527249993,
46.1251279452837));
#149954=CARTESIAN_POINT('Ctrl Pts',(-6.60494461383931,2.35848305007732,
46.1172789431233));
#149955=CARTESIAN_POINT('Ctrl Pts',(-6.54452682210903,2.52128846690054,
46.1094299409629));
#149956=CARTESIAN_POINT('Ctrl Pts',(-6.47817045745705,2.68159170766743,
46.1015809388025));
#149957=CARTESIAN_POINT('Ctrl Pts',(-6.41178049842918,2.8419761054922,46.0937279629113));
#149958=CARTESIAN_POINT('Ctrl Pts',(-6.33944610536298,2.99985544324744,
46.0858749870201));
#149959=CARTESIAN_POINT('Ctrl Pts',(-6.26140374268369,3.1547503441012,46.078022011129));
#149960=CARTESIAN_POINT('Ctrl Pts',(-6.18334155971995,3.30968458334621,
46.070167040831));
#149961=CARTESIAN_POINT('Ctrl Pts',(-6.0995687033109,3.4616325415747,46.0623120705331));
#149962=CARTESIAN_POINT('Ctrl Pts',(-6.01036689279294,3.61014076962637,
46.0544571002351));
#149963=CARTESIAN_POINT('Ctrl Pts',(-5.92107654222664,3.75879640416695,
46.0465943332406));
#149964=CARTESIAN_POINT('Ctrl Pts',(-5.82634668332283,3.9040051701298,46.0387315662461));
#149965=CARTESIAN_POINT('Ctrl Pts',(-5.72650185387007,4.04534338222637,
46.0308687992516));
#149966=CARTESIAN_POINT('Ctrl Pts',(-5.65325785170397,4.14902603028829,
46.0251008438558));
#149967=CARTESIAN_POINT('Ctrl Pts',(-5.57726218538689,4.25062642081654,
46.0193328884601));
#149968=CARTESIAN_POINT('Ctrl Pts',(-5.49865615895209,4.34998931126483,
46.0135649330644));
#149969=CARTESIAN_POINT('Ctrl Pts',(-5.38447935815423,4.49431586565217,
46.0051868643068));
#149970=CARTESIAN_POINT('Ctrl Pts',(-5.26454100877773,4.63424025674379,
45.9968087955492));
#149971=CARTESIAN_POINT('Ctrl Pts',(-5.13920747913321,4.76929481673353,
45.9884307267917));
#149972=CARTESIAN_POINT('Ctrl Pts',(-5.01395965020853,4.90425702894497,
45.9800583868006));
#149973=CARTESIAN_POINT('Ctrl Pts',(-4.88332421893273,5.03435580870373,
45.9716860468095));
#149974=CARTESIAN_POINT('Ctrl Pts',(-4.74770737391496,5.15915702941609,
45.9633137068184));
#149975=CARTESIAN_POINT('Ctrl Pts',(-4.61216337295632,5.28389121548023,
45.9549458638737));
#149976=CARTESIAN_POINT('Ctrl Pts',(-4.47164353464269,5.40333329402616,
45.9465780209289));
#149977=CARTESIAN_POINT('Ctrl Pts',(-4.32659072151918,5.51708612321433,
45.9382101779841));
#149978=CARTESIAN_POINT('Ctrl Pts',(-4.18159457173026,5.63079451607285,
45.9298456038479));
#149979=CARTESIAN_POINT('Ctrl Pts',(-4.03206923655545,5.73881788889823,
45.9214810297117));
#149980=CARTESIAN_POINT('Ctrl Pts',(-3.87849080642846,5.8407992284404,45.9131164555755));
#149981=CARTESIAN_POINT('Ctrl Pts',(-3.72494989001698,5.94275565759017,
45.9047539246055));
#149982=CARTESIAN_POINT('Ctrl Pts',(-3.56735812681624,6.03867281536022,
45.8963913936355));
#149983=CARTESIAN_POINT('Ctrl Pts',(-3.4062211180323,6.12823663524596,45.8880288626655));
#149984=CARTESIAN_POINT('Ctrl Pts',(-3.2450712491949,6.21780760305832,45.879665664297));
#149985=CARTESIAN_POINT('Ctrl Pts',(-3.0803758538419,6.30102405501996,45.8713024659285));
#149986=CARTESIAN_POINT('Ctrl Pts',(-2.91266637200884,6.37761720142161,
45.8629392675601));
#149987=CARTESIAN_POINT('Ctrl Pts',(-2.74494545227208,6.45421557152931,
45.8545754988156));
#149988=CARTESIAN_POINT('Ctrl Pts',(-2.57421033517372,6.52418959855192,
45.8462117300712));
#149989=CARTESIAN_POINT('Ctrl Pts',(-2.40101389697498,6.58731803005085,
45.8378479613267));
#149990=CARTESIAN_POINT('Ctrl Pts',(-2.22778255561159,6.65045918341671,
45.8294825070857));
#149991=CARTESIAN_POINT('Ctrl Pts',(-2.05208921299349,6.70675187782401,
45.8211170528447));
#149992=CARTESIAN_POINT('Ctrl Pts',(-1.87450381991222,6.75602412604,45.8127515986037));
#149993=CARTESIAN_POINT('Ctrl Pts',(-1.69685895358428,6.80531287550376,
45.8043833427769));
#149994=CARTESIAN_POINT('Ctrl Pts',(-1.51732108997272,6.84757640266265,
45.7960150869501));
#149995=CARTESIAN_POINT('Ctrl Pts',(-1.33647275299985,6.88269330589334,
45.7876468311232));
#149996=CARTESIAN_POINT('Ctrl Pts',(-1.15545674383999,6.91784276749899,
45.7792708167304));
#149997=CARTESIAN_POINT('Ctrl Pts',(-0.973128156483563,6.94583230183678,
45.7708948023376));
#149998=CARTESIAN_POINT('Ctrl Pts',(-0.790078298962019,6.96659191025348,
45.7625187879448));
#149999=CARTESIAN_POINT('Ctrl Pts',(-0.60693867152268,6.98736169943933,
45.7541386658507));
#150000=CARTESIAN_POINT('Ctrl Pts',(-0.423077395749594,7.00089446147565,
45.7457585437567));
#150001=CARTESIAN_POINT('Ctrl Pts',(-0.239088889927075,7.00717225885117,
45.7373784216626));
#150002=CARTESIAN_POINT('Ctrl Pts',(-0.0548901544622398,7.01345722938727,
45.7289887242418));
#150003=CARTESIAN_POINT('Ctrl Pts',(0.129435772677918,7.01247066604149,
45.7205990268209));
#150004=CARTESIAN_POINT('Ctrl Pts',(0.313295138123823,7.00424676313792,
45.7122093294001));
#150005=CARTESIAN_POINT('Ctrl Pts',(0.430023579301856,6.99902558028435,
45.7068828870972));
#150006=CARTESIAN_POINT('Ctrl Pts',(0.546564033290414,6.99088828203294,
45.7015564447944));
#150007=CARTESIAN_POINT('Ctrl Pts',(0.662766037441756,6.97985442126938,
45.6962300024915));
#150008=CARTESIAN_POINT('Ctrl Pts',(0.845612827108903,6.96249236255977,
45.687848710942));
#150009=CARTESIAN_POINT('Ctrl Pts',(1.02799010320501,6.9379208979741,45.6794674193925));
#150010=CARTESIAN_POINT('Ctrl Pts',(1.20930600317479,6.90617155544122,45.671086127843));
#150011=CARTESIAN_POINT('Ctrl Pts',(1.39039211228032,6.87446245046535,45.6627154583307));
#150012=CARTESIAN_POINT('Ctrl Pts',(1.57041920585015,6.83559365275416,45.6543447888184));
#150013=CARTESIAN_POINT('Ctrl Pts',(1.74879955144228,6.7896484954212,45.6459741193061));
#150014=CARTESIAN_POINT('Ctrl Pts',(1.92697746686699,6.743755477722,45.6376129490243));
#150015=CARTESIAN_POINT('Ctrl Pts',(2.10351204360695,6.69080218713475,45.6292517787426));
#150016=CARTESIAN_POINT('Ctrl Pts',(2.27782432946017,6.63092323033674,45.6208906084608));
#150017=CARTESIAN_POINT('Ctrl Pts',(2.45191042672466,6.57112197280511,45.61254028768));
#150018=CARTESIAN_POINT('Ctrl Pts',(2.6237796764463,6.504413080099,45.6041899668992));
#150019=CARTESIAN_POINT('Ctrl Pts',(2.79286698831164,6.43098130522077,45.5958396461183));
#150020=CARTESIAN_POINT('Ctrl Pts',(2.96182419905083,6.35760603107286,45.5874957503384));
#150021=CARTESIAN_POINT('Ctrl Pts',(3.12800343832374,6.27751831316035,45.5791518545585));
#150022=CARTESIAN_POINT('Ctrl Pts',(3.29085726817442,6.19095186566683,45.5708079587786));
#150023=CARTESIAN_POINT('Ctrl Pts',(3.45358029544781,6.10445494748343,45.5624707647329));
#150024=CARTESIAN_POINT('Ctrl Pts',(3.6129829516199,6.01148983100343,45.5541335706871));
#150025=CARTESIAN_POINT('Ctrl Pts',(3.7685400521827,5.9123373074948,45.5457963766414));
#150026=CARTESIAN_POINT('Ctrl Pts',(3.81974961510443,5.87969619131885,45.5430517634959));
#150027=CARTESIAN_POINT('Ctrl Pts',(3.87054261038123,5.84638490046712,45.5403071503504));
#150028=CARTESIAN_POINT('Ctrl Pts',(3.92090088251406,5.81241454406002,45.537562537205));
#150029=CARTESIAN_POINT('Ctrl Pts',(4.07389262539419,5.70921036701297,45.5292242219516));
#150030=CARTESIAN_POINT('Ctrl Pts',(4.22274432084454,5.60000454975874,45.5208859066983));
#150031=CARTESIAN_POINT('Ctrl Pts',(4.36698754506551,5.48516602699888,45.5125475914449));
#150032=CARTESIAN_POINT('Ctrl Pts',(4.5113215240873,5.3702552502575,45.5042040298991));
#150033=CARTESIAN_POINT('Ctrl Pts',(4.65104099202757,5.24970490318,45.4958604683533));
#150034=CARTESIAN_POINT('Ctrl Pts',(4.78571191560507,5.12392310864787,45.4875169068074));
#150035=CARTESIAN_POINT('Ctrl Pts',(4.92048529777488,4.99804561843575,45.4791669974209));
#150036=CARTESIAN_POINT('Ctrl Pts',(5.0502022349229,4.86692896511709,45.4708170880344));
#150037=CARTESIAN_POINT('Ctrl Pts',(5.17446643729791,4.7310171899685,45.4624671786479));
#150038=CARTESIAN_POINT('Ctrl Pts',(5.29891702836845,4.59490155547835,45.4541047449085));
#150039=CARTESIAN_POINT('Ctrl Pts',(5.41789831963236,4.45397666852577,45.4457423111691));
#150040=CARTESIAN_POINT('Ctrl Pts',(5.53105416893855,4.30871980323246,45.4373798774297));
#150041=CARTESIAN_POINT('Ctrl Pts',(5.64430678273894,4.1633387224683,45.4290102926091));
#150042=CARTESIAN_POINT('Ctrl Pts',(5.75172382447618,4.01361853758819,45.4206407077884));
#150043=CARTESIAN_POINT('Ctrl Pts',(5.85299289451728,3.86006486204963,45.4122711229678));
#150044=CARTESIAN_POINT('Ctrl Pts',(5.95441816036588,3.7062743477573,45.4038886290323));
#150045=CARTESIAN_POINT('Ctrl Pts',(6.04967633645704,3.54863880731891,45.3955061350968));
#150046=CARTESIAN_POINT('Ctrl Pts',(6.13850062200587,3.38768898751547,45.3871236411613));
#150047=CARTESIAN_POINT('Ctrl Pts',(6.16756503448613,3.3350242019505,45.3843807847471));
#150048=CARTESIAN_POINT('Ctrl Pts',(6.19594096614935,3.28200472518559,45.3816379283329));
#150049=CARTESIAN_POINT('Ctrl Pts',(6.22362019657571,3.22864959561655,45.3788950719187));
#150050=CARTESIAN_POINT('Ctrl Pts',(6.31278769891644,3.0567682402662,45.370059072797));
#150051=CARTESIAN_POINT('Ctrl Pts',(6.39488058095618,2.88109530724048,45.3612230736754));
#150052=CARTESIAN_POINT('Ctrl Pts',(6.46959591630812,2.7022130267966,45.3523870745538));
#150053=CARTESIAN_POINT('Ctrl Pts',(6.50510935421322,2.61718731247782,45.348187177643));
#150054=CARTESIAN_POINT('Ctrl Pts',(6.53895666757272,2.53143690837865,45.3439872807322));
#150055=CARTESIAN_POINT('Ctrl Pts',(6.57110895151812,2.4450263208764,45.3397873838214));
#150056=CARTESIAN_POINT('Origin',(0.,0.,50.));
#150057=CARTESIAN_POINT('',(6.57110895151813,2.44502632087639,43.3397490455966));
#150058=CARTESIAN_POINT('',(6.57110895151816,2.4450263208763,43.8869849718596));
#150059=CARTESIAN_POINT('',(6.57110895151814,2.44502632087636,50.));
#150060=CARTESIAN_POINT('',(7.01124983644072,-0.00151443390808588,45.7735343569105));
#150061=CARTESIAN_POINT('Ctrl Pts',(6.57110895151816,2.4450263208763,43.8869849718596));
#150062=CARTESIAN_POINT('Ctrl Pts',(6.50404500432959,2.62526344140636,43.8957172526382));
#150063=CARTESIAN_POINT('Ctrl Pts',(6.42955170457269,2.80276609009301,43.9044495334167));
#150064=CARTESIAN_POINT('Ctrl Pts',(6.3478724394879,2.97693501012198,43.9131818141953));
#150065=CARTESIAN_POINT('Ctrl Pts',(6.26622358124146,3.1510390920774,43.9219108441972));
#150066=CARTESIAN_POINT('Ctrl Pts',(6.17739421514608,3.32181167559486,43.9306398741991));
#150067=CARTESIAN_POINT('Ctrl Pts',(6.08167515762305,3.48867508370307,43.9393689042009));
#150068=CARTESIAN_POINT('Ctrl Pts',(6.07063410843983,3.50792252662069,43.9403757846704));
#150069=CARTESIAN_POINT('Ctrl Pts',(6.05950144112564,3.52711798220248,43.9413826651398));
#150070=CARTESIAN_POINT('Ctrl Pts',(6.04827764177913,3.546260584116,43.9423895456092));
#150071=CARTESIAN_POINT('Ctrl Pts',(5.95881474222489,3.69884284430472,43.9504152099604));
#150072=CARTESIAN_POINT('Ctrl Pts',(5.86351692601779,3.84813525201835,43.9584408743116));
#150073=CARTESIAN_POINT('Ctrl Pts',(5.76266405141671,3.99366117654085,43.9664665386628));
#150074=CARTESIAN_POINT('Ctrl Pts',(5.66184318505012,4.13914091469596,43.9744896558645));
#150075=CARTESIAN_POINT('Ctrl Pts',(5.55547097888886,4.28085624863615,43.9825127730662));
#150076=CARTESIAN_POINT('Ctrl Pts',(5.44387112403516,4.41835871646883,43.9905358902679));
#150077=CARTESIAN_POINT('Ctrl Pts',(5.33228534290148,4.55584384403494,43.9985579956842));
#150078=CARTESIAN_POINT('Ctrl Pts',(5.21547345762989,4.68911687957163,44.0065801011005));
#150079=CARTESIAN_POINT('Ctrl Pts',(5.09379998788155,4.81776174649162,44.0146022065168));
#150080=CARTESIAN_POINT('Ctrl Pts',(4.97208130383797,4.94645441830289,44.0226272929761));
#150081=CARTESIAN_POINT('Ctrl Pts',(4.84549767628146,5.07051521716184,44.0306523794354));
#150082=CARTESIAN_POINT('Ctrl Pts',(4.71445140948555,5.18956399614647,44.0386774658947));
#150083=CARTESIAN_POINT('Ctrl Pts',(4.58337933377496,5.30863622119984,44.0467041328551));
#150084=CARTESIAN_POINT('Ctrl Pts',(4.44784314516642,5.4226942199669,44.0547307998155));
#150085=CARTESIAN_POINT('Ctrl Pts',(4.30827872167567,5.53139774549405,44.0627574667759));
#150086=CARTESIAN_POINT('Ctrl Pts',(4.16860225630352,5.64018853787052,44.0707905775193));
#150087=CARTESIAN_POINT('Ctrl Pts',(4.02489139208581,5.74361605384356,44.0788236882628));
#150088=CARTESIAN_POINT('Ctrl Pts',(3.87761201195225,5.84138268282978,44.0868567990063));
#150089=CARTESIAN_POINT('Ctrl Pts',(3.79082959056224,5.89899037228956,44.0915902029694));
#150090=CARTESIAN_POINT('Ctrl Pts',(3.70280870566545,5.95463343971279,44.0963236069325));
#150091=CARTESIAN_POINT('Ctrl Pts',(3.61364869604596,6.0082584551653,44.1010570108956));
#150092=CARTESIAN_POINT('Ctrl Pts',(3.42997638890585,6.11872760328026,44.1108079657267));
#150093=CARTESIAN_POINT('Ctrl Pts',(3.24136075414954,6.22069591698319,44.1205589205577));
#150094=CARTESIAN_POINT('Ctrl Pts',(3.04853359889174,6.31379992230734,44.1303098753887));
#150095=CARTESIAN_POINT('Ctrl Pts',(2.85542863918095,6.40703806178514,44.140074878338));
#150096=CARTESIAN_POINT('Ctrl Pts',(2.65810005696907,6.49138633085964,44.1498398812872));
#150097=CARTESIAN_POINT('Ctrl Pts',(2.4573027054613,6.5665280001103,44.1596048842364));
#150098=CARTESIAN_POINT('Ctrl Pts',(2.25684004256104,6.64154442338308,44.1693536108991));
#150099=CARTESIAN_POINT('Ctrl Pts',(2.05292020121408,6.7073849030508,44.1791023375617));
#150100=CARTESIAN_POINT('Ctrl Pts',(1.84631346506595,6.76378245889208,44.1888510642244));
#150101=CARTESIAN_POINT('Ctrl Pts',(1.64027378596704,6.8200252248548,44.1985730343336));
#150102=CARTESIAN_POINT('Ctrl Pts',(1.43156197258665,6.86687679600982,44.2082950044428));
#150103=CARTESIAN_POINT('Ctrl Pts',(1.22096058025326,6.90412064089031,44.218016974552));
#150104=CARTESIAN_POINT('Ctrl Pts',(1.01175268593837,6.94111805233811,44.2276746167576));
#150105=CARTESIAN_POINT('Ctrl Pts',(0.800680176714006,6.96863442466148,
44.2373322589631));
#150106=CARTESIAN_POINT('Ctrl Pts',(0.588527999355292,6.98650566137857,
44.2469899011686));
#150107=CARTESIAN_POINT('Ctrl Pts',(0.495279987078003,6.99436067055903,
44.2512347595065));
#150108=CARTESIAN_POINT('Ctrl Pts',(0.401823622799947,7.00035296964335,
44.2554796178443));
#150109=CARTESIAN_POINT('Ctrl Pts',(0.308226627566987,7.0044716366446,44.2597244761821));
#150110=CARTESIAN_POINT('Ctrl Pts',(0.135097350216412,7.01209006328105,
44.2675763228644));
#150111=CARTESIAN_POINT('Ctrl Pts',(-0.0384421541657765,7.01329092209141,
44.2754281695466));
#150112=CARTESIAN_POINT('Ctrl Pts',(-0.211858735308332,7.0080484044257,
44.2832800162288));
#150113=CARTESIAN_POINT('Ctrl Pts',(-0.385226136917442,7.0028073734954,
44.2911296361911));
#150114=CARTESIAN_POINT('Ctrl Pts',(-0.55847030371583,6.99112661239508,
44.2989792561534));
#150115=CARTESIAN_POINT('Ctrl Pts',(-0.731057755024403,6.9730324193509,
44.3068288761157));
#150116=CARTESIAN_POINT('Ctrl Pts',(-0.903631427442471,6.95493967089556,
44.3146778693867));
#150117=CARTESIAN_POINT('Ctrl Pts',(-1.07554810943842,6.93043455032811,
44.3225268626577));
#150118=CARTESIAN_POINT('Ctrl Pts',(-1.24627937678613,6.89959522562719,
44.3303758559287));
#150119=CARTESIAN_POINT('Ctrl Pts',(-1.41709708041024,6.86874028787288,
44.3382288229168));
#150120=CARTESIAN_POINT('Ctrl Pts',(-1.5867277943957,6.83154480648655,44.3460817899048));
#150121=CARTESIAN_POINT('Ctrl Pts',(-1.75465289030244,6.78813816867728,
44.3539347568929));
#150122=CARTESIAN_POINT('Ctrl Pts',(-1.92262063355348,6.74472050703731,
44.3617897182713));
#150123=CARTESIAN_POINT('Ctrl Pts',(-2.08888153018173,6.69508865550268,
44.3696446796497));
#150124=CARTESIAN_POINT('Ctrl Pts',(-2.25293268892498,6.63942172645128,
44.3774996410281));
#150125=CARTESIAN_POINT('Ctrl Pts',(-2.41714668220807,6.58369954330203,
44.3853623991147));
#150126=CARTESIAN_POINT('Ctrl Pts',(-2.57914620064869,6.52193045428565,
44.3932251572014));
#150127=CARTESIAN_POINT('Ctrl Pts',(-2.73844835592382,6.45434172975356,
44.401087915288));
#150128=CARTESIAN_POINT('Ctrl Pts',(-2.85531017612821,6.40475959220826,
44.4068559240149));
#150129=CARTESIAN_POINT('Ctrl Pts',(-2.97072084266621,6.35204663273512,
44.4126239327417));
#150130=CARTESIAN_POINT('Ctrl Pts',(-3.0844986649886,6.29630800931653,44.4183919414685));
#150131=CARTESIAN_POINT('Ctrl Pts',(-3.24976160263635,6.21534734001759,
44.426770007133));
#150132=CARTESIAN_POINT('Ctrl Pts',(-3.41194482915532,6.12782239026753,
44.4351480727975));
#150133=CARTESIAN_POINT('Ctrl Pts',(-3.57051360017444,6.03399197824039,
44.4435261384619));
#150134=CARTESIAN_POINT('Ctrl Pts',(-3.7289739436089,5.94022572641882,44.451898475297));
#150135=CARTESIAN_POINT('Ctrl Pts',(-3.88382447702945,5.84016277525746,
44.4602708121322));
#150136=CARTESIAN_POINT('Ctrl Pts',(-4.03455478636337,5.73410797232948,
44.4686431489673));
#150137=CARTESIAN_POINT('Ctrl Pts',(-4.18520413270094,5.62811013547991,
44.4770109887011));
#150138=CARTESIAN_POINT('Ctrl Pts',(-4.33173739947828,5.51612705289056,
44.4853788284348));
#150139=CARTESIAN_POINT('Ctrl Pts',(-4.4736725355593,5.39850725729645,44.4937466681686));
#150140=CARTESIAN_POINT('Ctrl Pts',(-4.61555222536714,5.28093340930558,
44.5021112390464));
#150141=CARTESIAN_POINT('Ctrl Pts',(-4.75283711370391,5.15772744875434,
44.5104758099241));
#150142=CARTESIAN_POINT('Ctrl Pts',(-4.88507731569834,5.02927889285825,
44.5188403808018));
#150143=CARTESIAN_POINT('Ctrl Pts',(-5.01728521550296,4.90086171297014,
44.5272029084737));
#150144=CARTESIAN_POINT('Ctrl Pts',(-5.14445065112782,4.76720472068888,
44.5355654361456));
#150145=CARTESIAN_POINT('Ctrl Pts',(-5.26615944653201,4.62873538303948,
44.5439279638174));
#150146=CARTESIAN_POINT('Ctrl Pts',(-5.38787795471531,4.49025499506224,
44.5522911588477));
#150147=CARTESIAN_POINT('Ctrl Pts',(-5.50413873117204,4.34696173733183,
44.5606543538779));
#150148=CARTESIAN_POINT('Ctrl Pts',(-5.61456636467825,4.19931793260807,
44.5690175489081));
#150149=CARTESIAN_POINT('Ctrl Pts',(-5.72500152916311,4.05166405882544,
44.5773813142942));
#150150=CARTESIAN_POINT('Ctrl Pts',(-5.82960256033757,3.89965930961281,
44.5857450796803));
#150151=CARTESIAN_POINT('Ctrl Pts',(-5.92803595478912,3.74379704060296,
44.5941088450663));
#150152=CARTESIAN_POINT('Ctrl Pts',(-6.02648918573965,3.58790336190987,
44.6024742959355));
#150153=CARTESIAN_POINT('Ctrl Pts',(-6.11877212601422,3.42815089131091,
44.6108397468047));
#150154=CARTESIAN_POINT('Ctrl Pts',(-6.20459579391003,3.26506012145167,
44.6192051976738));
#150155=CARTESIAN_POINT('Ctrl Pts',(-6.29044820404645,3.1019147326946,44.6275734501222));
#150156=CARTESIAN_POINT('Ctrl Pts',(-6.36983687526782,2.93542910621001,
44.6359417025705));
#150157=CARTESIAN_POINT('Ctrl Pts',(-6.44251959285939,2.76614675281753,
44.6443099550189));
#150158=CARTESIAN_POINT('Ctrl Pts',(-6.51526969783219,2.59670745022359,
44.6526859660464));
#150159=CARTESIAN_POINT('Ctrl Pts',(-6.58130129513043,2.42446654162041,
44.6610619770739));
#150160=CARTESIAN_POINT('Ctrl Pts',(-6.64042053958726,2.24998702661318,
44.6694379881014));
#150161=CARTESIAN_POINT('Ctrl Pts',(-6.6995687769112,2.07542194452135,44.6778181068366));
#150162=CARTESIAN_POINT('Ctrl Pts',(-6.75179780201015,1.89861638000929,
44.6861982255718));
#150163=CARTESIAN_POINT('Ctrl Pts',(-6.7969639861086,1.7201474163695,44.694578344307));
#150164=CARTESIAN_POINT('Ctrl Pts',(-6.84218177840511,1.54147452889142,
44.7029680384101));
#150165=CARTESIAN_POINT('Ctrl Pts',(-6.88032052940223,1.36113476478182,
44.7113577325132));
#150166=CARTESIAN_POINT('Ctrl Pts',(-6.9112876966623,1.17971561677563,44.7197474266162));
#150167=CARTESIAN_POINT('Ctrl Pts',(-6.93094825294038,1.06453551846891,
44.7250739084246));
#150168=CARTESIAN_POINT('Ctrl Pts',(-6.94771914402347,0.948920498281068,
44.7304003902331));
#150169=CARTESIAN_POINT('Ctrl Pts',(-6.96158755844055,0.833021745613987,
44.7357268720415));
#150170=CARTESIAN_POINT('Ctrl Pts',(-6.98340973414702,0.650653172769248,
44.744108177822));
#150171=CARTESIAN_POINT('Ctrl Pts',(-6.99808696749465,0.467214027019617,
44.7524894836025));
#150172=CARTESIAN_POINT('Ctrl Pts',(-7.00552451169838,0.283289390011714,
44.7608707893831));
#150173=CARTESIAN_POINT('Ctrl Pts',(-7.0129526298601,0.0995978516326951,
44.7692414730364));
#150174=CARTESIAN_POINT('Ctrl Pts',(-7.01315933114402,-0.0845776270624559,
44.7776121566898));
#150175=CARTESIAN_POINT('Ctrl Pts',(-7.00610137100075,-0.268645010676497,
44.7859828403431));
#150176=CARTESIAN_POINT('Ctrl Pts',(-6.99905142048172,-0.452503508076084,
44.7943440246469));
#150177=CARTESIAN_POINT('Ctrl Pts',(-6.98475325260364,-0.636253829470594,
44.8027052089507));
#150178=CARTESIAN_POINT('Ctrl Pts',(-6.96321559200029,-0.819301642756818,
44.8110663932545));
#150179=CARTESIAN_POINT('Ctrl Pts',(-6.94170587934826,-1.00211192739643,
44.8194167278204));
#150180=CARTESIAN_POINT('Ctrl Pts',(-6.91297544979655,-1.18422119833501,
44.8277670623864));
#150181=CARTESIAN_POINT('Ctrl Pts',(-6.87708497359292,-1.36503803188133,
44.8361173969523));
#150182=CARTESIAN_POINT('Ctrl Pts',(-6.84122211328002,-1.54571573609741,
44.8444613063617));
#150183=CARTESIAN_POINT('Ctrl Pts',(-6.79821024884859,-1.72510266469258,
44.8528052157711));
#150184=CARTESIAN_POINT('Ctrl Pts',(-6.74816164210157,-1.90261425795381,
44.8611491251805));
#150185=CARTESIAN_POINT('Ctrl Pts',(-6.69815323546132,-2.07998327012302,
44.8694863325842));
#150186=CARTESIAN_POINT('Ctrl Pts',(-6.64111944739184,-2.25547963663527,
44.8778235399879));
#150187=CARTESIAN_POINT('Ctrl Pts',(-6.57722326611108,-2.4285305578121,
44.8861607473916));
#150188=CARTESIAN_POINT('Ctrl Pts',(-6.55618924637733,-2.48549728756052,
44.8889052773703));
#150189=CARTESIAN_POINT('Ctrl Pts',(-6.5344119802445,-2.54219911730051,
44.8916498073491));
#150190=CARTESIAN_POINT('Ctrl Pts',(-6.51189847181606,-2.59861594993559,
44.8943943373278));
#150191=CARTESIAN_POINT('Ctrl Pts',(-6.44349898993794,-2.77001891601304,
44.9027326391586));
#150192=CARTESIAN_POINT('Ctrl Pts',(-6.36835622157593,-2.93864926190625,
44.9110709409894));
#150193=CARTESIAN_POINT('Ctrl Pts',(-6.28673133156438,-3.10397096107982,
44.9194092428202));
#150194=CARTESIAN_POINT('Ctrl Pts',(-6.20505508710549,-3.26939667269976,
44.9277527907086));
#150195=CARTESIAN_POINT('Ctrl Pts',(-6.11688873149893,-3.4315092917151,
44.9360963385971));
#150196=CARTESIAN_POINT('Ctrl Pts',(-6.02253902143441,-3.58979808593741,
44.9444398864856));
#150197=CARTESIAN_POINT('Ctrl Pts',(-5.92811753164527,-3.74820730369947,
44.9527897820095));
#150198=CARTESIAN_POINT('Ctrl Pts',(-5.82750347163371,-3.90278661282742,
44.9611396775335));
#150199=CARTESIAN_POINT('Ctrl Pts',(-5.72104670588304,-4.05305454584623,
44.9694895730575));
#150200=CARTESIAN_POINT('Ctrl Pts',(-5.61443026401084,-4.20354786802249,
44.9778519927167));
#150201=CARTESIAN_POINT('Ctrl Pts',(-5.50195379361739,-4.34971662400249,
44.9862144123759));
#150202=CARTESIAN_POINT('Ctrl Pts',(-5.3840081525361,-4.49111153011421,
44.9945768320351));
#150203=CARTESIAN_POINT('Ctrl Pts',(-5.26596165255812,-4.63262734730071,
45.0029464026532));
#150204=CARTESIAN_POINT('Ctrl Pts',(-5.14243686948065,-4.76936092689429,
45.0113159732712));
#150205=CARTESIAN_POINT('Ctrl Pts',(-5.01386163497974,-4.90089972023284,
45.0196855438892));
#150206=CARTESIAN_POINT('Ctrl Pts',(-4.88508808900859,-5.03264139596629,
45.0280680235395));
#150207=CARTESIAN_POINT('Ctrl Pts',(-4.75124876310388,-5.15917204978774,
45.0364505031899));
#150208=CARTESIAN_POINT('Ctrl Pts',(-4.61280572352955,-5.28011836225979,
45.0448329828402));
#150209=CARTESIAN_POINT('Ctrl Pts',(-4.56750398032389,-5.31969477437937,
45.0475759227649));
#150210=CARTESIAN_POINT('Ctrl Pts',(-4.52170953464011,-5.35867358369052,
45.0503188626896));
#150211=CARTESIAN_POINT('Ctrl Pts',(-4.47543924925462,-5.39704271696373,
45.0530618026143));
#150212=CARTESIAN_POINT('Ctrl Pts',(-4.33391186585346,-5.51440276759424,
45.0614516603196));
#150213=CARTESIAN_POINT('Ctrl Pts',(-4.18764471001657,-5.62629262909133,
45.069841518025));
#150214=CARTESIAN_POINT('Ctrl Pts',(-4.03708740208148,-5.7323251713816,
45.0782313757303));
#150215=CARTESIAN_POINT('Ctrl Pts',(-3.88666902607069,-5.83825986850352,
45.0866134914064));
#150216=CARTESIAN_POINT('Ctrl Pts',(-3.7319686574599,-5.938347832997,45.0949956070826));
#150217=CARTESIAN_POINT('Ctrl Pts',(-3.57346855336625,-6.03224245704718,
45.1033777227587));
#150218=CARTESIAN_POINT('Ctrl Pts',(-3.41509141161372,-6.12606423885628,
45.1117533356974));
#150219=CARTESIAN_POINT('Ctrl Pts',(-3.25292069317565,-6.21370209241489,
45.120128948636));
#150220=CARTESIAN_POINT('Ctrl Pts',(-3.08746754778098,-6.29485271502831,
45.1285045615747));
#150221=CARTESIAN_POINT('Ctrl Pts',(-2.92211847483946,-6.37595229271086,
45.13687490613));
#150222=CARTESIAN_POINT('Ctrl Pts',(-2.75349138613453,-6.45057263134097,
45.1452452506854));
#150223=CARTESIAN_POINT('Ctrl Pts',(-2.58212234248166,-6.51845616468785,
45.1536155952408));
#150224=CARTESIAN_POINT('Ctrl Pts',(-2.41083597181675,-6.5863069492114,
45.1619819017192));
#150225=CARTESIAN_POINT('Ctrl Pts',(-2.23681058913936,-6.64742728865912,
45.1703482081975));
#150226=CARTESIAN_POINT('Ctrl Pts',(-2.06060298057893,-6.70160741307108,
45.1787145146759));
#150227=CARTESIAN_POINT('Ctrl Pts',(-1.88444465281964,-6.75577238467574,
45.1870784813104));
#150228=CARTESIAN_POINT('Ctrl Pts',(-1.70610562957134,-6.80300091368879,
45.195442447945));
#150229=CARTESIAN_POINT('Ctrl Pts',(-1.52615916427333,-6.84313267208846,
45.2038064145795));
#150230=CARTESIAN_POINT('Ctrl Pts',(-1.3462403901275,-6.88325825479234,
45.2121690941209));
#150231=CARTESIAN_POINT('Ctrl Pts',(-1.16471498780618,-6.91628917277313,
45.2205317736622));
#150232=CARTESIAN_POINT('Ctrl Pts',(-0.982168157556564,-6.94211583544829,
45.2288944532035));
#150233=CARTESIAN_POINT('Ctrl Pts',(-0.799625086118805,-6.96794196632805,
45.2372569605494));
#150234=CARTESIAN_POINT('Ctrl Pts',(-0.616060954154885,-6.9865640920567,
45.2456194678953));
#150235=CARTESIAN_POINT('Ctrl Pts',(-0.432068301071265,-6.99792423120667,
45.2539819752411));
#150236=CARTESIAN_POINT('Ctrl Pts',(-0.248054911779567,-7.00928565065889,
45.2623454250523));
#150237=CARTESIAN_POINT('Ctrl Pts',(-0.0636132331261454,-7.01338343209129,
45.2707088748634));
#150238=CARTESIAN_POINT('Ctrl Pts',(0.120661524372453,-7.01021164866198,
45.2790723246746));
#150239=CARTESIAN_POINT('Ctrl Pts',(0.305044786671953,-7.00703799762078,
45.2874406990586));
#150240=CARTESIAN_POINT('Ctrl Pts',(0.48926060244824,-6.99658623301968,
45.2958090734425));
#150241=CARTESIAN_POINT('Ctrl Pts',(0.672715169568648,-6.97890255435138,
45.3041774478265));
#150242=CARTESIAN_POINT('Ctrl Pts',(0.856224703716667,-6.96121357726359,
45.3125483295597));
#150243=CARTESIAN_POINT('Ctrl Pts',(1.03897220771171,-6.93628840228828,
45.3209192112928));
#150244=CARTESIAN_POINT('Ctrl Pts',(1.22037071740043,-6.90422492931767,
45.329290093026));
#150245=CARTESIAN_POINT('Ctrl Pts',(1.40192292243896,-6.87213428960405,
45.3376680672408));
#150246=CARTESIAN_POINT('Ctrl Pts',(1.58212352634415,-6.83289332918547,
45.3460460414556));
#150247=CARTESIAN_POINT('Ctrl Pts',(1.76039630212137,-6.78665097245891,
45.3544240156704));
#150248=CARTESIAN_POINT('Ctrl Pts',(1.87368942905185,-6.75726375297266,
45.3597482548427));
#150249=CARTESIAN_POINT('Ctrl Pts',(1.98620423357189,-6.72504992663875,
45.3650724940149));
#150250=CARTESIAN_POINT('Ctrl Pts',(2.09779627068701,-6.6900580990894,45.3703967331871));
#150251=CARTESIAN_POINT('Ctrl Pts',(2.26259546139358,-6.63838214612219,
45.3782595729506));
#150252=CARTESIAN_POINT('Ctrl Pts',(2.42572392454344,-6.58053746583258,
45.3861224127141));
#150253=CARTESIAN_POINT('Ctrl Pts',(2.58666585737656,-6.51665453317747,
45.3939852524775));
#150254=CARTESIAN_POINT('Ctrl Pts',(2.74748412769345,-6.45282068607797,
45.4018420506921));
#150255=CARTESIAN_POINT('Ctrl Pts',(2.90611885664721,-6.38295795286989,
45.4096988489067));
#150256=CARTESIAN_POINT('Ctrl Pts',(3.06206853905006,-6.30724684982757,
45.4175556471213));
#150257=CARTESIAN_POINT('Ctrl Pts',(3.21793027323985,-6.231578444251,45.425408014475));
#150258=CARTESIAN_POINT('Ctrl Pts',(3.37110963112841,-6.15006839571762,
45.4332603818286));
#150259=CARTESIAN_POINT('Ctrl Pts',(3.52112451134335,-6.06294554965794,
45.4411127491822));
#150260=CARTESIAN_POINT('Ctrl Pts',(3.67110397093754,-5.97584327452619,
45.4489632624816));
#150261=CARTESIAN_POINT('Ctrl Pts',(3.81792010630897,-5.88313102351259,
45.4568137757809));
#150262=CARTESIAN_POINT('Ctrl Pts',(3.96111494994963,-5.78508382962473,
45.4646642890803));
#150263=CARTESIAN_POINT('Ctrl Pts',(4.10428675798224,-5.68705240848869,
45.4725135394756));
#150264=CARTESIAN_POINT('Ctrl Pts',(4.24383812087141,-5.583687970988,45.480362789871));
#150265=CARTESIAN_POINT('Ctrl Pts',(4.3793400275334,-5.4753088940939,45.4882120402663));
#150266=CARTESIAN_POINT('Ctrl Pts',(4.51488758676616,-5.36689330270639,
45.4960639351887));
#150267=CARTESIAN_POINT('Ctrl Pts',(4.64638266641554,-5.25345993575891,
45.503915830111));
#150268=CARTESIAN_POINT('Ctrl Pts',(4.77342918296909,-5.13536760102713,
45.5117677250334));
#150269=CARTESIAN_POINT('Ctrl Pts',(4.86671692734786,-5.04865473526423,
45.5175332161801));
#150270=CARTESIAN_POINT('Ctrl Pts',(4.9576068291167,-4.95943075883898,45.5232987073268));
#150271=CARTESIAN_POINT('Ctrl Pts',(5.04595485518052,-4.86785026084207,
45.5290641984735));
#150272=CARTESIAN_POINT('Ctrl Pts',(5.19390725399777,-4.71448458910952,
45.5387194028229));
#150273=CARTESIAN_POINT('Ctrl Pts',(5.33465509669178,-4.55458791352578,
45.5483746071723));
#150274=CARTESIAN_POINT('Ctrl Pts',(5.46772197842277,-4.38880882805035,
45.5580298115217));
#150275=CARTESIAN_POINT('Ctrl Pts',(5.60152591377924,-4.22211149699502,
45.5677384957699));
#150276=CARTESIAN_POINT('Ctrl Pts',(5.72756357639558,-4.04946648164349,
45.5774471800181));
#150277=CARTESIAN_POINT('Ctrl Pts',(5.84539772643407,-3.87155679053007,
45.5871558642664));
#150278=CARTESIAN_POINT('Ctrl Pts',(5.96379884216781,-3.69279107684864,
45.5969112623994));
#150279=CARTESIAN_POINT('Ctrl Pts',(6.07391730816847,-3.50870995229964,
45.6066666605325));
#150280=CARTESIAN_POINT('Ctrl Pts',(6.17535690736826,-3.32002916088386,
45.6164220586655));
#150281=CARTESIAN_POINT('Ctrl Pts',(6.27689695335583,-3.13116153533657,
45.6261871167185));
#150282=CARTESIAN_POINT('Ctrl Pts',(6.36974093440355,-2.93768517167746,
45.6359521747715));
#150283=CARTESIAN_POINT('Ctrl Pts',(6.45353879309377,-2.74034005344844,
45.6457172328245));
#150284=CARTESIAN_POINT('Ctrl Pts',(6.53722245020253,-2.54326388152601,
45.6554689828396));
#150285=CARTESIAN_POINT('Ctrl Pts',(6.61188460991109,-2.34232952769541,
45.6652207328548));
#150286=CARTESIAN_POINT('Ctrl Pts',(6.67722392304667,-2.13829540615726,
45.67497248287));
#150287=CARTESIAN_POINT('Ctrl Pts',(6.70572055576135,-2.04930938619912,
45.6792255431666));
#150288=CARTESIAN_POINT('Ctrl Pts',(6.73244447982265,-1.95973402571245,
45.6834786034633));
#150289=CARTESIAN_POINT('Ctrl Pts',(6.75737353878295,-1.86963349880557,
45.6877316637599));
#150290=CARTESIAN_POINT('Ctrl Pts',(6.80473961416133,-1.69843937728265,
45.6958126256174));
#150291=CARTESIAN_POINT('Ctrl Pts',(6.84564464248862,-1.52526782050514,
45.7038935874748));
#150292=CARTESIAN_POINT('Ctrl Pts',(6.87992489828093,-1.3506516784553,45.7119745493323));
#150293=CARTESIAN_POINT('Ctrl Pts',(6.91418286331631,-1.1761490806568,45.7200502565394));
#150294=CARTESIAN_POINT('Ctrl Pts',(6.94182456104688,-1.0002041206424,45.7281259637466));
#150295=CARTESIAN_POINT('Ctrl Pts',(6.9627364815039,-0.823363377637502,
45.7362016709537));
#150296=CARTESIAN_POINT('Ctrl Pts',(6.98363769465593,-0.646613180490235,
45.7442732432436));
#150297=CARTESIAN_POINT('Ctrl Pts',(6.99781595120447,-0.46896847219117,
45.7523448155335));
#150298=CARTESIAN_POINT('Ctrl Pts',(7.0052091033809,-0.290984502008834,
45.7604163878234));
#150299=CARTESIAN_POINT('Ctrl Pts',(7.00921423555851,-0.19456428650892,
45.7647890441858));
#150300=CARTESIAN_POINT('Ctrl Pts',(7.01122898586229,-0.0980446382295471,
45.7691617005482));
#150301=CARTESIAN_POINT('Ctrl Pts',(7.01124983644072,-0.00151443390808588,
45.7735343569105));
#150302=CARTESIAN_POINT('Ctrl Pts',(7.01125,3.72163509519775E-12,45.7735343569105));
#150303=CARTESIAN_POINT('Ctrl Pts',(7.0112499999999,0.191008754744202,45.7822061308426));
#150304=CARTESIAN_POINT('Ctrl Pts',(7.00344012880995,0.382017367487347,
45.7908779047747));
#150305=CARTESIAN_POINT('Ctrl Pts',(6.98784644419141,0.572388534914368,
45.7995496787069));
#150306=CARTESIAN_POINT('Ctrl Pts',(6.97225169663157,0.762772678965089,
45.8082220437492));
#150307=CARTESIAN_POINT('Ctrl Pts',(6.94887209704267,0.952519007631466,
45.8168944087916));
#150308=CARTESIAN_POINT('Ctrl Pts',(6.91778566246033,1.14099434300015,45.8255667738339));
#150309=CARTESIAN_POINT('Ctrl Pts',(6.88670108297123,1.32945843104102,45.83423862135));
#150310=CARTESIAN_POINT('Ctrl Pts',(6.84791063501084,1.51665139731204,45.8429104688662));
#150311=CARTESIAN_POINT('Ctrl Pts',(6.80154374572903,1.70194865887145,45.8515823163823));
#150312=CARTESIAN_POINT('Ctrl Pts',(6.75517597619824,1.88724943819381,45.8602543285285));
#150313=CARTESIAN_POINT('Ctrl Pts',(6.70123154646052,2.07065416525576,45.8689263406747));
#150314=CARTESIAN_POINT('Ctrl Pts',(6.63989045285493,2.25155087363932,45.8775983528209));
#150315=CARTESIAN_POINT('Ctrl Pts',(6.61790934153613,2.31637382429861,45.880705901988));
#150316=CARTESIAN_POINT('Ctrl Pts',(6.59497889661499,2.38087486019109,45.8838134511551));
#150317=CARTESIAN_POINT('Ctrl Pts',(6.57110895151812,2.4450263208764,45.8869210003222));
#150318=CARTESIAN_POINT('',(7.01124961585759,0.00232091291924789,45.2264650997577));
#150319=CARTESIAN_POINT('Ctrl Pts',(6.57110895151812,2.4450263208764,45.3397873838214));
#150320=CARTESIAN_POINT('Ctrl Pts',(6.63862499196149,2.26357418110171,45.3309680909161));
#150321=CARTESIAN_POINT('Ctrl Pts',(6.69866370151301,2.07920961773414,45.3221487980108));
#150322=CARTESIAN_POINT('Ctrl Pts',(6.75099215188743,1.89254630792865,45.3133295051056));
#150323=CARTESIAN_POINT('Ctrl Pts',(6.80321535316924,1.70625843717859,45.3045279505925));
#150324=CARTESIAN_POINT('Ctrl Pts',(6.84775917915664,1.51768129892919,45.2957263960794));
#150325=CARTESIAN_POINT('Ctrl Pts',(6.88444035403814,1.32744400039749,45.2869248415663));
#150326=CARTESIAN_POINT('Ctrl Pts',(6.92107263670544,1.13746026851895,45.2781350186155));
#150327=CARTESIAN_POINT('Ctrl Pts',(6.94986312529546,0.945821045319097,
45.2693451956647));
#150328=CARTESIAN_POINT('Ctrl Pts',(6.97067887401658,0.753168372835053,
45.260555372714));
#150329=CARTESIAN_POINT('Ctrl Pts',(6.99145429853821,0.560888906470144,
45.2517825773791));
#150330=CARTESIAN_POINT('Ctrl Pts',(7.00428578375525,0.367600166895988,
45.2430097820442));
#150331=CARTESIAN_POINT('Ctrl Pts',(7.00909175428748,0.173952126975464,
45.2342369867093));
#150332=CARTESIAN_POINT('Ctrl Pts',(7.0105108705063,0.116771361435778,45.2316465388361));
#150333=CARTESIAN_POINT('Ctrl Pts',(7.01123057041653,0.0595593314933894,
45.2290560909628));
#150334=CARTESIAN_POINT('Ctrl Pts',(7.01124961187403,0.00233291583925055,
45.2264656430896));
#150335=CARTESIAN_POINT('Ctrl Pts',(7.01124961585759,0.00232091291924789,
45.2264650997577));
#150336=CARTESIAN_POINT('Ctrl Pts',(7.01131373062021,-0.191363477836033,
45.2176976568821));
#150337=CARTESIAN_POINT('Ctrl Pts',(7.00334774553214,-0.384934212827022,
45.2089302140066));
#150338=CARTESIAN_POINT('Ctrl Pts',(6.98740619787143,-0.577737992906812,
45.200162771131));
#150339=CARTESIAN_POINT('Ctrl Pts',(6.97144758934037,-0.770748114325792,
45.1913859452138));
#150340=CARTESIAN_POINT('Ctrl Pts',(6.94749639030405,-0.962989378600591,
45.1826091192966));
#150341=CARTESIAN_POINT('Ctrl Pts',(6.9156588509455,-1.15381507176808,45.1738322933794));
#150342=CARTESIAN_POINT('Ctrl Pts',(6.88378958982525,-1.34483089668847,
45.1650467225533));
#150343=CARTESIAN_POINT('Ctrl Pts',(6.84401833625513,-1.53442807346663,
45.1562611517272));
#150344=CARTESIAN_POINT('Ctrl Pts',(6.79650234356762,-1.72197051553732,
45.1474755809011));
#150345=CARTESIAN_POINT('Ctrl Pts',(6.74891995344015,-1.90977502385842,
45.1386777333787));
#150346=CARTESIAN_POINT('Ctrl Pts',(6.69357125003739,-2.0955188007609,45.1298798858563));
#150347=CARTESIAN_POINT('Ctrl Pts',(6.63066377754691,-2.27857947669757,
45.1210820383339));
#150348=CARTESIAN_POINT('Ctrl Pts',(6.56771463172738,-2.46176142197604,
45.1122783626391));
#150349=CARTESIAN_POINT('Ctrl Pts',(6.49719680749287,-2.64225646939765,
45.1034746869443));
#150350=CARTESIAN_POINT('Ctrl Pts',(6.41936645607332,-2.81946109480885,
45.0946710112495));
#150351=CARTESIAN_POINT('Ctrl Pts',(6.34146504499815,-2.99682750928338,
45.0858592977372));
#150352=CARTESIAN_POINT('Ctrl Pts',(6.25623787113032,-3.17089725727878,
45.0770475842249));
#150353=CARTESIAN_POINT('Ctrl Pts',(6.16398831554795,-3.34108883573729,
45.0682358707126));
#150354=CARTESIAN_POINT('Ctrl Pts',(6.14069231428679,-3.38406772275066,
45.0660106275903));
#150355=CARTESIAN_POINT('Ctrl Pts',(6.11694870338084,-3.42679941624926,
45.0637853844679));
#150356=CARTESIAN_POINT('Ctrl Pts',(6.0927628222351,-3.46927481680103,45.0615601413456));
#150357=CARTESIAN_POINT('Ctrl Pts',(6.0073027253985,-3.61936039038229,45.0536973104828));
#150358=CARTESIAN_POINT('Ctrl Pts',(5.91616874435837,-3.7665046418464,45.04583447962));
#150359=CARTESIAN_POINT('Ctrl Pts',(5.81959780561077,-3.91023118797729,
45.0379716487571));
#150360=CARTESIAN_POINT('Ctrl Pts',(5.72310106890137,-4.05384729920091,
45.0301148594434));
#150361=CARTESIAN_POINT('Ctrl Pts',(5.62117589347774,-4.19405061295756,
45.0222580701298));
#150362=CARTESIAN_POINT('Ctrl Pts',(5.51410507512597,-4.33038933387866,
45.0144012808161));
#150363=CARTESIAN_POINT('Ctrl Pts',(5.40709463966623,-4.46665116619097,
45.0065489223611));
#150364=CARTESIAN_POINT('Ctrl Pts',(5.29494456857491,-4.59905244216715,
44.9986965639061));
#150365=CARTESIAN_POINT('Ctrl Pts',(5.1779807704992,-4.72717058110245,44.990844205451));
#150366=CARTESIAN_POINT('Ctrl Pts',(5.06104458896047,-4.8552584698289,44.9829937010308));
#150367=CARTESIAN_POINT('Ctrl Pts',(4.93929719314165,-4.97906494726934,
44.9751431966105));
#150368=CARTESIAN_POINT('Ctrl Pts',(4.81310450828359,-5.09820081546816,
44.9672926921903));
#150369=CARTESIAN_POINT('Ctrl Pts',(4.68693212386762,-5.2173175184452,44.9594434506698));
#150370=CARTESIAN_POINT('Ctrl Pts',(4.55631615347341,-5.33176484818011,
44.9515942091492));
#150371=CARTESIAN_POINT('Ctrl Pts',(4.42165873698109,-5.44119109903143,
44.9437449676287));
#150372=CARTESIAN_POINT('Ctrl Pts',(4.28695595177435,-5.55065421772452,
44.9358930815454));
#150373=CARTESIAN_POINT('Ctrl Pts',(4.1482092970229,-5.6550926376447,44.9280411954621));
#150374=CARTESIAN_POINT('Ctrl Pts',(4.00585343795195,-5.75419540823464,
44.9201893093787));
#150375=CARTESIAN_POINT('Ctrl Pts',(3.90132326226839,-5.82696536718189,
44.914423764939));
#150376=CARTESIAN_POINT('Ctrl Pts',(3.7948477706504,-5.89685930138269,44.9086582204992));
#150377=CARTESIAN_POINT('Ctrl Pts',(3.6866085941152,-5.9637692474052,44.9028926760594));
#150378=CARTESIAN_POINT('Ctrl Pts',(3.50534516918806,-6.07582041377551,
44.8932373704189));
#150379=CARTESIAN_POINT('Ctrl Pts',(3.31922767169188,-6.17944533608273,
44.8835820647784));
#150380=CARTESIAN_POINT('Ctrl Pts',(3.12899101640001,-6.27431604095523,
44.8739267591378));
#150381=CARTESIAN_POINT('Ctrl Pts',(2.93770048295348,-6.36971231311773,
44.8642179647747));
#150382=CARTESIAN_POINT('Ctrl Pts',(2.74224509309065,-6.45625713339368,
44.8545091704115));
#150383=CARTESIAN_POINT('Ctrl Pts',(2.54338508578354,-6.53366810206287,
44.8448003760484));
#150384=CARTESIAN_POINT('Ctrl Pts',(2.34356814478508,-6.61145157984037,
44.8350448620227));
#150385=CARTESIAN_POINT('Ctrl Pts',(2.14031378982544,-6.68001309520664,
44.825289347997));
#150386=CARTESIAN_POINT('Ctrl Pts',(1.93440554885227,-6.73911728159331,
44.8155338339714));
#150387=CARTESIAN_POINT('Ctrl Pts',(1.72829342657662,-6.79827999035113,
44.8057686604639));
#150388=CARTESIAN_POINT('Ctrl Pts',(1.51952220209997,-6.84796663969157,
44.7960034869565));
#150389=CARTESIAN_POINT('Ctrl Pts',(1.30888929894411,-6.88799211422383,
44.786238313449));
#150390=CARTESIAN_POINT('Ctrl Pts',(1.09854358991336,-6.92796301475094,
44.7764864545777));
#150391=CARTESIAN_POINT('Ctrl Pts',(0.886341312769191,-6.9582990611913,
44.7667345957063));
#150392=CARTESIAN_POINT('Ctrl Pts',(0.673087568189201,-6.97886664781963,
44.756982736835));
#150393=CARTESIAN_POINT('Ctrl Pts',(0.580093666882398,-6.98783558820002,
44.7527302281476));
#150394=CARTESIAN_POINT('Ctrl Pts',(0.486899957340695,-6.99494762616512,
44.7484777194602));
#150395=CARTESIAN_POINT('Ctrl Pts',(0.393573826530796,-7.00019472626083,
44.7442252107729));
#150396=CARTESIAN_POINT('Ctrl Pts',(0.217279532242484,-7.01010656767551,
44.7361921656708));
#150397=CARTESIAN_POINT('Ctrl Pts',(0.0404264676274792,-7.01336469367874,
44.7281591205688));
#150398=CARTESIAN_POINT('Ctrl Pts',(-0.136435664693323,-7.0099223870097,
44.7201260754668));
#150399=CARTESIAN_POINT('Ctrl Pts',(-0.313184103180249,-7.00648229318881,
44.7120981943175));
#150400=CARTESIAN_POINT('Ctrl Pts',(-0.489941232798838,-6.99635034758006,
44.7040703131682));
#150401=CARTESIAN_POINT('Ctrl Pts',(-0.666154661791966,-6.97953182735582,
44.6960424320189));
#150402=CARTESIAN_POINT('Ctrl Pts',(-0.842288528648519,-6.96272090086272,
44.6880181755388));
#150403=CARTESIAN_POINT('Ctrl Pts',(-1.01787881951728,-6.93922944579692,
44.6799939190586));
#150404=CARTESIAN_POINT('Ctrl Pts',(-1.19237562897843,-6.90911477122202,
44.6719696625785));
#150405=CARTESIAN_POINT('Ctrl Pts',(-1.36685133997652,-6.87900373782171,
44.6639463763136));
#150406=CARTESIAN_POINT('Ctrl Pts',(-1.54023347058308,-6.84227113470735,
44.6559230900488));
#150407=CARTESIAN_POINT('Ctrl Pts',(-1.71197952886332,-6.79902586075777,
44.647899803784));
#150408=CARTESIAN_POINT('Ctrl Pts',(-1.88371151406891,-6.75578413037696,
44.6398771749567));
#150409=CARTESIAN_POINT('Ctrl Pts',(-2.05380733942037,-6.70603088557465,
44.6318545461294));
#150410=CARTESIAN_POINT('Ctrl Pts',(-2.22173725671783,-6.6499255728626,
44.6238319173021));
#150411=CARTESIAN_POINT('Ctrl Pts',(-2.38973030372378,-6.59379916854226,
44.6158062725369));
#150412=CARTESIAN_POINT('Ctrl Pts',(-2.55555546915972,-6.53131604511736,
44.6077806277716));
#150413=CARTESIAN_POINT('Ctrl Pts',(-2.71870028816019,-6.46268483725284,
44.5997549830063));
#150414=CARTESIAN_POINT('Ctrl Pts',(-2.81490048196455,-6.42221566674503,
44.5950225704997));
#150415=CARTESIAN_POINT('Ctrl Pts',(-2.91016908229907,-6.37960972293838,
44.5902901579931));
#150416=CARTESIAN_POINT('Ctrl Pts',(-3.00440465758325,-6.33491745928801,
44.5855577454865));
#150417=CARTESIAN_POINT('Ctrl Pts',(-3.1782443670222,-6.25247205473968,
44.5768276962178));
#150418=CARTESIAN_POINT('Ctrl Pts',(-3.3486543913784,-6.16288330584912,
44.5680976469492));
#150419=CARTESIAN_POINT('Ctrl Pts',(-3.51506610075752,-6.06645999490686,
44.5593675976805));
#150420=CARTESIAN_POINT('Ctrl Pts',(-3.68152592846285,-5.97000880294381,
44.5506350240981));
#150421=CARTESIAN_POINT('Ctrl Pts',(-3.84398489648174,-5.8667192416086,
44.5419024505158));
#150422=CARTESIAN_POINT('Ctrl Pts',(-4.00190118553436,-5.75694480290706,
44.5331698769334));
#150423=CARTESIAN_POINT('Ctrl Pts',(-4.16206091546047,-5.64561085147809,
44.5243132438723));
#150424=CARTESIAN_POINT('Ctrl Pts',(-4.31754767340672,-5.52760652875741,
44.5154566108112));
#150425=CARTESIAN_POINT('Ctrl Pts',(-4.46782846641096,-5.40334483049415,
44.5065999777501));
#150426=CARTESIAN_POINT('Ctrl Pts',(-4.61609852361058,-5.28074573621938,
44.4978618451896));
#150427=CARTESIAN_POINT('Ctrl Pts',(-4.75930086157089,-5.15205586697208,
44.4891237126291));
#150428=CARTESIAN_POINT('Ctrl Pts',(-4.89695780246188,-5.01771171385999,
44.4803855800686));
#150429=CARTESIAN_POINT('Ctrl Pts',(-5.03741495546275,-4.8806347372375,
44.4714696967572));
#150430=CARTESIAN_POINT('Ctrl Pts',(-5.17209847168035,-4.73767117845135,
44.4625538134458));
#150431=CARTESIAN_POINT('Ctrl Pts',(-5.30054060723454,-4.589324115113,44.4536379301343));
#150432=CARTESIAN_POINT('Ctrl Pts',(-5.42898274278872,-4.44097705177465,
44.4447220468229));
#150433=CARTESIAN_POINT('Ctrl Pts',(-5.55118330432975,-4.28724671649079,
44.4358061635115));
#150434=CARTESIAN_POINT('Ctrl Pts',(-5.66671764407193,-4.12867263231949,
44.4268902802001));
#150435=CARTESIAN_POINT('Ctrl Pts',(-5.7799817093088,-3.9732145628439,44.4181495959041));
#150436=CARTESIAN_POINT('Ctrl Pts',(-5.88685113604801,-3.81308482769952,
44.4094089116081));
#150437=CARTESIAN_POINT('Ctrl Pts',(-5.98696423681725,-3.64881978036341,
44.4006682273121));
#150438=CARTESIAN_POINT('Ctrl Pts',(-6.08705932554435,-3.48458428709097,
44.3919291156133));
#150439=CARTESIAN_POINT('Ctrl Pts',(-6.18040037346429,-3.31621520118869,
44.3831900039144));
#150440=CARTESIAN_POINT('Ctrl Pts',(-6.26667006107284,-3.14427621371808,
44.3744508922155));
#150441=CARTESIAN_POINT('Ctrl Pts',(-6.35405749967336,-2.97010950317195,
44.3655985524404));
#150442=CARTESIAN_POINT('Ctrl Pts',(-6.43418891288873,-2.79227998418195,
44.3567462126652));
#150443=CARTESIAN_POINT('Ctrl Pts',(-6.50678286800209,-2.61139871930246,
44.3478938728901));
#150444=CARTESIAN_POINT('Ctrl Pts',(-6.57841155959771,-2.43292258699575,
44.3391592404449));
#150445=CARTESIAN_POINT('Ctrl Pts',(-6.64270190388603,-2.25147562730464,
44.3304246079998));
#150446=CARTESIAN_POINT('Ctrl Pts',(-6.69943182549076,-2.06766529643982,
44.3216899755546));
#150447=CARTESIAN_POINT('Ctrl Pts',(-6.75730848011134,-1.88013944175451,
44.3127787821145));
#150448=CARTESIAN_POINT('Ctrl Pts',(-6.80731569909913,-1.69015392345087,
44.3038675886743));
#150449=CARTESIAN_POINT('Ctrl Pts',(-6.84927073622432,-1.49837143072108,
44.2949563952341));
#150450=CARTESIAN_POINT('Ctrl Pts',(-6.8912257733495,-1.30658893799135,
44.286045201794));
#150451=CARTESIAN_POINT('Ctrl Pts',(-6.9251285506676,-1.11300976408271,
44.2771340083538));
#150452=CARTESIAN_POINT('Ctrl Pts',(-6.95085125138724,-0.918310102083431,
44.2682228149136));
#150453=CARTESIAN_POINT('Ctrl Pts',(-6.97401782021059,-0.742958253583889,
44.2601971500202));
#150454=CARTESIAN_POINT('Ctrl Pts',(-6.99055941706707,-0.566616890051982,
44.2521714851268));
#150455=CARTESIAN_POINT('Ctrl Pts',(-7.00040398867454,-0.389834013202616,
44.2441458202334));
#150456=CARTESIAN_POINT('Ctrl Pts',(-7.01024543585677,-0.213107242896276,
44.2361227024889));
#150457=CARTESIAN_POINT('Ctrl Pts',(-7.01339406904623,-0.0359396038173357,
44.2280995847444));
#150458=CARTESIAN_POINT('Ctrl Pts',(-7.00982972561212,0.14111619476412,
44.2200764669999));
#150459=CARTESIAN_POINT('Ctrl Pts',(-7.00626583167286,0.318149665062288,
44.2120543610406));
#150460=CARTESIAN_POINT('Ctrl Pts',(-6.99599065533762,0.495070956576405,
44.2040322550814));
#150461=CARTESIAN_POINT('Ctrl Pts',(-6.9790361450392,0.671327825087306,
44.1960101491221));
#150462=CARTESIAN_POINT('Ctrl Pts',(-6.96207533438705,0.847650191250387,
44.187985062121));
#150463=CARTESIAN_POINT('Ctrl Pts',(-6.93843026353939,1.02330727566344,
44.1799599751198));
#150464=CARTESIAN_POINT('Ctrl Pts',(-6.90818476814346,1.19775196584715,
44.1719348881187));
#150465=CARTESIAN_POINT('Ctrl Pts',(-6.87793331604822,1.37223101204163,
44.1639082206168));
#150466=CARTESIAN_POINT('Ctrl Pts',(-6.8410789210492,1.5454968286583,44.1558815531148));
#150467=CARTESIAN_POINT('Ctrl Pts',(-6.79775642319675,1.71701315469256,
44.1478548856129));
#150468=CARTESIAN_POINT('Ctrl Pts',(-6.75439914619576,1.88866717342872,
44.1398217743306));
#150469=CARTESIAN_POINT('Ctrl Pts',(-6.7045634942428,2.05856854341172,44.1317886630483));
#150470=CARTESIAN_POINT('Ctrl Pts',(-6.64843417739367,2.22619620684338,
44.123755551766));
#150471=CARTESIAN_POINT('Ctrl Pts',(-6.61536074680689,2.32496850984203,
44.119022151053));
#150472=CARTESIAN_POINT('Ctrl Pts',(-6.5801030882891,2.42295172150919,44.11428875034));
#150473=CARTESIAN_POINT('Ctrl Pts',(-6.54270674875877,2.52004265087844,
44.1095553496271));
#150474=CARTESIAN_POINT('Ctrl Pts',(-6.46566912147763,2.72005299742754,
44.0998043963392));
#150475=CARTESIAN_POINT('Ctrl Pts',(-6.379508204051,2.91639371319058,44.0900534430514));
#150476=CARTESIAN_POINT('Ctrl Pts',(-6.28457804557364,3.10832838541777,
44.0803024897635));
#150477=CARTESIAN_POINT('Ctrl Pts',(-6.18951112239274,3.30053957555,44.070537488398));
#150478=CARTESIAN_POINT('Ctrl Pts',(-6.08564970409685,3.48833199018424,
44.0607724870325));
#150479=CARTESIAN_POINT('Ctrl Pts',(-5.97339474361976,3.67099193671082,
44.051007485667));
#150480=CARTESIAN_POINT('Ctrl Pts',(-5.86132688889493,3.85334742696608,
44.0412587605348));
#150481=CARTESIAN_POINT('Ctrl Pts',(-5.74089347275576,4.03058751430809,
44.0315100354026));
#150482=CARTESIAN_POINT('Ctrl Pts',(-5.61253818956788,4.20202827609978,
44.0217613102704));
#150483=CARTESIAN_POINT('Ctrl Pts',(-5.48453519185473,4.37299849948701,
44.0120393416081));
#150484=CARTESIAN_POINT('Ctrl Pts',(-5.34865375627933,4.53820114084512,
44.0023173729457));
#150485=CARTESIAN_POINT('Ctrl Pts',(-5.20537825628705,4.69698454026346,
43.9925954042833));
#150486=CARTESIAN_POINT('Ctrl Pts',(-5.06305077284174,4.85471731141641,
43.9829377633473));
#150487=CARTESIAN_POINT('Ctrl Pts',(-4.91342676057244,5.00611545474773,
43.9732801224114));
#150488=CARTESIAN_POINT('Ctrl Pts',(-4.75702469715459,5.15056721081875,
43.9636224814754));
#150489=CARTESIAN_POINT('Ctrl Pts',(-4.68828060523655,5.2140587311994,43.9593776157638));
#150490=CARTESIAN_POINT('Ctrl Pts',(-4.61822762680022,5.27620863318986,
43.9551327500523));
#150491=CARTESIAN_POINT('Ctrl Pts',(-4.54691248151948,5.33696668978759,
43.9508878843408));
#150492=CARTESIAN_POINT('Ctrl Pts',(-4.41499885970426,5.44935256895409,
43.9430360373324));
#150493=CARTESIAN_POINT('Ctrl Pts',(-4.27881845835598,5.55692720483943,
43.935184190324));
#150494=CARTESIAN_POINT('Ctrl Pts',(-4.13877606194018,5.65934265366668,
43.9273323433156));
#150495=CARTESIAN_POINT('Ctrl Pts',(-3.9987733804172,5.76172905829961,43.9194827230276));
#150496=CARTESIAN_POINT('Ctrl Pts',(-3.8549111900341,5.85895896128015,43.9116331027396));
#150497=CARTESIAN_POINT('Ctrl Pts',(-3.70762655175944,5.95072532681424,
43.9037834824516));
#150498=CARTESIAN_POINT('Ctrl Pts',(-3.56035367227979,6.04248436597748,
43.8959344888554));
#150499=CARTESIAN_POINT('Ctrl Pts',(-3.40965921301176,6.12878053494963,
43.8880854952592));
#150500=CARTESIAN_POINT('Ctrl Pts',(-3.25600811563665,6.20935082866223,
43.880236501663));
#150501=CARTESIAN_POINT('Ctrl Pts',(-3.10227922921283,6.28996191275386,
43.8723835343513));
#150502=CARTESIAN_POINT('Ctrl Pts',(-2.94559105215743,6.36484115217058,
43.8645305670397));
#150503=CARTESIAN_POINT('Ctrl Pts',(-2.78643226795437,6.43377197129356,
43.856677599728));
#150504=CARTESIAN_POINT('Ctrl Pts',(-2.62723306276852,6.50272029652825,
43.8488226380265));
#150505=CARTESIAN_POINT('Ctrl Pts',(-2.46556235588125,6.56571705328878,
43.840967676325));
#150506=CARTESIAN_POINT('Ctrl Pts',(-2.301926966983,6.62259456717505,43.8331127146235));
#150507=CARTESIAN_POINT('Ctrl Pts',(-2.1381291562848,6.67952853674761,43.8252499562161));
#150508=CARTESIAN_POINT('Ctrl Pts',(-1.97236313326889,6.73033102067285,
43.8173871978086));
#150509=CARTESIAN_POINT('Ctrl Pts',(-1.80514952533018,6.77488463028709,
43.8095244394011));
#150510=CARTESIAN_POINT('Ctrl Pts',(-1.68248402110205,6.80756851921147,
43.8037564326188));
#150511=CARTESIAN_POINT('Ctrl Pts',(-1.55903978214239,6.83689064534657,
43.7979884258366));
#150512=CARTESIAN_POINT('Ctrl Pts',(-1.43502476922851,6.86282234027668,
43.7922204190543));
#150513=CARTESIAN_POINT('Ctrl Pts',(-1.25489217619602,6.90048829167832,
43.7838423526097));
#150514=CARTESIAN_POINT('Ctrl Pts',(-1.07315613190083,6.93108293751319,
43.7754642861651));
#150515=CARTESIAN_POINT('Ctrl Pts',(-0.890397560720694,6.95448191789745,
43.7670862197205));
#150516=CARTESIAN_POINT('Ctrl Pts',(-0.707763957678036,6.97786489833721,
43.7587138820982));
#150517=CARTESIAN_POINT('Ctrl Pts',(-0.524109546755221,6.99406198135615,
43.7503415444758));
#150518=CARTESIAN_POINT('Ctrl Pts',(-0.340024337999865,7.00300007225959,
43.7419692068534));
#150519=CARTESIAN_POINT('Ctrl Pts',(-0.156038008303853,7.01193336217968,
43.7336013663271));
#150520=CARTESIAN_POINT('Ctrl Pts',(0.0283783302363337,7.01361541846707,
43.7252335258007));
#150521=CARTESIAN_POINT('Ctrl Pts',(0.212630203911086,7.00802503983003,
43.7168656852744));
#150522=CARTESIAN_POINT('Ctrl Pts',(0.396810100565737,7.00243684504485,
43.7085011136007));
#150523=CARTESIAN_POINT('Ctrl Pts',(0.580825332396124,6.98958189052553,
43.7001365419271));
#150524=CARTESIAN_POINT('Ctrl Pts',(0.76408162212722,6.96949107447792,43.6917719702534));
#150525=CARTESIAN_POINT('Ctrl Pts',(0.947293148055745,6.94940516599079,
43.683409441784));
#150526=CARTESIAN_POINT('Ctrl Pts',(1.12974577519655,6.92208695700521,43.6750469133146));
#150527=CARTESIAN_POINT('Ctrl Pts',(1.31085008228257,6.8876192275909,43.6666843848452));
#150528=CARTESIAN_POINT('Ctrl Pts',(1.49196884206102,6.85314874754353,43.6583211890198));
#150529=CARTESIAN_POINT('Ctrl Pts',(1.67173874281103,6.81152766269534,43.6499579931944));
#150530=CARTESIAN_POINT('Ctrl Pts',(1.84957953144805,6.76289007151147,43.6415947973689));
#150531=CARTESIAN_POINT('Ctrl Pts',(2.02743244847089,6.71424916334124,43.6332310311903));
#150532=CARTESIAN_POINT('Ctrl Pts',(2.20335567381335,6.6585908812086,43.6248672650117));
#150533=CARTESIAN_POINT('Ctrl Pts',(2.37678295118015,6.59609955697148,43.616503498833));
#150534=CARTESIAN_POINT('Ctrl Pts',(2.5502451778748,6.53359563938797,43.6081380471755));
#150535=CARTESIAN_POINT('Ctrl Pts',(2.72121014431174,6.46425604538771,43.599772595518));
#150536=CARTESIAN_POINT('Ctrl Pts',(2.88913004700044,6.3883138725347,43.5914071438606));
#150537=CARTESIAN_POINT('Ctrl Pts',(3.05710618573493,6.31234626679707,43.5830388906297));
#150538=CARTESIAN_POINT('Ctrl Pts',(3.22203492778689,6.22977180845838,43.5746706373989));
#150539=CARTESIAN_POINT('Ctrl Pts',(3.38339122465858,6.14087049068806,43.5663023841681));
#150540=CARTESIAN_POINT('Ctrl Pts',(3.5448971218377,6.05188674871287,43.5579263723726));
#150541=CARTESIAN_POINT('Ctrl Pts',(3.70282366687429,5.95656458430923,43.5495503605772));
#150542=CARTESIAN_POINT('Ctrl Pts',(3.85667199919042,5.85522908630914,43.5411743487818));
#150543=CARTESIAN_POINT('Ctrl Pts',(4.01059578063015,5.75384389212841,43.5327942292866));
#150544=CARTESIAN_POINT('Ctrl Pts',(4.16043709015145,5.64643966964964,43.5244141097915));
#150545=CARTESIAN_POINT('Ctrl Pts',(4.30572803323922,5.53338347363329,43.5160339902963));
#150546=CARTESIAN_POINT('Ctrl Pts',(4.45118498963338,5.42019809659221,43.5076442954532));
#150547=CARTESIAN_POINT('Ctrl Pts',(4.59208093466106,5.30134804849269,43.49925460061));
#150548=CARTESIAN_POINT('Ctrl Pts',(4.72798188378807,5.17723998565566,43.4908649057668));
#150549=CARTESIAN_POINT('Ctrl Pts',(4.81426305039246,5.09844591898154,43.4855384333384));
#150550=CARTESIAN_POINT('Ctrl Pts',(4.89853157930441,5.01753323209812,43.4802119609099));
#150551=CARTESIAN_POINT('Ctrl Pts',(4.98068446843869,4.93461333726906,43.4748854884815));
#150552=CARTESIAN_POINT('Ctrl Pts',(5.10997061793832,4.80412013085434,43.4665030795614));
#150553=CARTESIAN_POINT('Ctrl Pts',(5.23427606721581,4.66839085165557,43.4581206706413));
#150554=CARTESIAN_POINT('Ctrl Pts',(5.35316640439172,4.52782906141474,43.4497382617213));
#150555=CARTESIAN_POINT('Ctrl Pts',(5.47190490539542,4.38744678419992,43.4413665580689));
#150556=CARTESIAN_POINT('Ctrl Pts',(5.58524186683985,4.24224454396566,43.4329948544165));
#150557=CARTESIAN_POINT('Ctrl Pts',(5.69277926922287,4.09266303944099,43.4246231507641));
#150558=CARTESIAN_POINT('Ctrl Pts',(5.80015425178126,3.94330745632778,43.4162640913695));
#150559=CARTESIAN_POINT('Ctrl Pts',(5.90174695544359,3.78958606530125,43.4079050319749));
#150560=CARTESIAN_POINT('Ctrl Pts',(5.99719936852696,3.63197278302576,43.3995459725804));
#150561=CARTESIAN_POINT('Ctrl Pts',(6.09256670581634,3.47449997991365,43.3911943635329));
#150562=CARTESIAN_POINT('Ctrl Pts',(6.18180448879049,3.31314247621896,43.3828427544855));
#150563=CARTESIAN_POINT('Ctrl Pts',(6.26459705733132,3.14840440092688,43.3744911454381));
#150564=CARTESIAN_POINT('Ctrl Pts',(6.34730824439963,2.98382825595517,43.366147745657));
#150565=CARTESIAN_POINT('Ctrl Pts',(6.423586704806,2.8158784578497,43.3578043458758));
#150566=CARTESIAN_POINT('Ctrl Pts',(6.49316189671506,2.64508509230757,43.3494609460947));
#150567=CARTESIAN_POINT('Ctrl Pts',(6.52015758027675,2.57881601673478,43.3462236459287));
#150568=CARTESIAN_POINT('Ctrl Pts',(6.54614457413794,2.51211911340437,43.3429863457626));
#150569=CARTESIAN_POINT('Ctrl Pts',(6.57110895151813,2.44502632087639,43.3397490455966));
#150570=CARTESIAN_POINT('Origin',(0.,0.,50.));
#150571=CARTESIAN_POINT('',(6.57110895151812,2.44502632087641,41.3399811574536));
#150572=CARTESIAN_POINT('',(6.57110895151814,2.44502632087636,41.8868188187145));
#150573=CARTESIAN_POINT('',(6.57110895151814,2.44502632087636,50.));
#150574=CARTESIAN_POINT('',(7.01124999682068,0.000211144444567105,43.773534356952));
#150575=CARTESIAN_POINT('Ctrl Pts',(6.57110895151814,2.44502632087636,41.8868188187145));
#150576=CARTESIAN_POINT('Ctrl Pts',(6.49634775445724,2.64595011749914,41.8965749404131));
#150577=CARTESIAN_POINT('Ctrl Pts',(6.41241070130866,2.84332624237747,41.9063310621117));
#150578=CARTESIAN_POINT('Ctrl Pts',(6.31963860203007,3.03641145140632,41.9160871838103));
#150579=CARTESIAN_POINT('Ctrl Pts',(6.22273057746059,3.23810470105867,41.9262782486737));
#150580=CARTESIAN_POINT('Ctrl Pts',(6.11618184448681,3.43511568285639,41.9364693135372));
#150581=CARTESIAN_POINT('Ctrl Pts',(6.00043438823921,3.62662566512404,41.9466603784007));
#150582=CARTESIAN_POINT('Ctrl Pts',(5.88978216895778,3.80970532181327,41.9564028296004));
#150583=CARTESIAN_POINT('Ctrl Pts',(5.77072362067052,3.98775777918142,41.9661452808002));
#150584=CARTESIAN_POINT('Ctrl Pts',(5.64369136065054,4.16009307446581,41.9758877319999));
#150585=CARTESIAN_POINT('Ctrl Pts',(5.51705865913114,4.33188631821016,41.9855995399662));
#150586=CARTESIAN_POINT('Ctrl Pts',(5.38250232509575,4.49799825636314,41.9953113479326));
#150587=CARTESIAN_POINT('Ctrl Pts',(5.24049601625629,4.65777071849849,42.0050231558989));
#150588=CARTESIAN_POINT('Ctrl Pts',(5.09942435511159,4.81649160085094,42.0146710433324));
#150589=CARTESIAN_POINT('Ctrl Pts',(4.95100046635482,4.96895612026904,42.0243189307659));
#150590=CARTESIAN_POINT('Ctrl Pts',(4.79573326718458,5.11454484705327,42.0339668181994));
#150591=CARTESIAN_POINT('Ctrl Pts',(4.77205912059392,5.13674328225566,42.0354378661903));
#150592=CARTESIAN_POINT('Ctrl Pts',(4.7482259642621,5.15878191801865,42.0369089141811));
#150593=CARTESIAN_POINT('Ctrl Pts',(4.72423569406022,5.18065861348414,42.038379962172));
#150594=CARTESIAN_POINT('Ctrl Pts',(4.59618553349387,5.29742738446687,42.0462318091854));
#150595=CARTESIAN_POINT('Ctrl Pts',(4.46370883293055,5.40953147826222,42.0540836561987));
#150596=CARTESIAN_POINT('Ctrl Pts',(4.32719841771571,5.51660950369144,42.0619355032121));
#150597=CARTESIAN_POINT('Ctrl Pts',(4.19072671575122,5.62365716265816,42.0697851235051));
#150598=CARTESIAN_POINT('Ctrl Pts',(4.0502238744537,5.72568135332894,42.0776347437981));
#150599=CARTESIAN_POINT('Ctrl Pts',(3.90611635632225,5.82236048122854,42.0854843640911));
#150600=CARTESIAN_POINT('Ctrl Pts',(3.76202034333272,5.91903189053648,42.0933333576923));
#150601=CARTESIAN_POINT('Ctrl Pts',(3.614320543612,6.01035887468585,42.1011823512936));
#150602=CARTESIAN_POINT('Ctrl Pts',(3.46347276878749,6.09606290505335,42.1090313448948));
#150603=CARTESIAN_POINT('Ctrl Pts',(3.31254862415192,6.18181032486172,42.1168843122116));
#150604=CARTESIAN_POINT('Ctrl Pts',(3.15847365216846,6.26192891428101,42.1247372795285));
#150605=CARTESIAN_POINT('Ctrl Pts',(3.00172895789514,6.33618574742201,42.1325902468453));
#150606=CARTESIAN_POINT('Ctrl Pts',(2.84494445573594,6.41046143930366,42.140445208552));
#150607=CARTESIAN_POINT('Ctrl Pts',(2.68548923111737,6.47887225867085,42.1483001702587));
#150608=CARTESIAN_POINT('Ctrl Pts',(2.52386416344037,6.54123354169544,42.1561551319654));
#150609=CARTESIAN_POINT('Ctrl Pts',(2.36207866937374,6.6036567235061,42.1640178903782));
#150610=CARTESIAN_POINT('Ctrl Pts',(2.19811939124847,6.66001825216441,42.1718806487909));
#150611=CARTESIAN_POINT('Ctrl Pts',(2.03250270343796,6.71018325554656,42.1797434072037));
#150612=CARTESIAN_POINT('Ctrl Pts',(1.911008677637,6.74698358222734,42.1855114139553));
#150613=CARTESIAN_POINT('Ctrl Pts',(1.78862303579138,6.78045030764135,42.1912794207069));
#150614=CARTESIAN_POINT('Ctrl Pts',(1.66555265408132,6.81054776937822,42.1970474274585));
#150615=CARTESIAN_POINT('Ctrl Pts',(1.48679214299145,6.85426452370882,42.2054254938995));
#150616=CARTESIAN_POINT('Ctrl Pts',(1.30619072057563,6.89096804313974,42.2138035603405));
#150617=CARTESIAN_POINT('Ctrl Pts',(1.12432478892261,6.92051445569722,42.2221816267815));
#150618=CARTESIAN_POINT('Ctrl Pts',(0.942583215032855,6.95004066476883,
42.2305539644002));
#150619=CARTESIAN_POINT('Ctrl Pts',(0.759579179210775,6.97241947149838,
42.2389263020189));
#150620=CARTESIAN_POINT('Ctrl Pts',(0.575899892183811,6.98755793369062,
42.2472986396376));
#150621=CARTESIAN_POINT('Ctrl Pts',(0.392319266182059,7.00268826444776,
42.2556664801601));
#150622=CARTESIAN_POINT('Ctrl Pts',(0.208064439051259,7.01058597814459,
42.2640343206827));
#150623=CARTESIAN_POINT('Ctrl Pts',(0.0237288319533614,7.01120984602758,
42.2724021612053));
#150624=CARTESIAN_POINT('Ctrl Pts',(-0.160534765413851,7.01183347019988,
42.2807667328752));
#150625=CARTESIAN_POINT('Ctrl Pts',(-0.344878751594196,7.00518891378272,
42.289131304545));
#150626=CARTESIAN_POINT('Ctrl Pts',(-0.52870814549189,6.99128702453207,
42.2974958762149));
#150627=CARTESIAN_POINT('Ctrl Pts',(-0.712492635593976,6.97738853108,42.3058584046805));
#150628=CARTESIAN_POINT('Ctrl Pts',(-0.89576245665924,6.95623626526056,
42.314220933146));
#150629=CARTESIAN_POINT('Ctrl Pts',(-1.07792573191966,6.92789309090184,
42.3225834616116));
#150630=CARTESIAN_POINT('Ctrl Pts',(-1.26010354437941,6.89954765466913,
42.330946657433));
#150631=CARTESIAN_POINT('Ctrl Pts',(-1.4411743089208,6.86401020797288,42.3393098532545));
#150632=CARTESIAN_POINT('Ctrl Pts',(-1.62055358182172,6.8213952129271,42.347673049076));
#150633=CARTESIAN_POINT('Ctrl Pts',(-1.7999450880295,6.77877731162408,42.3560368152507));
#150634=CARTESIAN_POINT('Ctrl Pts',(-1.97764455260624,6.72908097530092,
42.3644005814254));
#150635=CARTESIAN_POINT('Ctrl Pts',(-2.15307982731324,6.67247134274227,
42.3727643476));
#150636=CARTESIAN_POINT('Ctrl Pts',(-2.32855045600308,6.61585030212454,
42.3811297992536));
#150637=CARTESIAN_POINT('Ctrl Pts',(-2.50175567208873,6.55231328821959,
42.3894952509071));
#150638=CARTESIAN_POINT('Ctrl Pts',(-2.67214012577323,6.48207479984092,
42.3978607025606));
#150639=CARTESIAN_POINT('Ctrl Pts',(-2.84258164087623,6.4118127887306,42.4062289557875));
#150640=CARTESIAN_POINT('Ctrl Pts',(-3.01020020603632,6.33484495318477,
42.4145972090143));
#150641=CARTESIAN_POINT('Ctrl Pts',(-3.17446163268164,6.2514334280333,42.4229654622412));
#150642=CARTESIAN_POINT('Ctrl Pts',(-3.33887535310399,6.16794456849803,
42.4313414740326));
#150643=CARTESIAN_POINT('Ctrl Pts',(-3.49992542175955,6.07800023010056,
42.439717485824));
#150644=CARTESIAN_POINT('Ctrl Pts',(-3.65710230295307,5.98190850049007,
42.4480934976155));
#150645=CARTESIAN_POINT('Ctrl Pts',(-3.81435626563119,5.88576964630808,
42.4564736171066));
#150646=CARTESIAN_POINT('Ctrl Pts',(-3.96773297603646,5.78347756587186,
42.4648537365977));
#150647=CARTESIAN_POINT('Ctrl Pts',(-4.11675243227998,5.67538333276413,
42.4732338560889));
#150648=CARTESIAN_POINT('Ctrl Pts',(-4.26594216212908,5.56716558830239,
42.481623550928));
#150649=CARTESIAN_POINT('Ctrl Pts',(-4.41076442696253,5.45313264202748,
42.4900132457672));
#150650=CARTESIAN_POINT('Ctrl Pts',(-4.55077178064475,5.33367628966995,
42.4984029406064));
#150651=CARTESIAN_POINT('Ctrl Pts',(-4.63966003343352,5.25783551297988,
42.5037294130814));
#150652=CARTESIAN_POINT('Ctrl Pts',(-4.72660821032529,5.17980947477562,
42.5090558855564));
#150653=CARTESIAN_POINT('Ctrl Pts',(-4.81150961210109,5.09970605183856,
42.5143823580314));
#150654=CARTESIAN_POINT('Ctrl Pts',(-4.94510349747565,4.9736618726126,42.5227636584386));
#150655=CARTESIAN_POINT('Ctrl Pts',(-5.0738972901008,4.84221812798493,42.5311449588458));
#150656=CARTESIAN_POINT('Ctrl Pts',(-5.19744339656311,4.70576334955579,
42.539526259253));
#150657=CARTESIAN_POINT('Ctrl Pts',(-5.32083292642105,4.56948150758307,
42.5478969375889));
#150658=CARTESIAN_POINT('Ctrl Pts',(-5.43898780609068,4.42820152911682,
42.5562676159247));
#150659=CARTESIAN_POINT('Ctrl Pts',(-5.55149553120376,4.28235028104015,
42.5646382942606));
#150660=CARTESIAN_POINT('Ctrl Pts',(-5.66387557936526,4.13666454908889,
42.5729994733137));
#150661=CARTESIAN_POINT('Ctrl Pts',(-5.77062104701019,3.98641814485308,
42.5813606523668));
#150662=CARTESIAN_POINT('Ctrl Pts',(-5.87135786099275,3.83207299391057,
42.5897218314199));
#150663=CARTESIAN_POINT('Ctrl Pts',(-5.97196395707572,3.67792812400876,
42.5980721608568));
#150664=CARTESIAN_POINT('Ctrl Pts',(-6.06657677307801,3.51969538901241,
42.6064224902938));
#150665=CARTESIAN_POINT('Ctrl Pts',(-6.15486398375714,3.35786776153398,
42.6147728197307));
#150666=CARTESIAN_POINT('Ctrl Pts',(-6.24308326270857,3.19616465073514,
42.6231167240886));
#150667=CARTESIAN_POINT('Ctrl Pts',(-6.32498647947614,3.0308724461063,42.6314606284466));
#150668=CARTESIAN_POINT('Ctrl Pts',(-6.40028531910473,2.86251190330321,
42.6398045328045));
#150669=CARTESIAN_POINT('Ctrl Pts',(-6.47552367823529,2.69428658873902,
42.6481417352864));
#150670=CARTESIAN_POINT('Ctrl Pts',(-6.544168106265,2.52299814934422,42.6564789377682));
#150671=CARTESIAN_POINT('Ctrl Pts',(-6.60597677102849,2.34919081028596,
42.6648161402501));
#150672=CARTESIAN_POINT('Ctrl Pts',(-6.62632384218751,2.29197439395809,
42.6675607012726));
#150673=CARTESIAN_POINT('Ctrl Pts',(-6.64593050743587,2.23448518751981,
42.6703052622952));
#150674=CARTESIAN_POINT('Ctrl Pts',(-6.6647892687086,2.17674310983329,42.6730498233177));
#150675=CARTESIAN_POINT('Ctrl Pts',(-6.72208447986242,2.00131565276619,
42.6813881336148));
#150676=CARTESIAN_POINT('Ctrl Pts',(-6.77242574458169,1.82369680875694,
42.689726443912));
#150677=CARTESIAN_POINT('Ctrl Pts',(-6.81567017131908,1.64446546886562,
42.6980647542091));
#150678=CARTESIAN_POINT('Ctrl Pts',(-6.85894180598198,1.46512136269862,
42.706408310688));
#150679=CARTESIAN_POINT('Ctrl Pts',(-6.89510761963726,1.28416305555848,
42.714751867167));
#150680=CARTESIAN_POINT('Ctrl Pts',(-6.92407593220817,1.10217922658505,
42.7230954236459));
#150681=CARTESIAN_POINT('Ctrl Pts',(-6.95306628374478,0.920056945109259,
42.7314453278662));
#150682=CARTESIAN_POINT('Ctrl Pts',(-6.97484816025958,0.73690790874185,
42.7397952320865));
#150683=CARTESIAN_POINT('Ctrl Pts',(-6.98938172955066,0.553325944740973,
42.7481451363067));
#150684=CARTESIAN_POINT('Ctrl Pts',(-7.00393709812007,0.369468621380576,
42.7565075647654));
#150685=CARTESIAN_POINT('Ctrl Pts',(-7.01122240806093,0.185177399674693,
42.764869993224));
#150686=CARTESIAN_POINT('Ctrl Pts',(-7.01124992172655,0.0010476590323406,
42.7732324216827));
#150687=CARTESIAN_POINT('Ctrl Pts',(-7.0112774589201,-0.183239537638157,
42.7816020011576));
#150688=CARTESIAN_POINT('Ctrl Pts',(-7.00403482930223,-0.367364651104122,
42.7899715806325));
#150689=CARTESIAN_POINT('Ctrl Pts',(-6.98958621938242,-0.55073681946946,
42.7983411601074));
#150690=CARTESIAN_POINT('Ctrl Pts',(-6.97511532424224,-0.734391817062343,
42.8067236486389));
#150691=CARTESIAN_POINT('Ctrl Pts',(-6.95341627754758,-0.91729122414129,
42.8151061371704));
#150692=CARTESIAN_POINT('Ctrl Pts',(-6.9246046847036,-1.09885236637184,
42.8234886257019));
#150693=CARTESIAN_POINT('Ctrl Pts',(-6.91517705931131,-1.15826214784472,
42.826231513336));
#150694=CARTESIAN_POINT('Ctrl Pts',(-6.90498829125242,-1.2175287479788,
42.8289744009701));
#150695=CARTESIAN_POINT('Ctrl Pts',(-6.89404359269516,-1.27663209442611,
42.8317172886042));
#150696=CARTESIAN_POINT('Ctrl Pts',(-6.86056630610528,-1.45741548074663,
42.8401071437409));
#150697=CARTESIAN_POINT('Ctrl Pts',(-6.81994515840763,-1.63703542479715,
42.8484969988776));
#150698=CARTESIAN_POINT('Ctrl Pts',(-6.77227735039567,-1.81490662344314,
42.8568868540143));
#150699=CARTESIAN_POINT('Ctrl Pts',(-6.72465352956857,-1.99261368504108,
42.8652689671104));
#150700=CARTESIAN_POINT('Ctrl Pts',(-6.66999609595334,-2.1685749021898,
42.8736510802064));
#150701=CARTESIAN_POINT('Ctrl Pts',(-6.60845327083364,-2.34221517579155,
42.8820331933024));
#150702=CARTESIAN_POINT('Ctrl Pts',(-6.54695818990252,-2.51572074134322,
42.8904088036553));
#150703=CARTESIAN_POINT('Ctrl Pts',(-6.47858847642109,-2.68690864438706,
42.8987844140081));
#150704=CARTESIAN_POINT('Ctrl Pts',(-6.40354228024374,-2.85521852537259,
42.9071600243609));
#150705=CARTESIAN_POINT('Ctrl Pts',(-6.32854328923818,-3.02342253694367,
42.9155303663304));
#150706=CARTESIAN_POINT('Ctrl Pts',(-6.24687632269961,-3.18875183660909,
42.9239007083));
#150707=CARTESIAN_POINT('Ctrl Pts',(-6.15878795967867,-3.35066522204429,
42.9322710502695));
#150708=CARTESIAN_POINT('Ctrl Pts',(-6.07074209278142,-3.5125004962396,
42.9406373541678));
#150709=CARTESIAN_POINT('Ctrl Pts',(-5.97628116383119,-3.67092285419517,
42.949003658066));
#150710=CARTESIAN_POINT('Ctrl Pts',(-5.87569828684232,-3.82541451407534,
42.9573699619643));
#150711=CARTESIAN_POINT('Ctrl Pts',(-5.7751435400653,-3.97986296696787,
42.9657339260418));
#150712=CARTESIAN_POINT('Ctrl Pts',(-5.66847043717592,-4.13038263781536,
42.9740978901194));
#150713=CARTESIAN_POINT('Ctrl Pts',(-5.55601641213195,-4.27648315682646,
42.9824618541969));
#150714=CARTESIAN_POINT('Ctrl Pts',(-5.443579691894,-4.42256119339517,42.9908245311993));
#150715=CARTESIAN_POINT('Ctrl Pts',(-5.32536402356713,-4.56422117361238,
42.9991872082018));
#150716=CARTESIAN_POINT('Ctrl Pts',(-5.20174852013774,-4.70100403060291,
43.0075498852042));
#150717=CARTESIAN_POINT('Ctrl Pts',(-5.07813556172623,-4.83778407148377,
43.0159123900343));
#150718=CARTESIAN_POINT('Ctrl Pts',(-4.94912321054614,-4.96968694579816,
43.0242748948645));
#150719=CARTESIAN_POINT('Ctrl Pts',(-4.81512927927796,-5.09628851090087,
43.0326373996947));
#150720=CARTESIAN_POINT('Ctrl Pts',(-4.68112024626328,-5.22290434459561,
43.0410008470185));
#150721=CARTESIAN_POINT('Ctrl Pts',(-4.54212875304066,-5.34421745256245,
43.0493642943423));
#150722=CARTESIAN_POINT('Ctrl Pts',(-4.39860801316389,-5.45984194908886,
43.057727741666));
#150723=CARTESIAN_POINT('Ctrl Pts',(-4.25500276424368,-5.57553452856696,
43.0660961136226));
#150724=CARTESIAN_POINT('Ctrl Pts',(-4.10686319507153,-5.68553159612633,
43.0744644855791));
#150725=CARTESIAN_POINT('Ctrl Pts',(-3.95467483375107,-5.78948819169674,
43.0828328575356));
#150726=CARTESIAN_POINT('Ctrl Pts',(-3.80244087282097,-5.8934759353795,
43.0912037368751));
#150727=CARTESIAN_POINT('Ctrl Pts',(-3.64615597522751,-5.99141941716492,
43.0995746162145));
#150728=CARTESIAN_POINT('Ctrl Pts',(-3.48633354181123,-6.08301775418599,
43.1079454955539));
#150729=CARTESIAN_POINT('Ctrl Pts',(-3.32637569257764,-6.17469370148621,
43.1163234674488));
#150730=CARTESIAN_POINT('Ctrl Pts',(-3.16287460639404,-6.26001360258637,
43.1247014393436));
#150731=CARTESIAN_POINT('Ctrl Pts',(-2.99636812996869,-6.33872263095712,
43.1330794112385));
#150732=CARTESIAN_POINT('Ctrl Pts',(-2.89055190929516,-6.38874285896196,
43.1384036805513));
#150733=CARTESIAN_POINT('Ctrl Pts',(-2.7835223511343,-6.4360940987398,43.1437279498642));
#150734=CARTESIAN_POINT('Ctrl Pts',(-2.67542150514982,-6.48072112748897,
43.149052219177));
#150735=CARTESIAN_POINT('Ctrl Pts',(-2.51577918564716,-6.54662590665278,
43.1569150503604));
#150736=CARTESIAN_POINT('Ctrl Pts',(-2.35346754120656,-6.60672387524485,
43.1647778815438));
#150737=CARTESIAN_POINT('Ctrl Pts',(-2.18896620306236,-6.66078475289142,
43.1726407127272));
#150738=CARTESIAN_POINT('Ctrl Pts',(-2.02459126248158,-6.7148040918898,
43.1804975023628));
#150739=CARTESIAN_POINT('Ctrl Pts',(-1.85803033394368,-6.76279544641317,
43.1883542919984));
#150740=CARTESIAN_POINT('Ctrl Pts',(-1.68978413096512,-6.80457611855716,
43.196211081634));
#150741=CARTESIAN_POINT('Ctrl Pts',(-1.52163281087943,-6.84633322838018,
43.2040634404122));
#150742=CARTESIAN_POINT('Ctrl Pts',(-1.3517984758257,-6.88188653155631,
43.2119157991904));
#150743=CARTESIAN_POINT('Ctrl Pts',(-1.18079790401445,-6.91110286946845,
43.2197681579686));
#150744=CARTESIAN_POINT('Ctrl Pts',(-1.00983770743147,-6.94031230906266,
43.2276186627133));
#150745=CARTESIAN_POINT('Ctrl Pts',(-0.837712196201336,-6.96318768883827,
43.2354691674581));
#150746=CARTESIAN_POINT('Ctrl Pts',(-0.664949209373088,-6.97964677555062,
43.2433196722029));
#150747=CARTESIAN_POINT('Ctrl Pts',(-0.49221401466333,-6.99610321451476,
43.2511689140489));
#150748=CARTESIAN_POINT('Ctrl Pts',(-0.318841928596641,-7.0061453819911,
43.2590181558949));
#150749=CARTESIAN_POINT('Ctrl Pts',(-0.145366326392328,-7.00974287642929,
43.266867397741));
#150750=CARTESIAN_POINT('Ctrl Pts',(0.0281677231400067,-7.01334158293382,
43.2747192841503));
#150751=CARTESIAN_POINT('Ctrl Pts',(0.201804976693194,-7.01049127137047,
43.2825711705596));
#150752=CARTESIAN_POINT('Ctrl Pts',(0.375011438366876,-7.00121367932689,
43.290423056969));
#150753=CARTESIAN_POINT('Ctrl Pts',(0.502194788160678,-6.99440125891994,
43.2961885994672));
#150754=CARTESIAN_POINT('Ctrl Pts',(0.629145838212761,-6.9841244781284,
43.3019541419654));
#150755=CARTESIAN_POINT('Ctrl Pts',(0.755654950975328,-6.97040975535632,
43.3077196844635));
#150756=CARTESIAN_POINT('Ctrl Pts',(0.967514283888188,-6.94744230301925,
43.3173749888197));
#150757=CARTESIAN_POINT('Ctrl Pts',(1.17802605320893,-6.91484429355787,
43.3270302931758));
#150758=CARTESIAN_POINT('Ctrl Pts',(1.3864089148058,-6.87280851497021,43.336685597532));
#150759=CARTESIAN_POINT('Ctrl Pts',(1.59594617834613,-6.83053986605855,
43.3463943904621));
#150760=CARTESIAN_POINT('Ctrl Pts',(1.80333084590281,-6.77872865440678,
43.3561031833923));
#150761=CARTESIAN_POINT('Ctrl Pts',(2.0077895948559,-6.71761918430097,43.3658119763224));
#150762=CARTESIAN_POINT('Ctrl Pts',(2.21323221664931,-6.65621565024225,
43.3755674887875));
#150763=CARTESIAN_POINT('Ctrl Pts',(2.41572065796738,-6.58542418978038,
43.3853230012527));
#150764=CARTESIAN_POINT('Ctrl Pts',(2.61449212019618,-6.50554052450156,
43.3950785137178));
#150765=CARTESIAN_POINT('Ctrl Pts',(2.8134603967454,-6.4255777621073,43.4048436856408));
#150766=CARTESIAN_POINT('Ctrl Pts',(3.0087043011956,-6.33650481214536,43.4146088575637));
#150767=CARTESIAN_POINT('Ctrl Pts',(3.19948094731155,-6.23866558089872,
43.4243740294867));
#150768=CARTESIAN_POINT('Ctrl Pts',(3.38999747379362,-6.14095975122681,
43.434125886819));
#150769=CARTESIAN_POINT('Ctrl Pts',(3.57605888192642,-6.0345115466269,43.4438777441513));
#150770=CARTESIAN_POINT('Ctrl Pts',(3.75694787726415,-5.91971023024104,
43.4536296014836));
#150771=CARTESIAN_POINT('Ctrl Pts',(3.83582858036914,-5.86964854165137,
43.4578821175724));
#150772=CARTESIAN_POINT('Ctrl Pts',(3.91372599458072,-5.8179990315438,43.4621346336612));
#150773=CARTESIAN_POINT('Ctrl Pts',(3.99058201580301,-5.76479676464397,
43.4663871497499));
#150774=CARTESIAN_POINT('Ctrl Pts',(4.13576381249401,-5.66429714764961,
43.4744201953904));
#150775=CARTESIAN_POINT('Ctrl Pts',(4.27729824822765,-5.55820459552755,
43.4824532410308));
#150776=CARTESIAN_POINT('Ctrl Pts',(4.41472291734786,-5.44682000120654,
43.4904862866713));
#150777=CARTESIAN_POINT('Ctrl Pts',(4.55205924459962,-5.3355070091913,43.4985141683607));
#150778=CARTESIAN_POINT('Ctrl Pts',(4.68529078044798,-5.21890897645063,
43.5065420500502));
#150779=CARTESIAN_POINT('Ctrl Pts',(4.81398494431232,-5.09736947046556,
43.5145699317396));
#150780=CARTESIAN_POINT('Ctrl Pts',(4.94262100149232,-4.97588484076622,
43.5225941887613));
#150781=CARTESIAN_POINT('Ctrl Pts',(5.06672349986906,-4.84946343141362,
43.5306184457829));
#150782=CARTESIAN_POINT('Ctrl Pts',(5.18589379026815,-4.71848833404919,
43.5386427028046));
#150783=CARTESIAN_POINT('Ctrl Pts',(5.30504967176225,-4.58752907291143,
43.5466659896117));
#150784=CARTESIAN_POINT('Ctrl Pts',(5.41927428085916,-4.45201748622546,
43.5546892764187));
#150785=CARTESIAN_POINT('Ctrl Pts',(5.5282065155607,-4.31237281363895,43.5627125632258));
#150786=CARTESIAN_POINT('Ctrl Pts',(5.63712982423646,-4.17273958368876,
43.570735192596));
#150787=CARTESIAN_POINT('Ctrl Pts',(5.74076139998949,-4.02897423399752,
43.5787578219662));
#150788=CARTESIAN_POINT('Ctrl Pts',(5.83878125308421,-3.88152805492018,
43.5867804513364));
#150789=CARTESIAN_POINT('Ctrl Pts',(5.93683795466156,-3.73402644658235,
43.5948060966438));
#150790=CARTESIAN_POINT('Ctrl Pts',(6.02927851871268,-3.58284155176477,
43.6028317419511));
#150791=CARTESIAN_POINT('Ctrl Pts',(6.1158268140924,-3.42845284968723,43.6108573872585));
#150792=CARTESIAN_POINT('Ctrl Pts',(6.16686096010099,-3.33741586820384,
43.6155897965178));
#150793=CARTESIAN_POINT('Ctrl Pts',(6.2158472163727,-3.24526542402008,43.6203222057771));
#150794=CARTESIAN_POINT('Ctrl Pts',(6.26273655600089,-3.15210364560401,
43.6250546150364));
#150795=CARTESIAN_POINT('Ctrl Pts',(6.34919623652668,-2.98032179363219,
43.6337807475842));
#150796=CARTESIAN_POINT('Ctrl Pts',(6.42856752581141,-2.8050140054996,43.642506880132));
#150797=CARTESIAN_POINT('Ctrl Pts',(6.50059165124866,-2.6267726864379,43.6512330126798));
#150798=CARTESIAN_POINT('Ctrl Pts',(6.57263660920447,-2.44847981221239,
43.6599616692058));
#150799=CARTESIAN_POINT('Ctrl Pts',(6.63733005850005,-2.26725196788813,
43.6686903257318));
#150800=CARTESIAN_POINT('Ctrl Pts',(6.6944618396993,-2.0837003717689,43.6774189822577));
#150801=CARTESIAN_POINT('Ctrl Pts',(6.75162131715772,-1.9000597937823,43.6861518702487));
#150802=CARTESIAN_POINT('Ctrl Pts',(6.80121171769005,-1.71409347458198,
43.6948847582397));
#150803=CARTESIAN_POINT('Ctrl Pts',(6.84307272926248,-1.52642791658307,
43.7036176462306));
#150804=CARTESIAN_POINT('Ctrl Pts',(6.88493932166326,-1.33873733937833,
43.7123516984732));
#150805=CARTESIAN_POINT('Ctrl Pts',(6.9190744118959,-1.14934733992793,43.7210857507157));
#150806=CARTESIAN_POINT('Ctrl Pts',(6.94536873237034,-0.958895058863315,
43.7298198029583));
#150807=CARTESIAN_POINT('Ctrl Pts',(6.97167056821407,-0.768388343259293,
43.7385563515433));
#150808=CARTESIAN_POINT('Ctrl Pts',(6.99012711894441,-0.576819011385682,
43.7472929001283));
#150809=CARTESIAN_POINT('Ctrl Pts',(7.00068079599258,-0.384831073486362,
43.7560294487132));
#150810=CARTESIAN_POINT('Ctrl Pts',(7.00772938984235,-0.256606096340531,
43.7618644181124));
#150811=CARTESIAN_POINT('Ctrl Pts',(7.01125386375248,-0.128194519087721,
43.7676993875115));
#150812=CARTESIAN_POINT('Ctrl Pts',(7.01124999682071,0.000211143533935008,
43.7735343569106));
#150813=CARTESIAN_POINT('Ctrl Pts',(7.01124999682068,0.000211144444558622,
43.773534356952));
#150814=CARTESIAN_POINT('Ctrl Pts',(7.01124774628611,0.0749422630139,43.7769302647423));
#150815=CARTESIAN_POINT('Ctrl Pts',(7.01005060800529,0.149671035510726,
43.7803261725325));
#150816=CARTESIAN_POINT('Ctrl Pts',(7.00765927269819,0.224361494617859,
43.7837220803227));
#150817=CARTESIAN_POINT('Ctrl Pts',(7.00150410130018,0.416610810819736,
43.7924629684945));
#150818=CARTESIAN_POINT('Ctrl Pts',(6.9874329611689,0.608616908168221,43.8012038566662));
#150819=CARTESIAN_POINT('Ctrl Pts',(6.96549004337687,0.799734342214806,
43.809944744838));
#150820=CARTESIAN_POINT('Ctrl Pts',(6.94355157327669,0.990813037955818,
43.8186838612865));
#150821=CARTESIAN_POINT('Ctrl Pts',(6.91374454384324,1.18100315827288,43.8274229777351));
#150822=CARTESIAN_POINT('Ctrl Pts',(6.87616494592498,1.36966499514754,43.8361620941836));
#150823=CARTESIAN_POINT('Ctrl Pts',(6.83859395994941,1.55828359726144,43.8448992079292));
#150824=CARTESIAN_POINT('Ctrl Pts',(6.79325401590017,1.74537434692778,43.8536363216748));
#150825=CARTESIAN_POINT('Ctrl Pts',(6.74029227680452,1.93030738115706,43.8623734354205));
#150826=CARTESIAN_POINT('Ctrl Pts',(6.69056304853439,2.10395305878985,43.8705772809002));
#150827=CARTESIAN_POINT('Ctrl Pts',(6.63411451374727,2.27569627709552,43.8787811263799));
#150828=CARTESIAN_POINT('Ctrl Pts',(6.57110895151816,2.4450263208763,43.8869849718596));
#150829=CARTESIAN_POINT('',(7.01124705281206,-0.0064286028199779,43.2264656431312));
#150830=CARTESIAN_POINT('Ctrl Pts',(6.57110895151813,2.44502632087639,43.3397490455966));
#150831=CARTESIAN_POINT('Ctrl Pts',(6.63159529232099,2.28246678844903,43.3319053714627));
#150832=CARTESIAN_POINT('Ctrl Pts',(6.68607576390869,2.11758215313251,43.3240616973289));
#150833=CARTESIAN_POINT('Ctrl Pts',(6.7343787389157,1.95083816943902,43.316218023195));
#150834=CARTESIAN_POINT('Ctrl Pts',(6.78297200597525,1.78309208487557,43.308327210013));
#150835=CARTESIAN_POINT('Ctrl Pts',(6.82529219205804,1.61353383424519,43.300436396831));
#150836=CARTESIAN_POINT('Ctrl Pts',(6.86121524490491,1.4426891299183,43.292545583649));
#150837=CARTESIAN_POINT('Ctrl Pts',(6.8971430406971,1.2718218688479,43.2846537286376));
#150838=CARTESIAN_POINT('Ctrl Pts',(6.9266719524471,1.09966818699195,43.2767618736261));
#150839=CARTESIAN_POINT('Ctrl Pts',(6.94972928823205,0.926762851429489,
43.2688700186146));
#150840=CARTESIAN_POINT('Ctrl Pts',(6.97280535074523,0.7537170854522,43.2609717539891));
#150841=CARTESIAN_POINT('Ctrl Pts',(6.9893992976703,0.579918821660726,43.2530734893635));
#150842=CARTESIAN_POINT('Ctrl Pts',(6.99949039421429,0.405907358644683,
43.245175224738));
#150843=CARTESIAN_POINT('Ctrl Pts',(7.00745839745054,0.268506641644989,
43.2389386975357));
#150844=CARTESIAN_POINT('Ctrl Pts',(7.01137303626983,0.130973126874985,
43.2327021703335));
#150845=CARTESIAN_POINT('Ctrl Pts',(7.01124705281206,-0.00642860282006959,
43.2264656431312));
#150846=CARTESIAN_POINT('Ctrl Pts',(7.01124705281122,-0.00642860373435615,
43.2264656430897));
#150847=CARTESIAN_POINT('Ctrl Pts',(7.01105339140945,-0.217642109582684,
43.2168788731295));
#150848=CARTESIAN_POINT('Ctrl Pts',(7.00131167626943,-0.428520885109439,
43.2072921031694));
#150849=CARTESIAN_POINT('Ctrl Pts',(6.98213567632272,-0.638285171315712,
43.1977053332092));
#150850=CARTESIAN_POINT('Ctrl Pts',(6.96281940757936,-0.849583843425604,
43.1880484378481));
#150851=CARTESIAN_POINT('Ctrl Pts',(6.93393038750432,-1.05975159588273,
43.1783915424869));
#150852=CARTESIAN_POINT('Ctrl Pts',(6.89563491529918,-1.26800854784458,
43.1687346471258));
#150853=CARTESIAN_POINT('Ctrl Pts',(6.88085100660889,-1.34840582680821,
43.1650066173867));
#150854=CARTESIAN_POINT('Ctrl Pts',(6.86466574336499,-1.4285185177329,43.1612785876477));
#150855=CARTESIAN_POINT('Ctrl Pts',(6.84709064208999,-1.50830245690437,
43.1575505579087));
#150856=CARTESIAN_POINT('Ctrl Pts',(6.8075382339915,-1.68785458991562,43.1491607027759));
#150857=CARTESIAN_POINT('Ctrl Pts',(6.76088524413027,-1.8660031247024,43.1407708476431));
#150858=CARTESIAN_POINT('Ctrl Pts',(6.70724854843079,-2.04216636738369,
43.1323809925103));
#150859=CARTESIAN_POINT('Ctrl Pts',(6.65366134792218,-2.21816704909422,
43.1239988794182));
#150860=CARTESIAN_POINT('Ctrl Pts',(6.59310338389595,-2.39218577783364,
43.1156167663261));
#150861=CARTESIAN_POINT('Ctrl Pts',(6.52574217979552,-2.56365277784212,
43.1072346532341));
#150862=CARTESIAN_POINT('Ctrl Pts',(6.4584332337127,-2.73498675579992,43.0988590428852));
#150863=CARTESIAN_POINT('Ctrl Pts',(6.38433168979245,-2.90377264688196,
43.0904834325363));
#150864=CARTESIAN_POINT('Ctrl Pts',(6.30365447480766,-3.06945708957421,
43.0821078221875));
#150865=CARTESIAN_POINT('Ctrl Pts',(6.22302800698904,-3.23503731429183,
43.0737374802219));
#150866=CARTESIAN_POINT('Ctrl Pts',(6.13583425884974,-3.39751968566467,
43.0653671382563));
#150867=CARTESIAN_POINT('Ctrl Pts',(6.04233791305133,-3.55637162104898,
43.0569967962907));
#150868=CARTESIAN_POINT('Ctrl Pts',(5.9488866723286,-3.71514692211667,43.0486304923964));
#150869=CARTESIAN_POINT('Ctrl Pts',(5.84913906371482,-3.87029499701398,
43.0402641885021));
#150870=CARTESIAN_POINT('Ctrl Pts',(5.74340548889108,-4.02130823895356,
43.0318978846077));
#150871=CARTESIAN_POINT('Ctrl Pts',(5.63770148478455,-4.17227924672222,
43.0235339205341));
#150872=CARTESIAN_POINT('Ctrl Pts',(5.52601503976411,-4.31911745755718,
43.0151699564605));
#150873=CARTESIAN_POINT('Ctrl Pts',(5.40869992621494,-4.46134415514681,
43.0068059923869));
#150874=CARTESIAN_POINT('Ctrl Pts',(5.29140286551229,-4.60354896641108,
42.9984433153883));
#150875=CARTESIAN_POINT('Ctrl Pts',(5.16847907229621,-4.74114342583738,
42.9900806383898));
#150876=CARTESIAN_POINT('Ctrl Pts',(5.04032291908206,-4.87368150722594,
42.9817179613912));
#150877=CARTESIAN_POINT('Ctrl Pts',(4.91216940436875,-5.00621685989779,
42.9733554565649));
#150878=CARTESIAN_POINT('Ctrl Pts',(4.77878397320084,-5.13369580612759,
42.9649929517386));
#150879=CARTESIAN_POINT('Ctrl Pts',(4.64059849850934,-5.25570852865081,
42.9566304469123));
#150880=CARTESIAN_POINT('Ctrl Pts',(4.50239744966423,-5.37773500258233,
42.9482669995923));
#150881=CARTESIAN_POINT('Ctrl Pts',(4.35939552542613,-5.49429380742749,
42.9399035522723));
#150882=CARTESIAN_POINT('Ctrl Pts',(4.21205868985145,-5.60501455446343,
42.9315401049523));
#150883=CARTESIAN_POINT('Ctrl Pts',(4.06463509820729,-5.71580049698688,
42.9231717329995));
#150884=CARTESIAN_POINT('Ctrl Pts',(3.91287175712499,-5.82074131411516,
42.9148033610467));
#150885=CARTESIAN_POINT('Ctrl Pts',(3.75726554725558,-5.91950860882103,
42.9064349890939));
#150886=CARTESIAN_POINT('Ctrl Pts',(3.60161271369882,-6.01830549678974,
42.8980641097582));
#150887=CARTESIAN_POINT('Ctrl Pts',(3.44211499581521,-6.11092500229065,
42.8896932304224));
#150888=CARTESIAN_POINT('Ctrl Pts',(3.27929564532388,-6.19708372002992,
42.8813223510867));
#150889=CARTESIAN_POINT('Ctrl Pts',(3.11633833975749,-6.28331543911907,
42.8729443791954));
#150890=CARTESIAN_POINT('Ctrl Pts',(2.95005407118001,-6.36307528302324,
42.8645664073041));
#150891=CARTESIAN_POINT('Ctrl Pts',(2.78098897074107,-6.43612670067305,
42.8561884354128));
#150892=CARTESIAN_POINT('Ctrl Pts',(2.67354672270923,-6.48255147144969,
42.8508641660538));
#150893=CARTESIAN_POINT('Ctrl Pts',(2.56498179745355,-6.52626786962235,
42.8455398966948));
#150894=CARTESIAN_POINT('Ctrl Pts',(2.45543802545239,-6.56722549221987,
42.8402156273357));
#150895=CARTESIAN_POINT('Ctrl Pts',(2.2936648075827,-6.62771132617328,42.8323527961471));
#150896=CARTESIAN_POINT('Ctrl Pts',(2.12941952748639,-6.68230366769121,
42.8244899649584));
#150897=CARTESIAN_POINT('Ctrl Pts',(1.96318930648301,-6.73078853548459,
42.8166271337697));
#150898=CARTESIAN_POINT('Ctrl Pts',(1.79708681146244,-6.77923614905696,
42.808770344129));
#150899=CARTESIAN_POINT('Ctrl Pts',(1.62900277219913,-6.82158551511934,
42.8009135544882));
#150900=CARTESIAN_POINT('Ctrl Pts',(1.45944377632387,-6.85767091848607,
42.7930567648474));
#150901=CARTESIAN_POINT('Ctrl Pts',(1.28998040369568,-6.89373597139351,
42.7852044060641));
#150902=CARTESIAN_POINT('Ctrl Pts',(1.11904410086539,-6.92354400959627,
42.7773520472808));
#150903=CARTESIAN_POINT('Ctrl Pts',(0.94715584107491,-6.94697937057666,
42.7694996884974));
#150904=CARTESIAN_POINT('Ctrl Pts',(0.775308166108197,-6.97040919819487,
42.7616491837476));
#150905=CARTESIAN_POINT('Ctrl Pts',(0.602509357826003,-6.98746928346902,
42.7537986789978));
#150906=CARTESIAN_POINT('Ctrl Pts',(0.429289727345191,-6.99809523316852,
42.745948174248));
#150907=CARTESIAN_POINT('Ctrl Pts',(0.256097962443485,-7.00871947348761,
42.738098932397));
#150908=CARTESIAN_POINT('Ctrl Pts',(0.0824858911056665,-7.01291161835322,
42.730249690546));
#150909=CARTESIAN_POINT('Ctrl Pts',(-0.0910123897566303,-7.01065926339391,
42.7224004486949));
#150910=CARTESIAN_POINT('Ctrl Pts',(-0.26456912558573,-7.00840614957212,
42.7145485622807));
#150911=CARTESIAN_POINT('Ctrl Pts',(-0.438011612530421,-6.99970420388659,
42.7066966758665));
#150912=CARTESIAN_POINT('Ctrl Pts',(-0.610806890943731,-6.98459315239447,
42.6988447894522));
#150913=CARTESIAN_POINT('Ctrl Pts',(-0.737688313234154,-6.97349729535931,
42.6930792469846));
#150914=CARTESIAN_POINT('Ctrl Pts',(-0.864220785375445,-6.95894687763085,
42.6873137045169));
#150915=CARTESIAN_POINT('Ctrl Pts',(-0.990195679522643,-6.94097536940989,
42.6815481620493));
#150916=CARTESIAN_POINT('Ctrl Pts',(-1.20116038087808,-6.9108792626387,
42.6718928576882));
#150917=CARTESIAN_POINT('Ctrl Pts',(-1.41045364162706,-6.87120349800956,
42.6622375533272));
#150918=CARTESIAN_POINT('Ctrl Pts',(-1.61730106051943,-6.82216709280436,
42.6525822489661));
#150919=CARTESIAN_POINT('Ctrl Pts',(-1.82529437531023,-6.772859035113,42.6428734560302));
#150920=CARTESIAN_POINT('Ctrl Pts',(-2.03081464088909,-6.71408640131081,
42.6331646630942));
#150921=CARTESIAN_POINT('Ctrl Pts',(-2.23309720955559,-6.64611942528684,
42.6234558701582));
#150922=CARTESIAN_POINT('Ctrl Pts',(-2.43635317912132,-6.57782538640216,
42.6137003576861));
#150923=CARTESIAN_POINT('Ctrl Pts',(-2.63634018328757,-6.50024834100388,
42.603944845214));
#150924=CARTESIAN_POINT('Ctrl Pts',(-2.83230582563868,-6.41370955629839,
42.5941893327419));
#150925=CARTESIAN_POINT('Ctrl Pts',(-3.02846550412476,-6.32708508488216,
42.5844241608115));
#150926=CARTESIAN_POINT('Ctrl Pts',(-3.22059582579476,-6.23148115084333,
42.5746589888812));
#150927=CARTESIAN_POINT('Ctrl Pts',(-3.40796591958496,-6.12726650746052,
42.5648938169509));
#150928=CARTESIAN_POINT('Ctrl Pts',(-3.59508053850253,-6.02319395837999,
42.5551419596109));
#150929=CARTESIAN_POINT('Ctrl Pts',(-3.77744786850087,-5.9105341834902,
42.545390102271));
#150930=CARTESIAN_POINT('Ctrl Pts',(-3.95436414472565,-5.78970040446034,
42.5356382449311));
#150931=CARTESIAN_POINT('Ctrl Pts',(-4.03151245391501,-5.73700812569414,
42.531385728875));
#150932=CARTESIAN_POINT('Ctrl Pts',(-4.1076245081266,-5.6827620741858,42.527133212819));
#150933=CARTESIAN_POINT('Ctrl Pts',(-4.18264341830858,-5.6269992534014,
42.5228806967629));
#150934=CARTESIAN_POINT('Ctrl Pts',(-4.32435489412508,-5.52166272411994,
42.5148476511644));
#150935=CARTESIAN_POINT('Ctrl Pts',(-4.46223254596517,-5.41085938973109,
42.5068146055659));
#150936=CARTESIAN_POINT('Ctrl Pts',(-4.5958243739763,-5.29490555969277,
42.4987815599674));
#150937=CARTESIAN_POINT('Ctrl Pts',(-4.72933032401663,-5.17902626924102,
42.4907536783199));
#150938=CARTESIAN_POINT('Ctrl Pts',(-4.85855565862773,-5.05800331292143,
42.4827257966724));
#150939=CARTESIAN_POINT('Ctrl Pts',(-4.98307962462678,-4.9321946450976,
42.4746979150249));
#150940=CARTESIAN_POINT('Ctrl Pts',(-5.10754736682769,-4.80644278112744,
42.4666736580451));
#150941=CARTESIAN_POINT('Ctrl Pts',(-5.22731770964945,-4.67590976803552,
42.4586494010653));
#150942=CARTESIAN_POINT('Ctrl Pts',(-5.3420051443773,-4.54099191806663,
42.4506251440856));
#150943=CARTESIAN_POINT('Ctrl Pts',(-5.45667871222614,-4.40609038104002,
42.4426018573202));
#150944=CARTESIAN_POINT('Ctrl Pts',(-5.56627035295775,-4.26680533728741,
42.4345785705548));
#150945=CARTESIAN_POINT('Ctrl Pts',(-5.67043330223153,-4.12356796081303,
42.4265552837894));
#150946=CARTESIAN_POINT('Ctrl Pts',(-5.77458771628075,-3.98034232136396,
42.4185326544608));
#150947=CARTESIAN_POINT('Ctrl Pts',(-5.87331411254904,-3.83316529317963,
42.4105100251322));
#150948=CARTESIAN_POINT('Ctrl Pts',(-5.96630789601164,-3.68249869687543,
42.4024873958036));
#150949=CARTESIAN_POINT('Ctrl Pts',(-6.05933663851642,-3.53177546065724,
42.3944617505376));
#150950=CARTESIAN_POINT('Ctrl Pts',(-6.1466282730285,-3.37756034944542,
42.3864361052715));
#150951=CARTESIAN_POINT('Ctrl Pts',(-6.22792298842453,-3.22034187824109,
42.3784104600054));
#150952=CARTESIAN_POINT('Ctrl Pts',(-6.27585930649862,-3.12763628715733,
42.3736780504957));
#150953=CARTESIAN_POINT('Ctrl Pts',(-6.32171136404131,-3.03388689975875,
42.3689456409861));
#150954=CARTESIAN_POINT('Ctrl Pts',(-6.36543360471897,-2.93919743916847,
42.3642132314764));
#150955=CARTESIAN_POINT('Ctrl Pts',(-6.4460896205419,-2.76452032945811,
42.3554831826414));
#150956=CARTESIAN_POINT('Ctrl Pts',(-6.51953573012396,-2.58655576672363,
42.3467531338065));
#150957=CARTESIAN_POINT('Ctrl Pts',(-6.58553315993489,-2.40590514399426,
42.3380230849715));
#150958=CARTESIAN_POINT('Ctrl Pts',(-6.6515496729849,-2.22520228591219,
42.329290511832));
#150959=CARTESIAN_POINT('Ctrl Pts',(-6.71011311316938,-2.04181207485348,
42.3205579386925));
#150960=CARTESIAN_POINT('Ctrl Pts',(-6.76103393682314,-1.85635305575902,
42.311825365553));
#150961=CARTESIAN_POINT('Ctrl Pts',(-6.8126781720589,-1.6682592952607,42.3029687322727));
#150962=CARTESIAN_POINT('Ctrl Pts',(-6.85646090787913,-1.4780377767837,
42.2941120989925));
#150963=CARTESIAN_POINT('Ctrl Pts',(-6.89223749999138,-1.28634707844057,
42.2852554657122));
#150964=CARTESIAN_POINT('Ctrl Pts',(-6.92753540364462,-1.09722118908503,
42.2765173336052));
#150965=CARTESIAN_POINT('Ctrl Pts',(-6.95504004824143,-0.90666546805699,
42.2677792014981));
#150966=CARTESIAN_POINT('Ctrl Pts',(-6.97466431409351,-0.715321094481741,
42.259041069391));
#150967=CARTESIAN_POINT('Ctrl Pts',(-6.99468777828065,-0.520084378847368,
42.2501251855241));
#150968=CARTESIAN_POINT('Ctrl Pts',(-7.00650678902527,-0.324026875597594,
42.2412093016573));
#150969=CARTESIAN_POINT('Ctrl Pts',(-7.01008451422186,-0.127834525723511,
42.2322934177905));
#150970=CARTESIAN_POINT('Ctrl Pts',(-7.01366223941844,0.0683578241506386,
42.2233775339236));
#150971=CARTESIAN_POINT('Ctrl Pts',(-7.00899867963518,0.264684718176251,
42.2144616500568));
#150972=CARTESIAN_POINT('Ctrl Pts',(-6.99611344218405,0.460459842539722,
42.20554576619));
#150973=CARTESIAN_POINT('Ctrl Pts',(-6.98348140290468,0.652387936240791,
42.196805081694));
#150974=CARTESIAN_POINT('Ctrl Pts',(-6.9629464611194,0.843806128503964,
42.188064397198));
#150975=CARTESIAN_POINT('Ctrl Pts',(-6.93457453528062,1.03407087626406,
42.179323712702));
#150976=CARTESIAN_POINT('Ctrl Pts',(-6.90620771402259,1.22430139223555,
42.1705846008004));
#150977=CARTESIAN_POINT('Ctrl Pts',(-6.87000676496269,1.41337860744149,
42.1618454888987));
#150978=CARTESIAN_POINT('Ctrl Pts',(-6.82608918734702,1.60066641399265,
42.1531063769971));
#150979=CARTESIAN_POINT('Ctrl Pts',(-6.78160259430321,1.79038080363917,
42.1442540373226));
#150980=CARTESIAN_POINT('Ctrl Pts',(-6.72919806190732,1.97825881004582,
42.1354016976482));
#150981=CARTESIAN_POINT('Ctrl Pts',(-6.66905099339334,2.16365094458865,
42.1265493579737));
#150982=CARTESIAN_POINT('Ctrl Pts',(-6.60970368322049,2.3465779730233,42.1178147253242));
#150983=CARTESIAN_POINT('Ctrl Pts',(-6.54281855873748,2.52708456395344,
42.1090800926747));
#150984=CARTESIAN_POINT('Ctrl Pts',(-6.46861428810261,2.70456202632788,
42.1003454600252));
#150985=CARTESIAN_POINT('Ctrl Pts',(-6.39291006361437,2.88562699116408,
42.0914342668383));
#150986=CARTESIAN_POINT('Ctrl Pts',(-6.30958773733975,3.06353878623212,
42.0825230736513));
#150987=CARTESIAN_POINT('Ctrl Pts',(-6.21893156113291,3.23767150903932,
42.0736118804644));
#150988=CARTESIAN_POINT('Ctrl Pts',(-6.12827538492605,3.41180423184659,
42.0647006872775));
#150989=CARTESIAN_POINT('Ctrl Pts',(-6.03028548681558,3.58215760729687,
42.0557894940906));
#150990=CARTESIAN_POINT('Ctrl Pts',(-5.92529694581475,3.74813055621311,
42.0468783009037));
#150991=CARTESIAN_POINT('Ctrl Pts',(-5.83074138790573,3.89761034355921,
42.0388526360512));
#150992=CARTESIAN_POINT('Ctrl Pts',(-5.73046512869765,4.04360545455386,
42.0308269711987));
#150993=CARTESIAN_POINT('Ctrl Pts',(-5.62476393450537,4.1856489632538,42.0228013063462));
#150994=CARTESIAN_POINT('Ctrl Pts',(-5.51909628727948,4.32764739082815,
42.0147781886429));
#150995=CARTESIAN_POINT('Ctrl Pts',(-5.40800735147344,4.46569641925513,
42.0067550709396));
#150996=CARTESIAN_POINT('Ctrl Pts',(-5.29183575177128,4.59935875299757,
41.9987319532363));
#150997=CARTESIAN_POINT('Ctrl Pts',(-5.17567880232444,4.73300423075006,
41.9907098473183));
#150998=CARTESIAN_POINT('Ctrl Pts',(-5.05444070656423,4.86226383952261,
41.9826877414003));
#150999=CARTESIAN_POINT('Ctrl Pts',(-4.92849980283099,4.98673402699551,
41.9746656354824));
#151000=CARTESIAN_POINT('Ctrl Pts',(-4.80251209903253,5.1112504680105,41.9666405485228));
#151001=CARTESIAN_POINT('Ctrl Pts',(-4.6718183550072,5.23097367226489,41.9586154615631));
#151002=CARTESIAN_POINT('Ctrl Pts',(-4.53683346105611,5.34553727039123,
41.9505903746035));
#151003=CARTESIAN_POINT('Ctrl Pts',(-4.40182198250564,5.46012343124491,
41.9425637071432));
#151004=CARTESIAN_POINT('Ctrl Pts',(-4.26251795558613,5.56954773113641,
41.9345370396829));
#151005=CARTESIAN_POINT('Ctrl Pts',(-4.11936848024561,5.67348480974956,
41.9265103722225));
#151006=CARTESIAN_POINT('Ctrl Pts',(-3.97610408501076,5.77750532868313,
41.9184772609818));
#151007=CARTESIAN_POINT('Ctrl Pts',(-3.82898837764871,5.87602962039594,
41.9104441497411));
#151008=CARTESIAN_POINT('Ctrl Pts',(-3.67849700871148,5.96877594816565,
41.9024110385005));
#151009=CARTESIAN_POINT('Ctrl Pts',(-3.58982202724712,6.02342545367514,
41.8976776375393));
#151010=CARTESIAN_POINT('Ctrl Pts',(-3.49997551438973,6.07606970805002,
41.8929442365782));
#151011=CARTESIAN_POINT('Ctrl Pts',(-3.40905855336876,6.12665866049377,
41.8882108356171));
#151012=CARTESIAN_POINT('Ctrl Pts',(-3.22176678412568,6.23087347696965,
41.8784598823231));
#151013=CARTESIAN_POINT('Ctrl Pts',(-3.0298210583233,6.32642565517752,41.8687089290291));
#151014=CARTESIAN_POINT('Ctrl Pts',(-2.83396501947201,6.41297659678476,
41.8589579757351));
#151015=CARTESIAN_POINT('Ctrl Pts',(-2.63782681325505,6.49965223125995,
41.8491929743637));
#151016=CARTESIAN_POINT('Ctrl Pts',(-2.43776706058922,6.57730067376265,
41.8394279729922));
#151017=CARTESIAN_POINT('Ctrl Pts',(-2.23455086222943,6.64563082081827,
41.8296629716208));
#151018=CARTESIAN_POINT('Ctrl Pts',(-2.03167338316677,6.71384707567646,
41.8199142464834));
#151019=CARTESIAN_POINT('Ctrl Pts',(-1.82565000922661,6.77277606450171,
41.8101655213459));
#151020=CARTESIAN_POINT('Ctrl Pts',(-1.61725958581747,6.82217692489586,
41.8004167962085));
#151021=CARTESIAN_POINT('Ctrl Pts',(-1.40944111331638,6.87144219908361,
41.7906948275415));
#151022=CARTESIAN_POINT('Ctrl Pts',(-1.19926859966887,6.91123154186169,
41.7809728588745));
#151023=CARTESIAN_POINT('Ctrl Pts',(-0.987531454394643,6.9413549245865,
41.7712508902075));
#151024=CARTESIAN_POINT('Ctrl Pts',(-0.777195318508695,6.97127898875551,
41.7615932492679));
#151025=CARTESIAN_POINT('Ctrl Pts',(-0.565315230214999,6.99166454918276,
41.7519356083283));
#151026=CARTESIAN_POINT('Ctrl Pts',(-0.35268122158664,7.00237406301893,
41.7422779673888));
#151027=CARTESIAN_POINT('Ctrl Pts',(-0.259221254235411,7.00708126305683,
41.7380331017028));
#151028=CARTESIAN_POINT('Ctrl Pts',(-0.16561584406838,7.0099197817077,41.7337882360168));
#151029=CARTESIAN_POINT('Ctrl Pts',(-0.0719330421799695,7.01088098600616,
41.7295433703308));
#151030=CARTESIAN_POINT('Ctrl Pts',(0.101354661761592,7.01265895253302,
41.7216915233168));
#151031=CARTESIAN_POINT('Ctrl Pts',(0.274836025484513,7.00800916941411,
41.7138396763029));
#151032=CARTESIAN_POINT('Ctrl Pts',(0.447977331687376,6.99692381499143,
41.705987829289));
#151033=CARTESIAN_POINT('Ctrl Pts',(0.621069536415629,6.98584160428565,
41.6981382089953));
#151034=CARTESIAN_POINT('Ctrl Pts',(0.793821495145662,6.96832747701359,
41.6902885887017));
#151035=CARTESIAN_POINT('Ctrl Pts',(0.965700916861905,6.94442569991732,
41.6824389684081));
#151036=CARTESIAN_POINT('Ctrl Pts',(1.13756661620472,6.92052583107223,41.6745899748063));
#151037=CARTESIAN_POINT('Ctrl Pts',(1.30855953948441,6.89023938090103,41.6667409812045));
#151038=CARTESIAN_POINT('Ctrl Pts',(1.47815419777677,6.85366228596762,41.6588919876026));
#151039=CARTESIAN_POINT('Ctrl Pts',(1.64783471687858,6.81706667312209,41.6510390202852));
#151040=CARTESIAN_POINT('Ctrl Pts',(1.81611518319584,6.77417413271322,41.6431860529677));
#151041=CARTESIAN_POINT('Ctrl Pts',(1.98248162460617,6.72513146121315,41.6353330856503));
#151042=CARTESIAN_POINT('Ctrl Pts',(2.14889031750256,6.67607633452239,41.627478123943));
#151043=CARTESIAN_POINT('Ctrl Pts',(2.31338365538907,6.62086808640719,41.6196231622357));
#151044=CARTESIAN_POINT('Ctrl Pts',(2.4754650705954,6.55970267975326,41.6117682005284));
#151045=CARTESIAN_POINT('Ctrl Pts',(2.63770736515455,6.49847656132048,41.603905442115));
#151046=CARTESIAN_POINT('Ctrl Pts',(2.79753260403959,6.4312816224051,41.5960426837016));
#151047=CARTESIAN_POINT('Ctrl Pts',(2.95446583453959,6.35836128220458,41.5881799252883));
#151048=CARTESIAN_POINT('Ctrl Pts',(3.06958980057272,6.30486796697987,41.5824119185403));
#151049=CARTESIAN_POINT('Ctrl Pts',(3.18315789977903,6.24829452919848,41.5766439117923));
#151050=CARTESIAN_POINT('Ctrl Pts',(3.29499208989923,6.18875219167818,41.5708759050443));
#151051=CARTESIAN_POINT('Ctrl Pts',(3.45744846422137,6.10225778185758,41.5624969874491));
#151052=CARTESIAN_POINT('Ctrl Pts',(3.61660492633648,6.00930532445614,41.5541180698539));
#151053=CARTESIAN_POINT('Ctrl Pts',(3.7719356013268,5.91017160342604,41.5457391522587));
#151054=CARTESIAN_POINT('Ctrl Pts',(3.93086885978249,5.8087386745655,41.5371659024751));
#151055=CARTESIAN_POINT('Ctrl Pts',(4.0857963892189,5.70083440572801,41.5285926526916));
#151056=CARTESIAN_POINT('Ctrl Pts',(4.23618184298822,5.58680498636179,41.520019402908));
#151057=CARTESIAN_POINT('Ctrl Pts',(4.38295992378626,5.47551084913252,41.5116518040619));
#151058=CARTESIAN_POINT('Ctrl Pts',(4.52541105514494,5.35838225339701,41.5032842052158));
#151059=CARTESIAN_POINT('Ctrl Pts',(4.66306599911358,5.23578475974814,41.4949166063697));
#151060=CARTESIAN_POINT('Ctrl Pts',(4.80067075234893,5.11323196669577,41.486552058456));
#151061=CARTESIAN_POINT('Ctrl Pts',(4.93348255967734,4.98521446964347,41.4781875105422));
#151062=CARTESIAN_POINT('Ctrl Pts',(5.06106576744254,4.85213765881815,41.4698229626285));
#151063=CARTESIAN_POINT('Ctrl Pts',(5.18861947139895,4.71909162220559,41.461460349029));
#151064=CARTESIAN_POINT('Ctrl Pts',(5.31094675979103,4.58098884209341,41.4530977354296));
#151065=CARTESIAN_POINT('Ctrl Pts',(5.42764901555431,4.43827136692343,41.4447351218301));
#151066=CARTESIAN_POINT('Ctrl Pts',(5.54947121660713,4.28929261034159,41.4360056247987));
#151067=CARTESIAN_POINT('Ctrl Pts',(5.66516342534486,4.13528538849491,41.4272761277673));
#151068=CARTESIAN_POINT('Ctrl Pts',(5.77431886242675,3.97679119863272,41.418546630736));
#151069=CARTESIAN_POINT('Ctrl Pts',(5.87889964190271,3.82493943236876,41.4101829831855));
#151070=CARTESIAN_POINT('Ctrl Pts',(5.97748020051843,3.66896942009114,41.4018193356349));
#151071=CARTESIAN_POINT('Ctrl Pts',(6.06974688604635,3.50938731145917,41.3934556880844));
#151072=CARTESIAN_POINT('Ctrl Pts',(6.16202538967972,3.34978476253312,41.3850909692646));
#151073=CARTESIAN_POINT('Ctrl Pts',(6.2479882470465,3.18656948144339,41.3767262504448));
#151074=CARTESIAN_POINT('Ctrl Pts',(6.32736743218011,3.02027282553852,41.368361531625));
#151075=CARTESIAN_POINT('Ctrl Pts',(6.40678194226691,2.85390216507471,41.3599930903772));
#151076=CARTESIAN_POINT('Ctrl Pts',(6.4796067910886,2.68444768954274,41.3516246491294));
#151077=CARTESIAN_POINT('Ctrl Pts',(6.54562151305036,2.51246205352286,41.3432562078816));
#151078=CARTESIAN_POINT('Ctrl Pts',(6.55423329378749,2.49002610979205,41.3421645244056));
#151079=CARTESIAN_POINT('Ctrl Pts',(6.56272924917659,2.46754711609132,41.3410728409296));
#151080=CARTESIAN_POINT('Ctrl Pts',(6.57110895151812,2.44502632087641,41.3399811574536));
#151081=CARTESIAN_POINT('Origin',(0.,0.,50.));
#151082=CARTESIAN_POINT('',(6.57110895151813,2.44502632087639,39.3399667765699));
#151083=CARTESIAN_POINT('',(6.57110895151814,2.44502632087636,39.8869210003223));
#151084=CARTESIAN_POINT('',(6.57110895151814,2.44502632087636,50.));
#151085=CARTESIAN_POINT('',(7.01125,4.02193903181747E-12,41.7735343569105));
#151086=CARTESIAN_POINT('Ctrl Pts',(6.57110895151814,2.44502632087636,39.8869210003223));
#151087=CARTESIAN_POINT('Ctrl Pts',(6.50449838733148,2.62404495591329,39.895592809261));
#151088=CARTESIAN_POINT('Ctrl Pts',(6.43056821795872,2.80033990715965,39.9042646181998));
#151089=CARTESIAN_POINT('Ctrl Pts',(6.34956511459257,2.97332295892139,39.9129364271386));
#151090=CARTESIAN_POINT('Ctrl Pts',(6.26856213015487,3.14630575671006,39.9216082233454));
#151091=CARTESIAN_POINT('Ctrl Pts',(6.18048635294215,3.31597640754793,39.9302800195523));
#151092=CARTESIAN_POINT('Ctrl Pts',(6.08563165071456,3.48176879966508,39.9389518157591));
#151093=CARTESIAN_POINT('Ctrl Pts',(5.99077708581872,3.64756095174606,39.9476235994108));
#151094=CARTESIAN_POINT('Ctrl Pts',(5.88914375658023,3.80947460983865,39.9562953830625));
#151095=CARTESIAN_POINT('Ctrl Pts',(5.78107076500159,3.96696954519996,39.9649671667143));
#151096=CARTESIAN_POINT('Ctrl Pts',(5.67299792768795,4.12446425575064,39.9736389379878));
#151097=CARTESIAN_POINT('Ctrl Pts',(5.55848560711295,4.27754002202605,39.9823107092612));
#151098=CARTESIAN_POINT('Ctrl Pts',(5.43791587524807,4.42568610457464,39.9909824805347));
#151099=CARTESIAN_POINT('Ctrl Pts',(5.31734631302823,4.57383197867747,39.9996542396068));
#151100=CARTESIAN_POINT('Ctrl Pts',(5.19071953583763,4.71704796266914,40.0083259986788));
#151101=CARTESIAN_POINT('Ctrl Pts',(5.05845803451528,4.85485621574396,40.0169977577509));
#151102=CARTESIAN_POINT('Ctrl Pts',(4.9261967165914,4.99266427772899,40.0256695047984));
#151103=CARTESIAN_POINT('Ctrl Pts',(4.78830088681711,5.12506441890963,40.0343412518459));
#151104=CARTESIAN_POINT('Ctrl Pts',(4.6452306340038,5.25161488681459,40.0430129988934));
#151105=CARTESIAN_POINT('Ctrl Pts',(4.49652806262312,5.38314733060955,40.0520261309664));
#151106=CARTESIAN_POINT('Ctrl Pts',(4.34223563523881,5.50835996364327,40.0610392630394));
#151107=CARTESIAN_POINT('Ctrl Pts',(4.1829094334448,5.6268015101031,40.0700523951124));
#151108=CARTESIAN_POINT('Ctrl Pts',(4.0260727035538,5.7433924073995,40.0789246969968));
#151109=CARTESIAN_POINT('Ctrl Pts',(3.86435862820325,5.85342208902676,40.0877969988811));
#151110=CARTESIAN_POINT('Ctrl Pts',(3.69833198496388,5.95650628233473,40.0966693007655));
#151111=CARTESIAN_POINT('Ctrl Pts',(3.53489950802516,6.05797978512224,40.1054029729329));
#151112=CARTESIAN_POINT('Ctrl Pts',(3.36728850947017,6.15272311279945,40.1141366451003));
#151113=CARTESIAN_POINT('Ctrl Pts',(3.19606623000903,6.24041562845744,40.1228703172678));
#151114=CARTESIAN_POINT('Ctrl Pts',(3.02603797481029,6.32749661743996,40.1315430848817));
#151115=CARTESIAN_POINT('Ctrl Pts',(2.85244891335269,6.40762471321637,40.1402158524957));
#151116=CARTESIAN_POINT('Ctrl Pts',(2.67587836095063,6.48053250588994,40.1488886201097));
#151117=CARTESIAN_POINT('Ctrl Pts',(2.49930871513362,6.55343992422525,40.1575613431942));
#151118=CARTESIAN_POINT('Ctrl Pts',(2.31975787164879,6.61912700519455,40.1662340662787));
#151119=CARTESIAN_POINT('Ctrl Pts',(2.13782503579984,6.6773745348608,40.1749067893631));
#151120=CARTESIAN_POINT('Ctrl Pts',(1.95589311921716,6.73562177021519,40.1835794686263));
#151121=CARTESIAN_POINT('Ctrl Pts',(1.77157950496912,6.78642944284926,40.1922521478894));
#151122=CARTESIAN_POINT('Ctrl Pts',(1.58549928668659,6.82962799678111,40.2009248271525));
#151123=CARTESIAN_POINT('Ctrl Pts',(1.39941999343734,6.87282633596633,40.2095974633024));
#151124=CARTESIAN_POINT('Ctrl Pts',(1.211574390505,6.90841556788942,40.2182700994524));
#151125=CARTESIAN_POINT('Ctrl Pts',(1.02258935228956,6.93627692491325,40.2269427356023));
#151126=CARTESIAN_POINT('Ctrl Pts',(0.833605238122552,6.96413814570808,
40.235615329347));
#151127=CARTESIAN_POINT('Ctrl Pts',(0.643481980913932,6.98427152577638,
40.2442879230918));
#151128=CARTESIAN_POINT('Ctrl Pts',(0.452854049805355,6.99660987708154,
40.2529605168366));
#151129=CARTESIAN_POINT('Ctrl Pts',(0.262227035219116,7.00894816906498,
40.2616330688843));
#151130=CARTESIAN_POINT('Ctrl Pts',(0.0710956351193099,7.0134914889309,
40.270305620932));
#151131=CARTESIAN_POINT('Ctrl Pts',(-0.119902323159135,7.01022467510144,
40.2789781729797));
#151132=CARTESIAN_POINT('Ctrl Pts',(-0.310899378724558,7.00695787671191,
40.2876506840384));
#151133=CARTESIAN_POINT('Ctrl Pts',(-0.50176270965486,6.99588102335268,
40.296323195097));
#151134=CARTESIAN_POINT('Ctrl Pts',(-0.691855389207205,6.97703107940082,
40.3049957061557));
#151135=CARTESIAN_POINT('Ctrl Pts',(-0.881947185839328,6.95818122300097,
40.3136681769333));
#151136=CARTESIAN_POINT('Ctrl Pts',(-1.07126805553219,6.93155837629096,
40.3223406477109));
#151137=CARTESIAN_POINT('Ctrl Pts',(-1.25918622472681,6.89725138109075,
40.3310131184885));
#151138=CARTESIAN_POINT('Ctrl Pts',(-1.44710353643705,6.86294454243587,
40.3396855496929));
#151139=CARTESIAN_POINT('Ctrl Pts',(-1.63361788097252,6.82095367647998,
40.3483579808974));
#151140=CARTESIAN_POINT('Ctrl Pts',(-1.81810685596866,6.77141890764261,
40.3570304121019));
#151141=CARTESIAN_POINT('Ctrl Pts',(-2.00259500418376,6.7218843607936,40.3657028044411));
#151142=CARTESIAN_POINT('Ctrl Pts',(-2.18505752664302,6.66480605238623,
40.3743751967804));
#151143=CARTESIAN_POINT('Ctrl Pts',(-2.3648855474509,6.60037445225329,40.3830475891197));
#151144=CARTESIAN_POINT('Ctrl Pts',(-2.54471277704058,6.5359431356104,40.3917199433016));
#151145=CARTESIAN_POINT('Ctrl Pts',(-2.72190526073146,6.46415868780839,
40.4003922974836));
#151146=CARTESIAN_POINT('Ctrl Pts',(-2.89587171390079,6.38526065083715,
40.4090646516655));
#151147=CARTESIAN_POINT('Ctrl Pts',(-3.06983741583811,6.30636295456799,
40.417736968398));
#151148=CARTESIAN_POINT('Ctrl Pts',(-3.24057685640974,6.22035184793663,
40.4264092851305));
#151149=CARTESIAN_POINT('Ctrl Pts',(-3.40752028946972,6.12751434427959,
40.435081601863));
#151150=CARTESIAN_POINT('Ctrl Pts',(-3.5744630152474,6.03467723394335,40.4437538818538));
#151151=CARTESIAN_POINT('Ctrl Pts',(-3.73760951742357,5.93501392252036,
40.4524261618447));
#151152=CARTESIAN_POINT('Ctrl Pts',(-3.89641539159049,5.82885697703047,
40.4610984418355));
#151153=CARTESIAN_POINT('Ctrl Pts',(-4.0552206059092,5.72270047262924,40.4697706857925));
#151154=CARTESIAN_POINT('Ctrl Pts',(-4.20968499214318,5.61005054602416,
40.4784429297495));
#151155=CARTESIAN_POINT('Ctrl Pts',(-4.35929312156135,5.49128309621785,
40.4871151737065));
#151156=CARTESIAN_POINT('Ctrl Pts',(-4.50890064155582,5.37251613020677,
40.4957873823374));
#151157=CARTESIAN_POINT('Ctrl Pts',(-4.65365172183535,5.24763186748207,
40.5044595909682));
#151158=CARTESIAN_POINT('Ctrl Pts',(-4.79306334971184,5.11704702813538,
40.5131317995991));
#151159=CARTESIAN_POINT('Ctrl Pts',(-4.93247442107444,4.98646271006714,
40.5218039736116));
#151160=CARTESIAN_POINT('Ctrl Pts',(-5.06654587536853,4.8501780551058,40.5304761476241));
#151161=CARTESIAN_POINT('Ctrl Pts',(-5.19483033978756,4.70864782111836,
40.5391483216367));
#151162=CARTESIAN_POINT('Ctrl Pts',(-5.32311430257757,4.56711814055468,
40.5478204617385));
#151163=CARTESIAN_POINT('Ctrl Pts',(-5.44561113000732,4.42034313247626,
40.5564926018403));
#151164=CARTESIAN_POINT('Ctrl Pts',(-5.56191207495295,4.26881255538265,
40.5651647419421));
#151165=CARTESIAN_POINT('Ctrl Pts',(-5.67821257461744,4.11728255845381,
40.573836848841));
#151166=CARTESIAN_POINT('Ctrl Pts',(-5.78831706632354,3.96099725427816,
40.5825089557398));
#151167=CARTESIAN_POINT('Ctrl Pts',(-5.89185815647442,3.80047813129952,
40.5911810626386));
#151168=CARTESIAN_POINT('Ctrl Pts',(-5.99539885864498,3.6399596098044,40.5998531370421));
#151169=CARTESIAN_POINT('Ctrl Pts',(-6.09237605450714,3.4752075399488,40.6085252114455));
#151170=CARTESIAN_POINT('Ctrl Pts',(-6.18246615568129,3.30677165772833,
40.6171972858489));
#151171=CARTESIAN_POINT('Ctrl Pts',(-6.27255592662742,3.13833639291476,
40.6258693284646));
#151172=CARTESIAN_POINT('Ctrl Pts',(-6.35575851943906,2.96621759322201,
40.6345413710803));
#151173=CARTESIAN_POINT('Ctrl Pts',(-6.43179631013703,2.79098957135417,
40.643213413696));
#151174=CARTESIAN_POINT('Ctrl Pts',(-6.50783382831937,2.61576217749477,
40.6518854252315));
#151175=CARTESIAN_POINT('Ctrl Pts',(-6.57670648270635,2.43742584431986,
40.6605574367671));
#151176=CARTESIAN_POINT('Ctrl Pts',(-6.63818446599503,2.25657562645756,
40.6692294483026));
#151177=CARTESIAN_POINT('Ctrl Pts',(-6.69966223396491,2.07572604200009,
40.6779014294655));
#151178=CARTESIAN_POINT('Ctrl Pts',(-6.75374529124769,1.89236285939106,
40.6865734106284));
#151179=CARTESIAN_POINT('Ctrl Pts',(-6.80025318023408,1.70709790205962,
40.6952453917913));
#151180=CARTESIAN_POINT('Ctrl Pts',(-6.8467609101265,1.52183357848165,40.7039173432892));
#151181=CARTESIAN_POINT('Ctrl Pts',(-6.88569345442305,1.33466776867736,
40.712589294787));
#151182=CARTESIAN_POINT('Ctrl Pts',(-6.91692090874696,1.14622497994031,
40.7212612462849));
#151183=CARTESIAN_POINT('Ctrl Pts',(-6.94814825879545,0.957782820455669,
40.7299331688251));
#151184=CARTESIAN_POINT('Ctrl Pts',(-6.97167052392514,0.76806397077045,
40.7386050913654));
#151185=CARTESIAN_POINT('Ctrl Pts',(-6.98740921903159,0.577701452562083,
40.7472770139056));
#151186=CARTESIAN_POINT('Ctrl Pts',(-7.00314786286689,0.387339554488134,
40.7559489081958));
#151187=CARTESIAN_POINT('Ctrl Pts',(-7.01110296401747,0.196334275137052,
40.764620802486));
#151188=CARTESIAN_POINT('Ctrl Pts',(-7.01124797942393,0.00532292437845766,
40.7732926967762));
#151189=CARTESIAN_POINT('Ctrl Pts',(-7.0113929943698,-0.185687819713,40.7819645635237));
#151190=CARTESIAN_POINT('Ctrl Pts',(-7.00372797299432,-0.376704351162253,
40.7906364302713));
#151191=CARTESIAN_POINT('Ctrl Pts',(-6.9882784903119,-0.567089326600318,
40.7993082970188));
#151192=CARTESIAN_POINT('Ctrl Pts',(-6.97282905543812,-0.757473712889477,
40.8079801369312));
#151193=CARTESIAN_POINT('Ctrl Pts',(-6.94959523043359,-0.947226264002061,
40.8166519768435));
#151194=CARTESIAN_POINT('Ctrl Pts',(-6.91865453650885,-1.13571385786456,
40.8253238167559));
#151195=CARTESIAN_POINT('Ctrl Pts',(-6.88771393580673,-1.32420088382415,
40.8339956305404));
#151196=CARTESIAN_POINT('Ctrl Pts',(-6.84906655865489,-1.51142267990864,
40.842667444325));
#151197=CARTESIAN_POINT('Ctrl Pts',(-6.80284135383486,-1.69675457183835,
40.8513392581096));
#151198=CARTESIAN_POINT('Ctrl Pts',(-6.75661628451863,-1.88208592048921,
40.8600110464737));
#151199=CARTESIAN_POINT('Ctrl Pts',(-6.70281350071476,-2.06552710051504,
40.8686828348379));
#151200=CARTESIAN_POINT('Ctrl Pts',(-6.64161251687655,-2.24646605542323,
40.877354623202));
#151201=CARTESIAN_POINT('Ctrl Pts',(-6.58041170744998,-2.4274044946884,
40.8860263868531));
#151202=CARTESIAN_POINT('Ctrl Pts',(-6.51181283117372,-2.60584045408377,
40.8946981505043));
#151203=CARTESIAN_POINT('Ctrl Pts',(-6.4360447687633,-2.78117858056159,
40.9033699141554));
#151204=CARTESIAN_POINT('Ctrl Pts',(-6.35684774728359,-2.96445180845089,
40.9124341271008));
#151205=CARTESIAN_POINT('Ctrl Pts',(-6.26981768815781,-3.14433998862013,
40.9214983400461));
#151206=CARTESIAN_POINT('Ctrl Pts',(-6.17527181578228,-3.32018742900233,
40.9305625529915));
#151207=CARTESIAN_POINT('Ctrl Pts',(-6.08368050191848,-3.49053963687257,
40.9393435092823));
#151208=CARTESIAN_POINT('Ctrl Pts',(-5.98503618716738,-3.65709956718416,
40.9481244655732));
#151209=CARTESIAN_POINT('Ctrl Pts',(-5.87967633130231,-3.81929742251417,
40.956905421864));
#151210=CARTESIAN_POINT('Ctrl Pts',(-5.77561495477829,-3.97949631379304,
40.9655781596095));
#151211=CARTESIAN_POINT('Ctrl Pts',(-5.6650027940536,-4.13543980257433,
40.9742508973549));
#151212=CARTESIAN_POINT('Ctrl Pts',(-5.54820899034715,-4.28660746534262,
40.9829236351004));
#151213=CARTESIAN_POINT('Ctrl Pts',(-5.431416363685,-4.43777360464794,40.9915962854423));
#151214=CARTESIAN_POINT('Ctrl Pts',(-5.30844239242835,-4.5841637894042,
41.0002689357843));
#151215=CARTESIAN_POINT('Ctrl Pts',(-5.17969746407253,-4.72528948776481,
41.0089415861262));
#151216=CARTESIAN_POINT('Ctrl Pts',(-5.05095379116967,-4.86641380994168,
41.0176141518969));
#151217=CARTESIAN_POINT('Ctrl Pts',(-4.91643946527104,-5.00227353854703,
41.0262867176677));
#151218=CARTESIAN_POINT('Ctrl Pts',(-4.77660337748089,-5.13241529269974,
41.0349592834385));
#151219=CARTESIAN_POINT('Ctrl Pts',(-4.63676860764683,-5.26255582026552,
41.0436317674703));
#151220=CARTESIAN_POINT('Ctrl Pts',(-4.49161238427127,-5.38697828766097,
41.0523042515021));
#151221=CARTESIAN_POINT('Ctrl Pts',(-4.34161910267748,-5.50526748939286,
41.0609767355338));
#151222=CARTESIAN_POINT('Ctrl Pts',(-4.19162718580667,-5.62355561486328,
41.0696491406585));
#151223=CARTESIAN_POINT('Ctrl Pts',(-4.03679852186487,-5.7357104104133,
41.0783215457832));
#151224=CARTESIAN_POINT('Ctrl Pts',(-3.87764977431715,-5.84135761533551,
41.0869939509078));
#151225=CARTESIAN_POINT('Ctrl Pts',(-3.71850242284401,-5.947003893506,41.095666279957));
#151226=CARTESIAN_POINT('Ctrl Pts',(-3.5550353002858,-6.04614253816382,
41.1043386090061));
#151227=CARTESIAN_POINT('Ctrl Pts',(-3.3877938870953,-6.13844272931334,
41.1130109380552));
#151228=CARTESIAN_POINT('Ctrl Pts',(-3.22055388638152,-6.23074214091986,
41.1216831938602));
#151229=CARTESIAN_POINT('Ctrl Pts',(-3.04953990753726,-6.31620307732892,
41.1303554496651));
#151230=CARTESIAN_POINT('Ctrl Pts',(-2.87532260481408,-6.39454036508843,
41.13902770547));
#151231=CARTESIAN_POINT('Ctrl Pts',(-2.70110671662252,-6.47287701679991,
41.1476998908619));
#151232=CARTESIAN_POINT('Ctrl Pts',(-2.52368781567764,-6.54409001910884,
41.1563720762537));
#151233=CARTESIAN_POINT('Ctrl Pts',(-2.34365791912555,-6.60794174615819,
41.1650442616456));
#151234=CARTESIAN_POINT('Ctrl Pts',(-2.16362942554456,-6.67179297561169,
41.1737163794552));
#151235=CARTESIAN_POINT('Ctrl Pts',(-1.98099024478836,-6.72828294965046,
41.1823884972648));
#151236=CARTESIAN_POINT('Ctrl Pts',(-1.79634980371301,-6.77722317363094,
41.1910606150743));
#151237=CARTESIAN_POINT('Ctrl Pts',(-1.61171074128267,-6.82616303219204,
41.1997326681323));
#151238=CARTESIAN_POINT('Ctrl Pts',(-1.4250707229976,-6.86755318072501,
41.2084047211902));
#151239=CARTESIAN_POINT('Ctrl Pts',(-1.23705251633973,-6.9012555114499,
41.2170767742482));
#151240=CARTESIAN_POINT('Ctrl Pts',(-1.04903565219232,-6.9349576015293,
41.2257487653849));
#151241=CARTESIAN_POINT('Ctrl Pts',(-0.859640898941661,-6.96097193353387,
41.2344207565216));
#151242=CARTESIAN_POINT('Ctrl Pts',(-0.669500206862725,-6.97921170588132,
41.2430927476583));
#151243=CARTESIAN_POINT('Ctrl Pts',(-0.479360810405145,-6.99745135394269,
41.2517646797039));
#151244=CARTESIAN_POINT('Ctrl Pts',(-0.288475768016168,-7.00791652123612,
41.2604366117495));
#151245=CARTESIAN_POINT('Ctrl Pts',(-0.0974819939220911,-7.01057228929001,
41.2691085437952));
#151246=CARTESIAN_POINT('Ctrl Pts',(0.0935105410571396,-7.01322804011401,
41.2777804195797));
#151247=CARTESIAN_POINT('Ctrl Pts',(0.284611522343203,-7.00807448913607,
41.2864522953642));
#151248=CARTESIAN_POINT('Ctrl Pts',(0.475183323465225,-6.99512883166569,
41.2951241711488));
#151249=CARTESIAN_POINT('Ctrl Pts',(0.665753950389368,-6.98218325395928,
41.303795993502));
#151250=CARTESIAN_POINT('Ctrl Pts',(0.855795120321911,-6.96144568508307,
41.3124678158552));
#151251=CARTESIAN_POINT('Ctrl Pts',(1.04467275075863,-6.93298531704218,
41.3211396382085));
#151252=CARTESIAN_POINT('Ctrl Pts',(1.23354927905906,-6.90452511507286,
41.32981140996));
#151253=CARTESIAN_POINT('Ctrl Pts',(1.42126200062351,-6.868342246432,41.3384831817115));
#151254=CARTESIAN_POINT('Ctrl Pts',(1.60718460924195,-6.82455743578408,
41.3471549534631));
#151255=CARTESIAN_POINT('Ctrl Pts',(1.79763389405345,-6.77970659200845,
41.3560378577016));
#151256=CARTESIAN_POINT('Ctrl Pts',(1.9862044843137,-6.72687898191017,41.36492076194));
#151257=CARTESIAN_POINT('Ctrl Pts',(2.17223623427354,-6.66625954377784,
41.3738036661785));
#151258=CARTESIAN_POINT('Ctrl Pts',(2.35386532185533,-6.60707473666791,
41.3824763459349));
#151259=CARTESIAN_POINT('Ctrl Pts',(2.53307410227177,-6.54046283696716,
41.3911490256912));
#151260=CARTESIAN_POINT('Ctrl Pts',(2.70926451773746,-6.46664614274114,
41.3998217054475));
#151261=CARTESIAN_POINT('Ctrl Pts',(2.88545151535656,-6.3928308804553,41.4084942169661));
#151262=CARTESIAN_POINT('Ctrl Pts',(3.05862000313874,-6.31181121311276,
41.4171667284846));
#151263=CARTESIAN_POINT('Ctrl Pts',(3.22819210343704,-6.22385751008221,
41.4258392400031));
#151264=CARTESIAN_POINT('Ctrl Pts',(3.39776113570586,-6.13590539837803,
41.4345115946119));
#151265=CARTESIAN_POINT('Ctrl Pts',(3.56373365850705,-6.04101963284194,
41.4431839492206));
#151266=CARTESIAN_POINT('Ctrl Pts',(3.72555582774893,-5.93951684371936,
41.4518563038294));
#151267=CARTESIAN_POINT('Ctrl Pts',(3.88737528046132,-5.83801575853711,
41.4605285128542));
#151268=CARTESIAN_POINT('Ctrl Pts',(4.04504427838579,-5.72989802299899,
41.469200721879));
#151269=CARTESIAN_POINT('Ctrl Pts',(4.19803670362892,-5.61552440983782,
41.4778729309039));
#151270=CARTESIAN_POINT('Ctrl Pts',(4.35102676029745,-5.50115256736847,
41.4865450056686));
#151271=CARTESIAN_POINT('Ctrl Pts',(4.49934016166134,-5.38052521116207,
41.4952170804334));
#151272=CARTESIAN_POINT('Ctrl Pts',(4.64248202336361,-5.25404484423627,
41.5038891551981));
#151273=CARTESIAN_POINT('Ctrl Pts',(4.78562185584173,-5.12756627033602,
41.5125611070248));
#151274=CARTESIAN_POINT('Ctrl Pts',(4.92359008252101,-4.9952350398253,41.5212330588515));
#151275=CARTESIAN_POINT('Ctrl Pts',(5.05592635131864,-4.85749269608733,
41.5299050106782));
#151276=CARTESIAN_POINT('Ctrl Pts',(5.18826091679979,-4.7197521252481,41.5385768508871));
#151277=CARTESIAN_POINT('Ctrl Pts',(5.31496347269136,-4.57660078535727,
41.547248691096));
#151278=CARTESIAN_POINT('Ctrl Pts',(5.43561126741548,-4.42851631046402,
41.555920531305));
#151279=CARTESIAN_POINT('Ctrl Pts',(5.56176013705297,-4.27367975368019,
41.5649877740385));
#151280=CARTESIAN_POINT('Ctrl Pts',(5.68128895686261,-4.11344992041455,
41.5740550167721));
#151281=CARTESIAN_POINT('Ctrl Pts',(5.79376175353782,-3.94841123817446,
41.5831222595057));
#151282=CARTESIAN_POINT('Ctrl Pts',(5.901338742361,-3.79055649463141,41.5917948158841));
#151283=CARTESIAN_POINT('Ctrl Pts',(6.00246078173993,-3.62830291662058,
41.6004673722625));
#151284=CARTESIAN_POINT('Ctrl Pts',(6.09679041553083,-3.4621919634231,41.6091399286409));
#151285=CARTESIAN_POINT('Ctrl Pts',(6.19111669178522,-3.29608692272168,
41.6178121763314));
#151286=CARTESIAN_POINT('Ctrl Pts',(6.2786509059609,-3.12612502861207,41.6264844240218));
#151287=CARTESIAN_POINT('Ctrl Pts',(6.35910096685908,-2.9528734235981,41.6351566717123));
#151288=CARTESIAN_POINT('Ctrl Pts',(6.43954858436857,-2.77962708049451,
41.6438286560136));
#151289=CARTESIAN_POINT('Ctrl Pts',(6.51291235951801,-2.60309148404341,
41.6525006403149));
#151290=CARTESIAN_POINT('Ctrl Pts',(6.5789475010232,-2.42385567666076,41.6611726246162));
#151291=CARTESIAN_POINT('Ctrl Pts',(6.64498098171,-2.24462437715255,41.6698443908126));
#151292=CARTESIAN_POINT('Ctrl Pts',(6.70368609940776,-2.06269326910285,
41.6785161570089));
#151293=CARTESIAN_POINT('Ctrl Pts',(6.75486698389305,-1.87866936750765,
41.6871879232053));
#151294=CARTESIAN_POINT('Ctrl Pts',(6.80605126222429,-1.69463326313834,
41.6958602644335));
#151295=CARTESIAN_POINT('Ctrl Pts',(6.84971023276557,-1.50850436118244,
41.7045326056617));
#151296=CARTESIAN_POINT('Ctrl Pts',(6.88569820761666,-1.32090376489917,
41.7132049468899));
#151297=CARTESIAN_POINT('Ctrl Pts',(6.92168406448176,-1.13331420939924,
41.7218767777283));
#151298=CARTESIAN_POINT('Ctrl Pts',(6.94999977553745,-0.944253411832044,
41.7305486085667));
#151299=CARTESIAN_POINT('Ctrl Pts',(6.97055086371812,-0.754352184870321,
41.739220439405));
#151300=CARTESIAN_POINT('Ctrl Pts',(6.99110229107982,-0.564447823724469,
41.7478924133658));
#151301=CARTESIAN_POINT('Ctrl Pts',(7.00388880856466,-0.373703287798768,
41.7565643873265));
#151302=CARTESIAN_POINT('Ctrl Pts',(7.00886775178448,-0.182755028646632,
41.7652363612872));
#151303=CARTESIAN_POINT('Ctrl Pts',(7.0104558273189,-0.121850486194127,
41.7680023598283));
#151304=CARTESIAN_POINT('Ctrl Pts',(7.01125000000004,-0.0609252433295258,
41.7707683583694));
#151305=CARTESIAN_POINT('Ctrl Pts',(7.01125,4.02193902006209E-12,41.7735343569105));
#151306=CARTESIAN_POINT('Ctrl Pts',(7.01124998181045,0.000505037549962183,
41.7735343569106));
#151307=CARTESIAN_POINT('Ctrl Pts',(7.01123724491749,0.17732662351218,41.7815445908137));
#151308=CARTESIAN_POINT('Ctrl Pts',(7.00453108467992,0.3541638119717,41.7895548247167));
#151309=CARTESIAN_POINT('Ctrl Pts',(6.99115392043893,0.530465289374704,
41.7975650586198));
#151310=CARTESIAN_POINT('Ctrl Pts',(6.97777149522567,0.70683610263744,41.8055784427883));
#151311=CARTESIAN_POINT('Ctrl Pts',(6.9577128515498,0.882670416907103,41.8135918269568));
#151312=CARTESIAN_POINT('Ctrl Pts',(6.93105236682085,1.05742122679996,41.8216052111253));
#151313=CARTESIAN_POINT('Ctrl Pts',(6.90438587959873,1.23221138108406,41.8296203994727));
#151314=CARTESIAN_POINT('Ctrl Pts',(6.87111465517143,1.40591718309873,41.8376355878201));
#151315=CARTESIAN_POINT('Ctrl Pts',(6.83136423289208,1.5780016730228,41.8456507761675));
#151316=CARTESIAN_POINT('Ctrl Pts',(6.79158278076775,1.75022049498012,41.8536722213051));
#151317=CARTESIAN_POINT('Ctrl Pts',(6.74531212447262,1.92081512213539,41.8616936664427));
#151318=CARTESIAN_POINT('Ctrl Pts',(6.69272786248699,2.08926310482675,41.8697151115803));
#151319=CARTESIAN_POINT('Ctrl Pts',(6.67088204297652,2.15924381935659,41.8730475733488));
#151320=CARTESIAN_POINT('Ctrl Pts',(6.64794711637243,2.2288542540769,41.8763800351172));
#151321=CARTESIAN_POINT('Ctrl Pts',(6.62393811560608,2.29805796339452,41.8797124968857));
#151322=CARTESIAN_POINT('Ctrl Pts',(6.60687208473663,2.3472492084192,41.8820812708286));
#151323=CARTESIAN_POINT('Ctrl Pts',(6.58926087510141,2.39624227854239,41.8844500447716));
#151324=CARTESIAN_POINT('Ctrl Pts',(6.57110895151814,2.44502632087636,41.8868188187145));
#151325=CARTESIAN_POINT('',(7.01124831048998,0.00486735569483713,41.2264656430603));
#151326=CARTESIAN_POINT('Ctrl Pts',(6.57110895151812,2.44502632087641,41.3399811574536));
#151327=CARTESIAN_POINT('Ctrl Pts',(6.63540837522956,2.27221897106586,41.3316044138032));
#151328=CARTESIAN_POINT('Ctrl Pts',(6.69285885618379,2.09694930863153,41.3232276701529));
#151329=CARTESIAN_POINT('Ctrl Pts',(6.74329558569568,1.91978936512241,41.3148509265025));
#151330=CARTESIAN_POINT('Ctrl Pts',(6.79375827707833,1.74253823006299,41.3064698709957));
#151331=CARTESIAN_POINT('Ctrl Pts',(6.83719993386948,1.56339519127442,41.2980888154889));
#151332=CARTESIAN_POINT('Ctrl Pts',(6.87350661199057,1.38294375063556,41.2897077599821));
#151333=CARTESIAN_POINT('Ctrl Pts',(6.90985313126439,1.20229429151141,41.2813175075196));
#151334=CARTESIAN_POINT('Ctrl Pts',(6.93904897149081,1.02033388554537,41.272927255057));
#151335=CARTESIAN_POINT('Ctrl Pts',(6.96103174076659,0.837653667418768,
41.2645370025945));
#151336=CARTESIAN_POINT('Ctrl Pts',(6.97063507313572,0.757848487737961,
41.2608716598869));
#151337=CARTESIAN_POINT('Ctrl Pts',(6.97886250284089,0.677905979988461,
41.2572063171792));
#151338=CARTESIAN_POINT('Ctrl Pts',(6.98571194797921,0.597875524135656,
41.2535409744716));
#151339=CARTESIAN_POINT('Ctrl Pts',(7.00257721922344,0.400817905817786,
41.2445158640109));
#151340=CARTESIAN_POINT('Ctrl Pts',(7.01111079365624,0.202955311596569,
41.2354907535503));
#151341=CARTESIAN_POINT('Ctrl Pts',(7.01124831048953,0.00486735634087431,
41.2264656430897));
#151342=CARTESIAN_POINT('Ctrl Pts',(7.01124831048998,0.00486735569473905,
41.2264656430603));
#151343=CARTESIAN_POINT('Ctrl Pts',(7.01137214962453,-0.173518399805182,
41.2183381870224));
#151344=CARTESIAN_POINT('Ctrl Pts',(7.00468390246701,-0.3521518018721,41.2102107309844));
#151345=CARTESIAN_POINT('Ctrl Pts',(6.99115346725259,-0.530471262013475,
41.2020832749465));
#151346=CARTESIAN_POINT('Ctrl Pts',(6.97763733581708,-0.708602210691984,
41.1939644108964));
#151347=CARTESIAN_POINT('Ctrl Pts',(6.9572934459719,-0.886419525895315,
41.1858455468463));
#151348=CARTESIAN_POINT('Ctrl Pts',(6.93014369785625,-1.0633601880658,41.1777266827962));
#151349=CARTESIAN_POINT('Ctrl Pts',(6.90302301034407,-1.24011145612475,
41.1696165090326));
#151350=CARTESIAN_POINT('Ctrl Pts',(6.86911103699095,-1.41598759104888,
41.161506335269));
#151351=CARTESIAN_POINT('Ctrl Pts',(6.8284815706003,-1.5904295025156,41.1533961615053));
#151352=CARTESIAN_POINT('Ctrl Pts',(6.78787723653177,-1.76476350879184,
41.1452910044825));
#151353=CARTESIAN_POINT('Ctrl Pts',(6.74056376343523,-1.93766471239729,
41.1371858474596));
#151354=CARTESIAN_POINT('Ctrl Pts',(6.6866663154689,-2.10858249733642,41.1290806904367));
#151355=CARTESIAN_POINT('Ctrl Pts',(6.63279534084035,-2.27941633091193,
41.1209795145032));
#151356=CARTESIAN_POINT('Ctrl Pts',(6.57234694147109,-2.44826834774683,
41.1128783385697));
#151357=CARTESIAN_POINT('Ctrl Pts',(6.50549659757984,-2.61460141921807,
41.1047771626363));
#151358=CARTESIAN_POINT('Ctrl Pts',(6.47825517631646,-2.68238191227508,
41.1014759448192));
#151359=CARTESIAN_POINT('Ctrl Pts',(6.44995125512438,-2.74974429710525,
41.0981747270021));
#151360=CARTESIAN_POINT('Ctrl Pts',(6.42059905730838,-2.81665303290817,
41.094873509185));
#151361=CARTESIAN_POINT('Ctrl Pts',(6.34646043726233,-2.9856530298607,41.0865351988832));
#151362=CARTESIAN_POINT('Ctrl Pts',(6.26567581471887,-3.15165466081349,
41.0781968885814));
#151363=CARTESIAN_POINT('Ctrl Pts',(6.17852427623076,-3.31413100684436,
41.0698585782795));
#151364=CARTESIAN_POINT('Ctrl Pts',(6.0913179049518,-3.47670957747911,41.0615150217958));
#151365=CARTESIAN_POINT('Ctrl Pts',(5.99773678244351,-3.63575815040036,
41.053171465312));
#151366=CARTESIAN_POINT('Ctrl Pts',(5.89810470852122,-3.79077662357199,
41.0448279088283));
#151367=CARTESIAN_POINT('Ctrl Pts',(5.79839683495163,-3.94591303412189,
41.0364780046032));
#151368=CARTESIAN_POINT('Ctrl Pts',(5.69262900436411,-4.09701295376923,
41.0281281003781));
#151369=CARTESIAN_POINT('Ctrl Pts',(5.58116711335151,-4.24360698172482,
41.0197781961529));
#151370=CARTESIAN_POINT('Ctrl Pts',(5.46953803775052,-4.39042088987445,
41.0114157676894));
#151371=CARTESIAN_POINT('Ctrl Pts',(5.35219803326611,-4.53271513966923,
41.0030533392258));
#151372=CARTESIAN_POINT('Ctrl Pts',(5.22955288163524,-4.6700538777064,40.9946909107622));
#151373=CARTESIAN_POINT('Ctrl Pts',(5.10680285168081,-4.80751005908653,
40.9863213312823));
#151374=CARTESIAN_POINT('Ctrl Pts',(4.97873885001386,-4.94000203849765,
40.9779517518025));
#151375=CARTESIAN_POINT('Ctrl Pts',(4.84580237287659,-5.06713192304321,
40.9695821723226));
#151376=CARTESIAN_POINT('Ctrl Pts',(4.71266085741989,-5.19445788994659,
40.9611996837861));
#151377=CARTESIAN_POINT('Ctrl Pts',(4.57463209395228,-5.31640501878586,
40.9528171952496));
#151378=CARTESIAN_POINT('Ctrl Pts',(4.4321904714524,-5.43261577762192,40.9444347067131));
#151379=CARTESIAN_POINT('Ctrl Pts',(4.38558123851817,-5.4706418421457,40.9416918191083));
#151380=CARTESIAN_POINT('Ctrl Pts',(4.33849974626909,-5.50805405801666,
40.9389489315035));
#151381=CARTESIAN_POINT('Ctrl Pts',(4.29096325386699,-5.54484092796748,
40.9362060438987));
#151382=CARTESIAN_POINT('Ctrl Pts',(4.14556018154508,-5.65736340578749,
40.9278161887659));
#151383=CARTESIAN_POINT('Ctrl Pts',(3.99560443078829,-5.7642590311646,40.9194263336331));
#151384=CARTESIAN_POINT('Ctrl Pts',(3.84155841605414,-5.86515605065574,
40.9110364785003));
#151385=CARTESIAN_POINT('Ctrl Pts',(3.68765455282264,-5.96595996379188,
40.9026543654082));
#151386=CARTESIAN_POINT('Ctrl Pts',(3.52966822361529,-6.0607761266698,40.894272252316));
#151387=CARTESIAN_POINT('Ctrl Pts',(3.36809309514428,-6.14927438523778,
40.8858901392239));
#151388=CARTESIAN_POINT('Ctrl Pts',(3.20664331472822,-6.23770398791371,
40.8775145288751));
#151389=CARTESIAN_POINT('Ctrl Pts',(3.04161057306857,-6.31982530073939,
40.8691389185262));
#151390=CARTESIAN_POINT('Ctrl Pts',(2.87351595328109,-6.39535242412325,
40.8607633081773));
#151391=CARTESIAN_POINT('Ctrl Pts',(2.70552706750532,-6.47083203982508,
40.8523929662117));
#151392=CARTESIAN_POINT('Ctrl Pts',(2.53448044288411,-6.5397256021328,40.8440226242461));
#151393=CARTESIAN_POINT('Ctrl Pts',(2.36092051771228,-6.60179376166396,
40.8356522822805));
#151394=CARTESIAN_POINT('Ctrl Pts',(2.18744432237532,-6.66383197789604,
40.8272859783861));
#151395=CARTESIAN_POINT('Ctrl Pts',(2.01145755334718,-6.71905124713815,
40.8189196744918));
#151396=CARTESIAN_POINT('Ctrl Pts',(1.83352375126998,-6.7672606877546,40.8105533705975));
#151397=CARTESIAN_POINT('Ctrl Pts',(1.65563971228979,-6.8154566455418,40.8021894065239));
#151398=CARTESIAN_POINT('Ctrl Pts',(1.47581004260668,-6.85664659655255,
40.7938254424502));
#151399=CARTESIAN_POINT('Ctrl Pts',(1.29461307415031,-6.89068962809522,
40.7854614783766));
#151400=CARTESIAN_POINT('Ctrl Pts',(1.11344398889634,-6.92472742098106,
40.7770988013781));
#151401=CARTESIAN_POINT('Ctrl Pts',(0.930908347286462,-6.95162042649606,
40.7687361243795));
#151402=CARTESIAN_POINT('Ctrl Pts',(0.74759471092878,-6.97127884327484,
40.760373447381));
#151403=CARTESIAN_POINT('Ctrl Pts',(0.564284848663807,-6.99093685532274,
40.7520109425547));
#151404=CARTESIAN_POINT('Ctrl Pts',(0.380197350407759,-7.00336054099146,
40.7436484377284));
#151405=CARTESIAN_POINT('Ctrl Pts',(0.195926373028393,-7.00851192614038,
40.735285932902));
#151406=CARTESIAN_POINT('Ctrl Pts',(0.0116346274421183,-7.01366389187466,
40.7269224855821));
#151407=CARTESIAN_POINT('Ctrl Pts',(-0.172840309972789,-7.01154191435022,
40.7185590382621));
#151408=CARTESIAN_POINT('Ctrl Pts',(-0.356903367504056,-7.00216013447024,
40.7101955909421));
#151409=CARTESIAN_POINT('Ctrl Pts',(-0.541074806536332,-6.99277283033461,
40.7018272189893));
#151410=CARTESIAN_POINT('Ctrl Pts',(-0.724833552436218,-6.97611719761188,
40.6934588470365));
#151411=CARTESIAN_POINT('Ctrl Pts',(-0.907587698239172,-6.95225942643864,
40.6850904750837));
#151412=CARTESIAN_POINT('Ctrl Pts',(-1.09039660196088,-6.92839450685358,
40.6767195957479));
#151413=CARTESIAN_POINT('Ctrl Pts',(-1.27219998011878,-6.89732319371964,
40.6683487164122));
#151414=CARTESIAN_POINT('Ctrl Pts',(-1.45241450265757,-6.85916311768207,
40.6599778370764));
#151415=CARTESIAN_POINT('Ctrl Pts',(-1.63278171901212,-6.82097070902481,
40.6515998651851));
#151416=CARTESIAN_POINT('Ctrl Pts',(-1.81155706909424,-6.77567760934077,
40.6432218932938));
#151417=CARTESIAN_POINT('Ctrl Pts',(-1.98816967393339,-6.72345208283302,
40.6348439214025));
#151418=CARTESIAN_POINT('Ctrl Pts',(-2.10040842246875,-6.6902623354638,
40.6295196520436));
#151419=CARTESIAN_POINT('Ctrl Pts',(-2.21177399737371,-6.65427379297501,
40.6241953826847));
#151420=CARTESIAN_POINT('Ctrl Pts',(-2.32212367178371,-6.61553990354844,
40.6188711133258));
#151421=CARTESIAN_POINT('Ctrl Pts',(-2.48508703881005,-6.55833805793604,
40.6110082821365));
#151422=CARTESIAN_POINT('Ctrl Pts',(-2.64617268895314,-6.49502732338543,
40.6031454509472));
#151423=CARTESIAN_POINT('Ctrl Pts',(-2.8048695116593,-6.42575548749438,
40.5952826197578));
#151424=CARTESIAN_POINT('Ctrl Pts',(-2.96344439680532,-6.35653687786528,
40.5874258301164));
#151425=CARTESIAN_POINT('Ctrl Pts',(-3.11963375749355,-6.28136642706268,
40.5795690404749));
#151426=CARTESIAN_POINT('Ctrl Pts',(-3.27294245944832,-6.20044145360961,
40.5717122508334));
#151427=CARTESIAN_POINT('Ctrl Pts',(-3.42616470255202,-6.119562118011,40.5638598920495));
#151428=CARTESIAN_POINT('Ctrl Pts',(-3.57650918240588,-6.03293489279218,
40.5560075332654));
#151429=CARTESIAN_POINT('Ctrl Pts',(-3.72350178664801,-5.94080474408384,
40.5481551744814));
#151430=CARTESIAN_POINT('Ctrl Pts',(-3.87045968422133,-5.84869634837849,
40.540304669731));
#151431=CARTESIAN_POINT('Ctrl Pts',(-4.01406695407394,-5.75108781031097,
40.5324541649805));
#151432=CARTESIAN_POINT('Ctrl Pts',(-4.15387516093496,-5.6482694438091,
40.52460366023));
#151433=CARTESIAN_POINT('Ctrl Pts',(-4.29366087706154,-5.54546761754209,
40.5167544183783));
#151434=CARTESIAN_POINT('Ctrl Pts',(-4.42964844123719,-5.43745785970932,
40.5089051765267));
#151435=CARTESIAN_POINT('Ctrl Pts',(-4.5614198192569,-5.3245728274661,40.501055934675));
#151436=CARTESIAN_POINT('Ctrl Pts',(-4.69323559363341,-5.21164976204569,
40.4932040482601));
#151437=CARTESIAN_POINT('Ctrl Pts',(-4.82083205446145,-5.09384838970508,
40.4853521618452));
#151438=CARTESIAN_POINT('Ctrl Pts',(-4.94382543929532,-4.97154066545537,
40.4775002754303));
#151439=CARTESIAN_POINT('Ctrl Pts',(-5.03413795090556,-4.8817316258778,
40.4717347329666));
#151440=CARTESIAN_POINT('Ctrl Pts',(-5.12196929038965,-4.78949368930015,
40.4659691905029));
#151441=CARTESIAN_POINT('Ctrl Pts',(-5.2071807138275,-4.69498621681076,
40.4602036480393));
#151442=CARTESIAN_POINT('Ctrl Pts',(-5.34988059565206,-4.5367186440878,
40.4505483436795));
#151443=CARTESIAN_POINT('Ctrl Pts',(-5.48515969510513,-4.3721665230661,
40.4408930393198));
#151444=CARTESIAN_POINT('Ctrl Pts',(-5.6125637345342,-4.20199415614675,
40.4312377349601));
#151445=CARTESIAN_POINT('Ctrl Pts',(-5.74067356843957,-4.03087906624053,
40.4215289420256));
#151446=CARTESIAN_POINT('Ctrl Pts',(-5.86082086345623,-3.85408135829778,
40.4118201490911));
#151447=CARTESIAN_POINT('Ctrl Pts',(-5.97259164393436,-3.67229841071031,
40.4021113561567));
#151448=CARTESIAN_POINT('Ctrl Pts',(-6.08490027489926,-3.4896407081428,
40.3923558436861));
#151449=CARTESIAN_POINT('Ctrl Pts',(-6.18875157813822,-3.30194972112196,
40.3826003312156));
#151450=CARTESIAN_POINT('Ctrl Pts',(-6.28377368037099,-3.10995416306685,
40.3728448187451));
#151451=CARTESIAN_POINT('Ctrl Pts',(-6.3788898691041,-2.9177684998708,40.3630796468164));
#151452=CARTESIAN_POINT('Ctrl Pts',(-6.46515936331029,-2.7212697796119,
40.3533144748877));
#151453=CARTESIAN_POINT('Ctrl Pts',(-6.54225724021333,-2.52120938546885,
40.3435493029589));
#151454=CARTESIAN_POINT('Ctrl Pts',(-6.61924999591036,-2.3214217691344,
40.3337974456206));
#151455=CARTESIAN_POINT('Ctrl Pts',(-6.68709611428237,-2.11808222026033,
40.3240455882822));
#151456=CARTESIAN_POINT('Ctrl Pts',(-6.74551997477061,-1.91195889926293,
40.3142937309439));
#151457=CARTESIAN_POINT('Ctrl Pts',(-6.77099700920683,-1.82207420312553,
40.3100412148802));
#151458=CARTESIAN_POINT('Ctrl Pts',(-6.79468293255453,-1.73166039905347,
40.3057886988166));
#151459=CARTESIAN_POINT('Ctrl Pts',(-6.81655777172292,-1.6407823460971,
40.301536182753));
#151460=CARTESIAN_POINT('Ctrl Pts',(-6.85787956284112,-1.46911279037676,
40.293503137154));
#151461=CARTESIAN_POINT('Ctrl Pts',(-6.89275525666553,-1.29570197245542,
40.2854700915551));
#151462=CARTESIAN_POINT('Ctrl Pts',(-6.92104045229321,-1.12108234319386,
40.2774370459562));
#151463=CARTESIAN_POINT('Ctrl Pts',(-6.94930746510802,-0.946574966153722,
40.2694091643083));
#151464=CARTESIAN_POINT('Ctrl Pts',(-6.97099235446394,-0.770860684894565,
40.2613812826604));
#151465=CARTESIAN_POINT('Ctrl Pts',(-6.98600139184853,-0.594483906923033,
40.2533534010125));
#151466=CARTESIAN_POINT('Ctrl Pts',(-7.00100365250474,-0.418186764805898,
40.2453291440324));
#151467=CARTESIAN_POINT('Ctrl Pts',(-7.00933603181675,-0.241228086057471,
40.2373048870522));
#151468=CARTESIAN_POINT('Ctrl Pts',(-7.01095643732055,-0.0641591497259766,
40.229280630072));
#151469=CARTESIAN_POINT('Ctrl Pts',(-7.01257664690082,0.112888377167703,
40.2212573433063));
#151470=CARTESIAN_POINT('Ctrl Pts',(-7.00748648807207,0.290045768821117,
40.2132340565405));
#151471=CARTESIAN_POINT('Ctrl Pts',(-6.995695951825,0.466759801310355,40.2052107697747));
#151472=CARTESIAN_POINT('Ctrl Pts',(-6.98390638170722,0.643459353660757,
40.1971881404457));
#151473=CARTESIAN_POINT('Ctrl Pts',(-6.96541755621622,0.819715253647495,
40.1891655111167));
#151474=CARTESIAN_POINT('Ctrl Pts',(-6.94029147898427,0.994977763187888,
40.1811428817878));
#151475=CARTESIAN_POINT('Ctrl Pts',(-6.91515595613599,1.17030615895504,
40.1731172365213));
#151476=CARTESIAN_POINT('Ctrl Pts',(-6.88337825212799,1.3446400555813,40.1650915912548));
#151477=CARTESIAN_POINT('Ctrl Pts',(-6.84507185866578,1.51743791049314,
40.1570659459883));
#151478=CARTESIAN_POINT('Ctrl Pts',(-6.8224840748064,1.61933005552018,40.152333536481));
#151479=CARTESIAN_POINT('Ctrl Pts',(-6.79762723464555,1.72068831273158,
40.1476011269737));
#151480=CARTESIAN_POINT('Ctrl Pts',(-6.7705328119863,1.82140385535907,40.1428687174664));
#151481=CARTESIAN_POINT('Ctrl Pts',(-6.7205507399375,2.00719749899378,40.1341386686318));
#151482=CARTESIAN_POINT('Ctrl Pts',(-6.66292661929775,2.1908961035576,40.1254086197973));
#151483=CARTESIAN_POINT('Ctrl Pts',(-6.59786241262099,2.37188493536746,
40.1166785709627));
#151484=CARTESIAN_POINT('Ctrl Pts',(-6.53277939254755,2.55292610032427,
40.1079459978237));
#151485=CARTESIAN_POINT('Ctrl Pts',(-6.46025208497953,2.73125567076011,
40.0992134246846));
#151486=CARTESIAN_POINT('Ctrl Pts',(-6.38053124061272,2.9062772837541,40.0904808515455));
#151487=CARTESIAN_POINT('Ctrl Pts',(-6.29967783439212,3.08378535815026,
40.081624218265));
#151488=CARTESIAN_POINT('Ctrl Pts',(-6.21142506240932,3.25789050536534,
40.0727675849846));
#151489=CARTESIAN_POINT('Ctrl Pts',(-6.11608379789225,3.42799439026086,
40.0639109517041));
#151490=CARTESIAN_POINT('Ctrl Pts',(-6.02201819325634,3.59582229630618,
40.0551728195975));
#151491=CARTESIAN_POINT('Ctrl Pts',(-5.92105276121328,3.75975511736256,
40.0464346874909));
#151492=CARTESIAN_POINT('Ctrl Pts',(-5.81353139612541,3.9192447319304,40.0376965553842));
#151493=CARTESIAN_POINT('Ctrl Pts',(-5.70382282309353,4.0819786966019,40.0287806715169));
#151494=CARTESIAN_POINT('Ctrl Pts',(-5.58728889987423,4.24008650266873,
40.0198647876495));
#151495=CARTESIAN_POINT('Ctrl Pts',(-5.46434081005095,4.39301787773641,
40.0109489037822));
#151496=CARTESIAN_POINT('Ctrl Pts',(-5.34139272022769,4.54594925280407,
40.0020330199148));
#151497=CARTESIAN_POINT('Ctrl Pts',(-5.21203065802288,4.69370396499372,
39.9931171360474));
#151498=CARTESIAN_POINT('Ctrl Pts',(-5.07670938084948,4.8357676148565,39.9842012521801));
#151499=CARTESIAN_POINT('Ctrl Pts',(-4.94404720096804,4.97503967810018,
39.9754605676838));
#151500=CARTESIAN_POINT('Ctrl Pts',(-4.80564374229953,5.10885705662395,
39.9667198831874));
#151501=CARTESIAN_POINT('Ctrl Pts',(-4.66196191853821,5.23676786124796,
39.9579791986911));
#151502=CARTESIAN_POINT('Ctrl Pts',(-4.5183059455227,5.36465565259437,39.9492400867891));
#151503=CARTESIAN_POINT('Ctrl Pts',(-4.36937370839542,5.48663881032757,
39.940500974887));
#151504=CARTESIAN_POINT('Ctrl Pts',(-4.2156629617881,5.602304200515,39.9317618629849));
#151505=CARTESIAN_POINT('Ctrl Pts',(-4.05996067123436,5.71946820230066,
39.9229095233107));
#151506=CARTESIAN_POINT('Ctrl Pts',(-3.89935539730565,5.83014939443262,
39.9140571836364));
#151507=CARTESIAN_POINT('Ctrl Pts',(-3.73439792679716,5.93396146657805,
39.9052048439621));
#151508=CARTESIAN_POINT('Ctrl Pts',(-3.57163384851286,6.03639317934285,
39.8964702113122));
#151509=CARTESIAN_POINT('Ctrl Pts',(-3.40463283988954,6.13213717324393,
39.8877355786624));
#151510=CARTESIAN_POINT('Ctrl Pts',(-3.23395276923682,6.22086618155748,
39.8790009460125));
#151511=CARTESIAN_POINT('Ctrl Pts',(-3.05982259758143,6.31138874455716,
39.870089752826));
#151512=CARTESIAN_POINT('Ctrl Pts',(-2.88186329143038,6.39460954863071,
39.8611785596395));
#151513=CARTESIAN_POINT('Ctrl Pts',(-2.70069410207354,6.47023012956457,
39.852267366453));
#151514=CARTESIAN_POINT('Ctrl Pts',(-2.5195249127167,6.54585071049844,39.8433561732665));
#151515=CARTESIAN_POINT('Ctrl Pts',(-2.33514611470285,6.61387093909444,
39.8344449800801));
#151516=CARTESIAN_POINT('Ctrl Pts',(-2.14820008149872,6.67404397440929,
39.8255337868936));
#151517=CARTESIAN_POINT('Ctrl Pts',(-1.97983135953655,6.72823745944292,
39.8175081220413));
#151518=CARTESIAN_POINT('Ctrl Pts',(-1.80930274092191,6.77609026319815,
39.8094824571889));
#151519=CARTESIAN_POINT('Ctrl Pts',(-1.6371404659451,6.81743336287675,39.8014567923366));
#151520=CARTESIAN_POINT('Ctrl Pts',(-1.46503283105088,6.85876334126976,
39.7934336746334));
#151521=CARTESIAN_POINT('Ctrl Pts',(-1.29129292805766,6.89358764334553,
39.7854105569303));
#151522=CARTESIAN_POINT('Ctrl Pts',(-1.11646092111208,6.92178745513972,
39.7773874392271));
#151523=CARTESIAN_POINT('Ctrl Pts',(-0.941650962013093,6.94998371069078,
39.7693653333093));
#151524=CARTESIAN_POINT('Ctrl Pts',(-0.765749535176425,6.97155708222192,
39.7613432273915));
#151525=CARTESIAN_POINT('Ctrl Pts',(-0.589305679083936,6.98644010774439,
39.7533211214737));
#151526=CARTESIAN_POINT('Ctrl Pts',(-0.412796255858879,7.00132866384939,
39.7452960345142));
#151527=CARTESIAN_POINT('Ctrl Pts',(-0.235744366070753,7.00952187356422,
39.7372709475548));
#151528=CARTESIAN_POINT('Ctrl Pts',(-0.058703291197909,7.01100424233951,
39.7292458605953));
#151529=CARTESIAN_POINT('Ctrl Pts',(0.118372651028557,7.0124869030599,39.7212191931352));
#151530=CARTESIAN_POINT('Ctrl Pts',(0.295437407472944,7.00725609560299,
39.713192525675));
#151531=CARTESIAN_POINT('Ctrl Pts',(0.471939239027446,6.99534844858826,
39.7051658582148));
#151532=CARTESIAN_POINT('Ctrl Pts',(0.648582765630539,6.98343124215647,
39.6971327469743));
#151533=CARTESIAN_POINT('Ctrl Pts',(0.824662099716163,6.9648265245611,39.6890996357338));
#151534=CARTESIAN_POINT('Ctrl Pts',(0.999631529077732,6.93962271082324,
39.6810665244933));
#151535=CARTESIAN_POINT('Ctrl Pts',(1.10272987297771,6.92477170818914,39.6763331235313));
#151536=CARTESIAN_POINT('Ctrl Pts',(1.20544302501413,6.90763047736772,39.6715997225693));
#151537=CARTESIAN_POINT('Ctrl Pts',(1.30766130588529,6.88822534994249,39.6668663216073));
#151538=CARTESIAN_POINT('Ctrl Pts',(1.51823414570626,6.84825018352223,39.6571153683131));
#151539=CARTESIAN_POINT('Ctrl Pts',(1.72683044092951,6.79864205883999,39.647364415019));
#151540=CARTESIAN_POINT('Ctrl Pts',(1.93266228092448,6.73961742759868,39.6376134617249));
#151541=CARTESIAN_POINT('Ctrl Pts',(2.13879066030014,6.68050776030271,39.6278484603532));
#151542=CARTESIAN_POINT('Ctrl Pts',(2.34214658070593,6.61195446061618,39.6180834589815));
#151543=CARTESIAN_POINT('Ctrl Pts',(2.54195608500686,6.53422419453118,39.6083184576098));
#151544=CARTESIAN_POINT('Ctrl Pts',(2.74143254826272,6.45662348869478,39.5985697324722));
#151545=CARTESIAN_POINT('Ctrl Pts',(2.9373743740537,6.36987640089905,39.5888210073346));
#151546=CARTESIAN_POINT('Ctrl Pts',(3.12902924000294,6.27429697876237,39.579072282197));
#151547=CARTESIAN_POINT('Ctrl Pts',(3.32015808765932,6.17897988507854,39.5693503135299));
#151548=CARTESIAN_POINT('Ctrl Pts',(3.50702342871833,6.07487886873456,39.5596283448627));
#151549=CARTESIAN_POINT('Ctrl Pts',(3.68889739733891,5.96235377635429,39.5499063761955));
#151550=CARTESIAN_POINT('Ctrl Pts',(3.86956795341381,5.85057323311923,39.5402487352557));
#151551=CARTESIAN_POINT('Ctrl Pts',(4.04531291705903,5.73047972519665,39.5305910943159));
#151552=CARTESIAN_POINT('Ctrl Pts',(4.21543757065316,5.6024737973886,39.520933453376));
#151553=CARTESIAN_POINT('Ctrl Pts',(4.29021321293793,5.54621078514499,39.5166885876909));
#151554=CARTESIAN_POINT('Ctrl Pts',(4.36390331476689,5.48841979199353,39.5124437220058));
#151555=CARTESIAN_POINT('Ctrl Pts',(4.43645009465356,5.42913778791333,39.5081988563207));
#151556=CARTESIAN_POINT('Ctrl Pts',(4.57064190642958,5.3194822036729,39.5003470093067));
#151557=CARTESIAN_POINT('Ctrl Pts',(4.70086432803269,5.20476723100338,39.4924951622927));
#151558=CARTESIAN_POINT('Ctrl Pts',(4.82670255274817,5.08532880252539,39.4846433152787));
#151559=CARTESIAN_POINT('Ctrl Pts',(4.95250509075984,4.9659242458207,39.476793694985));
#151560=CARTESIAN_POINT('Ctrl Pts',(5.07392562865895,4.84179916021885,39.4689440746914));
#151561=CARTESIAN_POINT('Ctrl Pts',(5.19058382647801,4.71332855875812,39.4610944543978));
#151562=CARTESIAN_POINT('Ctrl Pts',(5.30723271063323,4.58486821403047,39.4532454607958));
#151563=CARTESIAN_POINT('Ctrl Pts',(5.41911975572065,4.45206332700402,39.4453964671939));
#151564=CARTESIAN_POINT('Ctrl Pts',(5.52590294796685,4.31532422561171,39.437547473592));
#151565=CARTESIAN_POINT('Ctrl Pts',(5.63274020141575,4.17851589721728,39.4296945062745));
#151566=CARTESIAN_POINT('Ctrl Pts',(5.73446820410757,4.03776967582786,39.4218415389569));
#151567=CARTESIAN_POINT('Ctrl Pts',(5.83078636959375,3.893527561821,39.4139885716394));
#151568=CARTESIAN_POINT('Ctrl Pts',(5.92712899665755,3.74924881516388,39.4061336099321));
#151569=CARTESIAN_POINT('Ctrl Pts',(6.0180588494187,3.60147273203062,39.3982786482248));
#151570=CARTESIAN_POINT('Ctrl Pts',(6.10332020439736,3.45066791289671,39.3904236865174));
#151571=CARTESIAN_POINT('Ctrl Pts',(6.18866618839779,3.29971340737413,39.382560928104));
#151572=CARTESIAN_POINT('Ctrl Pts',(6.26833226194025,3.14572450021766,39.3746981696906));
#151573=CARTESIAN_POINT('Ctrl Pts',(6.34210970178402,2.98919238140289,39.3668354112771));
#151574=CARTESIAN_POINT('Ctrl Pts',(6.39623177300444,2.87436266515472,39.3610674045295));
#151575=CARTESIAN_POINT('Ctrl Pts',(6.44718587698939,2.75816478950835,39.3552993977819));
#151576=CARTESIAN_POINT('Ctrl Pts',(6.49490656785073,2.64079821974142,39.3495313910343));
#151577=CARTESIAN_POINT('Ctrl Pts',(6.5212836758092,2.57592508765594,39.3463431862128));
#151578=CARTESIAN_POINT('Ctrl Pts',(6.54668794650828,2.5106587777768,39.3431549813914));
#151579=CARTESIAN_POINT('Ctrl Pts',(6.57110895151813,2.44502632087639,39.3399667765699));
#151580=CARTESIAN_POINT('Origin',(0.,0.,50.));
#151581=CARTESIAN_POINT('',(6.57110895151815,2.44502632087632,37.3396717263878));
#151582=CARTESIAN_POINT('',(6.57110895151815,2.44502632087634,37.8869079341164));
#151583=CARTESIAN_POINT('',(6.57110895151814,2.44502632087636,50.));
#151584=CARTESIAN_POINT('',(7.01124859079596,-0.00444528532742304,39.7735343569106));
#151585=CARTESIAN_POINT('Ctrl Pts',(6.57110895151815,2.44502632087634,37.8869079341164));
#151586=CARTESIAN_POINT('Ctrl Pts',(6.50741728312095,2.61620030324556,37.8951906864515));
#151587=CARTESIAN_POINT('Ctrl Pts',(6.43702403551672,2.78490829906528,37.9034734387866));
#151588=CARTESIAN_POINT('Ctrl Pts',(6.36015189142897,2.9506091710785,37.9117561911217));
#151589=CARTESIAN_POINT('Ctrl Pts',(6.28327867586599,3.11631235269791,37.9200390589052));
#151590=CARTESIAN_POINT('Ctrl Pts',(6.1999265260549,3.27900801963681,37.9283219266887));
#151591=CARTESIAN_POINT('Ctrl Pts',(6.11036541085665,3.4381770036324,37.9366047944722));
#151592=CARTESIAN_POINT('Ctrl Pts',(6.02078937949257,3.59737249679946,37.9448890417453));
#151593=CARTESIAN_POINT('Ctrl Pts',(5.92500248757278,3.75303984112838,37.9531732890184));
#151594=CARTESIAN_POINT('Ctrl Pts',(5.8233197606272,3.90468609852173,37.9614575362915));
#151595=CARTESIAN_POINT('Ctrl Pts',(5.72160457869351,4.05638075821139,37.9697444277222));
#151596=CARTESIAN_POINT('Ctrl Pts',(5.6139899992133,4.204051491555,37.9780313191528));
#151597=CARTESIAN_POINT('Ctrl Pts',(5.50083348302282,4.34723562215749,37.9863182105834));
#151598=CARTESIAN_POINT('Ctrl Pts',(5.38757363012207,4.49055051126615,37.9946126697629));
#151599=CARTESIAN_POINT('Ctrl Pts',(5.26876193959305,4.62937034612297,38.0029071289424));
#151600=CARTESIAN_POINT('Ctrl Pts',(5.14479585166997,4.76326591816366,38.0112015881219));
#151601=CARTESIAN_POINT('Ctrl Pts',(5.02076609707923,4.89723025646961,38.0195003071808));
#151602=CARTESIAN_POINT('Ctrl Pts',(4.89157690281415,5.02626504698509,38.0277990262396));
#151603=CARTESIAN_POINT('Ctrl Pts',(4.75766173974975,5.14997877011366,38.0360977452985));
#151604=CARTESIAN_POINT('Ctrl Pts',(4.62359552391064,5.27383203906154,38.0444058250937));
#151605=CARTESIAN_POINT('Ctrl Pts',(4.48479294459382,5.39235202756019,38.0527139048889));
#151606=CARTESIAN_POINT('Ctrl Pts',(4.34172048039621,5.50518753836852,38.0610219846842));
#151607=CARTESIAN_POINT('Ctrl Pts',(4.28046381981624,5.55349820824982,38.0645790997932));
#151608=CARTESIAN_POINT('Ctrl Pts',(4.21842480052611,5.60076737341295,38.0681362149023));
#151609=CARTESIAN_POINT('Ctrl Pts',(4.15564160387849,5.64696993285906,38.0716933300113));
#151610=CARTESIAN_POINT('Ctrl Pts',(4.00771138083173,5.75583273834117,38.0800746304163));
#151611=CARTESIAN_POINT('Ctrl Pts',(3.85532845952342,5.85900610843247,38.0884559308212));
#151612=CARTESIAN_POINT('Ctrl Pts',(3.69895524447288,5.95611926189247,38.0968372312262));
#151613=CARTESIAN_POINT('Ctrl Pts',(3.54278020958101,6.05310933864683,38.1052079095598));
#151614=CARTESIAN_POINT('Ctrl Pts',(3.38262523533465,6.14405433362492,38.1135785878934));
#151615=CARTESIAN_POINT('Ctrl Pts',(3.21898415822728,6.22862485237165,38.121949266227));
#151616=CARTESIAN_POINT('Ctrl Pts',(3.05552878564632,6.31309939809982,38.1303104452779));
#151617=CARTESIAN_POINT('Ctrl Pts',(2.88859548451051,6.39121373611139,38.1386716243288));
#151618=CARTESIAN_POINT('Ctrl Pts',(2.71870570115949,6.46268256012802,38.1470328033797));
#151619=CARTESIAN_POINT('Ctrl Pts',(2.54903636984284,6.53405864491492,38.1553831328144));
#151620=CARTESIAN_POINT('Ctrl Pts',(2.37641850897576,6.59880628941818,38.1637334622492));
#151621=CARTESIAN_POINT('Ctrl Pts',(2.20139663399204,6.65668682020933,38.172083791684));
#151622=CARTESIAN_POINT('Ctrl Pts',(2.02650942787135,6.71452281539443,38.1804276960398));
#151623=CARTESIAN_POINT('Ctrl Pts',(1.84922220359946,6.76550212414569,38.1887716003956));
#151624=CARTESIAN_POINT('Ctrl Pts',(1.67009892933501,6.80943434719317,38.1971155047514));
#151625=CARTESIAN_POINT('Ctrl Pts',(1.49111952800193,6.85333128360502,38.2054527072312));
#151626=CARTESIAN_POINT('Ctrl Pts',(1.31030733510672,6.89019234507996,38.2137899097109));
#151627=CARTESIAN_POINT('Ctrl Pts',(1.12824108496155,6.91987706658903,38.2221271121907));
#151628=CARTESIAN_POINT('Ctrl Pts',(1.06830588040342,6.92964911305277,38.2248716732264));
#151629=CARTESIAN_POINT('Ctrl Pts',(1.00823488466737,6.93864387184466,38.2276162342621));
#151630=CARTESIAN_POINT('Ctrl Pts',(0.948049037357854,6.94685753310552,
38.2303607952978));
#151631=CARTESIAN_POINT('Ctrl Pts',(0.765197111634277,6.97181163520638,
38.2386991055997));
#151632=CARTESIAN_POINT('Ctrl Pts',(0.58143451101858,6.98953177441645,38.2470374159015));
#151633=CARTESIAN_POINT('Ctrl Pts',(0.397356357405064,6.99998103481215,
38.2553757262034));
#151634=CARTESIAN_POINT('Ctrl Pts',(0.213162388063885,7.0104368695279,38.2637192826871));
#151635=CARTESIAN_POINT('Ctrl Pts',(0.0286527968454356,7.01361268227092,
38.2720628391709));
#151636=CARTESIAN_POINT('Ctrl Pts',(-0.155576835271572,7.00952369357768,
38.2804063956546));
#151637=CARTESIAN_POINT('Ctrl Pts',(-0.339946628489893,7.00543159399967,
38.2887562998798));
#151638=CARTESIAN_POINT('Ctrl Pts',(-0.524035710558252,6.99406367562809,
38.297106204105));
#151639=CARTESIAN_POINT('Ctrl Pts',(-0.707252720335791,6.97548709066812,
38.3054561083301));
#151640=CARTESIAN_POINT('Ctrl Pts',(-0.890744542069787,6.9568826422054,
38.3138185367937));
#151641=CARTESIAN_POINT('Ctrl Pts',(-1.07336135136743,6.93104795352586,
38.3221809652573));
#151642=CARTESIAN_POINT('Ctrl Pts',(-1.25451958893951,6.89810170724287,
38.3305433937209));
#151643=CARTESIAN_POINT('Ctrl Pts',(-1.43583274150005,6.86512728742811,
38.3389129732008));
#151644=CARTESIAN_POINT('Ctrl Pts',(-1.61568451465483,6.82502924727088,
38.3472825526807));
#151645=CARTESIAN_POINT('Ctrl Pts',(-1.79350509200037,6.77797654521383,
38.3556521321606));
#151646=CARTESIAN_POINT('Ctrl Pts',(-1.9715999359211,6.73085127009667,38.3640346206971));
#151647=CARTESIAN_POINT('Ctrl Pts',(-2.147657011031,6.67674999395358,38.3724171092336));
#151648=CARTESIAN_POINT('Ctrl Pts',(-2.32112376405493,6.61589079674381,
38.3807995977701));
#151649=CARTESIAN_POINT('Ctrl Pts',(-2.37788492807296,6.59597667017714,
38.3835424853748));
#151650=CARTESIAN_POINT('Ctrl Pts',(-2.43436892247531,6.57533934513625,
38.3862853729796));
#151651=CARTESIAN_POINT('Ctrl Pts',(-2.49055693275816,6.5539875440216,38.3890282605843));
#151652=CARTESIAN_POINT('Ctrl Pts',(-2.66242298576839,6.48867735126408,
38.3974181157171));
#151653=CARTESIAN_POINT('Ctrl Pts',(-2.83186510552309,6.41654712207573,
38.4058079708499));
#151654=CARTESIAN_POINT('Ctrl Pts',(-2.99832485660819,6.33779730006771,
38.4141978259827));
#151655=CARTESIAN_POINT('Ctrl Pts',(-3.16463100096848,6.25912014729149,
38.4225799390747));
#151656=CARTESIAN_POINT('Ctrl Pts',(-3.32795996722671,6.17383571881745,
38.4309620521668));
#151657=CARTESIAN_POINT('Ctrl Pts',(-3.48777249563118,6.08219282670475,
38.4393441652589));
#151658=CARTESIAN_POINT('Ctrl Pts',(-3.64746104338508,5.99062103005306,
38.4477197756078));
#151659=CARTESIAN_POINT('Ctrl Pts',(-3.80363830796303,5.89270076724283,
38.4560953859567));
#151660=CARTESIAN_POINT('Ctrl Pts',(-3.95578847193318,5.78872733230894,
38.4644709963055));
#151661=CARTESIAN_POINT('Ctrl Pts',(-4.10784293119061,5.68481929820973,
38.4728413382711));
#151662=CARTESIAN_POINT('Ctrl Pts',(-4.255875069918,5.57486586886209,38.4812116802367));
#151663=CARTESIAN_POINT('Ctrl Pts',(-4.39939659076811,5.45920655403676,
38.4895820222023));
#151664=CARTESIAN_POINT('Ctrl Pts',(-4.54284887309337,5.34360303628143,
38.4979483260966));
#151665=CARTESIAN_POINT('Ctrl Pts',(-4.68179462141739,5.22229932821294,
38.5063146299909));
#151666=CARTESIAN_POINT('Ctrl Pts',(-4.81577691361292,5.095676528275,38.5146809338852));
#151667=CARTESIAN_POINT('Ctrl Pts',(-4.94972173471686,4.96908914118497,
38.5230448979588));
#151668=CARTESIAN_POINT('Ctrl Pts',(-5.07870562797996,4.83718585297268,
38.5314088620324));
#151669=CARTESIAN_POINT('Ctrl Pts',(-5.20230657686934,4.70038645674609,
38.539772826106));
#151670=CARTESIAN_POINT('Ctrl Pts',(-5.32588850562665,4.56360811167329,
38.5481355031046));
#151671=CARTESIAN_POINT('Ctrl Pts',(-5.44408892129556,4.42193540456572,
38.5564981801031));
#151672=CARTESIAN_POINT('Ctrl Pts',(-5.55652406798816,4.27582352820698,
38.5648608571016));
#151673=CARTESIAN_POINT('Ctrl Pts',(-5.66895689984657,4.12971466002473,
38.5732233619279));
#151674=CARTESIAN_POINT('Ctrl Pts',(-5.77562449930101,3.9791670655361,38.5815858667542));
#151675=CARTESIAN_POINT('Ctrl Pts',(-5.87618440035542,3.82466775753394,
38.5899483715805));
#151676=CARTESIAN_POINT('Ctrl Pts',(-5.97675563498432,3.67015103673206,
38.5983118189005));
#151677=CARTESIAN_POINT('Ctrl Pts',(-6.07121761998585,3.51168199018858,
38.6066752662205));
#151678=CARTESIAN_POINT('Ctrl Pts',(-6.15927186734454,3.34977560840097,
38.6150387135404));
#151679=CARTESIAN_POINT('Ctrl Pts',(-6.24737796351867,3.18777389158571,
38.6234070854932));
#151680=CARTESIAN_POINT('Ctrl Pts',(-6.32906862455444,3.02233108365615,
38.631775457446));
#151681=CARTESIAN_POINT('Ctrl Pts',(-6.40409141329911,2.85398663847758,
38.6401438293988));
#151682=CARTESIAN_POINT('Ctrl Pts',(-6.47913668083207,2.68559175290345,
38.6485147087346));
#151683=CARTESIAN_POINT('Ctrl Pts',(-6.54750996339649,2.51429379891466,
38.6568855880703));
#151684=CARTESIAN_POINT('Ctrl Pts',(-6.60900717989436,2.34065175936209,
38.6652564674061));
#151685=CARTESIAN_POINT('Ctrl Pts',(-6.67055650231875,2.16686259478713,
38.6736344392974));
#151686=CARTESIAN_POINT('Ctrl Pts',(-6.72521801252274,1.99072568787033,
38.6820124111886));
#151687=CARTESIAN_POINT('Ctrl Pts',(-6.77283731893325,1.8128158245572,38.6903903830799));
#151688=CARTESIAN_POINT('Ctrl Pts',(-6.80309977592282,1.69975265769545,
38.695714652439));
#151689=CARTESIAN_POINT('Ctrl Pts',(-6.8305191081714,1.5859737199079,38.701038921798));
#151690=CARTESIAN_POINT('Ctrl Pts',(-6.85506642330607,1.47162865375803,
38.706363191157));
#151691=CARTESIAN_POINT('Ctrl Pts',(-6.8913176686956,1.3027649295854,38.7142260223463));
#151692=CARTESIAN_POINT('Ctrl Pts',(-6.92137795629598,1.13231489320976,
38.7220888535356));
#151693=CARTESIAN_POINT('Ctrl Pts',(-6.94510661887911,0.960791660507956,
38.7299516847249));
#151694=CARTESIAN_POINT('Ctrl Pts',(-6.96881704911719,0.789400220769712,
38.7378084743663));
#151695=CARTESIAN_POINT('Ctrl Pts',(-6.98620547721606,0.616937599793814,
38.7456652640077));
#151696=CARTESIAN_POINT('Ctrl Pts',(-6.99718182459533,0.443929134043713,
38.7535220536491));
#151697=CARTESIAN_POINT('Ctrl Pts',(-7.00815198183427,0.27101823687844,
38.7613744124331));
#151698=CARTESIAN_POINT('Ctrl Pts',(-7.01271722755952,0.09756248660523,
38.7692267712171));
#151699=CARTESIAN_POINT('Ctrl Pts',(-7.01083909849228,-0.0759058466254896,
38.777079130001));
#151700=CARTESIAN_POINT('Ctrl Pts',(-7.00896141287323,-0.2493332219587,
38.7849296347515));
#151701=CARTESIAN_POINT('Ctrl Pts',(-7.00064337606947,-0.422772793341922,
38.7927801395019));
#151702=CARTESIAN_POINT('Ctrl Pts',(-6.98589860771008,-0.595690528122043,
38.8006306442524));
#151703=CARTESIAN_POINT('Ctrl Pts',(-6.97115621131921,-0.768580445888531,
38.808479886104));
#151704=CARTESIAN_POINT('Ctrl Pts',(-6.94998917689365,-0.940948314271634,
38.8163291279557));
#151705=CARTESIAN_POINT('Ctrl Pts',(-6.92246310930327,-1.11226393577931,
38.8241783698073));
#151706=CARTESIAN_POINT('Ctrl Pts',(-6.89492776764194,-1.28363727687313,
38.8320302562222));
#151707=CARTESIAN_POINT('Ctrl Pts',(-6.86102917391573,-1.45395728592724,
38.839882142637));
#151708=CARTESIAN_POINT('Ctrl Pts',(-6.82088434046041,-1.6227024916977,
38.8477340290519));
#151709=CARTESIAN_POINT('Ctrl Pts',(-6.79140648892726,-1.74660999596395,
38.8534995715158));
#151710=CARTESIAN_POINT('Ctrl Pts',(-6.75856187735805,-1.86966856995148,
38.8592651139797));
#151711=CARTESIAN_POINT('Ctrl Pts',(-6.72241403827056,-1.99167669579251,
38.8650306564436));
#151712=CARTESIAN_POINT('Ctrl Pts',(-6.66187881707776,-2.19599842211283,
38.8746859608036));
#151713=CARTESIAN_POINT('Ctrl Pts',(-6.59211003230734,-2.39726976124543,
38.8843412651637));
#151714=CARTESIAN_POINT('Ctrl Pts',(-6.51343727596498,-2.59475652317707,
38.8939965695238));
#151715=CARTESIAN_POINT('Ctrl Pts',(-6.43432868731119,-2.79333732472205,
38.9037053624587));
#151716=CARTESIAN_POINT('Ctrl Pts',(-6.34621726945475,-2.98809147764601,
38.9134141553936));
#151717=CARTESIAN_POINT('Ctrl Pts',(-6.24948186147165,-3.17830190913904,
38.9231229483285));
#151718=CARTESIAN_POINT('Ctrl Pts',(-6.15228095449145,-3.36942764937933,
38.9328784607994));
#151719=CARTESIAN_POINT('Ctrl Pts',(-6.04637289994086,-3.55596580573971,
38.9426339732703));
#151720=CARTESIAN_POINT('Ctrl Pts',(-5.93218523844047,-3.73721886692886,
38.9523894857412));
#151721=CARTESIAN_POINT('Ctrl Pts',(-5.8178845135879,-3.9186513965336,38.9621546576703));
#151722=CARTESIAN_POINT('Ctrl Pts',(-5.69528781363722,-4.09478833717525,
38.9719198295994));
#151723=CARTESIAN_POINT('Ctrl Pts',(-5.56486651916761,-4.2649603968088,
38.9816850015284));
#151724=CARTESIAN_POINT('Ctrl Pts',(-5.43462305117419,-4.43490043069964,
38.9914368588671));
#151725=CARTESIAN_POINT('Ctrl Pts',(-5.29657633458902,-4.59889180839344,
39.0011887162059));
#151726=CARTESIAN_POINT('Ctrl Pts',(-5.15123779077445,-4.75629853829606,
39.0109405735446));
#151727=CARTESIAN_POINT('Ctrl Pts',(-5.08785965976759,-4.82493927245572,
39.0151930896064));
#151728=CARTESIAN_POINT('Ctrl Pts',(-5.02309545812617,-4.89232827088929,
39.0194456056682));
#151729=CARTESIAN_POINT('Ctrl Pts',(-4.95699008883871,-4.95841464801552,
39.02369812173));
#151730=CARTESIAN_POINT('Ctrl Pts',(-4.83211638158264,-5.08325247888805,
39.0317311673287));
#151731=CARTESIAN_POINT('Ctrl Pts',(-4.70239330496352,-5.20350034449388,
39.0397642129274));
#151732=CARTESIAN_POINT('Ctrl Pts',(-4.568199694016,-5.31875719676055,39.0477972585261));
#151733=CARTESIAN_POINT('Ctrl Pts',(-4.4340923478886,-5.43393995748473,
39.0558251401738));
#151734=CARTESIAN_POINT('Ctrl Pts',(-4.29552046478516,-5.54413785345578,
39.0638530218215));
#151735=CARTESIAN_POINT('Ctrl Pts',(-4.15289952349382,-5.6489868215694,
39.0718809034692));
#151736=CARTESIAN_POINT('Ctrl Pts',(-4.01034297696333,-5.75378844934041,
39.0799051604492));
#151737=CARTESIAN_POINT('Ctrl Pts',(-3.86374130711362,-5.85324574130714,
39.0879294174292));
#151738=CARTESIAN_POINT('Ctrl Pts',(-3.71354280167257,-5.94703509512478,
39.0959536744092));
#151739=CARTESIAN_POINT('Ctrl Pts',(-3.56336245676058,-6.04081310885432,
39.1039769611748));
#151740=CARTESIAN_POINT('Ctrl Pts',(-3.40958644915615,-6.12892434887665,
39.1120002479404));
#151741=CARTESIAN_POINT('Ctrl Pts',(-3.25269190644824,-6.21108862633807,
39.120023534706));
#151742=CARTESIAN_POINT('Ctrl Pts',(-3.09581021984847,-6.29324617116993,
39.1280461640348));
#151743=CARTESIAN_POINT('Ctrl Pts',(-2.93581083381414,-6.3694575575606,
39.1360687933636));
#151744=CARTESIAN_POINT('Ctrl Pts',(-2.77319504630513,-6.43948878387475,
39.1440914226925));
#151745=CARTESIAN_POINT('Ctrl Pts',(-2.61051812683718,-6.50954633694424,
39.1521170679588));
#151746=CARTESIAN_POINT('Ctrl Pts',(-2.4452231791185,-6.57341894642677,
39.1601427132251));
#151747=CARTESIAN_POINT('Ctrl Pts',(-2.27783138026074,-6.63092080827388,
39.1681683584914));
#151748=CARTESIAN_POINT('Ctrl Pts',(-2.1791269752883,-6.66482741001396,
39.1729007679997));
#151749=CARTESIAN_POINT('Ctrl Pts',(-2.07969383548703,-6.69651983058423,
39.177633177508));
#151750=CARTESIAN_POINT('Ctrl Pts',(-1.9796412180197,-6.72596812439797,
39.1823655870163));
#151751=CARTESIAN_POINT('Ctrl Pts',(-1.79507049669824,-6.78029246861277,
39.1910956358511));
#151752=CARTESIAN_POINT('Ctrl Pts',(-1.608298733072,-6.8270046181273,39.1998256846859));
#151753=CARTESIAN_POINT('Ctrl Pts',(-1.41995570841795,-6.86595604039461,
39.2085557335207));
#151754=CARTESIAN_POINT('Ctrl Pts',(-1.23155822414363,-6.90491872551421,
39.21728830666));
#151755=CARTESIAN_POINT('Ctrl Pts',(-1.04158884023543,-6.93611614871323,
39.2260208797993));
#151756=CARTESIAN_POINT('Ctrl Pts',(-0.850687128366196,-6.95945098209134,
39.2347534529386));
#151757=CARTESIAN_POINT('Ctrl Pts',(-0.657073352947585,-6.98311732402648,
39.2436100862189));
#151758=CARTESIAN_POINT('Ctrl Pts',(-0.462500844959412,-6.99869593705051,
39.2524667194993));
#151759=CARTESIAN_POINT('Ctrl Pts',(-0.267642234618632,-7.00613975001558,
39.2613233527796));
#151760=CARTESIAN_POINT('Ctrl Pts',(-0.0753908197272747,-7.01348396525051,
39.2700614848865));
#151761=CARTESIAN_POINT('Ctrl Pts',(0.117138810563617,-7.01290972725781,
39.2787996169934));
#151762=CARTESIAN_POINT('Ctrl Pts',(0.30929962673723,-7.00442433775969,
39.2875377491003));
#151763=CARTESIAN_POINT('Ctrl Pts',(0.505369393118843,-6.99576633781109,
39.2964536329674));
#151764=CARTESIAN_POINT('Ctrl Pts',(0.701054883679541,-6.97887188955622,
39.3053695168345));
#151765=CARTESIAN_POINT('Ctrl Pts',(0.895672117856525,-6.95380457158485,
39.3142854007016));
#151766=CARTESIAN_POINT('Ctrl Pts',(1.09028935203351,-6.92873725361349,
39.3232012845686));
#151767=CARTESIAN_POINT('Ctrl Pts',(1.28383803066942,-6.89549711059129,
39.3321171684357));
#151768=CARTESIAN_POINT('Ctrl Pts',(1.47564203379495,-6.8542036116968,39.3410330523028));
#151769=CARTESIAN_POINT('Ctrl Pts',(1.66367703979096,-6.8137215404903,39.3497737367989));
#151770=CARTESIAN_POINT('Ctrl Pts',(1.85005527164544,-6.76549537689399,
39.358514421295));
#151771=CARTESIAN_POINT('Ctrl Pts',(2.03414967565739,-6.70968416987886,
39.3672551057911));
#151772=CARTESIAN_POINT('Ctrl Pts',(2.21821095802815,-6.65388300422693,
39.3759942176929));
#151773=CARTESIAN_POINT('Ctrl Pts',(2.39998897122777,-6.59049959992355,
39.3847333295946));
#151774=CARTESIAN_POINT('Ctrl Pts',(2.57887153826412,-6.51974295134641,
39.3934724414964));
#151775=CARTESIAN_POINT('Ctrl Pts',(2.76007178641663,-6.44806954854909,
39.4023247811708));
#151776=CARTESIAN_POINT('Ctrl Pts',(2.93830076272921,-6.36883059153292,
39.4111771208452));
#151777=CARTESIAN_POINT('Ctrl Pts',(3.11294149546067,-6.28229431086599,
39.4200294605196));
#151778=CARTESIAN_POINT('Ctrl Pts',(3.28526008039774,-6.19690867833332,
39.4287640931692));
#151779=CARTESIAN_POINT('Ctrl Pts',(3.45408500727737,-6.10441871503209,
39.4374987258189));
#151780=CARTESIAN_POINT('Ctrl Pts',(3.61884597437017,-6.00512950537162,
39.4462333584685));
#151781=CARTESIAN_POINT('Ctrl Pts',(3.78693739461582,-5.9038332787144,39.4551445516553));
#151782=CARTESIAN_POINT('Ctrl Pts',(3.95079854881783,-5.79546013156801,
39.4640557448421));
#151783=CARTESIAN_POINT('Ctrl Pts',(4.10985167050952,-5.68038254071943,
39.4729669380288));
#151784=CARTESIAN_POINT('Ctrl Pts',(4.26890479220121,-5.56530494987085,
39.4818781312156));
#151785=CARTESIAN_POINT('Ctrl Pts',(4.42314962789435,-5.44352308209216,
39.4907893244024));
#151786=CARTESIAN_POINT('Ctrl Pts',(4.57204038024953,-5.31545607863217,
39.4997005175891));
#151787=CARTESIAN_POINT('Ctrl Pts',(4.70613547312795,-5.20011542481734,
39.5077261824416));
#151788=CARTESIAN_POINT('Ctrl Pts',(4.83594899628487,-5.07962330971981,
39.5157518472941));
#151789=CARTESIAN_POINT('Ctrl Pts',(4.96106213968239,-4.95434042115699,
39.5237775121466));
#151790=CARTESIAN_POINT('Ctrl Pts',(5.08613557523666,-4.82909729431037,
39.5318006298499));
#151791=CARTESIAN_POINT('Ctrl Pts',(5.20651134231518,-4.69906668019109,
39.5398237475532));
#151792=CARTESIAN_POINT('Ctrl Pts',(5.32180619379329,-4.5646473465322,39.5478468652565));
#151793=CARTESIAN_POINT('Ctrl Pts',(5.43708650558191,-4.43024496432731,
39.5558689711744));
#151794=CARTESIAN_POINT('Ctrl Pts',(5.54728693992884,-4.29145524355056,
39.5638910770924));
#151795=CARTESIAN_POINT('Ctrl Pts',(5.65206342294826,-4.14871132105746,
39.5719131830103));
#151796=CARTESIAN_POINT('Ctrl Pts',(5.75687884126272,-4.00591435444058,
39.57993826997));
#151797=CARTESIAN_POINT('Ctrl Pts',(5.85626606227109,-3.85916054473022,
39.5879633569296));
#151798=CARTESIAN_POINT('Ctrl Pts',(5.94992312729261,-3.70891376845143,
39.5959884438892));
#151799=CARTESIAN_POINT('Ctrl Pts',(6.04359863760414,-3.55863740182233,
39.6040151113495));
#151800=CARTESIAN_POINT('Ctrl Pts',(6.13154155728599,-3.4048670139046,39.6120417788098));
#151801=CARTESIAN_POINT('Ctrl Pts',(6.21349519491764,-3.2480923671034,39.6200684462701));
#151802=CARTESIAN_POINT('Ctrl Pts',(6.29551462464098,-3.09119186216786,
39.6281015575108));
#151803=CARTESIAN_POINT('Ctrl Pts',(6.37153500763469,-2.93128261046679,
39.6361346687515));
#151804=CARTESIAN_POINT('Ctrl Pts',(6.44134697281337,-2.76887625912174,
39.6441677799922));
#151805=CARTESIAN_POINT('Ctrl Pts',(6.48248271875035,-2.67318053718666,
39.6489011809534));
#151806=CARTESIAN_POINT('Ctrl Pts',(6.52146382345709,-2.57661819013828,
39.6536345819146));
#151807=CARTESIAN_POINT('Ctrl Pts',(6.55825550999511,-2.47929651879699,
39.6583679828758));
#151808=CARTESIAN_POINT('Ctrl Pts',(6.63609765095225,-2.27338784834488,
39.6683826927056));
#151809=CARTESIAN_POINT('Ctrl Pts',(6.70417624722286,-2.06397613249315,
39.6783974025354));
#151810=CARTESIAN_POINT('Ctrl Pts',(6.76225540238797,-1.85189860288697,
39.6884121123653));
#151811=CARTESIAN_POINT('Ctrl Pts',(6.82040337169505,-1.63956979667062,
39.6984386879611));
#151812=CARTESIAN_POINT('Ctrl Pts',(6.86852822639077,-1.42456881701543,
39.7084652635569));
#151813=CARTESIAN_POINT('Ctrl Pts',(6.90644452585608,-1.20774607172724,
39.7184918391527));
#151814=CARTESIAN_POINT('Ctrl Pts',(6.94423360637603,-0.991650822565392,
39.7284847730064));
#151815=CARTESIAN_POINT('Ctrl Pts',(6.97188254054378,-0.773745968779786,
39.73847770686));
#151816=CARTESIAN_POINT('Ctrl Pts',(6.98925819898149,-0.554884123461851,
39.7484706407136));
#151817=CARTESIAN_POINT('Ctrl Pts',(7.00378508295101,-0.371905121907101,
39.7568252127792));
#151818=CARTESIAN_POINT('Ctrl Pts',(7.01113204989888,-0.188257378415018,
39.7651797848449));
#151819=CARTESIAN_POINT('Ctrl Pts',(7.01124859079596,-0.00444528532742304,
39.7735343569106));
#151820=CARTESIAN_POINT('Ctrl Pts',(7.01125,4.27274591884109E-12,39.7735343569106));
#151821=CARTESIAN_POINT('Ctrl Pts',(7.01124999999988,0.191008754744388,
39.7822061308427));
#151822=CARTESIAN_POINT('Ctrl Pts',(7.00344012880995,0.382017367487167,
39.7908779047748));
#151823=CARTESIAN_POINT('Ctrl Pts',(6.98784644419146,0.572388534913825,
39.7995496787069));
#151824=CARTESIAN_POINT('Ctrl Pts',(6.97225169663163,0.762772678964547,
39.8082220437493));
#151825=CARTESIAN_POINT('Ctrl Pts',(6.94887209704274,0.95251900763093,39.8168944087916));
#151826=CARTESIAN_POINT('Ctrl Pts',(6.91778566246042,1.14099434299962,39.825566773834));
#151827=CARTESIAN_POINT('Ctrl Pts',(6.88670108297129,1.32945843104071,39.8342386213501));
#151828=CARTESIAN_POINT('Ctrl Pts',(6.84791063501086,1.51665139731196,39.8429104688662));
#151829=CARTESIAN_POINT('Ctrl Pts',(6.80154374572899,1.7019486588716,39.8515823163824));
#151830=CARTESIAN_POINT('Ctrl Pts',(6.75517597619819,1.88724943819403,39.8602543285286));
#151831=CARTESIAN_POINT('Ctrl Pts',(6.70123154646044,2.07065416525604,39.8689263406748));
#151832=CARTESIAN_POINT('Ctrl Pts',(6.63989045285482,2.25155087363966,39.877598352821));
#151833=CARTESIAN_POINT('Ctrl Pts',(6.61790934153606,2.31637382429882,39.8807059019881));
#151834=CARTESIAN_POINT('Ctrl Pts',(6.59497889661496,2.38087486019118,39.8838134511552));
#151835=CARTESIAN_POINT('Ctrl Pts',(6.57110895151814,2.44502632087636,39.8869210003223));
#151836=CARTESIAN_POINT('',(7.01124999602994,0.000235945347496286,39.2264656431317));
#151837=CARTESIAN_POINT('Ctrl Pts',(6.57110895151813,2.44502632087639,39.3399667765699));
#151838=CARTESIAN_POINT('Ctrl Pts',(6.64421271995929,2.24855693194103,39.3304229520256));
#151839=CARTESIAN_POINT('Ctrl Pts',(6.70850190625911,2.04880522801078,39.3208791274812));
#151840=CARTESIAN_POINT('Ctrl Pts',(6.76372928243494,1.84650826059135,39.3113353029369));
#151841=CARTESIAN_POINT('Ctrl Pts',(6.81886334836796,1.6445530870513,39.3018076033046));
#151842=CARTESIAN_POINT('Ctrl Pts',(6.86496615835579,1.4400613342989,39.2922799036724));
#151843=CARTESIAN_POINT('Ctrl Pts',(6.90184075352121,1.23378311527345,39.2827522040401));
#151844=CARTESIAN_POINT('Ctrl Pts',(6.93853377568314,1.02852062416622,39.273271419446));
#151845=CARTESIAN_POINT('Ctrl Pts',(6.96608920614919,0.821489313606136,
39.2637906348519));
#151846=CARTESIAN_POINT('Ctrl Pts',(6.98436207776607,0.61344350119897,39.2543098502577));
#151847=CARTESIAN_POINT('Ctrl Pts',(7.0022506683511,0.409772921165857,39.2450284478824));
#151848=CARTESIAN_POINT('Ctrl Pts',(7.01124310084812,0.205130188839553,
39.235747045507));
#151849=CARTESIAN_POINT('Ctrl Pts',(7.01124999602994,0.000235945347480019,
39.2264656431317));
#151850=CARTESIAN_POINT('Ctrl Pts',(7.01124999602997,0.000235944418096841,
39.2264656430896));
#151851=CARTESIAN_POINT('Ctrl Pts',(7.01125624170091,-0.185358445530651,
39.2180584951759));
#151852=CARTESIAN_POINT('Ctrl Pts',(7.00388885553632,-0.370934254546438,
39.2096513472621));
#151853=CARTESIAN_POINT('Ctrl Pts',(6.98917832624288,-0.555889275374905,
39.2012441993484));
#151854=CARTESIAN_POINT('Ctrl Pts',(6.97446405541024,-0.740891338457691,
39.1928349131245));
#151855=CARTESIAN_POINT('Ctrl Pts',(6.95240294147731,-0.925271977684133,
39.1844256269007));
#151856=CARTESIAN_POINT('Ctrl Pts',(6.92307738877438,-1.10843404474104,
39.1760163406768));
#151857=CARTESIAN_POINT('Ctrl Pts',(6.89374093683712,-1.29166418643262,
39.1676039290291));
#151858=CARTESIAN_POINT('Ctrl Pts',(6.85713471151255,-1.47367453500346,
39.1591915173815));
#151859=CARTESIAN_POINT('Ctrl Pts',(6.81339236826982,-1.65387756454419,
39.1507791057338));
#151860=CARTESIAN_POINT('Ctrl Pts',(6.76962863059373,-1.83416873160611,
39.1423625795653));
#151861=CARTESIAN_POINT('Ctrl Pts',(6.71872188872574,-2.0126505040424,39.1339460533969));
#151862=CARTESIAN_POINT('Ctrl Pts',(6.66085597739889,-2.1887494627868,39.1255295272284));
#151863=CARTESIAN_POINT('Ctrl Pts',(6.60292446423264,-2.36504806265572,
39.1171034593525));
#151864=CARTESIAN_POINT('Ctrl Pts',(6.53801811449966,-2.53895814410867,
39.1086773914766));
#151865=CARTESIAN_POINT('Ctrl Pts',(6.46636985185425,-2.70992389220259,
39.1002513236007));
#151866=CARTESIAN_POINT('Ctrl Pts',(6.39467912786007,-2.88099096077507,
39.0918202621325));
#151867=CARTESIAN_POINT('Ctrl Pts',(6.31623865159298,-3.04910992165933,
39.0833892006644));
#151868=CARTESIAN_POINT('Ctrl Pts',(6.2313281825243,-3.21374791235692,39.0749581391963));
#151869=CARTESIAN_POINT('Ctrl Pts',(6.14630796696497,-3.37859869709397,
39.06651618061));
#151870=CARTESIAN_POINT('Ctrl Pts',(6.05480119927518,-3.5399592370319,39.0580742220238));
#151871=CARTESIAN_POINT('Ctrl Pts',(5.95713277845971,-3.69732276414988,
39.0496322634376));
#151872=CARTESIAN_POINT('Ctrl Pts',(5.8898921681621,-3.80566095077819,39.0438203291122));
#151873=CARTESIAN_POINT('Ctrl Pts',(5.81973201113902,-3.91210524289392,
39.0380083947868));
#151874=CARTESIAN_POINT('Ctrl Pts',(5.74676973213542,-4.01649899891836,
39.0321964604614));
#151875=CARTESIAN_POINT('Ctrl Pts',(5.64155196051087,-4.16704361636195,
39.0238151600566));
#151876=CARTESIAN_POINT('Ctrl Pts',(5.53029242921354,-4.31362675214747,
39.0154338596518));
#151877=CARTESIAN_POINT('Ctrl Pts',(5.41331025385954,-4.45574894467352,
39.007052559247));
#151878=CARTESIAN_POINT('Ctrl Pts',(5.29647633628785,-4.59769101812572,
38.9986818809135));
#151879=CARTESIAN_POINT('Ctrl Pts',(5.17393443490431,-4.73518316441594,
38.9903112025801));
#151880=CARTESIAN_POINT('Ctrl Pts',(5.04604670723755,-4.86775504631007,
38.9819405242466));
#151881=CARTESIAN_POINT('Ctrl Pts',(4.9183041101841,-5.00017648188007,38.9735793451959));
#151882=CARTESIAN_POINT('Ctrl Pts',(4.78522800433629,-5.12768854751416,
38.9652181661451));
#151883=CARTESIAN_POINT('Ctrl Pts',(4.64722083488818,-5.24985381456296,
38.9568569870944));
#151884=CARTESIAN_POINT('Ctrl Pts',(4.50939274602224,-5.37186055776671,
38.9485066576597));
#151885=CARTESIAN_POINT('Ctrl Pts',(4.36664660049408,-5.4885341250155,38.9401563282251));
#151886=CARTESIAN_POINT('Ctrl Pts',(4.21942164598243,-5.59947386241912,
38.9318059987905));
#151887=CARTESIAN_POINT('Ctrl Pts',(4.07230997226684,-5.71032823833081,
38.9234620944349));
#151888=CARTESIAN_POINT('Ctrl Pts',(3.92072661773254,-5.8154573800439,38.9151181900793));
#151889=CARTESIAN_POINT('Ctrl Pts',(3.76514473331342,-5.91450012255492,
38.9067742857237));
#151890=CARTESIAN_POINT('Ctrl Pts',(3.60968781323395,-6.01346331331762,
38.8984370832441));
#151891=CARTESIAN_POINT('Ctrl Pts',(3.45023904403302,-6.10634967911778,
38.8900998807645));
#151892=CARTESIAN_POINT('Ctrl Pts',(3.28730157298377,-6.19284061887261,
38.8817626782849));
#151893=CARTESIAN_POINT('Ctrl Pts',(3.23366345689626,-6.2213129588274,38.8790181172483));
#151894=CARTESIAN_POINT('Ctrl Pts',(3.17964750752207,-6.24909258139602,
38.8762735562117));
#151895=CARTESIAN_POINT('Ctrl Pts',(3.12527233755018,-6.27616916427877,
38.8735289951751));
#151896=CARTESIAN_POINT('Ctrl Pts',(2.9600739564974,-6.35843111691236,38.8651906848731));
#151897=CARTESIAN_POINT('Ctrl Pts',(2.79169365376994,-6.43413296875984,
38.8568523745711));
#151898=CARTESIAN_POINT('Ctrl Pts',(2.62068329857847,-6.50304894730556,
38.8485140642691));
#151899=CARTESIAN_POINT('Ctrl Pts',(2.44956534947534,-6.57200828544607,
38.8401705077853));
#151900=CARTESIAN_POINT('Ctrl Pts',(2.2758143512251,-6.63417311188344,38.8318269513015));
#151901=CARTESIAN_POINT('Ctrl Pts',(2.09999932365371,-6.68936689105583,
38.8234833948177));
#151902=CARTESIAN_POINT('Ctrl Pts',(1.92405053677385,-6.74460266141542,
38.8151334905923));
#151903=CARTESIAN_POINT('Ctrl Pts',(1.74603490058279,-6.7928567076473,38.806783586367));
#151904=CARTESIAN_POINT('Ctrl Pts',(1.56653408794348,-6.83400303729894,
38.7984336821417));
#151905=CARTESIAN_POINT('Ctrl Pts',(1.38676403736921,-6.87521108340002,
38.790071253678));
#151906=CARTESIAN_POINT('Ctrl Pts',(1.2055046784367,-6.90929003552121,38.7817088252142));
#151907=CARTESIAN_POINT('Ctrl Pts',(1.02334681547847,-6.93616521269138,
38.7733463967505));
#151908=CARTESIAN_POINT('Ctrl Pts',(0.841033182715451,-6.96306337180169,
38.7649768172705));
#151909=CARTESIAN_POINT('Ctrl Pts',(0.657819837884503,-6.98274542983526,
38.7566072377904));
#151910=CARTESIAN_POINT('Ctrl Pts',(0.474300687146857,-6.99518873374207,
38.7482376583104));
#151911=CARTESIAN_POINT('Ctrl Pts',(0.290498480479108,-7.00765122992908,
38.7398551697738));
#151912=CARTESIAN_POINT('Ctrl Pts',(0.106389852255073,-7.01285265196182,
38.7314726812371));
#151913=CARTESIAN_POINT('Ctrl Pts',(-0.0774318940327818,-7.01082240998062,
38.7230901927005));
#151914=CARTESIAN_POINT('Ctrl Pts',(-0.137581381506239,-7.010158081537,
38.7203473050965));
#151915=CARTESIAN_POINT('Ctrl Pts',(-0.197700200088622,-7.00871986779992,
38.7176044174926));
#151916=CARTESIAN_POINT('Ctrl Pts',(-0.257767731967355,-7.00650999848401,
38.7148615298886));
#151917=CARTESIAN_POINT('Ctrl Pts',(-0.441500339136088,-6.9997505223042,
38.7064716747558));
#151918=CARTESIAN_POINT('Ctrl Pts',(-0.625123584587192,-6.9857538927227,
38.6980818196231));
#151919=CARTESIAN_POINT('Ctrl Pts',(-0.808044247700737,-6.96453092865972,
38.6896919644903));
#151920=CARTESIAN_POINT('Ctrl Pts',(-0.990796114190347,-6.94332754885049,
38.6813098513982));
#151921=CARTESIAN_POINT('Ctrl Pts',(-1.17284636583428,-6.91491116563033,
38.6729277383062));
#151922=CARTESIAN_POINT('Ctrl Pts',(-1.35360443769717,-6.87934456098446,
38.6645456252141));
#151923=CARTESIAN_POINT('Ctrl Pts',(-1.53422227960679,-6.8438055484857,
38.6561700148653));
#151924=CARTESIAN_POINT('Ctrl Pts',(-1.71354961894566,-6.8011274369386,
38.6477944045164));
#151925=CARTESIAN_POINT('Ctrl Pts',(-1.89100319271344,-6.75142455246651,
38.6394187941676));
#151926=CARTESIAN_POINT('Ctrl Pts',(-2.06834514554848,-6.70175293184674,
38.631048452202));
#151927=CARTESIAN_POINT('Ctrl Pts',(-2.24381536715877,-6.64506543719887,
38.6226781102364));
#151928=CARTESIAN_POINT('Ctrl Pts',(-2.41684248556805,-6.581527099576,38.6143077682709));
#151929=CARTESIAN_POINT('Ctrl Pts',(-2.5897861311839,-6.51801941450389,
38.6059414643765));
#151930=CARTESIAN_POINT('Ctrl Pts',(-2.76028871592533,-6.44766759032456,
38.5975751604822));
#151931=CARTESIAN_POINT('Ctrl Pts',(-2.92779525273806,-6.37068611065908,
38.5892088565878));
#151932=CARTESIAN_POINT('Ctrl Pts',(-3.09525494266641,-6.29372616055623,
38.5808448925142));
#151933=CARTESIAN_POINT('Ctrl Pts',(-3.2597199564803,-6.21014038788161,
38.5724809284406));
#151934=CARTESIAN_POINT('Ctrl Pts',(-3.42065596391555,-6.12019111948548,
38.564116964367));
#151935=CARTESIAN_POINT('Ctrl Pts',(-3.58156720597369,-6.03025569278699,
38.5557542873685));
#151936=CARTESIAN_POINT('Ctrl Pts',(-3.73895023759169,-5.93395888306768,
38.54739161037));
#151937=CARTESIAN_POINT('Ctrl Pts',(-3.89229561965599,-5.83160881504468,
38.5390289333714));
#151938=CARTESIAN_POINT('Ctrl Pts',(-4.04563784461916,-5.7292608542225,
38.5306664285452));
#151939=CARTESIAN_POINT('Ctrl Pts',(-4.19494231265526,-5.62086006638377,
38.5223039237189));
#151940=CARTESIAN_POINT('Ctrl Pts',(-4.33972849282946,-5.50675795464302,
38.5139414188926));
#151941=CARTESIAN_POINT('Ctrl Pts',(-4.48453099108833,-5.39264298305669,
38.5055779715726));
#151942=CARTESIAN_POINT('Ctrl Pts',(-4.62481392843816,-5.27282561031236,
38.4972145242526));
#151943=CARTESIAN_POINT('Ctrl Pts',(-4.76012946020875,-5.14769794029844,
38.4888510769326));
#151944=CARTESIAN_POINT('Ctrl Pts',(-4.89552466956728,-5.02249659159589,
38.4804827049798));
#151945=CARTESIAN_POINT('Ctrl Pts',(-5.02594638639755,-4.89197892009062,
38.472114333027));
#151946=CARTESIAN_POINT('Ctrl Pts',(-5.15098254249893,-4.75657496623056,
38.4637459610742));
#151947=CARTESIAN_POINT('Ctrl Pts',(-5.27605616270038,-4.62113044180728,
38.4553750817385));
#151948=CARTESIAN_POINT('Ctrl Pts',(-5.39574078546048,-4.48079696082687,
38.4470042024027));
#151949=CARTESIAN_POINT('Ctrl Pts',(-5.50966388458783,-4.33603856548446,
38.438633323067));
#151950=CARTESIAN_POINT('Ctrl Pts',(-5.62368350952496,-4.1911575179193,
38.4302553511757));
#151951=CARTESIAN_POINT('Ctrl Pts',(-5.73193165718274,-4.04184432625667,
38.4218773792844));
#151952=CARTESIAN_POINT('Ctrl Pts',(-5.83407780103354,-3.88859393277155,
38.4134994073932));
#151953=CARTESIAN_POINT('Ctrl Pts',(-5.89899250723136,-3.7912020597869,
38.4081751380341));
#151954=CARTESIAN_POINT('Ctrl Pts',(-5.96144366641284,-3.69222065152121,
38.402850868675));
#151955=CARTESIAN_POINT('Ctrl Pts',(-6.02135593370038,-3.59178218746506,
38.3975265993159));
#151956=CARTESIAN_POINT('Ctrl Pts',(-6.10983380964514,-3.44345560319153,
38.3896637681265));
#151957=CARTESIAN_POINT('Ctrl Pts',(-6.19295614892028,-3.29164153103512,
38.3818009369372));
#151958=CARTESIAN_POINT('Ctrl Pts',(-6.27042519721691,-3.13678089904399,
38.3739381057479));
#151959=CARTESIAN_POINT('Ctrl Pts',(-6.34783472077548,-2.98203925700769,
38.3660813161065));
#151960=CARTESIAN_POINT('Ctrl Pts',(-6.41959942216686,-2.82425604909293,
38.3582245264651));
#151961=CARTESIAN_POINT('Ctrl Pts',(-6.48546554701166,-2.66389999831539,
38.3503677368237));
#151962=CARTESIAN_POINT('Ctrl Pts',(-6.55129452648003,-2.50363438075955,
38.3425153780397));
#151963=CARTESIAN_POINT('Ctrl Pts',(-6.61123140219707,-2.34079915821629,
38.3346630192557));
#151964=CARTESIAN_POINT('Ctrl Pts',(-6.66506908723199,-2.17588617002924,
38.3268106604717));
#151965=CARTESIAN_POINT('Ctrl Pts',(-6.71889406056143,-2.0110121197225,
38.3189601557213));
#151966=CARTESIAN_POINT('Ctrl Pts',(-6.76662258314972,-1.84406163967041,
38.3111096509708));
#151967=CARTESIAN_POINT('Ctrl Pts',(-6.80809633639841,-1.67554493727223,
38.3032591462203));
#151968=CARTESIAN_POINT('Ctrl Pts',(-6.84956341782725,-1.50705534390062,
38.2954099043687));
#151969=CARTESIAN_POINT('Ctrl Pts',(-6.88477764469847,-1.33700040094602,
38.287560662517));
#151970=CARTESIAN_POINT('Ctrl Pts',(-6.91363116893351,-1.16590335039021,
38.2797114206653));
#151971=CARTESIAN_POINT('Ctrl Pts',(-6.94249441448566,-0.99474865388884,
38.2718595342505));
#151972=CARTESIAN_POINT('Ctrl Pts',(-6.96499261329928,-0.822551525018547,
38.2640076478356));
#151973=CARTESIAN_POINT('Ctrl Pts',(-6.98106940870108,-0.649843422216428,
38.2561557614207));
#151974=CARTESIAN_POINT('Ctrl Pts',(-6.99287439946038,-0.523026011987538,
38.2503902189569));
#151975=CARTESIAN_POINT('Ctrl Pts',(-7.00121818321528,-0.395933280436445,
38.2446246764931));
#151976=CARTESIAN_POINT('Ctrl Pts',(-7.006096328775,-0.26877647669662,38.2388591340293));
#151977=CARTESIAN_POINT('Ctrl Pts',(-7.01426554795703,-0.0558324824022358,
38.2292038296696));
#151978=CARTESIAN_POINT('Ctrl Pts',(-7.01271064726137,0.157182581771933,
38.2195485253098));
#151979=CARTESIAN_POINT('Ctrl Pts',(-7.00150842649841,0.369467611803443,
38.2098932209501));
#151980=CARTESIAN_POINT('Ctrl Pts',(-6.99024414753392,0.582928661077378,
38.2001844280156));
#151981=CARTESIAN_POINT('Ctrl Pts',(-6.9692254208714,0.795651521071237,
38.190475635081));
#151982=CARTESIAN_POINT('Ctrl Pts',(-6.93858118165131,1.00683551195533,
38.1807668421465));
#151983=CARTESIAN_POINT('Ctrl Pts',(-6.90778947975004,1.21903573813549,
38.1710113296759));
#151984=CARTESIAN_POINT('Ctrl Pts',(-6.86727943479273,1.42968220986307,
38.1612558172054));
#151985=CARTESIAN_POINT('Ctrl Pts',(-6.81723238420865,1.63797716168356,
38.1515003047348));
#151986=CARTESIAN_POINT('Ctrl Pts',(-6.76713577934516,1.84647835755082,
38.1417351328061));
#151987=CARTESIAN_POINT('Ctrl Pts',(-6.7074833003174,2.05262334157793,38.1319699608774));
#151988=CARTESIAN_POINT('Ctrl Pts',(-6.63850685770685,2.25562702206706,
38.1222047889487));
#151989=CARTESIAN_POINT('Ctrl Pts',(-6.56962446291061,2.45835391164434,
38.1124529316103));
#151990=CARTESIAN_POINT('Ctrl Pts',(-6.49144352552242,2.65794802213785,
38.102701074272));
#151991=CARTESIAN_POINT('Ctrl Pts',(-6.40424455977526,2.85364296664614,
38.0929492169336));
#151992=CARTESIAN_POINT('Ctrl Pts',(-6.36621949545174,2.93898013537233,
38.0886967008701));
#151993=CARTESIAN_POINT('Ctrl Pts',(-6.32648020594196,3.02357604425985,
38.0844441848065));
#151994=CARTESIAN_POINT('Ctrl Pts',(-6.28505290906249,3.10736809740737,
38.080191668743));
#151995=CARTESIAN_POINT('Ctrl Pts',(-6.20679632874674,3.26565212824915,
38.0721586231441));
#151996=CARTESIAN_POINT('Ctrl Pts',(-6.12247476552803,3.42114328480809,
38.0641255775452));
#151997=CARTESIAN_POINT('Ctrl Pts',(-6.03231847320291,3.57334023014251,
38.0560925319463));
#151998=CARTESIAN_POINT('Ctrl Pts',(-5.94222013681373,3.72543933742053,
38.0480646502984));
#151999=CARTESIAN_POINT('Ctrl Pts',(-5.8462947233995,3.87424813462715,38.0400367686505));
#152000=CARTESIAN_POINT('Ctrl Pts',(-5.74481905402391,4.01928856876734,
38.0320088870026));
#152001=CARTESIAN_POINT('Ctrl Pts',(-5.64338920191287,4.16426351572245,
38.0239846300224));
#152002=CARTESIAN_POINT('Ctrl Pts',(-5.53641429326912,4.3054731876663,38.0159603730422));
#152003=CARTESIAN_POINT('Ctrl Pts',(-5.42421519844507,4.44246733735405,
38.007936116062));
#152004=CARTESIAN_POINT('Ctrl Pts',(-5.312029669635,4.57944492305299,37.9999128292962));
#152005=CARTESIAN_POINT('Ctrl Pts',(-5.19462143896387,4.71220771341635,
37.9918895425304));
#152006=CARTESIAN_POINT('Ctrl Pts',(-5.07235261321641,4.84033733635339,
37.9838662557646));
#152007=CARTESIAN_POINT('Ctrl Pts',(-4.9500938063094,4.96845646020989,37.9758436264357));
#152008=CARTESIAN_POINT('Ctrl Pts',(-4.82297545369296,5.0919429103813,37.9678209971067));
#152009=CARTESIAN_POINT('Ctrl Pts',(-4.69139736489977,5.2104143143431,37.9597983677778));
#152010=CARTESIAN_POINT('Ctrl Pts',(-4.55976981211172,5.32893025511929,
37.9517727225113));
#152011=CARTESIAN_POINT('Ctrl Pts',(-4.4236794485809,5.44242714026978,37.9437470772448));
#152012=CARTESIAN_POINT('Ctrl Pts',(-4.28356036646062,5.5505618769083,37.9357214319784));
#152013=CARTESIAN_POINT('Ctrl Pts',(-4.20093761721511,5.61432470702978,
37.930989022471));
#152014=CARTESIAN_POINT('Ctrl Pts',(-4.11691470232539,5.67622388780985,
37.9262566129637));
#152015=CARTESIAN_POINT('Ctrl Pts',(-4.03158551017522,5.73619602494939,
37.9215242034564));
#152016=CARTESIAN_POINT('Ctrl Pts',(-3.87417562978967,5.84682881890563,
37.9127941546218));
#152017=CARTESIAN_POINT('Ctrl Pts',(-3.71224031257984,5.95095695937954,
37.9040641057872));
#152018=CARTESIAN_POINT('Ctrl Pts',(-3.5463284714095,6.0482378372027,37.8953340569527));
#152019=CARTESIAN_POINT('Ctrl Pts',(-3.38036865662394,6.14554684391267,
37.8866014838136));
#152020=CARTESIAN_POINT('Ctrl Pts',(-3.21043025909689,6.23600449743395,
37.8778689106746));
#152021=CARTESIAN_POINT('Ctrl Pts',(-3.03708788225907,6.3193135511648,37.8691363375355));
#152022=CARTESIAN_POINT('Ctrl Pts',(-2.86128290024866,6.40380614299168,
37.8602797042551));
#152023=CARTESIAN_POINT('Ctrl Pts',(-2.68197674511356,6.48094534690321,
37.8514230709746));
#152024=CARTESIAN_POINT('Ctrl Pts',(-2.49979144674987,6.55047092087708,
37.8425664376942));
#152025=CARTESIAN_POINT('Ctrl Pts',(-2.32004377575778,6.61906624722028,
37.8338283055875));
#152026=CARTESIAN_POINT('Ctrl Pts',(-2.13749379631818,6.68025034069134,
37.8250901734809));
#152027=CARTESIAN_POINT('Ctrl Pts',(-1.95275672189837,6.73382266974567,
37.8163520413742));
#152028=CARTESIAN_POINT('Ctrl Pts',(-1.76426171158982,6.78848477127057,
37.8074361575068));
#152029=CARTESIAN_POINT('Ctrl Pts',(-1.5734899565185,6.83522202693568,37.7985202736395));
#152030=CARTESIAN_POINT('Ctrl Pts',(-1.38110971377457,6.87387536408812,
37.7896043897722));
#152031=CARTESIAN_POINT('Ctrl Pts',(-1.18872947103065,6.91252870124056,
37.7806885059048));
#152032=CARTESIAN_POINT('Ctrl Pts',(-0.994741038299275,6.94309806627354,
37.7717726220374));
#152033=CARTESIAN_POINT('Ctrl Pts',(-0.799823146441631,6.96547984685307,
37.7628567381701));
#152034=CARTESIAN_POINT('Ctrl Pts',(-0.608735440415276,6.98742181978826,
37.7541160536738));
#152035=CARTESIAN_POINT('Ctrl Pts',(-0.416734168982142,7.001497328095,37.7453753691775));
#152036=CARTESIAN_POINT('Ctrl Pts',(-0.224464276876075,7.00765598120417,
37.7366346846812));
#152037=CARTESIAN_POINT('Ctrl Pts',(-0.0322289773166385,7.01381352626936,
37.7278955727793));
#152038=CARTESIAN_POINT('Ctrl Pts',(0.160274572842149,7.01205705195769,
37.7191564608773));
#152039=CARTESIAN_POINT('Ctrl Pts',(0.352399506944261,7.00238824616327,
37.7104173489753));
#152040=CARTESIAN_POINT('Ctrl Pts',(0.547013696080467,6.9925941670741,37.701565009301));
#152041=CARTESIAN_POINT('Ctrl Pts',(0.741239103951189,6.97468128782051,
37.6927126696267));
#152042=CARTESIAN_POINT('Ctrl Pts',(0.934405330218199,6.94870586809946,
37.6838603299524));
#152043=CARTESIAN_POINT('Ctrl Pts',(1.12500308051652,6.9230758360925,37.6751256973025));
#152044=CARTESIAN_POINT('Ctrl Pts',(1.31456936496239,6.88959639388524,37.6663910646527));
#152045=CARTESIAN_POINT('Ctrl Pts',(1.50246617357085,6.84837367261567,37.6576564320028));
#152046=CARTESIAN_POINT('Ctrl Pts',(1.69416109970754,6.80631768152435,37.6487452388163));
#152047=CARTESIAN_POINT('Ctrl Pts',(1.88411804984048,6.75620207544141,37.6398340456297));
#152048=CARTESIAN_POINT('Ctrl Pts',(2.07167033626311,6.69819442688457,37.6309228524432));
#152049=CARTESIAN_POINT('Ctrl Pts',(2.25922262268577,6.64018677832772,37.6220116592566));
#152050=CARTESIAN_POINT('Ctrl Pts',(2.44436995182194,6.57428716399278,37.6131004660701));
#152051=CARTESIAN_POINT('Ctrl Pts',(2.62646095606413,6.5007176072162,37.6041892728836));
#152052=CARTESIAN_POINT('Ctrl Pts',(2.790457105859,6.43445884773664,37.5961636080312));
#152053=CARTESIAN_POINT('Ctrl Pts',(2.95204935192554,6.36194783750325,37.5881379431789));
#152054=CARTESIAN_POINT('Ctrl Pts',(3.1107253513043,6.28339194633382,37.5801122783266));
#152055=CARTESIAN_POINT('Ctrl Pts',(3.26935099081321,6.20486098687726,37.5720891606234));
#152056=CARTESIAN_POINT('Ctrl Pts',(3.42506189818271,6.12028912847709,37.5640660429202));
#152057=CARTESIAN_POINT('Ctrl Pts',(3.57736720696016,6.02993121263138,37.556042925217));
#152058=CARTESIAN_POINT('Ctrl Pts',(3.72965330870442,5.93958469171012,37.5480208192992));
#152059=CARTESIAN_POINT('Ctrl Pts',(3.87853435245044,5.84345375425896,37.5399987133815));
#152060=CARTESIAN_POINT('Ctrl Pts',(4.02354555772512,5.74183835608514,37.5319766074637));
#152061=CARTESIAN_POINT('Ctrl Pts',(4.168610649654,5.64018519728577,37.5239515205042));
#152062=CARTESIAN_POINT('Ctrl Pts',(4.30980272814773,5.53304371449926,37.5159264335448));
#152063=CARTESIAN_POINT('Ctrl Pts',(4.44668704903017,5.42075648323068,37.5079013465853));
#152064=CARTESIAN_POINT('Ctrl Pts',(4.58359832859468,5.30844713755373,37.4998746791251));
#152065=CARTESIAN_POINT('Ctrl Pts',(4.71619988259121,5.19099026376917,37.4918480116649));
#152066=CARTESIAN_POINT('Ctrl Pts',(4.84409154499778,5.06876747012339,37.4838213442047));
#152067=CARTESIAN_POINT('Ctrl Pts',(4.97208587838034,4.94644655644947,37.4757882329642));
#152068=CARTESIAN_POINT('Ctrl Pts',(5.09536250986243,4.81935234124115,37.4677551217237));
#152069=CARTESIAN_POINT('Ctrl Pts',(5.2135590791038,4.68790233379434,37.4597220104831));
#152070=CARTESIAN_POINT('Ctrl Pts',(5.28320479143095,4.6104472142185,37.4549886095211));
#152071=CARTESIAN_POINT('Ctrl Pts',(5.3510874609904,4.53148040746574,37.4502552085592));
#152072=CARTESIAN_POINT('Ctrl Pts',(5.41713974441532,4.45109239984702,37.4455218075972));
#152073=CARTESIAN_POINT('Ctrl Pts',(5.55327203889334,4.28541449503861,37.4357663729592));
#152074=CARTESIAN_POINT('Ctrl Pts',(5.68170806712042,4.1136009511796,37.4260109383213));
#152075=CARTESIAN_POINT('Ctrl Pts',(5.8019809021497,3.93632368760373,37.4162555036833));
#152076=CARTESIAN_POINT('Ctrl Pts',(5.92237218882039,3.75887183112954,37.4064904613293));
#152077=CARTESIAN_POINT('Ctrl Pts',(6.03458419037899,3.5759455307003,37.3967254189754));
#152078=CARTESIAN_POINT('Ctrl Pts',(6.13819351279977,3.38824541052192,37.3869603766214));
#152079=CARTESIAN_POINT('Ctrl Pts',(6.24164532400683,3.20083063989562,37.3772101794921));
#152080=CARTESIAN_POINT('Ctrl Pts',(6.33652057679012,3.00865658784191,37.3674599823628));
#152081=CARTESIAN_POINT('Ctrl Pts',(6.42244268309691,2.81244671857709,37.3577097852336));
#152082=CARTESIAN_POINT('Ctrl Pts',(6.47542855231128,2.69144933014814,37.3516970989516));
#152083=CARTESIAN_POINT('Ctrl Pts',(6.52501054568903,2.56891768540196,37.3456844126697));
#152084=CARTESIAN_POINT('Ctrl Pts',(6.57110895151815,2.44502632087632,37.3396717263878));
#152085=CARTESIAN_POINT('Origin',(0.,0.,50.));
#152086=CARTESIAN_POINT('',(6.57110895151813,2.44502632087638,35.339859805629));
#152087=CARTESIAN_POINT('',(6.57110895151814,2.44502632087637,35.887150555484));
#152088=CARTESIAN_POINT('',(6.57110895151814,2.44502632087636,50.));
#152089=CARTESIAN_POINT('',(7.01124977383073,0.0017808589384362,37.7735343569413));
#152090=CARTESIAN_POINT('Ctrl Pts',(6.57110895151814,2.44502632087637,35.887150555484));
#152091=CARTESIAN_POINT('Ctrl Pts',(6.50697260986517,2.61739538093721,35.8955166861323));
#152092=CARTESIAN_POINT('Ctrl Pts',(6.43598672426158,2.7874094371462,35.9038828167805));
#152093=CARTESIAN_POINT('Ctrl Pts',(6.35834255681135,2.95450613347506,35.9122489474287));
#152094=CARTESIAN_POINT('Ctrl Pts',(6.28080917678768,3.12136440606158,35.9206031407723));
#152095=CARTESIAN_POINT('Ctrl Pts',(6.19663660155576,3.28531332604793,35.9289573341158));
#152096=CARTESIAN_POINT('Ctrl Pts',(6.10606457648596,3.4458093316786,35.9373115274593));
#152097=CARTESIAN_POINT('Ctrl Pts',(6.01556812576292,3.60617141758325,35.9456587499672));
#152098=CARTESIAN_POINT('Ctrl Pts',(5.91868302593814,3.76308604655054,35.9540059724751));
#152099=CARTESIAN_POINT('Ctrl Pts',(5.81569599752269,3.91603200023935,35.9623531949829));
#152100=CARTESIAN_POINT('Ctrl Pts',(5.71280280293965,4.06883860137854,35.9706928121458));
#152101=CARTESIAN_POINT('Ctrl Pts',(5.60381895001064,4.21768346804293,35.9790324293087));
#152102=CARTESIAN_POINT('Ctrl Pts',(5.48907577094334,4.36207218456352,35.9873720464716));
#152103=CARTESIAN_POINT('Ctrl Pts',(5.38980949117741,4.48698532402578,35.9945867914103));
#152104=CARTESIAN_POINT('Ctrl Pts',(5.28623355591924,4.60856365262259,36.0018015363491));
#152105=CARTESIAN_POINT('Ctrl Pts',(5.17858847666944,4.72650483463273,36.0090162812878));
#152106=CARTESIAN_POINT('Ctrl Pts',(5.05417963327136,4.86281321161698,36.0173545915896));
#152107=CARTESIAN_POINT('Ctrl Pts',(4.92443695717153,4.99415069566618,36.0256929018913));
#152108=CARTESIAN_POINT('Ctrl Pts',(4.78979374023273,5.12010766376327,36.0340312121931));
#152109=CARTESIAN_POINT('Ctrl Pts',(4.6550658103508,5.24614387971047,36.0423747686768));
#152110=CARTESIAN_POINT('Ctrl Pts',(4.51543142896972,5.36679260359018,36.0507183251604));
#152111=CARTESIAN_POINT('Ctrl Pts',(4.37135764285955,5.48168394936387,36.0590618816441));
#152112=CARTESIAN_POINT('Ctrl Pts',(4.22717424604053,5.59666270397291,36.0674117858691));
#152113=CARTESIAN_POINT('Ctrl Pts',(4.07854496340376,5.70587513937817,36.0757616900942));
#152114=CARTESIAN_POINT('Ctrl Pts',(3.92596687288046,5.80899394693653,36.0841115943193));
#152115=CARTESIAN_POINT('Ctrl Pts',(3.77315992651249,5.91226742507521,36.0924740227828));
#152116=CARTESIAN_POINT('Ctrl Pts',(3.61639260810419,6.00942882716261,36.1008364512463));
#152117=CARTESIAN_POINT('Ctrl Pts',(3.45618901935108,6.10019540875676,36.1091988797098));
#152118=CARTESIAN_POINT('Ctrl Pts',(3.29584843469025,6.19103960815168,36.1175684591896));
#152119=CARTESIAN_POINT('Ctrl Pts',(3.13206600719092,6.27547792630944,36.1259380386695));
#152120=CARTESIAN_POINT('Ctrl Pts',(2.96538749692936,6.35327502596535,36.1343076181493));
#152121=CARTESIAN_POINT('Ctrl Pts',(2.79845190537391,6.43119211816865,36.1426901066857));
#152122=CARTESIAN_POINT('Ctrl Pts',(2.62861160649927,6.50244739624754,36.1510725952221));
#152123=CARTESIAN_POINT('Ctrl Pts',(2.45643057633427,6.56685429914126,36.1594550837585));
#152124=CARTESIAN_POINT('Ctrl Pts',(2.40009012189321,6.58792929314436,36.1621979713637));
#152125=CARTESIAN_POINT('Ctrl Pts',(2.34349914850339,6.60827143021347,36.1649408589689));
#152126=CARTESIAN_POINT('Ctrl Pts',(2.28667769040872,6.62787535358708,36.1676837465741));
#152127=CARTESIAN_POINT('Ctrl Pts',(2.11287406792392,6.68783919491568,36.176073601707));
#152128=CARTESIAN_POINT('Ctrl Pts',(1.93656216285418,6.74101356882624,36.1844634568398));
#152129=CARTESIAN_POINT('Ctrl Pts',(1.7582991684868,6.78719460429702,36.1928533119726));
#152130=CARTESIAN_POINT('Ctrl Pts',(1.58020067271138,6.83333302455573,36.2012354250648));
#152131=CARTESIAN_POINT('Ctrl Pts',(1.40015499349404,6.87249088908847,36.2096175381569));
#152132=CARTESIAN_POINT('Ctrl Pts',(1.21873558913368,6.90451375016945,36.2179996512491));
#152133=CARTESIAN_POINT('Ctrl Pts',(1.03745692778057,6.93651176829725,36.226375261598));
#152134=CARTESIAN_POINT('Ctrl Pts',(0.85480698856528,6.96138576164031,36.2347508719469));
#152135=CARTESIAN_POINT('Ctrl Pts',(0.671371010187525,6.97903199084084,
36.2431264822958));
#152136=CARTESIAN_POINT('Ctrl Pts',(0.488050415764371,6.99666712030114,
36.2514968242614));
#152137=CARTESIAN_POINT('Ctrl Pts',(0.303945094401395,7.00708351927838,
36.2598671662271));
#152138=CARTESIAN_POINT('Ctrl Pts',(0.119647482316103,7.01022902924544,
36.2682375081927));
#152139=CARTESIAN_POINT('Ctrl Pts',(-0.0645612197947758,7.01337302173646,
36.276603812087));
#152140=CARTESIAN_POINT('Ctrl Pts',(-0.248961699547538,7.00925311447268,
36.2849701159814));
#152141=CARTESIAN_POINT('Ctrl Pts',(-0.432958966321623,6.99786918254276,
36.2933364198758));
#152142=CARTESIAN_POINT('Ctrl Pts',(-0.616904774217498,6.98648843437953,
36.3017003839494));
#152143=CARTESIAN_POINT('Ctrl Pts',(-0.800447266164052,6.9678477312557,
36.3100643480231));
#152144=CARTESIAN_POINT('Ctrl Pts',(-0.982993461921201,6.9419990216306,
36.3184283120968));
#152145=CARTESIAN_POINT('Ctrl Pts',(-1.16551156685233,6.91615428969236,
36.3267909890953));
#152146=CARTESIAN_POINT('Ctrl Pts',(-1.34703335595318,6.88310380882598,
36.3351536660939));
#152147=CARTESIAN_POINT('Ctrl Pts',(-1.5269725464287,6.8429512204131,36.3435163430925));
#152148=CARTESIAN_POINT('Ctrl Pts',(-1.70690803228521,6.8027994586686,36.3518788479189));
#152149=CARTESIAN_POINT('Ctrl Pts',(-1.88526066381444,6.7555459529077,36.3602413527452));
#152150=CARTESIAN_POINT('Ctrl Pts',(-2.06145547495954,6.70134522967287,
36.3686038575716));
#152151=CARTESIAN_POINT('Ctrl Pts',(-2.2376701440898,6.64713839776123,36.3769673048916));
#152152=CARTESIAN_POINT('Ctrl Pts',(-2.41172619401986,6.58598288446914,
36.3853307522116));
#152153=CARTESIAN_POINT('Ctrl Pts',(-2.58306450104343,6.51808287351037,
36.3936941995317));
#152154=CARTESIAN_POINT('Ctrl Pts',(-2.75450369687716,6.45014288111702,
36.4020625714845));
#152155=CARTESIAN_POINT('Ctrl Pts',(-2.92322164584411,6.3754505756709,36.4104309434374));
#152156=CARTESIAN_POINT('Ctrl Pts',(-3.08867890971672,6.29425842773961,
36.4187993153902));
#152157=CARTESIAN_POINT('Ctrl Pts',(-3.25418574890983,6.21304195251884,
36.427170194726));
#152158=CARTESIAN_POINT('Ctrl Pts',(-3.4164296621465,6.12532190106307,36.4355410740618));
#152159=CARTESIAN_POINT('Ctrl Pts',(-3.57489582796128,6.03139671898019,
36.4439119533976));
#152160=CARTESIAN_POINT('Ctrl Pts',(-3.73349626044479,5.93739195510619,
36.4522899252889));
#152161=CARTESIAN_POINT('Ctrl Pts',(-3.88831226944412,5.83717172743768,
36.4606678971803));
#152162=CARTESIAN_POINT('Ctrl Pts',(-4.03885706119026,5.73107845014999,
36.4690458690716));
#152163=CARTESIAN_POINT('Ctrl Pts',(-4.13452950222651,5.66365530851938,
36.4743701384301));
#152164=CARTESIAN_POINT('Ctrl Pts',(-4.22847752743682,5.59386107507974,
36.4796944077886));
#152165=CARTESIAN_POINT('Ctrl Pts',(-4.32058308092259,5.52179213691945,
36.4850186771471));
#152166=CARTESIAN_POINT('Ctrl Pts',(-4.45660370082115,5.41536140312544,
36.4928815083364));
#152167=CARTESIAN_POINT('Ctrl Pts',(-4.58888712415335,5.30374629795429,
36.5007443395257));
#152168=CARTESIAN_POINT('Ctrl Pts',(-4.71699660523404,5.18725067725771,
36.5086071707149));
#152169=CARTESIAN_POINT('Ctrl Pts',(-4.84500765108876,5.0708445680684,36.5164639603563));
#152170=CARTESIAN_POINT('Ctrl Pts',(-4.96885085225944,4.94956565568369,
36.5243207499977));
#152171=CARTESIAN_POINT('Ctrl Pts',(-5.08812047633207,4.82375958986664,
36.532177539639));
#152172=CARTESIAN_POINT('Ctrl Pts',(-5.20732283798267,4.69802447271534,
36.540029898423));
#152173=CARTESIAN_POINT('Ctrl Pts',(-5.32195649181786,4.56776755666268,
36.5478822572069));
#152174=CARTESIAN_POINT('Ctrl Pts',(-5.43165089414721,4.43337288377707,
36.5557346159909));
#152175=CARTESIAN_POINT('Ctrl Pts',(-5.54131939634823,4.29900994304188,
36.5635851207413));
#152176=CARTESIAN_POINT('Ctrl Pts',(-5.64605072073049,4.16051147969021,
36.5714356254917));
#152177=CARTESIAN_POINT('Ctrl Pts',(-5.74551318439922,4.01829625717103,
36.5792861302421));
#152178=CARTESIAN_POINT('Ctrl Pts',(-5.84495964769236,3.87610391259889,
36.5871353720937));
#152179=CARTESIAN_POINT('Ctrl Pts',(-5.93913872138399,3.73019631349701,
36.5949846139453));
#152180=CARTESIAN_POINT('Ctrl Pts',(-6.02776109465621,3.58102258415791,
36.6028338557969));
#152181=CARTESIAN_POINT('Ctrl Pts',(-6.11641332654064,3.43179859526953,
36.6106857422118));
#152182=CARTESIAN_POINT('Ctrl Pts',(-6.19950492344001,3.27930660641339,
36.6185376286266));
#152183=CARTESIAN_POINT('Ctrl Pts',(-6.27679163657645,3.12402197711604,
36.6263895150414));
#152184=CARTESIAN_POINT('Ctrl Pts',(-6.33354230806458,3.00999840661106,
36.6321550575054));
#152185=CARTESIAN_POINT('Ctrl Pts',(-6.3871640476193,2.89446966478179,36.6379205999694));
#152186=CARTESIAN_POINT('Ctrl Pts',(-6.43757652936217,2.77763118341966,
36.6436861424334));
#152187=CARTESIAN_POINT('Ctrl Pts',(-6.52200013005698,2.58196683690696,
36.6533414467934));
#152188=CARTESIAN_POINT('Ctrl Pts',(-6.59737977147376,2.38272892649935,
36.6629967511533));
#152189=CARTESIAN_POINT('Ctrl Pts',(-6.66349814332539,2.18069233419095,
36.6726520555133));
#152190=CARTESIAN_POINT('Ctrl Pts',(-6.72998279855346,1.9775364970626,36.6823608484481));
#152191=CARTESIAN_POINT('Ctrl Pts',(-6.78710332593054,1.77155094565415,
36.6920696413829));
#152192=CARTESIAN_POINT('Ctrl Pts',(-6.83469119428504,1.56352897039438,
36.7017784343178));
#152193=CARTESIAN_POINT('Ctrl Pts',(-6.88250805950276,1.35450597572647,
36.7115339467886));
#152194=CARTESIAN_POINT('Ctrl Pts',(-6.92070031477104,1.14342695868886,
36.7212894592593));
#152195=CARTESIAN_POINT('Ctrl Pts',(-6.94914935517812,0.931101391862117,
36.7310449717301));
#152196=CARTESIAN_POINT('Ctrl Pts',(-6.97762656451199,0.71856559005865,
36.7408101436591));
#152197=CARTESIAN_POINT('Ctrl Pts',(-6.9963412682042,0.504780809117193,
36.7505753155881));
#152198=CARTESIAN_POINT('Ctrl Pts',(-7.00522660158058,0.290562941559598,
36.7603404875171));
#152199=CARTESIAN_POINT('Ctrl Pts',(-7.01409982000649,0.0766371552045,36.7700923448557));
#152200=CARTESIAN_POINT('Ctrl Pts',(-7.01317045261364,-0.13772049964646,
36.7798442021943));
#152201=CARTESIAN_POINT('Ctrl Pts',(-7.00242371329551,-0.351694045978458,
36.789596059533));
#152202=CARTESIAN_POINT('Ctrl Pts',(-6.99773735663737,-0.445002008871643,
36.7938485755953));
#152203=CARTESIAN_POINT('Ctrl Pts',(-6.99118480247846,-0.538236889470219,
36.7981010916576));
#152204=CARTESIAN_POINT('Ctrl Pts',(-6.98276792694817,-0.631330848988084,
36.80235360772));
#152205=CARTESIAN_POINT('Ctrl Pts',(-6.96686836444377,-0.807186274532689,
36.8103866533187));
#152206=CARTESIAN_POINT('Ctrl Pts',(-6.94430472223209,-0.982624320124002,
36.8184196989175));
#152207=CARTESIAN_POINT('Ctrl Pts',(-6.91511093451619,-1.15709434612508,
36.8264527445163));
#152208=CARTESIAN_POINT('Ctrl Pts',(-6.8859359136911,-1.33145221607574,
36.834480626164));
#152209=CARTESIAN_POINT('Ctrl Pts',(-6.85013929144488,-1.50484294506531,
36.8425085078118));
#152210=CARTESIAN_POINT('Ctrl Pts',(-6.80780683283171,-1.67672081437247,
36.8505363894595));
#152211=CARTESIAN_POINT('Ctrl Pts',(-6.7654934877409,-1.84852107912734,
36.8585606464396));
#152212=CARTESIAN_POINT('Ctrl Pts',(-6.71665026953412,-2.01880948907865,
36.8665849034197));
#152213=CARTESIAN_POINT('Ctrl Pts',(-6.66141405653836,-2.18705037204293,
36.8746091603997));
#152214=CARTESIAN_POINT('Ctrl Pts',(-6.60618452216337,-2.35527091297083,
36.8826324471654));
#152215=CARTESIAN_POINT('Ctrl Pts',(-6.54456363959391,-2.52144406954191,
36.890655733931));
#152216=CARTESIAN_POINT('Ctrl Pts',(-6.47673824465091,-2.68504902614017,
36.8986790206967));
#152217=CARTESIAN_POINT('Ctrl Pts',(-6.408918407394,-2.84864057677166,36.9067016500256));
#152218=CARTESIAN_POINT('Ctrl Pts',(-6.33489521457951,-3.00966400945426,
36.9147242793545));
#152219=CARTESIAN_POINT('Ctrl Pts',(-6.25490365127451,-3.16761848646153,
36.9227469086833));
#152220=CARTESIAN_POINT('Ctrl Pts',(-6.17488201683647,-3.32563234310704,
36.9307725539497));
#152221=CARTESIAN_POINT('Ctrl Pts',(-6.08888769818116,-3.48057461346246,
36.9387981992161));
#152222=CARTESIAN_POINT('Ctrl Pts',(-5.99720182275231,-3.63196873054771,
36.9468238444824));
#152223=CARTESIAN_POINT('Ctrl Pts',(-5.94313824353517,-3.72123992748797,
36.9515562539904));
#152224=CARTESIAN_POINT('Ctrl Pts',(-5.88709656573008,-3.80927792587232,
36.9562886634983));
#152225=CARTESIAN_POINT('Ctrl Pts',(-5.8291414931858,-3.89598973496076,
36.9610210730063));
#152226=CARTESIAN_POINT('Ctrl Pts',(-5.72222965204426,-4.05595017934251,
36.9697511218411));
#152227=CARTESIAN_POINT('Ctrl Pts',(-5.60875089323653,-4.21147602253064,
36.9784811706758));
#152228=CARTESIAN_POINT('Ctrl Pts',(-5.48909361083986,-4.36204973538095,
36.9872112195106));
#152229=CARTESIAN_POINT('Ctrl Pts',(-5.36940172939094,-4.51266698680788,
36.9959437926498));
#152230=CARTESIAN_POINT('Ctrl Pts',(-5.24352792878021,-4.65832903524911,
37.0046763657891));
#152231=CARTESIAN_POINT('Ctrl Pts',(-5.11190092571569,-4.79855139476146,
37.0134089389283));
#152232=CARTESIAN_POINT('Ctrl Pts',(-4.97840395095815,-4.94076583672582,
37.0222655722087));
#152233=CARTESIAN_POINT('Ctrl Pts',(-4.83898925941136,-5.07738464154304,
37.031122205489));
#152234=CARTESIAN_POINT('Ctrl Pts',(-4.69414314873293,-5.20794073139314,
37.0399788387694));
#152235=CARTESIAN_POINT('Ctrl Pts',(-4.55123506953378,-5.33674998930722,
37.0487169708763));
#152236=CARTESIAN_POINT('Ctrl Pts',(-4.40304023446243,-5.45965759341299,
37.0574551029831));
#152237=CARTESIAN_POINT('Ctrl Pts',(-4.2500601198248,-5.57625461581291,
37.0661932350899));
#152238=CARTESIAN_POINT('Ctrl Pts',(-4.09396807184302,-5.69522346387589,
37.0751091189571));
#152239=CARTESIAN_POINT('Ctrl Pts',(-3.93289420716951,-5.80762205691641,
37.0840250028242));
#152240=CARTESIAN_POINT('Ctrl Pts',(-3.76740442870148,-5.91306100366811,
37.0929408866914));
#152241=CARTESIAN_POINT('Ctrl Pts',(-3.60191465023345,-6.0184999504198,
37.1018567705585));
#152242=CARTESIAN_POINT('Ctrl Pts',(-3.43200921628418,-6.1169790935156,
37.1107726544257));
#152243=CARTESIAN_POINT('Ctrl Pts',(-3.25828380186181,-6.20815699133204,
37.1196885382928));
#152244=CARTESIAN_POINT('Ctrl Pts',(-3.08797213573322,-6.29754322041576,
37.128429222789));
#152245=CARTESIAN_POINT('Ctrl Pts',(-2.91397113395903,-6.37992197705981,
37.1371699072851));
#152246=CARTESIAN_POINT('Ctrl Pts',(-2.73686415548148,-6.45501364498486,
37.1459105917812));
#152247=CARTESIAN_POINT('Ctrl Pts',(-2.55978904149134,-6.53009180267147,
37.154649703683));
#152248=CARTESIAN_POINT('Ctrl Pts',(-2.37960931878053,-6.59788538310423,
37.1633888155848));
#152249=CARTESIAN_POINT('Ctrl Pts',(-2.19692892241399,-6.6581626498878,
37.1721279274866));
#152250=CARTESIAN_POINT('Ctrl Pts',(-2.01188163858686,-6.71922089541757,
37.180980267161));
#152251=CARTESIAN_POINT('Ctrl Pts',(-1.82426869335081,-6.77256658958483,
37.1898326068354));
#152252=CARTESIAN_POINT('Ctrl Pts',(-1.63473565426649,-6.81801040650203,
37.1986849465098));
#152253=CARTESIAN_POINT('Ctrl Pts',(-1.44772278170734,-6.86284997000397,
37.2074195791594));
#152254=CARTESIAN_POINT('Ctrl Pts',(-1.25884083652015,-6.89999643726298,
37.2161542118091));
#152255=CARTESIAN_POINT('Ctrl Pts',(-1.06872316363582,-6.92931867949572,
37.2248888444588));
#152256=CARTESIAN_POINT('Ctrl Pts',(-0.874762481001771,-6.95923363707719,
37.2338000376455));
#152257=CARTESIAN_POINT('Ctrl Pts',(-0.679515864651398,-6.98100461965341,
37.2427112308323));
#152258=CARTESIAN_POINT('Ctrl Pts',(-0.483665567513508,-6.99454746079415,
37.251622424019));
#152259=CARTESIAN_POINT('Ctrl Pts',(-0.287815270375584,-7.00809030193489,
37.2605336172057));
#152260=CARTESIAN_POINT('Ctrl Pts',(-0.0913615939282992,-7.01340496728706,
37.2694448103925));
#152261=CARTESIAN_POINT('Ctrl Pts',(0.105007858586513,-7.01046360179804,
37.2783560035792));
#152262=CARTESIAN_POINT('Ctrl Pts',(0.2818635702861,-7.00781452741163,37.2863816684316));
#152263=CARTESIAN_POINT('Ctrl Pts',(0.458732234533989,-6.99846700358845,
37.294407333284));
#152264=CARTESIAN_POINT('Ctrl Pts',(0.635061200238224,-6.98242965123545,
37.3024329981364));
#152265=CARTESIAN_POINT('Ctrl Pts',(0.811334203453862,-6.96639738874471,
37.3104561158397));
#152266=CARTESIAN_POINT('Ctrl Pts',(0.987067484512773,-6.94367955795455,
37.3184792335429));
#152267=CARTESIAN_POINT('Ctrl Pts',(1.16171130125491,-6.91433680225636,
37.3265023512461));
#152268=CARTESIAN_POINT('Ctrl Pts',(1.33633309388306,-6.8849977469365,37.334524457164));
#152269=CARTESIAN_POINT('Ctrl Pts',(1.50986533455861,-6.84903549215509,
37.3425465630818));
#152270=CARTESIAN_POINT('Ctrl Pts',(1.68176633951627,-6.80656216762692,
37.3505686689997));
#152271=CARTESIAN_POINT('Ctrl Pts',(1.85373122346835,-6.7640730598678,37.3585937559592));
#152272=CARTESIAN_POINT('Ctrl Pts',(2.02406330383963,-6.71506813399237,
37.3666188429188));
#152273=CARTESIAN_POINT('Ctrl Pts',(2.19223353943437,-6.65971010413209,
37.3746439298783));
#152274=CARTESIAN_POINT('Ctrl Pts',(2.36043689531531,-6.6043411717849,37.3826705973385));
#152275=CARTESIAN_POINT('Ctrl Pts',(2.52647721279758,-6.54261676581433,
37.3906972647988));
#152276=CARTESIAN_POINT('Ctrl Pts',(2.68984362313821,-6.47474847739762,
37.398723932259));
#152277=CARTESIAN_POINT('Ctrl Pts',(2.85334118345751,-6.40682570455806,
37.4067570434996));
#152278=CARTESIAN_POINT('Ctrl Pts',(3.01416021444236,-6.33274934744867,
37.4147901547402));
#152279=CARTESIAN_POINT('Ctrl Pts',(3.17181215961908,-6.25277811749246,
37.4228232659808));
#152280=CARTESIAN_POINT('Ctrl Pts',(3.26470641273613,-6.20565616368906,
37.4275566669424));
#152281=CARTESIAN_POINT('Ctrl Pts',(3.35650152545842,-6.15648838283711,
37.432290067904));
#152282=CARTESIAN_POINT('Ctrl Pts',(3.44710205084209,-6.10533488136239,
37.4370234688657));
#152283=CARTESIAN_POINT('Ctrl Pts',(3.63374195281166,-5.99995707631974,
37.44677442216));
#152284=CARTESIAN_POINT('Ctrl Pts',(3.81542117581783,-5.886088554131,37.4565253754544));
#152285=CARTESIAN_POINT('Ctrl Pts',(3.99146280133737,-5.76418695637469,
37.4662763287487));
#152286=CARTESIAN_POINT('Ctrl Pts',(4.16775804784398,-5.64210973649799,
37.4760413301206));
#152287=CARTESIAN_POINT('Ctrl Pts',(4.33839941867826,-5.51197631333704,
37.4858063314925));
#152288=CARTESIAN_POINT('Ctrl Pts',(4.50273931168685,-5.37428741820624,
37.4955713328643));
#152289=CARTESIAN_POINT('Ctrl Pts',(4.66680528414372,-5.23682802193557,
37.5053200580021));
#152290=CARTESIAN_POINT('Ctrl Pts',(4.82459074146358,-5.09183834714575,
37.5150687831399));
#152291=CARTESIAN_POINT('Ctrl Pts',(4.97548376543074,-4.93985706902894,
37.5248175082777));
#152292=CARTESIAN_POINT('Ctrl Pts',(5.12596264655483,-4.78829292059088,
37.5345394769451));
#152293=CARTESIAN_POINT('Ctrl Pts',(5.26958683100278,-4.62977550534586,
37.5442614456124));
#152294=CARTESIAN_POINT('Ctrl Pts',(5.4057822498977,-4.46487903858447,37.5539834142797));
#152295=CARTESIAN_POINT('Ctrl Pts',(5.54107649927796,-4.3010736486752,37.5636410552196));
#152296=CARTESIAN_POINT('Ctrl Pts',(5.66903991458593,-4.13097336285851,
37.5732986961594));
#152297=CARTESIAN_POINT('Ctrl Pts',(5.78914287372278,-3.95518031828194,
37.5829563370993));
#152298=CARTESIAN_POINT('Ctrl Pts',(5.8419322591425,-3.87791322302506,37.5872012027836));
#152299=CARTESIAN_POINT('Ctrl Pts',(5.89320351584413,-3.79954685122038,
37.5914460684679));
#152300=CARTESIAN_POINT('Ctrl Pts',(5.94291376581705,-3.7201347468287,37.5956909341521));
#152301=CARTESIAN_POINT('Ctrl Pts',(6.03486420826598,-3.57324395190023,
37.6035427811659));
#152302=CARTESIAN_POINT('Ctrl Pts',(6.12143268792315,-3.42283350555081,
37.6113946281797));
#152303=CARTESIAN_POINT('Ctrl Pts',(6.2023340012452,-3.26935459984042,37.6192464751936));
#152304=CARTESIAN_POINT('Ctrl Pts',(6.28321237160885,-3.11591921950686,
37.627096095487));
#152305=CARTESIAN_POINT('Ctrl Pts',(6.35842659485689,-2.95941744788961,
37.6349457157805));
#152306=CARTESIAN_POINT('Ctrl Pts',(6.4277366444663,-2.80032644380706,37.642795336074));
#152307=CARTESIAN_POINT('Ctrl Pts',(6.49704116055462,-2.64124814110666,
37.6506443296757));
#152308=CARTESIAN_POINT('Ctrl Pts',(6.56044228970657,-2.47958136747388,
37.6584933232774));
#152309=CARTESIAN_POINT('Ctrl Pts',(6.61774763083798,-2.31582444434768,
37.666342316879));
#152310=CARTESIAN_POINT('Ctrl Pts',(6.67508198398568,-2.15198461588623,
37.6741952841964));
#152311=CARTESIAN_POINT('Ctrl Pts',(6.72631425673012,-1.98605288415579,
37.6820482515137));
#152312=CARTESIAN_POINT('Ctrl Pts',(6.77130144301954,-1.81854428878197,
37.689901218831));
#152313=CARTESIAN_POINT('Ctrl Pts',(6.81630005454276,-1.65099315185304,
37.6977561805382));
#152314=CARTESIAN_POINT('Ctrl Pts',(6.8550503346414,-1.48186472532357,37.7056111422453));
#152315=CARTESIAN_POINT('Ctrl Pts',(6.88746030029639,-1.31168486091027,
37.7134661039525));
#152316=CARTESIAN_POINT('Ctrl Pts',(6.91990243555138,-1.14133607875651,
37.7213288623657));
#152317=CARTESIAN_POINT('Ctrl Pts',(6.94599162967876,-0.96993415126066,
37.729191620779));
#152318=CARTESIAN_POINT('Ctrl Pts',(6.96568766127409,-0.798011258112235,
37.7370543791922));
#152319=CARTESIAN_POINT('Ctrl Pts',(6.98013638743281,-0.67189109063118,
37.742822385941));
#152320=CARTESIAN_POINT('Ctrl Pts',(6.99114573199519,-0.545490689697603,
37.7485903926897));
#152321=CARTESIAN_POINT('Ctrl Pts',(6.99871765569711,-0.419019973669059,
37.7543583994384));
#152322=CARTESIAN_POINT('Ctrl Pts',(7.00710870499226,-0.278867740978047,
37.7607503852625));
#152323=CARTESIAN_POINT('Ctrl Pts',(7.01128541614013,-0.138543129237301,
37.7671423710865));
#152324=CARTESIAN_POINT('Ctrl Pts',(7.0112497738309,0.00178085826187677,
37.7735343569105));
#152325=CARTESIAN_POINT('Ctrl Pts',(7.01124977383073,0.00178085893843706,
37.7735343569413));
#152326=CARTESIAN_POINT('Ctrl Pts',(7.01120348839179,0.184006843444352,
37.7818350468696));
#152327=CARTESIAN_POINT('Ctrl Pts',(7.00404861198355,0.366382945871945,
37.7901357367978));
#152328=CARTESIAN_POINT('Ctrl Pts',(6.98977578673226,0.548325645680976,
37.7984364267261));
#152329=CARTESIAN_POINT('Ctrl Pts',(6.97551647180639,0.730096122749284,
37.8067292594137));
#152330=CARTESIAN_POINT('Ctrl Pts',(6.95415267047731,0.911433679039336,
37.8150220921014));
#152331=CARTESIAN_POINT('Ctrl Pts',(6.92572706700787,1.09175599646377,37.8233149247891));
#152332=CARTESIAN_POINT('Ctrl Pts',(6.89731729855115,1.27197786197714,37.8316031377995));
#152333=CARTESIAN_POINT('Ctrl Pts',(6.86185361922219,1.45118528206985,37.83989135081));
#152334=CARTESIAN_POINT('Ctrl Pts',(6.81943048606037,1.62880152513757,37.8481795638205));
#152335=CARTESIAN_POINT('Ctrl Pts',(6.7770261656842,1.80633900324712,37.8564641013746));
#152336=CARTESIAN_POINT('Ctrl Pts',(6.72766862248195,1.98228638225756,37.8647486389288));
#152337=CARTESIAN_POINT('Ctrl Pts',(6.67150335974477,2.15607733706709,37.8730331764829));
#152338=CARTESIAN_POINT('Ctrl Pts',(6.64014858575329,2.25309773444892,37.8776580956941));
#152339=CARTESIAN_POINT('Ctrl Pts',(6.60667307426906,2.34944627604572,37.8822830149052));
#152340=CARTESIAN_POINT('Ctrl Pts',(6.57110895151815,2.44502632087634,37.8869079341164));
#152341=CARTESIAN_POINT('',(7.01124996031773,-0.000745952192151278,37.2264656431214));
#152342=CARTESIAN_POINT('Ctrl Pts',(6.57110895151815,2.44502632087632,37.3396717263878));
#152343=CARTESIAN_POINT('Ctrl Pts',(6.64524608758582,2.24577971387883,37.3300019052085));
#152344=CARTESIAN_POINT('Ctrl Pts',(6.71037085531289,2.04301503505559,37.3203320840293));
#152345=CARTESIAN_POINT('Ctrl Pts',(6.7661879905331,1.83747833708746,37.31066226285));
#152346=CARTESIAN_POINT('Ctrl Pts',(6.81199683213143,1.66879540481726,37.3027262893369));
#152347=CARTESIAN_POINT('Ctrl Pts',(6.8515373949267,1.49824586114826,37.2947903158238));
#152348=CARTESIAN_POINT('Ctrl Pts',(6.88466960476146,1.32625449887027,37.2868543423107));
#152349=CARTESIAN_POINT('Ctrl Pts',(6.9159947625869,1.16364365598238,37.2793512018913));
#152350=CARTESIAN_POINT('Ctrl Pts',(6.94158734898268,0.999751854630932,
37.2718480614719));
#152351=CARTESIAN_POINT('Ctrl Pts',(6.96134279331623,0.835064713925977,
37.2643449210525));
#152352=CARTESIAN_POINT('Ctrl Pts',(6.98109422578551,0.67041101729056,37.2568433043437));
#152353=CARTESIAN_POINT('Ctrl Pts',(6.99501081379572,0.504962703640699,
37.2493416876349));
#152354=CARTESIAN_POINT('Ctrl Pts',(7.00303936527711,0.339214107724237,
37.2418400709261));
#152355=CARTESIAN_POINT('Ctrl Pts',(7.00852415564163,0.225981190936938,
37.2367152616579));
#152356=CARTESIAN_POINT('Ctrl Pts',(7.01126202048753,0.112608316228521,
37.2315904523896));
#152357=CARTESIAN_POINT('Ctrl Pts',(7.01124996031773,-0.000745952192208719,
37.2264656431214));
#152358=CARTESIAN_POINT('Ctrl Pts',(7.01124996031765,-0.000745952892359531,
37.2264656430897));
#152359=CARTESIAN_POINT('Ctrl Pts',(7.01123049451372,-0.183706054619841,
37.2181939155392));
#152360=CARTESIAN_POINT('Ctrl Pts',(7.00404513626149,-0.366557650698258,
37.2099221879888));
#152361=CARTESIAN_POINT('Ctrl Pts',(6.98974513960931,-0.548716179648486,
37.2016504604383));
#152362=CARTESIAN_POINT('Ctrl Pts',(6.97543598949301,-0.730991308735181,
37.1933734381341));
#152363=CARTESIAN_POINT('Ctrl Pts',(6.95400315525883,-0.912572151207703,
37.1850964158298));
#152364=CARTESIAN_POINT('Ctrl Pts',(6.92554947323097,-1.09288199561078,
37.1768193935256));
#152365=CARTESIAN_POINT('Ctrl Pts',(6.89705104070912,-1.2734754221036,37.1685293535445));
#152366=CARTESIAN_POINT('Ctrl Pts',(6.8615097511004,-1.45279352333023,37.1602393135635));
#152367=CARTESIAN_POINT('Ctrl Pts',(6.81907938420107,-1.63027081016129,
37.1519492735825));
#152368=CARTESIAN_POINT('Ctrl Pts',(6.77853887990636,-1.79984319981468,
37.1440284747298));
#152369=CARTESIAN_POINT('Ctrl Pts',(6.73170975518064,-1.96773496388468,
37.1361076758771));
#152370=CARTESIAN_POINT('Ctrl Pts',(6.67876767326906,-2.13346875510195,
37.1281868770244));
#152371=CARTESIAN_POINT('Ctrl Pts',(6.6227692458331,-2.30877035538027,37.1198088105833));
#152372=CARTESIAN_POINT('Ctrl Pts',(6.55982763905674,-2.48198229565792,
37.1114307441422));
#152373=CARTESIAN_POINT('Ctrl Pts',(6.49012093403737,-2.65253780822629,
37.1030526777011));
#152374=CARTESIAN_POINT('Ctrl Pts',(6.42046189363462,-2.82297669696172,
37.0946803400822));
#152375=CARTESIAN_POINT('Ctrl Pts',(6.3440471016209,-2.99076247609817,37.0863080024634));
#152376=CARTESIAN_POINT('Ctrl Pts',(6.2611037241574,-3.15534573665745,37.0779356648446));
#152377=CARTESIAN_POINT('Ctrl Pts',(6.17820489868872,-3.31984059338274,
37.0695678243219));
#152378=CARTESIAN_POINT('Ctrl Pts',(6.08878462750169,-3.48113606853503,
37.0611999837992));
#152379=CARTESIAN_POINT('Ctrl Pts',(5.99311743063674,-3.63870444321851,
37.0528321432765));
#152380=CARTESIAN_POINT('Ctrl Pts',(5.89748760565659,-3.79621126464925,
37.0444675716064));
#152381=CARTESIAN_POINT('Ctrl Pts',(5.79561589170577,-3.94999360846245,
37.0361029999364));
#152382=CARTESIAN_POINT('Ctrl Pts',(5.68782204544913,-4.09954960231035,
37.0277384282664));
#152383=CARTESIAN_POINT('Ctrl Pts',(5.58005452987191,-4.24906906428684,
37.0193758998007));
#152384=CARTESIAN_POINT('Ctrl Pts',(5.46636795920961,-4.39436396892815,
37.011013371335));
#152385=CARTESIAN_POINT('Ctrl Pts',(5.34712484105499,-4.53496223762367,
37.0026508428694));
#152386=CARTESIAN_POINT('Ctrl Pts',(5.22787220692641,-4.67557172650098,
36.9942876470477));
#152387=CARTESIAN_POINT('Ctrl Pts',(5.10306234737544,-4.81148357605525,
36.9859244512261));
#152388=CARTESIAN_POINT('Ctrl Pts',(4.97309790550928,-4.94225897588535,
36.9775612554045));
#152389=CARTESIAN_POINT('Ctrl Pts',(4.84312460032866,-5.07304329433561,
36.9691974892297));
#152390=CARTESIAN_POINT('Ctrl Pts',(4.70799624350507,-5.19869023117873,
36.9608337230549));
#152391=CARTESIAN_POINT('Ctrl Pts',(4.56815228993548,-5.31879791103754,
36.9524699568801));
#152392=CARTESIAN_POINT('Ctrl Pts',(4.42828015480015,-5.43892979517825,
36.9441045052264));
#152393=CARTESIAN_POINT('Ctrl Pts',(4.28369077743742,-5.55351998223701,
36.9357390535728));
#152394=CARTESIAN_POINT('Ctrl Pts',(4.1348569514438,-5.66220668587759,36.9273736019191));
#152395=CARTESIAN_POINT('Ctrl Pts',(3.98597328129447,-5.77092978848154,
36.9190053486921));
#152396=CARTESIAN_POINT('Ctrl Pts',(3.83284259350427,-5.87374527152244,
36.9106370954652));
#152397=CARTESIAN_POINT('Ctrl Pts',(3.67596727293508,-5.97033425955451,
36.9022688422382));
#152398=CARTESIAN_POINT('Ctrl Pts',(3.51894650656299,-6.06701279935841,
36.8938928304466));
#152399=CARTESIAN_POINT('Ctrl Pts',(3.35817444996285,-6.1574531357209,36.885516818655));
#152400=CARTESIAN_POINT('Ctrl Pts',(3.19417982126245,-6.24138140413962,
36.8771408068635));
#152401=CARTESIAN_POINT('Ctrl Pts',(3.03010476756985,-6.32535083201817,
36.8687606873722));
#152402=CARTESIAN_POINT('Ctrl Pts',(2.86280428564977,-6.40280167943196,
36.860380567881));
#152403=CARTESIAN_POINT('Ctrl Pts',(2.69282834885489,-6.47350770804388,
36.8520004483897));
#152404=CARTESIAN_POINT('Ctrl Pts',(2.52265819302079,-6.54429452725006,
36.8436107535504));
#152405=CARTESIAN_POINT('Ctrl Pts',(2.3498067798204,-6.60832100757938,36.8352210587111));
#152406=CARTESIAN_POINT('Ctrl Pts',(2.17484182970063,-6.66540993325125,
36.8268313638718));
#152407=CARTESIAN_POINT('Ctrl Pts',(2.06375960221987,-6.70165470698321,
36.8215048913983));
#152408=CARTESIAN_POINT('Ctrl Pts',(1.95182576201224,-6.735104124186,36.8161784189248));
#152409=CARTESIAN_POINT('Ctrl Pts',(1.83918801382648,-6.76572346555023,
36.8108519464514));
#152410=CARTESIAN_POINT('Ctrl Pts',(1.66195048764573,-6.81390355085991,
36.8024706460465));
#152411=CARTESIAN_POINT('Ctrl Pts',(1.48261202794092,-6.8551711637321,36.7940893456417));
#152412=CARTESIAN_POINT('Ctrl Pts',(1.30173764763535,-6.88934725930032,
36.7857080452369));
#152413=CARTESIAN_POINT('Ctrl Pts',(1.12109249912861,-6.92348004167044,
36.7773373669034));
#152414=CARTESIAN_POINT('Ctrl Pts',(0.938915628646759,-6.95053915747116,
36.7689666885699));
#152415=CARTESIAN_POINT('Ctrl Pts',(0.755786438101931,-6.97039549971745,
36.7605960102364));
#152416=CARTESIAN_POINT('Ctrl Pts',(0.572865067746541,-6.99022930842446,
36.7522348311856));
#152417=CARTESIAN_POINT('Ctrl Pts',(0.388993855082819,-7.00287659997662,
36.7438736521349));
#152418=CARTESIAN_POINT('Ctrl Pts',(0.204762051816867,-7.00825934627392,
36.7355124730841));
#152419=CARTESIAN_POINT('Ctrl Pts',(0.020769311047764,-7.01363510782295,
36.7271621436494));
#152420=CARTESIAN_POINT('Ctrl Pts',(-0.163582761064816,-7.01176511695514,
36.7188118142148));
#152421=CARTESIAN_POINT('Ctrl Pts',(-0.347700215944274,-7.00262316009739,
36.7104614847801));
#152422=CARTESIAN_POINT('Ctrl Pts',(-0.531676003455989,-6.99348823742857,
36.7021175804244));
#152423=CARTESIAN_POINT('Ctrl Pts',(-0.715417207627831,-6.97709251544897,
36.6937736760688));
#152424=CARTESIAN_POINT('Ctrl Pts',(-0.898329147949554,-6.95346182159967,
36.6854297717131));
#152425=CARTESIAN_POINT('Ctrl Pts',(-1.08109417226004,-6.92985010807105,
36.6770925692335));
#152426=CARTESIAN_POINT('Ctrl Pts',(-1.26303093709266,-6.89901505409134,
36.6687553667538));
#152427=CARTESIAN_POINT('Ctrl Pts',(-1.44354899987888,-6.86103438611473,
36.6604181642742));
#152428=CARTESIAN_POINT('Ctrl Pts',(-1.50297454971891,-6.84853135986369,
36.6576736032378));
#152429=CARTESIAN_POINT('Ctrl Pts',(-1.56224639998774,-6.83525438800011,
36.6549290422014));
#152430=CARTESIAN_POINT('Ctrl Pts',(-1.62134364638561,-6.82120746956322,
36.6521844811651));
#152431=CARTESIAN_POINT('Ctrl Pts',(-1.80088827007163,-6.77853122255637,
36.6438461708632));
#152432=CARTESIAN_POINT('Ctrl Pts',(-1.97867313897385,-6.72877946772553,
36.6355078605612));
#152433=CARTESIAN_POINT('Ctrl Pts',(-2.15412987388545,-6.67213242141778,
36.6271695502593));
#152434=CARTESIAN_POINT('Ctrl Pts',(-2.32969700022063,-6.61544973471078,
36.6188259937755));
#152435=CARTESIAN_POINT('Ctrl Pts',(-2.50293275907081,-6.55186320394812,
36.6104824372917));
#152436=CARTESIAN_POINT('Ctrl Pts',(-2.67328714752828,-6.48160183823105,
36.6021388808078));
#152437=CARTESIAN_POINT('Ctrl Pts',(-2.84377114086221,-6.41128701797309,
36.5937889765826));
#152438=CARTESIAN_POINT('Ctrl Pts',(-3.01136908865483,-6.3342873582255,
36.5854390723574));
#152439=CARTESIAN_POINT('Ctrl Pts',(-3.17555365441934,-6.25087878225166,
36.5770891681321));
#152440=CARTESIAN_POINT('Ctrl Pts',(-3.33998448488285,-6.16734509958608,
36.5687267396685));
#152441=CARTESIAN_POINT('Ctrl Pts',(-3.50099140993622,-6.0773834396258,
36.5603643112048));
#152442=CARTESIAN_POINT('Ctrl Pts',(-3.65807295569729,-5.98131497359035,
36.5520018827411));
#152443=CARTESIAN_POINT('Ctrl Pts',(-3.81528882759326,-5.88516435592044,
36.5436323032611));
#152444=CARTESIAN_POINT('Ctrl Pts',(-3.96857235073418,-5.7828966940442,
36.5352627237811));
#152445=CARTESIAN_POINT('Ctrl Pts',(-4.1174530024884,-5.67487509420245,
36.5268931443012));
#152446=CARTESIAN_POINT('Ctrl Pts',(-4.26656328450854,-5.56668688420415,
36.5185106557646));
#152447=CARTESIAN_POINT('Ctrl Pts',(-4.4112568680101,-5.4527272041818,36.510128167228));
#152448=CARTESIAN_POINT('Ctrl Pts',(-4.5510970485728,-5.33339874910661,
36.5017456786914));
#152449=CARTESIAN_POINT('Ctrl Pts',(-4.59685504706801,-5.29435252329516,
36.4990027910871));
#152450=CARTESIAN_POINT('Ctrl Pts',(-4.6420936902436,-5.25473174628446,
36.4962599034829));
#152451=CARTESIAN_POINT('Ctrl Pts',(-4.68679857597309,-5.21455133935381,
36.4935170158786));
#152452=CARTESIAN_POINT('Ctrl Pts',(-4.82354042219979,-5.09164882129161,
36.4851271607458));
#152453=CARTESIAN_POINT('Ctrl Pts',(-4.9555616510863,-4.96325958095893,
36.476737305613));
#152454=CARTESIAN_POINT('Ctrl Pts',(-5.08241371095259,-4.82977198563464,
36.4683474504802));
#152455=CARTESIAN_POINT('Ctrl Pts',(-5.20914871351634,-4.69640757079198,
36.4599653373881));
#152456=CARTESIAN_POINT('Ctrl Pts',(-5.33072383076894,-4.55795441689385,
36.4515832242959));
#152457=CARTESIAN_POINT('Ctrl Pts',(-5.44672584142834,-4.41483908776037,
36.4432011112038));
#152458=CARTESIAN_POINT('Ctrl Pts',(-5.56263785911342,-4.27183478578982,
36.4348255008549));
#152459=CARTESIAN_POINT('Ctrl Pts',(-5.67298518379625,-4.12417577395732,
36.426449890506));
#152460=CARTESIAN_POINT('Ctrl Pts',(-5.77739322365365,-3.97232351423961,
36.4180742801572));
#152461=CARTESIAN_POINT('Ctrl Pts',(-5.88173558930339,-3.82056677184845,
36.4097039381916));
#152462=CARTESIAN_POINT('Ctrl Pts',(-5.98014593340909,-3.6646223109188,
36.401333596226));
#152463=CARTESIAN_POINT('Ctrl Pts',(-6.07229127951492,-3.50498290712338,
36.3929632542604));
#152464=CARTESIAN_POINT('Ctrl Pts',(-6.16439217230274,-3.34542051753957,
36.384596950366));
#152465=CARTESIAN_POINT('Ctrl Pts',(-6.25023393020387,-3.18216702394998,
36.3762306464717));
#152466=CARTESIAN_POINT('Ctrl Pts',(-6.32952784025315,-3.01574267502389,
36.3678643425773));
#152467=CARTESIAN_POINT('Ctrl Pts',(-6.40879957401827,-2.84936487032361,
36.3595003785037));
#152468=CARTESIAN_POINT('Ctrl Pts',(-6.48152696887386,-2.67981827436776,
36.35113641443));
#152469=CARTESIAN_POINT('Ctrl Pts',(-6.54746782428572,-2.50764663627937,
36.3427724503564));
#152470=CARTESIAN_POINT('Ctrl Pts',(-6.61339853249572,-2.33550149254498,
36.3344097733578));
#152471=CARTESIAN_POINT('Ctrl Pts',(-6.6725446659447,-2.16073241890292,
36.3260470963593));
#152472=CARTESIAN_POINT('Ctrl Pts',(-6.72471247732225,-1.98390238163234,
36.3176844193607));
#152473=CARTESIAN_POINT('Ctrl Pts',(-6.77687921465991,-1.80707598496905,
36.3093219145344));
#152474=CARTESIAN_POINT('Ctrl Pts',(-6.82206782379734,-1.62818902461673,
36.3009594097081));
#152475=CARTESIAN_POINT('Ctrl Pts',(-6.86013454488979,-1.44781925270725,
36.2925969048817));
#152476=CARTESIAN_POINT('Ctrl Pts',(-6.89820555628098,-1.26742915227499,
36.2842334575617));
#152477=CARTESIAN_POINT('Ctrl Pts',(-6.92915301199516,-1.0855562287602,
36.2758700102417));
#152478=CARTESIAN_POINT('Ctrl Pts',(-6.95288426097215,-0.902788466932194,
36.2675065629217));
#152479=CARTESIAN_POINT('Ctrl Pts',(-6.97662948357546,-0.719913086309687,
36.2591381909689));
#152480=CARTESIAN_POINT('Ctrl Pts',(-6.99314996540156,-0.536142140628691,
36.2507698190161));
#152481=CARTESIAN_POINT('Ctrl Pts',(-7.0024048299875,-0.352069821864623,
36.2424014470632));
#152482=CARTESIAN_POINT('Ctrl Pts',(-7.01166246757275,-0.167942350223029,
36.2340305677275));
#152483=CARTESIAN_POINT('Ctrl Pts',(-7.01365013587314,0.0164863459830646,
36.2256596883917));
#152484=CARTESIAN_POINT('Ctrl Pts',(-7.00837910332929,0.200621301255173,
36.2172888090559));
#152485=CARTESIAN_POINT('Ctrl Pts',(-7.00310360469657,0.384912272083683,
36.2089108371646));
#152486=CARTESIAN_POINT('Ctrl Pts',(-6.99055713077544,0.568908676038571,
36.2005328652733));
#152487=CARTESIAN_POINT('Ctrl Pts',(-6.97080299477737,0.752018730154316,
36.192154893382));
#152488=CARTESIAN_POINT('Ctrl Pts',(-6.95824908049263,0.868386660610357,
36.1868306240232));
#152489=CARTESIAN_POINT('Ctrl Pts',(-6.94278524829619,0.984396730679544,
36.1815063546644));
#152490=CARTESIAN_POINT('Ctrl Pts',(-6.92443852335612,1.09989894934115,
36.1761820853057));
#152491=CARTESIAN_POINT('Ctrl Pts',(-6.89734425156818,1.2704715455265,36.1683192541164));
#152492=CARTESIAN_POINT('Ctrl Pts',(-6.86390358510984,1.44029073648348,
36.1604564229272));
#152493=CARTESIAN_POINT('Ctrl Pts',(-6.82417039470933,1.6088272083952,36.152593591738));
#152494=CARTESIAN_POINT('Ctrl Pts',(-6.78446773402093,1.77723418227481,
36.1447368020967));
#152495=CARTESIAN_POINT('Ctrl Pts',(-6.73848225135412,1.94436002841757,
36.1368800124554));
#152496=CARTESIAN_POINT('Ctrl Pts',(-6.68631940867869,2.10968228120413,
36.129023222814));
#152497=CARTESIAN_POINT('Ctrl Pts',(-6.63418598337725,2.27491130006613,
36.1211708640301));
#152498=CARTESIAN_POINT('Ctrl Pts',(-6.57588224238862,2.4383383864304,36.1133185052463));
#152499=CARTESIAN_POINT('Ctrl Pts',(-6.51156428960506,2.59945322420701,
36.1054661464624));
#152500=CARTESIAN_POINT('Ctrl Pts',(-6.4472615230406,2.76053002089053,36.097615641712));
#152501=CARTESIAN_POINT('Ctrl Pts',(-6.37694750432004,2.91929529867078,
36.0897651369616));
#152502=CARTESIAN_POINT('Ctrl Pts',(-6.30082755025666,3.0752558827562,36.0819146322113));
#152503=CARTESIAN_POINT('Ctrl Pts',(-6.22471984149481,3.23119137769909,
36.0740653903597));
#152504=CARTESIAN_POINT('Ctrl Pts',(-6.14280822674209,3.38432273557631,
36.0662161485082));
#152505=CARTESIAN_POINT('Ctrl Pts',(-6.05534512568461,3.53417910855515,
36.0583669066566));
#152506=CARTESIAN_POINT('Ctrl Pts',(-5.9678525565964,3.6840859710793,36.0505150202418));
#152507=CARTESIAN_POINT('Ctrl Pts',(-5.87480495767119,3.8307153149177,36.042663133827));
#152508=CARTESIAN_POINT('Ctrl Pts',(-5.77649954847457,3.97362297267533,
36.0348112474122));
#152509=CARTESIAN_POINT('Ctrl Pts',(-5.70431511007936,4.07855828703809,
36.0290457049479));
#152510=CARTESIAN_POINT('Ctrl Pts',(-5.62929671775047,4.1814874955054,36.0232801624836));
#152511=CARTESIAN_POINT('Ctrl Pts',(-5.55157631074784,4.28224555910138,
36.0175146200193));
#152512=CARTESIAN_POINT('Ctrl Pts',(-5.42142130985316,4.4509807261346,36.0078593156592));
#152513=CARTESIAN_POINT('Ctrl Pts',(-5.28375446149784,4.61354048175918,
35.9982040112991));
#152514=CARTESIAN_POINT('Ctrl Pts',(-5.13914797926629,4.76935893068483,
35.9885487069391));
#152515=CARTESIAN_POINT('Ctrl Pts',(-4.99374040425093,4.92604058458647,
35.9788399140041));
#152516=CARTESIAN_POINT('Ctrl Pts',(-4.84131616604515,5.07590603639355,
35.9691311210692));
#152517=CARTESIAN_POINT('Ctrl Pts',(-4.68248723669843,5.21842311820882,
35.9594223281343));
#152518=CARTESIAN_POINT('Ctrl Pts',(-4.52289400905709,5.36162600432332,
35.9496668156634));
#152519=CARTESIAN_POINT('Ctrl Pts',(-4.35683435035826,5.49740961728959,
35.9399113031925));
#152520=CARTESIAN_POINT('Ctrl Pts',(-4.18495860069878,5.6252775996334,35.9301557907215));
#152521=CARTESIAN_POINT('Ctrl Pts',(-4.0129126676046,5.75327219095182,35.9203906187924));
#152522=CARTESIAN_POINT('Ctrl Pts',(-3.83503916201762,5.87333546055584,
35.9106254468633));
#152523=CARTESIAN_POINT('Ctrl Pts',(-3.6520191350744,5.98501318290532,35.9008602749341));
#152524=CARTESIAN_POINT('Ctrl Pts',(-3.46924865178581,6.09653863521397,
35.8911084175954));
#152525=CARTESIAN_POINT('Ctrl Pts',(-3.2813457043459,6.19970137200236,35.8813565602566));
#152526=CARTESIAN_POINT('Ctrl Pts',(-3.08901667879727,6.29409266857522,
35.8716047029179));
#152527=CARTESIAN_POINT('Ctrl Pts',(-3.00514729454962,6.33525411001299,
35.8673521868562));
#152528=CARTESIAN_POINT('Ctrl Pts',(-2.92043660936041,6.37474814422477,
35.8630996707945));
#152529=CARTESIAN_POINT('Ctrl Pts',(-2.83494485713112,6.41254350624819,
35.8588471547329));
#152530=CARTESIAN_POINT('Ctrl Pts',(-2.67345007756686,6.48393932513552,
35.8508141091341));
#152531=CARTESIAN_POINT('Ctrl Pts',(-2.50908783830989,6.5493050661394,35.8427810635354));
#152532=CARTESIAN_POINT('Ctrl Pts',(-2.34235612441827,6.60840331312339,
35.8347480179366));
#152533=CARTESIAN_POINT('Ctrl Pts',(-2.17573159209201,6.66746356947876,
35.8267201362889));
#152534=CARTESIAN_POINT('Ctrl Pts',(-2.00674096114295,6.72026422965502,
35.8186922546412));
#152535=CARTESIAN_POINT('Ctrl Pts',(-1.83590305423349,6.76661558963978,
35.8106643729934));
#152536=CARTESIAN_POINT('Ctrl Pts',(-1.6651422823232,6.81294602152856,35.8026401160134));
#152537=CARTESIAN_POINT('Ctrl Pts',(-1.4925362482132,6.85283285541069,35.7946158590334));
#152538=CARTESIAN_POINT('Ctrl Pts',(-1.31861978183444,6.88613595810124,
35.7865916020533));
#152539=CARTESIAN_POINT('Ctrl Pts',(-1.14472434372789,6.91943503410747,
35.7785683152877));
#152540=CARTESIAN_POINT('Ctrl Pts',(-0.9695191473153,6.94615188802487,35.7705450285221));
#152541=CARTESIAN_POINT('Ctrl Pts',(-0.793550262889007,6.96619727992029,
35.7625217417564));
#152542=CARTESIAN_POINT('Ctrl Pts',(-0.617595797543047,6.98624102927465,
35.7544991124276));
#152543=CARTESIAN_POINT('Ctrl Pts',(-0.440878133575294,6.99961436800925,
35.7464764830987));
#152544=CARTESIAN_POINT('Ctrl Pts',(-0.263949226028385,7.00627985228816,
35.7384538537699));
#152545=CARTESIAN_POINT('Ctrl Pts',(-0.0869538058082248,7.01294784231463,
35.7304282085035));
#152546=CARTESIAN_POINT('Ctrl Pts',(0.0902526499616381,7.01290292960881,
35.7224025632372));
#152547=CARTESIAN_POINT('Ctrl Pts',(0.267117028962989,7.00615979373423,
35.7143769179709));
#152548=CARTESIAN_POINT('Ctrl Pts',(0.371407044414812,7.00218362991579,
35.7096445084627));
#152549=CARTESIAN_POINT('Ctrl Pts',(0.475578136999383,6.99587948197923,
35.7049120989546));
#152550=CARTESIAN_POINT('Ctrl Pts',(0.579517602897687,6.98725882663808,
35.7001796894465));
#152551=CARTESIAN_POINT('Ctrl Pts',(0.771258535626464,6.97135598856248,
35.6914496406118));
#152552=CARTESIAN_POINT('Ctrl Pts',(0.962306806831938,6.94755946216054,
35.6827195917771));
#152553=CARTESIAN_POINT('Ctrl Pts',(1.15202145315725,6.91595786091598,35.6739895429424));
#152554=CARTESIAN_POINT('Ctrl Pts',(1.34179095570927,6.88434712202898,35.6652569698032));
#152555=CARTESIAN_POINT('Ctrl Pts',(1.53022579344518,6.84492684852203,35.656524396664));
#152556=CARTESIAN_POINT('Ctrl Pts',(1.71669433999845,6.79783694313988,35.6477918235248));
#152557=CARTESIAN_POINT('Ctrl Pts',(1.90581196991434,6.75007805048239,35.6389351902444));
#152558=CARTESIAN_POINT('Ctrl Pts',(2.092906733217,6.69443001733014,35.630078556964));
#152559=CARTESIAN_POINT('Ctrl Pts',(2.2773342966685,6.6310915439102,35.6212219236836));
#152560=CARTESIAN_POINT('Ctrl Pts',(2.45929423139178,6.56860053511913,35.6124837915768));
#152561=CARTESIAN_POINT('Ctrl Pts',(2.63865764175701,6.4986237153111,35.6037456594701));
#152562=CARTESIAN_POINT('Ctrl Pts',(2.81482368315884,6.42140126415007,35.5950075273633));
#152563=CARTESIAN_POINT('Ctrl Pts',(2.99457330782607,6.34260794790351,35.5860916434961));
#152564=CARTESIAN_POINT('Ctrl Pts',(3.17099381509528,6.25627117582011,35.5771757596289));
#152565=CARTESIAN_POINT('Ctrl Pts',(3.34347019431484,6.16269694388977,35.5682598757617));
#152566=CARTESIAN_POINT('Ctrl Pts',(3.51594657353441,6.06912271195942,35.5593439918945));
#152567=CARTESIAN_POINT('Ctrl Pts',(3.68447856179311,5.9683111697409,35.5504281080273));
#152568=CARTESIAN_POINT('Ctrl Pts',(3.84847863845386,5.86061760669167,35.54151222416));
#152569=CARTESIAN_POINT('Ctrl Pts',(4.0092560721689,5.75504024936822,35.5327715396637));
#152570=CARTESIAN_POINT('Ctrl Pts',(4.16569512362814,5.64283761417073,35.5240308551673));
#152571=CARTESIAN_POINT('Ctrl Pts',(4.31726831139562,5.524384209115,35.5152901706709));
#152572=CARTESIAN_POINT('Ctrl Pts',(4.46881422862865,5.40595211579462,35.5065510587689));
#152573=CARTESIAN_POINT('Ctrl Pts',(4.6154958148557,5.28127166709487,35.4978119468669));
#152574=CARTESIAN_POINT('Ctrl Pts',(4.756817478221,5.15075858892564,35.4890728349649));
#152575=CARTESIAN_POINT('Ctrl Pts',(4.89997016712896,5.01855452599095,35.4802204952906));
#152576=CARTESIAN_POINT('Ctrl Pts',(5.03762284930191,4.88036581662593,35.4713681556163));
#152577=CARTESIAN_POINT('Ctrl Pts',(5.16929682606843,4.73666516512397,35.4625158159421));
#152578=CARTESIAN_POINT('Ctrl Pts',(5.29921997169161,4.59487526001356,35.4537811832922));
#152579=CARTESIAN_POINT('Ctrl Pts',(5.4233222392301,4.44771930042879,35.4450465506423));
#152580=CARTESIAN_POINT('Ctrl Pts',(5.54118175105719,4.29568753103048,35.4363119179924));
#152581=CARTESIAN_POINT('Ctrl Pts',(5.66142365713964,4.14058261455706,35.4274007248059));
#152582=CARTESIAN_POINT('Ctrl Pts',(5.77516754427766,3.98040288732872,35.4184895316194));
#152583=CARTESIAN_POINT('Ctrl Pts',(5.88200887951529,3.81570414259324,35.409578338433));
#152584=CARTESIAN_POINT('Ctrl Pts',(5.98885021475291,3.6510053978578,35.4006671452465));
#152585=CARTESIAN_POINT('Ctrl Pts',(6.0887888218152,3.48178788258962,35.39175595206));
#152586=CARTESIAN_POINT('Ctrl Pts',(6.18146681589465,3.30863938296292,35.3828447588735));
#152587=CARTESIAN_POINT('Ctrl Pts',(6.26488919567311,3.1527829680998,35.3748235133809));
#152588=CARTESIAN_POINT('Ctrl Pts',(6.34246700775347,2.99366895795854,35.3668022678882));
#152589=CARTESIAN_POINT('Ctrl Pts',(6.41393984207482,2.83178428993898,35.3587810223955));
#152590=CARTESIAN_POINT('Ctrl Pts',(6.47013863698517,2.7044950430028,35.35247395014));
#152591=CARTESIAN_POINT('Ctrl Pts',(6.52256380139321,2.57549341148191,35.3461668778845));
#152592=CARTESIAN_POINT('Ctrl Pts',(6.57110895151813,2.44502632087638,35.339859805629));
#152593=CARTESIAN_POINT('Origin',(0.,0.,50.));
#152594=CARTESIAN_POINT('',(6.57110895151813,2.44502632087639,33.3398701610928));
#152595=CARTESIAN_POINT('',(6.57110895151815,2.44502632087634,33.8866662574739));
#152596=CARTESIAN_POINT('',(6.57110895151814,2.44502632087636,50.));
#152597=CARTESIAN_POINT('',(7.01124858877573,0.00444847055755681,35.7735343569399));
#152598=CARTESIAN_POINT('Ctrl Pts',(6.57110895151815,2.44502632087633,33.8866662574739));
#152599=CARTESIAN_POINT('Ctrl Pts',(6.50684008859926,2.61775153729806,33.8950354753427));
#152600=CARTESIAN_POINT('Ctrl Pts',(6.4358134696495,2.78778929210781,33.9034046932115));
#152601=CARTESIAN_POINT('Ctrl Pts',(6.35829518664791,2.95460807586219,33.9117739110803));
#152602=CARTESIAN_POINT('Ctrl Pts',(6.2806561267985,3.1216867705186,33.9201561685536));
#152603=CARTESIAN_POINT('Ctrl Pts',(6.1965053400371,3.28553618062757,33.9285384260269));
#152604=CARTESIAN_POINT('Ctrl Pts',(6.10615428911975,3.44565035370167,33.9369206835002));
#152605=CARTESIAN_POINT('Ctrl Pts',(6.07231393013319,3.50562000586014,33.9400601998549));
#152606=CARTESIAN_POINT('Ctrl Pts',(6.03760421129288,3.56506597215157,33.9431997162095));
#152607=CARTESIAN_POINT('Ctrl Pts',(6.00204300290678,3.62396279696105,33.9463392325642));
#152608=CARTESIAN_POINT('Ctrl Pts',(5.90701136331561,3.78135513772714,33.9547290876969));
#152609=CARTESIAN_POINT('Ctrl Pts',(5.80570400173894,3.93514141929994,33.9631189428297));
#152610=CARTESIAN_POINT('Ctrl Pts',(5.69841812432295,4.0848081280383,33.9715087979625));
#152611=CARTESIAN_POINT('Ctrl Pts',(5.59123124881029,4.23433672643643,33.9798909110546));
#152612=CARTESIAN_POINT('Ctrl Pts',(5.47807704596683,4.37975306437033,33.9882730241467));
#152613=CARTESIAN_POINT('Ctrl Pts',(5.35929687460675,4.52057115554333,33.9966551372388));
#152614=CARTESIAN_POINT('Ctrl Pts',(5.24060885148502,4.66128000172298,34.0050307475877));
#152615=CARTESIAN_POINT('Ctrl Pts',(5.11630377263722,4.797397462809,34.0134063579365));
#152616=CARTESIAN_POINT('Ctrl Pts',(4.98676452950965,4.92846893971387,34.0217819682854));
#152617=CARTESIAN_POINT('Ctrl Pts',(4.85730676849,5.05945797071302,34.030152310251));
#152618=CARTESIAN_POINT('Ctrl Pts',(4.72262163835405,5.18540711299538,34.0385226522165));
#152619=CARTESIAN_POINT('Ctrl Pts',(4.58313060334181,5.30589676070047,34.0468929941821));
#152620=CARTESIAN_POINT('Ctrl Pts',(4.44370686244198,5.42632828105784,34.0552592980765));
#152621=CARTESIAN_POINT('Ctrl Pts',(4.2994820884425,5.54130534456897,34.0636256019708));
#152622=CARTESIAN_POINT('Ctrl Pts',(4.15091304341598,5.65044666097284,34.0719919058652));
#152623=CARTESIAN_POINT('Ctrl Pts',(4.00238554898793,5.75955745360903,34.0803558699388));
#152624=CARTESIAN_POINT('Ctrl Pts',(3.84951646994518,5.86283555794422,34.0887198340124));
#152625=CARTESIAN_POINT('Ctrl Pts',(3.69279438675831,5.95994095437416,34.097083798086));
#152626=CARTESIAN_POINT('Ctrl Pts',(3.5360964204957,6.05703140789724,34.1054464750845));
#152627=CARTESIAN_POINT('Ctrl Pts',(3.37554691153541,6.14795087432785,34.1138091520831));
#152628=CARTESIAN_POINT('Ctrl Pts',(3.21166241620954,6.23240331548008,34.1221718290816));
#152629=CARTESIAN_POINT('Ctrl Pts',(3.0477812949664,6.31685401791064,34.1305343339079));
#152630=CARTESIAN_POINT('Ctrl Pts',(2.88056561659312,6.39483781036505,34.1388968387341));
#152631=CARTESIAN_POINT('Ctrl Pts',(2.71055584901467,6.46610497532111,34.1472593435604));
#152632=CARTESIAN_POINT('Ctrl Pts',(2.54052692053521,6.5373801724221,34.1556227908803));
#152633=CARTESIAN_POINT('Ctrl Pts',(2.36770357830753,6.60193710623713,34.1639862382003));
#152634=CARTESIAN_POINT('Ctrl Pts',(2.19264594028158,6.65957433647727,34.1723496855202));
#152635=CARTESIAN_POINT('Ctrl Pts',(2.01748522339739,6.7172455051388,34.180718057473));
#152636=CARTESIAN_POINT('Ctrl Pts',(1.84008789399861,6.76798872457049,34.1890864294258));
#152637=CARTESIAN_POINT('Ctrl Pts',(1.66102989132753,6.81165224175578,34.1974548013786));
#152638=CARTESIAN_POINT('Ctrl Pts',(1.48191823819943,6.85532884167189,34.2058256807143));
#152639=CARTESIAN_POINT('Ctrl Pts',(1.30114524025199,6.89192143685681,34.2141965600501));
#152640=CARTESIAN_POINT('Ctrl Pts',(1.11929739059536,6.92132934586315,34.2225674393858));
#152641=CARTESIAN_POINT('Ctrl Pts',(0.937295463222451,6.95076217187274,
34.2309454112771));
#152642=CARTESIAN_POINT('Ctrl Pts',(0.754217189934041,6.97299810058162,
34.2393233831684));
#152643=CARTESIAN_POINT('Ctrl Pts',(0.570655713252553,6.98798816680683,
34.2477013550596));
#152644=CARTESIAN_POINT('Ctrl Pts',(0.454000900070819,6.99751447595783,
34.2530256244188));
#152645=CARTESIAN_POINT('Ctrl Pts',(0.337151023210004,7.00411544128752,
34.258349893778));
#152646=CARTESIAN_POINT('Ctrl Pts',(0.220258480229419,7.00778943493503,
34.2636741631371));
#152647=CARTESIAN_POINT('Ctrl Pts',(0.0476326661061512,7.0132151543891,
34.2715369943264));
#152648=CARTESIAN_POINT('Ctrl Pts',(-0.125445162474049,7.01226592069182,
34.2793998255156));
#152649=CARTESIAN_POINT('Ctrl Pts',(-0.298444993877957,7.00489522749122,
34.2872626567048));
#152650=CARTESIAN_POINT('Ctrl Pts',(-0.471311897746947,6.99753019769542,
34.2951194463462));
#152651=CARTESIAN_POINT('Ctrl Pts',(-0.644100545156358,6.983753536577,34.3029762359875));
#152652=CARTESIAN_POINT('Ctrl Pts',(-0.816277960669884,6.96357069709389,
34.3108330256288));
#152653=CARTESIAN_POINT('Ctrl Pts',(-0.988358276271211,6.94339923977687,
34.3186853844127));
#152654=CARTESIAN_POINT('Ctrl Pts',(-1.15982766817703,6.91682883499607,
34.3265377431966));
#152655=CARTESIAN_POINT('Ctrl Pts',(-1.33015558243525,6.88391695831787,
34.3343901019805));
#152656=CARTESIAN_POINT('Ctrl Pts',(-1.50044328028575,6.85101285251773,
34.3422406067309));
#152657=CARTESIAN_POINT('Ctrl Pts',(-1.66958966129264,6.81177031883781,
34.3500911114812));
#152658=CARTESIAN_POINT('Ctrl Pts',(-1.83707176431813,6.76629838946267,
34.3579416162316));
#152659=CARTESIAN_POINT('Ctrl Pts',(-2.00452692475201,6.72083377508777,
34.3657908580832));
#152660=CARTESIAN_POINT('Ctrl Pts',(-2.17031797276425,6.66914186280106,
34.3736400999347));
#152661=CARTESIAN_POINT('Ctrl Pts',(-2.3339350297199,6.61138214290676,34.3814893417863));
#152662=CARTESIAN_POINT('Ctrl Pts',(-2.49760721246457,6.55360296263228,
34.3893412282011));
#152663=CARTESIAN_POINT('Ctrl Pts',(-2.65910358102391,6.48975201837551,
34.3971931146159));
#152664=CARTESIAN_POINT('Ctrl Pts',(-2.81793204782319,6.42003781424619,
34.4050450010307));
#152665=CARTESIAN_POINT('Ctrl Pts',(-2.93455781410189,6.36884754186658,
34.410810543495));
#152666=CARTESIAN_POINT('Ctrl Pts',(-3.0497454652282,6.3144969561212,34.4165760859592));
#152667=CARTESIAN_POINT('Ctrl Pts',(-3.16330811802394,6.25708464965465,
34.4223416284234));
#152668=CARTESIAN_POINT('Ctrl Pts',(-3.35348657625233,6.16093874553613,
34.4319969327836));
#152669=CARTESIAN_POINT('Ctrl Pts',(-3.53901044182278,6.05625478979374,
34.4416522371438));
#152670=CARTESIAN_POINT('Ctrl Pts',(-3.71921641498869,5.9434885228272,34.4513075415041));
#152671=CARTESIAN_POINT('Ctrl Pts',(-3.90042069543694,5.8300975518981,34.461016334439));
#152672=CARTESIAN_POINT('Ctrl Pts',(-4.07624798905754,5.70853454413747,
34.4707251273739));
#152673=CARTESIAN_POINT('Ctrl Pts',(-4.24606065560468,5.57930062565426,
34.4804339203088));
#152674=CARTESIAN_POINT('Ctrl Pts',(-4.41669047512317,5.44944482258119,
34.4901894327797));
#152675=CARTESIAN_POINT('Ctrl Pts',(-4.58124762260269,5.31184415030478,
34.4999449452507));
#152676=CARTESIAN_POINT('Ctrl Pts',(-4.73912242441051,5.16704414621643,
34.5097004577216));
#152677=CARTESIAN_POINT('Ctrl Pts',(-4.8971535465599,5.02210076784771,34.5194656296508));
#152678=CARTESIAN_POINT('Ctrl Pts',(-5.04848906772519,4.86994383329936,
34.5292308015798));
#152679=CARTESIAN_POINT('Ctrl Pts',(-5.19255492806774,4.71115695785011,
34.538995973509));
#152680=CARTESIAN_POINT('Ctrl Pts',(-5.33642435787886,4.55258658470232,
34.5487478308477));
#152681=CARTESIAN_POINT('Ctrl Pts',(-5.47304391196111,4.38740436604411,
34.5584996881865));
#152682=CARTESIAN_POINT('Ctrl Pts',(-5.60187946299434,4.21622734735478,
34.5682515455253));
#152683=CARTESIAN_POINT('Ctrl Pts',(-5.65806109394264,4.14158176999892,
34.5725040615868));
#152684=CARTESIAN_POINT('Ctrl Pts',(-5.71276301056878,4.06579668412801,
34.5767565776484));
#152685=CARTESIAN_POINT('Ctrl Pts',(-5.76594319092083,3.98892537929374,
34.58100909371));
#152686=CARTESIAN_POINT('Ctrl Pts',(-5.86640108632521,3.84371471153147,
34.5890421393087));
#152687=CARTESIAN_POINT('Ctrl Pts',(-5.96147480433599,3.6945550188055,34.5970751849074));
#152688=CARTESIAN_POINT('Ctrl Pts',(-6.05083762022762,3.54189083063527,
34.6051082305062));
#152689=CARTESIAN_POINT('Ctrl Pts',(-6.14014299026016,3.38932478088372,
34.6131361121539));
#152690=CARTESIAN_POINT('Ctrl Pts',(-6.22374458135365,3.23325903502649,
34.6211639938016));
#152691=CARTESIAN_POINT('Ctrl Pts',(-6.30135861793038,3.07416755085577,
34.6291918754493));
#152692=CARTESIAN_POINT('Ctrl Pts',(-6.37893761100423,2.91514789805898,
34.6372161324292));
#152693=CARTESIAN_POINT('Ctrl Pts',(-6.45053427202727,2.75310555588188,
34.6452403894092));
#152694=CARTESIAN_POINT('Ctrl Pts',(-6.51591050745011,2.58853951513228,
34.6532646463892));
#152695=CARTESIAN_POINT('Ctrl Pts',(-6.58127883822066,2.42399337209203,
34.6612879331548));
#152696=CARTESIAN_POINT('Ctrl Pts',(-6.64042809904845,2.25692447589421,
34.6693112199205));
#152697=CARTESIAN_POINT('Ctrl Pts',(-6.69316807264476,2.08785241667817,
34.6773345066861));
#152698=CARTESIAN_POINT('Ctrl Pts',(-6.74590372467046,1.91879421140996,
34.6853571360149));
#152699=CARTESIAN_POINT('Ctrl Pts',(-6.79223103023467,1.74773352128503,
34.6933797653437));
#152700=CARTESIAN_POINT('Ctrl Pts',(-6.83200954100363,1.57520544505643,
34.7014023946725));
#152701=CARTESIAN_POINT('Ctrl Pts',(-6.87180300566088,1.40261251055307,
34.7094280399389));
#152702=CARTESIAN_POINT('Ctrl Pts',(-6.90504267801968,1.22855144608101,
34.7174536852052));
#152703=CARTESIAN_POINT('Ctrl Pts',(-6.93163908811575,1.05356827714478,
34.7254793304715));
#152704=CARTESIAN_POINT('Ctrl Pts',(-6.94732195221547,0.950387537779847,
34.7302117399798));
#152705=CARTESIAN_POINT('Ctrl Pts',(-6.96069592775399,0.846886351359701,
34.7349441494881));
#152706=CARTESIAN_POINT('Ctrl Pts',(-6.97175111860425,0.743177571472889,
34.7396765589963));
#152707=CARTESIAN_POINT('Ctrl Pts',(-6.99214503333859,0.551862193668865,
34.748406607831));
#152708=CARTESIAN_POINT('Ctrl Pts',(-7.00465564836262,0.359744518503252,
34.7571366566657));
#152709=CARTESIAN_POINT('Ctrl Pts',(-7.00924961118236,0.167470745624329,
34.7658667055004));
#152710=CARTESIAN_POINT('Ctrl Pts',(-7.01384490235216,-0.02485862345532,
34.7745992786395));
#152711=CARTESIAN_POINT('Ctrl Pts',(-7.0105189655873,-0.217343906477795,
34.7833318517787));
#152712=CARTESIAN_POINT('Ctrl Pts',(-6.99929057855495,-0.40933844120971,
34.7920644249178));
#152713=CARTESIAN_POINT('Ctrl Pts',(-6.98790267436091,-0.604060564788502,
34.8009210581982));
#152714=CARTESIAN_POINT('Ctrl Pts',(-6.96838609170347,-0.798277600731434,
34.8097776914787));
#152715=CARTESIAN_POINT('Ctrl Pts',(-6.94081497261864,-0.991319362452381,
34.8186343247591));
#152716=CARTESIAN_POINT('Ctrl Pts',(-6.91361275330271,-1.1817782380355,
34.8273724568658));
#152717=CARTESIAN_POINT('Ctrl Pts',(-6.87857025954447,-1.37109282257502,
34.8361105889726));
#152718=CARTESIAN_POINT('Ctrl Pts',(-6.83581054283597,-1.55862785325833,
34.8448487210794));
#152719=CARTESIAN_POINT('Ctrl Pts',(-6.7921810046565,-1.74997773606888,
34.8537646049466));
#152720=CARTESIAN_POINT('Ctrl Pts',(-6.74051697392869,-1.93947460023313,
34.8626804888138));
#152721=CARTESIAN_POINT('Ctrl Pts',(-6.68100348636997,-2.12645690706686,
34.8715963726811));
#152722=CARTESIAN_POINT('Ctrl Pts',(-6.62148999881125,-2.31343921390056,
34.8805122565483));
#152723=CARTESIAN_POINT('Ctrl Pts',(-6.55412715193734,-2.49790667708081,
34.8894281404155));
#152724=CARTESIAN_POINT('Ctrl Pts',(-6.47915356094348,-2.67921550014429,
34.8983440242828));
#152725=CARTESIAN_POINT('Ctrl Pts',(-6.40565321995713,-2.85696155902109,
34.9070847087791));
#152726=CARTESIAN_POINT('Ctrl Pts',(-6.32483065806215,-3.03169084006869,
34.9158253932755));
#152727=CARTESIAN_POINT('Ctrl Pts',(-6.23695464382761,-3.20281490775494,
34.9245660777718));
#152728=CARTESIAN_POINT('Ctrl Pts',(-6.14909443994743,-3.37390818737946,
34.9333051896739));
#152729=CARTESIAN_POINT('Ctrl Pts',(-6.05418344311144,-3.54139730555117,
34.942044301576));
#152730=CARTESIAN_POINT('Ctrl Pts',(-5.9525368958658,-3.70471740701721,
34.950783413478));
#152731=CARTESIAN_POINT('Ctrl Pts',(-5.84957337130876,-3.87015355545144,
34.9596357531523));
#152732=CARTESIAN_POINT('Ctrl Pts',(-5.73969867365878,-4.03131164901688,
34.9684880928265));
#152733=CARTESIAN_POINT('Ctrl Pts',(-5.62328718273507,-4.1876327230295,
34.9773404325008));
#152734=CARTESIAN_POINT('Ctrl Pts',(-5.50842358205335,-4.34187524050822,
34.9860750651507));
#152735=CARTESIAN_POINT('Ctrl Pts',(-5.38719612323055,-4.49140835549209,
34.9948096978006));
#152736=CARTESIAN_POINT('Ctrl Pts',(-5.26000708668644,-4.63572561855299,
35.0035443304505));
#152737=CARTESIAN_POINT('Ctrl Pts',(-5.13024707029253,-4.7829600888307,
35.0124555236369));
#152738=CARTESIAN_POINT('Ctrl Pts',(-4.9942820721572,-4.92476536432569,
35.0213667168234));
#152739=CARTESIAN_POINT('Ctrl Pts',(-4.85258201244914,-5.06063971993216,
35.0302779100099));
#152740=CARTESIAN_POINT('Ctrl Pts',(-4.71088195274109,-5.19651407553862,
35.0391891031963));
#152741=CARTESIAN_POINT('Ctrl Pts',(-4.56344704093036,-5.32645729173091,
35.0481002963828));
#152742=CARTESIAN_POINT('Ctrl Pts',(-4.41078738240292,-5.45000745226419,
35.0570114895692));
#152743=CARTESIAN_POINT('Ctrl Pts',(-4.27329790931377,-5.56128011352687,
35.0650371544215));
#152744=CARTESIAN_POINT('Ctrl Pts',(-4.13150697620872,-5.66741791019989,
35.0730628192738));
#152745=CARTESIAN_POINT('Ctrl Pts',(-3.98584443948815,-5.76807339297113,
35.0810884841261));
#152746=CARTESIAN_POINT('Ctrl Pts',(-3.8402281324836,-5.86869693016123,
35.0891116018292));
#152747=CARTESIAN_POINT('Ctrl Pts',(-3.69074296940803,-5.96384140938561,
35.0971347195323));
#152748=CARTESIAN_POINT('Ctrl Pts',(-3.53784990253808,-6.05320118859528,
35.1051578372354));
#152749=CARTESIAN_POINT('Ctrl Pts',(-3.38497611682184,-6.1425496987548,
35.1131799431532));
#152750=CARTESIAN_POINT('Ctrl Pts',(-3.22869560004598,-6.22611477757557,
35.1212020490709));
#152751=CARTESIAN_POINT('Ctrl Pts',(-3.0694961030301,-6.30363547772101,
35.1292241549887));
#152752=CARTESIAN_POINT('Ctrl Pts',(-2.91023744694386,-6.38118498482025,
35.1372492419481));
#152753=CARTESIAN_POINT('Ctrl Pts',(-2.74805797229307,-6.4526854628926,
35.1452743289075));
#152754=CARTESIAN_POINT('Ctrl Pts',(-2.58346813081979,-6.51792290377376,
35.1532994158669));
#152755=CARTESIAN_POINT('Ctrl Pts',(-2.41884587420058,-6.58317319284255,
35.161326083327));
#152756=CARTESIAN_POINT('Ctrl Pts',(-2.25181264907545,-6.6421578605573,
35.1693527507871));
#152757=CARTESIAN_POINT('Ctrl Pts',(-2.08289626832121,-6.69471206982896,
35.1773794182473));
#152758=CARTESIAN_POINT('Ctrl Pts',(-1.91384428209153,-6.7473084694347,
35.1854125294878));
#152759=CARTESIAN_POINT('Ctrl Pts',(-1.74290647352157,-6.79346400008821,
35.1934456407282));
#152760=CARTESIAN_POINT('Ctrl Pts',(-1.57062371247984,-6.83306429914837,
35.2014787519687));
#152761=CARTESIAN_POINT('Ctrl Pts',(-1.469108451146,-6.85639823391749,35.206212152931));
#152762=CARTESIAN_POINT('Ctrl Pts',(-1.36712641924262,-6.87745716469574,
35.2109455538933));
#152763=CARTESIAN_POINT('Ctrl Pts',(-1.26478941082167,-6.89622609176739,
35.2156789548556));
#152764=CARTESIAN_POINT('Ctrl Pts',(-1.05397198855979,-6.9348906656583,
35.22542990815));
#152765=CARTESIAN_POINT('Ctrl Pts',(-0.8415236726413,-6.96385777599858,
35.2351808614444));
#152766=CARTESIAN_POINT('Ctrl Pts',(-0.62825740909946,-6.98304512303992,
35.2449318147389));
#152767=CARTESIAN_POINT('Ctrl Pts',(-0.414683895494878,-7.00226011305435,
35.2546968161108));
#152768=CARTESIAN_POINT('Ctrl Pts',(-0.200290115584286,-7.01166715299412,
35.2644618174828));
#152769=CARTESIAN_POINT('Ctrl Pts',(0.0141058876919451,-7.01123581021438,
35.2742268188548));
#152770=CARTESIAN_POINT('Ctrl Pts',(0.22814453724969,-7.01080518639368,
35.2839755439926));
#152771=CARTESIAN_POINT('Ctrl Pts',(0.442185364857365,-7.00056895396267,
35.2937242691304));
#152772=CARTESIAN_POINT('Ctrl Pts',(0.655413416586412,-6.98054867584623,
35.3034729942682));
#152773=CARTESIAN_POINT('Ctrl Pts',(0.868056239992785,-6.96058334563034,
35.3131949629356));
#152774=CARTESIAN_POINT('Ctrl Pts',(1.07989070109874,-6.93088758190894,
35.322916931603));
#152775=CARTESIAN_POINT('Ctrl Pts',(1.29010813764909,-6.89153448483512,
35.3326389002704));
#152776=CARTESIAN_POINT('Ctrl Pts',(1.49893462032694,-6.85244177692628,
35.3422965412103));
#152777=CARTESIAN_POINT('Ctrl Pts',(1.70616535539039,-6.80381909355923,
35.3519541821502));
#152778=CARTESIAN_POINT('Ctrl Pts',(1.91100791866417,-6.74578944952352,
35.3616118230901));
#152779=CARTESIAN_POINT('Ctrl Pts',(2.00104327749264,-6.72028342313944,
35.3658566887741));
#152780=CARTESIAN_POINT('Ctrl Pts',(2.09061727257798,-6.69296073299207,
35.3701015544581));
#152781=CARTESIAN_POINT('Ctrl Pts',(2.17966267742205,-6.66383502010317,
35.3743464201421));
#152782=CARTESIAN_POINT('Ctrl Pts',(2.34437245817147,-6.60996037275328,
35.382198267156));
#152783=CARTESIAN_POINT('Ctrl Pts',(2.50720483799878,-6.54993521035217,
35.3900501141698));
#152784=CARTESIAN_POINT('Ctrl Pts',(2.66765176712923,-6.48392324228413,
35.3979019611837));
#152785=CARTESIAN_POINT('Ctrl Pts',(2.82805319480719,-6.41792999467677,
35.4057515814772));
#152786=CARTESIAN_POINT('Ctrl Pts',(2.98607016502616,-6.34595346363315,
35.4136012017706));
#152787=CARTESIAN_POINT('Ctrl Pts',(3.1412126793601,-6.26820623986858,35.4214508220641));
#152788=CARTESIAN_POINT('Ctrl Pts',(3.29634280755006,-6.19046522322467,
35.4292998156659));
#152789=CARTESIAN_POINT('Ctrl Pts',(3.44859859600243,-6.10695460259406,
35.4371488092677));
#152790=CARTESIAN_POINT('Ctrl Pts',(3.59751305545061,-6.0179337299743,35.4449978028695));
#152791=CARTESIAN_POINT('Ctrl Pts',(3.74650290592818,-5.92886778869399,
35.4528507701869));
#152792=CARTESIAN_POINT('Ctrl Pts',(3.89214771961881,-5.83428621749232,
35.4607037375042));
#152793=CARTESIAN_POINT('Ctrl Pts',(4.03400772256224,-5.73449285088125,
35.4685567048216));
#152794=CARTESIAN_POINT('Ctrl Pts',(4.17590375317967,-5.63467414010831,
35.4764116665288));
#152795=CARTESIAN_POINT('Ctrl Pts',(4.3140127544162,-5.5296412279062,35.484266628236));
#152796=CARTESIAN_POINT('Ctrl Pts',(4.4479272014945,-5.41973893953439,35.4921215899432));
#152797=CARTESIAN_POINT('Ctrl Pts',(4.58197456985542,-5.30972756395464,
35.4999843483565));
#152798=CARTESIAN_POINT('Ctrl Pts',(4.71181878303615,-5.194837411621,35.5078471067697));
#152799=CARTESIAN_POINT('Ctrl Pts',(4.8370880053887,-5.0754513287613,35.515709865183));
#152800=CARTESIAN_POINT('Ctrl Pts',(4.92898370940593,-4.98787141145826,
35.5214778719315));
#152801=CARTESIAN_POINT('Ctrl Pts',(5.01841814621858,-4.89787280850003,
35.52724587868));
#152802=CARTESIAN_POINT('Ctrl Pts',(5.10525833230909,-4.80561795432061,
35.5330138854284));
#152803=CARTESIAN_POINT('Ctrl Pts',(5.23025566707761,-4.67282677305959,
35.5413163258416));
#152804=CARTESIAN_POINT('Ctrl Pts',(5.3501682762267,-4.53505011661643,35.5496187662548));
#152805=CARTESIAN_POINT('Ctrl Pts',(5.46458990420554,-4.39270801913295,
35.557921206668));
#152806=CARTESIAN_POINT('Ctrl Pts',(5.57892382502303,-4.25047503057869,
35.5662172830441));
#152807=CARTESIAN_POINT('Ctrl Pts',(5.68777494342812,-4.10368383910192,
35.5745133594202));
#152808=CARTESIAN_POINT('Ctrl Pts',(5.79077567238571,-3.95278935368505,
35.5828094357964));
#152809=CARTESIAN_POINT('Ctrl Pts',(5.89370860513702,-3.80199418866874,
35.5911000516043));
#152810=CARTESIAN_POINT('Ctrl Pts',(5.99079863748047,-3.64710139406454,
35.5993906674122));
#152811=CARTESIAN_POINT('Ctrl Pts',(6.08171995297363,-3.48859699250321,
35.6076812832201));
#152812=CARTESIAN_POINT('Ctrl Pts',(6.1726072499452,-3.33015189590659,35.6159687970657));
#152813=CARTESIAN_POINT('Ctrl Pts',(6.25733026206948,-3.16809817812648,
35.6242563109114));
#152814=CARTESIAN_POINT('Ctrl Pts',(6.33560751908777,-3.00294920479493,
35.632543824757));
#152815=CARTESIAN_POINT('Ctrl Pts',(6.4138673460344,-2.83783700534318,35.640829493214));
#152816=CARTESIAN_POINT('Ctrl Pts',(6.48568413442165,-2.66963122940047,
35.649115161671));
#152817=CARTESIAN_POINT('Ctrl Pts',(6.55082310083938,-2.49886839669661,
35.6574008301279));
#152818=CARTESIAN_POINT('Ctrl Pts',(6.61595742777563,-2.32811772646699,
35.6656859084435));
#152819=CARTESIAN_POINT('Ctrl Pts',(6.67441476136455,-2.1548106784762,35.673970986759));
#152820=CARTESIAN_POINT('Ctrl Pts',(6.72600894094853,-1.97950253568426,
35.6822560650745));
#152821=CARTESIAN_POINT('Ctrl Pts',(6.77762160673699,-1.804131579951,35.6905441119352));
#152822=CARTESIAN_POINT('Ctrl Pts',(6.82236610686468,-1.62675842037421,
35.6988321587958));
#152823=CARTESIAN_POINT('Ctrl Pts',(6.8601063107952,-1.44795302654742,35.7071202056565));
#152824=CARTESIAN_POINT('Ctrl Pts',(6.8978531132488,-1.26911637026325,35.715409701605));
#152825=CARTESIAN_POINT('Ctrl Pts',(6.92859311351629,-1.08884731231442,
35.7236991975534));
#152826=CARTESIAN_POINT('Ctrl Pts',(6.95224146597921,-0.907725267478727,
35.7319886935019));
#152827=CARTESIAN_POINT('Ctrl Pts',(6.97590646120624,-0.726475756195862,
35.7402840232659));
#152828=CARTESIAN_POINT('Ctrl Pts',(6.9924697976193,-0.544372394531557,
35.7485793530299));
#152829=CARTESIAN_POINT('Ctrl Pts',(7.00189850003828,-0.36199994152164,
35.7568746827938));
#152830=CARTESIAN_POINT('Ctrl Pts',(7.00821044961767,-0.239912545301506,
35.7624279074994));
#152831=CARTESIAN_POINT('Ctrl Pts',(7.01132609200597,-0.117704634689895,
35.767981132205));
#152832=CARTESIAN_POINT('Ctrl Pts',(7.01124858877614,0.00444846991387958,
35.7735343569106));
#152833=CARTESIAN_POINT('Ctrl Pts',(7.01124858877573,0.00444847055756476,
35.7735343569399));
#152834=CARTESIAN_POINT('Ctrl Pts',(7.01109817222245,0.241520478409522,
35.7843119309956));
#152835=CARTESIAN_POINT('Ctrl Pts',(6.99891979680166,0.478179014117121,
35.7950895050514));
#152836=CARTESIAN_POINT('Ctrl Pts',(6.97486124732339,0.713398306058046,
35.8058670791071));
#152837=CARTESIAN_POINT('Ctrl Pts',(6.9503880517275,0.95267157333437,35.8168304033156));
#152838=CARTESIAN_POINT('Ctrl Pts',(6.91362159642911,1.19045596317276,35.827793727524));
#152839=CARTESIAN_POINT('Ctrl Pts',(6.86476735121365,1.4256913327264,35.8387570517325));
#152840=CARTESIAN_POINT('Ctrl Pts',(6.84754912788099,1.50859784598541,35.8426209731554));
#152841=CARTESIAN_POINT('Ctrl Pts',(6.82882987788821,1.59118788002895,35.8464848945784));
#152842=CARTESIAN_POINT('Ctrl Pts',(6.80862007451949,1.67341544254565,35.8503488160013));
#152843=CARTESIAN_POINT('Ctrl Pts',(6.76477985634542,1.85178799842287,35.8587306470908));
#152844=CARTESIAN_POINT('Ctrl Pts',(6.71387483226996,2.02864465740253,35.8671124781804));
#152845=CARTESIAN_POINT('Ctrl Pts',(6.65602251740218,2.2034043683208,35.8754943092699));
#152846=CARTESIAN_POINT('Ctrl Pts',(6.62920495534626,2.28441459933983,35.8793797246746));
#152847=CARTESIAN_POINT('Ctrl Pts',(6.60089528170328,2.36497433156186,35.8832651400793));
#152848=CARTESIAN_POINT('Ctrl Pts',(6.57110895151814,2.44502632087637,35.887150555484));
#152849=CARTESIAN_POINT('',(7.01124948002267,-0.00270025589932498,35.2264656431181));
#152850=CARTESIAN_POINT('Ctrl Pts',(6.57110895151813,2.44502632087638,35.339859805629));
#152851=CARTESIAN_POINT('Ctrl Pts',(6.63282047719562,2.27917405363134,35.3318421344416));
#152852=CARTESIAN_POINT('Ctrl Pts',(6.68826026819073,2.11095325019693,35.3238244632542));
#152853=CARTESIAN_POINT('Ctrl Pts',(6.73725316088305,1.94088804640335,35.3158067920668));
#152854=CARTESIAN_POINT('Ctrl Pts',(6.78626203881579,1.77076735429258,35.3077865049));
#152855=CARTESIAN_POINT('Ctrl Pts',(6.82881971018949,1.59880141134544,35.2997662177331));
#152856=CARTESIAN_POINT('Ctrl Pts',(6.86480108493105,1.42552889371963,35.2917459305662));
#152857=CARTESIAN_POINT('Ctrl Pts',(6.90078822874227,1.25222859446423,35.2837243574675));
#152858=CARTESIAN_POINT('Ctrl Pts',(6.93019690879352,1.07762166429827,35.2757027843688));
#152859=CARTESIAN_POINT('Ctrl Pts',(6.95295341791382,0.902255690378585,
35.2676812112701));
#152860=CARTESIAN_POINT('Ctrl Pts',(6.9757280400242,0.726750134323181,35.2596532534191));
#152861=CARTESIAN_POINT('Ctrl Pts',(6.99183987564174,0.550484692843579,
35.2516252955681));
#152862=CARTESIAN_POINT('Ctrl Pts',(7.0012671711373,0.374011444818397,35.2435973377171));
#152863=CARTESIAN_POINT('Ctrl Pts',(7.00797313340574,0.248479902585227,
35.2378867728508));
#152864=CARTESIAN_POINT('Ctrl Pts',(7.01129783084764,0.122843288533582,
35.2321762079845));
#152865=CARTESIAN_POINT('Ctrl Pts',(7.01124948002267,-0.00270025589932412,
35.2264656431181));
#152866=CARTESIAN_POINT('Ctrl Pts',(7.01124948002242,-0.00270025652633111,
35.2264656430896));
#152867=CARTESIAN_POINT('Ctrl Pts',(7.01124302160634,-0.0194696138004879,
35.2257028599221));
#152868=CARTESIAN_POINT('Ctrl Pts',(7.01117640060358,-0.0362375540527687,
35.2249400767546));
#152869=CARTESIAN_POINT('Ctrl Pts',(7.01104964859509,-0.0530036549186942,
35.2241772935871));
#152870=CARTESIAN_POINT('Ctrl Pts',(7.00942932847339,-0.267331229823478,
35.2144263402928));
#152871=CARTESIAN_POINT('Ctrl Pts',(6.99797781269597,-0.481439247429157,
35.2046753869986));
#152872=CARTESIAN_POINT('Ctrl Pts',(6.97676695775352,-0.694513772144772,
35.1949244337043));
#152873=CARTESIAN_POINT('Ctrl Pts',(6.95552554459554,-0.907895270684285,
35.1851594323327));
#152874=CARTESIAN_POINT('Ctrl Pts',(6.92449667164411,-1.12024025957128,
35.175394430961));
#152875=CARTESIAN_POINT('Ctrl Pts',(6.88380409671614,-1.33073953895348,
35.1656294295893));
#152876=CARTESIAN_POINT('Ctrl Pts',(6.84317934787919,-1.54088795965175,
35.1558807044516));
#152877=CARTESIAN_POINT('Ctrl Pts',(6.79292309638973,-1.74919678212994,
35.146131979314));
#152878=CARTESIAN_POINT('Ctrl Pts',(6.73320959005129,-1.95486960663398,
35.1363832541763));
#152879=CARTESIAN_POINT('Ctrl Pts',(6.67365997413402,-2.1599779389838,35.1266612855091));
#152880=CARTESIAN_POINT('Ctrl Pts',(6.60470493240658,-2.36246467808975,
35.1169393168419));
#152881=CARTESIAN_POINT('Ctrl Pts',(6.52656815093536,-2.56154928387025,
35.1072173481747));
#152882=CARTESIAN_POINT('Ctrl Pts',(6.44894838013919,-2.7593165988117,35.0975597072349));
#152883=CARTESIAN_POINT('Ctrl Pts',(6.36226796450537,-2.95372659967752,
35.0879020662952));
#152884=CARTESIAN_POINT('Ctrl Pts',(6.26679656646663,-3.14402407068108,
35.0782444253554));
#152885=CARTESIAN_POINT('Ctrl Pts',(6.22483360015293,-3.22766636072133,
35.0739995596705));
#152886=CARTESIAN_POINT('Ctrl Pts',(6.18117295769982,-3.31051428342778,
35.0697546939856));
#152887=CARTESIAN_POINT('Ctrl Pts',(6.13584066416399,-3.39250437088761,
35.0655098283007));
#152888=CARTESIAN_POINT('Ctrl Pts',(6.05198825043613,-3.54416373332055,
35.0576579812868));
#152889=CARTESIAN_POINT('Ctrl Pts',(5.96244740792944,-3.69282388791708,
35.049806134273));
#152890=CARTESIAN_POINT('Ctrl Pts',(5.8674743568157,-3.83801657560389,35.0419542872591));
#152891=CARTESIAN_POINT('Ctrl Pts',(5.77252823929148,-3.98316808781822,
35.0341046669656));
#152892=CARTESIAN_POINT('Ctrl Pts',(5.67215318614924,-4.12485377024618,
35.0262550466721));
#152893=CARTESIAN_POINT('Ctrl Pts',(5.56665003843469,-4.26263227502621,
35.0184054263786));
#152894=CARTESIAN_POINT('Ctrl Pts',(5.46115531379702,-4.40039977995492,
35.0105564327769));
#152895=CARTESIAN_POINT('Ctrl Pts',(5.3505335421293,-4.53426042580745,35.0027074391751));
#152896=CARTESIAN_POINT('Ctrl Pts',(5.23512717183371,-4.66380424731017,
34.9948584455734));
#152897=CARTESIAN_POINT('Ctrl Pts',(5.1196623746722,-4.79341365305638,34.987005478256));
#152898=CARTESIAN_POINT('Ctrl Pts',(4.99940839307808,-4.91870158254952,
34.9791525109387));
#152899=CARTESIAN_POINT('Ctrl Pts',(4.8747462545793,-5.03929315638266,34.9712995436213));
#152900=CARTESIAN_POINT('Ctrl Pts',(4.7500524560862,-5.15991535642348,34.9634445819141));
#152901=CARTESIAN_POINT('Ctrl Pts',(4.62094855420437,-5.27583856974625,
34.955589620207));
#152902=CARTESIAN_POINT('Ctrl Pts',(4.48784978047786,-5.38672729125625,
34.9477346584998));
#152903=CARTESIAN_POINT('Ctrl Pts',(4.35461889509275,-5.49772607909148,
34.9398719000865));
#152904=CARTESIAN_POINT('Ctrl Pts',(4.21738552007152,-5.60368016150462,
34.9320091416732));
#152905=CARTESIAN_POINT('Ctrl Pts',(4.07659552794209,-5.70429622863877,
34.92414638326));
#152906=CARTESIAN_POINT('Ctrl Pts',(3.9733140099245,-5.77810673173918,34.9183783765114));
#152907=CARTESIAN_POINT('Ctrl Pts',(3.86811914002211,-5.84904548256678,
34.9126103697629));
#152908=CARTESIAN_POINT('Ctrl Pts',(3.76119543936316,-5.91701237360662,
34.9068423630144));
#152909=CARTESIAN_POINT('Ctrl Pts',(3.60588808496919,-6.01573471457243,
34.8984642965733));
#152910=CARTESIAN_POINT('Ctrl Pts',(3.44658844908803,-6.10840427875434,
34.8900862301323));
#152911=CARTESIAN_POINT('Ctrl Pts',(3.28379637756903,-6.19469998572687,
34.8817081636913));
#152912=CARTESIAN_POINT('Ctrl Pts',(3.12111562133438,-6.28093668472027,
34.8733358260725));
#152913=CARTESIAN_POINT('Ctrl Pts',(2.95494748011312,-6.36080806232932,
34.8649634884538));
#152914=CARTESIAN_POINT('Ctrl Pts',(2.78581836668374,-6.43403781387299,
34.8565911508351));
#152915=CARTESIAN_POINT('Ctrl Pts',(2.61678009883622,-6.50722823097416,
34.8482233103125));
#152916=CARTESIAN_POINT('Ctrl Pts',(2.44478433097249,-6.57378400487779,
34.8398554697899));
#152917=CARTESIAN_POINT('Ctrl Pts',(2.2703799385927,-6.63347582319675,34.8314876292673));
#152918=CARTESIAN_POINT('Ctrl Pts',(2.09604367636725,-6.6931443232223,34.8231230575974));
#152919=CARTESIAN_POINT('Ctrl Pts',(1.91930097649018,-6.74595410840673,
34.8147584859275));
#152920=CARTESIAN_POINT('Ctrl Pts',(1.74071888859076,-6.7917246935814,34.8063939142575));
#152921=CARTESIAN_POINT('Ctrl Pts',(1.5621804227333,-6.83748409842768,34.798031385792));
#152922=CARTESIAN_POINT('Ctrl Pts',(1.38180378309701,-6.87620765116248,
34.7896688573264));
#152923=CARTESIAN_POINT('Ctrl Pts',(1.20016975603081,-6.90776513202418,
34.7813063288608));
#152924=CARTESIAN_POINT('Ctrl Pts',(1.01852123400088,-6.93932513127159,
34.7729431330393));
#152925=CARTESIAN_POINT('Ctrl Pts',(0.835615446853467,-6.96371785390745,
34.7645799372178));
#152926=CARTESIAN_POINT('Ctrl Pts',(0.652042683505966,-6.98086433770105,
34.7562167413963));
#152927=CARTESIAN_POINT('Ctrl Pts',(0.468457400863963,-6.99801199085048,
34.7478529752216));
#152928=CARTESIAN_POINT('Ctrl Pts',(0.2842053786976,-7.00791238895933,34.7394892090469));
#152929=CARTESIAN_POINT('Ctrl Pts',(0.0998815072620535,-7.01053851333883,
34.7311254428721));
#152930=CARTESIAN_POINT('Ctrl Pts',(-0.0844795093998785,-7.01316516693891,
34.7227599912186));
#152931=CARTESIAN_POINT('Ctrl Pts',(-0.268912075450206,-7.00851461905335,
34.714394539565));
#152932=CARTESIAN_POINT('Ctrl Pts',(-0.452821386676273,-6.99661199111889,
34.7060290879115));
#152933=CARTESIAN_POINT('Ctrl Pts',(-0.636792288769169,-6.98470537701773,
34.6976608346846));
#152934=CARTESIAN_POINT('Ctrl Pts',(-0.820239258643686,-6.96554186118292,
34.6892925814577));
#152935=CARTESIAN_POINT('Ctrl Pts',(-1.00257226334437,-6.93919847095272,
34.6809243282308));
#152936=CARTESIAN_POINT('Ctrl Pts',(-1.18507431675295,-6.91283065664149,
34.6725483164394));
#152937=CARTESIAN_POINT('Ctrl Pts',(-1.3664600153948,-6.87926971278993,
34.6641723046479));
#152938=CARTESIAN_POINT('Ctrl Pts',(-1.54614794455608,-6.83864409777589,
34.6557962928564));
#152939=CARTESIAN_POINT('Ctrl Pts',(-1.72592399489802,-6.79799855945829,
34.6474161733653));
#152940=CARTESIAN_POINT('Ctrl Pts',(-1.90400029633817,-6.75028151973047,
34.6390360538741));
#152941=CARTESIAN_POINT('Ctrl Pts',(-2.07980962689676,-6.69567162265053,
34.630655934383));
#152942=CARTESIAN_POINT('Ctrl Pts',(-2.25581984188595,-6.64099932684553,
34.6222662395437));
#152943=CARTESIAN_POINT('Ctrl Pts',(-2.42955759793642,-6.57941853965937,
34.6138765447045));
#152944=CARTESIAN_POINT('Ctrl Pts',(-2.60047345402414,-6.51115691543491,
34.6054868498653));
#152945=CARTESIAN_POINT('Ctrl Pts',(-2.70898498160337,-6.46781878818804,
34.6001603773907));
#152946=CARTESIAN_POINT('Ctrl Pts',(-2.81635948020739,-6.42178874201992,
34.5948339049161));
#152947=CARTESIAN_POINT('Ctrl Pts',(-2.9224612963494,-6.37313474938667,
34.5895074324415));
#152948=CARTESIAN_POINT('Ctrl Pts',(-3.08941441566749,-6.2965768153874,
34.5811261320365));
#152949=CARTESIAN_POINT('Ctrl Pts',(-3.25355202745786,-6.21336537748145,
34.5727448316316));
#152950=CARTESIAN_POINT('Ctrl Pts',(-3.41432559772511,-6.12372495097707,
34.5643635312266));
#152951=CARTESIAN_POINT('Ctrl Pts',(-3.57489541102764,-6.03419813059084,
34.555992852893));
#152952=CARTESIAN_POINT('Ctrl Pts',(-3.73210939552516,-5.93825871759483,
34.5476221745593));
#152953=CARTESIAN_POINT('Ctrl Pts',(-3.88543996300208,-5.83617878893428,
34.5392514962257));
#152954=CARTESIAN_POINT('Ctrl Pts',(-4.03859652661053,-5.73421470346647,
34.5308903171748));
#152955=CARTESIAN_POINT('Ctrl Pts',(-4.18787818577808,-5.62612417165473,
34.5225291381239));
#152956=CARTESIAN_POINT('Ctrl Pts',(-4.33278251433605,-5.51222480002075,
34.514167959073));
#152957=CARTESIAN_POINT('Ctrl Pts',(-4.47749881243468,-5.39847322625713,
34.5058176296382));
#152958=CARTESIAN_POINT('Ctrl Pts',(-4.61784885310891,-5.27892804884745,
34.4974673002034));
#152959=CARTESIAN_POINT('Ctrl Pts',(-4.75335980002938,-5.1539496673876,
34.4891169707686));
#152960=CARTESIAN_POINT('Ctrl Pts',(-4.88876647938222,-5.02906744931628,
34.4807730664128));
#152961=CARTESIAN_POINT('Ctrl Pts',(-5.01934124519349,-4.89876057941237,
34.472429162057));
#152962=CARTESIAN_POINT('Ctrl Pts',(-5.14464404041121,-4.7634298840186,
34.4640852577012));
#152963=CARTESIAN_POINT('Ctrl Pts',(-5.26984619164242,-4.62820788708329,
34.4557480552214));
#152964=CARTESIAN_POINT('Ctrl Pts',(-5.38978459538553,-4.48797035194954,
34.4474108527416));
#152965=CARTESIAN_POINT('Ctrl Pts',(-5.50405569882937,-4.34315523861213,
34.4390736502618));
#152966=CARTESIAN_POINT('Ctrl Pts',(-5.54167311531509,-4.2954829026701,
34.4363290892262));
#152967=CARTESIAN_POINT('Ctrl Pts',(-5.57867667316407,-4.24731479163512,
34.4335845281906));
#152968=CARTESIAN_POINT('Ctrl Pts',(-5.61505288383928,-4.19866736884315,
34.430839967155));
#152969=CARTESIAN_POINT('Ctrl Pts',(-5.7255682370334,-4.05087058044642,
34.4225016568532));
#152970=CARTESIAN_POINT('Ctrl Pts',(-5.83019934000186,-3.89876854558231,
34.4141633465514));
#152971=CARTESIAN_POINT('Ctrl Pts',(-5.92862524298497,-3.74286378201792,
34.4058250362496));
#152972=CARTESIAN_POINT('Ctrl Pts',(-6.02711307220633,-3.58686092846663,
34.3974814797659));
#152973=CARTESIAN_POINT('Ctrl Pts',(-6.119387739315,-3.42705085103788,34.3891379232822));
#152974=CARTESIAN_POINT('Ctrl Pts',(-6.20517366432427,-3.26396175805975,
34.3807943667985));
#152975=CARTESIAN_POINT('Ctrl Pts',(-6.29102485489143,-3.10074858761046,
34.3724444625734));
#152976=CARTESIAN_POINT('Ctrl Pts',(-6.37037730408053,-2.93425171523097,
34.3640945583483));
#152977=CARTESIAN_POINT('Ctrl Pts',(-6.44300289213029,-2.76502084883654,
34.3557446541232));
#152978=CARTESIAN_POINT('Ctrl Pts',(-6.51573741318775,-2.59553614866579,
34.3473822256597));
#152979=CARTESIAN_POINT('Ctrl Pts',(-6.5817247811968,-2.42330956117124,
34.3390197971961));
#152980=CARTESIAN_POINT('Ctrl Pts',(-6.64078572320307,-2.24890896681086,
34.3306573687326));
#152981=CARTESIAN_POINT('Ctrl Pts',(-6.699897170366,-2.07435923616785,34.3222877892528));
#152982=CARTESIAN_POINT('Ctrl Pts',(-6.75207028098247,-1.89763210282481,
34.3139182097729));
#152983=CARTESIAN_POINT('Ctrl Pts',(-6.79717641353081,-1.71930781590747,
34.3055486302931));
#152984=CARTESIAN_POINT('Ctrl Pts',(-6.84235211679289,-1.54070848550448,
34.2971661417566));
#152985=CARTESIAN_POINT('Ctrl Pts',(-6.88043899300769,-1.36050739883639,
34.2887836532202));
#152986=CARTESIAN_POINT('Ctrl Pts',(-6.91135973017388,-1.1792935353977,
34.2804011646837));
#152987=CARTESIAN_POINT('Ctrl Pts',(-6.92147750204344,-1.11999738990093,
34.2776582770787));
#152988=CARTESIAN_POINT('Ctrl Pts',(-6.93082840628247,-1.06059283284357,
34.2749153894737));
#152989=CARTESIAN_POINT('Ctrl Pts',(-6.93941094439624,-1.00110054804385,
34.2721725018687));
#152990=CARTESIAN_POINT('Ctrl Pts',(-6.96566293201507,-0.819127487944901,
34.2637826467358));
#152991=CARTESIAN_POINT('Ctrl Pts',(-6.98477516963711,-0.635966017424542,
34.255392791603));
#152992=CARTESIAN_POINT('Ctrl Pts',(-6.99665206940579,-0.452201705193195,
34.2470029364702));
#152993=CARTESIAN_POINT('Ctrl Pts',(-7.00851800933787,-0.268606968093,34.238620823378));
#152994=CARTESIAN_POINT('Ctrl Pts',(-7.01316190024741,-0.0844108247111611,
34.2302387102859));
#152995=CARTESIAN_POINT('Ctrl Pts',(-7.01053975293831,0.0997944636322941,
34.2218565971937));
#152996=CARTESIAN_POINT('Ctrl Pts',(-7.00791963985978,0.283856847713138,
34.2134809868448));
#152997=CARTESIAN_POINT('Ctrl Pts',(-6.99804473149739,0.467928035097267,
34.2051053764959));
#152998=CARTESIAN_POINT('Ctrl Pts',(-6.98092305719494,0.651413718019586,
34.196729766147));
#152999=CARTESIAN_POINT('Ctrl Pts',(-6.96381215267988,0.834783985722573,
34.1883594241814));
#153000=CARTESIAN_POINT('Ctrl Pts',(-6.93946360157599,1.01756915684159,
34.1799890822158));
#153001=CARTESIAN_POINT('Ctrl Pts',(-6.90793744792243,1.19917754235601,
34.1716187402501));
#153002=CARTESIAN_POINT('Ctrl Pts',(-6.87642650330757,1.38069831524898,
34.1632524363558));
#153003=CARTESIAN_POINT('Ctrl Pts',(-6.83774491737662,1.56104311134469,
34.1548861324614));
#153004=CARTESIAN_POINT('Ctrl Pts',(-6.79200432149817,1.73962750589032,
34.146519828567));
#153005=CARTESIAN_POINT('Ctrl Pts',(-6.74627651798235,1.91816195538625,
34.1381558644934));
#153006=CARTESIAN_POINT('Ctrl Pts',(-6.69349372113455,2.09493666658613,
34.1297919004197));
#153007=CARTESIAN_POINT('Ctrl Pts',(-6.63381833132013,2.26937897001383,
34.1214279363461));
#153008=CARTESIAN_POINT('Ctrl Pts',(-6.5741521245565,2.44379442966994,34.1130652593475));
#153009=CARTESIAN_POINT('Ctrl Pts',(-6.50759554590933,2.61587788629101,
34.1047025823489));
#153010=CARTESIAN_POINT('Ctrl Pts',(-6.43436051071591,2.78507295786657,
34.0963399053503));
#153011=CARTESIAN_POINT('Ctrl Pts',(-6.36112698329804,2.95426454602481,
34.087977400524));
#153012=CARTESIAN_POINT('Ctrl Pts',(-6.28121540442131,3.12056756626644,
34.0796148956976));
#153013=CARTESIAN_POINT('Ctrl Pts',(-6.19488554339137,3.28344630941038,
34.0712523908713));
#153014=CARTESIAN_POINT('Ctrl Pts',(-6.10854595257947,3.44634340975584,
34.0628889435512));
#153015=CARTESIAN_POINT('Ctrl Pts',(-6.01578679179923,3.60581517344633,
34.0545254962312));
#153016=CARTESIAN_POINT('Ctrl Pts',(-5.91691362816744,3.76135077855104,
34.0461620489112));
#153017=CARTESIAN_POINT('Ctrl Pts',(-5.81798224523829,3.916977967391,34.0377936769584));
#153018=CARTESIAN_POINT('Ctrl Pts',(-5.71292984129663,4.06866408812234,
34.0294253050055));
#153019=CARTESIAN_POINT('Ctrl Pts',(-5.60210571350595,4.21592672341492,
34.0210569330527));
#153020=CARTESIAN_POINT('Ctrl Pts',(-5.49124837991019,4.36323348244173,
34.0126860537169));
#153021=CARTESIAN_POINT('Ctrl Pts',(-5.37461607605661,4.50611385375815,
34.0043151743811));
#153022=CARTESIAN_POINT('Ctrl Pts',(-5.25259863226846,4.64411823393758,
33.9959442950453));
#153023=CARTESIAN_POINT('Ctrl Pts',(-5.13047780441964,4.78223954373601,
33.987566323154));
#153024=CARTESIAN_POINT('Ctrl Pts',(-5.00296294130388,4.915476364326,33.9791883512626));
#153025=CARTESIAN_POINT('Ctrl Pts',(-4.87048179498309,5.04341487954722,
33.9708103793713));
#153026=CARTESIAN_POINT('Ctrl Pts',(-4.78628894770581,5.1247208477702,33.9654861100127));
#153027=CARTESIAN_POINT('Ctrl Pts',(-4.70009109629953,5.20388774031651,
33.9601618406542));
#153028=CARTESIAN_POINT('Ctrl Pts',(-4.61200508624403,5.28081770627989,
33.9548375712957));
#153029=CARTESIAN_POINT('Ctrl Pts',(-4.48192049048814,5.39442716046626,
33.9469747401064));
#153030=CARTESIAN_POINT('Ctrl Pts',(-4.34744573065238,5.50339217667764,
33.9391119089171));
#153031=CARTESIAN_POINT('Ctrl Pts',(-4.20896128643917,5.60734085389469,
33.9312490777279));
#153032=CARTESIAN_POINT('Ctrl Pts',(-4.07058324924164,5.71120966027432,
33.9233922880865));
#153033=CARTESIAN_POINT('Ctrl Pts',(-3.92820195746167,5.81006956527347,
33.9155354984452));
#153034=CARTESIAN_POINT('Ctrl Pts',(-3.78223311582231,5.90358697912355,
33.9076787088038));
#153035=CARTESIAN_POINT('Ctrl Pts',(-3.63634659369978,5.99705165357913,
33.8998263500199));
#153036=CARTESIAN_POINT('Ctrl Pts',(-3.48687686637915,6.08517962522162,
33.8919739912359));
#153037=CARTESIAN_POINT('Ctrl Pts',(-3.33427073828417,6.16767907776677,
33.884121632452));
#153038=CARTESIAN_POINT('Ctrl Pts',(-3.1817006422766,6.2501590512286,33.8762711277016));
#153039=CARTESIAN_POINT('Ctrl Pts',(-3.02599595045765,6.32701296201526,
33.8684206229512));
#153040=CARTESIAN_POINT('Ctrl Pts',(-2.86763027165357,6.39799368455425,
33.8605701182008));
#153041=CARTESIAN_POINT('Ctrl Pts',(-2.70929006889604,6.46896298853206,
33.8527208763492));
#153042=CARTESIAN_POINT('Ctrl Pts',(-2.54829008070091,6.53406083180059,
33.8448716344975));
#153043=CARTESIAN_POINT('Ctrl Pts',(-2.38512577786037,6.59308740927086,
33.8370223926459));
#153044=CARTESIAN_POINT('Ctrl Pts',(-2.22190650177241,6.65213387395047,
33.8291705062311));
#153045=CARTESIAN_POINT('Ctrl Pts',(-2.05652181359439,6.70510485710954,
33.8213186198162));
#153046=CARTESIAN_POINT('Ctrl Pts',(-1.88948448865828,6.75184974133902,
33.8134667334014));
#153047=CARTESIAN_POINT('Ctrl Pts',(-1.76683106002812,6.78617392800723,
33.8077011909374));
#153048=CARTESIAN_POINT('Ctrl Pts',(-1.64328693966225,6.81714216116094,
33.8019356484734));
#153049=CARTESIAN_POINT('Ctrl Pts',(-1.51905916836066,6.84471225147701,
33.7961701060094));
#153050=CARTESIAN_POINT('Ctrl Pts',(-1.31102029788735,6.89088268815237,
33.7865148016494));
#153051=CARTESIAN_POINT('Ctrl Pts',(-1.10117014471705,6.92749892086688,
33.7768594972894));
#153052=CARTESIAN_POINT('Ctrl Pts',(-0.890310616186968,6.95449304904425,
33.7672041929294));
#153053=CARTESIAN_POINT('Ctrl Pts',(-0.678282965425719,6.98163671962767,
33.7574953999946));
#153054=CARTESIAN_POINT('Ctrl Pts',(-0.465234778571069,6.99905142935194,
33.7477866070598));
#153055=CARTESIAN_POINT('Ctrl Pts',(-0.251976881838503,7.00672064617386,
33.738077814125));
#153056=CARTESIAN_POINT('Ctrl Pts',(-0.0376927699988857,7.01442676791832,
33.7283223016542));
#153057=CARTESIAN_POINT('Ctrl Pts',(0.176803030758819,7.01229340123778,
33.7185667891834));
#153058=CARTESIAN_POINT('Ctrl Pts',(0.390693177463751,7.00035609119874,
33.7088112767126));
#153059=CARTESIAN_POINT('Ctrl Pts',(0.604795108320485,6.98840696138623,
33.6990461047835));
#153060=CARTESIAN_POINT('Ctrl Pts',(0.818290147948013,6.96663448446964,
33.6892809328545));
#153061=CARTESIAN_POINT('Ctrl Pts',(1.03036436579813,6.93512623073246,33.6795157609255));
#153062=CARTESIAN_POINT('Ctrl Pts',(1.24214942526335,6.90366093778445,33.6697639035869));
#153063=CARTESIAN_POINT('Ctrl Pts',(1.45251749730597,6.86248640460992,33.6600120462483));
#153064=CARTESIAN_POINT('Ctrl Pts',(1.66066435004057,6.81174136906301,33.6502601889097));
#153065=CARTESIAN_POINT('Ctrl Pts',(1.75143145253539,6.7896128584366,33.6460076728474));
#153066=CARTESIAN_POINT('Ctrl Pts',(1.84177625504733,6.7656650905832,33.6417551567851));
#153067=CARTESIAN_POINT('Ctrl Pts',(1.93163247853303,6.73991265005537,33.6375026407228));
#153068=CARTESIAN_POINT('Ctrl Pts',(2.10137178816052,6.69126603096936,33.629469595124));
#153069=CARTESIAN_POINT('Ctrl Pts',(2.2694494660046,6.63615233030146,33.6214365495252));
#153070=CARTESIAN_POINT('Ctrl Pts',(2.43533104611058,6.57470830214923,33.6134035039265));
#153071=CARTESIAN_POINT('Ctrl Pts',(2.60110599114994,6.51330377258407,33.6053756222787));
#153072=CARTESIAN_POINT('Ctrl Pts',(2.76468730623457,6.44557714252613,33.597347740631));
#153073=CARTESIAN_POINT('Ctrl Pts',(2.92555509387023,6.37171515019543,33.5893198589832));
#153074=CARTESIAN_POINT('Ctrl Pts',(3.08635024811383,6.29788650728245,33.5812956020031));
#153075=CARTESIAN_POINT('Ctrl Pts',(3.24443398195006,6.21792817047563,33.5732713450231));
#153076=CARTESIAN_POINT('Ctrl Pts',(3.39930586596518,6.13207519459071,33.565247088043));
#153077=CARTESIAN_POINT('Ctrl Pts',(3.55415902439219,6.04623259920498,33.5572238012774));
#153078=CARTESIAN_POINT('Ctrl Pts',(3.70580078236128,5.95449695524091,33.5492005145117));
#153079=CARTESIAN_POINT('Ctrl Pts',(3.85375468587841,5.8571495954577,33.5411772277461));
#153080=CARTESIAN_POINT('Ctrl Pts',(4.00169646589286,5.75981021242229,33.5331545984172));
#153081=CARTESIAN_POINT('Ctrl Pts',(4.1459506892983,5.65686023438918,33.5251319690883));
#153082=CARTESIAN_POINT('Ctrl Pts',(4.28606956806187,5.54862453408355,33.5171093397594));
#153083=CARTESIAN_POINT('Ctrl Pts',(4.42624112154857,5.44034814486009,33.5090836944931));
#153084=CARTESIAN_POINT('Ctrl Pts',(4.5622739363716,5.32678229050574,33.5010580492267));
#153085=CARTESIAN_POINT('Ctrl Pts',(4.69375272997403,5.20829260625412,33.4930324039604));
#153086=CARTESIAN_POINT('Ctrl Pts',(4.77128063860812,5.13842386801091,33.4882999944524));
#153087=CARTESIAN_POINT('Ctrl Pts',(4.8472257603242,5.06684386173666,33.4835675849445));
#153088=CARTESIAN_POINT('Ctrl Pts',(4.92150891237664,4.99363360569208,33.4788351754365));
#153089=CARTESIAN_POINT('Ctrl Pts',(5.05853405375793,4.85858756351571,33.4701056174683));
#153090=CARTESIAN_POINT('Ctrl Pts',(5.18997071682224,4.7179250387306,33.4613760595001));
#153091=CARTESIAN_POINT('Ctrl Pts',(5.31538360554547,4.57212463614001,33.4526465015319));
#153092=CARTESIAN_POINT('Ctrl Pts',(5.44083371828673,4.42628095827788,33.4439143525284));
#153093=CARTESIAN_POINT('Ctrl Pts',(5.56025630903054,4.27529656607037,33.4351822035249));
#153094=CARTESIAN_POINT('Ctrl Pts',(5.67325609237645,4.11968346755105,33.4264500545214));
#153095=CARTESIAN_POINT('Ctrl Pts',(5.78630777788146,3.96399889406464,33.4177138947368));
#153096=CARTESIAN_POINT('Ctrl Pts',(5.89293059881551,3.80368158680107,33.4089777349523));
#153097=CARTESIAN_POINT('Ctrl Pts',(5.99277161017516,3.6392739647873,33.4002415751678));
#153098=CARTESIAN_POINT('Ctrl Pts',(6.09262680060904,3.47484299417315,33.3915041747041));
#153099=CARTESIAN_POINT('Ctrl Pts',(6.18569811946792,3.30632078499796,33.3827667742404));
#153100=CARTESIAN_POINT('Ctrl Pts',(6.27167754167765,3.1342762124159,33.3740293737768));
#153101=CARTESIAN_POINT('Ctrl Pts',(6.35767791546194,2.9621897157944,33.3652898441723));
#153102=CARTESIAN_POINT('Ctrl Pts',(6.43658281800373,2.78657938614114,33.3565503145678));
#153103=CARTESIAN_POINT('Ctrl Pts',(6.50813099130387,2.60803710911676,33.3478107849634));
#153104=CARTESIAN_POINT('Ctrl Pts',(6.52980024043262,2.55396337246626,33.3451639103398));
#153105=CARTESIAN_POINT('Ctrl Pts',(6.5507950217826,2.49962084380071,33.3425170357163));
#153106=CARTESIAN_POINT('Ctrl Pts',(6.57110895151813,2.44502632087639,33.3398701610928));
#153107=CARTESIAN_POINT('Origin',(0.,0.,50.));
#153108=CARTESIAN_POINT('',(6.57110895151815,2.44502632087633,31.3397623334207));
#153109=CARTESIAN_POINT('',(6.57110895151813,2.44502632087638,31.8871164994866));
#153110=CARTESIAN_POINT('',(6.57110895151814,2.44502632087636,50.));
#153111=CARTESIAN_POINT('',(7.01124984252467,-0.00148600059847291,33.7735343568733));
#153112=CARTESIAN_POINT('Ctrl Pts',(6.57110895151814,2.44502632087638,31.8871164994866));
#153113=CARTESIAN_POINT('Ctrl Pts',(6.50762598931832,2.6156393967432,31.8953699009264));
#153114=CARTESIAN_POINT('Ctrl Pts',(6.43748316425011,2.78380827029697,31.9036233023662));
#153115=CARTESIAN_POINT('Ctrl Pts',(6.36090066196278,2.94899463057184,31.911876703806));
#153116=CARTESIAN_POINT('Ctrl Pts',(6.28432000714449,3.11417700590656,31.9201299061415));
#153117=CARTESIAN_POINT('Ctrl Pts',(6.20130012895755,3.27637670157163,31.928383108477));
#153118=CARTESIAN_POINT('Ctrl Pts',(6.11210852405168,3.43507728482414,31.9366363108125));
#153119=CARTESIAN_POINT('Ctrl Pts',(6.02290496113898,3.59379914522106,31.9448906196631));
#153120=CARTESIAN_POINT('Ctrl Pts',(5.92752819059685,3.74902066080693,31.9531449285136));
#153121=CARTESIAN_POINT('Ctrl Pts',(5.82629077728874,3.90025157406291,31.9613992373641));
#153122=CARTESIAN_POINT('Ctrl Pts',(5.72499006368819,4.05157704683718,31.9696587073517));
#153123=CARTESIAN_POINT('Ctrl Pts',(5.61782157723185,4.19890664855539,31.9779181773393));
#153124=CARTESIAN_POINT('Ctrl Pts',(5.50514067103692,4.34177990628212,31.9861776473268));
#153125=CARTESIAN_POINT('Ctrl Pts',(5.39241852474357,4.48470545420964,31.9944401401988));
#153126=CARTESIAN_POINT('Ctrl Pts',(5.27418015407174,4.62317114316824,32.0027026330708));
#153127=CARTESIAN_POINT('Ctrl Pts',(5.15082027315724,4.75675068467252,32.0109651259428));
#153128=CARTESIAN_POINT('Ctrl Pts',(5.02735435984748,4.89044504274954,32.019234720734));
#153129=CARTESIAN_POINT('Ctrl Pts',(4.89875838211137,5.01924462032444,32.0275043155252));
#153130=CARTESIAN_POINT('Ctrl Pts',(4.76546346532463,5.14276039915882,32.0357739103165));
#153131=CARTESIAN_POINT('Ctrl Pts',(4.73024018932418,5.1753995310415,32.0379591565866));
#153132=CARTESIAN_POINT('Ctrl Pts',(4.69468897339523,5.20766992130522,32.0401444028568));
#153133=CARTESIAN_POINT('Ctrl Pts',(4.65881814938141,5.2395648687171,32.042329649127));
#153134=CARTESIAN_POINT('Ctrl Pts',(4.52974975206116,5.35432748870817,32.0501924803163));
#153135=CARTESIAN_POINT('Ctrl Pts',(4.39625003216115,5.46448492412669,32.0580553115057));
#153136=CARTESIAN_POINT('Ctrl Pts',(4.25869614464996,5.5696619026691,32.065918142695));
#153137=CARTESIAN_POINT('Ctrl Pts',(4.12124794914417,5.67475806658689,32.0737749323364));
#153138=CARTESIAN_POINT('Ctrl Pts',(3.9797520817573,5.77488115372705,32.0816317219779));
#153139=CARTESIAN_POINT('Ctrl Pts',(3.83462126202782,5.86969388804085,32.0894885116194));
#153140=CARTESIAN_POINT('Ctrl Pts',(3.68957228921087,5.96445315246049,32.0973408704034));
#153141=CARTESIAN_POINT('Ctrl Pts',(3.54089276005286,6.05390781349602,32.1051932291874));
#153142=CARTESIAN_POINT('Ctrl Pts',(3.38902686431709,6.13776209016259,32.1130455879714));
#153143=CARTESIAN_POINT('Ctrl Pts',(3.23719682589128,6.22159656785603,32.1208960927218));
#153144=CARTESIAN_POINT('Ctrl Pts',(3.0821822476397,6.29983310144248,32.1287465974723));
#153145=CARTESIAN_POINT('Ctrl Pts',(2.92445452038378,6.37222036033806,32.1365971022228));
#153146=CARTESIAN_POINT('Ctrl Pts',(2.76675216654805,6.44459597440511,32.1444463440744));
#153147=CARTESIAN_POINT('Ctrl Pts',(2.60633788058183,6.51112403055832,32.1522955859261));
#153148=CARTESIAN_POINT('Ctrl Pts',(2.44370533552698,6.57160032226679,32.1601448277778));
#153149=CARTESIAN_POINT('Ctrl Pts',(2.2810179963844,6.63209698962167,32.1679967141927));
#153150=CARTESIAN_POINT('Ctrl Pts',(2.11611126323491,6.68653768674299,32.1758486006076));
#153151=CARTESIAN_POINT('Ctrl Pts',(1.94949655071189,6.73476723883331,32.1837004870225));
#153152=CARTESIAN_POINT('Ctrl Pts',(1.8271534411247,6.77018159863009,32.1894660294862));
#153153=CARTESIAN_POINT('Ctrl Pts',(1.70388980936199,6.80224806436027,32.1952315719499));
#153154=CARTESIAN_POINT('Ctrl Pts',(1.5799123125686,6.83092260584865,32.2009971144136));
#153155=CARTESIAN_POINT('Ctrl Pts',(1.37229256597395,6.87894261908909,32.2106524187732));
#153156=CARTESIAN_POINT('Ctrl Pts',(1.16277658247089,6.91742492590143,32.2203077231329));
#153157=CARTESIAN_POINT('Ctrl Pts',(0.952165633372154,6.94629449196656,
32.2299630274926));
#153158=CARTESIAN_POINT('Ctrl Pts',(0.740387939123326,6.97532399001214,
32.2396718204272));
#153159=CARTESIAN_POINT('Ctrl Pts',(0.52750316803832,6.99463399454275,32.2493806133618));
#153160=CARTESIAN_POINT('Ctrl Pts',(0.314321967100086,7.00420075836625,
32.2590894062964));
#153161=CARTESIAN_POINT('Ctrl Pts',(0.100114920123539,7.0138135582695,32.2688449187669));
#153162=CARTESIAN_POINT('Ctrl Pts',(-0.114391372164453,7.01358914327749,
32.2786004312374));
#153163=CARTESIAN_POINT('Ctrl Pts',(-0.328379282832671,7.00355578325084,
32.2883559437079));
#153164=CARTESIAN_POINT('Ctrl Pts',(-0.542579074453864,6.99351248865416,
32.2981211156366));
#153165=CARTESIAN_POINT('Ctrl Pts',(-0.756259420008023,6.97364083503563,
32.3078862875653));
#153166=CARTESIAN_POINT('Ctrl Pts',(-0.968605641862296,6.94402114578092,
32.317651459494));
#153167=CARTESIAN_POINT('Ctrl Pts',(-1.18066233446117,6.91444184230044,
32.3274033168324));
#153168=CARTESIAN_POINT('Ctrl Pts',(-1.39138850140542,6.87514107285008,
32.3371551741707));
#153169=CARTESIAN_POINT('Ctrl Pts',(-1.59997870798422,6.82625041267145,
32.346907031509));
#153170=CARTESIAN_POINT('Ctrl Pts',(-1.69093914489552,6.80493054399847,
32.3511595475727));
#153171=CARTESIAN_POINT('Ctrl Pts',(-1.78149348870259,6.78178773195593,
32.3554120636363));
#153172=CARTESIAN_POINT('Ctrl Pts',(-1.87157533319403,6.75683597068034,
32.3596645796999));
#153173=CARTESIAN_POINT('Ctrl Pts',(-2.04174084311919,6.70970184276628,
32.3676976252988));
#153174=CARTESIAN_POINT('Ctrl Pts',(-2.2103023397027,6.65608610196862,32.3757306708977));
#153175=CARTESIAN_POINT('Ctrl Pts',(-2.37672416113583,6.59612074058482,
32.3837637164966));
#153176=CARTESIAN_POINT('Ctrl Pts',(-2.54303900021432,6.53619392724419,
32.3917915981445));
#153177=CARTESIAN_POINT('Ctrl Pts',(-2.70721655861343,6.46992574194481,
32.3998194797924));
#153178=CARTESIAN_POINT('Ctrl Pts',(-2.86873529758317,6.39749828877667,
32.4078473614403));
#153179=CARTESIAN_POINT('Ctrl Pts',(-3.03018110924926,6.32510353731797,
32.4158716184204));
#153180=CARTESIAN_POINT('Ctrl Pts',(-3.18897015799944,6.24655520489625,
32.4238958754005));
#153181=CARTESIAN_POINT('Ctrl Pts',(-3.34459994240831,6.16208388353667,
32.4319201323807));
#153182=CARTESIAN_POINT('Ctrl Pts',(-3.50021090959193,6.07762277561976,
32.4399434191465));
#153183=CARTESIAN_POINT('Ctrl Pts',(-3.65266304762526,5.98724027320072,
32.4479667059122));
#153184=CARTESIAN_POINT('Ctrl Pts',(-3.80147741771086,5.89121345778053,
32.455989992678));
#153185=CARTESIAN_POINT('Ctrl Pts',(-3.95027959378598,5.79519451090147,
32.464012622007));
#153186=CARTESIAN_POINT('Ctrl Pts',(-4.09544428977,5.69353237444891,32.472035251336));
#153187=CARTESIAN_POINT('Ctrl Pts',(-4.23652084421534,5.58654792327328,
32.480057880665));
#153188=CARTESIAN_POINT('Ctrl Pts',(-4.37765043340174,5.47952325356036,
32.4880835259314));
#153189=CARTESIAN_POINT('Ctrl Pts',(-4.51468852047096,5.3671724962097,32.4961091711979));
#153190=CARTESIAN_POINT('Ctrl Pts',(-4.64721658540546,5.24985757624266,
32.5041348164644));
#153191=CARTESIAN_POINT('Ctrl Pts',(-4.72536320834495,5.18068155061841,
32.5088672259717));
#153192=CARTESIAN_POINT('Ctrl Pts',(-4.80194233617012,5.10978023899885,
32.5135996354791));
#153193=CARTESIAN_POINT('Ctrl Pts',(-4.87687406826338,5.03723395176363,
32.5183320449864));
#153194=CARTESIAN_POINT('Ctrl Pts',(-5.01510337395136,4.90340516341685,
32.527062093821));
#153195=CARTESIAN_POINT('Ctrl Pts',(-5.14779378229039,4.76390974366043,
32.5357921426555));
#153196=CARTESIAN_POINT('Ctrl Pts',(-5.27450568218276,4.61922248556202,
32.54452219149));
#153197=CARTESIAN_POINT('Ctrl Pts',(-5.40125422097954,4.47449339096188,
32.5532547646291));
#153198=CARTESIAN_POINT('Ctrl Pts',(-5.52202062028321,4.32456966757488,
32.5619873377682));
#153199=CARTESIAN_POINT('Ctrl Pts',(-5.63640499889543,4.16995986202824,
32.5707199109073));
#153200=CARTESIAN_POINT('Ctrl Pts',(-5.75241439019912,4.01315357738816,
32.5795765441878));
#153201=CARTESIAN_POINT('Ctrl Pts',(-5.86185887281638,3.85152728226869,
32.5884331774682));
#153202=CARTESIAN_POINT('Ctrl Pts',(-5.96436600366898,3.68564305607282,
32.5972898107487));
#153203=CARTESIAN_POINT('Ctrl Pts',(-6.06550159581761,3.52197834996995,
32.6060279428553));
#153204=CARTESIAN_POINT('Ctrl Pts',(-6.15988419962545,3.35416919531648,
32.6147660749619));
#153205=CARTESIAN_POINT('Ctrl Pts',(-6.24720130009147,3.18278219151664,
32.6235042070686));
#153206=CARTESIAN_POINT('Ctrl Pts',(-6.33629461178435,3.00790881999889,
32.6324200909359));
#153207=CARTESIAN_POINT('Ctrl Pts',(-6.41803174921255,2.82931074059938,
32.6413359748033));
#153208=CARTESIAN_POINT('Ctrl Pts',(-6.49213095548987,2.64761443931519,
32.6502518586706));
#153209=CARTESIAN_POINT('Ctrl Pts',(-6.56623016176718,2.46591813803099,
32.659167742538));
#153210=CARTESIAN_POINT('Ctrl Pts',(-6.63269132832819,2.28112389718056,
32.6680836264054));
#153211=CARTESIAN_POINT('Ctrl Pts',(-6.69128520431699,2.0938789069544,32.6769995102727));
#153212=CARTESIAN_POINT('Ctrl Pts',(-6.74872769583583,1.91031332810334,
32.685740194769));
#153213=CARTESIAN_POINT('Ctrl Pts',(-6.79861531624983,1.72437292502866,
32.6944808792653));
#153214=CARTESIAN_POINT('Ctrl Pts',(-6.84077743513127,1.53668169947419,
32.7032215637616));
#153215=CARTESIAN_POINT('Ctrl Pts',(-6.88293196834713,1.34902424268907,
32.7119606756636));
#153216=CARTESIAN_POINT('Ctrl Pts',(-6.9173637158717,1.15961685954915,32.7206997875655));
#153217=CARTESIAN_POINT('Ctrl Pts',(-6.94395283789062,0.969095221147462,
32.7294388994675));
#153218=CARTESIAN_POINT('Ctrl Pts',(-6.97088646025336,0.776105100714336,
32.7382912391418));
#153219=CARTESIAN_POINT('Ctrl Pts',(-6.98977275377,0.581971929352691,32.7471435788161));
#153220=CARTESIAN_POINT('Ctrl Pts',(-7.00054105897722,0.387364742941425,
32.7559959184904));
#153221=CARTESIAN_POINT('Ctrl Pts',(-7.01116618111522,0.195345192533053,
32.7647305511403));
#153222=CARTESIAN_POINT('Ctrl Pts',(-7.01388785773924,0.00286443576630693,
32.7734651837901));
#153223=CARTESIAN_POINT('Ctrl Pts',(-7.0086904969564,-0.189430938268088,
32.78219981644));
#153224=CARTESIAN_POINT('Ctrl Pts',(-7.00338807751271,-0.38561334176364,
32.7911110096265));
#153225=CARTESIAN_POINT('Ctrl Pts',(-6.98984304867562,-0.581602497256222,
32.8000222028131));
#153226=CARTESIAN_POINT('Ctrl Pts',(-6.96809478004038,-0.776712108103157,
32.8089333959996));
#153227=CARTESIAN_POINT('Ctrl Pts',(-6.94634651140514,-0.971821718950125,
32.8178445891861));
#153228=CARTESIAN_POINT('Ctrl Pts',(-6.91639502316164,-1.16605148239483,
32.8267557823727));
#153229=CARTESIAN_POINT('Ctrl Pts',(-6.87833604413308,-1.35871992201471,
32.8356669755592));
#153230=CARTESIAN_POINT('Ctrl Pts',(-6.84405908436904,-1.53224240005324,
32.8436926404116));
#153231=CARTESIAN_POINT('Ctrl Pts',(-6.80318963512244,-1.70457808617821,
32.8517183052639));
#153232=CARTESIAN_POINT('Ctrl Pts',(-6.75583514478471,-1.87518480662354,
32.8597439701162));
#153233=CARTESIAN_POINT('Ctrl Pts',(-6.70849568360071,-2.04573738068047,
32.8677670878194));
#153234=CARTESIAN_POINT('Ctrl Pts',(-6.65467537691853,-2.21456172873366,
32.8757902055225));
#153235=CARTESIAN_POINT('Ctrl Pts',(-6.59453233375685,-2.3811278549325,
32.8838133232257));
#153236=CARTESIAN_POINT('Ctrl Pts',(-6.53439687515926,-2.54767297568509,
32.8918354291435));
#153237=CARTESIAN_POINT('Ctrl Pts',(-6.46794039333055,-2.71196009735109,
32.8998575350613));
#153238=CARTESIAN_POINT('Ctrl Pts',(-6.39537020827451,-2.87347637220403,
32.9078796409791));
#153239=CARTESIAN_POINT('Ctrl Pts',(-6.32277305589253,-3.03505266705039,
32.9159047279386));
#153240=CARTESIAN_POINT('Ctrl Pts',(-6.24405780943784,-3.19385572224353,
32.9239298148981));
#153241=CARTESIAN_POINT('Ctrl Pts',(-6.15947929165377,-3.34939418674309,
32.9319549018575));
#153242=CARTESIAN_POINT('Ctrl Pts',(-6.07488411655371,-3.50496328376517,
32.9399815693177));
#153243=CARTESIAN_POINT('Ctrl Pts',(-5.98442355254028,-3.65726619141962,
32.9480082367779));
#153244=CARTESIAN_POINT('Ctrl Pts',(-5.8883972550525,-3.80583819009561,
32.9560349042381));
#153245=CARTESIAN_POINT('Ctrl Pts',(-5.79229386799168,-3.95452946184827,
32.9640680154786));
#153246=CARTESIAN_POINT('Ctrl Pts',(-5.69061603018767,-4.09948353977782,
32.9721011267192));
#153247=CARTESIAN_POINT('Ctrl Pts',(-5.58370576002964,-4.24026609399833,
32.9801342379597));
#153248=CARTESIAN_POINT('Ctrl Pts',(-5.52071034512014,-4.32322028915685,
32.9848676389217));
#153249=CARTESIAN_POINT('Ctrl Pts',(-5.45589900390423,-4.40472675175332,
32.9896010398836));
#153250=CARTESIAN_POINT('Ctrl Pts',(-5.38934796350373,-4.48470234137989,
32.9943344408456));
#153251=CARTESIAN_POINT('Ctrl Pts',(-5.25225074908031,-4.6494545450072,
33.00408539414));
#153252=CARTESIAN_POINT('Ctrl Pts',(-5.10768840988505,-4.80780577014889,
33.0138363474343));
#153253=CARTESIAN_POINT('Ctrl Pts',(-4.95623241000825,-4.95917199343639,
33.0235873007287));
#153254=CARTESIAN_POINT('Ctrl Pts',(-4.80455820934961,-5.11075628816571,
33.0333523021006));
#153255=CARTESIAN_POINT('Ctrl Pts',(-4.64597050918983,-5.25533542435829,
33.0431173034725));
#153256=CARTESIAN_POINT('Ctrl Pts',(-4.48107791694203,-5.39236193748106,
33.0528823048444));
#153257=CARTESIAN_POINT('Ctrl Pts',(-4.31646016648299,-5.52916005579566,
33.0626310299821));
#153258=CARTESIAN_POINT('Ctrl Pts',(-4.14555855621277,-5.65843068642626,
33.0723797551198));
#153259=CARTESIAN_POINT('Ctrl Pts',(-3.96901263390927,-5.77966826680984,
33.0821284802576));
#153260=CARTESIAN_POINT('Ctrl Pts',(-3.79295126170702,-5.90057309704499,
33.0918504489248));
#153261=CARTESIAN_POINT('Ctrl Pts',(-3.61127653653412,-6.01348886887274,
33.1015724175921));
#153262=CARTESIAN_POINT('Ctrl Pts',(-3.42465619383811,-6.11795362163741,
33.1112943862594));
#153263=CARTESIAN_POINT('Ctrl Pts',(-3.23927066920705,-6.22172715841779,
33.1209520271993));
#153264=CARTESIAN_POINT('Ctrl Pts',(-3.04900478506897,-6.31716109486227,
33.1306096681391));
#153265=CARTESIAN_POINT('Ctrl Pts',(-2.85454578800082,-6.40384219876683,
33.140267309079));
#153266=CARTESIAN_POINT('Ctrl Pts',(-2.76907436399434,-6.4419415281724,
33.1445121747634));
#153267=CARTESIAN_POINT('Ctrl Pts',(-2.6827932943079,-6.47835041455719,
33.1487570404477));
#153268=CARTESIAN_POINT('Ctrl Pts',(-2.59576293581742,-6.51303626149406,
33.1530019061321));
#153269=CARTESIAN_POINT('Ctrl Pts',(-2.43478044279226,-6.57719564460401,
33.160853753146));
#153270=CARTESIAN_POINT('Ctrl Pts',(-2.27129897621931,-6.63542977659479,
33.1687056001598));
#153271=CARTESIAN_POINT('Ctrl Pts',(-2.10581350796627,-6.68753886210516,
33.1765574471737));
#153272=CARTESIAN_POINT('Ctrl Pts',(-1.94037497005416,-6.73963316990016,
33.1844070674672));
#153273=CARTESIAN_POINT('Ctrl Pts',(-1.77293392443771,-6.78560577197313,
33.1922566877607));
#153274=CARTESIAN_POINT('Ctrl Pts',(-1.60400279985007,-6.82530596974034,
33.2001063080542));
#153275=CARTESIAN_POINT('Ctrl Pts',(-1.43508516225289,-6.86500299795434,
33.207955301656));
#153276=CARTESIAN_POINT('Ctrl Pts',(-1.26467805402748,-6.89842853222061,
33.2158042952577));
#153277=CARTESIAN_POINT('Ctrl Pts',(-1.09330619583859,-6.9254825192647,
33.2236532888594));
#153278=CARTESIAN_POINT('Ctrl Pts',(-0.921847577095081,-6.95255020295039,
33.2315062561767));
#153279=CARTESIAN_POINT('Ctrl Pts',(-0.74942360978009,-6.97323983468652,
33.2393592234941));
#153280=CARTESIAN_POINT('Ctrl Pts',(-0.576566617006927,-6.98750295160247,
33.2472121908115));
#153281=CARTESIAN_POINT('Ctrl Pts',(-0.403665724365122,-7.00176969087091,
33.2550671525187));
#153282=CARTESIAN_POINT('Ctrl Pts',(-0.23033196829142,-7.00960664652511,
33.262922114226));
#153283=CARTESIAN_POINT('Ctrl Pts',(-0.0570991721866667,-7.01101749013905,
33.2707770759332));
#153284=CARTESIAN_POINT('Ctrl Pts',(0.116305571947877,-7.0124297341332,
33.2786398343465));
#153285=CARTESIAN_POINT('Ctrl Pts',(0.289608774828138,-7.00740313774596,
33.2865025927598));
#153286=CARTESIAN_POINT('Ctrl Pts',(0.462279656661582,-6.99599343063849,
33.2943653511731));
#153287=CARTESIAN_POINT('Ctrl Pts',(0.588948537902381,-6.9876234332235,
33.3001333579215));
#153288=CARTESIAN_POINT('Ctrl Pts',(0.715277210139274,-6.97581946807651,
33.30590136467));
#153289=CARTESIAN_POINT('Ctrl Pts',(0.841059499435936,-6.96062105568954,
33.3116693714184));
#153290=CARTESIAN_POINT('Ctrl Pts',(1.02375907362051,-6.9385452651557,33.3200474378595));
#153291=CARTESIAN_POINT('Ctrl Pts',(1.20571028047133,-6.90925737613366,
33.3284255043006));
#153292=CARTESIAN_POINT('Ctrl Pts',(1.38632299124725,-6.8728258472363,33.3368035707416));
#153293=CARTESIAN_POINT('Ctrl Pts',(1.56681220119751,-6.83641922978552,
33.3451759083604));
#153294=CARTESIAN_POINT('Ctrl Pts',(1.74596441859894,-6.7928787759688,33.3535482459792));
#153295=CARTESIAN_POINT('Ctrl Pts',(1.92319734510185,-6.74232441627464,
33.3619205835979));
#153296=CARTESIAN_POINT('Ctrl Pts',(2.10033507316078,-6.69179721122085,
33.3702884241206));
#153297=CARTESIAN_POINT('Ctrl Pts',(2.27555525047526,-6.63426370215943,
33.3786562646432));
#153298=CARTESIAN_POINT('Ctrl Pts',(2.44828798851151,-6.56989440461643,
33.3870241051658));
#153299=CARTESIAN_POINT('Ctrl Pts',(2.62095324941777,-6.50555025259886,
33.3953886768358));
#153300=CARTESIAN_POINT('Ctrl Pts',(2.79113270119787,-6.43437575180299,
33.4037532485058));
#153301=CARTESIAN_POINT('Ctrl Pts',(2.95827334529808,-6.35659070390716,
33.4121178201758));
#153302=CARTESIAN_POINT('Ctrl Pts',(3.12537316214558,-6.27882465647543,
33.4204803486415));
#153303=CARTESIAN_POINT('Ctrl Pts',(3.28943535406032,-6.19445142109821,
33.4288428771072));
#153304=CARTESIAN_POINT('Ctrl Pts',(3.44992815628357,-6.10373838552914,
33.4372054055729));
#153305=CARTESIAN_POINT('Ctrl Pts',(3.61043376633267,-6.01301811077708,
33.4455686013944));
#153306=CARTESIAN_POINT('Ctrl Pts',(3.76736912850284,-5.91595718150947,
33.4539317972159));
#153307=CARTESIAN_POINT('Ctrl Pts',(3.92022761570562,-5.81286865528192,
33.4622949930375));
#153308=CARTESIAN_POINT('Ctrl Pts',(4.07309652755098,-5.70977309862342,
33.4706587592122));
#153309=CARTESIAN_POINT('Ctrl Pts',(4.22188773728259,-5.60064930899922,
33.4790225253869));
#153310=CARTESIAN_POINT('Ctrl Pts',(4.36612398131493,-5.48585343791526,
33.4873862915617));
#153311=CARTESIAN_POINT('Ctrl Pts',(4.51038929205391,-5.37103443299327,
33.4957517432153));
#153312=CARTESIAN_POINT('Ctrl Pts',(4.65009754948598,-5.25054127210444,
33.5041171948688));
#153313=CARTESIAN_POINT('Ctrl Pts',(4.78480460374487,-5.12477038182999,
33.5124826465224));
#153314=CARTESIAN_POINT('Ctrl Pts',(4.91955677113244,-4.99895737113069,
33.5208508997494));
#153315=CARTESIAN_POINT('Ctrl Pts',(5.04930415533888,-4.86786333088658,
33.5292191529763));
#153316=CARTESIAN_POINT('Ctrl Pts',(5.17363919570639,-4.73192181202844,
33.5375874062033));
#153317=CARTESIAN_POINT('Ctrl Pts',(5.29808951239366,-4.59585425598923,
33.5459634179948));
#153318=CARTESIAN_POINT('Ctrl Pts',(5.41711723562476,-4.45493048323752,
33.5543394297862));
#153319=CARTESIAN_POINT('Ctrl Pts',(5.53035406856111,-4.30961836348065,
33.5627154415777));
#153320=CARTESIAN_POINT('Ctrl Pts',(5.64364643423984,-4.16423498086432,
33.5710955610689));
#153321=CARTESIAN_POINT('Ctrl Pts',(5.75114204946101,-4.01445922273378,
33.5794756805601));
#153322=CARTESIAN_POINT('Ctrl Pts',(5.85251540366539,-3.86078878111187,
33.5878558000513));
#153323=CARTESIAN_POINT('Ctrl Pts',(5.95400458976775,-3.70694275154522,
33.5962454948905));
#153324=CARTESIAN_POINT('Ctrl Pts',(6.04935736084891,-3.54919342420882,
33.6046351897297));
#153325=CARTESIAN_POINT('Ctrl Pts',(6.1382930230822,-3.38806513002339,33.613024884569));
#153326=CARTESIAN_POINT('Ctrl Pts',(6.1947567402894,-3.28576755660341,33.6183513570431));
#153327=CARTESIAN_POINT('Ctrl Pts',(6.24863480532729,-3.18210848943555,
33.6236778295173));
#153328=CARTESIAN_POINT('Ctrl Pts',(6.299865374172,-3.07722648334644,33.6290043019914));
#153329=CARTESIAN_POINT('Ctrl Pts',(6.38140366550722,-2.91029685985858,
33.6374818862576));
#153330=CARTESIAN_POINT('Ctrl Pts',(6.45639289574677,-2.73994110069037,
33.6459594705238));
#153331=CARTESIAN_POINT('Ctrl Pts',(6.52454701389006,-2.56669297463455,
33.65443705479));
#153332=CARTESIAN_POINT('Ctrl Pts',(6.59260653858626,-2.39368530561771,
33.6629028727251));
#153333=CARTESIAN_POINT('Ctrl Pts',(6.6538497482956,-2.21779356304895,33.6713686906602));
#153334=CARTESIAN_POINT('Ctrl Pts',(6.70803706498751,-2.03957478344232,
33.6798345085954));
#153335=CARTESIAN_POINT('Ctrl Pts',(6.76212856497949,-1.86167113911769,
33.6882853568515));
#153336=CARTESIAN_POINT('Ctrl Pts',(6.80918896995622,-1.68144896544347,
33.6967362051076));
#153337=CARTESIAN_POINT('Ctrl Pts',(6.84902733914818,-1.49948360114435,
33.7051870533637));
#153338=CARTESIAN_POINT('Ctrl Pts',(6.88882413540738,-1.31770812498592,
33.7136290828215));
#153339=CARTESIAN_POINT('Ctrl Pts',(6.92141385003952,-1.13419338926625,
33.7220711122792));
#153340=CARTESIAN_POINT('Ctrl Pts',(6.94665528797605,-0.949529816558885,
33.7305131417369));
#153341=CARTESIAN_POINT('Ctrl Pts',(6.97186394570614,-0.76510606022219,
33.7389442078149));
#153342=CARTESIAN_POINT('Ctrl Pts',(6.98974332037367,-0.579536753288603,
33.747375273893));
#153343=CARTESIAN_POINT('Ctrl Pts',(7.00020323955213,-0.393422377939883,
33.755806339971));
#153344=CARTESIAN_POINT('Ctrl Pts',(7.00753460280148,-0.262974707329013,
33.7617156789384));
#153345=CARTESIAN_POINT('Ctrl Pts',(7.0112221257058,-0.132259529340179,
33.7676250179058));
#153346=CARTESIAN_POINT('Ctrl Pts',(7.01124984252467,-0.00148600059851424,
33.7735343568733));
#153347=CARTESIAN_POINT('Ctrl Pts',(7.01124984252485,-0.00148599977195217,
33.7735343569106));
#153348=CARTESIAN_POINT('Ctrl Pts',(7.0112719456076,0.102800850313519,33.778246827033));
#153349=CARTESIAN_POINT('Ctrl Pts',(7.008966713201,0.207099752356633,33.7829592971554));
#153350=CARTESIAN_POINT('Ctrl Pts',(7.00433593370125,0.31129518204029,33.7876717672778));
#153351=CARTESIAN_POINT('Ctrl Pts',(6.99614033435056,0.495701283843723,
33.7960119435002));
#153352=CARTESIAN_POINT('Ctrl Pts',(6.98066136702986,0.679707727527018,
33.8043521197226));
#153353=CARTESIAN_POINT('Ctrl Pts',(6.9579693378657,0.862722003788445,33.8126922959449));
#153354=CARTESIAN_POINT('Ctrl Pts',(6.9352661934101,1.04582592637477,33.821036557456));
#153355=CARTESIAN_POINT('Ctrl Pts',(6.90534298778614,1.22793638792556,33.829380818967));
#153356=CARTESIAN_POINT('Ctrl Pts',(6.86832139437408,1.40847001603985,33.8377250804781));
#153357=CARTESIAN_POINT('Ctrl Pts',(6.83125253035464,1.58923415649754,33.8460799962661));
#153358=CARTESIAN_POINT('Ctrl Pts',(6.78706723451658,1.76841711894936,33.8544349120541));
#153359=CARTESIAN_POINT('Ctrl Pts',(6.73593781222904,1.94544811092022,33.8627898278421));
#153360=CARTESIAN_POINT('Ctrl Pts',(6.68723243189414,2.11408607726602,33.8707486377194));
#153361=CARTESIAN_POINT('Ctrl Pts',(6.63222621110177,2.28077116823723,33.8787074475966));
#153362=CARTESIAN_POINT('Ctrl Pts',(6.57110895151815,2.44502632087633,33.8866662574739));
#153363=CARTESIAN_POINT('',(7.01124989960866,0.00118648116847724,33.2264656430502));
#153364=CARTESIAN_POINT('Ctrl Pts',(6.57110895151813,2.44502632087639,33.3398701610928));
#153365=CARTESIAN_POINT('Ctrl Pts',(6.62151232165559,2.30956518744441,33.3333026774452));
#153366=CARTESIAN_POINT('Ctrl Pts',(6.66772295152383,2.17255230094966,33.3267351937976));
#153367=CARTESIAN_POINT('Ctrl Pts',(6.70965433379238,2.03424808799741,33.32016771015));
#153368=CARTESIAN_POINT('Ctrl Pts',(6.76495279892197,1.8518546088549,33.3115066132381));
#153369=CARTESIAN_POINT('Ctrl Pts',(6.81281612487184,1.66718451890023,33.3028455163263));
#153370=CARTESIAN_POINT('Ctrl Pts',(6.85308001335555,1.48085140815909,33.2941844194144));
#153371=CARTESIAN_POINT('Ctrl Pts',(6.8933350640091,1.29455919710369,33.2855252235932));
#153372=CARTESIAN_POINT('Ctrl Pts',(6.92599394708551,1.10660497441285,33.276866027772));
#153373=CARTESIAN_POINT('Ctrl Pts',(6.95094321879609,0.917613715880841,
33.2682068319508));
#153374=CARTESIAN_POINT('Ctrl Pts',(6.97588795117122,0.728656842910447,
33.2595492116063));
#153375=CARTESIAN_POINT('Ctrl Pts',(6.99312583458587,0.53866359506697,33.2508915912618));
#153376=CARTESIAN_POINT('Ctrl Pts',(7.0025950358404,0.348266171948085,33.2422339709172));
#153377=CARTESIAN_POINT('Ctrl Pts',(7.00834386225785,0.232674401700854,
33.2369778616413));
#153378=CARTESIAN_POINT('Ctrl Pts',(7.01123031221648,0.116933788887199,
33.2317217523655));
#153379=CARTESIAN_POINT('Ctrl Pts',(7.01124989960851,0.00118648203690645,
33.2264656430896));
#153380=CARTESIAN_POINT('Ctrl Pts',(7.01124989960866,0.00118648116847724,
33.2264656430502));
#153381=CARTESIAN_POINT('Ctrl Pts',(7.01128401231658,-0.200395074715246,
33.2173117826749));
#153382=CARTESIAN_POINT('Ctrl Pts',(7.00262022694572,-0.401968332958667,
33.2081579222996));
#153383=CARTESIAN_POINT('Ctrl Pts',(6.98528696967019,-0.602820465690959,
33.1990040619243));
#153384=CARTESIAN_POINT('Ctrl Pts',(6.96796416524755,-0.803551474172744,
33.1898557218015));
#153385=CARTESIAN_POINT('Ctrl Pts',(6.94198235289239,-1.00356203552825,
33.1807073816787));
#153386=CARTESIAN_POINT('Ctrl Pts',(6.90742184977378,-1.20214389811195,
33.1715590415559));
#153387=CARTESIAN_POINT('Ctrl Pts',(6.8947551776495,-1.27492557419297,33.1682061093251));
#153388=CARTESIAN_POINT('Ctrl Pts',(6.88093665415477,-1.34751538291487,
33.1648531770944));
#153389=CARTESIAN_POINT('Ctrl Pts',(6.865971977599,-1.4198786445768,33.1615002448636));
#153390=CARTESIAN_POINT('Ctrl Pts',(6.83015214277981,-1.59308920947274,
33.1534745800109));
#153391=CARTESIAN_POINT('Ctrl Pts',(6.78775064118185,-1.76505436076465,
33.1454489151583));
#153392=CARTESIAN_POINT('Ctrl Pts',(6.73887974192064,-1.93523290237419,
33.1374232503056));
#153393=CARTESIAN_POINT('Ctrl Pts',(6.69002435308418,-2.10535743348863,
33.1294001326021));
#153394=CARTESIAN_POINT('Ctrl Pts',(6.63470375542867,-2.27369613190525,
33.1213770148986));
#153395=CARTESIAN_POINT('Ctrl Pts',(6.57308076831546,-2.43972042982418,
33.1133538971951));
#153396=CARTESIAN_POINT('Ctrl Pts',(6.51146555240038,-2.60572379062571,
33.105331791277));
#153397=CARTESIAN_POINT('Ctrl Pts',(6.4435496582257,-2.76941298893526,33.0973096853589));
#153398=CARTESIAN_POINT('Ctrl Pts',(6.36954496158249,-2.93027704234244,
33.0892875794408));
#153399=CARTESIAN_POINT('Ctrl Pts',(6.29551276454375,-3.09120087337585,
33.081262492481));
#153400=CARTESIAN_POINT('Ctrl Pts',(6.21538739565959,-3.24929712768591,
33.0732374055212));
#153401=CARTESIAN_POINT('Ctrl Pts',(6.12942804027358,-3.4040767414393,33.0652123185614));
#153402=CARTESIAN_POINT('Ctrl Pts',(6.04345175562286,-3.55888683826276,
33.0571856511009));
#153403=CARTESIAN_POINT('Ctrl Pts',(5.9516393811973,-3.71037867707376,33.0491589836404));
#153404=CARTESIAN_POINT('Ctrl Pts',(5.85429469625917,-3.85809022339445,
33.0411323161799));
#153405=CARTESIAN_POINT('Ctrl Pts',(5.75687186335079,-4.00592035202432,
33.033099204939));
#153406=CARTESIAN_POINT('Ctrl Pts',(5.65390805893699,-4.14996382599031,
33.0250660936982));
#153407=CARTESIAN_POINT('Ctrl Pts',(5.54574915310466,-4.28978937633761,
33.0170329824573));
#153408=CARTESIAN_POINT('Ctrl Pts',(5.48201799672505,-4.3721796700122,33.0122995814972));
#153409=CARTESIAN_POINT('Ctrl Pts',(5.41648386978901,-4.45310612794275,
33.0075661805371));
#153410=CARTESIAN_POINT('Ctrl Pts',(5.34922373629297,-4.53248629138356,
33.0028327795771));
#153411=CARTESIAN_POINT('Ctrl Pts',(5.21066576797738,-4.69601189859285,
32.9930818262833));
#153412=CARTESIAN_POINT('Ctrl Pts',(5.06469993487682,-4.85307034624515,
32.9833308729896));
#153413=CARTESIAN_POINT('Ctrl Pts',(4.91190287586367,-5.00308271974213,
32.9735799196959));
#153414=CARTESIAN_POINT('Ctrl Pts',(4.75888568402282,-5.15331121420491,
32.9638149183247));
#153415=CARTESIAN_POINT('Ctrl Pts',(4.59901760761635,-5.29647330207611,
32.9540499169535));
#153416=CARTESIAN_POINT('Ctrl Pts',(4.43291210201972,-5.43202695669555,
32.9442849155823));
#153417=CARTESIAN_POINT('Ctrl Pts',(4.26708345988466,-5.56735467145881,
32.9345361904451));
#153418=CARTESIAN_POINT('Ctrl Pts',(4.09503819631533,-5.69509927453355,
32.9247874653079));
#153419=CARTESIAN_POINT('Ctrl Pts',(3.91742033292767,-5.81476091491859,
32.9150387401707));
#153420=CARTESIAN_POINT('Ctrl Pts',(3.74028996170514,-5.9340941304986,32.9053167715041));
#153421=CARTESIAN_POINT('Ctrl Pts',(3.55761755700346,-6.04538864900124,
32.8955948028374));
#153422=CARTESIAN_POINT('Ctrl Pts',(3.37007493896457,-6.14818847045721,
32.8858728341707));
#153423=CARTESIAN_POINT('Ctrl Pts',(3.18377324144409,-6.25030809234538,
32.8762151932314));
#153424=CARTESIAN_POINT('Ctrl Pts',(2.99266559446705,-6.34404501225384,
32.8665575522921));
#153425=CARTESIAN_POINT('Ctrl Pts',(2.79744289488201,-6.42899213037115,
32.8568999113528));
#153426=CARTESIAN_POINT('Ctrl Pts',(2.71163579726229,-6.46632931335396,
32.8526550456654));
#153427=CARTESIAN_POINT('Ctrl Pts',(2.62503412982007,-6.50196891495713,
32.8484101799781));
#153428=CARTESIAN_POINT('Ctrl Pts',(2.53769853712739,-6.53587887717953,
32.8441653142908));
#153429=CARTESIAN_POINT('Ctrl Pts',(2.37615144395421,-6.59860308454728,
32.8363134672768));
#153430=CARTESIAN_POINT('Ctrl Pts',(2.21215820690979,-6.65538003626377,
32.8284616202628));
#153431=CARTESIAN_POINT('Ctrl Pts',(2.04621555630433,-6.70601434979364,
32.8206097732488));
#153432=CARTESIAN_POINT('Ctrl Pts',(1.88031996569292,-6.75663430384158,
32.8127601529552));
#153433=CARTESIAN_POINT('Ctrl Pts',(1.71247642570658,-6.80111497362436,
32.8049105326615));
#153434=CARTESIAN_POINT('Ctrl Pts',(1.54319868590164,-6.83931022679418,
32.7970609123679));
#153435=CARTESIAN_POINT('Ctrl Pts',(1.37393446075989,-6.87750243056139,
32.789211918766));
#153436=CARTESIAN_POINT('Ctrl Pts',(1.20323663601684,-6.90941013345148,
32.7813629251642));
#153437=CARTESIAN_POINT('Ctrl Pts',(1.03163080196475,-6.93493795581024,
32.7735139315624));
#153438=CARTESIAN_POINT('Ctrl Pts',(0.859938088903061,-6.96047870215808,
32.7656609642449));
#153439=CARTESIAN_POINT('Ctrl Pts',(0.687336825835717,-6.97963305817761,
32.7578079969274));
#153440=CARTESIAN_POINT('Ctrl Pts',(0.514359746082859,-6.99235730023213,
32.7499550296099));
#153441=CARTESIAN_POINT('Ctrl Pts',(0.34133873596433,-7.00508477381656,
32.7421000679026));
#153442=CARTESIAN_POINT('Ctrl Pts',(0.167942100270191,-7.01137886621337,
32.7342451061953));
#153443=CARTESIAN_POINT('Ctrl Pts',(-0.00529639141246658,-7.01124799951749,
32.726390144488));
#153444=CARTESIAN_POINT('Ctrl Pts',(-0.178706836779513,-7.01111700292548,
32.7185273860745));
#153445=CARTESIAN_POINT('Ctrl Pts',(-0.351958443599177,-7.00454832457666,
32.7106646276611));
#153446=CARTESIAN_POINT('Ctrl Pts',(-0.524520949053849,-6.99160241550559,
32.7028018692477));
#153447=CARTESIAN_POINT('Ctrl Pts',(-0.651110326921706,-6.98210548237448,
32.6970338624999));
#153448=CARTESIAN_POINT('Ctrl Pts',(-0.77732894927321,-6.96917774512589,
32.6912658557521));
#153449=CARTESIAN_POINT('Ctrl Pts',(-0.902971002042146,-6.9528605574951,
32.6854978490043));
#153450=CARTESIAN_POINT('Ctrl Pts',(-1.08546688179907,-6.92915973881047,
32.6771197825633));
#153451=CARTESIAN_POINT('Ctrl Pts',(-1.26715024107038,-6.89825376719693,
32.6687417161223));
#153452=CARTESIAN_POINT('Ctrl Pts',(-1.44743158371919,-6.86021635030209,
32.6603636496813));
#153453=CARTESIAN_POINT('Ctrl Pts',(-1.6275896521276,-6.82220494294106,
32.6519913120625));
#153454=CARTESIAN_POINT('Ctrl Pts',(-1.8063472946246,-6.77707188003955,
32.6436189744438));
#153455=CARTESIAN_POINT('Ctrl Pts',(-1.98312330321943,-6.72494226939742,
32.6352466368251));
#153456=CARTESIAN_POINT('Ctrl Pts',(-2.15980435879847,-6.6728406595218,
32.6268787963025));
#153457=CARTESIAN_POINT('Ctrl Pts',(-2.33450558821199,-6.61375008798809,
32.61851095578));
#153458=CARTESIAN_POINT('Ctrl Pts',(-2.50665864296621,-6.54784613519154,
32.6101431152574));
#153459=CARTESIAN_POINT('Ctrl Pts',(-2.67874444704001,-6.48196792742563,
32.6017785435875));
#153460=CARTESIAN_POINT('Ctrl Pts',(-2.8482837549517,-6.40928176337756,
32.5934139719175));
#153461=CARTESIAN_POINT('Ctrl Pts',(-3.01472554613214,-6.33001235733378,
32.5850494002476));
#153462=CARTESIAN_POINT('Ctrl Pts',(-3.18112668076744,-6.25076231433675,
32.576686871782));
#153463=CARTESIAN_POINT('Ctrl Pts',(-3.34443151126597,-6.16493237783986,
32.5683243433164));
#153464=CARTESIAN_POINT('Ctrl Pts',(-3.50411067349647,-6.07279465735407,
32.5599618148507));
#153465=CARTESIAN_POINT('Ctrl Pts',(-3.66380257862292,-5.98064958399037,
32.5515986190292));
#153466=CARTESIAN_POINT('Ctrl Pts',(-3.81986794972493,-5.88219587998511,
32.5432354232077));
#153467=CARTESIAN_POINT('Ctrl Pts',(-3.97180296577638,-5.77775109913451,
32.5348722273862));
#153468=CARTESIAN_POINT('Ctrl Pts',(-4.12374834349135,-5.67329919535922,
32.5265084612115));
#153469=CARTESIAN_POINT('Ctrl Pts',(-4.27156253338215,-5.56285558611907,
32.5181446950368));
#153470=CARTESIAN_POINT('Ctrl Pts',(-4.41477146026969,-5.44678065613884,
32.5097809288621));
#153471=CARTESIAN_POINT('Ctrl Pts',(-4.5580092468382,-5.33068233456201,
32.5014154772085));
#153472=CARTESIAN_POINT('Ctrl Pts',(-4.69663966441671,-5.2089506363984,
32.4930500255549));
#153473=CARTESIAN_POINT('Ctrl Pts',(-4.83022210865503,-5.08198592516352,
32.4846845739013));
#153474=CARTESIAN_POINT('Ctrl Pts',(-4.96384928939157,-4.95497869369621,
32.4763163206744));
#153475=CARTESIAN_POINT('Ctrl Pts',(-5.09242488755258,-4.82273518098884,
32.4679480674475));
#153476=CARTESIAN_POINT('Ctrl Pts',(-5.21554521692894,-4.6856925478172,
32.4595798142205));
#153477=CARTESIAN_POINT('Ctrl Pts',(-5.33877969641471,-4.54852285657442,
32.4512038024291));
#153478=CARTESIAN_POINT('Ctrl Pts',(-5.45654858014128,-4.40654539832958,
32.4428277906376));
#153479=CARTESIAN_POINT('Ctrl Pts',(-5.56848774957778,-4.26023130185465,
32.4344517788462));
#153480=CARTESIAN_POINT('Ctrl Pts',(-5.68048181536616,-4.11384545113887,
32.426071659355));
#153481=CARTESIAN_POINT('Ctrl Pts',(-5.78664027108274,-3.96311898599499,
32.4176915398639));
#153482=CARTESIAN_POINT('Ctrl Pts',(-5.88664204818,-3.80855247556066,32.4093114203727));
#153483=CARTESIAN_POINT('Ctrl Pts',(-5.98675808997502,-3.6538093533089,
32.4009217255335));
#153484=CARTESIAN_POINT('Ctrl Pts',(-6.08070322304552,-3.49521769779045,
32.3925320306944));
#153485=CARTESIAN_POINT('Ctrl Pts',(-6.16820143086998,-3.3333043171474,
32.3841423358552));
#153486=CARTESIAN_POINT('Ctrl Pts',(-6.22375253308335,-3.23050830587529,
32.3788158633806));
#153487=CARTESIAN_POINT('Ctrl Pts',(-6.27670596914686,-3.12637386532124,
32.3734893909061));
#153488=CARTESIAN_POINT('Ctrl Pts',(-6.32700113052968,-3.02104009519505,
32.3681629184315));
#153489=CARTESIAN_POINT('Ctrl Pts',(-6.40614147312532,-2.85529551012004,
32.3597816180266));
#153490=CARTESIAN_POINT('Ctrl Pts',(-6.47885731027182,-2.6862460912205,
32.3514003176217));
#153491=CARTESIAN_POINT('Ctrl Pts',(-6.54487131078258,-2.51441565533529,
32.3430190172168));
#153492=CARTESIAN_POINT('Ctrl Pts',(-6.61080164821146,-2.34280298937334,
32.3346483388832));
#153493=CARTESIAN_POINT('Ctrl Pts',(-6.67004695930937,-2.16841663382883,
32.3262776605496));
#153494=CARTESIAN_POINT('Ctrl Pts',(-6.72237646680245,-1.9918035046361,
32.317906982216));
#153495=CARTESIAN_POINT('Ctrl Pts',(-6.77464658928913,-1.81539080102177,
32.3095458031651));
#153496=CARTESIAN_POINT('Ctrl Pts',(-6.82001645808053,-1.63675667260096,
32.3011846241143));
#153497=CARTESIAN_POINT('Ctrl Pts',(-6.85830378523821,-1.45646687291105,
32.2928234450634));
#153498=CARTESIAN_POINT('Ctrl Pts',(-6.89654143007242,-1.27641102050369,
32.2844731156287));
#153499=CARTESIAN_POINT('Ctrl Pts',(-6.92771479682381,-1.0947041010865,
32.2761227861939));
#153500=CARTESIAN_POINT('Ctrl Pts',(-6.95169173340734,-0.91192576790882,
32.2677724567592));
#153501=CARTESIAN_POINT('Ctrl Pts',(-6.9756502211722,-0.729288071726782,
32.2594285524035));
#153502=CARTESIAN_POINT('Ctrl Pts',(-6.99242327101026,-0.545580928129063,
32.2510846480479));
#153503=CARTESIAN_POINT('Ctrl Pts',(-7.00192979954321,-0.361394029791344,
32.2427407436922));
#153504=CARTESIAN_POINT('Ctrl Pts',(-7.01142869237322,-0.177355071517599,
32.2344035412125));
#153505=CARTESIAN_POINT('Ctrl Pts',(-7.01367268715593,0.00716254671880051,
32.2260663387328));
#153506=CARTESIAN_POINT('Ctrl Pts',(-7.00863251950209,0.191564007782966,
32.2177291362531));
#153507=CARTESIAN_POINT('Ctrl Pts',(-7.00697332413152,0.252267950892913,
32.2149845752171));
#153508=CARTESIAN_POINT('Ctrl Pts',(-7.00452516987978,0.312959274457857,
32.212240014181));
#153509=CARTESIAN_POINT('Ctrl Pts',(-7.00128824767276,0.373616695958923,
32.209495453145));
#153510=CARTESIAN_POINT('Ctrl Pts',(-6.99145408423799,0.557901321422113,
32.2011571428431));
#153511=CARTESIAN_POINT('Ctrl Pts',(-6.97434365674282,0.741721695672878,
32.1928188325413));
#153512=CARTESIAN_POINT('Ctrl Pts',(-6.95003248498712,0.924486354752603,
32.1844805222394));
#153513=CARTESIAN_POINT('Ctrl Pts',(-6.92570601746714,1.10736600315381,
32.1761369657556));
#153514=CARTESIAN_POINT('Ctrl Pts',(-6.89416981231609,1.28918828672469,
32.1677934092719));
#153515=CARTESIAN_POINT('Ctrl Pts',(-6.85555068412416,1.46937108311846,
32.1594498527881));
#153516=CARTESIAN_POINT('Ctrl Pts',(-6.81690217466752,1.64969096179987,
32.1510999485629));
#153517=CARTESIAN_POINT('Ctrl Pts',(-6.77116006214715,1.82836854530606,
32.1427500443377));
#153518=CARTESIAN_POINT('Ctrl Pts',(-6.71850137597883,2.00483561008641,
32.1344001401125));
#153519=CARTESIAN_POINT('Ctrl Pts',(-6.66576370567854,2.1815673624036,32.1260377116489));
#153520=CARTESIAN_POINT('Ctrl Pts',(-6.60608882429062,2.35608165611188,
32.1176752831853));
#153521=CARTESIAN_POINT('Ctrl Pts',(-6.53970290914599,2.52782760935304,
32.1093128547217));
#153522=CARTESIAN_POINT('Ctrl Pts',(-6.47326022499415,2.69972042879672,
32.1009432752418));
#153523=CARTESIAN_POINT('Ctrl Pts',(-6.4000951863851,2.86883988437988,32.0925736957619));
#153524=CARTESIAN_POINT('Ctrl Pts',(-6.32048077044012,3.03465803559424,
32.084204116282));
#153525=CARTESIAN_POINT('Ctrl Pts',(-6.2407435589583,3.20073194110455,32.0758216277455));
#153526=CARTESIAN_POINT('Ctrl Pts',(-6.15453724537031,3.36349407820791,
32.067439139209));
#153527=CARTESIAN_POINT('Ctrl Pts',(-6.06217981162978,3.52244268852857,
32.0590566506724));
#153528=CARTESIAN_POINT('Ctrl Pts',(-6.03195894594133,3.5744532783568,32.0563137630678));
#153529=CARTESIAN_POINT('Ctrl Pts',(-6.00107981224043,3.62605579680324,
32.0535708754633));
#153530=CARTESIAN_POINT('Ctrl Pts',(-5.96955451152326,3.67723340249872,
32.0508279878587));
#153531=CARTESIAN_POINT('Ctrl Pts',(-5.87312595003434,3.83377379340367,
32.0424381327259));
#153532=CARTESIAN_POINT('Ctrl Pts',(-5.77045400655895,3.98665241824335,
32.034048277593));
#153533=CARTESIAN_POINT('Ctrl Pts',(-5.66184044539724,4.13535842864485,
32.0256584224602));
#153534=CARTESIAN_POINT('Ctrl Pts',(-5.55332711130731,4.28392721522439,
32.0172763093681));
#153535=CARTESIAN_POINT('Ctrl Pts',(-5.43888328252145,4.42833079901656,
32.008894196276));
#153536=CARTESIAN_POINT('Ctrl Pts',(-5.31885462928466,4.56808625083165,
32.0005120831839));
#153537=CARTESIAN_POINT('Ctrl Pts',(-5.19891909284367,4.70773328203619,
31.9921364728351));
#153538=CARTESIAN_POINT('Ctrl Pts',(-5.07340758332518,4.842739121977,31.9837608624862));
#153539=CARTESIAN_POINT('Ctrl Pts',(-4.94270702263677,4.97265259704287,
31.9753852521374));
#153540=CARTESIAN_POINT('Ctrl Pts',(-4.81208867454161,5.10248435460403,
31.9670149101718));
#153541=CARTESIAN_POINT('Ctrl Pts',(-4.67628801592536,5.22722990298551,
31.9586445682062));
#153542=CARTESIAN_POINT('Ctrl Pts',(-4.53573022854585,5.34647340368915,
31.9502742262406));
#153543=CARTESIAN_POINT('Ctrl Pts',(-4.39524024990846,5.46565937821839,
31.9419079223462));
#153544=CARTESIAN_POINT('Ctrl Pts',(-4.24999796925914,5.57934838595688,
31.9335416184519));
#153545=CARTESIAN_POINT('Ctrl Pts',(-4.1004635238077,5.68716321661534,31.9251753145575));
#153546=CARTESIAN_POINT('Ctrl Pts',(-3.95097089894964,5.79494789448741,
31.9168113504839));
#153547=CARTESIAN_POINT('Ctrl Pts',(-3.79718876837405,5.8968614778718,31.9084473864103));
#153548=CARTESIAN_POINT('Ctrl Pts',(-3.63960871914783,5.99256830866392,
31.9000834223367));
#153549=CARTESIAN_POINT('Ctrl Pts',(-3.48205291887242,6.08826041176529,
31.8917207453381));
#153550=CARTESIAN_POINT('Ctrl Pts',(-3.32070064602085,6.17774749602488,
31.8833580683396));
#153551=CARTESIAN_POINT('Ctrl Pts',(-3.1560710710089,6.26073813198099,31.874995391341));
#153552=CARTESIAN_POINT('Ctrl Pts',(-2.99144488541913,6.34372705931151,
31.8666328865147));
#153553=CARTESIAN_POINT('Ctrl Pts',(-2.82354182586127,6.42021965745607,
31.8582703816884));
#153554=CARTESIAN_POINT('Ctrl Pts',(-2.65290456117458,6.48997102857934,
31.8499078768621));
#153555=CARTESIAN_POINT('Ctrl Pts',(-2.48224806486497,6.55973026101045,
31.8415444295421));
#153556=CARTESIAN_POINT('Ctrl Pts',(-2.30885705345371,6.62274662780922,
31.8331809822221));
#153557=CARTESIAN_POINT('Ctrl Pts',(-2.13329341539225,6.67882368133372,
31.8248175349022));
#153558=CARTESIAN_POINT('Ctrl Pts',(-1.95762640052625,6.73493375460345,
31.8164491629493));
#153559=CARTESIAN_POINT('Ctrl Pts',(-1.77978451576621,6.78409624865335,
31.8080807909965));
#153560=CARTESIAN_POINT('Ctrl Pts',(-1.60034502804635,6.82616454194501,
31.7997124190437));
#153561=CARTESIAN_POINT('Ctrl Pts',(-1.4208517755662,6.86824543999682,31.7913415397079));
#153562=CARTESIAN_POINT('Ctrl Pts',(-1.23976028689496,6.90322782899965,
31.7829706603722));
#153563=CARTESIAN_POINT('Ctrl Pts',(-1.05765792791444,6.93101625088412,
31.7745997810364));
#153564=CARTESIAN_POINT('Ctrl Pts',(-0.875401275574798,6.95882821759789,
31.7662218091451));
#153565=CARTESIAN_POINT('Ctrl Pts',(-0.692132367449455,6.97943399325733,
31.7578438372538));
#153566=CARTESIAN_POINT('Ctrl Pts',(-0.508444758329448,6.99278989318479,
31.7494658653626));
#153567=CARTESIAN_POINT('Ctrl Pts',(-0.391709786961072,7.0012776763461,
31.7441415960036));
#153568=CARTESIAN_POINT('Ctrl Pts',(-0.274805793214833,7.00683849559473,
31.7388173266447));
#153569=CARTESIAN_POINT('Ctrl Pts',(-0.157885183101994,7.00947207936924,
31.7334930572857));
#153570=CARTESIAN_POINT('Ctrl Pts',(0.0147820803083811,7.01336133125448,
31.7256302260964));
#153571=CARTESIAN_POINT('Ctrl Pts',(0.187844607514974,7.0108718598126,31.7177673949071));
#153572=CARTESIAN_POINT('Ctrl Pts',(0.360771993997862,7.00196187727745,
31.7099045637178));
#153573=CARTESIAN_POINT('Ctrl Pts',(0.533566508610325,6.99305874088779,
31.7020477740764));
#153574=CARTESIAN_POINT('Ctrl Pts',(0.706225710690218,6.97774492350381,
31.694190984435));
#153575=CARTESIAN_POINT('Ctrl Pts',(0.878216694434533,6.95603062098755,
31.6863341947936));
#153576=CARTESIAN_POINT('Ctrl Pts',(1.05011068340587,6.93432856430999,31.6784818360096));
#153577=CARTESIAN_POINT('Ctrl Pts',(1.22133682657994,6.9062332503719,31.6706294772256));
#153578=CARTESIAN_POINT('Ctrl Pts',(1.39136510250798,6.87180687403415,31.6627771184416));
#153579=CARTESIAN_POINT('Ctrl Pts',(1.56135323277611,6.83738862616555,31.6549266136912));
#153580=CARTESIAN_POINT('Ctrl Pts',(1.73014368368552,6.79664235836334,31.6470761089407));
#153581=CARTESIAN_POINT('Ctrl Pts',(1.89721448512012,6.749681752494,31.6392256041903));
#153582=CARTESIAN_POINT('Ctrl Pts',(2.06425841012786,6.70272870110622,31.6313763623386));
#153583=CARTESIAN_POINT('Ctrl Pts',(2.22958286988284,6.64956340787834,31.623527120487));
#153584=CARTESIAN_POINT('Ctrl Pts',(2.39267942529673,6.59034989437296,31.6156778786353));
#153585=CARTESIAN_POINT('Ctrl Pts',(2.5558309311327,6.53111643067581,31.6078259922204));
#153586=CARTESIAN_POINT('Ctrl Pts',(2.716752674362,6.46583080670773,31.5999741058056));
#153587=CARTESIAN_POINT('Ctrl Pts',(2.87495444244162,6.39470589756755,31.5921222193907));
#153588=CARTESIAN_POINT('Ctrl Pts',(2.99112003164114,6.34247976206145,31.5863566769269));
#153589=CARTESIAN_POINT('Ctrl Pts',(3.10581943799112,6.28710623658754,31.5805911344631));
#153590=CARTESIAN_POINT('Ctrl Pts',(3.21886666312162,6.22868557301974,31.5748255919993));
#153591=CARTESIAN_POINT('Ctrl Pts',(3.40818195696215,6.1308510169134,31.5651702876393));
#153592=CARTESIAN_POINT('Ctrl Pts',(3.59276685959477,6.02452017000735,31.5555149832794));
#153593=CARTESIAN_POINT('Ctrl Pts',(3.77196215332,5.91015465757213,31.5458596789194));
#153594=CARTESIAN_POINT('Ctrl Pts',(3.95215015534536,5.79515558165942,31.5361508859852));
#153595=CARTESIAN_POINT('Ctrl Pts',(4.12688865788375,5.67203264406426,31.5264420930509));
#153596=CARTESIAN_POINT('Ctrl Pts',(4.29554450562247,5.54129262561694,31.5167333001167));
#153597=CARTESIAN_POINT('Ctrl Pts',(4.46501193962845,5.409923475094,31.506977787646));
#153598=CARTESIAN_POINT('Ctrl Pts',(4.62833801798703,5.27086380472715,31.4972222751754));
#153599=CARTESIAN_POINT('Ctrl Pts',(4.78491794612142,5.12466455598659,31.4874667627048));
#153600=CARTESIAN_POINT('Ctrl Pts',(4.94165291247532,4.97832054749623,31.4777015907758));
#153601=CARTESIAN_POINT('Ctrl Pts',(5.09162834723011,4.82482285479086,31.4679364188469));
#153602=CARTESIAN_POINT('Ctrl Pts',(5.2342754070601,4.66476017878153,31.458171246918));
#153603=CARTESIAN_POINT('Ctrl Pts',(5.37672797085845,4.5049157446016,31.4484193895796));
#153604=CARTESIAN_POINT('Ctrl Pts',(5.51187210507935,4.33852424571791,31.4386675322412));
#153605=CARTESIAN_POINT('Ctrl Pts',(5.63917919484042,4.16620745654594,31.4289156749028));
#153606=CARTESIAN_POINT('Ctrl Pts',(5.69469430600281,4.09106485667988,31.4246631588394));
#153607=CARTESIAN_POINT('Ctrl Pts',(5.74871962058488,4.01479596187637,31.4204106427761));
#153608=CARTESIAN_POINT('Ctrl Pts',(5.80121359253963,3.93745443354376,31.4161581267128));
#153609=CARTESIAN_POINT('Ctrl Pts',(5.90037610655681,3.79135422238041,31.4081250103752));
#153610=CARTESIAN_POINT('Ctrl Pts',(5.99411941724529,3.64135298941197,31.4000918940376));
#153611=CARTESIAN_POINT('Ctrl Pts',(6.08212076048457,3.48789816614285,31.3920587777));
#153612=CARTESIAN_POINT('Ctrl Pts',(6.17006761570061,3.33453835790041,31.3840306352482));
#153613=CARTESIAN_POINT('Ctrl Pts',(6.25227939740905,3.17772953174599,31.3760024927963));
#153614=CARTESIAN_POINT('Ctrl Pts',(6.32847653303838,3.01794819923778,31.3679743503445));
#153615=CARTESIAN_POINT('Ctrl Pts',(6.40463678429455,2.85824421129435,31.3599500940361));
#153616=CARTESIAN_POINT('Ctrl Pts',(6.47478803089947,2.69557091309334,31.3519258377278));
#153617=CARTESIAN_POINT('Ctrl Pts',(6.53869663140437,2.53042939537168,31.3439015814194));
#153618=CARTESIAN_POINT('Ctrl Pts',(6.54968554371298,2.50203375468457,31.3425218320865));
#153619=CARTESIAN_POINT('Ctrl Pts',(6.5604899992243,2.47356519257603,31.3411420827536));
#153620=CARTESIAN_POINT('Ctrl Pts',(6.57110895151815,2.44502632087633,31.3397623334207));
#153621=CARTESIAN_POINT('Origin',(0.,0.,50.));
#153622=CARTESIAN_POINT('',(6.57110895151813,2.4450263208764,29.3400595704968));
#153623=CARTESIAN_POINT('',(6.57110895151814,2.44502632087637,29.8870331279755));
#153624=CARTESIAN_POINT('',(6.57110895151814,2.44502632087636,50.));
#153625=CARTESIAN_POINT('',(7.0112494081677,-0.00288079295652949,31.7735343569381));
#153626=CARTESIAN_POINT('Ctrl Pts',(6.57110895151814,2.44502632087637,29.8870331279755));
#153627=CARTESIAN_POINT('Ctrl Pts',(6.51063509439985,2.6075523028872,29.894884053626));
#153628=CARTESIAN_POINT('Ctrl Pts',(6.44409497257938,2.76792041289768,29.9027349792766));
#153629=CARTESIAN_POINT('Ctrl Pts',(6.37167987579692,2.92563191855445,29.9105859049271));
#153630=CARTESIAN_POINT('Ctrl Pts',(6.29927905469288,3.08331233347408,29.9184352828715));
#153631=CARTESIAN_POINT('Ctrl Pts',(6.22100572524205,3.23833684075603,29.9262846608159));
#153632=CARTESIAN_POINT('Ctrl Pts',(6.13709891967929,3.39022763432948,29.9341340387603));
#153633=CARTESIAN_POINT('Ctrl Pts',(6.05316317315262,3.54217081776507,29.941986124096));
#153634=CARTESIAN_POINT('Ctrl Pts',(5.96359025085054,3.69097779240164,29.9498382094318));
#153635=CARTESIAN_POINT('Ctrl Pts',(5.86866479683627,3.83619604098575,29.9576902947676));
#153636=CARTESIAN_POINT('Ctrl Pts',(5.78016253938773,3.97158799624028,29.9650110633129));
#153637=CARTESIAN_POINT('Ctrl Pts',(5.68700818700101,4.10386050920121,29.9723318318582));
#153638=CARTESIAN_POINT('Ctrl Pts',(5.58946555198157,4.23267071784605,29.9796526004035));
#153639=CARTESIAN_POINT('Ctrl Pts',(5.4608173337849,4.40255749427359,29.9893079047635));
#153640=CARTESIAN_POINT('Ctrl Pts',(5.32460260862027,4.56633595418709,29.9989632091234));
#153641=CARTESIAN_POINT('Ctrl Pts',(5.18138853132814,4.72343513239265,30.0086185134833));
#153642=CARTESIAN_POINT('Ctrl Pts',(5.037381074914,4.88140461057452,30.0183273064181));
#153643=CARTESIAN_POINT('Ctrl Pts',(4.88629657359023,5.0326206001273,30.0280360993529));
#153644=CARTESIAN_POINT('Ctrl Pts',(4.72874223923885,5.17654550809112,30.0377448922877));
#153645=CARTESIAN_POINT('Ctrl Pts',(4.5704297400526,5.32116299493275,30.0475004047585));
#153646=CARTESIAN_POINT('Ctrl Pts',(4.40558503937709,5.4584190492802,30.0572559172293));
#153647=CARTESIAN_POINT('Ctrl Pts',(4.23485403431082,5.58781154572892,30.0670114297));
#153648=CARTESIAN_POINT('Ctrl Pts',(4.06395397928303,5.71733216065581,30.076776601629));
#153649=CARTESIAN_POINT('Ctrl Pts',(3.88715599914691,5.83897362939123,30.086541773558));
#153650=CARTESIAN_POINT('Ctrl Pts',(3.70513707577017,5.9522756834889,30.096306945487));
#153651=CARTESIAN_POINT('Ctrl Pts',(3.52336633106581,6.06542325280641,30.1060588028256));
#153652=CARTESIAN_POINT('Ctrl Pts',(3.33638890295605,6.1702541132167,30.1158106601642));
#153653=CARTESIAN_POINT('Ctrl Pts',(3.14490751213805,6.26635326985302,30.1255625175028));
#153654=CARTESIAN_POINT('Ctrl Pts',(3.06140775800607,6.30825946197511,30.1298150335652));
#153655=CARTESIAN_POINT('Ctrl Pts',(2.97705189745367,6.34850579990758,30.1340675496276));
#153656=CARTESIAN_POINT('Ctrl Pts',(2.89189988376014,6.38706048388522,30.13832006569));
#153657=CARTESIAN_POINT('Ctrl Pts',(2.73104687373191,6.45989066956716,30.1463531112888));
#153658=CARTESIAN_POINT('Ctrl Pts',(2.56727285395661,6.52671653460236,30.1543861568876));
#153659=CARTESIAN_POINT('Ctrl Pts',(2.4010736769296,6.58729624052659,30.1624192024864));
#153660=CARTESIAN_POINT('Ctrl Pts',(2.23498133913274,6.64783700348336,30.1704470841342));
#153661=CARTESIAN_POINT('Ctrl Pts',(2.06646729024776,6.70213947481297,30.178474965782));
#153662=CARTESIAN_POINT('Ctrl Pts',(1.8960486441547,6.75000934084532,30.1865028474298));
#153663=CARTESIAN_POINT('Ctrl Pts',(1.72570694376052,6.79785759316122,30.1945271044099));
#153664=CARTESIAN_POINT('Ctrl Pts',(1.5534627105848,6.83927892421778,30.20255136139));
#153665=CARTESIAN_POINT('Ctrl Pts',(1.37984950628901,6.87412844675556,30.21057561837));
#153666=CARTESIAN_POINT('Ctrl Pts',(1.20625729359781,6.90897375563113,30.2185989051357));
#153667=CARTESIAN_POINT('Ctrl Pts',(1.03129679715255,6.93724875903307,30.2266221919014));
#153668=CARTESIAN_POINT('Ctrl Pts',(0.855513271446454,6.95885936090671,
30.2346454786671));
#153669=CARTESIAN_POINT('Ctrl Pts',(0.679744149632396,6.98046819198429,
30.242668107996));
#153670=CARTESIAN_POINT('Ctrl Pts',(0.503152497286794,6.99541366853891,
30.2506907373249));
#153671=CARTESIAN_POINT('Ctrl Pts',(0.326289914370252,7.00365343619173,
30.2587133666538));
#153672=CARTESIAN_POINT('Ctrl Pts',(0.1493608437137,7.01189630141059,30.2667390119202));
#153673=CARTESIAN_POINT('Ctrl Pts',(-0.0278389944188127,7.01342840779966,
30.2747646571866));
#153674=CARTESIAN_POINT('Ctrl Pts',(-0.204756378974013,7.00825951201648,
30.282790302453));
#153675=CARTESIAN_POINT('Ctrl Pts',(-0.309077649721913,7.00521161608573,
30.2875227119608));
#153676=CARTESIAN_POINT('Ctrl Pts',(-0.413300719792258,6.99983476989188,
30.2922551214686));
#153677=CARTESIAN_POINT('Ctrl Pts',(-0.517312787694124,6.99213944670643,
30.2969875309764));
#153678=CARTESIAN_POINT('Ctrl Pts',(-0.709187652006507,6.97794360268724,
30.305717579811));
#153679=CARTESIAN_POINT('Ctrl Pts',(-0.900440130699299,6.95584821871191,
30.3144476286457));
#153680=CARTESIAN_POINT('Ctrl Pts',(-1.09042849719771,6.92593620061571,
30.3231776774803));
#153681=CARTESIAN_POINT('Ctrl Pts',(-1.28047179906911,6.8960155334222,30.3319102506195));
#153682=CARTESIAN_POINT('Ctrl Pts',(-1.46924998854034,6.85827376325242,
30.3406428237586));
#153683=CARTESIAN_POINT('Ctrl Pts',(-1.65613021921757,6.81284516626456,
30.3493753968978));
#153684=CARTESIAN_POINT('Ctrl Pts',(-1.84566538188862,6.76677118353879,
30.3582320301782));
#153685=CARTESIAN_POINT('Ctrl Pts',(-2.03324796605332,6.7127903705848,30.3670886634586));
#153686=CARTESIAN_POINT('Ctrl Pts',(-2.21823189569185,6.65109568563221,
30.3759452967391));
#153687=CARTESIAN_POINT('Ctrl Pts',(-2.40074075245821,6.59022647152664,
30.3846834288458));
#153688=CARTESIAN_POINT('Ctrl Pts',(-2.5807198063312,6.52184863553396,30.3934215609525));
#153689=CARTESIAN_POINT('Ctrl Pts',(-2.75756609906262,6.44619700069743,
30.4021596930593));
#153690=CARTESIAN_POINT('Ctrl Pts',(-2.9380098127859,6.36900645444226,30.4110755769265));
#153691=CARTESIAN_POINT('Ctrl Pts',(-3.11519167258611,6.28424312418134,
30.4199914607938));
#153692=CARTESIAN_POINT('Ctrl Pts',(-3.28849396900906,6.19220752060935,
30.428907344661));
#153693=CARTESIAN_POINT('Ctrl Pts',(-3.46179626543201,6.10017191703736,
30.4378232285283));
#153694=CARTESIAN_POINT('Ctrl Pts',(-3.6312187342459,6.00086418736742,30.4467391123955));
#153695=CARTESIAN_POINT('Ctrl Pts',(-3.79617071624401,5.89463437845227,
30.4556549962628));
#153696=CARTESIAN_POINT('Ctrl Pts',(-3.95788135011287,5.79049201212634,
30.464395680759));
#153697=CARTESIAN_POINT('Ctrl Pts',(-4.11531273400632,5.6796860216251,30.4731363652552));
#153698=CARTESIAN_POINT('Ctrl Pts',(-4.2679340745091,5.56258620590676,30.4818770497515));
#153699=CARTESIAN_POINT('Ctrl Pts',(-4.4205279558975,5.44550745839044,30.4906161616534));
#153700=CARTESIAN_POINT('Ctrl Pts',(-4.56831330503308,5.32213731368012,
30.4993552735553));
#153701=CARTESIAN_POINT('Ctrl Pts',(-4.71079085000666,5.19288707079151,
30.5080943854572));
#153702=CARTESIAN_POINT('Ctrl Pts',(-4.85511439663588,5.06196220498313,
30.5169467251315));
#153703=CARTESIAN_POINT('Ctrl Pts',(-4.99399141362478,4.92500398340368,
30.5257990648058));
#153704=CARTESIAN_POINT('Ctrl Pts',(-5.12693901451052,4.78248083153397,
30.5346514044802));
#153705=CARTESIAN_POINT('Ctrl Pts',(-5.25811884923516,4.64185276918352,
30.5433860371299));
#153706=CARTESIAN_POINT('Ctrl Pts',(-5.38352579062743,4.49580706298467,
30.5521206697797));
#153707=CARTESIAN_POINT('Ctrl Pts',(-5.50273361492177,4.34483018375978,
30.5608553024295));
#153708=CARTESIAN_POINT('Ctrl Pts',(-5.6243510880585,4.19080148084457,30.5697664956161));
#153709=CARTESIAN_POINT('Ctrl Pts',(-5.73951596194569,4.03164034017232,
30.5786776888027));
#153710=CARTESIAN_POINT('Ctrl Pts',(-5.84781877346367,3.86789893291253,
30.5875888819893));
#153711=CARTESIAN_POINT('Ctrl Pts',(-5.95612158498165,3.70415752565273,
30.596500075176));
#153712=CARTESIAN_POINT('Ctrl Pts',(-6.05756215566455,3.53583609720128,
30.6054112683626));
#153713=CARTESIAN_POINT('Ctrl Pts',(-6.15177738397854,3.3635192255241,30.6143224615492));
#153714=CARTESIAN_POINT('Ctrl Pts',(-6.23663020117184,3.20832592744051,
30.6223481264016));
#153715=CARTESIAN_POINT('Ctrl Pts',(-6.315660867571,3.04982023554652,30.630373791254));
#153716=CARTESIAN_POINT('Ctrl Pts',(-6.38860452752384,2.88848727769431,
30.6383994561063));
#153717=CARTESIAN_POINT('Ctrl Pts',(-6.4615250369482,2.72720552296571,30.6464225738096));
#153718=CARTESIAN_POINT('Ctrl Pts',(-6.52836223525133,2.56309862234801,
30.6544456915128));
#153719=CARTESIAN_POINT('Ctrl Pts',(-6.5888979667776,2.39667481020977,30.662468809216));
#153720=CARTESIAN_POINT('Ctrl Pts',(-6.6494260642183,2.23027198557082,30.6704909151338));
#153721=CARTESIAN_POINT('Ctrl Pts',(-6.70365415305941,2.06155317599891,
30.6785130210517));
#153722=CARTESIAN_POINT('Ctrl Pts',(-6.75141284886433,1.89104497743699,
30.6865351269695));
#153723=CARTESIAN_POINT('Ctrl Pts',(-6.79918929196198,1.72047341745238,
30.6945602139291));
#153724=CARTESIAN_POINT('Ctrl Pts',(-6.84049143764329,1.54811149263829,
30.7025853008886));
#153725=CARTESIAN_POINT('Ctrl Pts',(-6.87520014708154,1.37449972719894,
30.7106103878481));
#153726=CARTESIAN_POINT('Ctrl Pts',(-6.90991569222643,1.2008537697912,30.7186370553083));
#153727=CARTESIAN_POINT('Ctrl Pts',(-6.93803515099065,1.02595784256382,
30.7266637227685));
#153728=CARTESIAN_POINT('Ctrl Pts',(-6.95949086975134,0.850360744829992,
30.7346903902288));
#153729=CARTESIAN_POINT('Ctrl Pts',(-6.98096381308744,0.674622678364829,
30.7427235014694));
#153730=CARTESIAN_POINT('Ctrl Pts',(-6.99576229664982,0.498182682066907,
30.7507566127099));
#153731=CARTESIAN_POINT('Ctrl Pts',(-7.00387066355227,0.321593362387762,
30.7587897239505));
#153732=CARTESIAN_POINT('Ctrl Pts',(-7.00864840788377,0.217540520274141,
30.7635231249122));
#153733=CARTESIAN_POINT('Ctrl Pts',(-7.01110433567621,0.113435852690615,
30.768256525874));
#153734=CARTESIAN_POINT('Ctrl Pts',(-7.01124370937302,0.00939203265171227,
30.7729899268357));
#153735=CARTESIAN_POINT('Ctrl Pts',(-7.01153082352604,-0.204941474683194,
30.7827408801298));
#153736=CARTESIAN_POINT('Ctrl Pts',(-7.00198517742529,-0.419142924389543,
30.792491833424));
#153737=CARTESIAN_POINT('Ctrl Pts',(-6.98267138124105,-0.632397773633994,
30.8022427867182));
#153738=CARTESIAN_POINT('Ctrl Pts',(-6.96332975991021,-0.84595985649458,
30.8120077880898));
#153739=CARTESIAN_POINT('Ctrl Pts',(-6.93419184213379,-1.05857257250479,
30.8217727894614));
#153740=CARTESIAN_POINT('Ctrl Pts',(-6.89537417949784,-1.26942565249582,
30.8315377908331));
#153741=CARTESIAN_POINT('Ctrl Pts',(-6.85662121786268,-1.47992728409023,
30.8412865159707));
#153742=CARTESIAN_POINT('Ctrl Pts',(-6.80822076380325,-1.68867510415602,
30.8510352411083));
#153743=CARTESIAN_POINT('Ctrl Pts',(-6.75033997080507,-1.89487119378904,
30.8607839662459));
#153744=CARTESIAN_POINT('Ctrl Pts',(-6.69261803814045,-2.10050135510829,
30.870505934913));
#153745=CARTESIAN_POINT('Ctrl Pts',(-6.62546772171576,-2.30359372891132,
30.8802279035802));
#153746=CARTESIAN_POINT('Ctrl Pts',(-6.54910575246193,-2.50336581537138,
30.8899498722473));
#153747=CARTESIAN_POINT('Ctrl Pts',(-6.47324905041402,-2.70181606211292,
30.8996075131871));
#153748=CARTESIAN_POINT('Ctrl Pts',(-6.38830218450866,-2.89698976132389,
30.9092651541268));
#153749=CARTESIAN_POINT('Ctrl Pts',(-6.29452808559151,-3.08812932731123,
30.9189227950665));
#153750=CARTESIAN_POINT('Ctrl Pts',(-6.25331114067329,-3.17214174709414,
30.9231676607517));
#153751=CARTESIAN_POINT('Ctrl Pts',(-6.21038951751227,-3.25537493916658,
30.9274125264369));
#153752=CARTESIAN_POINT('Ctrl Pts',(-6.16578867531316,-3.33776520652366,
30.9316573921221));
#153753=CARTESIAN_POINT('Ctrl Pts',(-6.08328924762561,-3.49016479291804,
30.939509239136));
#153754=CARTESIAN_POINT('Ctrl Pts',(-5.99507492550315,-3.63961591340342,
30.9473610861499));
#153755=CARTESIAN_POINT('Ctrl Pts',(-5.90139775178298,-3.78564804726361,
30.9552129331638));
#153756=CARTESIAN_POINT('Ctrl Pts',(-5.8077471441519,-3.93163876759131,
30.9630625534573));
#153757=CARTESIAN_POINT('Ctrl Pts',(-5.70863697235183,-4.07421210922496,
30.9709121737509));
#153758=CARTESIAN_POINT('Ctrl Pts',(-5.6043641378185,-4.21292406449889,
30.9787617940445));
#153759=CARTESIAN_POINT('Ctrl Pts',(-5.50009962813733,-4.35162494539737,
30.9866107876462));
#153760=CARTESIAN_POINT('Ctrl Pts',(-5.39067350605877,-4.48646474917287,
30.994459781248));
#153761=CARTESIAN_POINT('Ctrl Pts',(-5.27642455801112,-4.61703047922765,
31.0023087748498));
#153762=CARTESIAN_POINT('Ctrl Pts',(-5.16211776906659,-4.74766231088826,
31.0101617421672));
#153763=CARTESIAN_POINT('Ctrl Pts',(-5.04298352713106,-4.87401545791966,
31.0180147094846));
#153764=CARTESIAN_POINT('Ctrl Pts',(-4.91939950847132,-4.99571166487339,
31.0258676768021));
#153765=CARTESIAN_POINT('Ctrl Pts',(-4.79578410362338,-5.11743877857459,
31.0337226385093));
#153766=CARTESIAN_POINT('Ctrl Pts',(-4.66771695222961,-5.23450633856665,
31.0415776002165));
#153767=CARTESIAN_POINT('Ctrl Pts',(-4.5356102836231,-5.3465751577615,31.0494325619238));
#153768=CARTESIAN_POINT('Ctrl Pts',(-4.40337248810524,-5.45875521462721,
31.0572953203371));
#153769=CARTESIAN_POINT('Ctrl Pts',(-4.26708746699066,-5.56592638528403,
31.0651580787504));
#153770=CARTESIAN_POINT('Ctrl Pts',(-4.12719846489199,-5.66779140352688,
31.0730208371638));
#153771=CARTESIAN_POINT('Ctrl Pts',(-4.02457790023861,-5.74251811923491,
31.078788843912));
#153772=CARTESIAN_POINT('Ctrl Pts',(-3.92001850282062,-5.81439022392568,
31.0845568506602));
#153773=CARTESIAN_POINT('Ctrl Pts',(-3.81370389557021,-5.88330597193556,
31.0903248574085));
#153774=CARTESIAN_POINT('Ctrl Pts',(-3.65928125321288,-5.98340653368293,
31.0987029238495));
#153775=CARTESIAN_POINT('Ctrl Pts',(-3.50081262185188,-6.07749008693342,
31.1070809902906));
#153776=CARTESIAN_POINT('Ctrl Pts',(-3.33879497014469,-6.16523111568711,
31.1154590567316));
#153777=CARTESIAN_POINT('Ctrl Pts',(-3.17688810418275,-6.25291214816782,
31.1238313943504));
#153778=CARTESIAN_POINT('Ctrl Pts',(-3.01143734428889,-6.33425914669135,
31.1322037319691));
#153779=CARTESIAN_POINT('Ctrl Pts',(-2.84296662347145,-6.40899113280143,
31.1405760695879));
#153780=CARTESIAN_POINT('Ctrl Pts',(-2.67458639458861,-6.48368297756252,
31.1489439101105));
#153781=CARTESIAN_POINT('Ctrl Pts',(-2.50318973897938,-6.55176676160134,
31.1573117506331));
#153782=CARTESIAN_POINT('Ctrl Pts',(-2.32932346968383,-6.61300829699163,
31.1656795911557));
#153783=CARTESIAN_POINT('Ctrl Pts',(-2.15552512032786,-6.67422590869965,
31.1740441628256));
#153784=CARTESIAN_POINT('Ctrl Pts',(-1.97925939070246,-6.72860649283356,
31.1824087344955));
#153785=CARTESIAN_POINT('Ctrl Pts',(-1.80109170178626,-6.77596452501463,
31.1907733061655));
#153786=CARTESIAN_POINT('Ctrl Pts',(-1.6229675336869,-6.82331098910354,
31.1991358346311));
#153787=CARTESIAN_POINT('Ctrl Pts',(-1.44294265028617,-6.86363823819933,
31.2074983630967));
#153788=CARTESIAN_POINT('Ctrl Pts',(-1.26159665606641,-6.8968108890923,
31.2158608915623));
#153789=CARTESIAN_POINT('Ctrl Pts',(-1.08023618986904,-6.92998618726657,
31.2242240873838));
#153790=CARTESIAN_POINT('Ctrl Pts',(-0.897554724438878,-6.9560056814588,
31.2325872832053));
#153791=CARTESIAN_POINT('Ctrl Pts',(-0.714141822607698,-6.97478515939398,
31.2409504790269));
#153792=CARTESIAN_POINT('Ctrl Pts',(-0.530716412384352,-6.99356591805191,
31.2493142452016));
#153793=CARTESIAN_POINT('Ctrl Pts',(-0.346559793382873,-7.00510564218847,
31.2576780113763));
#153794=CARTESIAN_POINT('Ctrl Pts',(-0.162266591852918,-7.00937202006488,
31.266041777551));
#153795=CARTESIAN_POINT('Ctrl Pts',(0.0220637487227761,-7.01363925770824,
31.2744072292046));
#153796=CARTESIAN_POINT('Ctrl Pts',(0.20653039801308,-7.01063021878234,
31.2827726808582));
#153797=CARTESIAN_POINT('Ctrl Pts',(0.390538351795674,-7.00036473037489,
31.2911381325117));
#153798=CARTESIAN_POINT('Ctrl Pts',(0.574607929480229,-6.99009580407556,
31.2995063857386));
#153799=CARTESIAN_POINT('Ctrl Pts',(0.758218177199506,-6.97256560077253,
31.3078746389655));
#153800=CARTESIAN_POINT('Ctrl Pts',(0.940778399872127,-6.94784589386049,
31.3162428921924));
#153801=CARTESIAN_POINT('Ctrl Pts',(1.12350788191618,-6.9231032682535,31.3246189039839));
#153802=CARTESIAN_POINT('Ctrl Pts',(1.30518506737711,-6.8911578631517,31.3329949157754));
#153803=CARTESIAN_POINT('Ctrl Pts',(1.48522742137247,-6.85213295764927,
31.3413709275669));
#153804=CARTESIAN_POINT('Ctrl Pts',(1.66535807036304,-6.81308891385094,
31.349751047058));
#153805=CARTESIAN_POINT('Ctrl Pts',(1.84385196932977,-6.76695852205919,
31.3581311665492));
#153806=CARTESIAN_POINT('Ctrl Pts',(2.02014032894375,-6.71391537136678,
31.3665112860404));
#153807=CARTESIAN_POINT('Ctrl Pts',(2.19663012033953,-6.66081161215557,
31.3749009808796));
#153808=CARTESIAN_POINT('Ctrl Pts',(2.37090902367499,-6.60077941179378,
31.3832906757188));
#153809=CARTESIAN_POINT('Ctrl Pts',(2.5424255937145,-6.53404152595662,31.3916803705581));
#153810=CARTESIAN_POINT('Ctrl Pts',(2.65131850421169,-6.49167079391852,
31.3970068430325));
#153811=CARTESIAN_POINT('Ctrl Pts',(2.75909838701318,-6.44659813077163,
31.402333315507));
#153812=CARTESIAN_POINT('Ctrl Pts',(2.86562898909525,-6.39889029905631,
31.4076597879814));
#153813=CARTESIAN_POINT('Ctrl Pts',(3.033256810818,-6.32382116630708,31.4160410883863));
#153814=CARTESIAN_POINT('Ctrl Pts',(3.19812844818045,-6.24207373702027,
31.4244223887911));
#153815=CARTESIAN_POINT('Ctrl Pts',(3.35969339087501,-6.15386763603271,
31.4328036891959));
#153816=CARTESIAN_POINT('Ctrl Pts',(3.52105357365609,-6.06577332336571,
31.4411743675294));
#153817=CARTESIAN_POINT('Ctrl Pts',(3.67911512824899,-5.97123680742495,
31.4495450458629));
#153818=CARTESIAN_POINT('Ctrl Pts',(3.83334806603012,-5.87052545920407,
31.4579157241964));
#153819=CARTESIAN_POINT('Ctrl Pts',(3.98740597590764,-5.76992840107195,
31.4662769032472));
#153820=CARTESIAN_POINT('Ctrl Pts',(4.13764365600859,-5.66317065517934,
31.474638082298));
#153821=CARTESIAN_POINT('Ctrl Pts',(4.28355587357753,-5.55056534421851,
31.4829992613488));
#153822=CARTESIAN_POINT('Ctrl Pts',(4.42927875283216,-5.43810615193172,
31.4913495907835));
#153823=CARTESIAN_POINT('Ctrl Pts',(4.57068710670983,-5.31981472869339,
31.4996999202181));
#153824=CARTESIAN_POINT('Ctrl Pts',(4.70730491029333,-5.19604725190488,
31.5080502496528));
#153825=CARTESIAN_POINT('Ctrl Pts',(4.84381759464959,-5.07237500678587,
31.5163941540085));
#153826=CARTESIAN_POINT('Ctrl Pts',(4.97554683253056,-4.94323532389461,
31.5247380583642));
#153827=CARTESIAN_POINT('Ctrl Pts',(5.10204901722773,-4.80902509749175,
31.5330819627199));
#153828=CARTESIAN_POINT('Ctrl Pts',(5.22844959458117,-4.6749226695798,31.5414191651996));
#153829=CARTESIAN_POINT('Ctrl Pts',(5.34963126777935,-4.53575805829959,
31.5497563676793));
#153830=CARTESIAN_POINT('Ctrl Pts',(5.46518660244469,-4.39196561495637,
31.558093570159));
#153831=CARTESIAN_POINT('Ctrl Pts',(5.50322678076923,-4.34462993631947,
31.5608381311952));
#153832=CARTESIAN_POINT('Ctrl Pts',(5.5406575368276,-4.29679303929625,31.5635826922315));
#153833=CARTESIAN_POINT('Ctrl Pts',(5.57746523610436,-4.24847126653192,
31.5663272532677));
#153834=CARTESIAN_POINT('Ctrl Pts',(5.68929150413603,-4.10166384256667,
31.5746655635697));
#153835=CARTESIAN_POINT('Ctrl Pts',(5.79527206873142,-3.9504989767829,31.5830038738716));
#153836=CARTESIAN_POINT('Ctrl Pts',(5.89508152077292,-3.79547631081286,
31.5913421841736));
#153837=CARTESIAN_POINT('Ctrl Pts',(5.9949537695349,-3.64035610984164,31.5996857406574));
#153838=CARTESIAN_POINT('Ctrl Pts',(6.08864698393497,-3.48137354282746,
31.6080292971413));
#153839=CARTESIAN_POINT('Ctrl Pts',(6.17588089420329,-3.31905434470645,
31.6163728536251));
#153840=CARTESIAN_POINT('Ctrl Pts',(6.26318117165118,-3.15661165484542,
31.6247227578504));
#153841=CARTESIAN_POINT('Ctrl Pts',(6.34401218779013,-2.99082755869547,
31.6330726620758));
#153842=CARTESIAN_POINT('Ctrl Pts',(6.41814093986457,-2.82224971229236,
31.6414225663011));
#153843=CARTESIAN_POINT('Ctrl Pts',(6.49238087958084,-2.65341901159613,
31.6497849947648));
#153844=CARTESIAN_POINT('Ctrl Pts',(6.5598983343723,-2.48178648706626,31.6581474232285));
#153845=CARTESIAN_POINT('Ctrl Pts',(6.62050898463268,-2.30791840126508,
31.6665098516922));
#153846=CARTESIAN_POINT('Ctrl Pts',(6.68117146526149,-2.13390163454882,
31.6748794311722));
#153847=CARTESIAN_POINT('Ctrl Pts',(6.73491526150781,-1.95764580486575,
31.6832490106522));
#153848=CARTESIAN_POINT('Ctrl Pts',(6.78160657312031,-1.77972999354158,
31.6916185901322));
#153849=CARTESIAN_POINT('Ctrl Pts',(6.82836990039218,-1.60153976875538,
31.7000010786688));
#153850=CARTESIAN_POINT('Ctrl Pts',(6.86805893587711,-1.42168476537843,
31.7083835672054));
#153851=CARTESIAN_POINT('Ctrl Pts',(6.9005911291171,-1.24075325155743,31.716766055742));
#153852=CARTESIAN_POINT('Ctrl Pts',(6.91123619581566,-1.18154949550305,
31.7195089433461));
#153853=CARTESIAN_POINT('Ctrl Pts',(6.92111539004135,-1.12223050757922,
31.7222518309502));
#153854=CARTESIAN_POINT('Ctrl Pts',(6.93022702928683,-1.0628169574495,31.7249947185543));
#153855=CARTESIAN_POINT('Ctrl Pts',(6.97711648276298,-0.757068582255461,
31.7391099065285));
#153856=CARTESIAN_POINT('Ctrl Pts',(7.00374762286509,-0.448352345442656,
31.7532250945026));
#153857=CARTESIAN_POINT('Ctrl Pts',(7.00987641222234,-0.138777692259644,
31.7673402824768));
#153858=CARTESIAN_POINT('Ctrl Pts',(7.010772897567,-0.0934948274911753,
31.7694049739547));
#153859=CARTESIAN_POINT('Ctrl Pts',(7.01123078995131,-0.048193640247624,
31.7714696654327));
#153860=CARTESIAN_POINT('Ctrl Pts',(7.01124940816745,-0.00288079356036475,
31.7735343569106));
#153861=CARTESIAN_POINT('Ctrl Pts',(7.0112494081677,-0.00288079295658086,
31.7735343569381));
#153862=CARTESIAN_POINT('Ctrl Pts',(7.01132401614023,0.178699456341272,
31.7818081075562));
#153863=CARTESIAN_POINT('Ctrl Pts',(7.00434040300367,0.360449743185088,
31.7900818581744));
#153864=CARTESIAN_POINT('Ctrl Pts',(6.99028539102326,0.541790286500964,
31.7983556087925));
#153865=CARTESIAN_POINT('Ctrl Pts',(6.97624480014575,0.722944765896102,
31.8066208701536));
#153866=CARTESIAN_POINT('Ctrl Pts',(6.95514730409161,0.903690000783933,
31.8148861315147));
#153867=CARTESIAN_POINT('Ctrl Pts',(6.92703176507304,1.08344703985431,31.8231513928758));
#153868=CARTESIAN_POINT('Ctrl Pts',(6.89893310426121,1.26309616790559,31.8314116924687));
#153869=CARTESIAN_POINT('Ctrl Pts',(6.86382484659498,1.44175794545868,31.8396719920615));
#153870=CARTESIAN_POINT('Ctrl Pts',(6.82179765978736,1.61885862613749,31.8479322916543));
#153871=CARTESIAN_POINT('Ctrl Pts',(6.77979130111409,1.79587153799204,31.8561884975487));
#153872=CARTESIAN_POINT('Ctrl Pts',(6.73087292716555,1.97132456327243,31.864444703443));
#153873=CARTESIAN_POINT('Ctrl Pts',(6.67518430983552,2.14465404954405,31.8727009093374));
#153874=CARTESIAN_POINT('Ctrl Pts',(6.64277296198895,2.24553359263494,31.8775061060538));
#153875=CARTESIAN_POINT('Ctrl Pts',(6.60806924282777,2.345694015534,31.8823113027702));
#153876=CARTESIAN_POINT('Ctrl Pts',(6.57110895151814,2.44502632087638,31.8871164994866));
#153877=CARTESIAN_POINT('',(7.01124987764386,-0.00130986217405227,31.2264656430654));
#153878=CARTESIAN_POINT('Ctrl Pts',(6.57110895151815,2.44502632087633,31.3397623334207));
#153879=CARTESIAN_POINT('Ctrl Pts',(6.63285687696087,2.27907622776285,31.3317392576425));
#153880=CARTESIAN_POINT('Ctrl Pts',(6.68832843807726,2.11074736469941,31.3237161818643));
#153881=CARTESIAN_POINT('Ctrl Pts',(6.73734652205013,1.94056393976572,31.3156931060861));
#153882=CARTESIAN_POINT('Ctrl Pts',(6.78636203415064,1.77038944398654,31.3076704512613));
#153883=CARTESIAN_POINT('Ctrl Pts',(6.82892464653872,1.59836093374321,31.2996477964365));
#153884=CARTESIAN_POINT('Ctrl Pts',(6.86490740091012,1.42501682075319,31.2916251416116));
#153885=CARTESIAN_POINT('Ctrl Pts',(6.90090345642949,1.25160863052012,31.2835995211851));
#153886=CARTESIAN_POINT('Ctrl Pts',(6.93031472605805,1.07688422620562,31.2755739007585));
#153887=CARTESIAN_POINT('Ctrl Pts',(6.95306549893561,0.901391551996848,
31.2675482803319));
#153888=CARTESIAN_POINT('Ctrl Pts',(6.96256917139311,0.828083058111971,
31.2641957406968));
#153889=CARTESIAN_POINT('Ctrl Pts',(6.97091122194759,0.754640578532504,
31.2608432010616));
#153890=CARTESIAN_POINT('Ctrl Pts',(6.97808881553906,0.681104283460815,
31.2574906614265));
#153891=CARTESIAN_POINT('Ctrl Pts',(6.99876795302476,0.46924119361102,31.2478317657035));
#153892=CARTESIAN_POINT('Ctrl Pts',(7.00978401741194,0.256539866432542,
31.2381728699806));
#153893=CARTESIAN_POINT('Ctrl Pts',(7.0111131591244,0.0438044798241868,
31.2285139742577));
#153894=CARTESIAN_POINT('Ctrl Pts',(7.01120711473708,0.0287664418181586,
31.2278311972017));
#153895=CARTESIAN_POINT('Ctrl Pts',(7.01125268710363,0.0137282333579481,
31.2271484201457));
#153896=CARTESIAN_POINT('Ctrl Pts',(7.01124987764396,-0.00130986163894219,
31.2264656430897));
#153897=CARTESIAN_POINT('Ctrl Pts',(7.01124987764386,-0.00130986217404309,
31.2264656430654));
#153898=CARTESIAN_POINT('Ctrl Pts',(7.01121431189105,-0.19168132644035,
31.2178221767256));
#153899=CARTESIAN_POINT('Ctrl Pts',(7.00342087638219,-0.382039512845058,
31.2091787103858));
#153900=CARTESIAN_POINT('Ctrl Pts',(6.98789859162277,-0.571751550672562,
31.200535244046));
#153901=CARTESIAN_POINT('Ctrl Pts',(6.97237161482203,-0.76152093422815,
31.1918891649787));
#153902=CARTESIAN_POINT('Ctrl Pts',(6.94911114148364,-0.950643490621212,
31.1832430859113));
#153903=CARTESIAN_POINT('Ctrl Pts',(6.91819815905292,-1.13849057728942,
31.174597006844));
#153904=CARTESIAN_POINT('Ctrl Pts',(6.88728354559609,-1.32634757511729,
31.1659504715935));
#153905=CARTESIAN_POINT('Ctrl Pts',(6.84871566768912,-1.51292868433962,
31.157303936343));
#153906=CARTESIAN_POINT('Ctrl Pts',(6.80262687431758,-1.69761425869135,
31.1486574010926));
#153907=CARTESIAN_POINT('Ctrl Pts',(6.75652405074711,-1.88235605441837,
31.1400082336923));
#153908=CARTESIAN_POINT('Ctrl Pts',(6.70289580584609,-2.06520088150153,
31.131359066292));
#153909=CARTESIAN_POINT('Ctrl Pts',(6.64192504571639,-2.24554186101825,
31.1227098988917));
#153910=CARTESIAN_POINT('Ctrl Pts',(6.58579669808265,-2.41155982060071,
31.1147476646412));
#153911=CARTESIAN_POINT('Ctrl Pts',(6.52344643640313,-2.57545584263654,
31.1067854303906));
#153912=CARTESIAN_POINT('Ctrl Pts',(6.45505378653801,-2.73676947794317,
31.0988231961401));
#153913=CARTESIAN_POINT('Ctrl Pts',(6.37997453672923,-2.91385439491354,
31.0900825116438));
#153914=CARTESIAN_POINT('Ctrl Pts',(6.29760020324757,-3.08785749071656,
31.0813418271476));
#153915=CARTESIAN_POINT('Ctrl Pts',(6.20820478069621,-3.25819274498006,
31.0726011426514));
#153916=CARTESIAN_POINT('Ctrl Pts',(6.11882544186649,-3.42849735310156,
31.0638620307495));
#153917=CARTESIAN_POINT('Ctrl Pts',(6.02242766388431,-3.5951351952172,31.0551229188476));
#153918=CARTESIAN_POINT('Ctrl Pts',(5.91933170364109,-3.75754424388715,
31.0463838069457));
#153919=CARTESIAN_POINT('Ctrl Pts',(5.81489998685208,-3.92205753552982,
31.0375314672714));
#153920=CARTESIAN_POINT('Ctrl Pts',(5.70359544243871,-4.08223143695854,
31.028679127597));
#153921=CARTESIAN_POINT('Ctrl Pts',(5.58579740980158,-4.2375103373507,31.0198267879227));
#153922=CARTESIAN_POINT('Ctrl Pts',(5.46956570385669,-4.39072453868989,
31.0110921552729));
#153923=CARTESIAN_POINT('Ctrl Pts',(5.34701230226747,-4.53917289000252,
31.0023575226231));
#153924=CARTESIAN_POINT('Ctrl Pts',(5.21854397658004,-4.68235254193875,
30.9936228899733));
#153925=CARTESIAN_POINT('Ctrl Pts',(5.08747881168255,-4.8284264055979,30.9847116967867));
#153926=CARTESIAN_POINT('Ctrl Pts',(4.95025722691191,-4.96901606933813,
30.9758005036001));
#153927=CARTESIAN_POINT('Ctrl Pts',(4.80735358884143,-5.10362400989272,
30.9668893104135));
#153928=CARTESIAN_POINT('Ctrl Pts',(4.66444995077095,-5.23823195044731,
30.9579781172268));
#153929=CARTESIAN_POINT('Ctrl Pts',(4.51586447081601,-5.36685795016344,
30.9490669240402));
#153930=CARTESIAN_POINT('Ctrl Pts',(4.36211134490397,-5.48904465068013,
30.9401557308536));
#153931=CARTESIAN_POINT('Ctrl Pts',(4.22363706511502,-5.59908934247726,
30.9321300660012));
#153932=CARTESIAN_POINT('Ctrl Pts',(4.08090719246041,-5.703961092946,30.9241044011488));
#153933=CARTESIAN_POINT('Ctrl Pts',(3.93435465838164,-5.80331629196365,
30.9160787362964));
#153934=CARTESIAN_POINT('Ctrl Pts',(3.78784863648236,-5.90263995807824,
30.9080556185932));
#153935=CARTESIAN_POINT('Ctrl Pts',(3.63752267161901,-5.99645035300017,
30.90003250089));
#153936=CARTESIAN_POINT('Ctrl Pts',(3.48384041782166,-6.08444594894656,
30.8920093831867));
#153937=CARTESIAN_POINT('Ctrl Pts',(3.33017754470146,-6.17243044787821,
30.8839872772689));
#153938=CARTESIAN_POINT('Ctrl Pts',(3.17315954404523,-6.25460142689658,
30.875965171351));
#153939=CARTESIAN_POINT('Ctrl Pts',(3.01327646961216,-6.33070228965015,
30.8679430654331));
#153940=CARTESIAN_POINT('Ctrl Pts',(2.85333398208868,-6.40683143174133,
30.8599179784736));
#153941=CARTESIAN_POINT('Ctrl Pts',(2.6905246239216,-6.47688579104044,30.8518928915141));
#153942=CARTESIAN_POINT('Ctrl Pts',(2.52536073116679,-6.54065591053227,
30.8438678045545));
#153943=CARTESIAN_POINT('Ctrl Pts',(2.36016431020983,-6.60443858923002,
30.8358411370943));
#153944=CARTESIAN_POINT('Ctrl Pts',(2.19261277600286,-6.66193443870541,
30.827814469634));
#153945=CARTESIAN_POINT('Ctrl Pts',(2.02323538745976,-6.7129833255737,30.8197878021738));
#153946=CARTESIAN_POINT('Ctrl Pts',(1.85372202334592,-6.76407319430851,
30.8117546909332));
#153947=CARTESIAN_POINT('Ctrl Pts',(1.68238023093686,-6.80870566660739,
30.8037215796926));
#153948=CARTESIAN_POINT('Ctrl Pts',(1.50975187643278,-6.84677119773311,
30.795688468452));
#153949=CARTESIAN_POINT('Ctrl Pts',(1.40803297889223,-6.86920079147817,
30.7909550674904));
#153950=CARTESIAN_POINT('Ctrl Pts',(1.30586757525944,-6.88935131738097,
30.7862216665288));
#153951=CARTESIAN_POINT('Ctrl Pts',(1.20336758864659,-6.90720877121105,
30.7814882655671));
#153952=CARTESIAN_POINT('Ctrl Pts',(0.992214426213876,-6.94399568186168,
30.771737312273));
#153953=CARTESIAN_POINT('Ctrl Pts',(0.779516735558681,-6.97107099913154,
30.7619863589789));
#153954=CARTESIAN_POINT('Ctrl Pts',(0.566088162933685,-6.98835966119993,
30.7522354056848));
#153955=CARTESIAN_POINT('Ctrl Pts',(0.352352106411399,-7.00567323082932,
30.7424704043132));
#153956=CARTESIAN_POINT('Ctrl Pts',(0.137883100171667,-7.0131719389632,
30.7327054029416));
#153957=CARTESIAN_POINT('Ctrl Pts',(-0.0765005744095588,-7.0108326341894,
30.72294040157));
#153958=CARTESIAN_POINT('Ctrl Pts',(-0.290526915824577,-7.00849722855196,
30.7131916764325));
#153959=CARTESIAN_POINT('Ctrl Pts',(-0.504468171934545,-6.9963565832212,
30.7034429512949));
#153960=CARTESIAN_POINT('Ctrl Pts',(-0.717509612978354,-6.97443951280558,
30.6936942261573));
#153961=CARTESIAN_POINT('Ctrl Pts',(-0.92996633787348,-6.95258259624988,
30.6839722574902));
#153962=CARTESIAN_POINT('Ctrl Pts',(-1.14152813821791,-6.92100282538834,
30.6742502888231));
#153963=CARTESIAN_POINT('Ctrl Pts',(-1.35138703432115,-6.87978049402513,
30.6645283201559));
#153964=CARTESIAN_POINT('Ctrl Pts',(-1.55985734892056,-6.83883092006196,
30.6548706792163));
#153965=CARTESIAN_POINT('Ctrl Pts',(-1.76664716877632,-6.7883659490976,
30.6452130382766));
#153966=CARTESIAN_POINT('Ctrl Pts',(-1.97096519584124,-6.72851564308819,
30.6355553973369));
#153967=CARTESIAN_POINT('Ctrl Pts',(-2.06077000297908,-6.70220937307606,
30.6313105316515));
#153968=CARTESIAN_POINT('Ctrl Pts',(-2.15009729756754,-6.6740906170634,
30.6270656659661));
#153969=CARTESIAN_POINT('Ctrl Pts',(-2.23887997716637,-6.64417361380206,
30.6228208002807));
#153970=CARTESIAN_POINT('Ctrl Pts',(-2.4031037876147,-6.5888352944928,30.6149689532668));
#153971=CARTESIAN_POINT('Ctrl Pts',(-2.56539553607136,-6.52736341128647,
30.6071171062529));
#153972=CARTESIAN_POINT('Ctrl Pts',(-2.72524864978274,-6.45992618838306,
30.599265259239));
#153973=CARTESIAN_POINT('Ctrl Pts',(-2.88505643044338,-6.39250809013089,
30.5914156389454));
#153974=CARTESIAN_POINT('Ctrl Pts',(-3.04242660090272,-6.31912816543368,
30.5835660186518));
#153975=CARTESIAN_POINT('Ctrl Pts',(-3.1968710740518,-6.24000335724196,
30.5757163983582));
#153976=CARTESIAN_POINT('Ctrl Pts',(-3.35130321678492,-6.16088486615423,
30.5678674047564));
#153977=CARTESIAN_POINT('Ctrl Pts',(-3.50280978803967,-6.07602257922963,
30.5600184111546));
#153978=CARTESIAN_POINT('Ctrl Pts',(-3.65092612509904,-5.98567999408332,
30.5521694175528));
#153979=CARTESIAN_POINT('Ctrl Pts',(-3.79911744912295,-5.89529167113142,
30.5443164502354));
#153980=CARTESIAN_POINT('Ctrl Pts',(-3.94391478345556,-5.79941770523523,
30.536463482918));
#153981=CARTESIAN_POINT('Ctrl Pts',(-4.08488107547273,-5.69836583256505,
30.5286105156005));
#153982=CARTESIAN_POINT('Ctrl Pts',(-4.22588316819149,-5.59728829611463,
30.5207555538933));
#153983=CARTESIAN_POINT('Ctrl Pts',(-4.36305197863703,-5.49103046671003,
30.512900592186));
#153984=CARTESIAN_POINT('Ctrl Pts',(-4.49598306688087,-5.37994078264998,
30.5050456304787));
#153985=CARTESIAN_POINT('Ctrl Pts',(-4.62904610034134,-5.26874083279265,
30.4971828720654));
#153986=CARTESIAN_POINT('Ctrl Pts',(-4.75786272725996,-5.1526997046112,
30.489320113652));
#153987=CARTESIAN_POINT('Ctrl Pts',(-4.88206453378519,-5.03220353825805,
30.4814573552387));
#153988=CARTESIAN_POINT('Ctrl Pts',(-4.97317719686141,-4.94380927963927,
30.4756893484905));
#153989=CARTESIAN_POINT('Ctrl Pts',(-5.06180716553638,-4.85301833475441,
30.4699213417424));
#153990=CARTESIAN_POINT('Ctrl Pts',(-5.14782290711501,-4.75999431506824,
30.4641533349943));
#153991=CARTESIAN_POINT('Ctrl Pts',(-5.27276131814498,-4.62487633556926,
30.4557752685533));
#153992=CARTESIAN_POINT('Ctrl Pts',(-5.39245971855703,-4.48474669895984,
30.4473972021123));
#153993=CARTESIAN_POINT('Ctrl Pts',(-5.50651270748305,-4.34003967318592,
30.4390191356713));
#153994=CARTESIAN_POINT('Ctrl Pts',(-5.62048770833041,-4.19543159635682,
30.4306467980525));
#153995=CARTESIAN_POINT('Ctrl Pts',(-5.72882479108331,-4.04625262793735,
30.4222744604338));
#153996=CARTESIAN_POINT('Ctrl Pts',(-5.83115784931125,-3.89297119163703,
30.4139021228151));
#153997=CARTESIAN_POINT('Ctrl Pts',(-5.93343594062039,-3.73977208853781,
30.4055342822925));
#153998=CARTESIAN_POINT('Ctrl Pts',(-6.02971625560733,-3.58247518408994,
30.3971664417699));
#153999=CARTESIAN_POINT('Ctrl Pts',(-6.11967489796566,-3.42157941683501,
30.3887986012473));
#154000=CARTESIAN_POINT('Ctrl Pts',(-6.20959839845578,-3.26074650266123,
30.3804340295774));
#154001=CARTESIAN_POINT('Ctrl Pts',(-6.29320499072888,-3.09631781568865,
30.3720694579075));
#154002=CARTESIAN_POINT('Ctrl Pts',(-6.37021556185225,-2.92881891861471,
30.3637048862376));
#154003=CARTESIAN_POINT('Ctrl Pts',(-6.44720732169168,-2.76136093630438,
30.355342357772));
#154004=CARTESIAN_POINT('Ctrl Pts',(-6.51760613671886,-2.59083453803814,
30.3469798293064));
#154005=CARTESIAN_POINT('Ctrl Pts',(-6.58117988695108,-2.41778780253574,
30.3386173008408));
#154006=CARTESIAN_POINT('Ctrl Pts',(-6.64475871056746,-2.24472725736247,
30.3302541050193));
#154007=CARTESIAN_POINT('Ctrl Pts',(-6.70151126222156,-2.06914627954793,
30.3218909091978));
#154008=CARTESIAN_POINT('Ctrl Pts',(-6.75125414920415,-1.89161147579352,
30.3135277133763));
#154009=CARTESIAN_POINT('Ctrl Pts',(-6.80100042855192,-1.71406456452137,
30.3051639472016));
#154010=CARTESIAN_POINT('Ctrl Pts',(-6.84373600107348,-1.53456387818199,
30.2968001810269));
#154011=CARTESIAN_POINT('Ctrl Pts',(-6.8793277539502,-1.35368985230387,
30.2884364148522));
#154012=CARTESIAN_POINT('Ctrl Pts',(-6.91492667933099,-1.17277937641747,
30.2800709631986));
#154013=CARTESIAN_POINT('Ctrl Pts',(-6.94337885093577,-0.990495331733168,
30.2717055115451));
#154014=CARTESIAN_POINT('Ctrl Pts',(-6.96460246864214,-0.807427406200588,
30.2633400598915));
#154015=CARTESIAN_POINT('Ctrl Pts',(-6.98583319409635,-0.62429817157966,
30.2549718066647));
#154016=CARTESIAN_POINT('Ctrl Pts',(-6.99983050060385,-0.440384859104023,
30.2466035534378));
#154017=CARTESIAN_POINT('Ctrl Pts',(-7.00656450931262,-0.256281757721546,
30.2382353002109));
#154018=CARTESIAN_POINT('Ctrl Pts',(-7.01330476140818,-0.0720079664988862,
30.2298592884195));
#154019=CARTESIAN_POINT('Ctrl Pts',(-7.01276824690753,0.112455636350494,
30.221483276628));
#154020=CARTESIAN_POINT('Ctrl Pts',(-7.00497722994792,0.296514030715599,
30.2131072648365));
#154021=CARTESIAN_POINT('Ctrl Pts',(-6.99718239217732,0.480662689591468,
30.2047271453454));
#154022=CARTESIAN_POINT('Ctrl Pts',(-6.98212597764208,0.664405415695956,
30.1963470258542));
#154023=CARTESIAN_POINT('Ctrl Pts',(-6.95988216650108,0.847152165151158,
30.1879669063631));
#154024=CARTESIAN_POINT('Ctrl Pts',(-6.93761293898814,1.0301077259168,30.1795772115239));
#154025=CARTESIAN_POINT('Ctrl Pts',(-6.90813995077994,1.21206471037733,
30.1711875166847));
#154026=CARTESIAN_POINT('Ctrl Pts',(-6.87158878422795,1.39244179159226,
30.1627978218455));
#154027=CARTESIAN_POINT('Ctrl Pts',(-6.8483830793379,1.50696008773605,30.1574713493708));
#154028=CARTESIAN_POINT('Ctrl Pts',(-6.82232535479647,1.62084179431224,
30.1521448768961));
#154029=CARTESIAN_POINT('Ctrl Pts',(-6.79345819193923,1.73394127838109,
30.1468184044215));
#154030=CARTESIAN_POINT('Ctrl Pts',(-6.74803519108937,1.91190535425455,
30.1384371040166));
#154031=CARTESIAN_POINT('Ctrl Pts',(-6.69556204792646,2.08829092126232,
30.1300558036117));
#154032=CARTESIAN_POINT('Ctrl Pts',(-6.63616141893694,2.26251810695801,
30.1216745032068));
#154033=CARTESIAN_POINT('Ctrl Pts',(-6.57683607154906,2.43652448520081,
30.1133038248732));
#154034=CARTESIAN_POINT('Ctrl Pts',(-6.51060083998953,2.6083776259555,30.1049331465396));
#154035=CARTESIAN_POINT('Ctrl Pts',(-6.43762892445247,2.7775097467971,30.0965624682061));
#154036=CARTESIAN_POINT('Ctrl Pts',(-6.3647398195109,2.94644993172011,30.0882012891553));
#154037=CARTESIAN_POINT('Ctrl Pts',(-6.28512939688715,3.11267495222,30.0798401101044));
#154038=CARTESIAN_POINT('Ctrl Pts',(-6.19902015630494,3.27563362789935,
30.0714789310536));
#154039=CARTESIAN_POINT('Ctrl Pts',(-6.11302265261986,3.43838084547435,
30.0631286016189));
#154040=CARTESIAN_POINT('Ctrl Pts',(-6.02054330380952,3.59786988397599,
30.0547782721842));
#154041=CARTESIAN_POINT('Ctrl Pts',(-5.92185200977382,3.75357101129547,
30.0464279427494));
#154042=CARTESIAN_POINT('Ctrl Pts',(-5.8232366527853,3.90915233591134,30.0380840383937));
#154043=CARTESIAN_POINT('Ctrl Pts',(-5.71841905035115,4.0609512819887,30.029740134038));
#154044=CARTESIAN_POINT('Ctrl Pts',(-5.60771474562497,4.20846312734237,
30.0213962296822));
#154045=CARTESIAN_POINT('Ctrl Pts',(-5.49709935928672,4.35585649026193,
30.0130590272025));
#154046=CARTESIAN_POINT('Ctrl Pts',(-5.38060689655022,4.49896935857856,
30.0047218247228));
#154047=CARTESIAN_POINT('Ctrl Pts',(-5.25859597101388,4.6373262744966,29.9963846222431));
#154048=CARTESIAN_POINT('Ctrl Pts',(-5.21843064781213,4.68287260750423,
29.9936400612071));
#154049=CARTESIAN_POINT('Ctrl Pts',(-5.17766763597383,4.7279037864933,29.9908955001711));
#154050=CARTESIAN_POINT('Ctrl Pts',(-5.13632071722715,4.77240359276992,
29.988150939135));
#154051=CARTESIAN_POINT('Ctrl Pts',(-5.01070374824296,4.90759941761722,
29.9798126288331));
#154052=CARTESIAN_POINT('Ctrl Pts',(-4.87979739535233,5.03777707888049,
29.9714743185312));
#154053=CARTESIAN_POINT('Ctrl Pts',(-4.74403857862696,5.16253082576744,
29.9631360082293));
#154054=CARTESIAN_POINT('Ctrl Pts',(-4.60819434706087,5.28736306347862,
29.9547924517455));
#154055=CARTESIAN_POINT('Ctrl Pts',(-4.46749180331662,5.40676435837349,
29.9464488952617));
#154056=CARTESIAN_POINT('Ctrl Pts',(-4.32240126740431,5.52036899546051,
29.9381053387779));
#154057=CARTESIAN_POINT('Ctrl Pts',(-4.17720034724476,5.63406006246019,
29.9297554345527));
#154058=CARTESIAN_POINT('Ctrl Pts',(-4.02760503365489,5.74194547323107,
29.9214055303275));
#154059=CARTESIAN_POINT('Ctrl Pts',(-3.87411529770678,5.84370235574797,
29.9130556261023));
#154060=CARTESIAN_POINT('Ctrl Pts',(-3.72039533851287,5.94561186605871,
29.9046931976387));
#154061=CARTESIAN_POINT('Ctrl Pts',(-3.56276955744135,6.04137429772846,
29.896330769175));
#154062=CARTESIAN_POINT('Ctrl Pts',(-3.40176455166731,6.1307115816616,29.8879683407114));
#154063=CARTESIAN_POINT('Ctrl Pts',(-3.24062186466519,6.22012526115094,
29.8795987612314));
#154064=CARTESIAN_POINT('Ctrl Pts',(-3.07609447912067,6.30310268300638,
29.8712291817515));
#154065=CARTESIAN_POINT('Ctrl Pts',(-2.90873022784017,6.37941337617723,
29.8628596022715));
#154066=CARTESIAN_POINT('Ctrl Pts',(-2.74110783759349,6.4558417692947,29.8544771137349));
#154067=CARTESIAN_POINT('Ctrl Pts',(-2.57064014068247,6.52558276216785,
29.8460946251984));
#154068=CARTESIAN_POINT('Ctrl Pts',(-2.39789275106961,6.588454820128,29.8377121366618));
#154069=CARTESIAN_POINT('Ctrl Pts',(-2.34136697455426,6.60902758771239,
29.8349692490574));
#154070=CARTESIAN_POINT('Ctrl Pts',(-2.28459721094064,6.62886529793537,
29.832226361453));
#154071=CARTESIAN_POINT('Ctrl Pts',(-2.22760354135085,6.64796277253876,
29.8294834738486));
#154072=CARTESIAN_POINT('Ctrl Pts',(-2.05327316391254,6.7063775049062,29.8210936187158));
#154073=CARTESIAN_POINT('Ctrl Pts',(-1.87649502487367,6.75798071670244,
29.812703763583));
#154074=CARTESIAN_POINT('Ctrl Pts',(-1.6978281097707,6.80257350362144,29.8043139084503));
#154075=CARTESIAN_POINT('Ctrl Pts',(-1.51932606599218,6.84712514094184,
29.7959317953582));
#154076=CARTESIAN_POINT('Ctrl Pts',(-1.33893903809313,6.88467917035211,
29.7875496822661));
#154077=CARTESIAN_POINT('Ctrl Pts',(-1.15724183614367,6.91508625363262,
29.779167569174));
#154078=CARTESIAN_POINT('Ctrl Pts',(-0.975685592713515,6.94546974746107,
29.7707919588251));
#154079=CARTESIAN_POINT('Ctrl Pts',(-0.792821524714185,6.96871729517118,
29.7624163484762));
#154080=CARTESIAN_POINT('Ctrl Pts',(-0.609235770880054,6.98473036974085,
29.7540407381274));
#154081=CARTESIAN_POINT('Ctrl Pts',(-0.425765495211278,7.00073337184883,
29.7456703961618));
#154082=CARTESIAN_POINT('Ctrl Pts',(-0.241574765484927,7.009510945796,29.7373000541962));
#154083=CARTESIAN_POINT('Ctrl Pts',(-0.0572564586337002,7.01101620740137,
29.7289297122306));
#154084=CARTESIAN_POINT('Ctrl Pts',(0.126972928259185,7.01252074282929,
29.7205634083363));
#154085=CARTESIAN_POINT('Ctrl Pts',(0.311329441416462,7.00675995946011,
29.712197104442));
#154086=CARTESIAN_POINT('Ctrl Pts',(0.495218112667432,6.99373902740059,
29.7038308005477));
#154087=CARTESIAN_POINT('Ctrl Pts',(0.679055355411382,6.98072173693079,
29.695466836474));
#154088=CARTESIAN_POINT('Ctrl Pts',(0.862424689500081,6.96044836823139,
29.6871028724004));
#154089=CARTESIAN_POINT('Ctrl Pts',(1.04473362048138,6.93297614482668,29.6787389083268));
#154090=CARTESIAN_POINT('Ctrl Pts',(1.2270144971478,6.90550814894063,29.6703762313283));
#154091=CARTESIAN_POINT('Ctrl Pts',(1.40823497115759,6.87084355600778,29.6620135543297));
#154092=CARTESIAN_POINT('Ctrl Pts',(1.58780970527041,6.829091220825,29.6536508773312));
#154093=CARTESIAN_POINT('Ctrl Pts',(1.76738074226754,6.78733974524652,29.6452883725049));
#154094=CARTESIAN_POINT('Ctrl Pts',(1.94530578691105,6.73850089320938,29.6369258676786));
#154095=CARTESIAN_POINT('Ctrl Pts',(2.12101127109405,6.68273430194498,29.6285633628523));
#154096=CARTESIAN_POINT('Ctrl Pts',(2.29673655811301,6.62696142552298,29.6201999155323));
#154097=CARTESIAN_POINT('Ctrl Pts',(2.47024147285925,6.56425935313404,29.6118364682123));
#154098=CARTESIAN_POINT('Ctrl Pts',(2.64096873086428,6.49483723622826,29.6034730208923));
#154099=CARTESIAN_POINT('Ctrl Pts',(2.81179651787647,6.42537424162919,29.5951046489395));
#154100=CARTESIAN_POINT('Ctrl Pts',(2.97984307477428,6.34918341861954,29.5867362769867));
#154101=CARTESIAN_POINT('Ctrl Pts',(3.14457123150864,6.26652202840365,29.5783679050339));
#154102=CARTESIAN_POINT('Ctrl Pts',(3.30934874510399,6.18383587067488,29.5699970256981));
#154103=CARTESIAN_POINT('Ctrl Pts',(3.47080558453469,6.09467543208002,29.5616261463624));
#154104=CARTESIAN_POINT('Ctrl Pts',(3.62842960468568,5.99934372797063,29.5532552670266));
#154105=CARTESIAN_POINT('Ctrl Pts',(3.78618717796451,5.9039312503392,29.5448772951353));
#154106=CARTESIAN_POINT('Ctrl Pts',(3.94010516420754,5.80233723384743,29.536499323244));
#154107=CARTESIAN_POINT('Ctrl Pts',(4.08969983617666,5.69490841124566,29.5281213513527));
#154108=CARTESIAN_POINT('Ctrl Pts',(4.18476846836697,5.62663651968609,29.5227970819937));
#154109=CARTESIAN_POINT('Ctrl Pts',(4.27809165190787,5.55600897634346,29.5174728126348));
#154110=CARTESIAN_POINT('Ctrl Pts',(4.36955219335547,5.48312321510674,29.5121485432758));
#154111=CARTESIAN_POINT('Ctrl Pts',(4.50462026549713,5.37548620464291,29.5042857120865));
#154112=CARTESIAN_POINT('Ctrl Pts',(4.63590515167403,5.26269828661749,29.4964228808972));
#154113=CARTESIAN_POINT('Ctrl Pts',(4.76297282760709,5.14506719159008,29.4885600497079));
#154114=CARTESIAN_POINT('Ctrl Pts',(4.88994286880393,5.02752648053207,29.4807032600665));
#154115=CARTESIAN_POINT('Ctrl Pts',(5.01270186571746,4.90515025023247,29.4728464704251));
#154116=CARTESIAN_POINT('Ctrl Pts',(5.13084717804913,4.77828774751011,29.4649896807837));
#154117=CARTESIAN_POINT('Ctrl Pts',(5.2489258620171,4.65149678923421,29.4571373219998));
#154118=CARTESIAN_POINT('Ctrl Pts',(5.36239577814475,4.52022486952118,29.4492849632159));
#154119=CARTESIAN_POINT('Ctrl Pts',(5.47088981512912,4.38485931281911,29.4414326044319));
#154120=CARTESIAN_POINT('Ctrl Pts',(5.57935823540567,4.24952571750415,29.4335820996815));
#154121=CARTESIAN_POINT('Ctrl Pts',(5.68285287002689,4.1101007008737,29.4257315949311));
#154122=CARTESIAN_POINT('Ctrl Pts',(5.78104577594338,3.96700596154673,29.4178810901807));
#154123=CARTESIAN_POINT('Ctrl Pts',(5.87922288571611,3.8239342416533,29.410031848329));
#154124=CARTESIAN_POINT('Ctrl Pts',(5.97209975122812,3.6771942905496,29.4021826064774));
#154125=CARTESIAN_POINT('Ctrl Pts',(6.05939107001984,3.52723778941311,29.3943333646257));
#154126=CARTESIAN_POINT('Ctrl Pts',(6.14671179896544,3.37723076499623,29.3864814782109));
#154127=CARTESIAN_POINT('Ctrl Pts',(6.2284430301416,3.224005355905,29.378629591796));
#154128=CARTESIAN_POINT('Ctrl Pts',(6.30434475482012,3.06803907649039,29.3707777053812));
#154129=CARTESIAN_POINT('Ctrl Pts',(6.36007844652168,2.95351497878972,29.3650121629172));
#154130=CARTESIAN_POINT('Ctrl Pts',(6.41266993519047,2.83751361474207,29.3592466204533));
#154131=CARTESIAN_POINT('Ctrl Pts',(6.46204063733937,2.7202311232457,29.3534810779893));
#154132=CARTESIAN_POINT('Ctrl Pts',(6.50035037448015,2.62922448925273,29.3490072421585));
#154133=CARTESIAN_POINT('Ctrl Pts',(6.53671425519462,2.53746348401301,29.3445334063276));
#154134=CARTESIAN_POINT('Ctrl Pts',(6.57110895151813,2.4450263208764,29.3400595704968));
#154135=CARTESIAN_POINT('Origin',(0.,0.,50.));
#154136=CARTESIAN_POINT('',(6.57110895151815,2.44502632087633,27.3397910544677));
#154137=CARTESIAN_POINT('',(6.57110895151815,2.44502632087634,27.8869594752573));
#154138=CARTESIAN_POINT('',(6.57110895151814,2.44502632087636,50.));
#154139=CARTESIAN_POINT('',(7.01124999898235,0.000119457237031912,29.7735343568796));
#154140=CARTESIAN_POINT('Ctrl Pts',(6.57110895151814,2.44502632087635,27.8869594752573));
#154141=CARTESIAN_POINT('Ctrl Pts',(6.49449213640473,2.65093716745085,27.8969648340648));
#154142=CARTESIAN_POINT('Ctrl Pts',(6.40816968419754,2.85330601056279,27.9069701928724));
#154143=CARTESIAN_POINT('Ctrl Pts',(6.31245749192074,3.05131233655189,27.9169755516799));
#154144=CARTESIAN_POINT('Ctrl Pts',(6.23561263111062,3.21028652989345,27.9250085972787));
#154145=CARTESIAN_POINT('Ctrl Pts',(6.15267817288181,3.36652193378537,27.9330416428775));
#154146=CARTESIAN_POINT('Ctrl Pts',(6.063879900354,3.51951518203612,27.9410746884763));
#154147=CARTESIAN_POINT('Ctrl Pts',(5.9751387107748,3.67241008033615,27.9491025701241));
#154148=CARTESIAN_POINT('Ctrl Pts',(5.88054139339257,3.82206665589529,27.9571304517719));
#154149=CARTESIAN_POINT('Ctrl Pts',(5.78036050396136,3.96800441112955,27.9651583334197));
#154150=CARTESIAN_POINT('Ctrl Pts',(5.68022484718948,4.11387627402842,27.9731825903997));
#154151=CARTESIAN_POINT('Ctrl Pts',(5.57451084507305,4.25603235826394,27.9812068473798));
#154152=CARTESIAN_POINT('Ctrl Pts',(5.46353534836288,4.39401957889235,27.9892311043599));
#154153=CARTESIAN_POINT('Ctrl Pts',(5.35257326972032,4.53199011546066,27.9972543911256));
#154154=CARTESIAN_POINT('Ctrl Pts',(5.23635118721347,4.66579250210413,28.0052776778913));
#154155=CARTESIAN_POINT('Ctrl Pts',(5.11522747005976,4.79500516079452,28.013300964657));
#154156=CARTESIAN_POINT('Ctrl Pts',(4.99411367791395,4.92420723166043,28.0213235939859));
#154157=CARTESIAN_POINT('Ctrl Pts',(4.86809930484048,5.04882005895622,28.0293462233148));
#154158=CARTESIAN_POINT('Ctrl Pts',(4.73758074168348,5.16845772726544,28.0373688526438));
#154159=CARTESIAN_POINT('Ctrl Pts',(4.60701311283887,5.28814037082046,28.0453944979101));
#154160=CARTESIAN_POINT('Ctrl Pts',(4.47193818378545,5.40284387349322,28.0534201431765));
#154161=CARTESIAN_POINT('Ctrl Pts',(4.33278697619247,5.51222129285799,28.0614457884429));
#154162=CARTESIAN_POINT('Ctrl Pts',(4.25073494473848,5.57671688444728,28.0661781979507));
#154163=CARTESIAN_POINT('Ctrl Pts',(4.16726621787055,5.63936136101981,28.0709106074586));
#154164=CARTESIAN_POINT('Ctrl Pts',(4.08247411608823,5.70009049524388,28.0756430169664));
#154165=CARTESIAN_POINT('Ctrl Pts',(3.92605502595416,5.8121197493877,28.084373065801));
#154166=CARTESIAN_POINT('Ctrl Pts',(3.76505279119581,5.91768488095134,28.0931031146357));
#154167=CARTESIAN_POINT('Ctrl Pts',(3.60001325395084,6.01643840938128,28.1018331634704));
#154168=CARTESIAN_POINT('Ctrl Pts',(3.43492599531807,6.11522049251699,28.1105657366095));
#154169=CARTESIAN_POINT('Ctrl Pts',(3.26579933909619,6.20718690046475,28.1192983097487));
#154170=CARTESIAN_POINT('Ctrl Pts',(3.09320522066855,6.29203528481277,28.1280308828878));
#154171=CARTESIAN_POINT('Ctrl Pts',(2.91815912727661,6.37808907590394,28.1368875161683));
#154172=CARTESIAN_POINT('Ctrl Pts',(2.73954655923852,6.45682092833929,28.1457441494487));
#154173=CARTESIAN_POINT('Ctrl Pts',(2.55798720584053,6.52796507475769,28.1546007827291));
#154174=CARTESIAN_POINT('Ctrl Pts',(2.37885710470831,6.59815731715325,28.1633389148358));
#154175=CARTESIAN_POINT('Ctrl Pts',(2.1968588511512,6.66096355880477,28.1720770469426));
#154176=CARTESIAN_POINT('Ctrl Pts',(2.01260584967943,6.71617780112589,28.1808151790494));
#154177=CARTESIAN_POINT('Ctrl Pts',(1.82460475937334,6.77251521584304,28.1897310629166));
#154178=CARTESIAN_POINT('Ctrl Pts',(1.63425648870766,6.82094836000736,28.1986469467838));
#154179=CARTESIAN_POINT('Ctrl Pts',(1.44222785267097,6.86131222023019,28.2075628306511));
#154180=CARTESIAN_POINT('Ctrl Pts',(1.25019921663424,6.90167608045302,28.2164787145183));
#154181=CARTESIAN_POINT('Ctrl Pts',(1.05649051242281,6.93397060048049,28.2253945983855));
#154182=CARTESIAN_POINT('Ctrl Pts',(0.861779521940682,6.95808613183709,
28.2343104822528));
#154183=CARTESIAN_POINT('Ctrl Pts',(0.670894651624785,6.98172778690857,
28.243051166749));
#154184=CARTESIAN_POINT('Ctrl Pts',(0.479026245877058,6.99751141897453,
28.2517918512452));
#154185=CARTESIAN_POINT('Ctrl Pts',(0.28681877544978,7.00538089989042,28.2605325357414));
#154186=CARTESIAN_POINT('Ctrl Pts',(0.0946458863390992,7.01324896495598,
28.2692716476433));
#154187=CARTESIAN_POINT('Ctrl Pts',(-0.0978656721553102,7.01320571128652,
28.2780107595452));
#154188=CARTESIAN_POINT('Ctrl Pts',(-0.2900690439721,7.00524707003466,28.286749871447));
#154189=CARTESIAN_POINT('Ctrl Pts',(-0.484762687099649,6.99718531313089,
28.2956022111214));
#154190=CARTESIAN_POINT('Ctrl Pts',(-0.679139816174599,6.9810016176754,
28.3044545507957));
#154191=CARTESIAN_POINT('Ctrl Pts',(-0.872529556733192,6.95674627502879,
28.3133068904701));
#154192=CARTESIAN_POINT('Ctrl Pts',(-1.06334784931464,6.93281344872459,
28.3220415231198));
#154193=CARTESIAN_POINT('Ctrl Pts',(-1.25320457131862,6.90102234370817,
28.3307761557696));
#154194=CARTESIAN_POINT('Ctrl Pts',(-1.44146079353006,6.86147340905841,
28.3395107884193));
#154195=CARTESIAN_POINT('Ctrl Pts',(-1.63352239840614,6.82112503825429,
28.348421981606));
#154196=CARTESIAN_POINT('Ctrl Pts',(-1.82391782121114,6.77270190480895,
28.3573331747926));
#154197=CARTESIAN_POINT('Ctrl Pts',(-2.01197890935735,6.7163656415357,28.3662443679792));
#154198=CARTESIAN_POINT('Ctrl Pts',(-2.20003999750359,6.66002937826244,
28.3751555611659));
#154199=CARTESIAN_POINT('Ctrl Pts',(-2.38576645674396,6.5957800592414,28.3840667543525));
#154200=CARTESIAN_POINT('Ctrl Pts',(-2.56850496940774,6.52383390228689,
28.3929779475392));
#154201=CARTESIAN_POINT('Ctrl Pts',(-2.73308428303568,6.45903722118701,
28.4010036123916));
#154202=CARTESIAN_POINT('Ctrl Pts',(-2.89531542892217,6.38796714380733,
28.409029277244));
#154203=CARTESIAN_POINT('Ctrl Pts',(-3.05468423894557,6.3108264722489,28.4170549420963));
#154204=CARTESIAN_POINT('Ctrl Pts',(-3.21400246921774,6.23371028324748,
28.4250780597996));
#154205=CARTESIAN_POINT('Ctrl Pts',(-3.37045984267823,6.15052749538051,
28.4331011775028));
#154206=CARTESIAN_POINT('Ctrl Pts',(-3.523563244396,6.06152857167576,28.441124295206));
#154207=CARTESIAN_POINT('Ctrl Pts',(-3.67664733843497,5.97254087151414,
28.4491464011239));
#154208=CARTESIAN_POINT('Ctrl Pts',(-3.82637798670055,5.87773868117624,
28.4571685070418));
#154209=CARTESIAN_POINT('Ctrl Pts',(-3.9722877577215,5.77741780836006,28.4651906129596));
#154210=CARTESIAN_POINT('Ctrl Pts',(-4.11825174930623,5.67705965596866,
28.4732156999191));
#154211=CARTESIAN_POINT('Ctrl Pts',(-4.2603917231887,5.57117892973248,28.4812407868787));
#154212=CARTESIAN_POINT('Ctrl Pts',(-4.39826990371879,5.46011432266226,
28.4892658738382));
#154213=CARTESIAN_POINT('Ctrl Pts',(-4.53617523866651,5.3490278419735,28.4972925412984));
#154214=CARTESIAN_POINT('Ctrl Pts',(-4.66981682822056,5.23275568338216,
28.5053192087587));
#154215=CARTESIAN_POINT('Ctrl Pts',(-4.79879112615074,5.11167587881674,
28.5133458762189));
#154216=CARTESIAN_POINT('Ctrl Pts',(-4.92786896419288,4.99049887181083,
28.5213789874595));
#154217=CARTESIAN_POINT('Ctrl Pts',(-5.05227176630182,4.86450676794351,
28.5294120987001));
#154218=CARTESIAN_POINT('Ctrl Pts',(-5.17163347093701,4.73411383521605,
28.5374452099407));
#154219=CARTESIAN_POINT('Ctrl Pts',(-5.24196572335827,4.65728158247163,
28.5421786109023));
#154220=CARTESIAN_POINT('Ctrl Pts',(-5.31054845581914,4.57892201252761,
28.546912011864));
#154221=CARTESIAN_POINT('Ctrl Pts',(-5.37731352235279,4.49912500880136,
28.5516454128256));
#154222=CARTESIAN_POINT('Ctrl Pts',(-5.51485163727835,4.33474069767834,
28.5613963661197));
#154223=CARTESIAN_POINT('Ctrl Pts',(-5.64475541595091,4.16415819944942,
28.5711473194139));
#154224=CARTESIAN_POINT('Ctrl Pts',(-5.76655261146059,3.98804432545039,
28.580898272708));
#154225=CARTESIAN_POINT('Ctrl Pts',(-5.88852527867925,3.81167672637735,
28.5906632740796));
#154226=CARTESIAN_POINT('Ctrl Pts',(-6.00236797921543,3.6297618429951,28.6004282754512));
#154227=CARTESIAN_POINT('Ctrl Pts',(-6.10765108552397,3.44299648271646,
28.6101932768228));
#154228=CARTESIAN_POINT('Ctrl Pts',(-6.21275870670836,3.25654242159665,
28.6199420019604));
#154229=CARTESIAN_POINT('Ctrl Pts',(-6.30933522912802,3.0652540747158,28.629690727098));
#154230=CARTESIAN_POINT('Ctrl Pts',(-6.39699779056177,2.86985118604569,
28.6394394522356));
#154231=CARTESIAN_POINT('Ctrl Pts',(-6.48441975225538,2.67498460253787,
28.6491614209027));
#154232=CARTESIAN_POINT('Ctrl Pts',(-6.56297657772261,2.4760260579487,28.6588833895698));
#154233=CARTESIAN_POINT('Ctrl Pts',(-6.6323333495813,2.27371522019176,28.668605358237));
#154234=CARTESIAN_POINT('Ctrl Pts',(-6.70123120579561,2.07274302040754,
28.6782629991767));
#154235=CARTESIAN_POINT('Ctrl Pts',(-6.7610503122403,1.86846277810626,28.6879206401164));
#154236=CARTESIAN_POINT('Ctrl Pts',(-6.81150718628199,1.66162463081433,
28.697578281056));
#154237=CARTESIAN_POINT('Ctrl Pts',(-6.8336847195478,1.57071214407534,28.7018231467414));
#154238=CARTESIAN_POINT('Ctrl Pts',(-6.85405414701578,1.4793058181311,28.7060680124267));
#154239=CARTESIAN_POINT('Ctrl Pts',(-6.87259420767519,1.38747087145262,
28.7103128781121));
#154240=CARTESIAN_POINT('Ctrl Pts',(-6.90688827743316,1.21760119705035,
28.718164725126));
#154241=CARTESIAN_POINT('Ctrl Pts',(-6.93490536937299,1.04633401805437,
28.7260165721399));
#154242=CARTESIAN_POINT('Ctrl Pts',(-6.95653755564094,0.874192083844924,
28.7338684191538));
#154243=CARTESIAN_POINT('Ctrl Pts',(-6.97816360719576,0.702098967696304,
28.7417180394474));
#154244=CARTESIAN_POINT('Ctrl Pts',(-6.99340830737022,0.529131967908664,
28.749567659741));
#154245=CARTESIAN_POINT('Ctrl Pts',(-7.00221515756077,0.355822216459495,
28.7574172800346));
#154246=CARTESIAN_POINT('Ctrl Pts',(-7.01102130463699,0.182526301577319,
28.7652662736364));
#154247=CARTESIAN_POINT('Ctrl Pts',(-7.01339060631142,0.0088880705190284,
28.7731152672382));
#154248=CARTESIAN_POINT('Ctrl Pts',(-7.00931859181233,-0.164558320889845,
28.78096426084));
#154249=CARTESIAN_POINT('Ctrl Pts',(-7.00524451577152,-0.338092523127861,
28.7888172281574));
#154250=CARTESIAN_POINT('Ctrl Pts',(-6.9947226167812,-0.51143430980403,
28.7966701954748));
#154251=CARTESIAN_POINT('Ctrl Pts',(-6.97780054194222,-0.684051284167264,
28.8045231627923));
#154252=CARTESIAN_POINT('Ctrl Pts',(-6.96087416946482,-0.856712097441932,
28.8123781244995));
#154253=CARTESIAN_POINT('Ctrl Pts',(-6.93754443419944,-1.02864735363224,
28.8202330862068));
#154254=CARTESIAN_POINT('Ctrl Pts',(-6.9079105436122,-1.19933251600692,
28.828088047914));
#154255=CARTESIAN_POINT('Ctrl Pts',(-6.87824723891148,-1.37018709767266,
28.8359508063274));
#154256=CARTESIAN_POINT('Ctrl Pts',(-6.84226736039405,-1.53978873428667,
28.8438135647407));
#154257=CARTESIAN_POINT('Ctrl Pts',(-6.80012078706305,-1.70762520590818,
28.8516763231541));
#154258=CARTESIAN_POINT('Ctrl Pts',(-6.76920266563492,-1.83074763317909,
28.8574443299022));
#154259=CARTESIAN_POINT('Ctrl Pts',(-6.73496700950739,-1.95292040784697,
28.8632123366503));
#154260=CARTESIAN_POINT('Ctrl Pts',(-6.69748962124275,-2.07394776593957,
28.8689803433985));
#154261=CARTESIAN_POINT('Ctrl Pts',(-6.64305347672562,-2.24974077235539,
28.8773584098395));
#154262=CARTESIAN_POINT('Ctrl Pts',(-6.58165583125913,-2.42350599110958,
28.8857364762805));
#154263=CARTESIAN_POINT('Ctrl Pts',(-6.51346971504031,-2.59467509213634,
28.8941145427215));
#154264=CARTESIAN_POINT('Ctrl Pts',(-6.44533022367758,-2.76572714976562,
28.9024868803403));
#154265=CARTESIAN_POINT('Ctrl Pts',(-6.37041163735338,-2.93418632446769,
28.910859217959));
#154266=CARTESIAN_POINT('Ctrl Pts',(-6.28893622386575,-3.099501207396,28.9192315555777));
#154267=CARTESIAN_POINT('Ctrl Pts',(-6.20750457387462,-3.26472729350828,
28.9275993961003));
#154268=CARTESIAN_POINT('Ctrl Pts',(-6.11952326408598,-3.426812161188,28.9359672366229));
#154269=CARTESIAN_POINT('Ctrl Pts',(-6.02526210732891,-3.58522566939466,
28.9443350771455));
#154270=CARTESIAN_POINT('Ctrl Pts',(-5.93103777319457,-3.74357729420153,
28.9526996488154));
#154271=CARTESIAN_POINT('Ctrl Pts',(-5.8305386519412,-3.89826013745946,
28.9610642204853));
#154272=CARTESIAN_POINT('Ctrl Pts',(-5.72408002124771,-4.04876950107718,
28.9694287921552));
#154273=CARTESIAN_POINT('Ctrl Pts',(-5.61764739508189,-4.19924209994522,
28.9777913206208));
#154274=CARTESIAN_POINT('Ctrl Pts',(-5.50525835252799,-4.345542984347,28.9861538490864));
#154275=CARTESIAN_POINT('Ctrl Pts',(-5.38727118564399,-4.48719686829428,
28.994516377552));
#154276=CARTESIAN_POINT('Ctrl Pts',(-5.26927460301499,-4.62886205666461,
29.0028795733735));
#154277=CARTESIAN_POINT('Ctrl Pts',(-5.14567920922331,-4.76587924727605,
29.011242769195));
#154278=CARTESIAN_POINT('Ctrl Pts',(-5.01688372631647,-4.89780606385359,
29.0196059650165));
#154279=CARTESIAN_POINT('Ctrl Pts',(-4.88807945981585,-5.02974187757559,
29.0279697311912));
#154280=CARTESIAN_POINT('Ctrl Pts',(-4.75407462659777,-5.15658638959434,
29.0363334973659));
#154281=CARTESIAN_POINT('Ctrl Pts',(-4.61530508773846,-5.27793382959615,
29.0446972635406));
#154282=CARTESIAN_POINT('Ctrl Pts',(-4.47650758383102,-5.39930572371829,
29.0530627151942));
#154283=CARTESIAN_POINT('Ctrl Pts',(-4.33294370715091,-5.51517812046617,
29.0614281668478));
#154284=CARTESIAN_POINT('Ctrl Pts',(-4.18508301291899,-5.62518504028773,
29.0697936185013));
#154285=CARTESIAN_POINT('Ctrl Pts',(-4.03717280043112,-5.73522880121059,
29.0781618717282));
#154286=CARTESIAN_POINT('Ctrl Pts',(-3.8849631646743,-5.83940297208849,
29.0865301249551));
#154287=CARTESIAN_POINT('Ctrl Pts',(-3.7289536328408,-5.93738421921837,
29.094898378182));
#154288=CARTESIAN_POINT('Ctrl Pts',(-3.57279945791429,-6.03545630894279,
29.1032743899734));
#154289=CARTESIAN_POINT('Ctrl Pts',(-3.41283862552856,-6.12732382619703,
29.1116504017649));
#154290=CARTESIAN_POINT('Ctrl Pts',(-3.24959739566591,-6.21270821209087,
29.1200264135564));
#154291=CARTESIAN_POINT('Ctrl Pts',(-3.08627611028722,-6.29813447154251,
29.1284065330475));
#154292=CARTESIAN_POINT('Ctrl Pts',(-2.91967151346045,-6.37707111278823,
29.1367866525387));
#154293=CARTESIAN_POINT('Ctrl Pts',(-2.75033154339166,-6.44928701205993,
29.1451667720298));
#154294=CARTESIAN_POINT('Ctrl Pts',(-2.58079808095614,-6.5215854271444,
29.153556466869));
#154295=CARTESIAN_POINT('Ctrl Pts',(-2.40852330489872,-6.5871476324327,
29.1619461617082));
#154296=CARTESIAN_POINT('Ctrl Pts',(-2.23407333608442,-6.64579136683485,
29.1703358565475));
#154297=CARTESIAN_POINT('Ctrl Pts',(-2.12331806132192,-6.68302326180712,
29.1756623290221));
#154298=CARTESIAN_POINT('Ctrl Pts',(-2.01168633077783,-6.71746748972033,
29.1809888014967));
#154299=CARTESIAN_POINT('Ctrl Pts',(-1.89932553437362,-6.74908801816782,
29.1863152739714));
#154300=CARTESIAN_POINT('Ctrl Pts',(-1.72252379684822,-6.79884348938106,
29.1946965743762));
#154301=CARTESIAN_POINT('Ctrl Pts',(-1.54355969267688,-6.84170545877291,
29.2030778747811));
#154302=CARTESIAN_POINT('Ctrl Pts',(-1.36299661903062,-6.87748986033503,
29.211459175186));
#154303=CARTESIAN_POINT('Ctrl Pts',(-1.18266238264766,-6.91322891040663,
29.2198298535196));
#154304=CARTESIAN_POINT('Ctrl Pts',(-1.00073353410862,-6.94190820531127,
29.2282005318531));
#154305=CARTESIAN_POINT('Ctrl Pts',(-0.817788303416799,-6.96339348689234,
29.2365712101867));
#154306=CARTESIAN_POINT('Ctrl Pts',(-0.635050684151665,-6.98485438636766,
29.2449323892375));
#154307=CARTESIAN_POINT('Ctrl Pts',(-0.45129930506122,-6.9991375062249,
29.2532935682883));
#154308=CARTESIAN_POINT('Ctrl Pts',(-0.267122700120177,-7.00615957751324,
29.2616547473392));
#154309=CARTESIAN_POINT('Ctrl Pts',(-0.0831850860494773,-7.01317253683577,
29.2700050767739));
#154310=CARTESIAN_POINT('Ctrl Pts',(0.101176327419426,-7.01294322847668,
29.2783554062086));
#154311=CARTESIAN_POINT('Ctrl Pts',(0.285367848513169,-7.00544015416126,
29.2867057356433));
#154312=CARTESIAN_POINT('Ctrl Pts',(0.469417645249815,-6.99794285301269,
29.2950496399991));
#154313=CARTESIAN_POINT('Ctrl Pts',(0.653297484127329,-6.98318295244637,
29.3033935443548));
#154314=CARTESIAN_POINT('Ctrl Pts',(0.836412478337948,-6.96118098662724,
29.3117374487106));
#154315=CARTESIAN_POINT('Ctrl Pts',(1.01938039344278,-6.93919669292432,
29.3200746511903));
#154316=CARTESIAN_POINT('Ctrl Pts',(1.20158436470146,-6.90998197386488,
29.32841185367));
#154317=CARTESIAN_POINT('Ctrl Pts',(1.38243328121407,-6.87360929828658,
29.3367490561497));
#154318=CARTESIAN_POINT('Ctrl Pts',(1.44196774626718,-6.86163561425871,
29.3394936171857));
#154319=CARTESIAN_POINT('Ctrl Pts',(1.50135540542682,-6.84888664744455,
29.3422381782218));
#154320=CARTESIAN_POINT('Ctrl Pts',(1.56057531963233,-6.83536621069087,
29.3449827392578));
#154321=CARTESIAN_POINT('Ctrl Pts',(1.74049262306095,-6.79428947907898,
29.3533210495597));
#154322=CARTESIAN_POINT('Ctrl Pts',(1.91871320861433,-6.74612185920696,
29.3616593598616));
#154323=CARTESIAN_POINT('Ctrl Pts',(2.09466711579002,-6.69103850209576,
29.3699976701635));
#154324=CARTESIAN_POINT('Ctrl Pts',(2.27073172719311,-6.63592048840553,
29.3783412266473));
#154325=CARTESIAN_POINT('Ctrl Pts',(2.44452650296433,-6.57387815646015,
29.3866847831311));
#154326=CARTESIAN_POINT('Ctrl Pts',(2.61549942395021,-6.50513561163917,
29.3950283396149));
#154327=CARTESIAN_POINT('Ctrl Pts',(2.78660242038971,-6.4363407677895,29.4033782438401));
#154328=CARTESIAN_POINT('Ctrl Pts',(2.95487897611399,-6.36083566531951,
29.4117281480654));
#154329=CARTESIAN_POINT('Ctrl Pts',(3.11979931998863,-6.27889152362887,
29.4200780522906));
#154330=CARTESIAN_POINT('Ctrl Pts',(3.28496703217464,-6.19682447178973,
29.4284404807543));
#154331=CARTESIAN_POINT('Ctrl Pts',(3.44676817917632,-6.10829922676537,
29.4368029092179));
#154332=CARTESIAN_POINT('Ctrl Pts',(3.60469844876366,-6.01363248427944,
29.4451653376816));
#154333=CARTESIAN_POINT('Ctrl Pts',(3.76276377026057,-5.9188847888237,29.4535349171615));
#154334=CARTESIAN_POINT('Ctrl Pts',(3.9169513362688,-5.81798529615717,29.4619044966415));
#154335=CARTESIAN_POINT('Ctrl Pts',(4.06678741138989,-5.71129291080932,
29.4702740761214));
#154336=CARTESIAN_POINT('Ctrl Pts',(4.21685459040094,-5.60443596545639,
29.478656564658));
#154337=CARTESIAN_POINT('Ctrl Pts',(4.36255660796396,-5.49176847300578,
29.4870390531946));
#154338=CARTESIAN_POINT('Ctrl Pts',(4.50345319323985,-5.37368922610881,
29.4954215417311));
#154339=CARTESIAN_POINT('Ctrl Pts',(4.54955686466963,-5.33505176168087,
29.4981644293355));
#154340=CARTESIAN_POINT('Ctrl Pts',(4.59514631446224,-5.2958351468955,29.5009073169399));
#154341=CARTESIAN_POINT('Ctrl Pts',(4.64020700827224,-5.25605417427191,
29.5036502045443));
#154342=CARTESIAN_POINT('Ctrl Pts',(4.77571791990833,-5.13642095493618,
29.5118988835671));
#154343=CARTESIAN_POINT('Ctrl Pts',(4.90674524486949,-5.01141517077875,
29.52014756259));
#154344=CARTESIAN_POINT('Ctrl Pts',(5.03284519947687,-4.88140305246378,
29.5283962416128));
#154345=CARTESIAN_POINT('Ctrl Pts',(5.15882230318774,-4.75151759640924,
29.5366368844899));
#154346=CARTESIAN_POINT('Ctrl Pts',(5.27988136223031,-4.6166357707436,29.544877527367));
#154347=CARTESIAN_POINT('Ctrl Pts',(5.39561293035008,-4.47716290393135,
29.5531181702441));
#154348=CARTESIAN_POINT('Ctrl Pts',(5.51125271317169,-4.33780065135232,
29.5613522775677));
#154349=CARTESIAN_POINT('Ctrl Pts',(5.62157320513941,-4.1938548782192,29.5695863848912));
#154350=CARTESIAN_POINT('Ctrl Pts',(5.72620281943154,-4.04576665580633,
29.5778204922147));
#154351=CARTESIAN_POINT('Ctrl Pts',(5.83076368565356,-3.89777573643299,
29.586049189225));
#154352=CARTESIAN_POINT('Ctrl Pts',(5.92964092982658,-3.74564807526189,
29.5942778862353));
#154353=CARTESIAN_POINT('Ctrl Pts',(6.02250405524087,-3.58985674743537,
29.6025065832456));
#154354=CARTESIAN_POINT('Ctrl Pts',(6.11533308220262,-3.43412262469619,
29.610732258757));
#154355=CARTESIAN_POINT('Ctrl Pts',(6.20215221349858,-3.27472781168244,
29.6189579342683));
#154356=CARTESIAN_POINT('Ctrl Pts',(6.28267476045562,-3.11217358398176,
29.6271836097797));
#154357=CARTESIAN_POINT('Ctrl Pts',(6.3631809559691,-2.94965236562295,29.6354076149307));
#154358=CARTESIAN_POINT('Ctrl Pts',(6.43739296194922,-2.78397332036744,
29.6436316200817));
#154359=CARTESIAN_POINT('Ctrl Pts',(6.50507036382054,-2.61566169912007,
29.6518556252327));
#154360=CARTESIAN_POINT('Ctrl Pts',(6.57274512885284,-2.44735663561043,
29.660079309961));
#154361=CARTESIAN_POINT('Ctrl Pts',(6.63388566909423,-2.27641952117878,
29.6683029946893));
#154362=CARTESIAN_POINT('Ctrl Pts',(6.68829989246451,-2.10339513904528,
29.6765266794176));
#154363=CARTESIAN_POINT('Ctrl Pts',(6.74274013189878,-1.93028803197112,
29.6847542959838));
#154364=CARTESIAN_POINT('Ctrl Pts',(6.79044752185053,-1.75509199202338,
29.69298191255));
#154365=CARTESIAN_POINT('Ctrl Pts',(6.83127976266757,-1.57836731044091,
29.7012095291163));
#154366=CARTESIAN_POINT('Ctrl Pts',(6.87212112187813,-1.40160316383868,
29.7094389830209));
#154367=CARTESIAN_POINT('Ctrl Pts',(6.90608420006113,-1.22331003323168,
29.7176684369256));
#154368=CARTESIAN_POINT('Ctrl Pts',(6.93307788002744,-1.04405827039217,
29.7258978908303));
#154369=CARTESIAN_POINT('Ctrl Pts',(6.96009610059357,-0.86464354548948,
29.7341348263283));
#154370=CARTESIAN_POINT('Ctrl Pts',(6.98013221510365,-0.684268789542715,
29.7423717618262));
#154371=CARTESIAN_POINT('Ctrl Pts',(6.99314691492785,-0.503510465368024,
29.7506086973242));
#154372=CARTESIAN_POINT('Ctrl Pts',(7.00522141267682,-0.335810402528576,
29.7582505838427));
#154373=CARTESIAN_POINT('Ctrl Pts',(7.01125285965042,-0.16778045001463,
29.7658924703612));
#154374=CARTESIAN_POINT('Ctrl Pts',(7.01124999898235,0.000119457236979679,
29.7735343568796));
#154375=CARTESIAN_POINT('Ctrl Pts',(7.01124999898234,0.000119457914987822,
29.7735343569105));
#154376=CARTESIAN_POINT('Ctrl Pts',(7.01124407803179,0.347633178975341,
29.7893512829794));
#154377=CARTESIAN_POINT('Ctrl Pts',(6.98539996000983,0.694636108610281,
29.8051682090482));
#154378=CARTESIAN_POINT('Ctrl Pts',(6.93395267227691,1.0382325852736,29.820985135117));
#154379=CARTESIAN_POINT('Ctrl Pts',(6.90837589769859,1.20904994060521,29.8288484447376));
#154380=CARTESIAN_POINT('Ctrl Pts',(6.87644550131219,1.37917031431264,29.8367117543582));
#154381=CARTESIAN_POINT('Ctrl Pts',(6.83821065173588,1.54806383750348,29.8445750639788));
#154382=CARTESIAN_POINT('Ctrl Pts',(6.80000851446076,1.7168128617395,29.8524316460471));
#154383=CARTESIAN_POINT('Ctrl Pts',(6.75551274019734,1.88433675449325,29.8602882281153));
#154384=CARTESIAN_POINT('Ctrl Pts',(6.70482413161581,2.05011217415103,29.8681448101836));
#154385=CARTESIAN_POINT('Ctrl Pts',(6.66420330613044,2.18296124182378,29.8744409161142));
#154386=CARTESIAN_POINT('Ctrl Pts',(6.61960639339951,2.31468744814057,29.8807370220449));
#154387=CARTESIAN_POINT('Ctrl Pts',(6.57110895151814,2.44502632087637,29.8870331279755));
#154388=CARTESIAN_POINT('',(7.01124997488654,0.000593425250984153,29.2264656431291));
#154389=CARTESIAN_POINT('Ctrl Pts',(6.57110895151813,2.4450263208764,29.3400595704968));
#154390=CARTESIAN_POINT('Ctrl Pts',(6.64399555118415,2.24914058196973,29.3305789610997));
#154391=CARTESIAN_POINT('Ctrl Pts',(6.70803579118306,2.05021802406892,29.3210983517026));
#154392=CARTESIAN_POINT('Ctrl Pts',(6.76304630522514,1.84900817626114,29.3116177423055));
#154393=CARTESIAN_POINT('Ctrl Pts',(6.81821243560133,1.6472291365553,29.3021103137138));
#154394=CARTESIAN_POINT('Ctrl Pts',(6.864297702838,1.44314996512382,29.2926028851222));
#154395=CARTESIAN_POINT('Ctrl Pts',(6.90116951794474,1.23753216002269,29.2830954565305));
#154396=CARTESIAN_POINT('Ctrl Pts',(6.93813914256544,1.03136891452158,29.2735628076733));
#154397=CARTESIAN_POINT('Ctrl Pts',(6.96584637654926,0.823658970759291,
29.264030158816));
#154398=CARTESIAN_POINT('Ctrl Pts',(6.98420988671341,0.615173813515072,
29.2544975099588));
#154399=CARTESIAN_POINT('Ctrl Pts',(7.00220990185979,0.410815498865802,
29.2451535543489));
#154400=CARTESIAN_POINT('Ctrl Pts',(7.01123261381448,0.205712462309202,
29.235809598739));
#154401=CARTESIAN_POINT('Ctrl Pts',(7.01124997488654,0.000593425251026187,
29.2264656431291));
#154402=CARTESIAN_POINT('Ctrl Pts',(7.01124997488661,0.000593424383951388,
29.2264656430896));
#154403=CARTESIAN_POINT('Ctrl Pts',(7.01126957801832,-0.231015623751386,
29.2159149662941));
#154404=CARTESIAN_POINT('Ctrl Pts',(6.9998102786117,-0.46267258523056,29.2053642894985));
#154405=CARTESIAN_POINT('Ctrl Pts',(6.97687299454424,-0.693447748932306,
29.1948136127029));
#154406=CARTESIAN_POINT('Ctrl Pts',(6.95940906759447,-0.869154715321837,
29.186780567104));
#154407=CARTESIAN_POINT('Ctrl Pts',(6.93528503923172,-1.04438501249477,
29.1787475215051));
#154408=CARTESIAN_POINT('Ctrl Pts',(6.90453974263472,-1.21858832461075,
29.1707144759062));
#154409=CARTESIAN_POINT('Ctrl Pts',(6.8738142102982,-1.39267965213017,29.1626865942583));
#154410=CARTESIAN_POINT('Ctrl Pts',(6.83647594565298,-1.56574494922353,
29.1546587126104));
#154411=CARTESIAN_POINT('Ctrl Pts',(6.79261556688361,-1.73723928203066,
29.1466308309625));
#154412=CARTESIAN_POINT('Ctrl Pts',(6.74877499150779,-1.90865618345534,
29.1386065739824));
#154413=CARTESIAN_POINT('Ctrl Pts',(6.69841825607998,-2.07850317850176,
29.1305823170023));
#154414=CARTESIAN_POINT('Ctrl Pts',(6.64168700062609,-2.24624583432321,
29.1225580600221));
#154415=CARTESIAN_POINT('Ctrl Pts',(6.5849626045586,-2.41396820834972,29.1145347732563));
#154416=CARTESIAN_POINT('Ctrl Pts',(6.52186533372496,-2.57958640042939,
29.1065114864905));
#154417=CARTESIAN_POINT('Ctrl Pts',(6.45258665145337,-2.74258127828253,
29.0984881997248));
#154418=CARTESIAN_POINT('Ctrl Pts',(6.3833136459519,-2.90556280015916,29.0904655703958));
#154419=CARTESIAN_POINT('Ctrl Pts',(6.30786038505268,-3.06592110012482,
29.0824429410668));
#154420=CARTESIAN_POINT('Ctrl Pts',(6.22646630163365,-3.2231574514939,29.0744203117378));
#154421=CARTESIAN_POINT('Ctrl Pts',(6.14504161983387,-3.3804529125371,29.0663946664714));
#154422=CARTESIAN_POINT('Ctrl Pts',(6.05767182536901,-3.53462375608389,
29.0583690212049));
#154423=CARTESIAN_POINT('Ctrl Pts',(5.9646422756733,-3.68519593586974,29.0503433759384));
#154424=CARTESIAN_POINT('Ctrl Pts',(5.90978638423711,-3.77398246847858,
29.0456109664311));
#154425=CARTESIAN_POINT('Ctrl Pts',(5.85296344717681,-3.86151824762984,
29.0408785569238));
#154426=CARTESIAN_POINT('Ctrl Pts',(5.79423899333342,-3.94771086208635,
29.0361461474164));
#154427=CARTESIAN_POINT('Ctrl Pts',(5.68590784636769,-4.10671352916862,
29.0274160985818));
#154428=CARTESIAN_POINT('Ctrl Pts',(5.57104950672835,-4.26122332955139,
29.0186860497472));
#154429=CARTESIAN_POINT('Ctrl Pts',(5.45005695877084,-4.41072621102847,
29.0099560009125));
#154430=CARTESIAN_POINT('Ctrl Pts',(5.32902942566769,-4.56027232144957,
29.0012234277734));
#154431=CARTESIAN_POINT('Ctrl Pts',(5.20186431615247,-4.70480841022049,
28.9924908546343));
#154432=CARTESIAN_POINT('Ctrl Pts',(5.06899464155256,-4.84385382587165,
28.9837582814952));
#154433=CARTESIAN_POINT('Ctrl Pts',(4.9342373411241,-4.98487460361137,28.9749016482147));
#154434=CARTESIAN_POINT('Ctrl Pts',(4.79361235562339,-5.12024730212231,
28.9660450149343));
#154435=CARTESIAN_POINT('Ctrl Pts',(4.64761012012673,-5.24950918980009,
28.9571883816539));
#154436=CARTESIAN_POINT('Ctrl Pts',(4.50356138498687,-5.37704156187942,
28.9484502495472));
#154437=CARTESIAN_POINT('Ctrl Pts',(4.35427862404699,-5.49862546531161,
28.9397121174405));
#154438=CARTESIAN_POINT('Ctrl Pts',(4.20026693293569,-5.61385645119173,
28.9309739853338));
#154439=CARTESIAN_POINT('Ctrl Pts',(4.04312232406658,-5.73143147471801,
28.9220581014665));
#154440=CARTESIAN_POINT('Ctrl Pts',(3.88105456659959,-5.84239216861101,
28.9131422175992));
#154441=CARTESIAN_POINT('Ctrl Pts',(3.71463300634061,-5.94635419317626,
28.9042263337319));
#154442=CARTESIAN_POINT('Ctrl Pts',(3.54821144608166,-6.0503162177415,28.8953104498646));
#154443=CARTESIAN_POINT('Ctrl Pts',(3.37743634273424,-6.14727941791697,
28.8863945659973));
#154444=CARTESIAN_POINT('Ctrl Pts',(3.20290638631692,-6.23690766670393,
28.87747868213));
#154445=CARTESIAN_POINT('Ctrl Pts',(3.03180598764778,-6.32477469775273,
28.8687379976338));
#154446=CARTESIAN_POINT('Ctrl Pts',(2.85707876118365,-6.40560170126986,
28.8599973131376));
#154447=CARTESIAN_POINT('Ctrl Pts',(2.67931053116122,-6.4791142635478,28.8512566286414));
#154448=CARTESIAN_POINT('Ctrl Pts',(2.50157428459663,-6.55261359969453,
28.8425175167395));
#154449=CARTESIAN_POINT('Ctrl Pts',(2.32079838005193,-6.61880101814192,
28.8337784048377));
#154450=CARTESIAN_POINT('Ctrl Pts',(2.13758879097322,-6.67745016628396,
28.8250392929358));
#154451=CARTESIAN_POINT('Ctrl Pts',(1.95200545798299,-6.73685919855116,
28.8161869532615));
#154452=CARTESIAN_POINT('Ctrl Pts',(1.76392520166172,-6.7885331522239,28.8073346135871));
#154453=CARTESIAN_POINT('Ctrl Pts',(1.57399524887777,-6.8322884540255,28.7984822739128));
#154454=CARTESIAN_POINT('Ctrl Pts',(1.38659074026424,-6.87546195411422,
28.789747641263));
#154455=CARTESIAN_POINT('Ctrl Pts',(1.19738569637837,-6.91092602912531,
28.7810130086133));
#154456=CARTESIAN_POINT('Ctrl Pts',(1.00701460402804,-6.93855519180861,
28.7722783759635));
#154457=CARTESIAN_POINT('Ctrl Pts',(0.81279537934934,-6.96674284618735,
28.7633671827769));
#154458=CARTESIAN_POINT('Ctrl Pts',(0.617362747733219,-6.98677540412211,
28.7544559895902));
#154459=CARTESIAN_POINT('Ctrl Pts',(0.421399684115591,-6.99857477410417,
28.7455447964036));
#154460=CARTESIAN_POINT('Ctrl Pts',(0.225436620497963,-7.01037414408624,
28.7366336032169));
#154461=CARTESIAN_POINT('Ctrl Pts',(0.028943426650755,-7.01394029444683,
28.7277224100303));
#154462=CARTESIAN_POINT('Ctrl Pts',(-0.167392073522051,-7.00925149043905,
28.7188112168436));
#154463=CARTESIAN_POINT('Ctrl Pts',(-0.34421720681354,-7.00502862502284,
28.7107855519912));
#154464=CARTESIAN_POINT('Ctrl Pts',(-0.520995680481737,-6.99410746015789,
28.7027598871388));
#154465=CARTESIAN_POINT('Ctrl Pts',(-0.697174942039755,-6.97650153462979,
28.6947342222864));
#154466=CARTESIAN_POINT('Ctrl Pts',(-0.873298288621336,-6.95890119679064,
28.6867111045832));
#154467=CARTESIAN_POINT('Ctrl Pts',(-1.04882243739377,-6.9346203585602,
28.67868798688));
#154468=CARTESIAN_POINT('Ctrl Pts',(-1.22319820765172,-6.90372455326092,
28.6706648691767));
#154469=CARTESIAN_POINT('Ctrl Pts',(-1.39755198759884,-6.8728326441931,
28.6626427632589));
#154470=CARTESIAN_POINT('Ctrl Pts',(-1.57075731675442,-6.83532749421448,
28.654620657341));
#154471=CARTESIAN_POINT('Ctrl Pts',(-1.74227353068216,-6.79132604921781,
28.6465985514231));
#154472=CARTESIAN_POINT('Ctrl Pts',(-1.91385348061453,-6.7473082531355,
28.6385734644636));
#154473=CARTESIAN_POINT('Ctrl Pts',(-2.08374270526097,-6.69678942780656,
28.6305483775041));
#154474=CARTESIAN_POINT('Ctrl Pts',(-2.2514136324211,-6.63993698902696,
28.6225232905446));
#154475=CARTESIAN_POINT('Ctrl Pts',(-2.41911758153125,-6.58307335344406,
28.6144966230843));
#154476=CARTESIAN_POINT('Ctrl Pts',(-2.58460201849207,-6.51987374548824,
28.6064699556241));
#154477=CARTESIAN_POINT('Ctrl Pts',(-2.74735797780886,-6.45055429434324,
28.5984432881638));
#154478=CARTESIAN_POINT('Ctrl Pts',(-2.91024459703649,-6.38117919378703,
28.5904101769232));
#154479=CARTESIAN_POINT('Ctrl Pts',(-3.07039803027066,-6.30567458973652,
28.5823770656826));
#154480=CARTESIAN_POINT('Ctrl Pts',(-3.22733204274069,-6.2243035311912,
28.574343954442));
#154481=CARTESIAN_POINT('Ctrl Pts',(-3.31980326382667,-6.17635674753153,
28.5696105534804));
#154482=CARTESIAN_POINT('Ctrl Pts',(-3.41115718156983,-6.12637399944188,
28.5648771525187));
#154483=CARTESIAN_POINT('Ctrl Pts',(-3.50129888771244,-6.07441624038093,
28.5601437515571));
#154484=CARTESIAN_POINT('Ctrl Pts',(-3.68699360776096,-5.96738163968337,
28.550392798263));
#154485=CARTESIAN_POINT('Ctrl Pts',(-3.86765228366181,-5.85190080475005,
28.5406418449689));
#154486=CARTESIAN_POINT('Ctrl Pts',(-4.04260209639738,-5.72843738315289,
28.5308908916748));
#154487=CARTESIAN_POINT('Ctrl Pts',(-4.21780395715782,-5.60479608933586,
28.5211258903033));
#154488=CARTESIAN_POINT('Ctrl Pts',(-4.38728047139096,-5.47314922691908,
28.5113608889317));
#154489=CARTESIAN_POINT('Ctrl Pts',(-4.55038851875762,-5.33400327060819,
28.5015958875602));
#154490=CARTESIAN_POINT('Ctrl Pts',(-4.71322469880496,-5.19508924177572,
28.4918471624226));
#154491=CARTESIAN_POINT('Ctrl Pts',(-4.86971359804892,-5.04870112494837,
28.4820984372851));
#154492=CARTESIAN_POINT('Ctrl Pts',(-5.01924811634967,-4.89538301964415,
28.4723497121475));
#154493=CARTESIAN_POINT('Ctrl Pts',(-5.16837222038109,-4.74248571308847,
28.4626277434803));
#154494=CARTESIAN_POINT('Ctrl Pts',(-5.31058001982027,-4.58269641722677,
28.4529057748131));
#154495=CARTESIAN_POINT('Ctrl Pts',(-5.44530257865017,-4.41659443343464,
28.4431838061459));
#154496=CARTESIAN_POINT('Ctrl Pts',(-5.57913371349427,-4.2515915030878,
28.4335261652063));
#154497=CARTESIAN_POINT('Ctrl Pts',(-5.70557828425975,-4.0803591655633,
28.4238685242666));
#154498=CARTESIAN_POINT('Ctrl Pts',(-5.82411204843313,-3.90350424744178,
28.414210883327));
#154499=CARTESIAN_POINT('Ctrl Pts',(-5.87621171865758,-3.82577042218146,
28.4099660176416));
#154500=CARTESIAN_POINT('Ctrl Pts',(-5.92678353746462,-3.74695087422018,
28.4057211519561));
#154501=CARTESIAN_POINT('Ctrl Pts',(-5.97578510504653,-3.66709952698369,
28.4014762862707));
#154502=CARTESIAN_POINT('Ctrl Pts',(-6.06642467779386,-3.51939625229324,
28.3936244392568));
#154503=CARTESIAN_POINT('Ctrl Pts',(-6.15165117836221,-3.36822136137917,
28.3857725922429));
#154504=CARTESIAN_POINT('Ctrl Pts',(-6.23118342980562,-3.21402856655256,
28.377920745229));
#154505=CARTESIAN_POINT('Ctrl Pts',(-6.31069312654532,-3.05987949955634,
28.3700711249354));
#154506=CARTESIAN_POINT('Ctrl Pts',(-6.38451161166455,-2.90271456977397,
28.3622215046419));
#154507=CARTESIAN_POINT('Ctrl Pts',(-6.45240311453528,-2.74301305320179,
28.3543718843483));
#154508=CARTESIAN_POINT('Ctrl Pts',(-6.5202891971378,-2.58332428675323,
28.3465228907465));
#154509=CARTESIAN_POINT('Ctrl Pts',(-6.58224909094005,-2.42109968801649,
28.3386738971447));
#154510=CARTESIAN_POINT('Ctrl Pts',(-6.63809483719985,-2.25683927093638,
28.330824903543));
#154511=CARTESIAN_POINT('Ctrl Pts',(-6.69396885652599,-2.09249569361617,
28.3229719362255));
#154512=CARTESIAN_POINT('Ctrl Pts',(-6.74372242056868,-1.92611460024439,
28.3151189689081));
#154513=CARTESIAN_POINT('Ctrl Pts',(-6.78721711244265,-1.75821228270811,
28.3072660015906));
#154514=CARTESIAN_POINT('Ctrl Pts',(-6.83072285050694,-1.59026732362469,
28.2994110398834));
#154515=CARTESIAN_POINT('Ctrl Pts',(-6.86796646777074,-1.42080074331452,
28.2915560781761));
#154516=CARTESIAN_POINT('Ctrl Pts',(-6.89886066458123,-1.25033919125723,
28.2837011164688));
#154517=CARTESIAN_POINT('Ctrl Pts',(-6.92978552646445,-1.07970844186098,
28.2758383580555));
#154518=CARTESIAN_POINT('Ctrl Pts',(-6.95434832651521,-0.908081125695903,
28.2679755996421));
#154519=CARTESIAN_POINT('Ctrl Pts',(-6.97251358096026,-0.735989759320567,
28.2601128412287));
#154520=CARTESIAN_POINT('Ctrl Pts',(-6.98583935096519,-0.609746002312418,
28.2543448344806));
#154521=CARTESIAN_POINT('Ctrl Pts',(-6.99572338168541,-0.483252631113423,
28.2485768277325));
#154522=CARTESIAN_POINT('Ctrl Pts',(-7.00216950191021,-0.356719538319117,
28.2428088209843));
#154523=CARTESIAN_POINT('Ctrl Pts',(-7.01153253248354,-0.172929417276127,
28.2344307545433));
#154524=CARTESIAN_POINT('Ctrl Pts',(-7.01366137701737,0.011351591344907,
28.2260526881023));
#154525=CARTESIAN_POINT('Ctrl Pts',(-7.008522986763,0.195530321215718,28.2176746216613));
#154526=CARTESIAN_POINT('Ctrl Pts',(-7.00338811007882,0.37958311185948,
28.2093022840425));
#154527=CARTESIAN_POINT('Ctrl Pts',(-6.99099591495653,0.563533435637692,
28.2009299464238));
#154528=CARTESIAN_POINT('Ctrl Pts',(-6.97136540613618,0.746787075830669,
28.1925576088051));
#154529=CARTESIAN_POINT('Ctrl Pts',(-6.95174544159739,0.929942283629653,
28.1841897682825));
#154530=CARTESIAN_POINT('Ctrl Pts',(-6.92489495053835,1.11240122786889,
28.1758219277599));
#154531=CARTESIAN_POINT('Ctrl Pts',(-6.89088489724653,1.29357330499653,
28.1674540872373));
#154532=CARTESIAN_POINT('Ctrl Pts',(-6.85688812980253,1.4746746082085,28.1590895155674));
#154533=CARTESIAN_POINT('Ctrl Pts',(-6.81573743799202,1.65448972418672,
28.1507249438975));
#154534=CARTESIAN_POINT('Ctrl Pts',(-6.76755522877617,1.8324362984738,28.1423603722277));
#154535=CARTESIAN_POINT('Ctrl Pts',(-6.71938478897285,2.01033940595693,
28.133997843762));
#154536=CARTESIAN_POINT('Ctrl Pts',(-6.66418634327921,2.18637456510496,
28.1256353152964));
#154537=CARTESIAN_POINT('Ctrl Pts',(-6.60213280590384,2.3599722404529,28.1172727868308));
#154538=CARTESIAN_POINT('Ctrl Pts',(-6.54007431646243,2.5335837694374,28.1089095910093));
#154539=CARTESIAN_POINT('Ctrl Pts',(-6.471159747336,2.70475711447586,28.1005463951878));
#154540=CARTESIAN_POINT('Ctrl Pts',(-6.39561129658887,2.87293973230293,
28.0921831993663));
#154541=CARTESIAN_POINT('Ctrl Pts',(-6.32005769358875,3.04113381984761,
28.0838194331916));
#154542=CARTESIAN_POINT('Ctrl Pts',(-6.23786944137973,3.20633647343993,
28.0754556670168));
#154543=CARTESIAN_POINT('Ctrl Pts',(-6.14931620338209,3.36801674481029,
28.0670919008421));
#154544=CARTESIAN_POINT('Ctrl Pts',(-6.06074512000138,3.5297295982346,28.0587264491886));
#154545=CARTESIAN_POINT('Ctrl Pts',(-5.96580665108505,3.68791836564707,
28.050360997535));
#154546=CARTESIAN_POINT('Ctrl Pts',(-5.86481578643275,3.84207786929276,
28.0419955458814));
#154547=CARTESIAN_POINT('Ctrl Pts',(-5.7637911001383,3.99628900065335,28.0336272926545));
#154548=CARTESIAN_POINT('Ctrl Pts',(-5.65671015643922,4.14646790260694,
28.0252590394276));
#154549=CARTESIAN_POINT('Ctrl Pts',(-5.54393075874577,4.2921391292376,28.0168907862007));
#154550=CARTESIAN_POINT('Ctrl Pts',(-5.4310467984613,4.43794541387715,28.0085147744092));
#154551=CARTESIAN_POINT('Ctrl Pts',(-5.31245402809585,4.57923541154522,
28.0001387626178));
#154552=CARTESIAN_POINT('Ctrl Pts',(-5.18855075561073,4.71556652152754,
27.9917627508263));
#154553=CARTESIAN_POINT('Ctrl Pts',(-5.06458671942991,4.85196448997062,
27.9833826313352));
#154554=CARTESIAN_POINT('Ctrl Pts',(-4.93530721340992,4.98339848229445,
27.975002511844));
#154555=CARTESIAN_POINT('Ctrl Pts',(-4.80114721922023,5.10946297979287,
27.9666223923529));
#154556=CARTESIAN_POINT('Ctrl Pts',(-4.66683393024254,5.23567152194885,
27.9582326975136));
#154557=CARTESIAN_POINT('Ctrl Pts',(-4.5276292540479,5.35649808919911,27.9498430026744));
#154558=CARTESIAN_POINT('Ctrl Pts',(-4.38400205492107,5.47157678781426,
27.9414533078352));
#154559=CARTESIAN_POINT('Ctrl Pts',(-4.29281562473338,5.54463826768128,
27.9361268353606));
#154560=CARTESIAN_POINT('Ctrl Pts',(-4.19984721973464,5.61538375356261,
27.930800362886));
#154561=CARTESIAN_POINT('Ctrl Pts',(-4.10522283754282,5.68372870716196,
27.9254738904114));
#154562=CARTESIAN_POINT('Ctrl Pts',(-3.95632966733273,5.79127072300983,
27.9170925900065));
#154563=CARTESIAN_POINT('Ctrl Pts',(-3.80303460730463,5.89308390277139,
27.9087112896016));
#154564=CARTESIAN_POINT('Ctrl Pts',(-3.64580334336836,5.98880159497575,
27.9003299891967));
#154565=CARTESIAN_POINT('Ctrl Pts',(-3.48877134704259,6.08439797901702,
27.8919593108632));
#154566=CARTESIAN_POINT('Ctrl Pts',(-3.32781336609644,6.17391410190386,
27.8835886325296));
#154567=CARTESIAN_POINT('Ctrl Pts',(-3.16342614885495,6.25702497703507,
27.8752179541961));
#154568=CARTESIAN_POINT('Ctrl Pts',(-2.99922548288099,6.34004153559252,
27.8668567751452));
#154569=CARTESIAN_POINT('Ctrl Pts',(-2.83160362761403,6.41666718708988,
27.8584955960944));
#154570=CARTESIAN_POINT('Ctrl Pts',(-2.661084547777,6.48662127706578,27.8501344170436));
#154571=CARTESIAN_POINT('Ctrl Pts',(-2.49078673655989,6.5564845933584,27.8417840876088));
#154572=CARTESIAN_POINT('Ctrl Pts',(-2.3175995011781,6.619693491938,27.8334337581741));
#154573=CARTESIAN_POINT('Ctrl Pts',(-2.14206945953442,6.67601415464572,
27.8250834287393));
#154574=CARTESIAN_POINT('Ctrl Pts',(-1.96667447775937,6.732291481972,27.8167395243836));
#154575=CARTESIAN_POINT('Ctrl Pts',(-1.78894059273396,6.78169103585329,
27.8083956200279));
#154576=CARTESIAN_POINT('Ctrl Pts',(-1.60943344470827,6.82402744349365,
27.8000517156722));
#154577=CARTESIAN_POINT('Ctrl Pts',(-1.43007047794205,6.86632984626767,
27.7917145131925));
#154578=CARTESIAN_POINT('Ctrl Pts',(-1.24893740670868,6.9015803421214,27.7833773107128));
#154579=CARTESIAN_POINT('Ctrl Pts',(-1.06661419244611,6.92964362193126,
27.775040108233));
#154580=CARTESIAN_POINT('Ctrl Pts',(-1.0065943967124,6.93888189873884,27.772295547197));
#154581=CARTESIAN_POINT('Ctrl Pts',(-0.946445732511336,6.94734171020539,
27.769550986161));
#154582=CARTESIAN_POINT('Ctrl Pts',(-0.886189172523352,6.95501943297087,
27.766806425125));
#154583=CARTESIAN_POINT('Ctrl Pts',(-0.703122413097995,6.97834528872371,
27.7584681148231));
#154584=CARTESIAN_POINT('Ctrl Pts',(-0.519209392208376,6.99442936365961,
27.7501298045212));
#154585=CARTESIAN_POINT('Ctrl Pts',(-0.335045536708833,7.00324003949825,
27.7417914942192));
#154586=CARTESIAN_POINT('Ctrl Pts',(-0.150765811561441,7.01205625871512,
27.7334479377355));
#154587=CARTESIAN_POINT('Ctrl Pts',(0.0337647357046807,7.01358993542549,
27.7251043812517));
#154588=CARTESIAN_POINT('Ctrl Pts',(0.217950683148152,7.00786158983004,
27.7167608247679));
#154589=CARTESIAN_POINT('Ctrl Pts',(0.402276758457761,7.00212888613423,
27.7084109205427));
#154590=CARTESIAN_POINT('Ctrl Pts',(0.586257383878938,6.98912314990432,
27.7000610163175));
#154591=CARTESIAN_POINT('Ctrl Pts',(0.769301819297712,6.96891679339948,
27.6917111120923));
#154592=CARTESIAN_POINT('Ctrl Pts',(0.952620807823779,6.94868012885521,
27.6833486836287));
#154593=CARTESIAN_POINT('Ctrl Pts',(1.13500047432767,6.92122129742725,27.674986255165));
#154594=CARTESIAN_POINT('Ctrl Pts',(1.31585833882374,6.8866641703112,27.6666238267014));
#154595=CARTESIAN_POINT('Ctrl Pts',(1.4968708614489,6.85207749214056,27.6582542472215));
#154596=CARTESIAN_POINT('Ctrl Pts',(1.67635866714702,6.81038048100691,27.6498846677415));
#154597=CARTESIAN_POINT('Ctrl Pts',(1.85375346569482,6.76174715964184,27.6415150882616));
#154598=CARTESIAN_POINT('Ctrl Pts',(2.03142187410601,6.71303882730393,27.633132599725));
#154599=CARTESIAN_POINT('Ctrl Pts',(2.20699051272182,6.65737290494878,27.6247501111885));
#154600=CARTESIAN_POINT('Ctrl Pts',(2.37990879091184,6.59497238124926,27.6163676226519));
#154601=CARTESIAN_POINT('Ctrl Pts',(2.43649048497056,6.57455390740123,27.6136247350475));
#154602=CARTESIAN_POINT('Ctrl Pts',(2.49278858441337,6.55341473033929,27.6108818474431));
#154603=CARTESIAN_POINT('Ctrl Pts',(2.54878435310499,6.53156373955481,27.6081389598386));
#154604=CARTESIAN_POINT('Ctrl Pts',(2.72007692581268,6.46472096705356,27.5997483923835));
#154605=CARTESIAN_POINT('Ctrl Pts',(2.88888454541639,6.3910788444342,27.5913578249283));
#154606=CARTESIAN_POINT('Ctrl Pts',(3.0546504413274,6.31084283149235,27.5829672574732));
#154607=CARTESIAN_POINT('Ctrl Pts',(3.22026085090869,6.23068207892354,27.574584560265));
#154608=CARTESIAN_POINT('Ctrl Pts',(3.38283493013489,6.14393990895742,27.5662018630568));
#154609=CARTESIAN_POINT('Ctrl Pts',(3.54183554505036,6.05086998160742,27.5578191658486));
#154610=CARTESIAN_POINT('Ctrl Pts',(3.70071039710015,5.95787366869457,27.5494430990048));
#154611=CARTESIAN_POINT('Ctrl Pts',(3.85601713748993,5.85855974291226,27.541067032161));
#154612=CARTESIAN_POINT('Ctrl Pts',(4.00724251775276,5.75322813439677,27.5326909653173));
#154613=CARTESIAN_POINT('Ctrl Pts',(4.15835538266826,5.64797489515037,27.5243211304702));
#154614=CARTESIAN_POINT('Ctrl Pts',(4.30539267594718,5.53671309200644,27.5159512956232));
#154615=CARTESIAN_POINT('Ctrl Pts',(4.44786923437015,5.41978651207255,27.5075814607761));
#154616=CARTESIAN_POINT('Ctrl Pts',(4.59028295293201,5.30291150307864,27.4992153174785));
#154617=CARTESIAN_POINT('Ctrl Pts',(4.72813969320088,5.18037690635018,27.4908491741808));
#154618=CARTESIAN_POINT('Ctrl Pts',(4.86098597337318,5.05256785497921,27.4824830308832));
#154619=CARTESIAN_POINT('Ctrl Pts',(4.99379138380543,4.9247981236607,27.4741194614032));
#154620=CARTESIAN_POINT('Ctrl Pts',(5.12158917111287,4.79175740083689,27.4657558919233));
#154621=CARTESIAN_POINT('Ctrl Pts',(5.24396113443014,4.65386916265231,27.4573923224433));
#154622=CARTESIAN_POINT('Ctrl Pts',(5.36631176667809,4.51600496023122,27.4490302108453));
#154623=CARTESIAN_POINT('Ctrl Pts',(5.48323824341888,4.37329517355471,27.4406680992473));
#154624=CARTESIAN_POINT('Ctrl Pts',(5.59436095381705,4.22619830118124,27.4323059876494));
#154625=CARTESIAN_POINT('Ctrl Pts',(5.70550116287917,4.07907826523726,27.4239425592568));
#154626=CARTESIAN_POINT('Ctrl Pts',(5.81083557781614,3.92757002288179,27.4155791308643));
#154627=CARTESIAN_POINT('Ctrl Pts',(5.91002597127305,3.77216377976593,27.4072157024717));
#154628=CARTESIAN_POINT('Ctrl Pts',(6.00922162718179,3.61674929171991,27.3988518303654));
#154629=CARTESIAN_POINT('Ctrl Pts',(6.10227243811671,3.45743666978052,27.3904879582592));
#154630=CARTESIAN_POINT('Ctrl Pts',(6.18888447304698,3.29474362307266,27.3821240861529));
#154631=CARTESIAN_POINT('Ctrl Pts',(6.27553806438576,3.13197251632713,27.3737562010652));
#154632=CARTESIAN_POINT('Ctrl Pts',(6.35574655392168,2.965818035204,27.3653883159775));
#154633=CARTESIAN_POINT('Ctrl Pts',(6.42926236551352,2.7968217672729,27.3570204308899));
#154634=CARTESIAN_POINT('Ctrl Pts',(6.4797184276934,2.68083466166572,27.3512773054158));
#154635=CARTESIAN_POINT('Ctrl Pts',(6.52702289263795,2.56350942008527,27.3455341799418));
#154636=CARTESIAN_POINT('Ctrl Pts',(6.57110895151815,2.44502632087633,27.3397910544677));
#154637=CARTESIAN_POINT('Origin',(0.,0.,50.));
#154638=CARTESIAN_POINT('',(6.57110895151814,2.44502632087636,25.3397663899914));
#154639=CARTESIAN_POINT('',(6.57110895151813,2.4450263208764,25.8869210003222));
#154640=CARTESIAN_POINT('',(6.57110895151814,2.44502632087636,50.));
#154641=CARTESIAN_POINT('',(7.01125,3.98146142790989E-12,27.7735343569105));
#154642=CARTESIAN_POINT('Ctrl Pts',(6.57110895151813,2.4450263208764,25.8869210003222));
#154643=CARTESIAN_POINT('Ctrl Pts',(6.50449838733137,2.62404495591359,25.895592809261));
#154644=CARTESIAN_POINT('Ctrl Pts',(6.43056821795849,2.8003399071602,25.9042646181997));
#154645=CARTESIAN_POINT('Ctrl Pts',(6.3495651145922,2.97332295892218,25.9129364271385));
#154646=CARTESIAN_POINT('Ctrl Pts',(6.26856213015488,3.14630575670998,25.9216082233453));
#154647=CARTESIAN_POINT('Ctrl Pts',(6.18048635294261,3.31597640754702,25.9302800195521));
#154648=CARTESIAN_POINT('Ctrl Pts',(6.08563165071554,3.48176879966337,25.9389518157589));
#154649=CARTESIAN_POINT('Ctrl Pts',(5.99077708581931,3.64756095174514,25.9476235994107));
#154650=CARTESIAN_POINT('Ctrl Pts',(5.88914375658037,3.80947460983848,25.9562953830625));
#154651=CARTESIAN_POINT('Ctrl Pts',(5.78107076500122,3.9669695452005,25.9649671667142));
#154652=CARTESIAN_POINT('Ctrl Pts',(5.67299792768767,4.12446425575102,25.9736389379877));
#154653=CARTESIAN_POINT('Ctrl Pts',(5.55848560711277,4.27754002202627,25.9823107092612));
#154654=CARTESIAN_POINT('Ctrl Pts',(5.43791587524801,4.42568610457471,25.9909824805347));
#154655=CARTESIAN_POINT('Ctrl Pts',(5.3173463130282,4.57383197867751,25.9996542396067));
#154656=CARTESIAN_POINT('Ctrl Pts',(5.19071953583764,4.71704796266913,26.0083259986788));
#154657=CARTESIAN_POINT('Ctrl Pts',(5.05845803451533,4.85485621574392,26.0169977577508));
#154658=CARTESIAN_POINT('Ctrl Pts',(4.92619671659181,4.99266427772857,26.0256695047983));
#154659=CARTESIAN_POINT('Ctrl Pts',(4.78830088681791,5.12506441890887,26.0343412518458));
#154660=CARTESIAN_POINT('Ctrl Pts',(4.64523063400501,5.25161488681352,26.0430129988932));
#154661=CARTESIAN_POINT('Ctrl Pts',(4.49652806262435,5.38314733060852,26.0520261309662));
#154662=CARTESIAN_POINT('Ctrl Pts',(4.34223563524006,5.50835996364229,26.0610392630392));
#154663=CARTESIAN_POINT('Ctrl Pts',(4.18290943344607,5.62680151010216,26.0700523951122));
#154664=CARTESIAN_POINT('Ctrl Pts',(4.02607270355511,5.74339240739859,26.0789246969966));
#154665=CARTESIAN_POINT('Ctrl Pts',(3.86435862820459,5.85342208902587,26.087796998881));
#154666=CARTESIAN_POINT('Ctrl Pts',(3.69833198496527,5.95650628233387,26.0966693007653));
#154667=CARTESIAN_POINT('Ctrl Pts',(3.53489950802656,6.05797978512143,26.1054029729328));
#154668=CARTESIAN_POINT('Ctrl Pts',(3.36728850947157,6.15272311279868,26.1141366451002));
#154669=CARTESIAN_POINT('Ctrl Pts',(3.19606623001045,6.24041562845671,26.1228703172676));
#154670=CARTESIAN_POINT('Ctrl Pts',(3.02603797481171,6.32749661743928,26.1315430848816));
#154671=CARTESIAN_POINT('Ctrl Pts',(2.85244891335412,6.40762471321573,26.1402158524956));
#154672=CARTESIAN_POINT('Ctrl Pts',(2.67587836095206,6.48053250588935,26.1488886201096));
#154673=CARTESIAN_POINT('Ctrl Pts',(2.49930871513515,6.55343992422466,26.1575613431941));
#154674=CARTESIAN_POINT('Ctrl Pts',(2.31975787165042,6.61912700519397,26.1662340662785));
#154675=CARTESIAN_POINT('Ctrl Pts',(2.13782503580156,6.67737453486024,26.174906789363));
#154676=CARTESIAN_POINT('Ctrl Pts',(1.95589311921898,6.73562177021466,26.1835794686261));
#154677=CARTESIAN_POINT('Ctrl Pts',(1.77157950497104,6.78642944284875,26.1922521478892));
#154678=CARTESIAN_POINT('Ctrl Pts',(1.5854992866886,6.82962799678064,26.2009248271524));
#154679=CARTESIAN_POINT('Ctrl Pts',(1.39941999343939,6.87282633596591,26.2095974633023));
#154680=CARTESIAN_POINT('Ctrl Pts',(1.21157439050707,6.90841556788906,26.2182700994522));
#154681=CARTESIAN_POINT('Ctrl Pts',(1.02258935229166,6.93627692491294,26.2269427356021));
#154682=CARTESIAN_POINT('Ctrl Pts',(0.833605238124551,6.96413814570784,
26.2356153293469));
#154683=CARTESIAN_POINT('Ctrl Pts',(0.643481980915828,6.98427152577621,
26.2442879230917));
#154684=CARTESIAN_POINT('Ctrl Pts',(0.452854049807141,6.99660987708142,
26.2529605168364));
#154685=CARTESIAN_POINT('Ctrl Pts',(0.262227035220992,7.00894816906491,
26.2616330688842));
#154686=CARTESIAN_POINT('Ctrl Pts',(0.0710956351212699,7.01349148893088,
26.2703056209319));
#154687=CARTESIAN_POINT('Ctrl Pts',(-0.11990232315709,7.01022467510147,
26.2789781729796));
#154688=CARTESIAN_POINT('Ctrl Pts',(-0.31089937872256,7.006957876712,26.2876506840382));
#154689=CARTESIAN_POINT('Ctrl Pts',(-0.501762709652909,6.99588102335283,
26.2963231950969));
#154690=CARTESIAN_POINT('Ctrl Pts',(-0.691855389205306,6.97703107940101,
26.3049957061555));
#154691=CARTESIAN_POINT('Ctrl Pts',(-0.881947185837381,6.95818122300121,
26.3136681769331));
#154692=CARTESIAN_POINT('Ctrl Pts',(-1.0712680555302,6.93155837629127,26.3223406477107));
#154693=CARTESIAN_POINT('Ctrl Pts',(-1.25918622472477,6.89725138109112,
26.3310131184883));
#154694=CARTESIAN_POINT('Ctrl Pts',(-1.44710353643495,6.86294454243631,
26.3396855496928));
#154695=CARTESIAN_POINT('Ctrl Pts',(-1.63361788097034,6.8209536764805,26.3483579808972));
#154696=CARTESIAN_POINT('Ctrl Pts',(-1.81810685596641,6.77141890764321,
26.3570304121017));
#154697=CARTESIAN_POINT('Ctrl Pts',(-2.0025950041816,6.72188436079425,26.365702804441));
#154698=CARTESIAN_POINT('Ctrl Pts',(-2.18505752664097,6.6648060523869,26.3743751967802));
#154699=CARTESIAN_POINT('Ctrl Pts',(-2.36488554744894,6.60037445225399,
26.3830475891195));
#154700=CARTESIAN_POINT('Ctrl Pts',(-2.54471277703887,6.53594313561107,
26.3917199433015));
#154701=CARTESIAN_POINT('Ctrl Pts',(-2.72190526072999,6.46415868780901,
26.4003922974834));
#154702=CARTESIAN_POINT('Ctrl Pts',(-2.89587171389957,6.38526065083771,
26.4090646516654));
#154703=CARTESIAN_POINT('Ctrl Pts',(-3.06983741583694,6.30636295456856,
26.4177369683979));
#154704=CARTESIAN_POINT('Ctrl Pts',(-3.24057685640863,6.22035184793722,
26.4264092851304));
#154705=CARTESIAN_POINT('Ctrl Pts',(-3.40752028946867,6.12751434428018,
26.4350816018629));
#154706=CARTESIAN_POINT('Ctrl Pts',(-3.57446301524634,6.03467723394397,
26.4437538818537));
#154707=CARTESIAN_POINT('Ctrl Pts',(-3.73760951742251,5.93501392252102,
26.4524261618445));
#154708=CARTESIAN_POINT('Ctrl Pts',(-3.89641539158944,5.82885697703117,
26.4610984418354));
#154709=CARTESIAN_POINT('Ctrl Pts',(-4.05522060590818,5.72270047262997,
26.4697706857924));
#154710=CARTESIAN_POINT('Ctrl Pts',(-4.20968499214218,5.61005054602491,
26.4784429297494));
#154711=CARTESIAN_POINT('Ctrl Pts',(-4.35929312156039,5.49128309621862,
26.4871151737063));
#154712=CARTESIAN_POINT('Ctrl Pts',(-4.50890064155473,5.37251613020767,
26.4957873823372));
#154713=CARTESIAN_POINT('Ctrl Pts',(-4.65365172183414,5.24763186748313,
26.5044595909681));
#154714=CARTESIAN_POINT('Ctrl Pts',(-4.79306334971054,5.1170470281366,26.513131799599));
#154715=CARTESIAN_POINT('Ctrl Pts',(-4.93247442107311,4.98646271006846,
26.5218039736115));
#154716=CARTESIAN_POINT('Ctrl Pts',(-5.06654587536718,4.85017805510722,
26.530476147624));
#154717=CARTESIAN_POINT('Ctrl Pts',(-5.19483033978618,4.70864782111988,
26.5391483216365));
#154718=CARTESIAN_POINT('Ctrl Pts',(-5.32311430257632,4.56711814055615,
26.5478204617383));
#154719=CARTESIAN_POINT('Ctrl Pts',(-5.44561113000617,4.42034313247767,
26.5564926018402));
#154720=CARTESIAN_POINT('Ctrl Pts',(-5.56191207495191,4.26881255538401,
26.565164741942));
#154721=CARTESIAN_POINT('Ctrl Pts',(-5.6782125746164,4.11728255845523,26.5738368488408));
#154722=CARTESIAN_POINT('Ctrl Pts',(-5.78831706632251,3.96099725427966,
26.5825089557396));
#154723=CARTESIAN_POINT('Ctrl Pts',(-5.89185815647341,3.80047813130109,
26.5911810626385));
#154724=CARTESIAN_POINT('Ctrl Pts',(-5.99539885864402,3.63995960980598,
26.5998531370419));
#154725=CARTESIAN_POINT('Ctrl Pts',(-6.09237605450623,3.47520753995039,
26.6085252114454));
#154726=CARTESIAN_POINT('Ctrl Pts',(-6.18246615568043,3.30677165772994,
26.6171972858488));
#154727=CARTESIAN_POINT('Ctrl Pts',(-6.2725559266266,3.13833639291638,26.6258693284645));
#154728=CARTESIAN_POINT('Ctrl Pts',(-6.3557585194383,2.96621759322364,26.6345413710802));
#154729=CARTESIAN_POINT('Ctrl Pts',(-6.43179631013632,2.79098957135581,
26.6432134136959));
#154730=CARTESIAN_POINT('Ctrl Pts',(-6.50783382831866,2.61576217749653,
26.6518854252314));
#154731=CARTESIAN_POINT('Ctrl Pts',(-6.57670648270564,2.43742584432176,
26.6605574367669));
#154732=CARTESIAN_POINT('Ctrl Pts',(-6.63818446599434,2.25657562645958,
26.6692294483025));
#154733=CARTESIAN_POINT('Ctrl Pts',(-6.69966223396433,2.07572604200197,
26.6779014294654));
#154734=CARTESIAN_POINT('Ctrl Pts',(-6.75374529124721,1.89236285939279,
26.6865734106283));
#154735=CARTESIAN_POINT('Ctrl Pts',(-6.80025318023369,1.70709790206118,
26.6952453917912));
#154736=CARTESIAN_POINT('Ctrl Pts',(-6.8467609101261,1.52183357848343,26.703917343289));
#154737=CARTESIAN_POINT('Ctrl Pts',(-6.88569345442265,1.33466776867936,
26.7125892947869));
#154738=CARTESIAN_POINT('Ctrl Pts',(-6.91692090874659,1.14622497994254,
26.7212612462847));
#154739=CARTESIAN_POINT('Ctrl Pts',(-6.94814825879519,0.957782820457667,
26.729933168825));
#154740=CARTESIAN_POINT('Ctrl Pts',(-6.97167052392495,0.76806397077221,
26.7386050913653));
#154741=CARTESIAN_POINT('Ctrl Pts',(-6.98740921903147,0.577701452563602,
26.7472770139055));
#154742=CARTESIAN_POINT('Ctrl Pts',(-7.00314786286679,0.387339554489842,
26.7559489081957));
#154743=CARTESIAN_POINT('Ctrl Pts',(-7.01110296401741,0.196334275138949,
26.7646208024859));
#154744=CARTESIAN_POINT('Ctrl Pts',(-7.01124797942392,0.00532292438054067,
26.773292696776));
#154745=CARTESIAN_POINT('Ctrl Pts',(-7.01139299436986,-0.185687819710631,
26.7819645635236));
#154746=CARTESIAN_POINT('Ctrl Pts',(-7.00372797299446,-0.376704351159606,
26.7906364302711));
#154747=CARTESIAN_POINT('Ctrl Pts',(-6.98827849031214,-0.567089326597393,
26.7993082970187));
#154748=CARTESIAN_POINT('Ctrl Pts',(-6.97282905543841,-0.757473712886903,
26.807980136931));
#154749=CARTESIAN_POINT('Ctrl Pts',(-6.94959523043391,-0.947226263999834,
26.8166519768434));
#154750=CARTESIAN_POINT('Ctrl Pts',(-6.91865453650915,-1.13571385786268,
26.8253238167557));
#154751=CARTESIAN_POINT('Ctrl Pts',(-6.88771393580715,-1.3242008838219,
26.8339956305403));
#154752=CARTESIAN_POINT('Ctrl Pts',(-6.84906655865545,-1.51142267990603,
26.8426674443248));
#154753=CARTESIAN_POINT('Ctrl Pts',(-6.8028413538356,-1.69675457183538,
26.8513392581094));
#154754=CARTESIAN_POINT('Ctrl Pts',(-6.7566162845193,-1.88208592048689,
26.8600110464736));
#154755=CARTESIAN_POINT('Ctrl Pts',(-6.70281350071529,-2.06552710051335,
26.8686828348377));
#154756=CARTESIAN_POINT('Ctrl Pts',(-6.64161251687691,-2.24646605542217,
26.8773546232019));
#154757=CARTESIAN_POINT('Ctrl Pts',(-6.58041170745033,-2.42740449468745,
26.8860263868531));
#154758=CARTESIAN_POINT('Ctrl Pts',(-6.51181283117406,-2.60584045408293,
26.8946981505042));
#154759=CARTESIAN_POINT('Ctrl Pts',(-6.43604476876361,-2.78117858056086,
26.9033699141553));
#154760=CARTESIAN_POINT('Ctrl Pts',(-6.35684774728392,-2.96445180845019,
26.9124341271007));
#154761=CARTESIAN_POINT('Ctrl Pts',(-6.26981768815816,-3.14433998861945,
26.9214983400461));
#154762=CARTESIAN_POINT('Ctrl Pts',(-6.17527181578263,-3.32018742900167,
26.9305625529914));
#154763=CARTESIAN_POINT('Ctrl Pts',(-6.08368050191884,-3.49053963687194,
26.9393435092823));
#154764=CARTESIAN_POINT('Ctrl Pts',(-5.98503618716775,-3.65709956718355,
26.9481244655731));
#154765=CARTESIAN_POINT('Ctrl Pts',(-5.87967633130269,-3.81929742251359,
26.9569054218639));
#154766=CARTESIAN_POINT('Ctrl Pts',(-5.77561495477872,-3.97949631379242,
26.9655781596094));
#154767=CARTESIAN_POINT('Ctrl Pts',(-5.66500279405408,-4.13543980257367,
26.9742508973549));
#154768=CARTESIAN_POINT('Ctrl Pts',(-5.54820899034767,-4.28660746534194,
26.9829236351004));
#154769=CARTESIAN_POINT('Ctrl Pts',(-5.4314163636855,-4.43777360464733,
26.9915962854423));
#154770=CARTESIAN_POINT('Ctrl Pts',(-5.30844239242882,-4.58416378940367,
27.0002689357842));
#154771=CARTESIAN_POINT('Ctrl Pts',(-5.17969746407295,-4.72528948776435,
27.0089415861261));
#154772=CARTESIAN_POINT('Ctrl Pts',(-5.05095379117012,-4.86641380994122,
27.0176141518969));
#154773=CARTESIAN_POINT('Ctrl Pts',(-4.91643946527151,-5.00227353854657,
27.0262867176676));
#154774=CARTESIAN_POINT('Ctrl Pts',(-4.77660337748139,-5.13241529269928,
27.0349592834384));
#154775=CARTESIAN_POINT('Ctrl Pts',(-4.63676860764736,-5.26255582026506,
27.0436317674702));
#154776=CARTESIAN_POINT('Ctrl Pts',(-4.49161238427182,-5.3869782876605,
27.052304251502));
#154777=CARTESIAN_POINT('Ctrl Pts',(-4.34161910267806,-5.50526748939241,
27.0609767355338));
#154778=CARTESIAN_POINT('Ctrl Pts',(-4.19162718580731,-5.62355561486281,
27.0696491406584));
#154779=CARTESIAN_POINT('Ctrl Pts',(-4.03679852186557,-5.73571041041281,
27.0783215457831));
#154780=CARTESIAN_POINT('Ctrl Pts',(-3.8776497743179,-5.84135761533501,
27.0869939509077));
#154781=CARTESIAN_POINT('Ctrl Pts',(-3.71850242284481,-5.94700389350549,
27.0956662799569));
#154782=CARTESIAN_POINT('Ctrl Pts',(-3.55503530028666,-6.04614253816331,
27.104338609006));
#154783=CARTESIAN_POINT('Ctrl Pts',(-3.38779388709622,-6.13844272931282,
27.1130109380551));
#154784=CARTESIAN_POINT('Ctrl Pts',(-3.22055388638227,-6.23074214091948,
27.1216831938601));
#154785=CARTESIAN_POINT('Ctrl Pts',(-3.04953990753783,-6.31620307732865,
27.130355449665));
#154786=CARTESIAN_POINT('Ctrl Pts',(-2.87532260481446,-6.39454036508825,
27.13902770547));
#154787=CARTESIAN_POINT('Ctrl Pts',(-2.70110671662283,-6.47287701679978,
27.1476998908618));
#154788=CARTESIAN_POINT('Ctrl Pts',(-2.52368781567789,-6.54409001910875,
27.1563720762537));
#154789=CARTESIAN_POINT('Ctrl Pts',(-2.34365791912572,-6.60794174615813,
27.1650442616455));
#154790=CARTESIAN_POINT('Ctrl Pts',(-2.16362942554482,-6.6717929756116,
27.1737163794551));
#154791=CARTESIAN_POINT('Ctrl Pts',(-1.9809902447887,-6.72828294965036,
27.1823884972647));
#154792=CARTESIAN_POINT('Ctrl Pts',(-1.79634980371343,-6.77722317363083,
27.1910606150743));
#154793=CARTESIAN_POINT('Ctrl Pts',(-1.61171074128322,-6.82616303219191,
27.1997326681322));
#154794=CARTESIAN_POINT('Ctrl Pts',(-1.42507072299827,-6.86755318072487,
27.2084047211902));
#154795=CARTESIAN_POINT('Ctrl Pts',(-1.23705251634051,-6.90125551144975,
27.2170767742481));
#154796=CARTESIAN_POINT('Ctrl Pts',(-1.04903565219333,-6.93495760152914,
27.2257487653848));
#154797=CARTESIAN_POINT('Ctrl Pts',(-0.859640898942888,-6.96097193353372,
27.2344207565215));
#154798=CARTESIAN_POINT('Ctrl Pts',(-0.669500206864174,-6.97921170588118,
27.2430927476582));
#154799=CARTESIAN_POINT('Ctrl Pts',(-0.479360810406287,-6.99745135394262,
27.2517646797038));
#154800=CARTESIAN_POINT('Ctrl Pts',(-0.288475768017,-7.00791652123609,27.2604366117495));
#154801=CARTESIAN_POINT('Ctrl Pts',(-0.0974819939226111,-7.01057228929,
27.2691085437951));
#154802=CARTESIAN_POINT('Ctrl Pts',(0.0935105410567989,-7.01322804011402,
27.2777804195797));
#154803=CARTESIAN_POINT('Ctrl Pts',(0.284611522343041,-7.00807448913608,
27.2864522953642));
#154804=CARTESIAN_POINT('Ctrl Pts',(0.475183323465242,-6.99512883166569,
27.2951241711487));
#154805=CARTESIAN_POINT('Ctrl Pts',(0.665753950389365,-6.98218325395928,
27.303795993502));
#154806=CARTESIAN_POINT('Ctrl Pts',(0.855795120321891,-6.96144568508307,
27.3124678158552));
#154807=CARTESIAN_POINT('Ctrl Pts',(1.04467275075859,-6.93298531704218,
27.3211396382084));
#154808=CARTESIAN_POINT('Ctrl Pts',(1.23354927905871,-6.90452511507291,
27.32981140996));
#154809=CARTESIAN_POINT('Ctrl Pts',(1.42126200062285,-6.86834224643213,
27.3384831817115));
#154810=CARTESIAN_POINT('Ctrl Pts',(1.60718460924098,-6.82455743578431,
27.347154953463));
#154811=CARTESIAN_POINT('Ctrl Pts',(1.7976338940525,-6.7797065920087,27.3560378577015));
#154812=CARTESIAN_POINT('Ctrl Pts',(1.98620448431277,-6.72687898191044,
27.36492076194));
#154813=CARTESIAN_POINT('Ctrl Pts',(2.17223623427263,-6.66625954377814,
27.3738036661785));
#154814=CARTESIAN_POINT('Ctrl Pts',(2.35386532185444,-6.60707473666823,
27.3824763459348));
#154815=CARTESIAN_POINT('Ctrl Pts',(2.5330741022709,-6.5404628369675,27.3911490256911));
#154816=CARTESIAN_POINT('Ctrl Pts',(2.70926451773662,-6.46664614274149,
27.3998217054475));
#154817=CARTESIAN_POINT('Ctrl Pts',(2.88545151535583,-6.39283088045563,
27.408494216966));
#154818=CARTESIAN_POINT('Ctrl Pts',(3.05862000313812,-6.31181121311306,
27.4171667284846));
#154819=CARTESIAN_POINT('Ctrl Pts',(3.22819210343652,-6.22385751008248,
27.4258392400031));
#154820=CARTESIAN_POINT('Ctrl Pts',(3.39776113570525,-6.13590539837837,
27.4345115946118));
#154821=CARTESIAN_POINT('Ctrl Pts',(3.56373365850634,-6.04101963284236,
27.4431839492206));
#154822=CARTESIAN_POINT('Ctrl Pts',(3.72555582774813,-5.93951684371986,
27.4518563038293));
#154823=CARTESIAN_POINT('Ctrl Pts',(3.8873752804605,-5.83801575853765,27.4605285128542));
#154824=CARTESIAN_POINT('Ctrl Pts',(4.04504427838494,-5.72989802299959,
27.469200721879));
#154825=CARTESIAN_POINT('Ctrl Pts',(4.19803670362804,-5.61552440983848,
27.4778729309038));
#154826=CARTESIAN_POINT('Ctrl Pts',(4.35102676029652,-5.5011525673692,27.4865450056686));
#154827=CARTESIAN_POINT('Ctrl Pts',(4.49934016166036,-5.38052521116288,
27.4952170804333));
#154828=CARTESIAN_POINT('Ctrl Pts',(4.64248202336259,-5.25404484423717,
27.5038891551981));
#154829=CARTESIAN_POINT('Ctrl Pts',(4.7856218558408,-5.12756627033689,27.5125611070247));
#154830=CARTESIAN_POINT('Ctrl Pts',(4.92359008252016,-4.99523503982615,
27.5212330588514));
#154831=CARTESIAN_POINT('Ctrl Pts',(5.05592635131787,-4.85749269608814,
27.5299050106781));
#154832=CARTESIAN_POINT('Ctrl Pts',(5.18826091679903,-4.71975212524894,
27.5385768508871));
#154833=CARTESIAN_POINT('Ctrl Pts',(5.31496347269061,-4.57660078535814,
27.547248691096));
#154834=CARTESIAN_POINT('Ctrl Pts',(5.43561126741474,-4.42851631046493,
27.5559205313049));
#154835=CARTESIAN_POINT('Ctrl Pts',(5.56176013705229,-4.27367975368109,
27.5649877740385));
#154836=CARTESIAN_POINT('Ctrl Pts',(5.68128895686198,-4.11344992041542,
27.574055016772));
#154837=CARTESIAN_POINT('Ctrl Pts',(5.79376175353724,-3.94841123817531,
27.5831222595056));
#154838=CARTESIAN_POINT('Ctrl Pts',(5.90133874236041,-3.79055649463233,
27.591794815884));
#154839=CARTESIAN_POINT('Ctrl Pts',(6.00246078173934,-3.62830291662156,
27.6004673722625));
#154840=CARTESIAN_POINT('Ctrl Pts',(6.09679041553024,-3.46219196342413,
27.6091399286409));
#154841=CARTESIAN_POINT('Ctrl Pts',(6.19111669178468,-3.29608692272269,
27.6178121763313));
#154842=CARTESIAN_POINT('Ctrl Pts',(6.27865090596041,-3.12612502861305,
27.6264844240218));
#154843=CARTESIAN_POINT('Ctrl Pts',(6.35910096685864,-2.95287342359905,
27.6351566717122));
#154844=CARTESIAN_POINT('Ctrl Pts',(6.43954858436819,-2.77962708049541,
27.6438286560135));
#154845=CARTESIAN_POINT('Ctrl Pts',(6.51291235951768,-2.60309148404424,
27.6525006403149));
#154846=CARTESIAN_POINT('Ctrl Pts',(6.57894750102292,-2.42385567666153,
27.6611726246162));
#154847=CARTESIAN_POINT('Ctrl Pts',(6.64498098170959,-2.24462437715371,
27.6698443908125));
#154848=CARTESIAN_POINT('Ctrl Pts',(6.70368609940726,-2.06269326910442,
27.6785161570089));
#154849=CARTESIAN_POINT('Ctrl Pts',(6.7548669838925,-1.87866936750964,27.6871879232052));
#154850=CARTESIAN_POINT('Ctrl Pts',(6.80605126222379,-1.69463326314033,
27.6958602644334));
#154851=CARTESIAN_POINT('Ctrl Pts',(6.84971023276513,-1.50850436118443,
27.7045326056616));
#154852=CARTESIAN_POINT('Ctrl Pts',(6.88569820761627,-1.32090376490116,
27.7132049468899));
#154853=CARTESIAN_POINT('Ctrl Pts',(6.92168406448144,-1.1333142094012,27.7218767777282));
#154854=CARTESIAN_POINT('Ctrl Pts',(6.94999977553719,-0.944253411833958,
27.7305486085666));
#154855=CARTESIAN_POINT('Ctrl Pts',(6.97055086371791,-0.754352184872193,
27.7392204394049));
#154856=CARTESIAN_POINT('Ctrl Pts',(6.99110229107969,-0.564447823726136,
27.7478924133657));
#154857=CARTESIAN_POINT('Ctrl Pts',(7.00388880856458,-0.373703287800228,
27.7565643873264));
#154858=CARTESIAN_POINT('Ctrl Pts',(7.00886775178444,-0.18275502864788,
27.7652363612872));
#154859=CARTESIAN_POINT('Ctrl Pts',(7.01045582731889,-0.121850486194973,
27.7680023598283));
#154860=CARTESIAN_POINT('Ctrl Pts',(7.01125000000004,-0.0609252433299691,
27.7707683583694));
#154861=CARTESIAN_POINT('Ctrl Pts',(7.01125,3.98146195391879E-12,27.7735343569105));
#154862=CARTESIAN_POINT('Ctrl Pts',(7.01124849188977,0.0045986382217964,
27.7735343569106));
#154863=CARTESIAN_POINT('Ctrl Pts',(7.01110746258416,0.219616967251206,
27.7832889411837));
#154864=CARTESIAN_POINT('Ctrl Pts',(7.00107121144239,0.43435405131007,27.7930435254568));
#154865=CARTESIAN_POINT('Ctrl Pts',(6.98124137501422,0.647993384448971,
27.8027981097299));
#154866=CARTESIAN_POINT('Ctrl Pts',(6.96133438247261,0.862463969054885,
27.8125906482147));
#154867=CARTESIAN_POINT('Ctrl Pts',(6.93155750156275,1.07582822248848,27.8223831866996));
#154868=CARTESIAN_POINT('Ctrl Pts',(6.89206436059057,1.2872744120728,27.8321757251844));
#154869=CARTESIAN_POINT('Ctrl Pts',(6.85246177079178,1.49930659043311,27.8419954020994));
#154870=CARTESIAN_POINT('Ctrl Pts',(6.80308901990283,1.70941004109375,27.8518150790144));
#154871=CARTESIAN_POINT('Ctrl Pts',(6.74415134707051,1.91678093957212,27.8616347559293));
#154872=CARTESIAN_POINT('Ctrl Pts',(6.69348504934856,2.09504918764271,27.8700763290386));
#154873=CARTESIAN_POINT('Ctrl Pts',(6.63575095573061,2.2712982718579,27.878517902148));
#154874=CARTESIAN_POINT('Ctrl Pts',(6.57110895151814,2.44502632087635,27.8869594752573));
#154875=CARTESIAN_POINT('',(7.01124919374723,0.00336239182502676,27.2264656430545));
#154876=CARTESIAN_POINT('Ctrl Pts',(6.57110895151815,2.44502632087633,27.3397910544677));
#154877=CARTESIAN_POINT('Ctrl Pts',(6.63541756143711,2.27219428275467,27.3314135214061));
#154878=CARTESIAN_POINT('Ctrl Pts',(6.69287570619621,2.09689805609267,27.3230359883445));
#154879=CARTESIAN_POINT('Ctrl Pts',(6.7433182271924,1.91970983466637,27.3146584552828));
#154880=CARTESIAN_POINT('Ctrl Pts',(6.7911953837239,1.75153290684378,27.3067069799438));
#154881=CARTESIAN_POINT('Ctrl Pts',(6.83275269263724,1.58165188370494,27.2987555046048));
#154882=CARTESIAN_POINT('Ctrl Pts',(6.867891461695,1.41056493394559,27.2908040292657));
#154883=CARTESIAN_POINT('Ctrl Pts',(6.90680224734355,1.22111243438856,27.281998992527));
#154884=CARTESIAN_POINT('Ctrl Pts',(6.93790954720012,1.02985490892179,27.2731939557883));
#154885=CARTESIAN_POINT('Ctrl Pts',(6.96105872276864,0.837429412348653,
27.2643889190496));
#154886=CARTESIAN_POINT('Ctrl Pts',(6.98414320400172,0.64554168177873,27.2556084894939));
#154887=CARTESIAN_POINT('Ctrl Pts',(6.99931389611967,0.452492746196682,
27.2468280599383));
#154888=CARTESIAN_POINT('Ctrl Pts',(7.00646718374326,0.258928881411138,
27.2380476303826));
#154889=CARTESIAN_POINT('Ctrl Pts',(7.00961240899805,0.173820887999565,
27.2341869679516));
#154890=CARTESIAN_POINT('Ctrl Pts',(7.01120830977233,0.0886135121272676,
27.2303263055206));
#154891=CARTESIAN_POINT('Ctrl Pts',(7.01124919374686,0.00336239260024742,
27.2264656430896));
#154892=CARTESIAN_POINT('Ctrl Pts',(7.01124919374723,0.00336239182502279,
27.2264656430545));
#154893=CARTESIAN_POINT('Ctrl Pts',(7.01133243824318,-0.170218777617792,
27.2186048864649));
#154894=CARTESIAN_POINT('Ctrl Pts',(7.00496446246311,-0.343967021434672,
27.2107441298753));
#154895=CARTESIAN_POINT('Ctrl Pts',(6.99213931214691,-0.517314606433853,
27.2028833732857));
#154896=CARTESIAN_POINT('Ctrl Pts',(6.97984637489577,-0.683468681239413,
27.1953488192945));
#154897=CARTESIAN_POINT('Ctrl Pts',(6.96162145168017,-0.849254241412167,
27.1878142653033));
#154898=CARTESIAN_POINT('Ctrl Pts',(6.93751249916856,-1.01417300613852,
27.1802797113122));
#154899=CARTESIAN_POINT('Ctrl Pts',(6.91340523989964,-1.17908018813461,
27.1727456864949));
#154900=CARTESIAN_POINT('Ctrl Pts',(6.88341483877647,-1.34312029690605,
27.1652116616776));
#154901=CARTESIAN_POINT('Ctrl Pts',(6.84764077591788,-1.50580289762199,
27.1576776368603));
#154902=CARTESIAN_POINT('Ctrl Pts',(6.81185484725471,-1.66853945810081,
27.1501411131022));
#154903=CARTESIAN_POINT('Ctrl Pts',(6.77028152667223,-1.82991722014581,
27.1426045893441));
#154904=CARTESIAN_POINT('Ctrl Pts',(6.72307070525454,-1.98945893515002,
27.135068065586));
#154905=CARTESIAN_POINT('Ctrl Pts',(6.71694946583952,-2.01014472296088,
27.1340908983838));
#154906=CARTESIAN_POINT('Ctrl Pts',(6.71073352178257,-2.03079966839598,
27.1331137311815));
#154907=CARTESIAN_POINT('Ctrl Pts',(6.70442326004343,-2.05142275328336,
27.1321365639793));
#154908=CARTESIAN_POINT('Ctrl Pts',(6.64207211118979,-2.25519766608262,
27.1224812596194));
#154909=CARTESIAN_POINT('Ctrl Pts',(6.57051491078361,-2.45584014003303,
27.1128259552595));
#154910=CARTESIAN_POINT('Ctrl Pts',(6.49008777157213,-2.65261894734052,
27.1031706508996));
#154911=CARTESIAN_POINT('Ctrl Pts',(6.40921508109799,-2.85048787232372,
27.093461857965));
#154912=CARTESIAN_POINT('Ctrl Pts',(6.31937397250988,-3.04445018114414,
27.0837530650303));
#154913=CARTESIAN_POINT('Ctrl Pts',(6.22094965134369,-3.23379220079876,
27.0740442720957));
#154914=CARTESIAN_POINT('Ctrl Pts',(6.12205170398593,-3.42404535033072,
27.064288759625));
#154915=CARTESIAN_POINT('Ctrl Pts',(6.01448778024528,-3.6096336099399,27.0545332471543));
#154916=CARTESIAN_POINT('Ctrl Pts',(5.89869161118943,-3.78986330077795,
27.0447777346835));
#154917=CARTESIAN_POINT('Ctrl Pts',(5.78278078611118,-3.97027144673792,
27.0350125627546));
#154918=CARTESIAN_POINT('Ctrl Pts',(5.65862144160521,-4.14531038488499,
27.0252473908257));
#154919=CARTESIAN_POINT('Ctrl Pts',(5.52669089582952,-4.31431504464557,
27.0154822188968));
#154920=CARTESIAN_POINT('Ctrl Pts',(5.39494023436033,-4.48308927038622,
27.0057303615582));
#154921=CARTESIAN_POINT('Ctrl Pts',(5.25543957231355,-4.64584563187324,
26.9959785042197));
#154922=CARTESIAN_POINT('Ctrl Pts',(5.10870597069337,-4.80195271400104,
26.9862266468812));
#154923=CARTESIAN_POINT('Ctrl Pts',(5.0447194934325,-4.87002670762308,26.9819741308184));
#154924=CARTESIAN_POINT('Ctrl Pts',(4.9793581400238,-4.93683667999793,26.9777216147556));
#154925=CARTESIAN_POINT('Ctrl Pts',(4.91266726452488,-5.00233214716553,
26.9734690986928));
#154926=CARTESIAN_POINT('Ctrl Pts',(4.78668753017544,-5.12605374315805,
26.965436053094));
#154927=CARTESIAN_POINT('Ctrl Pts',(4.6558994660757,-5.24514239954555,26.9574030074952));
#154928=CARTESIAN_POINT('Ctrl Pts',(4.5206854613145,-5.35920045551197,26.9493699618964));
#154929=CARTESIAN_POINT('Ctrl Pts',(4.38555837732173,-5.47318519056842,
26.9413420802486));
#154930=CARTESIAN_POINT('Ctrl Pts',(4.2460112950641,-5.58214552691869,26.9333141986008));
#154931=CARTESIAN_POINT('Ctrl Pts',(4.10246291679174,-5.68572111335481,
26.925286316953));
#154932=CARTESIAN_POINT('Ctrl Pts',(3.95897935202721,-5.78924993439265,
26.9172620599729));
#154933=CARTESIAN_POINT('Ctrl Pts',(3.81149838509464,-5.88739863240532,
26.9092378029927));
#154934=CARTESIAN_POINT('Ctrl Pts',(3.66047116581132,-5.97984760731943,
26.9012135460126));
#154935=CARTESIAN_POINT('Ctrl Pts',(3.50946220725726,-6.07228540421074,
26.8931902592469));
#154936=CARTESIAN_POINT('Ctrl Pts',(3.35490815884217,-6.15902465283727,
26.8851669724813));
#154937=CARTESIAN_POINT('Ctrl Pts',(3.19728862275171,-6.23978942155282,
26.8771436857156));
#154938=CARTESIAN_POINT('Ctrl Pts',(3.03968200217577,-6.32054757231625,
26.8691210563866));
#154939=CARTESIAN_POINT('Ctrl Pts',(2.87901072240415,-6.39533205469342,
26.8610984270577));
#154940=CARTESIAN_POINT('Ctrl Pts',(2.71577814400141,-6.46391333752737,
26.8530757977287));
#154941=CARTESIAN_POINT('Ctrl Pts',(2.55248420177032,-6.53252040204112,
26.8450501524623));
#154942=CARTESIAN_POINT('Ctrl Pts',(2.38662737676646,-6.59491946921344,
26.8370245071959));
#154943=CARTESIAN_POINT('Ctrl Pts',(2.21873047899309,-6.65092938047662,
26.8289988619295));
#154944=CARTESIAN_POINT('Ctrl Pts',(2.11972823693536,-6.68395623723245,
26.8242664524218));
#154945=CARTESIAN_POINT('Ctrl Pts',(2.02001699361798,-6.71476251525415,
26.8195340429141));
#154946=CARTESIAN_POINT('Ctrl Pts',(1.91970626837255,-6.74331924245554,
26.8148016334064));
#154947=CARTESIAN_POINT('Ctrl Pts',(1.73465940617455,-6.79599888115151,
26.8060715845718));
#154948=CARTESIAN_POINT('Ctrl Pts',(1.54747933220458,-6.84104703880416,
26.7973415357371));
#154949=CARTESIAN_POINT('Ctrl Pts',(1.35879712463937,-6.87832079337478,
26.7886114869024));
#154950=CARTESIAN_POINT('Ctrl Pts',(1.1700603593783,-6.91560532569806,26.7798789137632));
#154951=CARTESIAN_POINT('Ctrl Pts',(0.979820862296732,-6.94511091476232,
26.771146340624));
#154952=CARTESIAN_POINT('Ctrl Pts',(0.788719045892941,-6.96674592827568,
26.7624137674848));
#154953=CARTESIAN_POINT('Ctrl Pts',(0.594902323132202,-6.98868830169187,
26.7535571342044));
#154954=CARTESIAN_POINT('Ctrl Pts',(0.400198881071557,-7.00253473439903,
26.744700500924));
#154955=CARTESIAN_POINT('Ctrl Pts',(0.205281742193317,-7.00824414306623,
26.7358438676436));
#154956=CARTESIAN_POINT('Ctrl Pts',(0.0129725818766674,-7.01387716021912,
26.7271057355369));
#154957=CARTESIAN_POINT('Ctrl Pts',(-0.179544313956954,-7.01158956178497,
26.7183676034302));
#154958=CARTESIAN_POINT('Ctrl Pts',(-0.371622006393339,-7.00139440732089,
26.7096294713234));
#154959=CARTESIAN_POINT('Ctrl Pts',(-0.567606958134552,-6.99099186223461,
26.7007135874562));
#154960=CARTESIAN_POINT('Ctrl Pts',(-0.763134350466151,-6.97235661479738,
26.691797703589));
#154961=CARTESIAN_POINT('Ctrl Pts',(-0.957520795717108,-6.94555832804457,
26.6828818197217));
#154962=CARTESIAN_POINT('Ctrl Pts',(-1.15190724096807,-6.91876004129176,
26.6739659358545));
#154963=CARTESIAN_POINT('Ctrl Pts',(-1.34515244039036,-6.88379876254957,
26.6650500519873));
#154964=CARTESIAN_POINT('Ctrl Pts',(-1.53658136398352,-6.84079997327495,
26.65613416812));
#154965=CARTESIAN_POINT('Ctrl Pts',(-1.72424866085428,-6.7986461210753,
26.6473934836238));
#154966=CARTESIAN_POINT('Ctrl Pts',(-1.91019033201925,-6.74876322731641,
26.6386527991276));
#154967=CARTESIAN_POINT('Ctrl Pts',(-2.09378076403657,-6.69131591502378,
26.6299121146314));
#154968=CARTESIAN_POINT('Ctrl Pts',(-2.27733816508554,-6.63387893845688,
26.6211730027295));
#154969=CARTESIAN_POINT('Ctrl Pts',(-2.45854491059668,-6.56888034304077,
26.6124338908276));
#154970=CARTESIAN_POINT('Ctrl Pts',(-2.63679070772815,-6.49653456283721,
26.6036947789258));
#154971=CARTESIAN_POINT('Ctrl Pts',(-2.81734593570198,-6.42325143892735,
26.5948424392514));
#154972=CARTESIAN_POINT('Ctrl Pts',(-2.99486268119414,-6.34242950269776,
26.5859900995771));
#154973=CARTESIAN_POINT('Ctrl Pts',(-3.16872638396559,-6.25434246472484,
26.5771377599027));
#154974=CARTESIAN_POINT('Ctrl Pts',(-3.34027827089012,-6.16742669486049,
26.568403127253));
#154975=CARTESIAN_POINT('Ctrl Pts',(-3.50827341437775,-6.07343796674531,
26.5596684946033));
#154976=CARTESIAN_POINT('Ctrl Pts',(-3.6721442503273,-5.97268642800609,
26.5509338619535));
#154977=CARTESIAN_POINT('Ctrl Pts',(-3.83932754645015,-5.86989831297471,
26.5420226687669));
#154978=CARTESIAN_POINT('Ctrl Pts',(-4.00221776425247,-5.76007120419847,
26.5331114755802));
#154979=CARTESIAN_POINT('Ctrl Pts',(-4.16024047493792,-5.64358270544415,
26.5242002823936));
#154980=CARTESIAN_POINT('Ctrl Pts',(-4.31826318562334,-5.52709420668986,
26.5152890892069));
#154981=CARTESIAN_POINT('Ctrl Pts',(-4.47141813719785,-5.40394448697886,
26.5063778960203));
#154982=CARTESIAN_POINT('Ctrl Pts',(-4.61916328400845,-5.27455752818834,
26.4974667028336));
#154983=CARTESIAN_POINT('Ctrl Pts',(-4.75222661313107,-5.15802808642069,
26.4894410379812));
#154984=CARTESIAN_POINT('Ctrl Pts',(-4.88096269756848,-5.03638549043477,
26.4814153731288));
#154985=CARTESIAN_POINT('Ctrl Pts',(-5.00495595374457,-4.90999414089028,
26.4733897082764));
#154986=CARTESIAN_POINT('Ctrl Pts',(-5.12890985750245,-4.78364290486,26.4653665905732));
#154987=CARTESIAN_POINT('Ctrl Pts',(-5.24812367342016,-4.65254617720502,
26.4573434728699));
#154988=CARTESIAN_POINT('Ctrl Pts',(-5.36221771831204,-4.51710612050685,
26.4493203551667));
#154989=CARTESIAN_POINT('Ctrl Pts',(-5.47629737494666,-4.38168314398478,
26.4412982492488));
#154990=CARTESIAN_POINT('Ctrl Pts',(-5.5852583109627,-4.24191821009367,
26.4332761433309));
#154991=CARTESIAN_POINT('Ctrl Pts',(-5.68876032072398,-4.09824750056124,
26.425254037413));
#154992=CARTESIAN_POINT('Ctrl Pts',(-5.79230079218135,-3.95452340250834,
26.4172289504535));
#154993=CARTESIAN_POINT('Ctrl Pts',(-5.89037806806708,-3.80689092532794,
26.409203863494));
#154994=CARTESIAN_POINT('Ctrl Pts',(-5.98269432984447,-3.65581661440324,
26.4011787765344));
#154995=CARTESIAN_POINT('Ctrl Pts',(-6.07502877284792,-3.50471255014858,
26.3931521090742));
#154996=CARTESIAN_POINT('Ctrl Pts',(-6.16159975781025,-3.35016561913782,
26.3851254416139));
#154997=CARTESIAN_POINT('Ctrl Pts',(-6.24215496202924,-3.19266784876124,
26.3770987741536));
#154998=CARTESIAN_POINT('Ctrl Pts',(-6.32277483568218,-3.03504363972989,
26.369065662913));
#154999=CARTESIAN_POINT('Ctrl Pts',(-6.39736912435996,-2.87446419052744,
26.3610325516724));
#155000=CARTESIAN_POINT('Ctrl Pts',(-6.46573301858075,-2.71144299127506,
26.3529994404318));
#155001=CARTESIAN_POINT('Ctrl Pts',(-6.50601550850889,-2.61538497860908,
26.3482660394702));
#155002=CARTESIAN_POINT('Ctrl Pts',(-6.54413573015374,-2.51847954999399,
26.3435326385087));
#155003=CARTESIAN_POINT('Ctrl Pts',(-6.58005986285852,-2.42083431149228,
26.3387992375471));
#155004=CARTESIAN_POINT('Ctrl Pts',(-6.65406469426429,-2.21968208125537,
26.329048284253));
#155005=CARTESIAN_POINT('Ctrl Pts',(-6.71879150752572,-2.01527117141818,
26.3192973309588));
#155006=CARTESIAN_POINT('Ctrl Pts',(-6.77402074923731,-1.80838863395079,
26.3095463776647));
#155007=CARTESIAN_POINT('Ctrl Pts',(-6.82932955903277,-1.60120804337632,
26.299781376293));
#155008=CARTESIAN_POINT('Ctrl Pts',(-6.8751134172199,-1.39154873976351,
26.2900163749214));
#155009=CARTESIAN_POINT('Ctrl Pts',(-6.91120301163579,-1.1802116312155,
26.2802513735497));
#155010=CARTESIAN_POINT('Ctrl Pts',(-6.94723245217505,-0.969226777841337,
26.2705026484122));
#155011=CARTESIAN_POINT('Ctrl Pts',(-6.97359991649955,-0.75656974607434,
26.2607539232746));
#155012=CARTESIAN_POINT('Ctrl Pts',(-6.99018785445479,-0.54304725570876,
26.2510051981371));
#155013=CARTESIAN_POINT('Ctrl Pts',(-7.00673026495205,-0.330110801789158,
26.2412832294701));
#155014=CARTESIAN_POINT('Ctrl Pts',(-7.01354672967217,-0.116313671079241,
26.2315612608032));
#155015=CARTESIAN_POINT('Ctrl Pts',(-7.01057155428194,0.0975348388676593,
26.2218392921362));
#155016=CARTESIAN_POINT('Ctrl Pts',(-7.00761606485012,0.309968369083623,
26.2121816511964));
#155017=CARTESIAN_POINT('Ctrl Pts',(-6.99499805624369,0.522452553789386,
26.2025240102567));
#155018=CARTESIAN_POINT('Ctrl Pts',(-6.97270378507736,0.73418559511063,
26.1928663693169));
#155019=CARTESIAN_POINT('Ctrl Pts',(-6.96290468535469,0.827249556296496,
26.1886215036315));
#155020=CARTESIAN_POINT('Ctrl Pts',(-6.95123688691085,0.920168297558035,
26.1843766379461));
#155021=CARTESIAN_POINT('Ctrl Pts',(-6.93770238185817,1.01287325132982,
26.1801317722607));
#155022=CARTESIAN_POINT('Ctrl Pts',(-6.91266722857905,1.18435220223187,
26.1722799252468));
#155023=CARTESIAN_POINT('Ctrl Pts',(-6.88125167260407,1.35502869998381,
26.1644280782329));
#155024=CARTESIAN_POINT('Ctrl Pts',(-6.84353050352254,1.52437423550011,
26.156576231219));
#155025=CARTESIAN_POINT('Ctrl Pts',(-6.80582003185968,1.69367174599126,
26.1487266109254));
#155026=CARTESIAN_POINT('Ctrl Pts',(-6.76180758702288,1.86163867308816,
26.1408769906318));
#155027=CARTESIAN_POINT('Ctrl Pts',(-6.71161920016561,2.02775597014738,
26.1330273703382));
#155028=CARTESIAN_POINT('Ctrl Pts',(-6.66143482020923,2.19386000486471,
26.1251783767365));
#155029=CARTESIAN_POINT('Ctrl Pts',(-6.60507559084176,2.35811433856822,
26.1173293831347));
#155030=CARTESIAN_POINT('Ctrl Pts',(-6.5427175400908,2.52001463350676,26.1094803895329));
#155031=CARTESIAN_POINT('Ctrl Pts',(-6.48032791928435,2.68199689382481,
26.1016274222155));
#155032=CARTESIAN_POINT('Ctrl Pts',(-6.41193354624725,2.84162237770336,
26.093774454898));
#155033=CARTESIAN_POINT('Ctrl Pts',(-6.33775891677217,2.99840598908401,
26.0859214875806));
#155034=CARTESIAN_POINT('Ctrl Pts',(-6.26356544943364,3.15522941823366,
26.0780665258733));
#155035=CARTESIAN_POINT('Ctrl Pts',(-6.18358897692535,3.30920919844509,
26.070211564166));
#155036=CARTESIAN_POINT('Ctrl Pts',(-6.09809987939284,3.45988503038022,
26.0623566024587));
#155037=CARTESIAN_POINT('Ctrl Pts',(-6.01252592678512,3.61071042067329,
26.0544938440454));
#155038=CARTESIAN_POINT('Ctrl Pts',(-5.92142862103876,3.75822498838122,
26.0466310856321));
#155039=CARTESIAN_POINT('Ctrl Pts',(-5.82512188613292,3.90199712636943,
26.0387683272187));
#155040=CARTESIAN_POINT('Ctrl Pts',(-5.75447264732586,4.00746630378949,
26.0330003204706));
#155041=CARTESIAN_POINT('Ctrl Pts',(-5.68102087203422,4.1109221094603,26.0272323137224));
#155042=CARTESIAN_POINT('Ctrl Pts',(-5.60490397254878,4.21220583791996,
26.0214643069743));
#155043=CARTESIAN_POINT('Ctrl Pts',(-5.49434369253848,4.35932109687934,
26.0130862405333));
#155044=CARTESIAN_POINT('Ctrl Pts',(-5.37791440519695,4.50217851939109,
26.0047081740923));
#155045=CARTESIAN_POINT('Ctrl Pts',(-5.2559707608116,4.64030149063545,25.9963301076512));
#155046=CARTESIAN_POINT('Ctrl Pts',(-5.1341105000411,4.77833001503352,25.9879577700325));
#155047=CARTESIAN_POINT('Ctrl Pts',(-5.00674361665911,4.91163029686316,
25.9795854324137));
#155048=CARTESIAN_POINT('Ctrl Pts',(-4.87426540130525,5.03975826405777,
25.971213094795));
#155049=CARTESIAN_POINT('Ctrl Pts',(-4.74185834496274,5.16781740892225,
25.9628452542723));
#155050=CARTESIAN_POINT('Ctrl Pts',(-4.60434566665319,5.29070955068675,
25.9544774137497));
#155051=CARTESIAN_POINT('Ctrl Pts',(-4.46216023742309,5.40802668059805,
25.946109573227));
#155052=CARTESIAN_POINT('Ctrl Pts',(-4.32003035217989,5.52529798119222,
25.9377450015571));
#155053=CARTESIAN_POINT('Ctrl Pts',(-4.1732316092692,5.63699840398083,25.9293804298871));
#155054=CARTESIAN_POINT('Ctrl Pts',(-4.02223109316899,5.74275923190626,
25.9210158582172));
#155055=CARTESIAN_POINT('Ctrl Pts',(-3.87126746179278,5.84849422575477,
25.9126533297516));
#155056=CARTESIAN_POINT('Ctrl Pts',(-3.71610437327031,5.94829233005975,
25.9042908012861));
#155057=CARTESIAN_POINT('Ctrl Pts',(-3.5572394794681,6.0418270289883,25.8959282728205));
#155058=CARTESIAN_POINT('Ctrl Pts',(-3.39836190775007,6.1353691922786,25.887565076999));
#155059=CARTESIAN_POINT('Ctrl Pts',(-3.23578222071404,6.22264677962363,
25.8792018811775));
#155060=CARTESIAN_POINT('Ctrl Pts',(-3.07002502461718,6.30337789686802,
25.870838685356));
#155061=CARTESIAN_POINT('Ctrl Pts',(-2.90425652421129,6.38411451981303,
25.8624749191813));
#155062=CARTESIAN_POINT('Ctrl Pts',(-2.7353103781694,6.45830363823885,25.8541111530066));
#155063=CARTESIAN_POINT('Ctrl Pts',(-2.56373380198316,6.52571034869531,
25.8457473868319));
#155064=CARTESIAN_POINT('Ctrl Pts',(-2.39212264942504,6.5931306430543,25.8373819351783));
#155065=CARTESIAN_POINT('Ctrl Pts',(-2.21788031573532,6.6537656837975,25.8290164835247));
#155066=CARTESIAN_POINT('Ctrl Pts',(-2.04157230816241,6.70742939381731,
25.8206510318712));
#155067=CARTESIAN_POINT('Ctrl Pts',(-1.86520525538438,6.7611110757081,25.8122827786443));
#155068=CARTESIAN_POINT('Ctrl Pts',(-1.68677146368532,6.8078166757492,25.8039145254174));
#155069=CARTESIAN_POINT('Ctrl Pts',(-1.5068502648184,6.84741037487288,25.7955462721905));
#155070=CARTESIAN_POINT('Ctrl Pts',(-1.32676225333157,6.8870407830043,25.7871702603991));
#155071=CARTESIAN_POINT('Ctrl Pts',(-1.14518440037874,6.91954604321055,
25.7787942486076));
#155072=CARTESIAN_POINT('Ctrl Pts',(-0.962706094642602,6.94484150559521,
25.7704182368161));
#155073=CARTESIAN_POINT('Ctrl Pts',(-0.780138299290921,6.97014937318714,
25.762038117325));
#155074=CARTESIAN_POINT('Ctrl Pts',(-0.596669496892935,6.98824035330412,
25.7536579978338));
#155075=CARTESIAN_POINT('Ctrl Pts',(-0.412893477279431,6.99908176398305,
25.7452778783427));
#155076=CARTESIAN_POINT('Ctrl Pts',(-0.228907470283813,7.00993556234702,
25.7368881835035));
#155077=CARTESIAN_POINT('Ctrl Pts',(-0.0446138732810691,7.0135232261692,
25.7284984886643));
#155078=CARTESIAN_POINT('Ctrl Pts',(0.139392895001137,7.00986420576913,
25.720108793825));
#155079=CARTESIAN_POINT('Ctrl Pts',(0.256215616824345,7.00754115685993,
25.7147823213505));
#155080=CARTESIAN_POINT('Ctrl Pts',(0.372922769241343,7.00229819252713,
25.709455848876));
#155081=CARTESIAN_POINT('Ctrl Pts',(0.489363448129637,6.99415112634369,
25.7041293764015));
#155082=CARTESIAN_POINT('Ctrl Pts',(0.67258495425426,6.9813315709196,25.6957480759965));
#155083=CARTESIAN_POINT('Ctrl Pts',(0.855515982903206,6.96129316380636,
25.6873667755916));
#155084=CARTESIAN_POINT('Ctrl Pts',(1.03756407028496,6.9340527372204,25.6789854751867));
#155085=CARTESIAN_POINT('Ctrl Pts',(1.21938143836511,6.90684683388755,25.6706147968532));
#155086=CARTESIAN_POINT('Ctrl Pts',(1.40031777380958,6.87245714934698,25.6622441185196));
#155087=CARTESIAN_POINT('Ctrl Pts',(1.57978345622306,6.8309524075303,25.6538734401861));
#155088=CARTESIAN_POINT('Ctrl Pts',(1.75904547589867,6.78949476646981,25.6455122611353));
#155089=CARTESIAN_POINT('Ctrl Pts',(1.93683985163729,6.74093823461556,25.6371510820845));
#155090=CARTESIAN_POINT('Ctrl Pts',(2.11258446831307,6.68540301154257,25.6287899030338));
#155091=CARTESIAN_POINT('Ctrl Pts',(2.28810103561878,6.62993985197216,25.6204395735991));
#155092=CARTESIAN_POINT('Ctrl Pts',(2.46157283817462,6.56751616194645,25.6120892441644));
#155093=CARTESIAN_POINT('Ctrl Pts',(2.63243037417588,6.49830261588488,25.6037389147297));
#155094=CARTESIAN_POINT('Ctrl Pts',(2.80315644552294,6.42914232550703,25.595395010374));
#155095=CARTESIAN_POINT('Ctrl Pts',(2.97127195652179,6.35320271284423,25.5870511060183));
#155096=CARTESIAN_POINT('Ctrl Pts',(3.13622383737408,6.27070383644345,25.5787072016627));
#155097=CARTESIAN_POINT('Ctrl Pts',(3.30104322784797,6.18827122365419,25.570369999183));
#155098=CARTESIAN_POINT('Ctrl Pts',(3.46270376373737,6.09929000042067,25.5620327967032));
#155099=CARTESIAN_POINT('Ctrl Pts',(3.62067345367302,6.00402784007266,25.5536955942235));
#155100=CARTESIAN_POINT('Ctrl Pts',(3.67267620362997,5.97266806271945,25.5509510331874));
#155101=CARTESIAN_POINT('Ctrl Pts',(3.72427915896482,5.94062800628429,25.5482064721512));
#155102=CARTESIAN_POINT('Ctrl Pts',(3.77546389517242,5.90791832532826,25.545461911115));
#155103=CARTESIAN_POINT('Ctrl Pts',(3.93096935036048,5.80854233547277,25.5371236008131));
#155104=CARTESIAN_POINT('Ctrl Pts',(4.08248496436116,5.70306382850009,25.5287852905112));
#155105=CARTESIAN_POINT('Ctrl Pts',(4.22953330315354,5.59184000128895,25.5204469802093));
#155106=CARTESIAN_POINT('Ctrl Pts',(4.37667415977078,5.48054619581996,25.5121034237255));
#155107=CARTESIAN_POINT('Ctrl Pts',(4.51934187365447,5.36350005767804,25.5037598672417));
#155108=CARTESIAN_POINT('Ctrl Pts',(4.65709241826652,5.24109881324752,25.4954163107579));
#155109=CARTESIAN_POINT('Ctrl Pts',(4.79494776289289,5.11860444648338,25.4870664065326));
#155110=CARTESIAN_POINT('Ctrl Pts',(4.9278782316006,4.9907470642378,25.4787165023074));
#155111=CARTESIAN_POINT('Ctrl Pts',(5.05547663845835,4.85796073682177,25.4703665980822));
#155112=CARTESIAN_POINT('Ctrl Pts',(5.18326643348369,4.72497523974123,25.4620041696185));
#155113=CARTESIAN_POINT('Ctrl Pts',(5.30570795752275,4.58704626030353,25.4536417411548));
#155114=CARTESIAN_POINT('Ctrl Pts',(5.42243333523086,4.44464208766883,25.4452793126912));
#155115=CARTESIAN_POINT('Ctrl Pts',(5.53925852904966,4.30211614005307,25.4369097332112));
#155116=CARTESIAN_POINT('Ctrl Pts',(5.65035762646628,4.1551076243623,25.4285401537312));
#155117=CARTESIAN_POINT('Ctrl Pts',(5.7554057779623,4.00411424580995,25.4201705742511));
#155118=CARTESIAN_POINT('Ctrl Pts',(5.86061595343287,3.8528879783683,25.4117880857145));
#155119=CARTESIAN_POINT('Ctrl Pts',(5.95975635714806,3.69766484179189,25.4034055971779));
#155120=CARTESIAN_POINT('Ctrl Pts',(6.05254710073434,3.53896879837791,25.3950231086413));
#155121=CARTESIAN_POINT('Ctrl Pts',(6.08290975250043,3.48704085258712,25.3922802210371));
#155122=CARTESIAN_POINT('Ctrl Pts',(6.11259292136257,3.43474123219163,25.3895373334329));
#155123=CARTESIAN_POINT('Ctrl Pts',(6.1415879167107,3.38208876640061,25.3867944458286));
#155124=CARTESIAN_POINT('Ctrl Pts',(6.23396022342135,3.21434844912426,25.3780561497189));
#155125=CARTESIAN_POINT('Ctrl Pts',(6.31951401861006,3.04271762722003,25.3693178536093));
#155126=CARTESIAN_POINT('Ctrl Pts',(6.39793694776335,2.86775685422328,25.3605795574996));
#155127=CARTESIAN_POINT('Ctrl Pts',(6.46020040433268,2.72884770343746,25.3536418349969));
#155128=CARTESIAN_POINT('Ctrl Pts',(6.51796974249906,2.58784013399584,25.3467041124941));
#155129=CARTESIAN_POINT('Ctrl Pts',(6.57110895151814,2.44502632087636,25.3397663899914));
#155130=CARTESIAN_POINT('Origin',(0.,0.,50.));
#155131=CARTESIAN_POINT('',(6.57110895151814,2.44502632087637,23.3397812382711));
#155132=CARTESIAN_POINT('',(6.57110895151814,2.44502632087635,23.8869833201214));
#155133=CARTESIAN_POINT('',(6.57110895151814,2.44502632087636,50.));
#155134=CARTESIAN_POINT('',(7.01124974356013,-0.001896293246826,25.7735343569105));
#155135=CARTESIAN_POINT('Ctrl Pts',(6.57110895151814,2.44502632087635,23.8869833201214));
#155136=CARTESIAN_POINT('Ctrl Pts',(6.50404482602339,2.62526392061162,23.8957163741572));
#155137=CARTESIAN_POINT('Ctrl Pts',(6.42955178260845,2.8027657603483,23.9044494281931));
#155138=CARTESIAN_POINT('Ctrl Pts',(6.34787351276833,2.97693272150956,23.9131824822289));
#155139=CARTESIAN_POINT('Ctrl Pts',(6.26622575892236,3.15103461177769,23.9219122734896));
#155140=CARTESIAN_POINT('Ctrl Pts',(6.17739825529668,3.32180386372133,23.9306420647503));
#155141=CARTESIAN_POINT('Ctrl Pts',(6.08168209537615,3.48866298935297,23.939371856011));
#155142=CARTESIAN_POINT('Ctrl Pts',(6.04178272988089,3.55821836271232,23.9430108771804));
#155143=CARTESIAN_POINT('Ctrl Pts',(6.00068692045035,3.62709456677471,23.9466498983498));
#155144=CARTESIAN_POINT('Ctrl Pts',(5.95841812638918,3.69525100549569,23.9502889195193));
#155145=CARTESIAN_POINT('Ctrl Pts',(5.8651965816224,3.84556635383936,23.9583145843718));
#155146=CARTESIAN_POINT('Ctrl Pts',(5.76622355083788,3.99244807418705,23.9663402492242));
#155147=CARTESIAN_POINT('Ctrl Pts',(5.66179063331389,4.13542662696597,23.9743659140767));
#155148=CARTESIAN_POINT('Ctrl Pts',(5.55739086023635,4.27835980185925,23.98238903178));
#155149=CARTESIAN_POINT('Ctrl Pts',(5.44753486628551,4.41739197979333,23.9904121494833));
#155150=CARTESIAN_POINT('Ctrl Pts',(5.33255737110211,4.55208286901772,23.9984352671866));
#155151=CARTESIAN_POINT('Ctrl Pts',(5.21759437558721,4.68675677254207,24.0064573731045));
#155152=CARTESIAN_POINT('Ctrl Pts',(5.09751140371063,4.8170901995232,24.0144794790224));
#155153=CARTESIAN_POINT('Ctrl Pts',(4.97268318748858,4.94267624666723,24.0225015849403));
#155154=CARTESIAN_POINT('Ctrl Pts',(4.84780858467955,5.06830896201076,24.0305266718999));
#155155=CARTESIAN_POINT('Ctrl Pts',(4.71818547144416,5.18919051097218,24.0385517588595));
#155156=CARTESIAN_POINT('Ctrl Pts',(4.58422546121499,5.30495084644978,24.0465768458191));
#155157=CARTESIAN_POINT('Ctrl Pts',(4.45023906823207,5.42073398034625,24.0546035132794));
#155158=CARTESIAN_POINT('Ctrl Pts',(4.31191435980095,5.53139365845925,24.0626301807397));
#155159=CARTESIAN_POINT('Ctrl Pts',(4.1696955226784,5.63660055447038,24.0706568482));
#155160=CARTESIAN_POINT('Ctrl Pts',(4.0273625127746,5.74189191020686,24.0786899594406));
#155161=CARTESIAN_POINT('Ctrl Pts',(3.88112943055859,5.84172153043871,24.0867230706813));
#155162=CARTESIAN_POINT('Ctrl Pts',(3.73146940048094,5.93580345663285,24.094756181922));
#155163=CARTESIAN_POINT('Ctrl Pts',(3.64328427407108,5.99123994525314,24.0994895828831));
#155164=CARTESIAN_POINT('Ctrl Pts',(3.55390981728491,6.04468168798134,24.1042229838443));
#155165=CARTESIAN_POINT('Ctrl Pts',(3.46344666393083,6.09607773643073,24.1089563848055));
#155166=CARTESIAN_POINT('Ctrl Pts',(3.27708975260619,6.20195519579622,24.1187073380996));
#155167=CARTESIAN_POINT('Ctrl Pts',(3.08600197741005,6.29921177699002,24.1284582913937));
#155168=CARTESIAN_POINT('Ctrl Pts',(2.89092393910911,6.38750227716483,24.1382092446878));
#155169=CARTESIAN_POINT('Ctrl Pts',(2.69556485429831,6.47591997636801,24.1479742460593));
#155170=CARTESIAN_POINT('Ctrl Pts',(2.49620404244238,6.55534574017783,24.1577392474308));
#155171=CARTESIAN_POINT('Ctrl Pts',(2.29360398337489,6.62548166776929,24.1675042488024));
#155172=CARTESIAN_POINT('Ctrl Pts',(2.09134161662808,6.69550069330128,24.1772529739399));
#155173=CARTESIAN_POINT('Ctrl Pts',(1.8858508292091,6.7562608169052,24.1870016990774));
#155174=CARTESIAN_POINT('Ctrl Pts',(1.67790829217237,6.80751425452486,24.1967504242149));
#155175=CARTESIAN_POINT('Ctrl Pts',(1.47053647677048,6.85862702133169,24.206472392882));
#155176=CARTESIAN_POINT('Ctrl Pts',(1.26072638407638,6.90028518134357,24.2161943615491));
#155177=CARTESIAN_POINT('Ctrl Pts',(1.04926570122329,6.93229168823243,24.2259163302161));
#155178=CARTESIAN_POINT('Ctrl Pts',(0.839204198477849,6.96408641642489,
24.2355739711558));
#155179=CARTESIAN_POINT('Ctrl Pts',(0.627513918248232,6.9863567587275,24.2452316120954));
#155180=CARTESIAN_POINT('Ctrl Pts',(0.414983637284344,6.99895814698776,
24.2548892530351));
#155181=CARTESIAN_POINT('Ctrl Pts',(0.321569261820565,7.004496890968,24.2591341187208));
#155182=CARTESIAN_POINT('Ctrl Pts',(0.227992819303063,7.00816832190326,
24.2633789844064));
#155183=CARTESIAN_POINT('Ctrl Pts',(0.134322281303897,7.00996320156143,
24.2676238500921));
#155184=CARTESIAN_POINT('Ctrl Pts',(-0.038942737790631,7.0132832407636,
24.275475697106));
#155185=CARTESIAN_POINT('Ctrl Pts',(-0.212458611611713,7.01017750829807,
24.28332754412));
#155186=CARTESIAN_POINT('Ctrl Pts',(-0.385691713600459,7.00063343309446,
24.2911793911339));
#155187=CARTESIAN_POINT('Ctrl Pts',(-0.558875688082151,6.99109206451341,
24.2990290114275));
#155188=CARTESIAN_POINT('Ctrl Pts',(-0.731776669736127,6.97511600610969,
24.3068786317211));
#155189=CARTESIAN_POINT('Ctrl Pts',(-0.903861994681407,6.95274478584325,
24.3147282520147));
#155190=CARTESIAN_POINT('Ctrl Pts',(-1.07593358081459,6.93037535163261,
24.3225772456165));
#155191=CARTESIAN_POINT('Ctrl Pts',(-1.2471892616903,6.90161182188765,24.3304262392183));
#155192=CARTESIAN_POINT('Ctrl Pts',(-1.41710271542319,6.86654545287805,
24.3382752328201));
#155193=CARTESIAN_POINT('Ctrl Pts',(-1.58710219136203,6.83146133079269,
24.3461282001375));
#155194=CARTESIAN_POINT('Ctrl Pts',(-1.7557577083443,6.7900680709802,24.3539811674549));
#155195=CARTESIAN_POINT('Ctrl Pts',(-1.92255400821172,6.74250789009617,
24.3618341347724));
#155196=CARTESIAN_POINT('Ctrl Pts',(-2.08939266873477,6.69493563052426,
24.3696890964796));
#155197=CARTESIAN_POINT('Ctrl Pts',(-2.25437080870463,6.64119344782899,
24.3775440581869));
#155198=CARTESIAN_POINT('Ctrl Pts',(-2.41699013617812,6.58147287802037,
24.3853990198941));
#155199=CARTESIAN_POINT('Ctrl Pts',(-2.57977087692747,6.52169303055417,
24.3932617783075));
#155200=CARTESIAN_POINT('Ctrl Pts',(-2.74018777617318,6.4559230888124,24.4011245367208));
#155201=CARTESIAN_POINT('Ctrl Pts',(-2.89776373374651,6.38440223559602,
24.4089872951342));
#155202=CARTESIAN_POINT('Ctrl Pts',(-3.01335919514051,6.33193556394028,
24.4147553018822));
#155203=CARTESIAN_POINT('Ctrl Pts',(-3.12742626232211,6.27637504553989,
24.4205233086303));
#155204=CARTESIAN_POINT('Ctrl Pts',(-3.23978591027477,6.21783031435284,
24.4262913153784));
#155205=CARTESIAN_POINT('Ctrl Pts',(-3.40298901265464,6.13279372041702,
24.4346693818195));
#155206=CARTESIAN_POINT('Ctrl Pts',(-3.56295046482453,6.04127128635174,
24.4430474482605));
#155207=CARTESIAN_POINT('Ctrl Pts',(-3.7191421093381,5.94353501992275,24.4514255147015));
#155208=CARTESIAN_POINT('Ctrl Pts',(-3.87522695186101,5.84586558439145,
24.4597978523202));
#155209=CARTESIAN_POINT('Ctrl Pts',(-4.02754684822184,5.74199096145221,
24.468170189939));
#155210=CARTESIAN_POINT('Ctrl Pts',(-4.17559910596323,5.63222857035997,
24.4765425275577));
#155211=CARTESIAN_POINT('Ctrl Pts',(-4.32357183929128,5.52252513675943,
24.4849103680803));
#155212=CARTESIAN_POINT('Ctrl Pts',(-4.46728124116798,5.4069404361491,24.4932782086029));
#155213=CARTESIAN_POINT('Ctrl Pts',(-4.60625405735026,5.2858348556916,24.5016460491255));
#155214=CARTESIAN_POINT('Ctrl Pts',(-4.74517258453623,5.16477658448919,
24.5100106207954));
#155215=CARTESIAN_POINT('Ctrl Pts',(-4.87935796838042,5.03820194985158,
24.5183751924653));
#155216=CARTESIAN_POINT('Ctrl Pts',(-5.00837012799503,4.90651151262352,
24.5267397641352));
#155217=CARTESIAN_POINT('Ctrl Pts',(-5.13735077395742,4.77485324326747,
24.5351022926008));
#155218=CARTESIAN_POINT('Ctrl Pts',(-5.26116048622341,4.63808189827305,
24.5434648210664));
#155219=CARTESIAN_POINT('Ctrl Pts',(-5.37939582343168,4.49663509052556,
24.551827349532));
#155220=CARTESIAN_POINT('Ctrl Pts',(-5.49764059618969,4.35517699488037,
24.5601905453535));
#155221=CARTESIAN_POINT('Ctrl Pts',(-5.61030988971127,4.20904293934588,
24.568553741175));
#155222=CARTESIAN_POINT('Ctrl Pts',(-5.71703988042991,4.05870441989485,
24.5769169369966));
#155223=CARTESIAN_POINT('Ctrl Pts',(-5.82377714991998,3.90835564765814,
24.5852807031713));
#155224=CARTESIAN_POINT('Ctrl Pts',(-5.92457411840601,3.75380210774675,
24.593644469346));
#155225=CARTESIAN_POINT('Ctrl Pts',(-6.01910962728124,3.59554527954666,
24.6020082355207));
#155226=CARTESIAN_POINT('Ctrl Pts',(-6.11366418709565,3.43725655919045,
24.6103736871743));
#155227=CARTESIAN_POINT('Ctrl Pts',(-6.20195460260338,3.27526334468759,
24.6187391388278));
#155228=CARTESIAN_POINT('Ctrl Pts',(-6.28370489657797,3.11009313931625,
24.6271045904814));
#155229=CARTESIAN_POINT('Ctrl Pts',(-6.36548256856545,2.94486761876756,
24.6354728437083));
#155230=CARTESIAN_POINT('Ctrl Pts',(-6.44071560576633,2.77646328031728,
24.6438410969352));
#155231=CARTESIAN_POINT('Ctrl Pts',(-6.50917535471592,2.60542947785176,
24.652209350162));
#155232=CARTESIAN_POINT('Ctrl Pts',(-6.57769857561956,2.43423710265091,
24.6605853619535));
#155233=CARTESIAN_POINT('Ctrl Pts',(-6.63943583704474,2.2604106973618,24.668961373745));
#155234=CARTESIAN_POINT('Ctrl Pts',(-6.69420732377659,2.08451789841101,
24.6773373855365));
#155235=CARTESIAN_POINT('Ctrl Pts',(-6.74900567112229,1.90853883945832,
24.6857175050276));
#155236=CARTESIAN_POINT('Ctrl Pts',(-6.79683133996421,1.73049168161851,
24.6940976245188));
#155237=CARTESIAN_POINT('Ctrl Pts',(-6.83755506548899,1.55095689459954,
24.7024777440099));
#155238=CARTESIAN_POINT('Ctrl Pts',(-6.8783253230288,1.37121696634411,24.7108674388492));
#155239=CARTESIAN_POINT('Ctrl Pts',(-6.91197735568175,1.18998633447894,
24.7192571336884));
#155240=CARTESIAN_POINT('Ctrl Pts',(-6.93843322754209,1.00785460729208,
24.7276468285276));
#155241=CARTESIAN_POINT('Ctrl Pts',(-6.95522960404399,0.892222316701829,
24.7329733010022));
#155242=CARTESIAN_POINT('Ctrl Pts',(-6.9691264230549,0.776226943854541,
24.7382997734768));
#155243=CARTESIAN_POINT('Ctrl Pts',(-6.98011462870249,0.660019948693604,
24.7436262459514));
#155244=CARTESIAN_POINT('Ctrl Pts',(-6.99740476826154,0.477166148126987,
24.7520075463562));
#155245=CARTESIAN_POINT('Ctrl Pts',(-7.0075256093269,0.293419399643907,
24.7603888467611));
#155246=CARTESIAN_POINT('Ctrl Pts',(-7.01039695250101,0.109366955085041,
24.768770147166));
#155247=CARTESIAN_POINT('Ctrl Pts',(-7.01326465666798,-0.0744522299437054,
24.7771408254996));
#155248=CARTESIAN_POINT('Ctrl Pts',(-7.00890116796093,-0.258576013994685,
24.7855115038331));
#155249=CARTESIAN_POINT('Ctrl Pts',(-6.99727794590954,-0.442411471582774,
24.7938821821667));
#155250=CARTESIAN_POINT('Ctrl Pts',(-6.98566791421957,-0.626038307489429,
24.8022433612175));
#155251=CARTESIAN_POINT('Ctrl Pts',(-6.96681459007259,-0.80937714407093,
24.8106045402683));
#155252=CARTESIAN_POINT('Ctrl Pts',(-6.94074144317052,-0.991834049403023,
24.8189657193191));
#155253=CARTESIAN_POINT('Ctrl Pts',(-6.91470212925214,-1.17405419537787,
24.8273160487539));
#155254=CARTESIAN_POINT('Ctrl Pts',(-6.8814617253198,-1.35539436992544,
24.8356663781886));
#155255=CARTESIAN_POINT('Ctrl Pts',(-6.84109555852682,-1.53526483761095,
24.8440167076233));
#155256=CARTESIAN_POINT('Ctrl Pts',(-6.80076045108455,-1.71499690573115,
24.852360611979));
#155257=CARTESIAN_POINT('Ctrl Pts',(-6.75331057854142,-1.89326120222885,
24.8607045163347));
#155258=CARTESIAN_POINT('Ctrl Pts',(-6.69887267339629,-2.0694761337412,
24.8690484206904));
#155259=CARTESIAN_POINT('Ctrl Pts',(-6.64447849311608,-2.24554952832158,
24.8773856231701));
#155260=CARTESIAN_POINT('Ctrl Pts',(-6.58310757065704,-2.41957652860795,
24.8857228256499));
#155261=CARTESIAN_POINT('Ctrl Pts',(-6.51493705749792,-2.59098855638932,
24.8940600281296));
#155262=CARTESIAN_POINT('Ctrl Pts',(-6.49249570085809,-2.64741644976337,
24.8968045891656));
#155263=CARTESIAN_POINT('Ctrl Pts',(-6.46931788325442,-2.70356107538801,
24.8995491502017));
#155264=CARTESIAN_POINT('Ctrl Pts',(-6.44541110559393,-2.75940251547079,
24.9022937112378));
#155265=CARTESIAN_POINT('Ctrl Pts',(-6.37277940681515,-2.92905560352234,
24.9106320215397));
#155266=CARTESIAN_POINT('Ctrl Pts',(-6.29347528529428,-3.09576958922512,
24.9189703318416));
#155267=CARTESIAN_POINT('Ctrl Pts',(-6.20777312731114,-3.25901509084167,
24.9273086421435));
#155268=CARTESIAN_POINT('Ctrl Pts',(-6.12201704843831,-3.42236330098845,
24.9356521986273));
#155269=CARTESIAN_POINT('Ctrl Pts',(-6.02985505618818,-3.58223838417279,
24.9439957551111));
#155270=CARTESIAN_POINT('Ctrl Pts',(-5.93160648698461,-3.73813737656364,
24.9523393115949));
#155271=CARTESIAN_POINT('Ctrl Pts',(-5.83328317069781,-3.89415497622842,
24.9606892158201));
#155272=CARTESIAN_POINT('Ctrl Pts',(-5.72886421533329,-4.04619017434361,
24.9690391200453));
#155273=CARTESIAN_POINT('Ctrl Pts',(-5.61871132564573,-4.19377033247654,
24.9773890242705));
#155274=CARTESIAN_POINT('Ctrl Pts',(-5.50839321477503,-4.34157184992565,
24.9857514527342));
#155275=CARTESIAN_POINT('Ctrl Pts',(-5.39232417927697,-4.48490471139241,
24.9941138811978));
#155276=CARTESIAN_POINT('Ctrl Pts',(-5.27090610601988,-4.62332946955139,
25.0024763096615));
#155277=CARTESIAN_POINT('Ctrl Pts',(-5.14938420375849,-4.76187259974862,
25.0108458891414));
#155278=CARTESIAN_POINT('Ctrl Pts',(-5.02250436218446,-4.89549901530344,
25.0192154686214));
#155279=CARTESIAN_POINT('Ctrl Pts',(-4.89070451907986,-5.02380691005854,
25.0275850481013));
#155280=CARTESIAN_POINT('Ctrl Pts',(-4.75870139077554,-5.15231270410847,
25.0359675366379));
#155281=CARTESIAN_POINT('Ctrl Pts',(-4.62176333998194,-5.27548336628875,
25.0443500251745));
#155282=CARTESIAN_POINT('Ctrl Pts',(-4.48036155510013,-5.39295715707818,
25.052732513711));
#155283=CARTESIAN_POINT('Ctrl Pts',(-4.43409257408121,-5.43139650634665,
25.0554754013154));
#155284=CARTESIAN_POINT('Ctrl Pts',(-4.38734588961209,-5.46922623405847,
25.0582182889198));
#155285=CARTESIAN_POINT('Ctrl Pts',(-4.34013865785327,-5.50643468980679,
25.0609611765242));
#155286=CARTESIAN_POINT('Ctrl Pts',(-4.19574271722335,-5.62024670053037,
25.069351031657));
#155287=CARTESIAN_POINT('Ctrl Pts',(-4.04674420327156,-5.72847259738455,
25.0777408867898));
#155288=CARTESIAN_POINT('Ctrl Pts',(-3.89360220379027,-5.83073652647241,
25.0861307419226));
#155289=CARTESIAN_POINT('Ctrl Pts',(-3.74060152159914,-5.9329060878402,
25.0945128550146));
#155290=CARTESIAN_POINT('Ctrl Pts',(-3.58346524817898,-6.02912446724261,
25.1028949681067));
#155291=CARTESIAN_POINT('Ctrl Pts',(-3.42268409254566,-6.11905713040293,
25.1112770811988));
#155292=CARTESIAN_POINT('Ctrl Pts',(-3.26202766901266,-6.20892002487724,
25.1196526915477));
#155293=CARTESIAN_POINT('Ctrl Pts',(-3.09773228661755,-6.29250676523397,
25.1280283018966));
#155294=CARTESIAN_POINT('Ctrl Pts',(-2.93031646352881,-6.36952682591667,
25.1364039122455));
#155295=CARTESIAN_POINT('Ctrl Pts',(-2.7630059474789,-6.44649843983745,
25.144774254211));
#155296=CARTESIAN_POINT('Ctrl Pts',(-2.59257920225916,-6.51691147297294,
25.1531445961766));
#155297=CARTESIAN_POINT('Ctrl Pts',(-2.41957851455754,-6.58052174028713,
25.1615149381422));
#155298=CARTESIAN_POINT('Ctrl Pts',(-2.24666128689977,-6.64410132034932,
25.1698812420365));
#155299=CARTESIAN_POINT('Ctrl Pts',(-2.07117290096369,-6.70088456585396,
25.1782475459308));
#155300=CARTESIAN_POINT('Ctrl Pts',(-1.8936751763582,-6.75067558759453,
25.1866138498251));
#155301=CARTESIAN_POINT('Ctrl Pts',(-1.716227092891,-6.80045268418197,25.1949778138988));
#155302=CARTESIAN_POINT('Ctrl Pts',(-1.53677110705684,-6.84324136622329,
25.2033417779724));
#155303=CARTESIAN_POINT('Ctrl Pts',(-1.3558842738562,-6.87889557984488,
25.211705742046));
#155304=CARTESIAN_POINT('Ctrl Pts',(-1.17502527613319,-6.9145443068755,
25.2200684190445));
#155305=CARTESIAN_POINT('Ctrl Pts',(-0.992736192405863,-6.9430606908922,
25.2284310960431));
#155306=CARTESIAN_POINT('Ctrl Pts',(-0.80960476180415,-6.96434969628637,
25.2367937730416));
#155307=CARTESIAN_POINT('Ctrl Pts',(-0.626477101543896,-6.98563826337883,
25.2451562778679));
#155308=CARTESIAN_POINT('Ctrl Pts',(-0.442507455486583,-6.99969971100276,
25.2535187826942));
#155309=CARTESIAN_POINT('Ctrl Pts',(-0.258289619027391,-7.00649077892797,
25.2618812875205));
#155310=CARTESIAN_POINT('Ctrl Pts',(-0.0740510203503235,-7.01328261223853,
25.2702447348405));
#155311=CARTESIAN_POINT('Ctrl Pts',(0.11043549606457,-7.01280242061977,
25.2786081821605));
#155312=CARTESIAN_POINT('Ctrl Pts',(0.294574756225263,-7.00505904868009,
25.2869716294805));
#155313=CARTESIAN_POINT('Ctrl Pts',(0.478822442757081,-6.99731111722541,
25.2953400014333));
#155314=CARTESIAN_POINT('Ctrl Pts',(0.662722135695841,-6.98229147231855,
25.3037083733861));
#155315=CARTESIAN_POINT('Ctrl Pts',(0.845681362469007,-6.96006103390427,
25.3120767453389));
#155316=CARTESIAN_POINT('Ctrl Pts',(1.02869540860835,-6.93782393466963,
25.3204476246747));
#155317=CARTESIAN_POINT('Ctrl Pts',(1.21076810101937,-6.90837177876169,
25.3288185040105));
#155318=CARTESIAN_POINT('Ctrl Pts',(1.3913150859135,-6.87181700092556,25.3371893833462));
#155319=CARTESIAN_POINT('Ctrl Pts',(1.5720150463155,-6.83523125062147,25.3455673552375));
#155320=CARTESIAN_POINT('Ctrl Pts',(1.75118639481871,-6.79153092394558,
25.3539453271288));
#155321=CARTESIAN_POINT('Ctrl Pts',(1.92825677762194,-6.74087919800193,
25.3623232990201));
#155322=CARTESIAN_POINT('Ctrl Pts',(2.0407864477829,-6.70868961370619,25.3676475683791));
#155323=CARTESIAN_POINT('Ctrl Pts',(2.15246788626999,-6.67369357446904,
25.3729718377381));
#155324=CARTESIAN_POINT('Ctrl Pts',(2.26315789621798,-6.63594325618342,
25.3782961070971));
#155325=CARTESIAN_POINT('Ctrl Pts',(2.42662386757984,-6.58019393923352,
25.3861589382864));
#155326=CARTESIAN_POINT('Ctrl Pts',(2.58826656138555,-6.51831926484871,
25.3940217694757));
#155327=CARTESIAN_POINT('Ctrl Pts',(2.74757357211185,-6.45046246623702,
25.4018846006649));
#155328=CARTESIAN_POINT('Ctrl Pts',(2.90675817642854,-6.38265780661813,
25.4097413903063));
#155329=CARTESIAN_POINT('Ctrl Pts',(3.06361031810499,-6.3088803119669,25.4175981799477));
#155330=CARTESIAN_POINT('Ctrl Pts',(3.21763312647164,-6.22932288663322,
25.4254549695891));
#155331=CARTESIAN_POINT('Ctrl Pts',(3.3715690732653,-6.14981032792144,25.4333073283731));
#155332=CARTESIAN_POINT('Ctrl Pts',(3.52267852308861,-6.06452449706262,
25.441159687157));
#155333=CARTESIAN_POINT('Ctrl Pts',(3.67048520232198,-5.97370613120828,
25.4490120459409));
#155334=CARTESIAN_POINT('Ctrl Pts',(3.81825698267394,-5.88290920862968,
25.4568625506914));
#155335=CARTESIAN_POINT('Ctrl Pts',(3.9627272155274,-5.78658254317813,25.4647130554418));
#155336=CARTESIAN_POINT('Ctrl Pts',(4.10344489977226,-5.68501244651523,
25.4725635601922));
#155337=CARTESIAN_POINT('Ctrl Pts',(4.24413994697689,-5.58345868927958,
25.4804128020438));
#155338=CARTESIAN_POINT('Ctrl Pts',(4.38108333969664,-5.47666340573365,
25.4882620438955));
#155339=CARTESIAN_POINT('Ctrl Pts',(4.51385409985741,-5.36495551963858,
25.4961112857471));
#155340=CARTESIAN_POINT('Ctrl Pts',(4.6466695930859,-5.25320999697032,25.503963172162));
#155341=CARTESIAN_POINT('Ctrl Pts',(4.77530935347403,-5.13654881153163,
25.5118150585768));
#155342=CARTESIAN_POINT('Ctrl Pts',(4.89938632362559,-5.01534048837869,
25.5196669449917));
#155343=CARTESIAN_POINT('Ctrl Pts',(4.9904944984531,-4.92633872533693,25.5254324874556));
#155344=CARTESIAN_POINT('Ctrl Pts',(5.07914321494458,-4.83488608072877,
25.5311980299196));
#155345=CARTESIAN_POINT('Ctrl Pts',(5.16519231646852,-4.74114067460507,
25.5369635723836));
#155346=CARTESIAN_POINT('Ctrl Pts',(5.30929502151379,-4.58414930143849,
25.5466188767435));
#155347=CARTESIAN_POINT('Ctrl Pts',(5.44603316626756,-4.4208075889074,25.5562741811034));
#155348=CARTESIAN_POINT('Ctrl Pts',(5.5749465792256,-4.25177577034359,25.5659294854633));
#155349=CARTESIAN_POINT('Ctrl Pts',(5.70457414830735,-4.0818075472152,25.5756382783981));
#155350=CARTESIAN_POINT('Ctrl Pts',(5.8262900652624,-3.90608606988243,25.5853470713328));
#155351=CARTESIAN_POINT('Ctrl Pts',(5.93967416463933,-3.72530500501852,
25.5950558642676));
#155352=CARTESIAN_POINT('Ctrl Pts',(6.05360387793019,-3.54365400631993,
25.6048113767383));
#155353=CARTESIAN_POINT('Ctrl Pts',(6.15912139122199,-3.3568946580016,25.6145668892091));
#155354=CARTESIAN_POINT('Ctrl Pts',(6.25584836090517,-3.16575233520566,
25.6243224016798));
#155355=CARTESIAN_POINT('Ctrl Pts',(6.35267110516921,-2.97442075210404,
25.6340875736087));
#155356=CARTESIAN_POINT('Ctrl Pts',(6.44068588851664,-2.77869755315185,
25.6438527455376));
#155357=CARTESIAN_POINT('Ctrl Pts',(6.51956111423719,-2.57933120018085,
25.6536179174666));
#155358=CARTESIAN_POINT('Ctrl Pts',(6.59832879537709,-2.38023667870864,
25.6633697748051));
#155359=CARTESIAN_POINT('Ctrl Pts',(6.66798181118765,-2.17750896648122,
25.6731216321437));
#155360=CARTESIAN_POINT('Ctrl Pts',(6.72823771591766,-1.97191374065986,
25.6828734894822));
#155361=CARTESIAN_POINT('Ctrl Pts',(6.75451365431931,-1.88225933229006,
25.6871260055448));
#155362=CARTESIAN_POINT('Ctrl Pts',(6.77900326126279,-1.79205989726403,
25.6913785216074));
#155363=CARTESIAN_POINT('Ctrl Pts',(6.80168598724666,-1.70138011431673,
25.69563103767));
#155364=CARTESIAN_POINT('Ctrl Pts',(6.84497028679044,-1.5283404677396,25.7037458991376));
#155365=CARTESIAN_POINT('Ctrl Pts',(6.88169100112746,-1.35347215330042,
25.7118607606052));
#155366=CARTESIAN_POINT('Ctrl Pts',(6.91169686818472,-1.17731600041179,
25.7199756220728));
#155367=CARTESIAN_POINT('Ctrl Pts',(6.94168248721917,-1.00127871806913,
25.7280850076147));
#155368=CARTESIAN_POINT('Ctrl Pts',(6.96496221977847,-0.823955678787677,
25.7361943931566));
#155369=CARTESIAN_POINT('Ctrl Pts',(6.98143534720324,-0.64590018990645,
25.7443037786985));
#155370=CARTESIAN_POINT('Ctrl Pts',(6.9978989439945,-0.46794771617018,25.7524084725034));
#155371=CARTESIAN_POINT('Ctrl Pts',(7.00756374903863,-0.289263992872046,
25.7605131663082));
#155372=CARTESIAN_POINT('Ctrl Pts',(7.01038060736483,-0.110409702395602,
25.7686178601131));
#155373=CARTESIAN_POINT('Ctrl Pts',(7.01095019807662,-0.0742439706399554,
25.7702566923789));
#155374=CARTESIAN_POINT('Ctrl Pts',(7.01123995951459,-0.0380712819292277,
25.7718955246447));
#155375=CARTESIAN_POINT('Ctrl Pts',(7.01124974356013,-0.001896293246826,
25.7735343569105));
#155376=CARTESIAN_POINT('Ctrl Pts',(7.01125,3.93647490780448E-12,25.7735343569105));
#155377=CARTESIAN_POINT('Ctrl Pts',(7.01124999999989,0.191008754744065,
25.7822061308426));
#155378=CARTESIAN_POINT('Ctrl Pts',(7.00344012880997,0.382017367486861,
25.7908779047747));
#155379=CARTESIAN_POINT('Ctrl Pts',(6.98784644419148,0.572388534913533,
25.7995496787068));
#155380=CARTESIAN_POINT('Ctrl Pts',(6.97225169663166,0.762772678964236,
25.8082220437492));
#155381=CARTESIAN_POINT('Ctrl Pts',(6.94887209704279,0.952519007630594,
25.8168944087915));
#155382=CARTESIAN_POINT('Ctrl Pts',(6.91778566246047,1.14099434299926,25.8255667738339));
#155383=CARTESIAN_POINT('Ctrl Pts',(6.88670108297135,1.32945843104044,25.83423862135));
#155384=CARTESIAN_POINT('Ctrl Pts',(6.84791063501091,1.51665139731177,25.8429104688661));
#155385=CARTESIAN_POINT('Ctrl Pts',(6.80154374572902,1.70194865887149,25.8515823163823));
#155386=CARTESIAN_POINT('Ctrl Pts',(6.75517597619818,1.88724943819406,25.8602543285285));
#155387=CARTESIAN_POINT('Ctrl Pts',(6.70123154646039,2.07065416525621,25.8689263406747));
#155388=CARTESIAN_POINT('Ctrl Pts',(6.63989045285471,2.25155087363996,25.8775983528209));
#155389=CARTESIAN_POINT('Ctrl Pts',(6.61790934153598,2.31637382429903,25.880705901988));
#155390=CARTESIAN_POINT('Ctrl Pts',(6.59497889661491,2.3808748601913,25.8838134511551));
#155391=CARTESIAN_POINT('Ctrl Pts',(6.57110895151813,2.4450263208764,25.8869210003222));
#155392=CARTESIAN_POINT('',(7.01124976619934,0.00181065449874002,25.226465446522));
#155393=CARTESIAN_POINT('Ctrl Pts',(6.57110895151814,2.44502632087636,25.3397663899914));
#155394=CARTESIAN_POINT('Ctrl Pts',(6.63790538062555,2.26550816620888,25.3310456149202));
#155395=CARTESIAN_POINT('Ctrl Pts',(6.69738434870032,2.08313550795474,25.3223248398489));
#155396=CARTESIAN_POINT('Ctrl Pts',(6.74931780320426,1.89850882374829,25.3136040647777));
#155397=CARTESIAN_POINT('Ctrl Pts',(6.8011622294282,1.71419864065453,25.3048982395227));
#155398=CARTESIAN_POINT('Ctrl Pts',(6.84548688543691,1.52764241001528,25.2961924142678));
#155399=CARTESIAN_POINT('Ctrl Pts',(6.88211327509476,1.33945639393918,25.2874865890128));
#155400=CARTESIAN_POINT('Ctrl Pts',(6.91869907638936,1.15147892045898,25.2787904113153));
#155401=CARTESIAN_POINT('Ctrl Pts',(6.94760357468004,0.961875534795149,
25.2700942336178));
#155402=CARTESIAN_POINT('Ctrl Pts',(6.96869864591293,0.771275401495021,
25.2613980559203));
#155403=CARTESIAN_POINT('Ctrl Pts',(6.98976139966878,0.580967266044245,
25.2527152006961));
#155404=CARTESIAN_POINT('Ctrl Pts',(7.00303857133397,0.389665704772105,
25.2440323454718));
#155405=CARTESIAN_POINT('Ctrl Pts',(7.00845342637586,0.198007911004861,
25.2353494902476));
#155406=CARTESIAN_POINT('Ctrl Pts',(7.01030015932765,0.132643139375614,
25.2323882078616));
#155407=CARTESIAN_POINT('Ctrl Pts',(7.01123282932787,0.0672370078704981,
25.2294269254756));
#155408=CARTESIAN_POINT('Ctrl Pts',(7.0112497650765,0.00181499715977043,
25.2264656430896));
#155409=CARTESIAN_POINT('Ctrl Pts',(7.01124976619934,0.00181065449874002,
25.226465446522));
#155410=CARTESIAN_POINT('Ctrl Pts',(7.01130034097044,-0.194025907512635,
25.2176010389394));
#155411=CARTESIAN_POINT('Ctrl Pts',(7.00314147806038,-0.389720306454623,
25.2087366313568));
#155412=CARTESIAN_POINT('Ctrl Pts',(6.98683502308065,-0.584604928779768,
25.1998722237742));
#155413=CARTESIAN_POINT('Ctrl Pts',(6.97050530574478,-0.779767568337832,
25.1909951704629));
#155414=CARTESIAN_POINT('Ctrl Pts',(6.94600479014023,-0.974117878634766,
25.1821181171515));
#155415=CARTESIAN_POINT('Ctrl Pts',(6.91344697393,-1.16699507332213,25.1732410638402));
#155416=CARTESIAN_POINT('Ctrl Pts',(6.88082450327225,-1.3602552902731,25.1643463821666));
#155417=CARTESIAN_POINT('Ctrl Pts',(6.84011276527309,-1.55203629727069,
25.1554517004931));
#155418=CARTESIAN_POINT('Ctrl Pts',(6.79147657483599,-1.74168668133912,
25.1465570188195));
#155419=CARTESIAN_POINT('Ctrl Pts',(6.74279912605188,-1.93149794686815,
25.1376547917387));
#155420=CARTESIAN_POINT('Ctrl Pts',(6.68618386337597,-2.11917474334998,
25.1287525646579));
#155421=CARTESIAN_POINT('Ctrl Pts',(6.62184551843366,-2.304080834628,25.1198503375771));
#155422=CARTESIAN_POINT('Ctrl Pts',(6.55742811921313,-2.48921412506071,
25.1109371720872));
#155423=CARTESIAN_POINT('Ctrl Pts',(6.48526874591048,-2.67156967222017,
25.1020240065974));
#155424=CARTESIAN_POINT('Ctrl Pts',(6.40563111334279,-2.85052917934105,
25.0931108411075));
#155425=CARTESIAN_POINT('Ctrl Pts',(6.33519090890342,-3.008820477833,25.0852270658235));
#155426=CARTESIAN_POINT('Ctrl Pts',(6.25890078141443,-3.1644550562951,25.0773432905396));
#155427=CARTESIAN_POINT('Ctrl Pts',(6.17697358078289,-3.31702034133199,
25.0694595152557));
#155428=CARTESIAN_POINT('Ctrl Pts',(6.0952640285474,-3.46918032032493,25.0615966840664));
#155429=CARTESIAN_POINT('Ctrl Pts',(6.00780935259729,-3.61854067465449,
25.0537338528771));
#155430=CARTESIAN_POINT('Ctrl Pts',(5.91483458551074,-3.76461928865935,
25.0458710216878));
#155431=CARTESIAN_POINT('Ctrl Pts',(5.82193125726022,-3.91058566053142,
25.0380142320465));
#155432=CARTESIAN_POINT('Ctrl Pts',(5.72351647602592,-4.0532749870423,25.0301574424051));
#155433=CARTESIAN_POINT('Ctrl Pts',(5.61986173967537,-4.19222859460609,
25.0223006527637));
#155434=CARTESIAN_POINT('Ctrl Pts',(5.51626545968907,-4.33110383891333,
25.0144482939797));
#155435=CARTESIAN_POINT('Ctrl Pts',(5.40743533019381,-4.46624725046369,
25.0065959351958));
#155436=CARTESIAN_POINT('Ctrl Pts',(5.29368667357636,-4.59722829153612,
24.9987435764118));
#155437=CARTESIAN_POINT('Ctrl Pts',(5.17996487434422,-4.72817840645615,
24.9908930716614));
#155438=CARTESIAN_POINT('Ctrl Pts',(5.06132710274201,-4.85496781377019,
24.983042566911));
#155439=CARTESIAN_POINT('Ctrl Pts',(4.9381295137889,-4.97719835525439,24.9751920621605));
#155440=CARTESIAN_POINT('Ctrl Pts',(4.81495174344497,-5.09940923369686,
24.9673428203089));
#155441=CARTESIAN_POINT('Ctrl Pts',(4.68721588895584,-5.2170624396675,24.9594935784573));
#155442=CARTESIAN_POINT('Ctrl Pts',(4.55531523916441,-5.3297963970809,24.9516443366056));
#155443=CARTESIAN_POINT('Ctrl Pts',(4.42337014946246,-5.44256833677102,
24.9437924501908));
#155444=CARTESIAN_POINT('Ctrl Pts',(4.28725775193319,-5.55041746926412,
24.935940563776));
#155445=CARTESIAN_POINT('Ctrl Pts',(4.14740486204788,-5.65302215392454,
24.9280886773611));
#155446=CARTESIAN_POINT('Ctrl Pts',(4.04471262571944,-5.72836349677554,
24.9223231348972));
#155447=CARTESIAN_POINT('Ctrl Pts',(3.94000430801992,-5.80087797357664,
24.9165575924333));
#155448=CARTESIAN_POINT('Ctrl Pts',(3.83345880483282,-5.87045314725786,
24.9107920499693));
#155449=CARTESIAN_POINT('Ctrl Pts',(3.6550316632605,-5.98696767854257,24.9011367456094));
#155450=CARTESIAN_POINT('Ctrl Pts',(3.47154285546835,-6.09517901204503,
24.8914814412495));
#155451=CARTESIAN_POINT('Ctrl Pts',(3.28371893132749,-6.19474103918327,
24.8818261368895));
#155452=CARTESIAN_POINT('Ctrl Pts',(3.09485449788327,-6.2948546212737,24.8721173439548));
#155453=CARTESIAN_POINT('Ctrl Pts',(2.90160685089553,-6.38622282673731,
24.8624085510201));
#155454=CARTESIAN_POINT('Ctrl Pts',(2.70472898748495,-6.46854447822373,
24.8526997580854));
#155455=CARTESIAN_POINT('Ctrl Pts',(2.50690373107783,-6.5512622684874,24.8429442456146));
#155456=CARTESIAN_POINT('Ctrl Pts',(2.3054132855391,-6.62484623516559,24.8331887331439));
#155457=CARTESIAN_POINT('Ctrl Pts',(2.10103509685722,-6.68904164169085,
24.8234332206731));
#155458=CARTESIAN_POINT('Ctrl Pts',(1.89645454232499,-6.75330061154502,
24.8136680487442));
#155459=CARTESIAN_POINT('Ctrl Pts',(1.68898056530443,-6.80815242605906,
24.8039028768152));
#155460=CARTESIAN_POINT('Ctrl Pts',(1.47940575001441,-6.8533922395646,24.7941377048862));
#155461=CARTESIAN_POINT('Ctrl Pts',(1.27011668523058,-6.89857036961076,
24.7843858475476));
#155462=CARTESIAN_POINT('Ctrl Pts',(1.05873254427478,-6.93416268435699,
24.774633990209));
#155463=CARTESIAN_POINT('Ctrl Pts',(0.846054864332172,-6.96001564143644,
24.7648821328705));
#155464=CARTESIAN_POINT('Ctrl Pts',(0.753311993030767,-6.97128940308283,
24.7606296168079));
#155465=CARTESIAN_POINT('Ctrl Pts',(0.660323296768818,-6.98071178572341,
24.7563771007454));
#155466=CARTESIAN_POINT('Ctrl Pts',(0.567155942728443,-6.98827308418381,
24.7521245846828));
#155467=CARTESIAN_POINT('Ctrl Pts',(0.391161874200898,-7.0025564530001,
24.744091539084));
#155468=CARTESIAN_POINT('Ctrl Pts',(0.214444101747245,-7.01020201969531,
24.7360584934852));
#155469=CARTESIAN_POINT('Ctrl Pts',(0.0375509995440148,-7.01114944106409,
24.7280254478864));
#155470=CARTESIAN_POINT('Ctrl Pts',(-0.139228388962544,-7.01209625339393,
24.7199975662386));
#155471=CARTESIAN_POINT('Ctrl Pts',(-0.316182517834179,-7.00635348929287,
24.7119696845908));
#155472=CARTESIAN_POINT('Ctrl Pts',(-0.492759034396457,-6.99391271725067,
24.7039418029429));
#155473=CARTESIAN_POINT('Ctrl Pts',(-0.669255824920628,-6.98147756233971,
24.6959175459628));
#155474=CARTESIAN_POINT('Ctrl Pts',(-0.845374977707885,-6.96235044675952,
24.6878932889827));
#155475=CARTESIAN_POINT('Ctrl Pts',(-1.02056533453558,-6.93657501656576,
24.6798690320026));
#155476=CARTESIAN_POINT('Ctrl Pts',(-1.1957345090647,-6.91080270288405,
24.6718457452369));
#155477=CARTESIAN_POINT('Ctrl Pts',(-1.36997474774258,-6.87838372141819,
24.6638224584712));
#155478=CARTESIAN_POINT('Ctrl Pts',(-1.54274102339802,-6.83941347611218,
24.6557991717055));
#155479=CARTESIAN_POINT('Ctrl Pts',(-1.71549314239819,-6.80044642407017,
24.6477765423766));
#155480=CARTESIAN_POINT('Ctrl Pts',(-1.88677118217955,-6.75492926207253,
24.6397539130477));
#155481=CARTESIAN_POINT('Ctrl Pts',(-2.05604160109105,-6.70300824235529,
24.6317312837188));
#155482=CARTESIAN_POINT('Ctrl Pts',(-2.22537565362933,-6.65106770403101,
24.6237056384524));
#155483=CARTESIAN_POINT('Ctrl Pts',(-2.3927002278046,-6.5927186092541,24.615679993186));
#155484=CARTESIAN_POINT('Ctrl Pts',(-2.5574978394213,-6.52815681213736,
24.6076543479196));
#155485=CARTESIAN_POINT('Ctrl Pts',(-2.65467255350088,-6.49008724235576,
24.6029219384119));
#155486=CARTESIAN_POINT('Ctrl Pts',(-2.75096898407471,-6.44985844336345,
24.5981895289042));
#155487=CARTESIAN_POINT('Ctrl Pts',(-2.84628447904216,-6.40751833605365,
24.5934571193964));
#155488=CARTESIAN_POINT('Ctrl Pts',(-3.02211645732037,-6.32941199215503,
24.5847270705618));
#155489=CARTESIAN_POINT('Ctrl Pts',(-3.19469706244835,-6.24407939971261,
24.5759970217271));
#155490=CARTESIAN_POINT('Ctrl Pts',(-3.36345017752334,-6.15181513586179,
24.5672669728924));
#155491=CARTESIAN_POINT('Ctrl Pts',(-3.53225208777275,-6.05952419368361,
24.5585343997532));
#155492=CARTESIAN_POINT('Ctrl Pts',(-3.69722405852661,-5.96029771081905,
24.549801826614));
#155493=CARTESIAN_POINT('Ctrl Pts',(-3.8578156658095,-5.85447562563333,
24.5410692534748));
#155494=CARTESIAN_POINT('Ctrl Pts',(-4.02068873322492,-5.74715016880462,
24.5322126201944));
#155495=CARTESIAN_POINT('Ctrl Pts',(-4.17905578646859,-5.63304043873814,
24.523355986914));
#155496=CARTESIAN_POINT('Ctrl Pts',(-4.33237374851257,-5.51254607832888,
24.5144993536336));
#155497=CARTESIAN_POINT('Ctrl Pts',(-4.48364032625899,-5.3936639245756,
24.5057612215268));
#155498=CARTESIAN_POINT('Ctrl Pts',(-4.62999188266194,-5.26856712115267,
24.4970230894201));
#155499=CARTESIAN_POINT('Ctrl Pts',(-4.77094005590083,-5.13768017158533,
24.4882849573133));
#155500=CARTESIAN_POINT('Ctrl Pts',(-4.914755407802,-5.00413070954728,24.4793690734461));
#155501=CARTESIAN_POINT('Ctrl Pts',(-5.05294497010798,-4.86455320968231,
24.4704531895789));
#155502=CARTESIAN_POINT('Ctrl Pts',(-5.18502865944739,-4.7194389881859,
24.4615373057117));
#155503=CARTESIAN_POINT('Ctrl Pts',(-5.31711234878681,-4.57432476668949,
24.4526214218445));
#155504=CARTESIAN_POINT('Ctrl Pts',(-5.44308996609738,-4.4236740512991,
24.4437055379772));
#155505=CARTESIAN_POINT('Ctrl Pts',(-5.56252360649249,-4.26801566184027,
24.43478965411));
#155506=CARTESIAN_POINT('Ctrl Pts',(-5.6796103456734,-4.11541599906859,
24.4260489696138));
#155507=CARTESIAN_POINT('Ctrl Pts',(-5.79042033807267,-3.95798743193461,
24.4173082851176));
#155508=CARTESIAN_POINT('Ctrl Pts',(-5.8945786984682,-3.79625717385756,
24.4085676006214));
#155509=CARTESIAN_POINT('Ctrl Pts',(-5.99871831904458,-3.63455601374034,
24.3998284887195));
#155510=CARTESIAN_POINT('Ctrl Pts',(-6.09620854940289,-3.4685549384139,
24.3910893768176));
#155511=CARTESIAN_POINT('Ctrl Pts',(-6.18671818027138,-3.29880959141318,
24.3823502649158));
#155512=CARTESIAN_POINT('Ctrl Pts',(-6.27840049367379,-3.12686494913601,
24.3734979252414));
#155513=CARTESIAN_POINT('Ctrl Pts',(-6.36291990525879,-2.95107857488779,
24.3646455855671));
#155514=CARTESIAN_POINT('Ctrl Pts',(-6.43997990604259,-2.77205435954413,
24.3557932458927));
#155515=CARTESIAN_POINT('Ctrl Pts',(-6.51601526207242,-2.59541057790436,
24.347058613243));
#155516=CARTESIAN_POINT('Ctrl Pts',(-6.58478824835879,-2.41561478928434,
24.3383239805932));
#155517=CARTESIAN_POINT('Ctrl Pts',(-6.64606178443819,-2.23326875228448,
24.3295893479435));
#155518=CARTESIAN_POINT('Ctrl Pts',(-6.70857389446358,-2.04723680020555,
24.3206781547568));
#155519=CARTESIAN_POINT('Ctrl Pts',(-6.7632800266861,-1.8585506693559,24.3117669615702));
#155520=CARTESIAN_POINT('Ctrl Pts',(-6.80998104715273,-1.66786831012541,
24.3028557683836));
#155521=CARTESIAN_POINT('Ctrl Pts',(-6.85668206761938,-1.47718595089489,
24.2939445751969));
#155522=CARTESIAN_POINT('Ctrl Pts',(-6.89537789113301,-1.28450765450624,
24.2850333820103));
#155523=CARTESIAN_POINT('Ctrl Pts',(-6.92592396116732,-1.09050623410796,
24.2761221888236));
#155524=CARTESIAN_POINT('Ctrl Pts',(-6.95343458915158,-0.915783237041549,
24.2680965239712));
#155525=CARTESIAN_POINT('Ctrl Pts',(-6.97434683907059,-0.739906637125955,
24.2600708591188));
#155526=CARTESIAN_POINT('Ctrl Pts',(-6.9885750816751,-0.563422479396998,
24.2520451942664));
#155527=CARTESIAN_POINT('Ctrl Pts',(-7.00279880858434,-0.386994333411741,
24.2440220765632));
#155528=CARTESIAN_POINT('Ctrl Pts',(-7.0103427221453,-0.209959378457967,
24.23599895886));
#155529=CARTESIAN_POINT('Ctrl Pts',(-7.01117295096849,-0.0328696532956069,
24.2279758411568));
#155530=CARTESIAN_POINT('Ctrl Pts',(-7.01200307509257,0.144197739303647,
24.2199537352389));
#155531=CARTESIAN_POINT('Ctrl Pts',(-7.00612119979062,0.321319521888407,
24.211931629321));
#155532=CARTESIAN_POINT('Ctrl Pts',(-6.9935455602307,0.497942827518838,
24.2039095234031));
#155533=CARTESIAN_POINT('Ctrl Pts',(-6.98096524752066,0.674631766966055,
24.1958844364435));
#155534=CARTESIAN_POINT('Ctrl Pts',(-6.96168622452858,0.85082149321643,
24.187859349484));
#155535=CARTESIAN_POINT('Ctrl Pts',(-6.9357787249994,1.02596298195681,24.1798342625244));
#155536=CARTESIAN_POINT('Ctrl Pts',(-6.90986612311783,1.201138963937,24.1718075950642));
#155537=CARTESIAN_POINT('Ctrl Pts',(-6.87732250639086,1.37526593580663,
24.1637809276039));
#155538=CARTESIAN_POINT('Ctrl Pts',(-6.83826936653071,1.54780445575909,
24.1557542601437));
#155539=CARTESIAN_POINT('Ctrl Pts',(-6.79918487494756,1.72048148902712,
24.1477211489031));
#155540=CARTESIAN_POINT('Ctrl Pts',(-6.75358051292866,1.89156716807226,
24.1396880376624));
#155541=CARTESIAN_POINT('Ctrl Pts',(-6.70162800408928,2.06053601213529,
24.1316549264218));
#155542=CARTESIAN_POINT('Ctrl Pts',(-6.67101569860373,2.16009859318383,
24.1269215254603));
#155543=CARTESIAN_POINT('Ctrl Pts',(-6.63820025694798,2.25892652538069,
24.1221881244987));
#155544=CARTESIAN_POINT('Ctrl Pts',(-6.60322465143547,2.35691551931225,
24.1174547235371));
#155545=CARTESIAN_POINT('Ctrl Pts',(-6.5311738155657,2.55877589643372,24.1077037702429));
#155546=CARTESIAN_POINT('Ctrl Pts',(-6.44991144028197,2.75719415864556,
24.0979528169488));
#155547=CARTESIAN_POINT('Ctrl Pts',(-6.35977319226589,2.95142533455213,
24.0882018636546));
#155548=CARTESIAN_POINT('Ctrl Pts',(-6.26950508319346,3.14593633690568,
24.0784368622829));
#155549=CARTESIAN_POINT('Ctrl Pts',(-6.17033553916897,3.33624815156836,
24.0686718609112));
#155550=CARTESIAN_POINT('Ctrl Pts',(-6.0626476800497,3.52163735641364,24.0589068595395));
#155551=CARTESIAN_POINT('Ctrl Pts',(-5.95513931428039,3.7067175558641,24.0491581344019));
#155552=CARTESIAN_POINT('Ctrl Pts',(-5.83914102902578,3.88689151112113,
24.0394094092644));
#155553=CARTESIAN_POINT('Ctrl Pts',(-5.71507941112824,4.0614645002755,24.0296606841268));
#155554=CARTESIAN_POINT('Ctrl Pts',(-5.59135829426732,4.23555835426478,
24.0199387154597));
#155555=CARTESIAN_POINT('Ctrl Pts',(-5.45961804826436,4.40408189824422,
24.0102167467926));
#155556=CARTESIAN_POINT('Ctrl Pts',(-5.32032672708516,4.56637165368341,
24.0004947781255));
#155557=CARTESIAN_POINT('Ctrl Pts',(-5.1819570601973,4.72758758019861,23.9908371371859));
#155558=CARTESIAN_POINT('Ctrl Pts',(-5.03613592331542,4.88265188598419,
23.9811794962462));
#155559=CARTESIAN_POINT('Ctrl Pts',(-4.88336645422707,5.03094013443112,
23.9715218553065));
#155560=CARTESIAN_POINT('Ctrl Pts',(-4.81621901303099,5.09611792487628,
23.9672769896213));
#155561=CARTESIAN_POINT('Ctrl Pts',(-4.7477297973509,5.15998698885246,23.963032123936));
#155562=CARTESIAN_POINT('Ctrl Pts',(-4.67794426613782,5.22249595551862,
23.9587872582507));
#155563=CARTESIAN_POINT('Ctrl Pts',(-4.54886001342004,5.33812054287933,
23.9509354112368));
#155564=CARTESIAN_POINT('Ctrl Pts',(-4.41539090845914,5.44904124456702,
23.9430835642229));
#155565=CARTESIAN_POINT('Ctrl Pts',(-4.27793297718134,5.55490017959319,
23.935231717209));
#155566=CARTESIAN_POINT('Ctrl Pts',(-4.14051402786141,5.66072909388133,
23.9273820969154));
#155567=CARTESIAN_POINT('Ctrl Pts',(-3.99910880430221,5.76149886439373,
23.9195324766218));
#155568=CARTESIAN_POINT('Ctrl Pts',(-3.85414661408788,5.8568917046173,23.9116828563283));
#155569=CARTESIAN_POINT('Ctrl Pts',(-3.70919599725087,5.95227692894233,
23.9038338627265));
#155570=CARTESIAN_POINT('Ctrl Pts',(-3.56068929815195,6.04228586848726,
23.8959848691247));
#155571=CARTESIAN_POINT('Ctrl Pts',(-3.40908478908445,6.12664406207289,
23.8881358755229));
#155572=CARTESIAN_POINT('Ctrl Pts',(-3.25740352709307,6.21104496374189,
23.8802829082055));
#155573=CARTESIAN_POINT('Ctrl Pts',(-3.10262165529976,6.28978921769403,
23.8724299408881));
#155574=CARTESIAN_POINT('Ctrl Pts',(-2.94522233259348,6.36264818877271,
23.8645769735707));
#155575=CARTESIAN_POINT('Ctrl Pts',(-2.7877830357479,6.43552566358196,23.8567220118634));
#155576=CARTESIAN_POINT('Ctrl Pts',(-2.62772531559183,6.50251473050419,
23.8488670501562));
#155577=CARTESIAN_POINT('Ctrl Pts',(-2.46555167507444,6.56343519051096,
23.8410120884489));
#155578=CARTESIAN_POINT('Ctrl Pts',(-2.30321706366306,6.62441611916651,
23.8331493300356));
#155579=CARTESIAN_POINT('Ctrl Pts',(-2.13876269887763,6.67931628950445,
23.8252865716223));
#155580=CARTESIAN_POINT('Ctrl Pts',(-1.97270613491372,6.72800543012368,
23.817423813209));
#155581=CARTESIAN_POINT('Ctrl Pts',(-1.85088942235821,6.7637230850348,23.8116558064608));
#155582=CARTESIAN_POINT('Ctrl Pts',(-1.72821079585807,6.79609933591454,
23.8058877997125));
#155583=CARTESIAN_POINT('Ctrl Pts',(-1.60487744077216,6.82510036282256,
23.8001197929643));
#155584=CARTESIAN_POINT('Ctrl Pts',(-1.42573495907763,6.86722453862539,
23.7917417265233));
#155585=CARTESIAN_POINT('Ctrl Pts',(-1.24481405199267,6.90231937438808,
23.7833636600822));
#155586=CARTESIAN_POINT('Ctrl Pts',(-1.06269237914367,6.93024613342196,
23.7749855936412));
#155587=CARTESIAN_POINT('Ctrl Pts',(-0.880695238931423,6.9581537964697,
23.7666132560225));
#155588=CARTESIAN_POINT('Ctrl Pts',(-0.6974992938152,6.9789031051554,23.7582409184038));
#155589=CARTESIAN_POINT('Ctrl Pts',(-0.513692558391576,6.99240634674167,
23.749868580785));
#155590=CARTESIAN_POINT('Ctrl Pts',(-0.329984552450935,7.00590233523104,
23.7415007402625));
#155591=CARTESIAN_POINT('Ctrl Pts',(-0.145666737467837,7.01215999313698,
23.7331328997399));
#155592=CARTESIAN_POINT('Ctrl Pts',(0.0386671219871292,7.01114337438461,
23.7247650592174));
#155593=CARTESIAN_POINT('Ctrl Pts',(0.222928972394616,7.01012715276899,
23.7164004875475));
#155594=CARTESIAN_POINT('Ctrl Pts',(0.407206526552163,7.00184232297608,
23.7080359158776));
#155595=CARTESIAN_POINT('Ctrl Pts',(0.590904923462759,6.98630502726065,
23.6996713442077));
#155596=CARTESIAN_POINT('Ctrl Pts',(0.774558448575304,6.97077152682275,
23.6913088157421));
#155597=CARTESIAN_POINT('Ctrl Pts',(0.957632771375497,6.9479891214706,23.6829462872766));
#155598=CARTESIAN_POINT('Ctrl Pts',(1.13953659797897,6.91802593984487,23.6745837588111));
#155599=CARTESIAN_POINT('Ctrl Pts',(1.32145494107814,6.8880603670633,23.6662205629896));
#155600=CARTESIAN_POINT('Ctrl Pts',(1.50220227608055,6.8509129205959,23.6578573671681));
#155601=CARTESIAN_POINT('Ctrl Pts',(1.68119520104314,6.80670325917691,23.6494941713466));
#155602=CARTESIAN_POINT('Ctrl Pts',(1.86020033296453,6.7624905827476,23.6411304051719));
#155603=CARTESIAN_POINT('Ctrl Pts',(2.0374504969865,6.71121480962573,23.6327666389972));
#155604=CARTESIAN_POINT('Ctrl Pts',(2.21237503715055,6.65304616378792,23.6244028728225));
#155605=CARTESIAN_POINT('Ctrl Pts',(2.38733482837268,6.59486579571656,23.616037421169));
#155606=CARTESIAN_POINT('Ctrl Pts',(2.55996774922694,6.52978988886511,23.6076719695155));
#155607=CARTESIAN_POINT('Ctrl Pts',(2.72972038080205,6.45803787578967,23.5993065178619));
#155608=CARTESIAN_POINT('Ctrl Pts',(2.89952986220081,6.38626183310566,23.5909382646351));
#155609=CARTESIAN_POINT('Ctrl Pts',(3.06645682815355,6.30780535387567,23.5825700114082));
#155610=CARTESIAN_POINT('Ctrl Pts',(3.22996944406444,6.22293531646522,23.5742017581813));
#155611=CARTESIAN_POINT('Ctrl Pts',(3.39363365949794,6.13798659242204,23.5658257463898));
#155612=CARTESIAN_POINT('Ctrl Pts',(3.55387690697908,6.04661257937223,23.5574497345983));
#155613=CARTESIAN_POINT('Ctrl Pts',(3.7101924127613,5.94912588728701,23.5490737228068));
#155614=CARTESIAN_POINT('Ctrl Pts',(3.86658457759864,5.85159138652367,23.5406936033157));
#155615=CARTESIAN_POINT('Ctrl Pts',(4.01904488415931,5.74793840808889,23.5323134838245));
#155616=CARTESIAN_POINT('Ctrl Pts',(4.16709647387925,5.63852228335432,23.5239333643334));
#155617=CARTESIAN_POINT('Ctrl Pts',(4.31531723129459,5.52898113683716,23.5155436694942));
#155618=CARTESIAN_POINT('Ctrl Pts',(4.45911894529113,5.41366388626498,23.507153974655));
#155619=CARTESIAN_POINT('Ctrl Pts',(4.59805767416841,5.2929662938206,23.4987642798158));
#155620=CARTESIAN_POINT('Ctrl Pts',(4.68626747550549,5.21633747522254,23.493437807341));
#155621=CARTESIAN_POINT('Ctrl Pts',(4.77251783042629,5.13754074700647,23.4881113348662));
#155622=CARTESIAN_POINT('Ctrl Pts',(4.85670300396736,5.05668493123256,23.4827848623915));
#155623=CARTESIAN_POINT('Ctrl Pts',(4.9891814242929,4.9294457714459,23.4744028322823));
#155624=CARTESIAN_POINT('Ctrl Pts',(5.1168110448189,4.79684904428586,23.4660208021732));
#155625=CARTESIAN_POINT('Ctrl Pts',(5.23914763292184,4.65928735354984,23.457638772064));
#155626=CARTESIAN_POINT('Ctrl Pts',(5.36132838271575,4.52190089560071,23.4492674193934));
#155627=CARTESIAN_POINT('Ctrl Pts',(5.47822932135505,4.37956232150529,23.4408960667228));
#155628=CARTESIAN_POINT('Ctrl Pts',(5.58944166541492,4.23270226113575,23.4325247140521));
#155629=CARTESIAN_POINT('Ctrl Pts',(5.70048456162258,4.08606596299347,23.4241661163301));
#155630=CARTESIAN_POINT('Ctrl Pts',(5.80585595371169,3.93492217855557,23.415807518608));
#155631=CARTESIAN_POINT('Ctrl Pts',(5.90518623718454,3.77973571386497,23.407448920886));
#155632=CARTESIAN_POINT('Ctrl Pts',(6.00442800788643,3.62468753513838,23.3990977714729));
#155633=CARTESIAN_POINT('Ctrl Pts',(6.09763922092593,3.46560412870264,23.3907466220599));
#155634=CARTESIAN_POINT('Ctrl Pts',(6.18449185087015,3.30298154839241,23.3823954726469));
#155635=CARTESIAN_POINT('Ctrl Pts',(6.2712577169811,3.14052142439988,23.3740526658452));
#155636=CARTESIAN_POINT('Ctrl Pts',(6.35167751446895,2.9745294654463,23.3657098590435));
#155637=CARTESIAN_POINT('Ctrl Pts',(6.4254676812057,2.80552876304647,23.3573670522418));
#155638=CARTESIAN_POINT('Ctrl Pts',(6.47731514597153,2.68678315844126,23.3515051142516));
#155639=CARTESIAN_POINT('Ctrl Pts',(6.52589050575783,2.56655275647024,23.3456431762613));
#155640=CARTESIAN_POINT('Ctrl Pts',(6.57110895151814,2.44502632087637,23.3397812382711));
#155641=CARTESIAN_POINT('Origin',(0.,0.,50.));
#155642=CARTESIAN_POINT('',(6.57110895151816,2.44502632087631,21.3399745565681));
#155643=CARTESIAN_POINT('',(6.57110895151813,2.44502632087638,21.886801314899));
#155644=CARTESIAN_POINT('',(6.57110895151814,2.44502632087636,50.));
#155645=CARTESIAN_POINT('',(7.01124999042383,0.000366444892493489,23.7735343569435));
#155646=CARTESIAN_POINT('Ctrl Pts',(6.57110895151813,2.44502632087638,21.886801314899));
#155647=CARTESIAN_POINT('Ctrl Pts',(6.56903774075831,2.45059278510957,21.8870715001979));
#155648=CARTESIAN_POINT('Ctrl Pts',(6.56695953073157,2.45615641900482,21.8873416854967));
#155649=CARTESIAN_POINT('Ctrl Pts',(6.56487433029739,2.46171720347857,21.8876118707956));
#155650=CARTESIAN_POINT('Ctrl Pts',(6.48961971012513,2.66240521244526,21.8973628240897));
#155651=CARTESIAN_POINT('Ctrl Pts',(6.40520950384978,2.85950492703563,21.9071137773838));
#155652=CARTESIAN_POINT('Ctrl Pts',(6.31199119297193,3.0522768128636,21.9168647306779));
#155653=CARTESIAN_POINT('Ctrl Pts',(6.21863858362937,3.2453264227574,21.9266297320495));
#155654=CARTESIAN_POINT('Ctrl Pts',(6.11645250331447,3.434035697175,21.9363947334211));
#155655=CARTESIAN_POINT('Ctrl Pts',(6.00582753770331,3.61768740355832,21.9461597347927));
#155656=CARTESIAN_POINT('Ctrl Pts',(5.89538696098912,3.80103300059845,21.9559084599303));
#155657=CARTESIAN_POINT('Ctrl Pts',(5.77653563050745,3.97933784511388,21.9656571850678));
#155658=CARTESIAN_POINT('Ctrl Pts',(5.64971113660622,4.15191409297058,21.9754059102054));
#155659=CARTESIAN_POINT('Ctrl Pts',(5.52323472676498,4.32401668594277,21.9851278788725));
#155660=CARTESIAN_POINT('Ctrl Pts',(5.38882886346775,4.49042203803086,21.9948498475396));
#155661=CARTESIAN_POINT('Ctrl Pts',(5.24697210164763,4.6504742045335,22.0045718162067));
#155662=CARTESIAN_POINT('Ctrl Pts',(5.10605396896906,4.80946734765424,22.0142294571464));
#155663=CARTESIAN_POINT('Ctrl Pts',(4.957783222508,4.96219104795769,22.0238870980861));
#155664=CARTESIAN_POINT('Ctrl Pts',(4.80267287516415,5.10802895613,22.0335447390258));
#155665=CARTESIAN_POINT('Ctrl Pts',(4.73449653738069,5.17212973766682,22.0377896047112));
#155666=CARTESIAN_POINT('Ctrl Pts',(4.66499942543247,5.23490060216006,22.0420344703966));
#155667=CARTESIAN_POINT('Ctrl Pts',(4.59422781015614,5.29629090882364,22.0462793360821));
#155668=CARTESIAN_POINT('Ctrl Pts',(4.46331957011812,5.40984627942447,22.054131183096));
#155669=CARTESIAN_POINT('Ctrl Pts',(4.32810190270302,5.51862856870388,22.0619830301099));
#155670=CARTESIAN_POINT('Ctrl Pts',(4.18897647988422,5.62228624435619,22.0698348771238));
#155671=CARTESIAN_POINT('Ctrl Pts',(4.04989051191047,5.72591452352978,22.0776844974174));
#155672=CARTESIAN_POINT('Ctrl Pts',(3.9068992985402,5.82442085224993,22.085534117711));
#155673=CARTESIAN_POINT('Ctrl Pts',(3.7604371510249,5.91749431733498,22.0933837380046));
#155674=CARTESIAN_POINT('Ctrl Pts',(3.61398669663878,6.01056035169428,22.1012327316064));
#155675=CARTESIAN_POINT('Ctrl Pts',(3.46406618211453,6.09819418192184,22.1090817252082));
#155676=CARTESIAN_POINT('Ctrl Pts',(3.31113819015592,6.18012867569851,22.1169307188101));
#155677=CARTESIAN_POINT('Ctrl Pts',(3.15813277523306,6.26210465051015,22.1247836861275));
#155678=CARTESIAN_POINT('Ctrl Pts',(3.0021171773325,6.3383753432974,22.1326366534449));
#155679=CARTESIAN_POINT('Ctrl Pts',(2.84357813321102,6.40871983806627,22.1404896207624));
#155680=CARTESIAN_POINT('Ctrl Pts',(2.68499882549949,6.47908219797313,22.1483445824696));
#155681=CARTESIAN_POINT('Ctrl Pts',(2.523895149032,6.54351521976674,22.1561995441769));
#155682=CARTESIAN_POINT('Ctrl Pts',(2.36077241124134,6.6018467253354,22.1640545058842));
#155683=CARTESIAN_POINT('Ctrl Pts',(2.19748776049796,6.66023612979928,22.1719172642975));
#155684=CARTESIAN_POINT('Ctrl Pts',(2.03218040931206,6.71251180716714,22.1797800227109));
#155685=CARTESIAN_POINT('Ctrl Pts',(1.86536991978293,6.75855174019324,22.1876427811242));
#155686=CARTESIAN_POINT('Ctrl Pts',(1.74300013825431,6.79232597442694,22.1934107878723));
#155687=CARTESIAN_POINT('Ctrl Pts',(1.61982173543324,6.82274550924742,22.1991787946204));
#155688=CARTESIAN_POINT('Ctrl Pts',(1.49604240872844,6.84977982666494,22.2049468013685));
#155689=CARTESIAN_POINT('Ctrl Pts',(1.31625215042091,6.88904734444081,22.2133248678095));
#155690=CARTESIAN_POINT('Ctrl Pts',(1.1347955745208,6.92125810630837,22.2217029342505));
#155691=CARTESIAN_POINT('Ctrl Pts',(0.952252475682128,6.94628258747492,
22.2300810006915));
#155692=CARTESIAN_POINT('Ctrl Pts',(0.769834197645309,6.97128995719861,
22.2384533383103));
#155693=CARTESIAN_POINT('Ctrl Pts',(0.586331202535501,6.98912079856643,
22.246825675929));
#155694=CARTESIAN_POINT('Ctrl Pts',(0.402332826542288,6.99969676908839,
22.2551980135478));
#155695=CARTESIAN_POINT('Ctrl Pts',(0.218433282969056,7.01026705886043,
22.2635658540703));
#155696=CARTESIAN_POINT('Ctrl Pts',(0.0340392165147784,7.01359022894086,
22.2719336945929));
#155697=CARTESIAN_POINT('Ctrl Pts',(-0.150255111329594,7.00963978846412,
22.2803015351155));
#155698=CARTESIAN_POINT('Ctrl Pts',(-0.334477445569004,7.00569089120608,
22.2886661067855));
#155699=CARTESIAN_POINT('Ctrl Pts',(-0.518599790742253,6.99447405657695,
22.2970306784554));
#155700=CARTESIAN_POINT('Ctrl Pts',(-0.702027618134933,6.97601489289378,
22.3053952501253));
#155701=CARTESIAN_POINT('Ctrl Pts',(-0.88541063982203,6.95756023820941,
22.3137577785909));
#155702=CARTESIAN_POINT('Ctrl Pts',(-1.06809915534767,6.9318668157454,22.3221203070565));
#155703=CARTESIAN_POINT('Ctrl Pts',(-1.24950303009968,6.89901215684331,
22.3304828355221));
#155704=CARTESIAN_POINT('Ctrl Pts',(-1.43092138144848,6.86615487603664,
22.3388460313436));
#155705=CARTESIAN_POINT('Ctrl Pts',(-1.61105456272152,6.82613526966641,
22.3472092271651));
#155706=CARTESIAN_POINT('Ctrl Pts',(-1.78932115042715,6.77908226702804,
22.3555724229866));
#155707=CARTESIAN_POINT('Ctrl Pts',(-1.96759989555667,6.73202605546923,
22.3639361891613));
#155708=CARTESIAN_POINT('Ctrl Pts',(-2.14401147529566,6.67793557489219,
22.372299955336));
#155709=CARTESIAN_POINT('Ctrl Pts',(-2.31798801534422,6.61699011055786,
22.3806637215107));
#155710=CARTESIAN_POINT('Ctrl Pts',(-2.49199961540934,6.55603236440101,
22.3890291731643));
#155711=CARTESIAN_POINT('Ctrl Pts',(-2.66357488699754,6.48821698860045,
22.3973946248178));
#155712=CARTESIAN_POINT('Ctrl Pts',(-2.83216397390128,6.41377219640951,
22.4057600764714));
#155713=CARTESIAN_POINT('Ctrl Pts',(-3.00080952095862,6.3393024728041,22.4141283296982));
#155714=CARTESIAN_POINT('Ctrl Pts',(-3.16646658852308,6.25819903846777,
22.4224965829251));
#155715=CARTESIAN_POINT('Ctrl Pts',(-3.32860765713966,6.17073720290625,
22.430864836152));
#155716=CARTESIAN_POINT('Ctrl Pts',(-3.49089905365884,6.08319427774534,
22.4392408479434));
#155717=CARTESIAN_POINT('Ctrl Pts',(-3.64966764744425,5.98928132735308,
22.4476168597349));
#155718=CARTESIAN_POINT('Ctrl Pts',(-3.80441170460284,5.8893189881667,22.4559928715264));
#155719=CARTESIAN_POINT('Ctrl Pts',(-3.95923165015915,5.78930762621401,
22.4643729910175));
#155720=CARTESIAN_POINT('Ctrl Pts',(-4.11002285073835,5.6832411430872,22.4727531105087));
#155721=CARTESIAN_POINT('Ctrl Pts',(-4.25631416381568,5.57148241506711,
22.4811332299998));
#155722=CARTESIAN_POINT('Ctrl Pts',(-4.40277263324938,5.45959598854343,
22.4895229248391));
#155723=CARTESIAN_POINT('Ctrl Pts',(-4.5447206836691,5.34200452537568,22.4979126196783));
#155724=CARTESIAN_POINT('Ctrl Pts',(-4.68172072876112,5.21911080361286,
22.5063023145175));
#155725=CARTESIAN_POINT('Ctrl Pts',(-4.76869969321592,5.14108770041062,
22.5116287869921));
#155726=CARTESIAN_POINT('Ctrl Pts',(-4.85368495392768,5.06092814974724,
22.5169552594667));
#155727=CARTESIAN_POINT('Ctrl Pts',(-4.93657252139366,4.97874264282871,
22.5222817319414));
#155728=CARTESIAN_POINT('Ctrl Pts',(-5.066997602171,4.8494222669717,22.5306630323462));
#155729=CARTESIAN_POINT('Ctrl Pts',(-5.19249008304699,4.71482309815738,
22.5390443327511));
#155730=CARTESIAN_POINT('Ctrl Pts',(-5.31261214947924,4.57534465496378,
22.547425633156));
#155731=CARTESIAN_POINT('Ctrl Pts',(-5.43258197877688,4.43604298027876,
22.5557963114895));
#155732=CARTESIAN_POINT('Ctrl Pts',(-5.54719474562594,4.29187460107555,
22.5641669898231));
#155733=CARTESIAN_POINT('Ctrl Pts',(-5.65604866497901,4.14327648870905,
22.5725376681566));
#155734=CARTESIAN_POINT('Ctrl Pts',(-5.76477905382293,3.99484700968703,
22.5808988472075));
#155735=CARTESIAN_POINT('Ctrl Pts',(-5.86776342830181,3.84199807955139,
22.5892600262583));
#155736=CARTESIAN_POINT('Ctrl Pts',(-5.96463929270588,3.68520076392171,
22.5976212053091));
#155737=CARTESIAN_POINT('Ctrl Pts',(-6.06138944924839,3.5286069113049,22.6059715347438));
#155738=CARTESIAN_POINT('Ctrl Pts',(-6.15204673458099,3.36807516997443,
22.6143218641785));
#155739=CARTESIAN_POINT('Ctrl Pts',(-6.23629115844561,3.20410660708928,
22.6226721936132));
#155740=CARTESIAN_POINT('Ctrl Pts',(-6.32047076126546,3.04026420820486,
22.6310160979689));
#155741=CARTESIAN_POINT('Ctrl Pts',(-6.39824718670623,2.87299054782822,
22.6393600023246));
#155742=CARTESIAN_POINT('Ctrl Pts',(-6.46934513065601,2.7028133755325,22.6477039066804));
#155743=CARTESIAN_POINT('Ctrl Pts',(-6.54038596829378,2.53277289060295,
22.6560411091601));
#155744=CARTESIAN_POINT('Ctrl Pts',(-6.60475889662637,2.35983384628395,
22.6643783116398));
#155745=CARTESIAN_POINT('Ctrl Pts',(-6.66223566239289,2.18454630100633,
22.6727155141195));
#155746=CARTESIAN_POINT('Ctrl Pts',(-6.68115669641936,2.12684260866413,
22.6754600751556));
#155747=CARTESIAN_POINT('Ctrl Pts',(-6.69933078347864,2.06888458268803,
22.6782046361917));
#155748=CARTESIAN_POINT('Ctrl Pts',(-6.71675092208239,2.01069232186463,
22.6809491972278));
#155749=CARTESIAN_POINT('Ctrl Pts',(-6.76967542231021,1.83389715442881,
22.6892875075297));
#155750=CARTESIAN_POINT('Ctrl Pts',(-6.81559374010498,1.6550838305122,22.6976258178316));
#155751=CARTESIAN_POINT('Ctrl Pts',(-6.85437739256016,1.47483460864606,
22.7059641281335));
#155752=CARTESIAN_POINT('Ctrl Pts',(-6.89318544637344,1.29447198008583,
22.7143076846173));
#155753=CARTESIAN_POINT('Ctrl Pts',(-6.92484981227702,1.11267197191541,
22.7226512411012));
#155754=CARTESIAN_POINT('Ctrl Pts',(-6.94929344594818,0.930025356967012,
22.730994797585));
#155755=CARTESIAN_POINT('Ctrl Pts',(-6.9737556762293,0.747239785270095,
22.7393447018102));
#155756=CARTESIAN_POINT('Ctrl Pts',(-6.9909861731223,0.563606646424557,
22.7476946060354));
#155757=CARTESIAN_POINT('Ctrl Pts',(-7.00095985196023,0.379720573239007,
22.7560445102606));
#155758=CARTESIAN_POINT('Ctrl Pts',(-7.01094849057836,0.195558684551334,
22.7644069387243));
#155759=CARTESIAN_POINT('Ctrl Pts',(-7.01365854234677,0.0111434308513623,
22.772769367188));
#155760=CARTESIAN_POINT('Ctrl Pts',(-7.00911703962814,-0.1729302960572,
22.7811317956516));
#155761=CARTESIAN_POINT('Ctrl Pts',(-7.00457165330559,-0.357161431095265,
22.7895013751316));
#155762=CARTESIAN_POINT('Ctrl Pts',(-6.99276236071042,-0.541050130422998,
22.7978709546116));
#155763=CARTESIAN_POINT('Ctrl Pts',(-6.9737679902753,-0.724007306808131,
22.8062405340916));
#155764=CARTESIAN_POINT('Ctrl Pts',(-6.95474432333805,-0.9072466723465,
22.8146230226281));
#155765=CARTESIAN_POINT('Ctrl Pts',(-6.92851347977865,-1.08955132018455,
22.8230055111647));
#155766=CARTESIAN_POINT('Ctrl Pts',(-6.89520548792601,-1.27034162404253,
22.8313879997013));
#155767=CARTESIAN_POINT('Ctrl Pts',(-6.88430656720839,-1.32949917388767,
22.8341308873056));
#155768=CARTESIAN_POINT('Ctrl Pts',(-6.87265029112042,-1.38849469943956,
22.8368737749099));
#155769=CARTESIAN_POINT('Ctrl Pts',(-6.86024236830183,-1.44730826386657,
22.8396166625142));
#155770=CARTESIAN_POINT('Ctrl Pts',(-6.8222894187228,-1.62720527627531,
22.848006517647));
#155771=CARTESIAN_POINT('Ctrl Pts',(-6.77722367748968,-1.80576193640548,
22.8563963727798));
#155772=CARTESIAN_POINT('Ctrl Pts',(-6.72515683921751,-1.98239553329449,
22.8647862279126));
#155773=CARTESIAN_POINT('Ctrl Pts',(-6.67313804749378,-2.1588661351765,
22.8731683410047));
#155774=CARTESIAN_POINT('Ctrl Pts',(-6.61413113025516,-2.33341689764163,
22.8815504540967));
#155775=CARTESIAN_POINT('Ctrl Pts',(-6.5482985336932,-2.50547657664796,
22.8899325671888));
#155776=CARTESIAN_POINT('Ctrl Pts',(-6.48251700927337,-2.6774027738103,
22.8983081775377));
#155777=CARTESIAN_POINT('Ctrl Pts',(-6.4099204797556,-2.84684143451612,
22.9066837878866));
#155778=CARTESIAN_POINT('Ctrl Pts',(-6.3307209387802,-3.01323728866314,
22.9150593982354));
#155779=CARTESIAN_POINT('Ctrl Pts',(-6.25157121549219,-3.17952847734691,
22.923429740201));
#155780=CARTESIAN_POINT('Ctrl Pts',(-6.16582690315162,-3.3427803797026,
22.9318000821666));
#155781=CARTESIAN_POINT('Ctrl Pts',(-6.07374793431425,-3.50245807868037,
22.9401704241322));
#155782=CARTESIAN_POINT('Ctrl Pts',(-5.98171338677288,-3.66205874497174,
22.9485367280265));
#155783=CARTESIAN_POINT('Ctrl Pts',(-5.88335044082126,-3.81808836213549,
22.9569030319208));
#155784=CARTESIAN_POINT('Ctrl Pts',(-5.77896496849237,-3.97003658112088,
22.9652693358151));
#155785=CARTESIAN_POINT('Ctrl Pts',(-5.67460868985427,-4.12194230444839,
22.9736332998887));
#155786=CARTESIAN_POINT('Ctrl Pts',(-5.5642334281146,-4.26976863416818,
22.9819972639624));
#155787=CARTESIAN_POINT('Ctrl Pts',(-5.44818868139861,-4.41303372459129,
22.990361228036));
#155788=CARTESIAN_POINT('Ctrl Pts',(-5.3321617920407,-4.55627676889777,
22.9987239050345));
#155789=CARTESIAN_POINT('Ctrl Pts',(-5.21046736398084,-4.69495971803971,
23.0070865820331));
#155790=CARTESIAN_POINT('Ctrl Pts',(-5.08349578478654,-4.82863305383185,
23.0154492590316));
#155791=CARTESIAN_POINT('Ctrl Pts',(-4.95652681970505,-4.96230363753426,
23.0238117638579));
#155792=CARTESIAN_POINT('Ctrl Pts',(-4.82428114676228,-5.09096457553647,
23.0321742686842));
#155793=CARTESIAN_POINT('Ctrl Pts',(-4.68718697469135,-5.2142022234263,
23.0405367735105));
#155794=CARTESIAN_POINT('Ctrl Pts',(-4.55007735146155,-5.33745376077946,
23.0489002208305));
#155795=CARTESIAN_POINT('Ctrl Pts',(-4.40811838440423,-5.45528057010076,
23.0572636681505));
#155796=CARTESIAN_POINT('Ctrl Pts',(-4.26177272291521,-5.56730813057046,
23.0656271154704));
#155797=CARTESIAN_POINT('Ctrl Pts',(-4.11534088898789,-5.67940165601611,
23.0739954874233));
#155798=CARTESIAN_POINT('Ctrl Pts',(-3.96451745982217,-5.78568890835989,
23.0823638593761));
#155799=CARTESIAN_POINT('Ctrl Pts',(-3.80979637388184,-5.88583708167808,
23.0907322313289));
#155800=CARTESIAN_POINT('Ctrl Pts',(-3.65502892946048,-5.9860152620064,
23.0991031106646));
#155801=CARTESIAN_POINT('Ctrl Pts',(-3.4963617784528,-6.08005052135353,
23.1074739900004));
#155802=CARTESIAN_POINT('Ctrl Pts',(-3.3343156297423,-6.16765480906286,
23.1158448693361));
#155803=CARTESIAN_POINT('Ctrl Pts',(-3.17213218108231,-6.25533332293784,
23.1242228412274));
#155804=CARTESIAN_POINT('Ctrl Pts',(-3.00656430585668,-6.33656982562772,
23.1326008131187));
#155805=CARTESIAN_POINT('Ctrl Pts',(-2.83815600844423,-6.41112291523349,
23.14097878501));
#155806=CARTESIAN_POINT('Ctrl Pts',(-2.73113116408414,-6.45850201076629,
23.146303054369));
#155807=CARTESIAN_POINT('Ctrl Pts',(-2.62295958427795,-6.50318283201215,
23.151627323728));
#155808=CARTESIAN_POINT('Ctrl Pts',(-2.5137846452561,-6.5451136980021,23.1569515930871));
#155809=CARTESIAN_POINT('Ctrl Pts',(-2.3525561164677,-6.60703680869905,
23.1648144242763));
#155810=CARTESIAN_POINT('Ctrl Pts',(-2.18880317525843,-6.66308866001819,
23.1726772554656));
#155811=CARTESIAN_POINT('Ctrl Pts',(-2.02301101936965,-6.71305094409457,
23.1805400866549));
#155812=CARTESIAN_POINT('Ctrl Pts',(-1.85734625286848,-6.76297483875054,
23.1883968762963));
#155813=CARTESIAN_POINT('Ctrl Pts',(-1.68964575032468,-6.80681836178494,
23.1962536659377));
#155814=CARTESIAN_POINT('Ctrl Pts',(-1.52041460455554,-6.84441129628796,
23.204110455579));
#155815=CARTESIAN_POINT('Ctrl Pts',(-1.3512788971414,-6.88198303015552,
23.211962814363));
#155816=CARTESIAN_POINT('Ctrl Pts',(-1.18061463466396,-6.91331110517384,
23.219815173147));
#155817=CARTESIAN_POINT('Ctrl Pts',(-1.00894174041677,-6.93827522709678,
23.2276675319309));
#155818=CARTESIAN_POINT('Ctrl Pts',(-0.837309380143093,-6.96323345469923,
23.2355180366813));
#155819=CARTESIAN_POINT('Ctrl Pts',(-0.664669237830203,-6.98183065663853,
23.2433685414318));
#155820=CARTESIAN_POINT('Ctrl Pts',(-0.491551030538751,-6.99399772282464,
23.2512190461822));
#155821=CARTESIAN_POINT('Ctrl Pts',(-0.318460672510607,-7.00616283171328,
23.2590682880338));
#155822=CARTESIAN_POINT('Ctrl Pts',(-0.144892783401678,-7.01189984029918,
23.2669175298855));
#155823=CARTESIAN_POINT('Ctrl Pts',(0.0286186714169425,-7.0111915916017,
23.2747667717371));
#155824=CARTESIAN_POINT('Ctrl Pts',(0.202188585640859,-7.01048310428137,
23.282618658152));
#155825=CARTESIAN_POINT('Ctrl Pts',(0.37570164573594,-7.00332502373086,
23.2904705445668));
#155826=CARTESIAN_POINT('Ctrl Pts',(0.548624559625237,-6.98975233145467,
23.2983224309817));
#155827=CARTESIAN_POINT('Ctrl Pts',(0.675599702965492,-6.9797860724522,
23.3040879734456));
#155828=CARTESIAN_POINT('Ctrl Pts',(0.802256653223391,-6.96636228414092,
23.3098535159095));
#155829=CARTESIAN_POINT('Ctrl Pts',(0.928386492953912,-6.94951257874973,
23.3156190583735));
#155830=CARTESIAN_POINT('Ctrl Pts',(1.13961067508076,-6.92129510659616,
23.3252743627334));
#155831=CARTESIAN_POINT('Ctrl Pts',(1.34924873525073,-6.88348348125073,
23.3349296670933));
#155832=CARTESIAN_POINT('Ctrl Pts',(1.5565243537746,-6.83628981967606,23.3445849714532));
#155833=CARTESIAN_POINT('Ctrl Pts',(1.76494824034017,-6.78883471406981,
23.3542937643879));
#155834=CARTESIAN_POINT('Ctrl Pts',(1.97098340393757,-6.73189339868861,
23.3640025573226));
#155835=CARTESIAN_POINT('Ctrl Pts',(2.17386282224807,-6.66572929187405,
23.3737113502573));
#155836=CARTESIAN_POINT('Ctrl Pts',(2.37771851354603,-6.59924679775948,
23.383466862728));
#155837=CARTESIAN_POINT('Ctrl Pts',(2.57838798136036,-6.52345257316277,
23.3932223751987));
#155838=CARTESIAN_POINT('Ctrl Pts',(2.77511600001003,-6.43866117675005,
23.4029778876694));
#155839=CARTESIAN_POINT('Ctrl Pts',(2.97203880966447,-6.35378582380986,
23.4127430595983));
#155840=CARTESIAN_POINT('Ctrl Pts',(3.16501233319539,-6.25989550529004,
23.4225082315272));
#155841=CARTESIAN_POINT('Ctrl Pts',(3.35330244682744,-6.15735245560956,
23.4322734034561));
#155842=CARTESIAN_POINT('Ctrl Pts',(3.54133583116123,-6.05494922105097,
23.4420252607947));
#155843=CARTESIAN_POINT('Ctrl Pts',(3.72469853505676,-5.94391685308443,
23.4517771181332));
#155844=CARTESIAN_POINT('Ctrl Pts',(3.90268314413615,-5.82466229398543,
23.4615289754717));
#155845=CARTESIAN_POINT('Ctrl Pts',(3.98029732395359,-5.77265866939207,
23.4657814915344));
#155846=CARTESIAN_POINT('Ctrl Pts',(4.05688911734959,-5.71909211161391,
23.4700340075972));
#155847=CARTESIAN_POINT('Ctrl Pts',(4.13240130821906,-5.66399911637788,
23.4742865236599));
#155848=CARTESIAN_POINT('Ctrl Pts',(4.27504459599879,-5.55992789445181,
23.4823195692587));
#155849=CARTESIAN_POINT('Ctrl Pts',(4.41390286247934,-5.45035596546787,
23.4903526148575));
#155850=CARTESIAN_POINT('Ctrl Pts',(4.54852131076749,-5.33559560386599,
23.4983856604564));
#155851=CARTESIAN_POINT('Ctrl Pts',(4.68305322113387,-5.22090901464315,
23.5064135421042));
#155852=CARTESIAN_POINT('Ctrl Pts',(4.81335046072091,-5.10104086866477,
23.514441423752));
#155853=CARTESIAN_POINT('Ctrl Pts',(4.9389891074563,-4.9763453617015,23.5224693053999));
#155854=CARTESIAN_POINT('Ctrl Pts',(5.06457102710433,-4.8517061559887,23.53049356238));
#155855=CARTESIAN_POINT('Ctrl Pts',(5.18549828237431,-4.72224418681631,
23.5385178193601));
#155856=CARTESIAN_POINT('Ctrl Pts',(5.30138185290725,-4.58835231996909,
23.5465420763403));
#155857=CARTESIAN_POINT('Ctrl Pts',(5.417251411936,-4.45447664201253,23.554565363106));
#155858=CARTESIAN_POINT('Ctrl Pts',(5.5280782553281,-4.31617240520948,23.5625886498717));
#155859=CARTESIAN_POINT('Ctrl Pts',(5.6335117953184,-4.17386768052228,23.5706119366374));
#155860=CARTESIAN_POINT('Ctrl Pts',(5.73893669597062,-4.03157461643784,
23.5786345659664));
#155861=CARTESIAN_POINT('Ctrl Pts',(5.83896895847041,-3.88528201441365,
23.5866571952953));
#155862=CARTESIAN_POINT('Ctrl Pts',(5.9332998899645,-3.73544896608791,23.5946798246243));
#155863=CARTESIAN_POINT('Ctrl Pts',(6.02766628317316,-3.58555959120303,
23.6027054698907));
#155864=CARTESIAN_POINT('Ctrl Pts',(6.11632687089674,-3.43212742323012,
23.6107311151571));
#155865=CARTESIAN_POINT('Ctrl Pts',(6.19901750484803,-3.27563864568236,
23.6187567604235));
#155866=CARTESIAN_POINT('Ctrl Pts',(6.24777694154283,-3.18336332648741,
23.6234891699311));
#155867=CARTESIAN_POINT('Ctrl Pts',(6.29446148932374,-3.09002570380697,
23.6282215794388));
#155868=CARTESIAN_POINT('Ctrl Pts',(6.33902467059575,-2.99572909123613,
23.6329539889464));
#155869=CARTESIAN_POINT('Ctrl Pts',(6.42123645572228,-2.82176725481528,
23.6416845109259));
#155870=CARTESIAN_POINT('Ctrl Pts',(6.49626706470883,-2.6444536424203,23.6504150329054));
#155871=CARTESIAN_POINT('Ctrl Pts',(6.56387238010522,-2.46438753855636,
23.6591455548849));
#155872=CARTESIAN_POINT('Ctrl Pts',(6.6314977521916,-2.28426801389257,23.6678786669769));
#155873=CARTESIAN_POINT('Ctrl Pts',(6.69169333708936,-2.10139462394241,
23.6766117790689));
#155874=CARTESIAN_POINT('Ctrl Pts',(6.74426407861609,-1.91638425175869,
23.6853448911609));
#155875=CARTESIAN_POINT('Ctrl Pts',(6.7968591561174,-1.73128823483065,23.694082045973));
#155876=CARTESIAN_POINT('Ctrl Pts',(6.84182226067417,-1.54405352189869,
23.7028192007851));
#155877=CARTESIAN_POINT('Ctrl Pts',(6.87900855322177,-1.35531099279898,
23.7115563555972));
#155878=CARTESIAN_POINT('Ctrl Pts',(6.91620003221789,-1.16654213939147,
23.7202947289982));
#155879=CARTESIAN_POINT('Ctrl Pts',(6.94561248434305,-0.976265319218672,
23.7290331023993));
#155880=CARTESIAN_POINT('Ctrl Pts',(6.96715235187015,-0.785120798559216,
23.7377714758003));
#155881=CARTESIAN_POINT('Ctrl Pts',(6.98869753821513,-0.593929078774995,
23.7465120069591));
#155882=CARTESIAN_POINT('Ctrl Pts',(7.00236622588051,-0.401869502479807,
23.7552525381179));
#155883=CARTESIAN_POINT('Ctrl Pts',(7.00811668633663,-0.209587865083013,
23.7639930692767));
#155884=CARTESIAN_POINT('Ctrl Pts',(7.01020911436883,-0.139622078649738,
23.7671734984879));
#155885=CARTESIAN_POINT('Ctrl Pts',(7.01125364863884,-0.0696269189312333,
23.7703539276992));
#155886=CARTESIAN_POINT('Ctrl Pts',(7.01124999042387,0.000366444167520355,
23.7735343569105));
#155887=CARTESIAN_POINT('Ctrl Pts',(7.01124999042383,0.000366444892447644,
23.7735343569434));
#155888=CARTESIAN_POINT('Ctrl Pts',(7.01124305565533,0.133050503538856,
23.7795633893733));
#155889=CARTESIAN_POINT('Ctrl Pts',(7.00746885027521,0.265723050043453,
23.785592421803));
#155890=CARTESIAN_POINT('Ctrl Pts',(6.99993417826157,0.398180941916439,
23.7916214542327));
#155891=CARTESIAN_POINT('Ctrl Pts',(6.98901051473158,0.590216566040994,
23.8003622622672));
#155892=CARTESIAN_POINT('Ctrl Pts',(6.97017950023319,0.781812626957233,
23.8091030703016));
#155893=CARTESIAN_POINT('Ctrl Pts',(6.94350132643035,0.972324993178723,
23.8178438783361));
#155894=CARTESIAN_POINT('Ctrl Pts',(6.91682833312505,1.16280036478232,23.826582989038));
#155895=CARTESIAN_POINT('Ctrl Pts',(6.88231126202484,1.35219219094782,23.8353220997399));
#155896=CARTESIAN_POINT('Ctrl Pts',(6.84006194747097,1.53986334369634,23.8440612104418));
#155897=CARTESIAN_POINT('Ctrl Pts',(6.79782233411896,1.72749140377562,23.8527983144869));
#155898=CARTESIAN_POINT('Ctrl Pts',(6.7478540829149,1.91339931244425,23.8615354185319));
#155899=CARTESIAN_POINT('Ctrl Pts',(6.69031993997926,2.09696105429165,23.870272522577));
#155900=CARTESIAN_POINT('Ctrl Pts',(6.65363953994698,2.21398927054781,23.8758427884251));
#155901=CARTESIAN_POINT('Ctrl Pts',(6.61388493874407,2.33006409320201,23.8814130542733));
#155902=CARTESIAN_POINT('Ctrl Pts',(6.57110895151814,2.44502632087635,23.8869833201214));
#155903=CARTESIAN_POINT('',(7.01124707280511,-0.00640676063125135,23.2264656431175));
#155904=CARTESIAN_POINT('Ctrl Pts',(6.57110895151814,2.44502632087637,23.3397812382711));
#155905=CARTESIAN_POINT('Ctrl Pts',(6.61138542398337,2.33678164208002,23.3345599578824));
#155906=CARTESIAN_POINT('Ctrl Pts',(6.64899878954924,2.22750884430548,23.3293386774937));
#155907=CARTESIAN_POINT('Ctrl Pts',(6.68389688264738,2.11734480532496,23.324117397105));
#155908=CARTESIAN_POINT('Ctrl Pts',(6.73828743675399,1.94564822849709,23.3159797509394));
#155909=CARTESIAN_POINT('Ctrl Pts',(6.78605493295745,1.77186261854152,23.3078421047737));
#155910=CARTESIAN_POINT('Ctrl Pts',(6.82705109833992,1.59655875656229,23.2997044586081));
#155911=CARTESIAN_POINT('Ctrl Pts',(6.86695367326194,1.42593120099738,23.2917838876771));
#155912=CARTESIAN_POINT('Ctrl Pts',(6.90044152218367,1.25386574377418,23.283863316746));
#155913=CARTESIAN_POINT('Ctrl Pts',(6.9274298551555,1.08089877620446,23.275942745815));
#155914=CARTESIAN_POINT('Ctrl Pts',(6.95552767229742,0.900821176323035,
23.2676965620321));
#155915=CARTESIAN_POINT('Ctrl Pts',(6.97658018198758,0.719766819360145,
23.2594503782491));
#155916=CARTESIAN_POINT('Ctrl Pts',(6.99055149854557,0.53834590059025,23.2512041944662));
#155917=CARTESIAN_POINT('Ctrl Pts',(7.00452281510356,0.356924981820356,
23.2429580106833));
#155918=CARTESIAN_POINT('Ctrl Pts',(7.01141296534021,0.175137957219189,
23.2347118269004));
#155919=CARTESIAN_POINT('Ctrl Pts',(7.01124707280511,-0.00640676063126676,
23.2264656431175));
#155920=CARTESIAN_POINT('Ctrl Pts',(7.01124707280455,-0.00640676124481819,
23.2264656430896));
#155921=CARTESIAN_POINT('Ctrl Pts',(7.01104249227252,-0.230289718879575,
23.2162963578778));
#155922=CARTESIAN_POINT('Ctrl Pts',(7.00010998406549,-0.453798136458237,
23.206127072666));
#155923=CARTESIAN_POINT('Ctrl Pts',(6.97858319956031,-0.676020036178396,
23.1959577874541));
#155924=CARTESIAN_POINT('Ctrl Pts',(6.95705641505512,-0.898241935898589,
23.1857885022423));
#155925=CARTESIAN_POINT('Ctrl Pts',(6.92493548555938,-1.11917735600806,
23.1756192170305));
#155926=CARTESIAN_POINT('Ctrl Pts',(6.88240943016724,-1.33793385413669,
23.1654499318186));
#155927=CARTESIAN_POINT('Ctrl Pts',(6.84732461971334,-1.51841215624182,
23.1570600766858));
#155928=CARTESIAN_POINT('Ctrl Pts',(6.80510658490061,-1.69766348663097,
23.148670221553));
#155929=CARTESIAN_POINT('Ctrl Pts',(6.75585773147409,-1.87510343036906,
23.1402803664202));
#155930=CARTESIAN_POINT('Ctrl Pts',(6.70665432419899,-2.05237963501495,
23.1318982533281));
#155931=CARTESIAN_POINT('Ctrl Pts',(6.65043311950308,-2.22784746996435,
23.123516140236));
#155932=CARTESIAN_POINT('Ctrl Pts',(6.58734745079217,-2.40093317796267,
23.1151340271439));
#155933=CARTESIAN_POINT('Ctrl Pts',(6.52431072318973,-2.57388460813557,
23.106758416795));
#155934=CARTESIAN_POINT('Ctrl Pts',(6.45442026090144,-2.74445728801398,
23.0983828064462));
#155935=CARTESIAN_POINT('Ctrl Pts',(6.37787919275471,-2.91209264363731,
23.0900071960973));
#155936=CARTESIAN_POINT('Ctrl Pts',(6.30138627007631,-3.07962255413295,
23.0816368541317));
#155937=CARTESIAN_POINT('Ctrl Pts',(6.21825121890737,-3.24421852610303,
23.0732665121661));
#155938=CARTESIAN_POINT('Ctrl Pts',(6.12872542486748,-3.40534157304123,
23.0648961702005));
#155939=CARTESIAN_POINT('Ctrl Pts',(6.03924282040576,-3.56638689001897,
23.0565298663062));
#155940=CARTESIAN_POINT('Ctrl Pts',(5.94337578057158,-3.72396233620873,
23.0481635624119));
#155941=CARTESIAN_POINT('Ctrl Pts',(5.841422015679,-3.87755275879526,23.0397972585176));
#155942=CARTESIAN_POINT('Ctrl Pts',(5.73949676439662,-4.03110022644583,
23.031433294444));
#155943=CARTESIAN_POINT('Ctrl Pts',(5.63148836278843,-4.18066461841331,
23.0230693303703));
#155944=CARTESIAN_POINT('Ctrl Pts',(5.51773859540824,-4.32575858725869,
23.0147053662967));
#155945=CARTESIAN_POINT('Ctrl Pts',(5.40400633222695,-4.47083022855345,
23.0063426892982));
#155946=CARTESIAN_POINT('Ctrl Pts',(5.28453466751206,-4.61143255973544,
22.9979800122996));
#155947=CARTESIAN_POINT('Ctrl Pts',(5.1597067846208,-4.74710990595731,22.9896173353011));
#155948=CARTESIAN_POINT('Ctrl Pts',(5.03488147170754,-4.88278445883057,
22.9812548304748));
#155949=CARTESIAN_POINT('Ctrl Pts',(4.90470038332,-5.01353398734206,22.9728923256485));
#155950=CARTESIAN_POINT('Ctrl Pts',(4.769585090175,-5.13893808389246,22.9645298208222));
#155951=CARTESIAN_POINT('Ctrl Pts',(4.6344545689001,-5.26435631407518,22.9561663735022));
#155952=CARTESIAN_POINT('Ctrl Pts',(4.49438897538875,-5.38442768800414,
22.9478029261822));
#155953=CARTESIAN_POINT('Ctrl Pts',(4.34984493936847,-5.49877036854154,
22.9394394788622));
#155954=CARTESIAN_POINT('Ctrl Pts',(4.20521579175774,-5.61318037726256,
22.9310711069094));
#155955=CARTESIAN_POINT('Ctrl Pts',(4.05610318965071,-5.72185474723528,
22.9227027349566));
#155956=CARTESIAN_POINT('Ctrl Pts',(3.90299571183461,-5.82445285292109,
22.9143343630038));
#155957=CARTESIAN_POINT('Ctrl Pts',(3.74984235901648,-5.92708169968091,
22.9059634836681));
#155958=CARTESIAN_POINT('Ctrl Pts',(3.59269201978674,-6.02363047331074,
22.8975926043323));
#155959=CARTESIAN_POINT('Ctrl Pts',(3.43206075230852,-6.11380287177821,
22.8892217249966));
#155960=CARTESIAN_POINT('Ctrl Pts',(3.27129338369452,-6.20405167234373,
22.8808437531053));
#155961=CARTESIAN_POINT('Ctrl Pts',(3.10703948294594,-6.28791314600656,
22.872465781214));
#155962=CARTESIAN_POINT('Ctrl Pts',(2.93983914325539,-6.36513726279987,
22.8640878093227));
#155963=CARTESIAN_POINT('Ctrl Pts',(2.83358196586494,-6.41421381786019,
22.8587635399637));
#155964=CARTESIAN_POINT('Ctrl Pts',(2.72613525119984,-6.46061069245768,
22.8534392706047));
#155965=CARTESIAN_POINT('Ctrl Pts',(2.61764153474794,-6.50427393012183,
22.8481150012457));
#155966=CARTESIAN_POINT('Ctrl Pts',(2.45741902907789,-6.56875539110413,
22.8402521700565));
#155967=CARTESIAN_POINT('Ctrl Pts',(2.29457898084835,-6.62740651627266,
22.8323893388672));
#155968=CARTESIAN_POINT('Ctrl Pts',(2.1296030516401,-6.68000130276523,22.8245265076779));
#155969=CARTESIAN_POINT('Ctrl Pts',(1.96475388465679,-6.73255567710685,
22.8166697180365));
#155970=CARTESIAN_POINT('Ctrl Pts',(1.79777246125311,-6.77906285186108,
22.8088129283952));
#155971=CARTESIAN_POINT('Ctrl Pts',(1.62916110100544,-6.81934459236889,
22.8009561387538));
#155972=CARTESIAN_POINT('Ctrl Pts',(1.46064482958318,-6.85960361588191,
22.7931037799698));
#155973=CARTESIAN_POINT('Ctrl Pts',(1.29050081951073,-6.8936441007166,22.7852514211859));
#155974=CARTESIAN_POINT('Ctrl Pts',(1.11924701355631,-6.92133749250427,
22.7773990624019));
#155975=CARTESIAN_POINT('Ctrl Pts',(0.948033642623864,-6.94902434555898,
22.7695485576515));
#155976=CARTESIAN_POINT('Ctrl Pts',(0.775711372026825,-6.97036701910334,
22.7616980529011));
#155977=CARTESIAN_POINT('Ctrl Pts',(0.602808751732648,-6.98528798055846,
22.7538475481506));
#155978=CARTESIAN_POINT('Ctrl Pts',(0.429933946020593,-7.00020654170116,
22.745998306299));
#155979=CARTESIAN_POINT('Ctrl Pts',(0.2564793568388,-7.00870541744943,22.7381490644474));
#155980=CARTESIAN_POINT('Ctrl Pts',(0.082978608838857,-7.01075895413437,
22.7302998225957));
#155981=CARTESIAN_POINT('Ctrl Pts',(-0.0905805949590776,-7.012813182696,
22.7224479361809));
#155982=CARTESIAN_POINT('Ctrl Pts',(-0.264185606802933,-7.00841773011439,
22.714596049766));
#155983=CARTESIAN_POINT('Ctrl Pts',(-0.437302645387597,-6.99759908531755,
22.7067441633512));
#155984=CARTESIAN_POINT('Ctrl Pts',(-0.564420332075718,-6.98965508910021,
22.7009786208872));
#155985=CARTESIAN_POINT('Ctrl Pts',(-0.691274897765848,-6.97824893703722,
22.6952130784233));
#155986=CARTESIAN_POINT('Ctrl Pts',(-0.817656948321552,-6.96340891211779,
22.6894475359593));
#155987=CARTESIAN_POINT('Ctrl Pts',(-1.02930349699858,-6.93855696484626,
22.6797922315994));
#155988=CARTESIAN_POINT('Ctrl Pts',(-1.23951683001374,-6.90408683421205,
22.6701369272395));
#155989=CARTESIAN_POINT('Ctrl Pts',(-1.44751734985819,-6.86019825401275,
22.6604816228796));
#155990=CARTESIAN_POINT('Ctrl Pts',(-1.65667015356232,-6.8160665393125,
22.6507728299448));
#155991=CARTESIAN_POINT('Ctrl Pts',(-1.86358552418146,-6.76241179639087,
22.64106403701));
#155992=CARTESIAN_POINT('Ctrl Pts',(-2.06749234386089,-6.69948520190743,
22.6313552440753));
#155993=CARTESIAN_POINT('Ctrl Pts',(-2.27238038047024,-6.63625579930827,
22.6215997316045));
#155994=CARTESIAN_POINT('Ctrl Pts',(-2.47423080740267,-6.56366513225861,
22.6118442191338));
#155995=CARTESIAN_POINT('Ctrl Pts',(-2.67228348797172,-6.48201569902555,
22.6020887066631));
#155996=CARTESIAN_POINT('Ctrl Pts',(-2.87053227116404,-6.4002854202922,
22.5923235347341));
#155997=CARTESIAN_POINT('Ctrl Pts',(-3.06497575524139,-6.30947845912893,
22.5825583628052));
#155998=CARTESIAN_POINT('Ctrl Pts',(-3.25487414391858,-6.20994531938489,
22.5727931908763));
#155999=CARTESIAN_POINT('Ctrl Pts',(-3.44451361045146,-6.11054789081856,
22.5630413335377));
#156000=CARTESIAN_POINT('Ctrl Pts',(-3.62962033383856,-6.00244808104336,
22.5532894761991));
#156001=CARTESIAN_POINT('Ctrl Pts',(-3.80948051221595,-5.88604152122179,
22.5435376188606));
#156002=CARTESIAN_POINT('Ctrl Pts',(-3.88791257607909,-5.83527983057753,
22.539285102798));
#156003=CARTESIAN_POINT('Ctrl Pts',(-3.96534725946363,-5.78293913191706,
22.5350325867355));
#156004=CARTESIAN_POINT('Ctrl Pts',(-4.041726772628,-5.72905500566385,22.5307800706729));
#156005=CARTESIAN_POINT('Ctrl Pts',(-4.18600844094843,-5.62726734939705,
22.5227470250741));
#156006=CARTESIAN_POINT('Ctrl Pts',(-4.32659311946212,-5.51991943857312,
22.5147139794753));
#156007=CARTESIAN_POINT('Ctrl Pts',(-4.46302109857033,-5.40731626929812,
22.5066809338765));
#156008=CARTESIAN_POINT('Ctrl Pts',(-4.59936137652064,-5.29478548567592,
22.4986530522287));
#156009=CARTESIAN_POINT('Ctrl Pts',(-4.73154999238677,-5.17700640052288,
22.4906251705809));
#156010=CARTESIAN_POINT('Ctrl Pts',(-4.85915744023882,-5.05432641738459,
22.4825972889331));
#156011=CARTESIAN_POINT('Ctrl Pts',(-4.98670727207014,-4.93170182546813,
22.474573031953));
#156012=CARTESIAN_POINT('Ctrl Pts',(-5.10967979068683,-4.80418099503689,
22.4665487749729));
#156013=CARTESIAN_POINT('Ctrl Pts',(-5.22767977195964,-4.67215055026527,
22.4585245179928));
#156014=CARTESIAN_POINT('Ctrl Pts',(-5.3456654858329,-4.54013606931913,
22.4505012312271));
#156015=CARTESIAN_POINT('Ctrl Pts',(-5.45867961003044,-4.40361332811601,
22.4424779444614));
#156016=CARTESIAN_POINT('Ctrl Pts',(-5.56636478780507,-4.26300476326075,
22.4344546576957));
#156017=CARTESIAN_POINT('Ctrl Pts',(-5.67404114174001,-4.12240772002305,
22.4264320283668));
#156018=CARTESIAN_POINT('Ctrl Pts',(-5.77638919929735,-3.97772581354571,
22.4184093990379));
#156019=CARTESIAN_POINT('Ctrl Pts',(-5.87309299959403,-3.82941316400041,
22.4103867697089));
#156020=CARTESIAN_POINT('Ctrl Pts',(-5.96983315363501,-3.68104475945767,
22.4023611244425));
#156021=CARTESIAN_POINT('Ctrl Pts',(-6.06092461385538,-3.52904319413968,
22.3943354791761));
#156022=CARTESIAN_POINT('Ctrl Pts',(-6.14609552708751,-3.37389038565495,
22.3863098339097));
#156023=CARTESIAN_POINT('Ctrl Pts',(-6.19631748758872,-3.28240283522638,
22.381577424402));
#156024=CARTESIAN_POINT('Ctrl Pts',(-6.2444817301707,-3.18982009090364,
22.3768450148942));
#156025=CARTESIAN_POINT('Ctrl Pts',(-6.29054013873481,-3.09624471343373,
22.3721126053864));
#156026=CARTESIAN_POINT('Ctrl Pts',(-6.37550576889667,-2.92362279352308,
22.3633825565517));
#156027=CARTESIAN_POINT('Ctrl Pts',(-6.45334528794889,-2.74753552574655,
22.3546525077171));
#156028=CARTESIAN_POINT('Ctrl Pts',(-6.52380507287605,-2.568578193012,22.3459224588824));
#156029=CARTESIAN_POINT('Ctrl Pts',(-6.59428523133781,-2.38956911454171,
22.3371898857432));
#156030=CARTESIAN_POINT('Ctrl Pts',(-6.65738129601697,-2.20768856951921,
22.3284573126041));
#156031=CARTESIAN_POINT('Ctrl Pts',(-6.71288843299581,-2.02355020907588,
22.3197247394649));
#156032=CARTESIAN_POINT('Ctrl Pts',(-6.76918413746143,-1.83679586928257,
22.3108681061845));
#156033=CARTESIAN_POINT('Ctrl Pts',(-6.81767356152658,-1.64771935090213,
22.3020114729041));
#156034=CARTESIAN_POINT('Ctrl Pts',(-6.85819576343518,-1.45697544004688,
22.2931548396237));
#156035=CARTESIAN_POINT('Ctrl Pts',(-6.89817578093431,-1.26878367023517,
22.2844167075169));
#156036=CARTESIAN_POINT('Ctrl Pts',(-6.93040041898989,-1.07896912656069,
22.2756785754102));
#156037=CARTESIAN_POINT('Ctrl Pts',(-6.9547666744769,-0.888170628925281,
22.2669404433034));
#156038=CARTESIAN_POINT('Ctrl Pts',(-6.97962859022127,-0.693490893465223,
22.2580245594362));
#156039=CARTESIAN_POINT('Ctrl Pts',(-6.9963089458876,-0.49778703725925,
22.249108675569));
#156040=CARTESIAN_POINT('Ctrl Pts',(-7.00475389972531,-0.301743876131736,
22.2401927917017));
#156041=CARTESIAN_POINT('Ctrl Pts',(-7.01319885356303,-0.10570071500419,
22.2312769078345));
#156042=CARTESIAN_POINT('Ctrl Pts',(-7.01340839863455,0.0906814486510902,
22.2223610239673));
#156043=CARTESIAN_POINT('Ctrl Pts',(-7.00538510597693,0.286716025810481,
22.2134451401));
#156044=CARTESIAN_POINT('Ctrl Pts',(-6.99751947304751,0.478898473990961,
22.2047044556038));
#156045=CARTESIAN_POINT('Ctrl Pts',(-6.98174071831608,0.670767280899435,
22.1959637711076));
#156046=CARTESIAN_POINT('Ctrl Pts',(-6.95809877101642,0.861677465923196,
22.1872230866114));
#156047=CARTESIAN_POINT('Ctrl Pts',(-6.9344610772958,1.05255330303345,22.1784839747095));
#156048=CARTESIAN_POINT('Ctrl Pts',(-6.90296304994579,1.24247059107705,
22.1697448628077));
#156049=CARTESIAN_POINT('Ctrl Pts',(-6.86370636760827,1.4307905023985,22.1610057509058));
#156050=CARTESIAN_POINT('Ctrl Pts',(-6.8239410584508,1.62155036921092,22.1521534112314));
#156051=CARTESIAN_POINT('Ctrl Pts',(-6.77621467986645,1.81067089452022,
22.1433010715571));
#156052=CARTESIAN_POINT('Ctrl Pts',(-6.72068646462487,1.99749843722293,
22.1344487318827));
#156053=CARTESIAN_POINT('Ctrl Pts',(-6.66589659215342,2.1818417876134,22.125714099233));
#156054=CARTESIAN_POINT('Ctrl Pts',(-6.60351116548751,2.36395248962728,
22.1169794665832));
#156055=CARTESIAN_POINT('Ctrl Pts',(-6.53373368135293,2.54321661359277,
22.1082448339335));
#156056=CARTESIAN_POINT('Ctrl Pts',(-6.46254572575882,2.72610435531557,
22.0993336407469));
#156057=CARTESIAN_POINT('Ctrl Pts',(-6.38366377114866,2.90602893427757,
22.0904224475602));
#156058=CARTESIAN_POINT('Ctrl Pts',(-6.29735645066384,3.08235758726702,
22.0815112543736));
#156059=CARTESIAN_POINT('Ctrl Pts',(-6.21104913017901,3.25868624025649,
22.0726000611869));
#156060=CARTESIAN_POINT('Ctrl Pts',(-6.11731656498246,3.43141868908508,
22.0636888680003));
#156061=CARTESIAN_POINT('Ctrl Pts',(-6.01647881569159,3.59994572498453,
22.0547776748136));
#156062=CARTESIAN_POINT('Ctrl Pts',(-5.92566157457379,3.75172579308185,
22.0467520099612));
#156063=CARTESIAN_POINT('Ctrl Pts',(-5.82903892465932,3.90016421168691,
22.0387263451088));
#156064=CARTESIAN_POINT('Ctrl Pts',(-5.72689495485971,4.04478685946521,
22.0307006802564));
#156065=CARTESIAN_POINT('Ctrl Pts',(-5.62478340305075,4.18936360756237,
22.0226775625532));
#156066=CARTESIAN_POINT('Ctrl Pts',(-5.51715423130696,4.33012669681961,
22.0146544448499));
#156067=CARTESIAN_POINT('Ctrl Pts',(-5.40433510896315,4.46663056369433,
22.0066313271467));
#156068=CARTESIAN_POINT('Ctrl Pts',(-5.29153021409795,4.60311721623688,
21.9986092212288));
#156069=CARTESIAN_POINT('Ctrl Pts',(-5.17353690623727,4.73534543418988,
21.9905871153109));
#156070=CARTESIAN_POINT('Ctrl Pts',(-5.05072339345024,4.86290240138074,
21.9825650093931));
#156071=CARTESIAN_POINT('Ctrl Pts',(-4.92786424274702,4.99050676917146,
21.9745399224335));
#156072=CARTESIAN_POINT('Ctrl Pts',(-4.80018156118176,5.1134361521193,21.966514835474));
#156073=CARTESIAN_POINT('Ctrl Pts',(-4.66808102018971,5.23131399855186,
21.9584897485145));
#156074=CARTESIAN_POINT('Ctrl Pts',(-4.53595446265715,5.3492150604364,21.9504630810542));
#156075=CARTESIAN_POINT('Ctrl Pts',(-4.39940859173352,5.4620623663669,21.942436413594));
#156076=CARTESIAN_POINT('Ctrl Pts',(-4.25888229618446,5.56951956184253,
21.9344097461337));
#156077=CARTESIAN_POINT('Ctrl Pts',(-4.11824318662046,5.67706302357608,
21.9263766348931));
#156078=CARTESIAN_POINT('Ctrl Pts',(-3.9736175670563,5.77920751718783,21.9183435236525));
#156079=CARTESIAN_POINT('Ctrl Pts',(-3.82547395054926,5.87565958988172,
21.9103104124119));
#156080=CARTESIAN_POINT('Ctrl Pts',(-3.73818235009383,5.93249265492502,
21.9055770114503));
#156081=CARTESIAN_POINT('Ctrl Pts',(-3.64966982054114,5.98735015674246,
21.9008436104887));
#156082=CARTESIAN_POINT('Ctrl Pts',(-3.56003617203163,6.04017955166288,
21.8961102095271));
#156083=CARTESIAN_POINT('Ctrl Pts',(-3.37538806651734,6.14900974935908,
21.886359256233));
#156084=CARTESIAN_POINT('Ctrl Pts',(-3.18587248217942,6.24929545974911,
21.8766083029389));
#156085=CARTESIAN_POINT('Ctrl Pts',(-2.99222443154627,6.3406797359398,21.8668573496447));
#156086=CARTESIAN_POINT('Ctrl Pts',(-2.79829739456872,6.4321956683236,21.8570923482732));
#156087=CARTESIAN_POINT('Ctrl Pts',(-2.60022601729658,6.51478449787464,
21.8473273469016));
#156088=CARTESIAN_POINT('Ctrl Pts',(-2.39876794143634,6.5881362254918,21.83756234553));
#156089=CARTESIAN_POINT('Ctrl Pts',(-2.1976456544473,6.66136569097718,21.8278136203924));
#156090=CARTESIAN_POINT('Ctrl Pts',(-1.99314798640384,6.72538881257968,
21.8180648952549));
#156091=CARTESIAN_POINT('Ctrl Pts',(-1.78604756611937,6.77994547574382,
21.8083161701173));
#156092=CARTESIAN_POINT('Ctrl Pts',(-1.57951555618622,6.8343524020217,21.7985942014502));
#156093=CARTESIAN_POINT('Ctrl Pts',(-1.37039509354959,6.87934472802108,
21.7888722327832));
#156094=CARTESIAN_POINT('Ctrl Pts',(-1.15947062927344,6.9147128951499,21.7791502641161));
#156095=CARTESIAN_POINT('Ctrl Pts',(-0.949941797086738,6.94984704035452,
21.7694926231764));
#156096=CARTESIAN_POINT('Ctrl Pts',(-0.738632798821536,6.97548393061858,
21.7598349822368));
#156097=CARTESIAN_POINT('Ctrl Pts',(-0.526330010289526,6.99146646153499,
21.7501773412971));
#156098=CARTESIAN_POINT('Ctrl Pts',(-0.433015625586685,6.99849133411802,
21.7459324756116));
#156099=CARTESIAN_POINT('Ctrl Pts',(-0.339509473265604,7.00365170974,21.7416876099262));
#156100=CARTESIAN_POINT('Ctrl Pts',(-0.245879369247645,7.00693726946934,
21.7374427442407));
#156101=CARTESIAN_POINT('Ctrl Pts',(-0.0726891420124154,7.01301466137321,
21.7295908972268));
#156102=CARTESIAN_POINT('Ctrl Pts',(0.100854183988949,7.01267108832776,
21.7217390502129));
#156103=CARTESIAN_POINT('Ctrl Pts',(0.274217249882488,7.00588548738608,
21.713887203199));
#156104=CARTESIAN_POINT('Ctrl Pts',(0.447531151412028,6.99910181078597,
21.7060375829054));
#156105=CARTESIAN_POINT('Ctrl Pts',(0.620664513724713,6.98587975522486,
21.6981879626118));
#156106=CARTESIAN_POINT('Ctrl Pts',(0.793084111268163,6.96625036550898,
21.6903383423182));
#156107=CARTESIAN_POINT('Ctrl Pts',(0.965489943311692,6.94662254294885,
21.6824893487164));
#156108=CARTESIAN_POINT('Ctrl Pts',(1.13718174509647,6.92058844847128,21.6746403551146));
#156109=CARTESIAN_POINT('Ctrl Pts',(1.30763180892856,6.88823094958192,21.6667913615129));
#156110=CARTESIAN_POINT('Ctrl Pts',(1.47816816663717,6.85585706903831,21.6589383941954));
#156111=CARTESIAN_POINT('Ctrl Pts',(1.64746115504819,6.81715345885381,21.651085426878));
#156112=CARTESIAN_POINT('Ctrl Pts',(1.8149933176821,6.77225411656041,21.6432324595606));
#156113=CARTESIAN_POINT('Ctrl Pts',(1.98256802785633,6.72734337134265,21.6353774978533));
#156114=CARTESIAN_POINT('Ctrl Pts',(2.14838065676238,6.67623387159824,21.627522536146));
#156115=CARTESIAN_POINT('Ctrl Pts',(2.31192992699491,6.61910919800885,21.6196675744388));
#156116=CARTESIAN_POINT('Ctrl Pts',(2.47564153354891,6.56192782340598,21.6118048160254));
#156117=CARTESIAN_POINT('Ctrl Pts',(2.63708493939628,6.49871948923473,21.603942057612));
#156118=CARTESIAN_POINT('Ctrl Pts',(2.79577929785132,6.42971575423097,21.5960792991987));
#156119=CARTESIAN_POINT('Ctrl Pts',(2.91219520208469,6.37909560437721,21.5903112924506));
#156120=CARTESIAN_POINT('Ctrl Pts',(3.02713214893815,6.32535767300183,21.5845432857024));
#156121=CARTESIAN_POINT('Ctrl Pts',(3.14040939108398,6.2686087307226,21.5787752789543));
#156122=CARTESIAN_POINT('Ctrl Pts',(3.304960287799,6.18617302552018,21.5703964495912));
#156123=CARTESIAN_POINT('Ctrl Pts',(3.46637260497444,6.09719951480489,21.5620176202281));
#156124=CARTESIAN_POINT('Ctrl Pts',(3.6241137781913,6.00195183962884,21.553638790865));
#156125=CARTESIAN_POINT('Ctrl Pts',(3.78174325263786,5.90677161068749,21.5452658946703));
#156126=CARTESIAN_POINT('Ctrl Pts',(3.93570648585905,5.80532624533494,21.5368929984755));
#156127=CARTESIAN_POINT('Ctrl Pts',(4.08549569848543,5.69792518906286,21.5285201022808));
#156128=CARTESIAN_POINT('Ctrl Pts',(4.2351917523392,5.59059092899329,21.5201524134619));
#156129=CARTESIAN_POINT('Ctrl Pts',(4.38071869727635,5.47730855774819,21.511784724643));
#156130=CARTESIAN_POINT('Ctrl Pts',(4.52159763341181,5.35843087144219,21.5034170358241));
#156131=CARTESIAN_POINT('Ctrl Pts',(4.66242521850144,5.23959651662126,21.4950523970678));
#156132=CARTESIAN_POINT('Ctrl Pts',(4.79860792169724,5.11517112458317,21.4866877583116));
#156133=CARTESIAN_POINT('Ctrl Pts',(4.92969933646971,4.98554821604506,21.4783231195553));
#156134=CARTESIAN_POINT('Ctrl Pts',(5.06076045028385,4.85595526902928,21.4699604142328));
#156135=CARTESIAN_POINT('Ctrl Pts',(5.18673238887386,4.72116743212467,21.4615977089103));
#156136=CARTESIAN_POINT('Ctrl Pts',(5.30720477662809,4.58161587449625,21.4532350035878));
#156137=CARTESIAN_POINT('Ctrl Pts',(5.42766537763979,4.44207797027265,21.4448731164532));
#156138=CARTESIAN_POINT('Ctrl Pts',(5.5426272867884,4.29777752399853,21.4365112293186));
#156139=CARTESIAN_POINT('Ctrl Pts',(5.65171939997368,4.14917996554273,21.4281493421841));
#156140=CARTESIAN_POINT('Ctrl Pts',(5.76083930437926,4.00054455185283,21.4197853248584));
#156141=CARTESIAN_POINT('Ctrl Pts',(5.86408622814664,3.84761010204599,21.4114213075328));
#156142=CARTESIAN_POINT('Ctrl Pts',(5.96113104311383,3.69087296575276,21.4030572902071));
#156143=CARTESIAN_POINT('Ctrl Pts',(6.05818750621396,3.53411701655336,21.3946922689619));
#156144=CARTESIAN_POINT('Ctrl Pts',(6.14904020684982,3.37355775255416,21.3863272477167));
#156145=CARTESIAN_POINT('Ctrl Pts',(6.23340485140487,3.20971813731085,21.3779622264715));
#156146=CARTESIAN_POINT('Ctrl Pts',(6.31781451050954,3.04579110195775,21.3695927418914));
#156147=CARTESIAN_POINT('Ctrl Pts',(6.39572904963281,2.87858051234587,21.3612232573113));
#156148=CARTESIAN_POINT('Ctrl Pts',(6.46691099881845,2.70863225556018,21.3528537727312));
#156149=CARTESIAN_POINT('Ctrl Pts',(6.50342331136282,2.62145841529419,21.3485607006768));
#156150=CARTESIAN_POINT('Ctrl Pts',(6.53816498276623,2.53356459390674,21.3442676286225));
#156151=CARTESIAN_POINT('Ctrl Pts',(6.57110895151816,2.44502632087631,21.3399745565681));
#156152=CARTESIAN_POINT('Origin',(0.,0.,50.));
#156153=CARTESIAN_POINT('',(6.57110895151814,2.44502632087635,19.3399454697435));
#156154=CARTESIAN_POINT('',(6.57110895151814,2.44502632087636,19.8869210003222));
#156155=CARTESIAN_POINT('',(6.57110895151814,2.44502632087636,50.));
#156156=CARTESIAN_POINT('',(7.01125,3.83823506831804E-12,21.7735343569105));
#156157=CARTESIAN_POINT('Ctrl Pts',(6.57110895151814,2.44502632087636,19.8869210003222));
#156158=CARTESIAN_POINT('Ctrl Pts',(6.50449838733151,2.6240449559132,19.8955928092609));
#156159=CARTESIAN_POINT('Ctrl Pts',(6.43056821795879,2.80033990715949,19.9042646181997));
#156160=CARTESIAN_POINT('Ctrl Pts',(6.34956511459268,2.97332295892115,19.9129364271385));
#156161=CARTESIAN_POINT('Ctrl Pts',(6.26856213015524,3.14630575670929,19.9216082233453));
#156162=CARTESIAN_POINT('Ctrl Pts',(6.18048635294281,3.31597640754666,19.9302800195521));
#156163=CARTESIAN_POINT('Ctrl Pts',(6.08563165071556,3.48176879966333,19.9389518157589));
#156164=CARTESIAN_POINT('Ctrl Pts',(5.99077708581969,3.64756095174446,19.9476235994107));
#156165=CARTESIAN_POINT('Ctrl Pts',(5.88914375658117,3.8094746098372,19.9562953830624));
#156166=CARTESIAN_POINT('Ctrl Pts',(5.78107076500248,3.96696954519866,19.9649671667141));
#156167=CARTESIAN_POINT('Ctrl Pts',(5.67299792768891,4.12446425574932,19.9736389379876));
#156168=CARTESIAN_POINT('Ctrl Pts',(5.55848560711398,4.27754002202472,19.9823107092611));
#156169=CARTESIAN_POINT('Ctrl Pts',(5.43791587524917,4.42568610457329,19.9909824805346));
#156170=CARTESIAN_POINT('Ctrl Pts',(5.31734631302946,4.57383197867604,19.9996542396066));
#156171=CARTESIAN_POINT('Ctrl Pts',(5.19071953583901,4.71704796266763,20.0083259986787));
#156172=CARTESIAN_POINT('Ctrl Pts',(5.0584580345168,4.85485621574238,20.0169977577507));
#156173=CARTESIAN_POINT('Ctrl Pts',(4.9261967165933,4.9926642777271,20.0256695047982));
#156174=CARTESIAN_POINT('Ctrl Pts',(4.78830088681942,5.12506441890746,20.0343412518457));
#156175=CARTESIAN_POINT('Ctrl Pts',(4.64523063400654,5.25161488681217,20.0430129988931));
#156176=CARTESIAN_POINT('Ctrl Pts',(4.49652806262589,5.38314733060724,20.0520261309661));
#156177=CARTESIAN_POINT('Ctrl Pts',(4.34223563524161,5.50835996364107,20.0610392630392));
#156178=CARTESIAN_POINT('Ctrl Pts',(4.18290943344762,5.626801510101,20.0700523951122));
#156179=CARTESIAN_POINT('Ctrl Pts',(4.02607270355667,5.7433924073975,20.0789246969965));
#156180=CARTESIAN_POINT('Ctrl Pts',(3.86435862820615,5.85342208902484,20.0877969988809));
#156181=CARTESIAN_POINT('Ctrl Pts',(3.69833198496683,5.9565062823329,20.0966693007653));
#156182=CARTESIAN_POINT('Ctrl Pts',(3.53489950802812,6.05797978512052,20.1054029729327));
#156183=CARTESIAN_POINT('Ctrl Pts',(3.36728850947313,6.15272311279783,20.1141366451001));
#156184=CARTESIAN_POINT('Ctrl Pts',(3.196066230012,6.24041562845592,20.1228703172675));
#156185=CARTESIAN_POINT('Ctrl Pts',(3.02603797481334,6.3274966174385,20.1315430848815));
#156186=CARTESIAN_POINT('Ctrl Pts',(2.85244891335583,6.40762471321497,20.1402158524955));
#156187=CARTESIAN_POINT('Ctrl Pts',(2.67587836095385,6.48053250588861,20.1488886201095));
#156188=CARTESIAN_POINT('Ctrl Pts',(2.49930871513683,6.55343992422402,20.157561343194));
#156189=CARTESIAN_POINT('Ctrl Pts',(2.319757871652,6.61912700519343,20.1662340662785));
#156190=CARTESIAN_POINT('Ctrl Pts',(2.13782503580303,6.67737453485978,20.1749067893629));
#156191=CARTESIAN_POINT('Ctrl Pts',(1.9558931192204,6.73562177021425,20.1835794686261));
#156192=CARTESIAN_POINT('Ctrl Pts',(1.7715795049724,6.7864294428484,20.1922521478892));
#156193=CARTESIAN_POINT('Ctrl Pts',(1.58549928668991,6.82962799678034,20.2009248271523));
#156194=CARTESIAN_POINT('Ctrl Pts',(1.39941999344073,6.87282633596564,20.2095974633022));
#156195=CARTESIAN_POINT('Ctrl Pts',(1.21157439050846,6.90841556788882,20.2182700994521));
#156196=CARTESIAN_POINT('Ctrl Pts',(1.02258935229308,6.93627692491273,20.226942735602));
#156197=CARTESIAN_POINT('Ctrl Pts',(0.833605238126011,6.96413814570766,
20.2356153293468));
#156198=CARTESIAN_POINT('Ctrl Pts',(0.643481980917327,6.98427152577607,
20.2442879230916));
#156199=CARTESIAN_POINT('Ctrl Pts',(0.452854049808676,6.99660987708132,
20.2529605168364));
#156200=CARTESIAN_POINT('Ctrl Pts',(0.262227035222496,7.00894816906485,
20.2616330688841));
#156201=CARTESIAN_POINT('Ctrl Pts',(0.071095635122742,7.01349148893086,
20.2703056209318));
#156202=CARTESIAN_POINT('Ctrl Pts',(-0.119902323155651,7.0102246751015,
20.2789781729795));
#156203=CARTESIAN_POINT('Ctrl Pts',(-0.310899378721189,7.00695787671206,
20.2876506840382));
#156204=CARTESIAN_POINT('Ctrl Pts',(-0.501762709651607,6.99588102335292,
20.2963231950968));
#156205=CARTESIAN_POINT('Ctrl Pts',(-0.691855389204073,6.97703107940113,
20.3049957061555));
#156206=CARTESIAN_POINT('Ctrl Pts',(-0.881947185836118,6.95818122300137,
20.3136681769331));
#156207=CARTESIAN_POINT('Ctrl Pts',(-1.07126805552891,6.93155837629147,
20.3223406477107));
#156208=CARTESIAN_POINT('Ctrl Pts',(-1.25918622472346,6.89725138109136,
20.3310131184882));
#156209=CARTESIAN_POINT('Ctrl Pts',(-1.44710353643374,6.86294454243657,
20.3396855496927));
#156210=CARTESIAN_POINT('Ctrl Pts',(-1.63361788096923,6.82095367648077,
20.3483579808972));
#156211=CARTESIAN_POINT('Ctrl Pts',(-1.81810685596541,6.77141890764348,
20.3570304121017));
#156212=CARTESIAN_POINT('Ctrl Pts',(-2.00259500418067,6.72188436079453,
20.3657028044409));
#156213=CARTESIAN_POINT('Ctrl Pts',(-2.1850575266401,6.66480605238719,20.3743751967802));
#156214=CARTESIAN_POINT('Ctrl Pts',(-2.36488554744815,6.60037445225427,
20.3830475891195));
#156215=CARTESIAN_POINT('Ctrl Pts',(-2.54471277703796,6.53594313561142,
20.3917199433014));
#156216=CARTESIAN_POINT('Ctrl Pts',(-2.72190526072897,6.46415868780944,
20.4003922974834));
#156217=CARTESIAN_POINT('Ctrl Pts',(-2.89587171389844,6.38526065083822,
20.4090646516653));
#156218=CARTESIAN_POINT('Ctrl Pts',(-3.06983741583579,6.30636295456912,
20.4177369683978));
#156219=CARTESIAN_POINT('Ctrl Pts',(-3.24057685640747,6.22035184793782,
20.4264092851303));
#156220=CARTESIAN_POINT('Ctrl Pts',(-3.4075202894675,6.12751434428083,20.4350816018628));
#156221=CARTESIAN_POINT('Ctrl Pts',(-3.57446301524516,6.03467723394467,
20.4437538818536));
#156222=CARTESIAN_POINT('Ctrl Pts',(-3.73760951742132,5.93501392252177,
20.4524261618445));
#156223=CARTESIAN_POINT('Ctrl Pts',(-3.89641539158824,5.82885697703197,
20.4610984418353));
#156224=CARTESIAN_POINT('Ctrl Pts',(-4.05522060590695,5.72270047263084,
20.4697706857923));
#156225=CARTESIAN_POINT('Ctrl Pts',(-4.20968499214093,5.61005054602585,
20.4784429297493));
#156226=CARTESIAN_POINT('Ctrl Pts',(-4.35929312155911,5.49128309621963,
20.4871151737063));
#156227=CARTESIAN_POINT('Ctrl Pts',(-4.50890064155348,5.37251613020872,
20.4957873823372));
#156228=CARTESIAN_POINT('Ctrl Pts',(-4.65365172183292,5.24763186748421,
20.504459590968));
#156229=CARTESIAN_POINT('Ctrl Pts',(-4.79306334970934,5.11704702813772,
20.5131317995989));
#156230=CARTESIAN_POINT('Ctrl Pts',(-4.93247442107197,4.98646271006959,
20.5218039736114));
#156231=CARTESIAN_POINT('Ctrl Pts',(-5.06654587536609,4.85017805510835,
20.5304761476239));
#156232=CARTESIAN_POINT('Ctrl Pts',(-5.19483033978515,4.70864782112102,
20.5391483216364));
#156233=CARTESIAN_POINT('Ctrl Pts',(-5.32311430257525,4.56711814055739,
20.5478204617383));
#156234=CARTESIAN_POINT('Ctrl Pts',(-5.44561113000508,4.42034313247902,
20.5564926018401));
#156235=CARTESIAN_POINT('Ctrl Pts',(-5.5619120749508,4.26881255538546,20.5651647419419));
#156236=CARTESIAN_POINT('Ctrl Pts',(-5.67821257461538,4.11728255845664,
20.5738368488408));
#156237=CARTESIAN_POINT('Ctrl Pts',(-5.78831706632159,3.96099725428101,
20.5825089557396));
#156238=CARTESIAN_POINT('Ctrl Pts',(-5.89185815647258,3.80047813130238,
20.5911810626384));
#156239=CARTESIAN_POINT('Ctrl Pts',(-5.99539885864335,3.6399596098071,20.5998531370419));
#156240=CARTESIAN_POINT('Ctrl Pts',(-6.0923760545057,3.47520753995133,20.6085252114453));
#156241=CARTESIAN_POINT('Ctrl Pts',(-6.18246615568003,3.30677165773069,
20.6171972858488));
#156242=CARTESIAN_POINT('Ctrl Pts',(-6.27255592662618,3.13833639291722,
20.6258693284645));
#156243=CARTESIAN_POINT('Ctrl Pts',(-6.35575851943786,2.96621759322458,
20.6345413710802));
#156244=CARTESIAN_POINT('Ctrl Pts',(-6.43179631013586,2.79098957135685,
20.6432134136958));
#156245=CARTESIAN_POINT('Ctrl Pts',(-6.50783382831831,2.61576217749741,
20.6518854252314));
#156246=CARTESIAN_POINT('Ctrl Pts',(-6.57670648270539,2.43742584432246,
20.6605574367669));
#156247=CARTESIAN_POINT('Ctrl Pts',(-6.63818446599417,2.2565756264601,20.6692294483024));
#156248=CARTESIAN_POINT('Ctrl Pts',(-6.69966223396417,2.07572604200249,
20.6779014294654));
#156249=CARTESIAN_POINT('Ctrl Pts',(-6.75374529124706,1.89236285939331,
20.6865734106283));
#156250=CARTESIAN_POINT('Ctrl Pts',(-6.80025318023355,1.7070979020617,20.6952453917912));
#156251=CARTESIAN_POINT('Ctrl Pts',(-6.84676091012601,1.52183357848386,
20.703917343289));
#156252=CARTESIAN_POINT('Ctrl Pts',(-6.88569345442259,1.3346677686797,20.7125892947869));
#156253=CARTESIAN_POINT('Ctrl Pts',(-6.91692090874655,1.14622497994278,
20.7212612462847));
#156254=CARTESIAN_POINT('Ctrl Pts',(-6.94814825879511,0.957782820458171,
20.729933168825));
#156255=CARTESIAN_POINT('Ctrl Pts',(-6.97167052392486,0.768063970772979,
20.7386050913652));
#156256=CARTESIAN_POINT('Ctrl Pts',(-6.98740921903138,0.577701452564639,
20.7472770139055));
#156257=CARTESIAN_POINT('Ctrl Pts',(-7.00314786286674,0.387339554490748,
20.7559489081957));
#156258=CARTESIAN_POINT('Ctrl Pts',(-7.01110296401739,0.196334275139723,
20.7646208024858));
#156259=CARTESIAN_POINT('Ctrl Pts',(-7.01124797942392,0.00532292438118208,
20.773292696776));
#156260=CARTESIAN_POINT('Ctrl Pts',(-7.01139299436988,-0.18568781970999,
20.7819645635235));
#156261=CARTESIAN_POINT('Ctrl Pts',(-7.00372797299449,-0.376704351158961,
20.7906364302711));
#156262=CARTESIAN_POINT('Ctrl Pts',(-6.98827849031219,-0.567089326596749,
20.7993082970186));
#156263=CARTESIAN_POINT('Ctrl Pts',(-6.97282905543853,-0.757473712885664,
20.807980136931));
#156264=CARTESIAN_POINT('Ctrl Pts',(-6.94959523043414,-0.947226263998012,
20.8166519768433));
#156265=CARTESIAN_POINT('Ctrl Pts',(-6.91865453650955,-1.13571385786028,
20.8253238167556));
#156266=CARTESIAN_POINT('Ctrl Pts',(-6.88771393580756,-1.3242008838198,
20.8339956305402));
#156267=CARTESIAN_POINT('Ctrl Pts',(-6.84906655865586,-1.51142267990424,
20.8426674443247));
#156268=CARTESIAN_POINT('Ctrl Pts',(-6.80284135383597,-1.69675457183389,
20.8513392581093));
#156269=CARTESIAN_POINT('Ctrl Pts',(-6.75661628451972,-1.88208592048537,
20.8600110464735));
#156270=CARTESIAN_POINT('Ctrl Pts',(-6.70281350071577,-2.06552710051182,
20.8686828348377));
#156271=CARTESIAN_POINT('Ctrl Pts',(-6.64161251687743,-2.24646605542062,
20.8773546232018));
#156272=CARTESIAN_POINT('Ctrl Pts',(-6.58041170745085,-2.42740449468607,
20.886026386853));
#156273=CARTESIAN_POINT('Ctrl Pts',(-6.51181283117455,-2.60584045408172,
20.8946981505041));
#156274=CARTESIAN_POINT('Ctrl Pts',(-6.43604476876406,-2.78117858055982,
20.9033699141553));
#156275=CARTESIAN_POINT('Ctrl Pts',(-6.3568477472844,-2.96445180844916,
20.9124341271007));
#156276=CARTESIAN_POINT('Ctrl Pts',(-6.26981768815867,-3.14433998861843,
20.921498340046));
#156277=CARTESIAN_POINT('Ctrl Pts',(-6.17527181578317,-3.32018742900067,
20.9305625529914));
#156278=CARTESIAN_POINT('Ctrl Pts',(-6.08368050191941,-3.49053963687095,
20.9393435092822));
#156279=CARTESIAN_POINT('Ctrl Pts',(-5.98503618716834,-3.65709956718258,
20.948124465573));
#156280=CARTESIAN_POINT('Ctrl Pts',(-5.87967633130331,-3.81929742251263,
20.9569054218639));
#156281=CARTESIAN_POINT('Ctrl Pts',(-5.77561495477929,-3.97949631379159,
20.9655781596094));
#156282=CARTESIAN_POINT('Ctrl Pts',(-5.66500279405459,-4.13543980257297,
20.9742508973548));
#156283=CARTESIAN_POINT('Ctrl Pts',(-5.54820899034813,-4.28660746534136,
20.9829236351003));
#156284=CARTESIAN_POINT('Ctrl Pts',(-5.43141636368597,-4.43777360464676,
20.9915962854423));
#156285=CARTESIAN_POINT('Ctrl Pts',(-5.3084423924293,-4.58416378940311,
21.0002689357842));
#156286=CARTESIAN_POINT('Ctrl Pts',(-5.17969746407345,-4.7252894877638,
21.0089415861261));
#156287=CARTESIAN_POINT('Ctrl Pts',(-5.05095379117065,-4.86641380994066,
21.0176141518968));
#156288=CARTESIAN_POINT('Ctrl Pts',(-4.91643946527209,-5.002273538546,21.0262867176676));
#156289=CARTESIAN_POINT('Ctrl Pts',(-4.776603377482,-5.13241529269871,21.0349592834384));
#156290=CARTESIAN_POINT('Ctrl Pts',(-4.63676860764796,-5.26255582026453,
21.0436317674702));
#156291=CARTESIAN_POINT('Ctrl Pts',(-4.49161238427241,-5.38697828766001,
21.052304251502));
#156292=CARTESIAN_POINT('Ctrl Pts',(-4.34161910267864,-5.50526748939195,
21.0609767355337));
#156293=CARTESIAN_POINT('Ctrl Pts',(-4.19162718580777,-5.62355561486247,
21.0696491406584));
#156294=CARTESIAN_POINT('Ctrl Pts',(-4.0367985218659,-5.73571041041258,
21.0783215457831));
#156295=CARTESIAN_POINT('Ctrl Pts',(-3.87764977431811,-5.84135761533488,
21.0869939509077));
#156296=CARTESIAN_POINT('Ctrl Pts',(-3.71850242284505,-5.94700389350534,
21.0956662799569));
#156297=CARTESIAN_POINT('Ctrl Pts',(-3.55503530028693,-6.04614253816315,
21.104338609006));
#156298=CARTESIAN_POINT('Ctrl Pts',(-3.38779388709652,-6.13844272931266,
21.1130109380551));
#156299=CARTESIAN_POINT('Ctrl Pts',(-3.22055388638266,-6.23074214091927,
21.1216831938601));
#156300=CARTESIAN_POINT('Ctrl Pts',(-3.04953990753832,-6.31620307732841,
21.130355449665));
#156301=CARTESIAN_POINT('Ctrl Pts',(-2.87532260481505,-6.39454036508799,
21.13902770547));
#156302=CARTESIAN_POINT('Ctrl Pts',(-2.7011067166233,-6.47287701679959,
21.1476998908618));
#156303=CARTESIAN_POINT('Ctrl Pts',(-2.52368781567824,-6.54409001910862,
21.1563720762537));
#156304=CARTESIAN_POINT('Ctrl Pts',(-2.34365791912595,-6.60794174615805,
21.1650442616455));
#156305=CARTESIAN_POINT('Ctrl Pts',(-2.16362942554496,-6.67179297561156,
21.1737163794551));
#156306=CARTESIAN_POINT('Ctrl Pts',(-1.98099024478875,-6.72828294965035,
21.1823884972647));
#156307=CARTESIAN_POINT('Ctrl Pts',(-1.79634980371338,-6.77722317363084,
21.1910606150743));
#156308=CARTESIAN_POINT('Ctrl Pts',(-1.61171074128287,-6.826163032192,21.1997326681323));
#156309=CARTESIAN_POINT('Ctrl Pts',(-1.42507072299763,-6.86755318072501,
21.2084047211902));
#156310=CARTESIAN_POINT('Ctrl Pts',(-1.23705251633957,-6.90125551144992,
21.2170767742482));
#156311=CARTESIAN_POINT('Ctrl Pts',(-1.04903565219215,-6.93495760152932,
21.2257487653849));
#156312=CARTESIAN_POINT('Ctrl Pts',(-0.859640898941481,-6.9609719335339,
21.2344207565216));
#156313=CARTESIAN_POINT('Ctrl Pts',(-0.669500206862531,-6.97921170588133,
21.2430927476583));
#156314=CARTESIAN_POINT('Ctrl Pts',(-0.479360810404673,-6.99745135394273,
21.2517646797039));
#156315=CARTESIAN_POINT('Ctrl Pts',(-0.288475768015417,-7.00791652123616,
21.2604366117496));
#156316=CARTESIAN_POINT('Ctrl Pts',(-0.0974819939210606,-7.01057228929003,
21.2691085437952));
#156317=CARTESIAN_POINT('Ctrl Pts',(0.0935105410582171,-7.013228040114,
21.2777804195797));
#156318=CARTESIAN_POINT('Ctrl Pts',(0.284611522344327,-7.00807448913602,
21.2864522953643));
#156319=CARTESIAN_POINT('Ctrl Pts',(0.475183323466393,-6.99512883166561,
21.2951241711488));
#156320=CARTESIAN_POINT('Ctrl Pts',(0.665753950390514,-6.98218325395917,
21.303795993502));
#156321=CARTESIAN_POINT('Ctrl Pts',(0.855795120323037,-6.96144568508293,
21.3124678158553));
#156322=CARTESIAN_POINT('Ctrl Pts',(1.04467275075973,-6.93298531704201,
21.3211396382085));
#156323=CARTESIAN_POINT('Ctrl Pts',(1.23354927906054,-6.9045251150726,21.32981140996));
#156324=CARTESIAN_POINT('Ctrl Pts',(1.42126200062534,-6.86834224643164,
21.3384831817116));
#156325=CARTESIAN_POINT('Ctrl Pts',(1.60718460924413,-6.82455743578357,
21.3471549534631));
#156326=CARTESIAN_POINT('Ctrl Pts',(1.79763389405557,-6.77970659200789,
21.3560378577016));
#156327=CARTESIAN_POINT('Ctrl Pts',(1.98620448431575,-6.72687898190956,
21.3649207619401));
#156328=CARTESIAN_POINT('Ctrl Pts',(2.17223623427553,-6.66625954377719,
21.3738036661786));
#156329=CARTESIAN_POINT('Ctrl Pts',(2.35386532185741,-6.60707473666718,
21.3824763459349));
#156330=CARTESIAN_POINT('Ctrl Pts',(2.53307410227393,-6.54046283696633,
21.3911490256913));
#156331=CARTESIAN_POINT('Ctrl Pts',(2.7092645177397,-6.4666461427402,21.3998217054476));
#156332=CARTESIAN_POINT('Ctrl Pts',(2.88545151535885,-6.39283088045427,
21.4084942169662));
#156333=CARTESIAN_POINT('Ctrl Pts',(3.05862000314107,-6.31181121311163,
21.4171667284847));
#156334=CARTESIAN_POINT('Ctrl Pts',(3.2281921034394,-6.22385751008099,21.4258392400032));
#156335=CARTESIAN_POINT('Ctrl Pts',(3.39776113570824,-6.13590539837672,
21.434511594612));
#156336=CARTESIAN_POINT('Ctrl Pts',(3.56373365850942,-6.04101963284054,
21.4431839492208));
#156337=CARTESIAN_POINT('Ctrl Pts',(3.7255558277513,-5.93951684371787,21.4518563038295));
#156338=CARTESIAN_POINT('Ctrl Pts',(3.88737528046358,-5.8380157585356,21.4605285128543));
#156339=CARTESIAN_POINT('Ctrl Pts',(4.04504427838794,-5.72989802299747,
21.4692007218791));
#156340=CARTESIAN_POINT('Ctrl Pts',(4.19803670363096,-5.6155244098363,21.477872930904));
#156341=CARTESIAN_POINT('Ctrl Pts',(4.35102676029949,-5.50115256736686,
21.4865450056687));
#156342=CARTESIAN_POINT('Ctrl Pts',(4.49934016166337,-5.38052521116037,
21.4952170804335));
#156343=CARTESIAN_POINT('Ctrl Pts',(4.64248202336562,-5.25404484423449,
21.5038891551982));
#156344=CARTESIAN_POINT('Ctrl Pts',(4.78562185584374,-5.12756627033415,
21.5125611070249));
#156345=CARTESIAN_POINT('Ctrl Pts',(4.92359008252299,-4.99523503982335,
21.5212330588516));
#156346=CARTESIAN_POINT('Ctrl Pts',(5.0559263513206,-4.85749269608529,21.5299050106783));
#156347=CARTESIAN_POINT('Ctrl Pts',(5.18826091680201,-4.71975212524569,
21.5385768508873));
#156348=CARTESIAN_POINT('Ctrl Pts',(5.3149634726938,-4.57660078535446,21.5472486910962));
#156349=CARTESIAN_POINT('Ctrl Pts',(5.43561126741811,-4.4285163104608,21.5559205313051));
#156350=CARTESIAN_POINT('Ctrl Pts',(5.56176013705541,-4.27367975367701,
21.5649877740387));
#156351=CARTESIAN_POINT('Ctrl Pts',(5.68128895686487,-4.11344992041142,
21.5740550167723));
#156352=CARTESIAN_POINT('Ctrl Pts',(5.79376175353991,-3.9484112381714,21.5831222595058));
#156353=CARTESIAN_POINT('Ctrl Pts',(5.90133874236296,-3.79055649462837,
21.5917948158842));
#156354=CARTESIAN_POINT('Ctrl Pts',(6.00246078174175,-3.62830291661756,
21.6004673722627));
#156355=CARTESIAN_POINT('Ctrl Pts',(6.09679041553253,-3.4621919634201,21.6091399286411));
#156356=CARTESIAN_POINT('Ctrl Pts',(6.19111669178686,-3.2960869227186,21.6178121763316));
#156357=CARTESIAN_POINT('Ctrl Pts',(6.27865090596248,-3.12612502860889,
21.626484424022));
#156358=CARTESIAN_POINT('Ctrl Pts',(6.35910096686059,-2.95287342359484,
21.6351566717124));
#156359=CARTESIAN_POINT('Ctrl Pts',(6.43954858437011,-2.77962708049096,
21.6438286560138));
#156360=CARTESIAN_POINT('Ctrl Pts',(6.51291235951956,-2.60309148403956,
21.6525006403151));
#156361=CARTESIAN_POINT('Ctrl Pts',(6.57894750102473,-2.42385567665661,
21.6611726246164));
#156362=CARTESIAN_POINT('Ctrl Pts',(6.64498098171129,-2.24462437714869,
21.6698443908128));
#156363=CARTESIAN_POINT('Ctrl Pts',(6.70368609940885,-2.06269326909929,
21.6785161570091));
#156364=CARTESIAN_POINT('Ctrl Pts',(6.75486698389396,-1.8786693675044,21.6871879232055));
#156365=CARTESIAN_POINT('Ctrl Pts',(6.80605126222514,-1.69463326313493,
21.6958602644337));
#156366=CARTESIAN_POINT('Ctrl Pts',(6.84971023276636,-1.50850436117886,
21.7045326056619));
#156367=CARTESIAN_POINT('Ctrl Pts',(6.88569820761737,-1.32090376489543,
21.7132049468901));
#156368=CARTESIAN_POINT('Ctrl Pts',(6.92168406448238,-1.13331420939547,
21.7218767777285));
#156369=CARTESIAN_POINT('Ctrl Pts',(6.94999977553796,-0.944253411828243,
21.7305486085668));
#156370=CARTESIAN_POINT('Ctrl Pts',(6.97055086371853,-0.754352184866494,
21.7392204394052));
#156371=CARTESIAN_POINT('Ctrl Pts',(6.99110229108013,-0.564447823720618,
21.7478924133659));
#156372=CARTESIAN_POINT('Ctrl Pts',(7.00388880856486,-0.373703287794897,
21.7565643873267));
#156373=CARTESIAN_POINT('Ctrl Pts',(7.00886775178458,-0.182755028642745,
21.7652363612874));
#156374=CARTESIAN_POINT('Ctrl Pts',(7.01045582731893,-0.121850486191596,
21.7680023598284));
#156375=CARTESIAN_POINT('Ctrl Pts',(7.01125000000004,-0.0609252433283521,
21.7707683583695));
#156376=CARTESIAN_POINT('Ctrl Pts',(7.01125,3.83823541218097E-12,21.7735343569105));
#156377=CARTESIAN_POINT('Ctrl Pts',(7.01124999865213,0.000137478978161555,
21.7735343569105));
#156378=CARTESIAN_POINT('Ctrl Pts',(7.01124653752022,0.176650728114333,
21.7815317420282));
#156379=CARTESIAN_POINT('Ctrl Pts',(7.00457296038423,0.353198568577369,
21.789529127146));
#156380=CARTESIAN_POINT('Ctrl Pts',(6.99124745647898,0.529231107150913,
21.7975265122637));
#156381=CARTESIAN_POINT('Ctrl Pts',(6.97791763612368,0.705320666882237,
21.8055264879262));
#156382=CARTESIAN_POINT('Ctrl Pts',(6.95793160765761,0.880894222625239,
21.8135264635886));
#156383=CARTESIAN_POINT('Ctrl Pts',(6.93135956303297,1.05540568998441,21.821526439251));
#156384=CARTESIAN_POINT('Ctrl Pts',(6.90478331956185,1.22994473319893,21.8295276790491));
#156385=CARTESIAN_POINT('Ctrl Pts',(6.87161905072997,1.40342099010502,21.8375289188472));
#156386=CARTESIAN_POINT('Ctrl Pts',(6.83198821305204,1.57529794617335,21.8455301586453));
#156387=CARTESIAN_POINT('Ctrl Pts',(6.7923256440326,1.74731251947895,21.8535378048201));
#156388=CARTESIAN_POINT('Ctrl Pts',(6.7461862551461,1.91772487634906,21.8615454509948));
#156389=CARTESIAN_POINT('Ctrl Pts',(6.69374175506267,2.0860124350134,21.8695530971696));
#156390=CARTESIAN_POINT('Ctrl Pts',(6.65608715443015,2.20684113588473,21.8753025030794));
#156391=CARTESIAN_POINT('Ctrl Pts',(6.61518326434292,2.3265747896752,21.8810519089892));
#156392=CARTESIAN_POINT('Ctrl Pts',(6.57110895151813,2.44502632087638,21.886801314899));
#156393=CARTESIAN_POINT('',(7.01124789938016,0.00542733243739705,21.2264656430542));
#156394=CARTESIAN_POINT('Ctrl Pts',(6.57110895151816,2.44502632087631,21.3399745565681));
#156395=CARTESIAN_POINT('Ctrl Pts',(6.63539956021585,2.2722426617783,21.3315965673332));
#156396=CARTESIAN_POINT('Ctrl Pts',(6.69284066714934,2.09700392013267,21.3232185780983));
#156397=CARTESIAN_POINT('Ctrl Pts',(6.74326910937081,1.91988236126734,21.3148405888634));
#156398=CARTESIAN_POINT('Ctrl Pts',(6.79372545835688,1.74266278450909,21.306457963305));
#156399=CARTESIAN_POINT('Ctrl Pts',(6.83716132020599,1.56355863023882,21.2980753377466));
#156400=CARTESIAN_POINT('Ctrl Pts',(6.87346441855802,1.3831534438799,21.2896927121881));
#156401=CARTESIAN_POINT('Ctrl Pts',(6.90980485689981,1.20256269959023,21.2813014645791));
#156402=CARTESIAN_POINT('Ctrl Pts',(6.93899782154279,1.02066857367475,21.27291021697));
#156403=CARTESIAN_POINT('Ctrl Pts',(6.9609826087011,0.838061861595461,21.2645189693609));
#156404=CARTESIAN_POINT('Ctrl Pts',(6.96367123658769,0.815729987520962,
21.2634927623678));
#156405=CARTESIAN_POINT('Ctrl Pts',(6.96625212254389,0.793387459064572,
21.2624665553746));
#156406=CARTESIAN_POINT('Ctrl Pts',(6.96872520897261,0.771035358676671,
21.2614403483814));
#156407=CARTESIAN_POINT('Ctrl Pts',(6.99682073277436,0.517104092395202,
21.2497821132842));
#156408=CARTESIAN_POINT('Ctrl Pts',(7.01104969501965,0.261475717700782,
21.2381238781869));
#156409=CARTESIAN_POINT('Ctrl Pts',(7.01124789937955,0.00542733321588756,
21.2264656430896));
#156410=CARTESIAN_POINT('Ctrl Pts',(7.01124789938016,0.00542733243739238,
21.2264656430541));
#156411=CARTESIAN_POINT('Ctrl Pts',(7.01138511315678,-0.171830982620558,
21.2183948281805));
#156412=CARTESIAN_POINT('Ctrl Pts',(7.00479604016339,-0.349336638244306,
21.2103240133068));
#156413=CARTESIAN_POINT('Ctrl Pts',(6.99145108150332,-0.526534269963628,
21.2022531984331));
#156414=CARTESIAN_POINT('Ctrl Pts',(6.97774366041824,-0.708544766595712,
21.1939631721549));
#156415=CARTESIAN_POINT('Ctrl Pts',(6.95690808489991,-0.890229896830883,
21.1856731458768));
#156416=CARTESIAN_POINT('Ctrl Pts',(6.92896952314784,-1.07098455161054,
21.1773831195986));
#156417=CARTESIAN_POINT('Ctrl Pts',(6.90182288203468,-1.2466157020749,21.1693280747402));
#156418=CARTESIAN_POINT('Ctrl Pts',(6.86797047923098,-1.42136801354171,
21.1612730298818));
#156419=CARTESIAN_POINT('Ctrl Pts',(6.82748809657842,-1.59468895198405,
21.1532179850234));
#156420=CARTESIAN_POINT('Ctrl Pts',(6.7852342884555,-1.77559405679175,21.1448104680353));
#156421=CARTESIAN_POINT('Ctrl Pts',(6.73575721398845,-1.95493929691785,
21.1364029510473));
#156422=CARTESIAN_POINT('Ctrl Pts',(6.67920292101102,-2.13210574373267,
21.1279954340592));
#156423=CARTESIAN_POINT('Ctrl Pts',(6.62264862803358,-2.30927219054752,
21.1195879170711));
#156424=CARTESIAN_POINT('Ctrl Pts',(6.55901722681694,-2.48425940783944,
21.1111804000831));
#156425=CARTESIAN_POINT('Ctrl Pts',(6.48851466909079,-2.6564645586745,21.102772883095));
#156426=CARTESIAN_POINT('Ctrl Pts',(6.41859245493036,-2.82725219850719,
21.0944345727931));
#156427=CARTESIAN_POINT('Ctrl Pts',(6.34195188302819,-2.995207309943,21.0860962624912));
#156428=CARTESIAN_POINT('Ctrl Pts',(6.25885887899983,-3.15979621103402,
21.0777579521894));
#156429=CARTESIAN_POINT('Ctrl Pts',(6.17571359567259,-3.32448866587731,
21.0694143957056));
#156430=CARTESIAN_POINT('Ctrl Pts',(6.08610793040353,-3.48581039346066,
21.0610708392217));
#156431=CARTESIAN_POINT('Ctrl Pts',(5.99035317373886,-3.64325341094697,
21.0527272827379));
#156432=CARTESIAN_POINT('Ctrl Pts',(5.89452556727291,-3.80081621039437,
21.0443773785127));
#156433=CARTESIAN_POINT('Ctrl Pts',(5.79253970798989,-3.95449413402541,
21.0360274742875));
#156434=CARTESIAN_POINT('Ctrl Pts',(5.68474973207407,-4.1038088462042,21.0276775700623));
#156435=CARTESIAN_POINT('Ctrl Pts',(5.57679807917088,-4.25334751940189,
21.0193151415987));
#156436=CARTESIAN_POINT('Ctrl Pts',(5.46302510476374,-4.39850963729829,
21.0109527131351));
#156437=CARTESIAN_POINT('Ctrl Pts',(5.34382565034685,-4.53884941160147,
21.0025902846714));
#156438=CARTESIAN_POINT('Ctrl Pts',(5.22452426414693,-4.67930919554309,
20.9942207051915));
#156439=CARTESIAN_POINT('Ctrl Pts',(5.09978736044891,-4.81493816732931,
20.9858511257115));
#156440=CARTESIAN_POINT('Ctrl Pts',(4.97004642620975,-4.94532760126361,
20.9774815462315));
#156441=CARTESIAN_POINT('Ctrl Pts',(4.84010538238685,-5.07591814501342,
20.969099057695));
#156442=CARTESIAN_POINT('Ctrl Pts',(4.70514512456409,-5.20125277943508,
20.9607165691584));
#156443=CARTESIAN_POINT('Ctrl Pts',(4.56563102382614,-5.32096231115917,
20.9523340806218));
#156444=CARTESIAN_POINT('Ctrl Pts',(4.51997972399048,-5.36013323149637,
20.9495911930174));
#156445=CARTESIAN_POINT('Ctrl Pts',(4.47384107817438,-5.39870221086967,
20.946848305413));
#156446=CARTESIAN_POINT('Ctrl Pts',(4.42723205493133,-5.43665732728195,
20.9441054178086));
#156447=CARTESIAN_POINT('Ctrl Pts',(4.28466589499679,-5.55275319928833,
20.9357155626758));
#156448=CARTESIAN_POINT('Ctrl Pts',(4.13740883337341,-5.66333692192345,
20.927325707543));
#156449=CARTESIAN_POINT('Ctrl Pts',(3.98591391741853,-5.76802538182949,
20.9189358524102));
#156450=CARTESIAN_POINT('Ctrl Pts',(3.83455879884845,-5.87261723669225,
20.9105537393182));
#156451=CARTESIAN_POINT('Ctrl Pts',(3.67897389091956,-5.97132448761094,
20.9021716262261));
#156452=CARTESIAN_POINT('Ctrl Pts',(3.51964451587096,-6.0638048323144,20.893789513134));
#156453=CARTESIAN_POINT('Ctrl Pts',(3.36043874664803,-6.1562134318713,20.8854139027851));
#156454=CARTESIAN_POINT('Ctrl Pts',(3.19749458510163,-6.24240459184712,
20.8770382924362));
#156455=CARTESIAN_POINT('Ctrl Pts',(3.03132585956567,-6.3220795704917,20.8686626820873));
#156456=CARTESIAN_POINT('Ctrl Pts',(2.86526165662619,-6.40170443239128,
20.8602923401217));
#156457=CARTESIAN_POINT('Ctrl Pts',(2.69597722959344,-6.47482114378974,
20.8519219981561));
#156458=CARTESIAN_POINT('Ctrl Pts',(2.52401090988896,-6.54117691927542,
20.8435516561905));
#156459=CARTESIAN_POINT('Ctrl Pts',(2.3521275512209,-6.60750068300487,20.8351853522961));
#156460=CARTESIAN_POINT('Ctrl Pts',(2.17756518609516,-6.66706989695571,
20.8268190484018));
#156461=CARTESIAN_POINT('Ctrl Pts',(2.00088244508062,-6.71967975453207,
20.8184527445074));
#156462=CARTESIAN_POINT('Ctrl Pts',(1.82424911727737,-6.77227489860562,
20.8100887804338));
#156463=CARTESIAN_POINT('Ctrl Pts',(1.64549691033531,-6.81791447217926,
20.8017248163601));
#156464=CARTESIAN_POINT('Ctrl Pts',(1.46520048148912,-6.85644325518297,
20.7933608522865));
#156465=CARTESIAN_POINT('Ctrl Pts',(1.28493179726724,-6.89496610924723,
20.784998175288));
#156466=CARTESIAN_POINT('Ctrl Pts',(1.10311968623601,-6.92638028575991,
20.7766354982894));
#156467=CARTESIAN_POINT('Ctrl Pts',(0.920350300438577,-6.95058140639923,
20.7682728212909));
#156468=CARTESIAN_POINT('Ctrl Pts',(0.737584677529384,-6.97478202878161,
20.7599103164646));
#156469=CARTESIAN_POINT('Ctrl Pts',(0.553862145010406,-6.99176984866476,
20.7515478116383));
#156470=CARTESIAN_POINT('Ctrl Pts',(0.369775734505855,-7.00149216015205,
20.743185306812));
#156471=CARTESIAN_POINT('Ctrl Pts',(0.18566857659615,-7.01121556738963,
20.734821859492));
#156472=CARTESIAN_POINT('Ctrl Pts',(0.00119778714406746,-7.01367181686933,
20.7264584121721));
#156473=CARTESIAN_POINT('Ctrl Pts',(-0.183041394477139,-7.00886027899029,
20.7180949648521));
#156474=CARTESIAN_POINT('Ctrl Pts',(-0.367389061307,-7.00404590794251,20.7097265928993));
#156475=CARTESIAN_POINT('Ctrl Pts',(-0.551504518878142,-6.99195520574972,
20.7013582209465));
#156476=CARTESIAN_POINT('Ctrl Pts',(-0.73479440003731,-6.9726396545479,
20.6929898489937));
#156477=CARTESIAN_POINT('Ctrl Pts',(-0.918139199635379,-6.9533183159021,
20.684618969658));
#156478=CARTESIAN_POINT('Ctrl Pts',(-1.1006576032259,-6.92676785149453,
20.6762480903222));
#156479=CARTESIAN_POINT('Ctrl Pts',(-1.2817635414756,-6.89309138095847,
20.6678772109864));
#156480=CARTESIAN_POINT('Ctrl Pts',(-1.46302292882833,-6.8593863767131,
20.6594992390951));
#156481=CARTESIAN_POINT('Ctrl Pts',(-1.64286713709922,-6.81854336718237,
20.6511212672038));
#156482=CARTESIAN_POINT('Ctrl Pts',(-1.82072128778139,-6.77071639892853,
20.6427432953125));
#156483=CARTESIAN_POINT('Ctrl Pts',(-1.93374904881,-6.74032197114721,20.6374190259536));
#156484=CARTESIAN_POINT('Ctrl Pts',(-2.04597335456467,-6.70710794305146,
20.6320947565947));
#156485=CARTESIAN_POINT('Ctrl Pts',(-2.15725019586194,-6.67112420473144,
20.6267704872357));
#156486=CARTESIAN_POINT('Ctrl Pts',(-2.32158279427387,-6.61798375655042,
20.6189076560465));
#156487=CARTESIAN_POINT('Ctrl Pts',(-2.48418984036692,-6.55868970666415,
20.6110448248572));
#156488=CARTESIAN_POINT('Ctrl Pts',(-2.64455671375529,-6.4933771144322,
20.6031819936679));
#156489=CARTESIAN_POINT('Ctrl Pts',(-2.80480036636881,-6.42811470630656,
20.5953252040265));
#156490=CARTESIAN_POINT('Ctrl Pts',(-2.96280691845738,-6.35684309511127,
20.5874684143852));
#156491=CARTESIAN_POINT('Ctrl Pts',(-3.11807649193003,-6.27974725231624,
20.5796116247438));
#156492=CARTESIAN_POINT('Ctrl Pts',(-3.27325850071401,-6.20269488792668,
20.5717592659599));
#156493=CARTESIAN_POINT('Ctrl Pts',(-3.42570626088162,-6.11982499477387,
20.5639069071759));
#156494=CARTESIAN_POINT('Ctrl Pts',(-3.5749397274518,-6.0313706989031,20.556054548392));
#156495=CARTESIAN_POINT('Ctrl Pts',(-3.72413795825914,-5.94293728812374,
20.5482040436415));
#156496=CARTESIAN_POINT('Ctrl Pts',(-3.87012307396475,-5.84892228586267,
20.5403535388911));
#156497=CARTESIAN_POINT('Ctrl Pts',(-4.01243957350879,-5.74960478915208,
20.5325030341407));
#156498=CARTESIAN_POINT('Ctrl Pts',(-4.15473317881393,-5.6503032694962,
20.5246537922891));
#156499=CARTESIAN_POINT('Ctrl Pts',(-4.29335903164857,-5.54570117428187,
20.5168045504374));
#156500=CARTESIAN_POINT('Ctrl Pts',(-4.42789097195009,-5.43612068510467,
20.5089553085858));
#156501=CARTESIAN_POINT('Ctrl Pts',(-4.56246823869516,-5.32650327611613,
20.5011034221709));
#156502=CARTESIAN_POINT('Ctrl Pts',(-4.69294854172649,-5.21190436398546,
20.4932515357561));
#156503=CARTESIAN_POINT('Ctrl Pts',(-4.81893900704827,-5.09268626648536,
20.4853996493412));
#156504=CARTESIAN_POINT('Ctrl Pts',(-4.91145223756234,-5.00514590136879,
20.4796341068773));
#156505=CARTESIAN_POINT('Ctrl Pts',(-5.0015453307585,-4.9151158191756,20.4738685644133));
#156506=CARTESIAN_POINT('Ctrl Pts',(-5.08907563104132,-4.8227518891232,
20.4681030219493));
#156507=CARTESIAN_POINT('Ctrl Pts',(-5.23565883552314,-4.66807401412598,
20.4584477175894));
#156508=CARTESIAN_POINT('Ctrl Pts',(-5.37497948782157,-4.50692938614802,
20.4487924132295));
#156509=CARTESIAN_POINT('Ctrl Pts',(-5.50656696611878,-4.33997083056435,
20.4391371088697));
#156510=CARTESIAN_POINT('Ctrl Pts',(-5.63888341436103,-4.17208735590279,
20.4294283159349));
#156511=CARTESIAN_POINT('Ctrl Pts',(-5.76338078437975,-3.99832542999536,
20.4197195230001));
#156512=CARTESIAN_POINT('Ctrl Pts',(-5.87962792320022,-3.81937194407984,
20.4100107300653));
#156513=CARTESIAN_POINT('Ctrl Pts',(-5.99643445312257,-3.6395573187962,
20.4002552175946));
#156514=CARTESIAN_POINT('Ctrl Pts',(-6.10491115573031,-3.45450109818584,
20.3904997051239));
#156515=CARTESIAN_POINT('Ctrl Pts',(-6.20466818990484,-3.26492254359625,
20.3807441926532));
#156516=CARTESIAN_POINT('Ctrl Pts',(-6.30452399889056,-3.07515627707146,
20.3709790207242));
#156517=CARTESIAN_POINT('Ctrl Pts',(-6.39564286188179,-2.88085875906645,
20.3612138487953));
#156518=CARTESIAN_POINT('Ctrl Pts',(-6.47768131127819,-2.68277307874096,
20.3514486768664));
#156519=CARTESIAN_POINT('Ctrl Pts',(-6.55960790311003,-2.48495748374668,
20.3416968195279));
#156520=CARTESIAN_POINT('Ctrl Pts',(-6.63247881191103,-2.28336408463178,
20.3319449621894));
#156521=CARTESIAN_POINT('Ctrl Pts',(-6.69599944080583,-2.07875396601617,
20.3221931048508));
#156522=CARTESIAN_POINT('Ctrl Pts',(-6.72369903538632,-1.98952913573145,
20.3179405887882));
#156523=CARTESIAN_POINT('Ctrl Pts',(-6.74962119971176,-1.89973091568127,
20.3136880727255));
#156524=CARTESIAN_POINT('Ctrl Pts',(-6.77374435742456,-1.80942364933117,
20.3094355566629));
#156525=CARTESIAN_POINT('Ctrl Pts',(-6.81931324488791,-1.63883231521045,
20.3014025110641));
#156526=CARTESIAN_POINT('Ctrl Pts',(-6.85848122771501,-1.46634030115633,
20.2933694654652));
#156527=CARTESIAN_POINT('Ctrl Pts',(-6.89109073719453,-1.29247631090546,
20.2853364198664));
#156528=CARTESIAN_POINT('Ctrl Pts',(-6.9236792840256,-1.1187240871228,20.2773085382186));
#156529=CARTESIAN_POINT('Ctrl Pts',(-6.94971768234484,-0.943602001488677,
20.2692806565709));
#156530=CARTESIAN_POINT('Ctrl Pts',(-6.96909872353552,-0.767651968092048,
20.2612527749231));
#156531=CARTESIAN_POINT('Ctrl Pts',(-6.98847101399519,-0.591781377868698,
20.253228517943));
#156532=CARTESIAN_POINT('Ctrl Pts',(-7.00119189229136,-0.415083947823816,
20.2452042609628));
#156533=CARTESIAN_POINT('Ctrl Pts',(-7.00720559944525,-0.23810974277255,
20.2371800039827));
#156534=CARTESIAN_POINT('Ctrl Pts',(-7.01321857948067,-0.0611569357055864,
20.229156717217));
#156535=CARTESIAN_POINT('Ctrl Pts',(-7.01252598353118,0.116072213828916,
20.2211334304513));
#156536=CARTESIAN_POINT('Ctrl Pts',(-7.00512407177512,0.293024404336646,
20.2131101436856));
#156537=CARTESIAN_POINT('Ctrl Pts',(-6.99772276653969,0.469962095190731,
20.2050875143566));
#156538=CARTESIAN_POINT('Ctrl Pts',(-6.9836132599218,0.646622506066317,
20.1970648850277));
#156539=CARTESIAN_POINT('Ctrl Pts',(-6.9628438952237,0.822454529591783,
20.1890422556988));
#156540=CARTESIAN_POINT('Ctrl Pts',(-6.94206672272314,0.998352653439866,
20.1810166104324));
#156541=CARTESIAN_POINT('Ctrl Pts',(-6.91462473673029,1.1734214039036,20.172990965166));
#156542=CARTESIAN_POINT('Ctrl Pts',(-6.88061795613055,1.34711658896841,
20.1649653198996));
#156543=CARTESIAN_POINT('Ctrl Pts',(-6.86056548601809,1.44953785454439,
20.1602329103919));
#156544=CARTESIAN_POINT('Ctrl Pts',(-6.83823141035492,1.55148170121444,
20.1555005008842));
#156545=CARTESIAN_POINT('Ctrl Pts',(-6.81364449281798,1.65283855472677,
20.1507680913764));
#156546=CARTESIAN_POINT('Ctrl Pts',(-6.76828810714593,1.83981524798255,
20.1420380425418));
#156547=CARTESIAN_POINT('Ctrl Pts',(-6.71524003955314,2.02488717757644,
20.1333079937072));
#156548=CARTESIAN_POINT('Ctrl Pts',(-6.65468693636266,2.20743478759943,
20.1245779448725));
#156549=CARTESIAN_POINT('Ctrl Pts',(-6.59411632416657,2.39003518149246,
20.1158453717334));
#156550=CARTESIAN_POINT('Ctrl Pts',(-6.52603643100342,2.57010953886378,
20.1071127985942));
#156551=CARTESIAN_POINT('Ctrl Pts',(-6.4506831321688,2.74705545827762,20.098380225455));
#156552=CARTESIAN_POINT('Ctrl Pts',(-6.37425931943792,2.92651517693516,
20.0895235921746));
#156553=CARTESIAN_POINT('Ctrl Pts',(-6.29035397886495,3.1027566245927,20.0806669588942));
#156554=CARTESIAN_POINT('Ctrl Pts',(-6.19926304082612,3.27517393631961,
20.0718103256138));
#156555=CARTESIAN_POINT('Ctrl Pts',(-6.10939089357683,3.44528431569942,
20.063072193507));
#156556=CARTESIAN_POINT('Ctrl Pts',(-6.01252439058699,3.61167202223607,
20.0543340614003));
#156557=CARTESIAN_POINT('Ctrl Pts',(-5.90899371920414,3.77378056978755,
20.0455959292935));
#156558=CARTESIAN_POINT('Ctrl Pts',(-5.80335701888056,3.93918674197647,
20.0366800454263));
#156559=CARTESIAN_POINT('Ctrl Pts',(-5.69078227619342,4.1001375447335,20.027764161559));
#156560=CARTESIAN_POINT('Ctrl Pts',(-5.57166689361946,4.25607267196472,
20.0188482776918));
#156561=CARTESIAN_POINT('Ctrl Pts',(-5.45255151104551,4.41200779919593,
20.0099323938245));
#156562=CARTESIAN_POINT('Ctrl Pts',(-5.32689567699348,4.56292701427444,
20.0010165099573));
#156563=CARTESIAN_POINT('Ctrl Pts',(-5.19514124450627,4.7083047917621,19.99210062609));
#156564=CARTESIAN_POINT('Ctrl Pts',(-5.06597581991149,4.85082585918546,
19.9833599415938));
#156565=CARTESIAN_POINT('Ctrl Pts',(-4.93093553144688,4.98803638595718,
19.9746192570976));
#156566=CARTESIAN_POINT('Ctrl Pts',(-4.79047193705921,5.1194731352697,19.9658785726013));
#156567=CARTESIAN_POINT('Ctrl Pts',(-4.65003361440603,5.25088623692714,
19.9571394606995));
#156568=CARTESIAN_POINT('Ctrl Pts',(-4.50417413431041,5.37652744868072,
19.9484003487976));
#156569=CARTESIAN_POINT('Ctrl Pts',(-4.35338084660384,5.49597141249141,
19.9396612368958));
#156570=CARTESIAN_POINT('Ctrl Pts',(-4.20063381482535,5.61696294476334,
19.9308088972214));
#156571=CARTESIAN_POINT('Ctrl Pts',(-4.04282444450216,5.73159532650693,
19.9219565575471));
#156572=CARTESIAN_POINT('Ctrl Pts',(-3.8804937669024,5.83946869907971,19.9131042178727));
#156573=CARTESIAN_POINT('Ctrl Pts',(-3.72032155381722,5.9459077103216,19.904369585223));
#156574=CARTESIAN_POINT('Ctrl Pts',(-3.5557477655038,6.04576619743504,19.8956349525732));
#156575=CARTESIAN_POINT('Ctrl Pts',(-3.38732197767626,6.13870315148496,
19.8869003199234));
#156576=CARTESIAN_POINT('Ctrl Pts',(-3.21549165657141,6.23351871899922,
19.8779891267368));
#156577=CARTESIAN_POINT('Ctrl Pts',(-3.03965219368265,6.32112979232151,
19.8690779335502));
#156578=CARTESIAN_POINT('Ctrl Pts',(-2.86041524351101,6.40122263299675,
19.8601667403635));
#156579=CARTESIAN_POINT('Ctrl Pts',(-2.68117829333937,6.481315473672,19.8512555471769));
#156580=CARTESIAN_POINT('Ctrl Pts',(-2.49854412714317,6.55388994572913,
19.8423443539902));
#156581=CARTESIAN_POINT('Ctrl Pts',(-2.31314879546395,6.61868334433244,
19.8334331608036));
#156582=CARTESIAN_POINT('Ctrl Pts',(-2.1461766778035,6.67703805519394,19.8254074959512));
#156583=CARTESIAN_POINT('Ctrl Pts',(-1.9768879904627,6.72910763299868,19.8173818310988));
#156584=CARTESIAN_POINT('Ctrl Pts',(-1.80580461755068,6.77471004883107,
19.8093561662464));
#156585=CARTESIAN_POINT('Ctrl Pts',(-1.63477554230475,6.82029799157525,
19.8013330485432));
#156586=CARTESIAN_POINT('Ctrl Pts',(-1.46195326926839,6.85942276441783,
19.79330993084));
#156587=CARTESIAN_POINT('Ctrl Pts',(-1.28787484800511,6.89195218630947,
19.7852868131368));
#156588=CARTESIAN_POINT('Ctrl Pts',(-1.11381837955452,6.92447750595626,
19.7772647072189));
#156589=CARTESIAN_POINT('Ctrl Pts',(-0.938506438753643,6.95040906463208,
19.7692426013011));
#156590=CARTESIAN_POINT('Ctrl Pts',(-0.762486221020042,6.96966579724269,
19.7612204953832));
#156591=CARTESIAN_POINT('Ctrl Pts',(-0.586400593578624,6.98892968572022,
19.7531954084237));
#156592=CARTESIAN_POINT('Ctrl Pts',(-0.409606527828915,7.00151375021644,
19.7451703214642));
#156593=CARTESIAN_POINT('Ctrl Pts',(-0.232656750402027,7.00738877178885,
19.7371452345047));
#156594=CARTESIAN_POINT('Ctrl Pts',(-0.0556721236026742,7.01326495041733,
19.7291185670444));
#156595=CARTESIAN_POINT('Ctrl Pts',(0.121467909313705,7.01242945049053,
19.7210918995842));
#156596=CARTESIAN_POINT('Ctrl Pts',(0.298210870223755,7.00490519845775,
19.713065232124));
#156597=CARTESIAN_POINT('Ctrl Pts',(0.475095719760626,6.99737490598193,
19.7050321208834));
#156598=CARTESIAN_POINT('Ctrl Pts',(0.65158249485985,6.9831451616253,19.6969990096428));
#156599=CARTESIAN_POINT('Ctrl Pts',(0.82712345741225,6.96229081184479,19.6889658984023));
#156600=CARTESIAN_POINT('Ctrl Pts',(0.930558569422978,6.95000267137836,
19.6842324974405));
#156601=CARTESIAN_POINT('Ctrl Pts',(1.03366543805472,6.93541544974664,19.6794990964788));
#156602=CARTESIAN_POINT('Ctrl Pts',(1.1363337643841,6.9185527488356,19.6747656955171));
#156603=CARTESIAN_POINT('Ctrl Pts',(1.34783371187111,6.88381506015708,19.6650147422229));
#156604=CARTESIAN_POINT('Ctrl Pts',(1.55759675625066,6.83939833325033,19.6552637889286));
#156605=CARTESIAN_POINT('Ctrl Pts',(1.76482985845557,6.78549940190136,19.6455128356344));
#156606=CARTESIAN_POINT('Ctrl Pts',(1.97236151881738,6.73152281903131,19.6357478342628));
#156607=CARTESIAN_POINT('Ctrl Pts',(2.17735590882976,6.6680367156351,19.6259828328913));
#156608=CARTESIAN_POINT('Ctrl Pts',(2.37903269260381,6.59528847056915,19.6162178315197));
#156609=CARTESIAN_POINT('Ctrl Pts',(2.58037332296702,6.52266148175417,19.6064691063821));
#156610=CARTESIAN_POINT('Ctrl Pts',(2.7784073631806,6.44080321856691,19.5967203812445));
#156611=CARTESIAN_POINT('Ctrl Pts',(2.97237492972121,6.35000896374681,19.5869716561069));
#156612=CARTESIAN_POINT('Ctrl Pts',(3.16581013049678,6.25946390395344,19.57724968744));
#156613=CARTESIAN_POINT('Ctrl Pts',(3.35520110233162,6.16003183127222,19.5675277187732));
#156614=CARTESIAN_POINT('Ctrl Pts',(3.53981127424797,6.05205442021195,19.5578057501063));
#156615=CARTESIAN_POINT('Ctrl Pts',(3.72319992887888,5.94479146747582,19.5481481091666));
#156616=CARTESIAN_POINT('Ctrl Pts',(3.90187078622064,5.82909588576575,19.5384904682269));
#156617=CARTESIAN_POINT('Ctrl Pts',(4.07511940342092,5.70535085777925,19.5288328272872));
#156618=CARTESIAN_POINT('Ctrl Pts',(4.15126813527024,5.65096065769506,19.5245879616017));
#156619=CARTESIAN_POINT('Ctrl Pts',(4.22636957634119,5.59501601051856,19.5203430959162));
#156620=CARTESIAN_POINT('Ctrl Pts',(4.30036504556353,5.5375524410515,19.5160982302307));
#156621=CARTESIAN_POINT('Ctrl Pts',(4.43723653858669,5.43126046628527,19.5082463832168));
#156622=CARTESIAN_POINT('Ctrl Pts',(4.57026540768506,5.31981216424165,19.5003945362029));
#156623=CARTESIAN_POINT('Ctrl Pts',(4.69902863801488,5.20353307106009,19.492542689189));
#156624=CARTESIAN_POINT('Ctrl Pts',(4.82775535213286,5.08728695368993,19.4846930688955));
#156625=CARTESIAN_POINT('Ctrl Pts',(4.95221855095236,4.96621302570285,19.4768434486019));
#156626=CARTESIAN_POINT('Ctrl Pts',(5.07202870601983,4.84067674688269,19.4689938283084));
#156627=CARTESIAN_POINT('Ctrl Pts',(5.19182929578005,4.71515049052748,19.4611448347065));
#156628=CARTESIAN_POINT('Ctrl Pts',(5.30697731848823,4.58516286903166,19.4532958411047));
#156629=CARTESIAN_POINT('Ctrl Pts',(5.41712068377745,4.45111559722847,19.4454468475029));
#156630=CARTESIAN_POINT('Ctrl Pts',(5.52731981142681,4.31700046121734,19.4375938801854));
#156631=CARTESIAN_POINT('Ctrl Pts',(5.63250897668519,4.17882186345816,19.429740912868));
#156632=CARTESIAN_POINT('Ctrl Pts',(5.73237671783214,4.0370142094568,19.4218879455506));
#156633=CARTESIAN_POINT('Ctrl Pts',(5.83226982203013,3.89517054107555,19.4140329838433));
#156634=CARTESIAN_POINT('Ctrl Pts',(5.92683860175204,3.74969630015664,19.406178022136));
#156635=CARTESIAN_POINT('Ctrl Pts',(6.01581578437549,3.60105359734602,19.3983230604287));
#156636=CARTESIAN_POINT('Ctrl Pts',(6.1048812842898,3.45226335422865,19.3904603020153));
#156637=CARTESIAN_POINT('Ctrl Pts',(6.18834391853178,3.300298702136,19.382597543602));
#156638=CARTESIAN_POINT('Ctrl Pts',(6.26598283970866,3.14564550052555,19.3747347851887));
#156639=CARTESIAN_POINT('Ctrl Pts',(6.32293763823132,3.03219413096644,19.3689667784406));
#156640=CARTESIAN_POINT('Ctrl Pts',(6.37675939458714,2.91729641313367,19.3631987716924));
#156641=CARTESIAN_POINT('Ctrl Pts',(6.42737773349486,2.80115012690761,19.3574307649443));
#156642=CARTESIAN_POINT('Ctrl Pts',(6.47852634438862,2.68378710534023,19.3516023332107));
#156643=CARTESIAN_POINT('Ctrl Pts',(6.52645943403865,2.56502373828055,19.3457739014771));
#156644=CARTESIAN_POINT('Ctrl Pts',(6.57110895151814,2.44502632087635,19.3399454697435));
#156645=CARTESIAN_POINT('Origin',(0.,0.,50.));
#156646=CARTESIAN_POINT('',(6.57110895151813,2.44502632087639,17.3396585048403));
#156647=CARTESIAN_POINT('',(6.57110895151814,2.44502632087637,17.886889234273));
#156648=CARTESIAN_POINT('',(6.57110895151814,2.44502632087636,50.));
#156649=CARTESIAN_POINT('',(7.01124873670978,-0.00420885798051574,19.7735343569105));
#156650=CARTESIAN_POINT('Ctrl Pts',(6.57110895151814,2.44502632087637,17.886889234273));
#156651=CARTESIAN_POINT('Ctrl Pts',(6.50720292022931,2.61677641234676,17.8952010218137));
#156652=CARTESIAN_POINT('Ctrl Pts',(6.43654999129877,2.7860443294507,17.9035128093544));
#156653=CARTESIAN_POINT('Ctrl Pts',(6.35937398010672,2.95228541026128,17.9118245968952));
#156654=CARTESIAN_POINT('Ctrl Pts',(6.28219796040125,3.11852650941021,17.9201363853528));
#156655=CARTESIAN_POINT('Ctrl Pts',(6.19849899777784,3.28174046743073,17.9284481738104));
#156656=CARTESIAN_POINT('Ctrl Pts',(6.10854821986263,3.44140454002622,17.936759962268));
#156657=CARTESIAN_POINT('Ctrl Pts',(6.01858428500979,3.6010919663969,17.9450729664759));
#156658=CARTESIAN_POINT('Ctrl Pts',(5.9223668763525,3.75722818017718,17.9533859706838));
#156659=CARTESIAN_POINT('Ctrl Pts',(5.82021223161276,3.90931658240738,17.9616989748917));
#156660=CARTESIAN_POINT('Ctrl Pts',(5.71802771142493,4.06144946337053,17.9700144102638));
#156661=CARTESIAN_POINT('Ctrl Pts',(5.60990268043997,4.20953189468716,17.978329845636));
#156662=CARTESIAN_POINT('Ctrl Pts',(5.49619589916734,4.35309742602622,17.9866452810082));
#156663=CARTESIAN_POINT('Ctrl Pts',(5.38238573978476,4.49679348197531,17.9949682764747));
#156664=CARTESIAN_POINT('Ctrl Pts',(5.26298389790001,4.63596416891988,18.0032912719412));
#156665=CARTESIAN_POINT('Ctrl Pts',(5.13838927820155,4.77017632673714,18.0116142674077));
#156666=CARTESIAN_POINT('Ctrl Pts',(5.01373525021222,4.9044524786091,18.0199412313838));
#156667=CARTESIAN_POINT('Ctrl Pts',(4.88388374072292,5.03376514662664,18.0282681953598));
#156668=CARTESIAN_POINT('Ctrl Pts',(4.74926986522116,5.15771871177579,18.0365951593359));
#156669=CARTESIAN_POINT('Ctrl Pts',(4.61449645450883,5.28181917826067,18.0449319918633));
#156670=CARTESIAN_POINT('Ctrl Pts',(4.47494965115375,5.40054762878076,18.0532688243908));
#156671=CARTESIAN_POINT('Ctrl Pts',(4.33109795261695,5.51354850231113,18.0616056569182));
#156672=CARTESIAN_POINT('Ctrl Pts',(4.22764270329482,5.59481645857174,18.0676013392526));
#156673=CARTESIAN_POINT('Ctrl Pts',(4.12196155486622,5.67312285929934,18.0735970215869));
#156674=CARTESIAN_POINT('Ctrl Pts',(4.0142377187002,5.74834951096962,18.0795927039213));
#156675=CARTESIAN_POINT('Ctrl Pts',(3.86365171675359,5.85350804521824,18.0879740043262));
#156676=CARTESIAN_POINT('Ctrl Pts',(3.70875556564004,5.95286840638979,18.0963553047311));
#156677=CARTESIAN_POINT('Ctrl Pts',(3.55002072808778,6.04607140155052,18.104736605136));
#156678=CARTESIAN_POINT('Ctrl Pts',(3.39148706370483,6.13915627555893,18.1131072834695));
#156679=CARTESIAN_POINT('Ctrl Pts',(3.2291246885253,6.22609917068576,18.1214779618031));
#156680=CARTESIAN_POINT('Ctrl Pts',(3.06343546059869,6.3065830479941,18.1298486401366));
#156681=CARTESIAN_POINT('Ctrl Pts',(2.89793426149854,6.38697558991999,18.1382098191875));
#156682=CARTESIAN_POINT('Ctrl Pts',(2.72911402738059,6.46092358098648,18.1465709982383));
#156683=CARTESIAN_POINT('Ctrl Pts',(2.55750312363193,6.52815474197058,18.1549321772891));
#156684=CARTESIAN_POINT('Ctrl Pts',(2.38611490527401,6.59529866259274,18.1632825067238));
#156685=CARTESIAN_POINT('Ctrl Pts',(2.21194354383317,6.65574301892446,18.1716328361585));
#156686=CARTESIAN_POINT('Ctrl Pts',(2.0355393095366,6.70926272267164,18.1799831655933));
#156687=CARTESIAN_POINT('Ctrl Pts',(1.85927080774591,6.76274124620831,18.188327069949));
#156688=CARTESIAN_POINT('Ctrl Pts',(1.68077316909132,6.80930564038414,18.1966709743047));
#156689=CARTESIAN_POINT('Ctrl Pts',(1.50061491265684,6.8487795589004,18.2050148786604));
#156690=CARTESIAN_POINT('Ctrl Pts',(1.32060136045763,6.88822177171909,18.2133520811402));
#156691=CARTESIAN_POINT('Ctrl Pts',(1.13893016972089,6.92058479704801,18.2216892836199));
#156692=CARTESIAN_POINT('Ctrl Pts',(0.95618338206577,6.94574257386216,18.2300264860996));
#156693=CARTESIAN_POINT('Ctrl Pts',(0.896024148307747,6.95402437512178,
18.2327710471356));
#156694=CARTESIAN_POINT('Ctrl Pts',(0.835748452853124,6.96152575851747,
18.2355156081717));
#156695=CARTESIAN_POINT('Ctrl Pts',(0.775377323396824,6.96824343495992,
18.2382601692078));
#156696=CARTESIAN_POINT('Ctrl Pts',(0.591962487993929,6.98865255319371,
18.2465984795097));
#156697=CARTESIAN_POINT('Ctrl Pts',(0.407816762156593,7.00180733844378,
18.2549367898116));
#156698=CARTESIAN_POINT('Ctrl Pts',(0.223536000565575,7.00768565354862,
18.2632751001135));
#156699=CARTESIAN_POINT('Ctrl Pts',(0.0391392957724966,7.01356766708986,
18.2716186565973));
#156700=CARTESIAN_POINT('Ctrl Pts',(-0.145392286753549,7.01216406843363,
18.2799622130811));
#156701=CARTESIAN_POINT('Ctrl Pts',(-0.329463727106422,7.00350485221658,
18.2883057695649));
#156702=CARTESIAN_POINT('Ctrl Pts',(-0.513675208208637,6.99483904810558,
18.2966556737901));
#156703=CARTESIAN_POINT('Ctrl Pts',(-0.697425521935273,6.97890663113029,
18.3050055780153));
#156704=CARTESIAN_POINT('Ctrl Pts',(-0.880125155554621,6.95578940689408,
18.3133554822406));
#156705=CARTESIAN_POINT('Ctrl Pts',(-1.0630988251048,6.93263750853218,18.3217179107042));
#156706=CARTESIAN_POINT('Ctrl Pts',(-1.24501833997801,6.90227930888075,
18.3300803391679));
#156707=CARTESIAN_POINT('Ctrl Pts',(-1.4253032655709,6.86484793448864,18.3384427676315));
#156708=CARTESIAN_POINT('Ctrl Pts',(-1.60574235935173,6.82738455116875,
18.3468123471115));
#156709=CARTESIAN_POINT('Ctrl Pts',(-1.78454375771095,6.78283600375344,
18.3551819265915));
#156710=CARTESIAN_POINT('Ctrl Pts',(-1.96114201224715,6.73138533812314,
18.3635515060714));
#156711=CARTESIAN_POINT('Ctrl Pts',(-2.13801264807444,6.6798553161098,18.371933994608));
#156712=CARTESIAN_POINT('Ctrl Pts',(-2.31267303959052,6.62140200642896,
18.3803164831446));
#156713=CARTESIAN_POINT('Ctrl Pts',(-2.48457621511136,6.55625713298395,
18.3886989716812));
#156714=CARTESIAN_POINT('Ctrl Pts',(-2.54082575094134,6.53494066293107,
18.3914418592855));
#156715=CARTESIAN_POINT('Ctrl Pts',(-2.59678025700478,6.51290809479449,
18.3941847468898));
#156716=CARTESIAN_POINT('Ctrl Pts',(-2.6524211410294,6.49016861515325,18.3969276344942));
#156717=CARTESIAN_POINT('Ctrl Pts',(-2.82261366211137,6.42061383657494,
18.405317489627));
#156718=CARTESIAN_POINT('Ctrl Pts',(-2.99021376345989,6.34430126921102,
18.4137073447597));
#156719=CARTESIAN_POINT('Ctrl Pts',(-3.15466815543368,6.26144515200706,
18.4220971998925));
#156720=CARTESIAN_POINT('Ctrl Pts',(-3.31897079120009,6.17866549326646,
18.4304793129846));
#156721=CARTESIAN_POINT('Ctrl Pts',(-3.48013321219892,6.08935446921592,
18.4388614260767));
#156722=CARTESIAN_POINT('Ctrl Pts',(-3.63762249876473,5.99377419652932,
18.4472435391688));
#156723=CARTESIAN_POINT('Ctrl Pts',(-3.79498960702314,5.89826807387661,
18.4556191495177));
#156724=CARTESIAN_POINT('Ctrl Pts',(-3.94868898201726,5.79650256908108,
18.4639947598666));
#156725=CARTESIAN_POINT('Ctrl Pts',(-4.09821229259012,5.68878568478047,
18.4723703702154));
#156726=CARTESIAN_POINT('Ctrl Pts',(-4.24764155078007,5.58113655599978,
18.480740712181));
#156727=CARTESIAN_POINT('Ctrl Pts',(-4.39289971613055,5.46754370358145,
18.4891110541466));
#156728=CARTESIAN_POINT('Ctrl Pts',(-4.53350706626756,5.34835864939909,
18.4974813961122));
#156729=CARTESIAN_POINT('Ctrl Pts',(-4.67404658375184,5.22923109319521,
18.5058477000065));
#156730=CARTESIAN_POINT('Ctrl Pts',(-4.80993950996139,5.10451692730062,
18.5142140039008));
#156731=CARTESIAN_POINT('Ctrl Pts',(-4.94073852006542,4.97460847090922,
18.5225803077952));
#156732=CARTESIAN_POINT('Ctrl Pts',(-5.07150094935249,4.84473634627187,
18.5309442718688));
#156733=CARTESIAN_POINT('Ctrl Pts',(-5.19717206921861,4.70967305816532,
18.5393082359424));
#156734=CARTESIAN_POINT('Ctrl Pts',(-5.31734040985135,4.56984874238326,
18.547672200016));
#156735=CARTESIAN_POINT('Ctrl Pts',(-5.43749025857343,4.43004594323979,
18.5560348770146));
#156736=CARTESIAN_POINT('Ctrl Pts',(-5.55213880223159,4.28548382634671,
18.5643975540131));
#156737=CARTESIAN_POINT('Ctrl Pts',(-5.66091369828726,4.13662696687092,
18.5727602310116));
#156738=CARTESIAN_POINT('Ctrl Pts',(-5.76968635486656,3.98777317208588,
18.581122735838));
#156739=CARTESIAN_POINT('Ctrl Pts',(-5.87258541139571,3.83462507661903,
18.5894852406643));
#156740=CARTESIAN_POINT('Ctrl Pts',(-5.96928059209804,3.67767804127845,
18.5978477454906));
#156741=CARTESIAN_POINT('Ctrl Pts',(-6.06598667080267,3.52071331726776,
18.6062111928106));
#156742=CARTESIAN_POINT('Ctrl Pts',(-6.15648730773891,3.35994907983606,
18.6145746401305));
#156743=CARTESIAN_POINT('Ctrl Pts',(-6.24049688580979,3.19590756760867,
18.6229380874505));
#156744=CARTESIAN_POINT('Ctrl Pts',(-6.32455593108116,3.0317694631288,18.6313064594033));
#156745=CARTESIAN_POINT('Ctrl Pts',(-6.40211612916342,2.86435052014575,
18.6396748313561));
#156746=CARTESIAN_POINT('Ctrl Pts',(-6.47293850667817,2.69419629041075,
18.6480432033089));
#156747=CARTESIAN_POINT('Ctrl Pts',(-6.54378210442819,2.52399107802149,
18.6564140826447));
#156748=CARTESIAN_POINT('Ctrl Pts',(-6.60788373468658,2.35104925020757,
18.6647849619805));
#156749=CARTESIAN_POINT('Ctrl Pts',(-6.66505324983363,2.1759346817821,18.6731558413162));
#156750=CARTESIAN_POINT('Ctrl Pts',(-6.72227120409265,2.00067174067645,
18.6815338132075));
#156751=CARTESIAN_POINT('Ctrl Pts',(-6.77254520996378,1.82323269477702,
18.6899117850988));
#156752=CARTESIAN_POINT('Ctrl Pts',(-6.81573518619107,1.6441959841263,18.6982897569901));
#156753=CARTESIAN_POINT('Ctrl Pts',(-6.84318276778077,1.5304166966065,18.7036140263491));
#156754=CARTESIAN_POINT('Ctrl Pts',(-6.86777033888593,1.41599240804873,
18.7089382957081));
#156755=CARTESIAN_POINT('Ctrl Pts',(-6.88947272927076,1.30107343187635,
18.7142625650671));
#156756=CARTESIAN_POINT('Ctrl Pts',(-6.92152261639967,1.13136216274959,
18.7221253962563));
#156757=CARTESIAN_POINT('Ctrl Pts',(-6.94734408917821,0.960218692717945,
18.7299882274456));
#156758=CARTESIAN_POINT('Ctrl Pts',(-6.96680925618418,0.788159470187608,
18.7378510586349));
#156759=CARTESIAN_POINT('Ctrl Pts',(-6.98625946677869,0.616232452458246,
18.7457078482763));
#156760=CARTESIAN_POINT('Ctrl Pts',(-6.99936304151817,0.443391457915472,
18.7535646379176));
#156761=CARTESIAN_POINT('Ctrl Pts',(-7.00604296529355,0.270163896479033,
18.761421427559));
#156762=CARTESIAN_POINT('Ctrl Pts',(-7.01271912190814,0.0970340271870361,
18.769273786343));
#156763=CARTESIAN_POINT('Ctrl Pts',(-7.01297881916429,-0.0764815955348706,
18.7771261451269));
#156764=CARTESIAN_POINT('Ctrl Pts',(-7.00679681341432,-0.249849911000555,
18.7849785039109));
#156765=CARTESIAN_POINT('Ctrl Pts',(-7.00061626730803,-0.423177292184107,
18.7928290086613));
#156766=CARTESIAN_POINT('Ctrl Pts',(-6.98799705047312,-0.596357054351083,
18.8006795134117));
#156767=CARTESIAN_POINT('Ctrl Pts',(-6.96896602986745,-0.768855667244176,
18.8085300181621));
#156768=CARTESIAN_POINT('Ctrl Pts',(-6.9499380707532,-0.941326530547105,
18.8163792600137));
#156769=CARTESIAN_POINT('Ctrl Pts',(-6.92450040602444,-1.11311608381016,
18.8242285018654));
#156770=CARTESIAN_POINT('Ctrl Pts',(-6.89273177670675,-1.28369592072148,
18.832077743717));
#156771=CARTESIAN_POINT('Ctrl Pts',(-6.86095244391603,-1.45433322931873,
18.8399296301318));
#156772=CARTESIAN_POINT('Ctrl Pts',(-6.82283795586274,-1.62375963204604,
18.8477815165467));
#156773=CARTESIAN_POINT('Ctrl Pts',(-6.77851822867546,-1.79145672178104,
18.8556334029615));
#156774=CARTESIAN_POINT('Ctrl Pts',(-6.74597480463827,-1.91459460749023,
18.8613989454255));
#156775=CARTESIAN_POINT('Ctrl Pts',(-6.71008672265903,-2.03680028130827,
18.8671644878895));
#156776=CARTESIAN_POINT('Ctrl Pts',(-6.67092249617087,-2.15787386391823,
18.8729300303535));
#156777=CARTESIAN_POINT('Ctrl Pts',(-6.60533586158689,-2.36063055114182,
18.8825853347134));
#156778=CARTESIAN_POINT('Ctrl Pts',(-6.53059419910574,-2.56010866816895,
18.8922406390733));
#156779=CARTESIAN_POINT('Ctrl Pts',(-6.44704521748711,-2.75558242957394,
18.9018959434332));
#156780=CARTESIAN_POINT('Ctrl Pts',(-6.36303339018411,-2.9521390789462,
18.9116047363679));
#156781=CARTESIAN_POINT('Ctrl Pts',(-6.27011646051596,-3.14464686117081,
18.9213135293026));
#156782=CARTESIAN_POINT('Ctrl Pts',(-6.16869094440121,-3.33239832477489,
18.9310223222373));
#156783=CARTESIAN_POINT('Ctrl Pts',(-6.06677736009053,-3.52105326436446,
18.9407778347081));
#156784=CARTESIAN_POINT('Ctrl Pts',(-5.9562731459008,-3.70490597291602,
18.9505333471788));
#156785=CARTESIAN_POINT('Ctrl Pts',(-5.83762301889833,-3.88326976293539,
18.9602888596495));
#156786=CARTESIAN_POINT('Ctrl Pts',(-5.71885541001622,-4.06181016054755,
18.9700540315785));
#156787=CARTESIAN_POINT('Ctrl Pts',(-5.59192578560676,-4.23485074290651,
18.9798192035074));
#156788=CARTESIAN_POINT('Ctrl Pts',(-5.45732198896148,-4.40173412092297,
18.9895843754363));
#156789=CARTESIAN_POINT('Ctrl Pts',(-5.32290172153903,-4.56838995723977,
18.9993362327749));
#156790=CARTESIAN_POINT('Ctrl Pts',(-5.18082821863161,-4.72890533870851,
19.0090880901134));
#156791=CARTESIAN_POINT('Ctrl Pts',(-5.03162852566511,-4.88265716001167,
19.018839947452));
#156792=CARTESIAN_POINT('Ctrl Pts',(-4.96656665397724,-4.94970408933509,
19.0230924635146));
#156793=CARTESIAN_POINT('Ctrl Pts',(-4.90015019910339,-5.01546527431112,
19.0273449795773));
#156794=CARTESIAN_POINT('Ctrl Pts',(-4.83242531288399,-5.07989095925277,
19.0315974956399));
#156795=CARTESIAN_POINT('Ctrl Pts',(-4.7044923218822,-5.20159172586942,
19.0396305412387));
#156796=CARTESIAN_POINT('Ctrl Pts',(-4.57182535042705,-5.31858360796435,
19.0476635868376));
#156797=CARTESIAN_POINT('Ctrl Pts',(-4.43481306853779,-5.43047508139265,
19.0556966324364));
#156798=CARTESIAN_POINT('Ctrl Pts',(-4.2978888634189,-5.54229462667351,
19.0637245140842));
#156799=CARTESIAN_POINT('Ctrl Pts',(-4.15662519080014,-5.64902005879922,
19.071752395732));
#156800=CARTESIAN_POINT('Ctrl Pts',(-4.01144643542351,-5.7502977364853,
19.0797802773798));
#156801=CARTESIAN_POINT('Ctrl Pts',(-3.86633322968604,-5.85152968630157,
19.0878045343599));
#156802=CARTESIAN_POINT('Ctrl Pts',(-3.71730876090025,-5.9473185699575,
19.09582879134));
#156803=CARTESIAN_POINT('Ctrl Pts',(-3.56482920864944,-6.03735200859283,
19.1038530483201));
#156804=CARTESIAN_POINT('Ctrl Pts',(-3.41236809272944,-6.12737456126846,
19.1118763350858));
#156805=CARTESIAN_POINT('Ctrl Pts',(-3.25645303698763,-6.21164286211121,
19.1198996218516));
#156806=CARTESIAN_POINT('Ctrl Pts',(-3.09756797472278,-6.28988864801849,
19.1279229086173));
#156807=CARTESIAN_POINT('Ctrl Pts',(-2.9386959316716,-6.36812802238152,
19.1359455379462));
#156808=CARTESIAN_POINT('Ctrl Pts',(-2.7768546975555,-6.44034570641755,
19.1439681672751));
#156809=CARTESIAN_POINT('Ctrl Pts',(-2.612551222509,-6.50632020978577,19.1519907966041));
#156810=CARTESIAN_POINT('Ctrl Pts',(-2.44818598105295,-6.57231951487041,
19.1600164418705));
#156811=CARTESIAN_POINT('Ctrl Pts',(-2.28135699108969,-6.63207081688275,
19.1680420871369));
#156812=CARTESIAN_POINT('Ctrl Pts',(-2.11258987980619,-6.68540130151066,
19.1760677324033));
#156813=CARTESIAN_POINT('Ctrl Pts',(-2.0130745068347,-6.71684820504616,
19.180800141911));
#156814=CARTESIAN_POINT('Ctrl Pts',(-1.91288556626571,-6.74606352631963,
19.1855325514187));
#156815=CARTESIAN_POINT('Ctrl Pts',(-1.81213302469172,-6.77302004007973,
19.1902649609264));
#156816=CARTESIAN_POINT('Ctrl Pts',(-1.62627112776042,-6.82274770653694,
19.198995009761));
#156817=CARTESIAN_POINT('Ctrl Pts',(-1.4383977557771,-6.86481090540057,
19.2077250585957));
#156818=CARTESIAN_POINT('Ctrl Pts',(-1.24914618179546,-6.89907677729461,
19.2164551074303));
#156819=CARTESIAN_POINT('Ctrl Pts',(-1.05983988548541,-6.93335255720821,
19.2251876805695));
#156820=CARTESIAN_POINT('Ctrl Pts',(-0.869154861291281,-6.95982646102874,
19.2339202537086));
#156821=CARTESIAN_POINT('Ctrl Pts',(-0.677732899052425,-6.97841706119963,
19.2426528268477));
#156822=CARTESIAN_POINT('Ctrl Pts',(-0.483591482272319,-6.99727177052219,
19.2515094601281));
#156823=CARTESIAN_POINT('Ctrl Pts',(-0.288692317585981,-7.00801745122277,
19.2603660934086));
#156824=CARTESIAN_POINT('Ctrl Pts',(-0.0937089961231848,-7.01062373733933,
19.269222726689));
#156825=CARTESIAN_POINT('Ctrl Pts',(0.0986654612588957,-7.01319515151821,
19.2779608587957));
#156826=CARTESIAN_POINT('Ctrl Pts',(0.29112155933783,-7.00784364703544,
19.2866989909025));
#156827=CARTESIAN_POINT('Ctrl Pts',(0.483012649013248,-6.99459257879923,
19.2954371230092));
#156828=CARTESIAN_POINT('Ctrl Pts',(0.678807202106398,-6.981071956306,19.3043530068765));
#156829=CARTESIAN_POINT('Ctrl Pts',(0.874013217916381,-6.95932695708988,
19.3132688907437));
#156830=CARTESIAN_POINT('Ctrl Pts',(1.06794850413261,-6.92943811250385,
19.322184774611));
#156831=CARTESIAN_POINT('Ctrl Pts',(1.26188379034882,-6.89954926791782,
19.3311006584782));
#156832=CARTESIAN_POINT('Ctrl Pts',(1.45454804901438,-6.86151663003711,
19.3400165423455));
#156833=CARTESIAN_POINT('Ctrl Pts',(1.64526833286464,-6.81547640854055,
19.3489324262128));
#156834=CARTESIAN_POINT('Ctrl Pts',(1.83224091494251,-6.7703408890307,19.357673110709));
#156835=CARTESIAN_POINT('Ctrl Pts',(2.01736507059274,-6.71750477296969,
19.3664137952052));
#156836=CARTESIAN_POINT('Ctrl Pts',(2.20001788584635,-6.65714262010783,
19.3751544797015));
#156837=CARTESIAN_POINT('Ctrl Pts',(2.38263783882449,-6.59679132739994,
19.3838935916034));
#156838=CARTESIAN_POINT('Ctrl Pts',(2.56278707950309,-6.52891678793202,
19.3926327035053));
#156839=CARTESIAN_POINT('Ctrl Pts',(2.73985880538999,-6.4537431223304,19.4013718154072));
#156840=CARTESIAN_POINT('Ctrl Pts',(2.91922475033559,-6.37759547369749,
19.4102241550815));
#156841=CARTESIAN_POINT('Ctrl Pts',(3.09543260616893,-6.29395832974499,
19.4190764947559));
#156842=CARTESIAN_POINT('Ctrl Pts',(3.26787224701603,-6.20311514802703,
19.4279288344302));
#156843=CARTESIAN_POINT('Ctrl Pts',(3.43801900736069,-6.11347988207089,
19.43666346708));
#156844=CARTESIAN_POINT('Ctrl Pts',(3.60449689805667,-6.01682916475391,
19.4453980997297));
#156845=CARTESIAN_POINT('Ctrl Pts',(3.76674336336508,-5.91348213805074,
19.4541327323795));
#156846=CARTESIAN_POINT('Ctrl Pts',(3.93226945406403,-5.80804607025709,
19.4630439255661));
#156847=CARTESIAN_POINT('Ctrl Pts',(4.09339097410259,-5.69564023118293,
19.4719551187527));
#156848=CARTESIAN_POINT('Ctrl Pts',(4.24953957758213,-5.57665131965978,
19.4808663119394));
#156849=CARTESIAN_POINT('Ctrl Pts',(4.40568818106166,-5.45766240813662,
19.489777505126));
#156850=CARTESIAN_POINT('Ctrl Pts',(4.5568636187103,-5.3320905971753,19.4986886983126));
#156851=CARTESIAN_POINT('Ctrl Pts',(4.70253066184799,-5.20036844241632,
19.5075998914992));
#156852=CARTESIAN_POINT('Ctrl Pts',(4.83372239383925,-5.08173585914821,
19.5156255563516));
#156853=CARTESIAN_POINT('Ctrl Pts',(4.96050604576484,-4.95805964397839,
19.523651221204));
#156854=CARTESIAN_POINT('Ctrl Pts',(5.08247188667733,-4.8297107660433,19.5316768860564));
#156855=CARTESIAN_POINT('Ctrl Pts',(5.20439901862358,-4.70140262289384,
19.5397000037596));
#156856=CARTESIAN_POINT('Ctrl Pts',(5.32151113154929,-4.56842503488184,
19.5477231214628));
#156857=CARTESIAN_POINT('Ctrl Pts',(5.43343499138747,-4.43118615687338,
19.555746239166));
#156858=CARTESIAN_POINT('Ctrl Pts',(5.54534473664729,-4.29396458588865,
19.5637683450839));
#156859=CARTESIAN_POINT('Ctrl Pts',(5.65206730092608,-4.15248307968907,
19.5717904510017));
#156860=CARTESIAN_POINT('Ctrl Pts',(5.75326946417137,-4.00718317963296,
19.5798125569196));
#156861=CARTESIAN_POINT('Ctrl Pts',(5.85450923448243,-3.8618292856431,19.5878376438791));
#156862=CARTESIAN_POINT('Ctrl Pts',(5.95022429354549,-3.7126544625929,19.5958627308386));
#156863=CARTESIAN_POINT('Ctrl Pts',(6.04012428632136,-3.56012993699541,
19.6038878177981));
#156864=CARTESIAN_POINT('Ctrl Pts',(6.13004198445088,-3.40757537245594,
19.6119144852583));
#156865=CARTESIAN_POINT('Ctrl Pts',(6.21414215622814,-3.25167011138713,
19.6199411527186));
#156866=CARTESIAN_POINT('Ctrl Pts',(6.29218034226967,-3.09291013494656,
19.6279678201788));
#156867=CARTESIAN_POINT('Ctrl Pts',(6.37028117709203,-2.93402270655622,
19.6360009314194));
#156868=CARTESIAN_POINT('Ctrl Pts',(6.44231015314334,-2.7722763185954,19.64403404266));
#156869=CARTESIAN_POINT('Ctrl Pts',(6.50807065985338,-2.60818765598941,
19.6520671539006));
#156870=CARTESIAN_POINT('Ctrl Pts',(6.54681913928817,-2.51150065513488,
19.6568005548623));
#156871=CARTESIAN_POINT('Ctrl Pts',(6.58339213644724,-2.41400076142861,
19.6615339558239));
#156872=CARTESIAN_POINT('Ctrl Pts',(6.61775754767034,-2.31579610560866,
19.6662673567856));
#156873=CARTESIAN_POINT('Ctrl Pts',(6.69106165164929,-2.10631791095802,
19.6763640704265));
#156874=CARTESIAN_POINT('Ctrl Pts',(6.75435454450432,-1.89353185208178,
19.6864607840674));
#156875=CARTESIAN_POINT('Ctrl Pts',(6.80741833042345,-1.67829742212602,
19.6965574977082));
#156876=CARTESIAN_POINT('Ctrl Pts',(6.86056137941349,-1.46274148963157,
19.7066692931326));
#156877=CARTESIAN_POINT('Ctrl Pts',(6.90344478032577,-1.24472979701641,
19.7167810885569));
#156878=CARTESIAN_POINT('Ctrl Pts',(6.93590123433321,-1.02513444487785,
19.7268928839812));
#156879=CARTESIAN_POINT('Ctrl Pts',(6.96825526148265,-0.806232097031962,
19.7369727683584));
#156880=CARTESIAN_POINT('Ctrl Pts',(6.99024806641376,-0.585755995177965,
19.7470526527356));
#156881=CARTESIAN_POINT('Ctrl Pts',(7.00176464560906,-0.364579771790776,
19.7571325371128));
#156882=CARTESIAN_POINT('Ctrl Pts',(7.0080111741597,-0.244615017441415,
19.7625998103787));
#156883=CARTESIAN_POINT('Ctrl Pts',(7.01117655918058,-0.124444468868163,
19.7680670836446));
#156884=CARTESIAN_POINT('Ctrl Pts',(7.01124873670978,-0.00420885798051574,
19.7735343569105));
#156885=CARTESIAN_POINT('Ctrl Pts',(7.01125,3.89288422118862E-12,19.7735343569105));
#156886=CARTESIAN_POINT('Ctrl Pts',(7.0112499999999,0.191008754744022,19.7822061308426));
#156887=CARTESIAN_POINT('Ctrl Pts',(7.00344012880997,0.382017367486818,
19.7908779047747));
#156888=CARTESIAN_POINT('Ctrl Pts',(6.98784644419149,0.57238853491349,19.7995496787068));
#156889=CARTESIAN_POINT('Ctrl Pts',(6.97225169663166,0.762772678964259,
19.8082220437492));
#156890=CARTESIAN_POINT('Ctrl Pts',(6.94887209704278,0.952519007630679,
19.8168944087915));
#156891=CARTESIAN_POINT('Ctrl Pts',(6.91778566246045,1.14099434299941,19.8255667738339));
#156892=CARTESIAN_POINT('Ctrl Pts',(6.8867010829714,1.3294584310401,19.83423862135));
#156893=CARTESIAN_POINT('Ctrl Pts',(6.84791063501108,1.51665139731095,19.8429104688661));
#156894=CARTESIAN_POINT('Ctrl Pts',(6.80154374572935,1.70194865887019,19.8515823163822));
#156895=CARTESIAN_POINT('Ctrl Pts',(6.75517597619855,1.88724943819274,19.8602543285284));
#156896=CARTESIAN_POINT('Ctrl Pts',(6.70123154646081,2.07065416525486,19.8689263406746));
#156897=CARTESIAN_POINT('Ctrl Pts',(6.63989045285517,2.2515508736386,19.8775983528208));
#156898=CARTESIAN_POINT('Ctrl Pts',(6.61790934153631,2.31637382429812,19.8807059019879));
#156899=CARTESIAN_POINT('Ctrl Pts',(6.59497889661509,2.38087486019083,19.8838134511551));
#156900=CARTESIAN_POINT('Ctrl Pts',(6.57110895151814,2.44502632087636,19.8869210003222));
#156901=CARTESIAN_POINT('',(7.01124999765299,-0.000181413711516228,19.2264656431264));
#156902=CARTESIAN_POINT('Ctrl Pts',(6.57110895151814,2.44502632087635,19.3399454697435));
#156903=CARTESIAN_POINT('Ctrl Pts',(6.64355296009685,2.25033006374781,19.3304888175255));
#156904=CARTESIAN_POINT('Ctrl Pts',(6.70735026907554,2.05238418768571,19.3210321653074));
#156905=CARTESIAN_POINT('Ctrl Pts',(6.76225087861329,1.85191512148745,19.3115755130893));
#156906=CARTESIAN_POINT('Ctrl Pts',(6.81648747471622,1.65387069418375,19.3022332374541));
#156907=CARTESIAN_POINT('Ctrl Pts',(6.86204130570839,1.4533639108226,19.292890961819));
#156908=CARTESIAN_POINT('Ctrl Pts',(6.89872045868837,1.251112543049,19.2835486861839));
#156909=CARTESIAN_POINT('Ctrl Pts',(6.93607320068683,1.04514695918164,19.2740348456743));
#156910=CARTESIAN_POINT('Ctrl Pts',(6.96422206952078,0.837372218825123,
19.2645210051647));
#156911=CARTESIAN_POINT('Ctrl Pts',(6.98301765280545,0.628562664423706,
19.2550071646552));
#156912=CARTESIAN_POINT('Ctrl Pts',(7.00181323609013,0.419753110022305,
19.2454933241456));
#156913=CARTESIAN_POINT('Ctrl Pts',(7.01125543366831,0.209908893479341,
19.235979483636));
#156914=CARTESIAN_POINT('Ctrl Pts',(7.01124999765299,-0.000181413711498942,
19.2264656431264));
#156915=CARTESIAN_POINT('Ctrl Pts',(7.01124999765297,-0.000181414524300546,
19.2264656430896));
#156916=CARTESIAN_POINT('Ctrl Pts',(7.01124516495315,-0.186954037711722,
19.2180077329065));
#156917=CARTESIAN_POINT('Ctrl Pts',(7.00377284192131,-0.373681608927717,
19.2095498227235));
#156918=CARTESIAN_POINT('Ctrl Pts',(6.98886978812648,-0.559754988466313,
19.2010919125404));
#156919=CARTESIAN_POINT('Ctrl Pts',(6.97396039576302,-0.745907508757027,
19.192630405038));
#156920=CARTESIAN_POINT('Ctrl Pts',(6.95161399222959,-0.931404968934443,
19.1841688975355));
#156921=CARTESIAN_POINT('Ctrl Pts',(6.92191919458265,-1.11564386170868,
19.1757073900331));
#156922=CARTESIAN_POINT('Ctrl Pts',(6.89220882192622,-1.29997938832901,
19.1672414444449));
#156923=CARTESIAN_POINT('Ctrl Pts',(6.85514241522061,-1.48305472035264,
19.1587754988566));
#156924=CARTESIAN_POINT('Ctrl Pts',(6.81085974217086,-1.66427645989969,
19.1503095532684));
#156925=CARTESIAN_POINT('Ctrl Pts',(6.7665494426539,-1.84561125758218,19.141838326062));
#156926=CARTESIAN_POINT('Ctrl Pts',(6.71501396877955,-2.02508985057409,
19.1333670988557));
#156927=CARTESIAN_POINT('Ctrl Pts',(6.65644314083335,-2.20213334640586,
19.1248958716493));
#156928=CARTESIAN_POINT('Ctrl Pts',(6.59780049088891,-2.37939394037492,
19.11641425667));
#156929=CARTESIAN_POINT('Ctrl Pts',(6.53210534447744,-2.55421317109245,
19.1079326416906));
#156930=CARTESIAN_POINT('Ctrl Pts',(6.45959646528243,-2.72603009304937,
19.0994510267112));
#156931=CARTESIAN_POINT('Ctrl Pts',(6.38703844263391,-2.89796346525362,
19.0909636632517));
#156932=CARTESIAN_POINT('Ctrl Pts',(6.30765760169667,-3.06689018248215,
19.0824762997922));
#156933=CARTESIAN_POINT('Ctrl Pts',(6.22173939182166,-3.23227249822082,
19.0739889363327));
#156934=CARTESIAN_POINT('Ctrl Pts',(6.13571527480889,-3.39785867257946,
19.0654911109191));
#156935=CARTESIAN_POINT('Ctrl Pts',(6.04313783782619,-3.55989144004833,
19.0569932855055));
#156936=CARTESIAN_POINT('Ctrl Pts',(5.94433741785836,-3.71785949507899,
19.0484954600919));
#156937=CARTESIAN_POINT('Ctrl Pts',(5.91178451919106,-3.76990702776921,
19.0456955848517));
#156938=CARTESIAN_POINT('Ctrl Pts',(5.87855640756592,-3.82151354934236,
19.0428957096116));
#156939=CARTESIAN_POINT('Ctrl Pts',(5.84466588621277,-3.87266151903838,
19.0400958343715));
#156940=CARTESIAN_POINT('Ctrl Pts',(5.74321613721404,-4.02577066225237,
19.0317145339666));
#156941=CARTESIAN_POINT('Ctrl Pts',(5.63562818842459,-4.17506946424774,
19.0233332335617));
#156942=CARTESIAN_POINT('Ctrl Pts',(5.52220866352554,-4.32005069865893,
19.0149519331568));
#156943=CARTESIAN_POINT('Ctrl Pts',(5.40893288127082,-4.46484819057929,
19.0065812548233));
#156944=CARTESIAN_POINT('Ctrl Pts',(5.28984045199139,-4.60533876384062,
18.9982105764897));
#156945=CARTESIAN_POINT('Ctrl Pts',(5.16528175072161,-4.74104323943183,
18.9898398981561));
#156946=CARTESIAN_POINT('Ctrl Pts',(5.04086440219207,-4.8765937137426,18.9814787191053));
#156947=CARTESIAN_POINT('Ctrl Pts',(4.91099336570416,-5.00736867584189,
18.9731175400545));
#156948=CARTESIAN_POINT('Ctrl Pts',(4.77606010814833,-5.13292084546939,
18.9647563610037));
#156949=CARTESIAN_POINT('Ctrl Pts',(4.64130194241101,-5.25831009634657,
18.9564060315689));
#156950=CARTESIAN_POINT('Ctrl Pts',(4.50149489657163,-5.37848985043261,
18.9480557021342));
#156951=CARTESIAN_POINT('Ctrl Pts',(4.35706814120457,-5.49304867768347,
18.9397053726995));
#156952=CARTESIAN_POINT('Ctrl Pts',(4.21275251358652,-5.60751935876939,
18.9313614683438));
#156953=CARTESIAN_POINT('Ctrl Pts',(4.06382451570365,-5.7163775291412,18.9230175639881));
#156954=CARTESIAN_POINT('Ctrl Pts',(3.91074819082601,-5.81925039420466,
18.9146736596324));
#156955=CARTESIAN_POINT('Ctrl Pts',(3.75779481780703,-5.92204063114144,
18.9063364571527));
#156956=CARTESIAN_POINT('Ctrl Pts',(3.60070003407538,-6.01885496828442,
18.8979992546729));
#156957=CARTESIAN_POINT('Ctrl Pts',(3.43995892618802,-6.10936241752275,
18.8896620521932));
#156958=CARTESIAN_POINT('Ctrl Pts',(3.38704384074103,-6.13915697022293,
18.8869174911572));
#156959=CARTESIAN_POINT('Ctrl Pts',(3.33373384921236,-6.16826839441706,
18.8841729301211));
#156960=CARTESIAN_POINT('Ctrl Pts',(3.28004730242159,-6.1966859091273,18.881428369085));
#156961=CARTESIAN_POINT('Ctrl Pts',(3.11694104233256,-6.28302177579195,
18.8730900587831));
#156962=CARTESIAN_POINT('Ctrl Pts',(2.95049105754875,-6.36287851805344,
18.8647517484812));
#156963=CARTESIAN_POINT('Ctrl Pts',(2.78124344501673,-6.43601673879516,
18.8564134381793));
#156964=CARTESIAN_POINT('Ctrl Pts',(2.61188934762992,-6.5092009756236,18.8480698816955));
#156965=CARTESIAN_POINT('Ctrl Pts',(2.4397344123806,-6.57565812955061,18.8397263252117));
#156966=CARTESIAN_POINT('Ctrl Pts',(2.26534310331881,-6.63519759967598,
18.8313827687279));
#156967=CARTESIAN_POINT('Ctrl Pts',(2.0908191181094,-6.69478236717065,18.8230328645027));
#156968=CARTESIAN_POINT('Ctrl Pts',(1.91405567502942,-6.7474388472641,18.8146829602774));
#156969=CARTESIAN_POINT('Ctrl Pts',(1.73563114144997,-6.79302665262908,
18.8063330560522));
#156970=CARTESIAN_POINT('Ctrl Pts',(1.55693898427338,-6.83868283632866,
18.7979706275886));
#156971=CARTESIAN_POINT('Ctrl Pts',(1.37658107549933,-6.87724907701198,
18.7896081991249));
#156972=CARTESIAN_POINT('Ctrl Pts',(1.1951461844033,-6.90863605644459,18.7812457706613));
#156973=CARTESIAN_POINT('Ctrl Pts',(1.01355614174206,-6.94004987602331,
18.7728761911813));
#156974=CARTESIAN_POINT('Ctrl Pts',(0.830887603227299,-6.96427214199749,
18.7645066117013));
#156975=CARTESIAN_POINT('Ctrl Pts',(0.647733730032479,-6.98126547106456,
18.7561370322213));
#156976=CARTESIAN_POINT('Ctrl Pts',(0.464297364303625,-6.99828501027126,
18.7477545436848));
#156977=CARTESIAN_POINT('Ctrl Pts',(0.280374494584013,-7.00805331469282,
18.7393720551482));
#156978=CARTESIAN_POINT('Ctrl Pts',(0.0965589714634512,-7.01058506314059,
18.7309895666116));
#156979=CARTESIAN_POINT('Ctrl Pts',(0.0364115203036668,-7.01141349271784,
18.7282466790073));
#156980=CARTESIAN_POINT('Ctrl Pts',(-0.0237244746506637,-7.01146751427345,
18.725503791403));
#156981=CARTESIAN_POINT('Ctrl Pts',(-0.0838283466072417,-7.01074884522368,
18.7227609037986));
#156982=CARTESIAN_POINT('Ctrl Pts',(-0.267672109595982,-7.00855060377677,
18.7143710486658));
#156983=CARTESIAN_POINT('Ctrl Pts',(-0.451586127756862,-6.99911472365721,
18.7059811935331));
#156984=CARTESIAN_POINT('Ctrl Pts',(-0.634977094670883,-6.98243730023717,
18.6975913384003));
#156985=CARTESIAN_POINT('Ctrl Pts',(-0.818198830971593,-6.96577526650966,
18.6892092253082));
#156986=CARTESIAN_POINT('Ctrl Pts',(-1.00089815242133,-6.94188504045475,
18.6808271122161));
#156987=CARTESIAN_POINT('Ctrl Pts',(-1.1824831180529,-6.91081473040769,
18.672444999124));
#156988=CARTESIAN_POINT('Ctrl Pts',(-1.36392721223693,-6.87976852433607,
18.6640693887751));
#156989=CARTESIAN_POINT('Ctrl Pts',(-1.54425835130521,-6.84155339484332,
18.6556937784263));
#156990=CARTESIAN_POINT('Ctrl Pts',(-1.72289061495748,-6.79626915972223,
18.6473181680774));
#156991=CARTESIAN_POINT('Ctrl Pts',(-1.90141051626331,-6.75101340905747,
18.6389478261118));
#156992=CARTESIAN_POINT('Ctrl Pts',(-2.07823335505521,-6.69869749940158,
18.6305774841462));
#156993=CARTESIAN_POINT('Ctrl Pts',(-2.25278384019998,-6.6394722329289,
18.6222071421806));
#156994=CARTESIAN_POINT('Ctrl Pts',(-2.42725011763826,-6.58027553826942,
18.6138408382863));
#156995=CARTESIAN_POINT('Ctrl Pts',(-2.59944591677695,-6.51417623927522,
18.605474534392));
#156996=CARTESIAN_POINT('Ctrl Pts',(-2.76881109924021,-6.44137498203794,
18.5971082304977));
#156997=CARTESIAN_POINT('Ctrl Pts',(-2.93812891500913,-6.36859408527174,
18.5887442664241));
#156998=CARTESIAN_POINT('Ctrl Pts',(-3.10461739038423,-6.28911509603682,
18.5803803023504));
#156999=CARTESIAN_POINT('Ctrl Pts',(-3.26773585023415,-6.20318700150129,
18.5720163382768));
#157000=CARTESIAN_POINT('Ctrl Pts',(-3.43082920886382,-6.11727212987154,
18.5636536612783));
#157001=CARTESIAN_POINT('Ctrl Pts',(-3.59055329523702,-6.0249102847418,
18.5552909842797));
#157002=CARTESIAN_POINT('Ctrl Pts',(-3.74639118127719,-5.92639685469582,
18.5469283072812));
#157003=CARTESIAN_POINT('Ctrl Pts',(-3.90222585890007,-5.82788545286134,
18.5385658024549));
#157004=CARTESIAN_POINT('Ctrl Pts',(-4.05417421814763,-5.72322289460059,
18.5302032976286));
#157005=CARTESIAN_POINT('Ctrl Pts',(-4.20174715382626,-5.61274865086732,
18.5218407928023));
#157006=CARTESIAN_POINT('Ctrl Pts',(-4.3493367216698,-5.50226195616646,
18.5134773454823));
#157007=CARTESIAN_POINT('Ctrl Pts',(-4.49254962002037,-5.38596246747935,
18.5051138981623));
#157008=CARTESIAN_POINT('Ctrl Pts',(-4.63092841241402,-5.26423105511114,
18.4967504508423));
#157009=CARTESIAN_POINT('Ctrl Pts',(-4.76938868612947,-5.14242796386633,
18.4883820788895));
#157010=CARTESIAN_POINT('Ctrl Pts',(-4.90300891833123,-5.01518677422067,
18.4800137069367));
#157011=CARTESIAN_POINT('Ctrl Pts',(-5.03136649664836,-4.88292716911736,
18.4716453349839));
#157012=CARTESIAN_POINT('Ctrl Pts',(-5.15976253425072,-4.7506279355796,
18.4632744556482));
#157013=CARTESIAN_POINT('Ctrl Pts',(-5.28289254867203,-4.61330752792642,
18.4549035763124));
#157014=CARTESIAN_POINT('Ctrl Pts',(-5.40037261365331,-4.47142060157656,
18.4465326969767));
#157015=CARTESIAN_POINT('Ctrl Pts',(-5.51795221822319,-4.32941345596842,
18.4381547250854));
#157016=CARTESIAN_POINT('Ctrl Pts',(-5.62987210217045,-4.18283231716381,
18.4297767531941));
#157017=CARTESIAN_POINT('Ctrl Pts',(-5.73578955921081,-4.03216377332919,
18.4213987813028));
#157018=CARTESIAN_POINT('Ctrl Pts',(-5.80310096564922,-3.93641268682348,
18.4160745119438));
#157019=CARTESIAN_POINT('Ctrl Pts',(-5.86798902647418,-3.83901142385793,
18.4107502425848));
#157020=CARTESIAN_POINT('Ctrl Pts',(-5.93037513265293,-3.74009055351763,
18.4054259732257));
#157021=CARTESIAN_POINT('Ctrl Pts',(-6.02250635073436,-3.59400513744734,
18.3975631420365));
#157022=CARTESIAN_POINT('Ctrl Pts',(-6.10937021996468,-3.44430041469862,
18.3897003108472));
#157023=CARTESIAN_POINT('Ctrl Pts',(-6.19065813649991,-3.29140978905506,
18.3818374796579));
#157024=CARTESIAN_POINT('Ctrl Pts',(-6.27188359400116,-3.138636639676,18.3739806900165));
#157025=CARTESIAN_POINT('Ctrl Pts',(-6.34754144109055,-2.98268278996627,
18.3661239003752));
#157026=CARTESIAN_POINT('Ctrl Pts',(-6.41736637059914,-2.82401052193565,
18.3582671107338));
#157027=CARTESIAN_POINT('Ctrl Pts',(-6.48715192215287,-2.66542773755293,
18.3504147519498));
#157028=CARTESIAN_POINT('Ctrl Pts',(-6.55111094658311,-2.50412993234406,
18.3425623931659));
#157029=CARTESIAN_POINT('Ctrl Pts',(-6.60902421618967,-2.34060365553814,
18.3347100343819));
#157030=CARTESIAN_POINT('Ctrl Pts',(-6.66692381179754,-2.17711598919423,
18.3268595296315));
#157031=CARTESIAN_POINT('Ctrl Pts',(-6.71878035852998,-2.01140125472944,
18.3190090248811));
#157032=CARTESIAN_POINT('Ctrl Pts',(-6.76442292621642,-1.84396557391339,
18.3111585201307));
#157033=CARTESIAN_POINT('Ctrl Pts',(-6.81005815145225,-1.67655682822124,
18.303309278279));
#157034=CARTESIAN_POINT('Ctrl Pts',(-6.84948129017765,-1.50742805618571,
18.2954600364274));
#157035=CARTESIAN_POINT('Ctrl Pts',(-6.88257154376019,-1.33709966252425,
18.2876107945758));
#157036=CARTESIAN_POINT('Ctrl Pts',(-6.91567294609685,-1.16671388189308,
18.2797589081609));
#157037=CARTESIAN_POINT('Ctrl Pts',(-6.94243712858477,-0.995128047173407,
18.2719070217461));
#157038=CARTESIAN_POINT('Ctrl Pts',(-6.9627945642581,-0.822872054719267,
18.2640551353312));
#157039=CARTESIAN_POINT('Ctrl Pts',(-6.97774277588914,-0.696386623487206,
18.2582895928673));
#157040=CARTESIAN_POINT('Ctrl Pts',(-6.9892376781199,-0.569540069083445,
18.2525240504033));
#157041=CARTESIAN_POINT('Ctrl Pts',(-6.99726959917371,-0.442543465638532,
18.2467585079393));
#157042=CARTESIAN_POINT('Ctrl Pts',(-7.01072030964093,-0.229867751844482,
18.2371032035794));
#157043=CARTESIAN_POINT('Ctrl Pts',(-7.01445165797877,-0.0168796950838728,
18.2274478992195));
#157044=CARTESIAN_POINT('Ctrl Pts',(-7.00852054170013,0.195617941578176,
18.2177925948596));
#157045=CARTESIAN_POINT('Ctrl Pts',(-7.00255656814998,0.409292775283142,
18.2080838019249));
#157046=CARTESIAN_POINT('Ctrl Pts',(-6.98682283297686,0.622471694535516,
18.1983750089902));
#157047=CARTESIAN_POINT('Ctrl Pts',(-6.9614283634964,0.834351066642706,
18.1886662160554));
#157048=CARTESIAN_POINT('Ctrl Pts',(-6.93591169367252,1.04725002027947,
18.1789107035847));
#157049=CARTESIAN_POINT('Ctrl Pts',(-6.90064111826093,1.25883684951397,
18.169155191114));
#157050=CARTESIAN_POINT('Ctrl Pts',(-6.85577812304805,1.46830953481742,
18.1593996786433));
#157051=CARTESIAN_POINT('Ctrl Pts',(-6.81087070656787,1.67798963030607,
18.1496345067144));
#157052=CARTESIAN_POINT('Ctrl Pts',(-6.7563518911328,1.88555135958048,18.1398693347854));
#157053=CARTESIAN_POINT('Ctrl Pts',(-6.69243403459657,2.09020411804049,
18.1301041628565));
#157054=CARTESIAN_POINT('Ctrl Pts',(-6.62860332860761,2.29457783710738,
18.1203523055179));
#157055=CARTESIAN_POINT('Ctrl Pts',(-6.55539920620729,2.49605047639107,
18.1106004481794));
#157056=CARTESIAN_POINT('Ctrl Pts',(-6.47308307807708,2.69384892427399,
18.1008485908409));
#157057=CARTESIAN_POINT('Ctrl Pts',(-6.43718728459529,2.78010337279462,
18.0965960747782));
#157058=CARTESIAN_POINT('Ctrl Pts',(-6.39955940009407,2.865659326623,18.0923435587156));
#157059=CARTESIAN_POINT('Ctrl Pts',(-6.36022408105815,2.95045355856146,
18.0880910426529));
#157060=CARTESIAN_POINT('Ctrl Pts',(-6.28591926790637,3.11063071524814,
18.0800579970541));
#157061=CARTESIAN_POINT('Ctrl Pts',(-6.20548203678741,3.26816635452103,
18.0720249514553));
#157062=CARTESIAN_POINT('Ctrl Pts',(-6.11913013039002,3.42255358027497,
18.0639919058564));
#157063=CARTESIAN_POINT('Ctrl Pts',(-6.03283373432293,3.57684155997572,
18.0559640242086));
#157064=CARTESIAN_POINT('Ctrl Pts',(-5.94063040950607,3.72798483623015,
18.0479361425608));
#157065=CARTESIAN_POINT('Ctrl Pts',(-5.84278502932592,3.87549863418695,
18.039908260913));
#157066=CARTESIAN_POINT('Ctrl Pts',(-5.74498382729946,4.02294582820981,
18.0318840039329));
#157067=CARTESIAN_POINT('Ctrl Pts',(-5.64154584436463,4.1667665020204,18.0238597469528));
#157068=CARTESIAN_POINT('Ctrl Pts',(-5.53278067960693,4.30650258491369,
18.0158354899726));
#157069=CARTESIAN_POINT('Ctrl Pts',(-5.42402866566543,4.44622177229134,
18.0078122032069));
#157070=CARTESIAN_POINT('Ctrl Pts',(-5.30995097180102,4.58185705861636,
17.9997889164412));
#157071=CARTESIAN_POINT('Ctrl Pts',(-5.19089921178639,4.71298121527929,
17.9917656296755));
#157072=CARTESIAN_POINT('Ctrl Pts',(-5.07185720700146,4.84409462748731,
17.9837430003466));
#157073=CARTESIAN_POINT('Ctrl Pts',(-4.94784219736173,4.97069737758333,
17.9757203710176));
#157074=CARTESIAN_POINT('Ctrl Pts',(-4.81924438107422,5.09239728988073,
17.9676977416887));
#157075=CARTESIAN_POINT('Ctrl Pts',(-4.69059822116308,5.21414295268094,
17.9596720964223));
#157076=CARTESIAN_POINT('Ctrl Pts',(-4.55736608149501,5.33098184579355,
17.9516464511559));
#157077=CARTESIAN_POINT('Ctrl Pts',(-4.41997340702905,5.44256021038408,
17.9436208058895));
#157078=CARTESIAN_POINT('Ctrl Pts',(-4.33895831386897,5.50835361339547,
17.9388883963818));
#157079=CARTESIAN_POINT('Ctrl Pts',(-4.25649724147723,5.57231868471863,
17.9341559868741));
#157080=CARTESIAN_POINT('Ctrl Pts',(-4.17268247625739,5.63438971982188,
17.9294235773664));
#157081=CARTESIAN_POINT('Ctrl Pts',(-4.01806631460727,5.74889442758001,
17.9206935285318));
#157082=CARTESIAN_POINT('Ctrl Pts',(-3.85876470267615,5.85700877924149,
17.9119634796971));
#157083=CARTESIAN_POINT('Ctrl Pts',(-3.69531788278139,5.95837665037182,
17.9032334308625));
#157084=CARTESIAN_POINT('Ctrl Pts',(-3.53182380203511,6.05977383214832,
17.8945008577234));
#157085=CARTESIAN_POINT('Ctrl Pts',(-3.36418235367525,6.15442049520198,
17.8857682845842));
#157086=CARTESIAN_POINT('Ctrl Pts',(-3.19296058830537,6.24200522620965,
17.8770357114451));
#157087=CARTESIAN_POINT('Ctrl Pts',(-3.01930634443635,6.33083423813319,
17.8681790781647));
#157088=CARTESIAN_POINT('Ctrl Pts',(-2.84196953804467,6.41239900471752,
17.8593224448842));
#157089=CARTESIAN_POINT('Ctrl Pts',(-2.66156554982998,6.48642392898107,
17.8504658116038));
#157090=CARTESIAN_POINT('Ctrl Pts',(-2.48357535517145,6.55945840460238,
17.8417276794971));
#157091=CARTESIAN_POINT('Ctrl Pts',(-2.30259981210677,6.62515346606341,
17.8329895473904));
#157092=CARTESIAN_POINT('Ctrl Pts',(-2.11924896866557,6.6832933776178,17.8242514152836));
#157093=CARTESIAN_POINT('Ctrl Pts',(-1.93216838815715,6.74261597575895,
17.8153355314164));
#157094=CARTESIAN_POINT('Ctrl Pts',(-1.7426151162702,6.79407266352937,17.8064196475491));
#157095=CARTESIAN_POINT('Ctrl Pts',(-1.55125325708798,6.83748783508051,
17.7975037636818));
#157096=CARTESIAN_POINT('Ctrl Pts',(-1.35989139790574,6.88090300663165,
17.7885878798146));
#157097=CARTESIAN_POINT('Ctrl Pts',(-1.16672124769152,6.91627660098644,
17.7796719959473));
#157098=CARTESIAN_POINT('Ctrl Pts',(-0.972418757270613,6.94348819564117,
17.77075611208));
#157099=CARTESIAN_POINT('Ctrl Pts',(-0.781934359886621,6.97016507558458,
17.7620154275838));
#157100=CARTESIAN_POINT('Ctrl Pts',(-0.590341479410634,6.98900058238697,
17.7532747430876));
#157101=CARTESIAN_POINT('Ctrl Pts',(-0.398283611592436,6.99992833729295,
17.7445340585913));
#157102=CARTESIAN_POINT('Ctrl Pts',(-0.206260298174957,7.01085412611431,
17.7357949466894));
#157103=CARTESIAN_POINT('Ctrl Pts',(-0.0137724377431587,7.01387498880377,
17.7270558347875));
#157104=CARTESIAN_POINT('Ctrl Pts',(0.178533260344289,7.00897656134267,
17.7183167228856));
#157105=CARTESIAN_POINT('Ctrl Pts',(0.373330555525936,7.00401466770375,
17.7094643832113));
#157106=CARTESIAN_POINT('Ctrl Pts',(0.567940649612334,6.99092682656728,
17.700612043537));
#157107=CARTESIAN_POINT('Ctrl Pts',(0.761691952660525,6.96975264494747,
17.6917597038626));
#157108=CARTESIAN_POINT('Ctrl Pts',(0.952867000139486,6.94886001035451,
17.6830250712129));
#157109=CARTESIAN_POINT('Ctrl Pts',(1.14320567516849,6.92009478765978,17.6742904385631));
#157110=CARTESIAN_POINT('Ctrl Pts',(1.33206753067108,6.88354724369869,17.6655558059133));
#157111=CARTESIAN_POINT('Ctrl Pts',(1.52474701101648,6.84626093323869,17.6566446127267));
#157112=CARTESIAN_POINT('Ctrl Pts',(1.71588904234259,6.80087436321998,17.6477334195401));
#157113=CARTESIAN_POINT('Ctrl Pts',(1.90482298407108,6.74753851132801,17.6388222263535));
#157114=CARTESIAN_POINT('Ctrl Pts',(2.09375692579957,6.69420265943603,17.6299110331668));
#157115=CARTESIAN_POINT('Ctrl Pts',(2.28048248254154,6.63291759505816,17.6209998399802));
#157116=CARTESIAN_POINT('Ctrl Pts',(2.46434297795406,6.56388911008623,17.6120886467936));
#157117=CARTESIAN_POINT('Ctrl Pts',(2.62993278000099,6.50172016435128,17.6040629819412));
#157118=CARTESIAN_POINT('Ctrl Pts',(2.79327456229531,6.43324124240267,17.5960373170888));
#157119=CARTESIAN_POINT('Ctrl Pts',(2.95385099394759,6.3586469368927,17.5880116522364));
#157120=CARTESIAN_POINT('Ctrl Pts',(3.11437646257926,6.28407630578556,17.5799885345332));
#157121=CARTESIAN_POINT('Ctrl Pts',(3.2721379958415,6.20339430946547,17.57196541683));
#157122=CARTESIAN_POINT('Ctrl Pts',(3.42663855477327,6.11684353056716,17.5639422991268));
#157123=CARTESIAN_POINT('Ctrl Pts',(3.58111962983246,6.03030366647952,17.5559201932089));
#157124=CARTESIAN_POINT('Ctrl Pts',(3.7323402302707,5.93789667363831,17.547898087291));
#157125=CARTESIAN_POINT('Ctrl Pts',(3.87982827560464,5.83991088239527,17.5398759813732));
#157126=CARTESIAN_POINT('Ctrl Pts',(4.02737112799429,5.74188867930132,17.5318508944136));
#157127=CARTESIAN_POINT('Ctrl Pts',(4.1711783471568,5.63828373694692,17.5238258074541));
#157128=CARTESIAN_POINT('Ctrl Pts',(4.31080682208906,5.52942773758103,17.5158007204946));
#157129=CARTESIAN_POINT('Ctrl Pts',(4.45046279615075,5.42055029957078,17.5077740530344));
#157130=CARTESIAN_POINT('Ctrl Pts',(4.58593810279121,5.30641997663847,17.4997473855741));
#157131=CARTESIAN_POINT('Ctrl Pts',(4.71682322995323,5.18740832978026,17.4917207181139));
#157132=CARTESIAN_POINT('Ctrl Pts',(4.84781343123415,5.06830114079129,17.4836876068733));
#157133=CARTESIAN_POINT('Ctrl Pts',(4.97420582830038,4.9443050546706,17.4756544956327));
#157134=CARTESIAN_POINT('Ctrl Pts',(5.09562781228434,4.81582846052207,17.4676213843921));
#157135=CARTESIAN_POINT('Ctrl Pts',(5.1671740561423,4.74012538408243,17.4628879834305));
#157136=CARTESIAN_POINT('Ctrl Pts',(5.23699531121069,4.6628673376765,17.4581545824688));
#157137=CARTESIAN_POINT('Ctrl Pts',(5.30502200952541,4.5841431086901,17.4534211815071));
#157138=CARTESIAN_POINT('Ctrl Pts',(5.44523849086005,4.42187690060242,17.4436647058287));
#157139=CARTESIAN_POINT('Ctrl Pts',(5.57791171544638,4.25328461661226,17.4339082301503));
#157140=CARTESIAN_POINT('Ctrl Pts',(5.70255807462325,4.07902659565357,17.4241517544719));
#157141=CARTESIAN_POINT('Ctrl Pts',(5.82731200848036,3.90461818321126,17.4143868585736));
#157142=CARTESIAN_POINT('Ctrl Pts',(5.94402521095326,3.72453429354533,17.4046219626753));
#157143=CARTESIAN_POINT('Ctrl Pts',(6.05225705726437,3.53946480068578,17.394857066777));
#157144=CARTESIAN_POINT('Ctrl Pts',(6.16027707130092,3.35475752738507,17.3851112828146));
#157145=CARTESIAN_POINT('Ctrl Pts',(6.25984888294183,3.1650841836814,17.3753654988522));
#157146=CARTESIAN_POINT('Ctrl Pts',(6.35057859735081,2.97115769379038,17.3656197148898));
#157147=CARTESIAN_POINT('Ctrl Pts',(6.43114174761781,2.79896130755009,17.3569659782066));
#157148=CARTESIAN_POINT('Ctrl Pts',(6.50473393484496,2.62341191226827,17.3483122415235));
#157149=CARTESIAN_POINT('Ctrl Pts',(6.57110895151813,2.44502632087639,17.3396585048403));
#157150=CARTESIAN_POINT('Origin',(0.,0.,50.));
#157151=CARTESIAN_POINT('',(6.57110895151814,2.44502632087634,15.3398759450547));
#157152=CARTESIAN_POINT('',(6.57110895151814,2.44502632087636,15.8871325193051));
#157153=CARTESIAN_POINT('',(6.57110895151814,2.44502632087636,50.));
#157154=CARTESIAN_POINT('',(7.01124960457286,0.00235475623571332,17.7735343569365));
#157155=CARTESIAN_POINT('Ctrl Pts',(6.57110895151814,2.44502632087636,15.8871325193051));
#157156=CARTESIAN_POINT('Ctrl Pts',(6.5069897366308,2.61734935204908,15.8955017124837));
#157157=CARTESIAN_POINT('Ctrl Pts',(6.43602216531024,2.78732527730889,15.9038709056622));
#157158=CARTESIAN_POINT('Ctrl Pts',(6.35839584537371,2.9543914493571,15.9122400988407));
#157159=CARTESIAN_POINT('Ctrl Pts',(6.27748822327716,3.12851958945502,15.9209630618705));
#157160=CARTESIAN_POINT('Ctrl Pts',(6.18934672976297,3.29948628853455,15.9296860249002));
#157161=CARTESIAN_POINT('Ctrl Pts',(6.09424340208908,3.46667332158566,15.93840898793));
#157162=CARTESIAN_POINT('Ctrl Pts',(6.00321710348158,3.62669313546637,15.9467580021749));
#157163=CARTESIAN_POINT('Ctrl Pts',(5.90581356536447,3.78325023446906,15.9551070164198));
#157164=CARTESIAN_POINT('Ctrl Pts',(5.80231996284411,3.9358238796065,15.9634560306648));
#157165=CARTESIAN_POINT('Ctrl Pts',(5.69890358042771,4.0882836843475,15.9717988154256));
#157166=CARTESIAN_POINT('Ctrl Pts',(5.58940637239973,4.23676568829624,15.9801416001865));
#157167=CARTESIAN_POINT('Ctrl Pts',(5.47416030766408,4.38077567201234,15.9884843849473));
#157168=CARTESIAN_POINT('Ctrl Pts',(5.3590020329863,4.52467595441383,15.9968208144928));
#157169=CARTESIAN_POINT('Ctrl Pts',(5.23810383945535,4.66411075531959,16.0051572440384));
#157170=CARTESIAN_POINT('Ctrl Pts',(5.11183979577424,4.79861651570938,16.0134936735839));
#157171=CARTESIAN_POINT('Ctrl Pts',(5.0945632853444,4.81702072726874,16.0146343341218));
#157172=CARTESIAN_POINT('Ctrl Pts',(5.07718637847166,4.83533270612563,16.0157749946598));
#157173=CARTESIAN_POINT('Ctrl Pts',(5.05971009278249,4.85355131213167,16.0169156551978));
#157174=CARTESIAN_POINT('Ctrl Pts',(4.93195719158946,4.98673062805503,16.0252539654997));
#157175=CARTESIAN_POINT('Ctrl Pts',(4.79899544814352,5.11480822757598,16.0335922758016));
#157176=CARTESIAN_POINT('Ctrl Pts',(4.66126818530316,5.23738536554077,16.0419305861035));
#157177=CARTESIAN_POINT('Ctrl Pts',(4.52345426914264,5.36003962488125,16.0502741425873));
#157178=CARTESIAN_POINT('Ctrl Pts',(4.3808690978533,5.47718630203073,16.0586176990712));
#157179=CARTESIAN_POINT('Ctrl Pts',(4.23398875277113,5.58846721417488,16.066961255555));
#157180=CARTESIAN_POINT('Ctrl Pts',(4.08699666176198,5.69983278835245,16.0753111597802));
#157181=CARTESIAN_POINT('Ctrl Pts',(3.93570313973195,5.80532349835782,16.0836610640055));
#157182=CARTESIAN_POINT('Ctrl Pts',(3.78061323341272,5.90462447085711,16.0920109682307));
#157183=CARTESIAN_POINT('Ctrl Pts',(3.62529070371132,6.00407438746646,16.1003733966944));
#157184=CARTESIAN_POINT('Ctrl Pts',(3.46616068690274,6.09731583709216,16.108735825158));
#157185=CARTESIAN_POINT('Ctrl Pts',(3.30375413934276,6.18407916744891,16.1170982536217));
#157186=CARTESIAN_POINT('Ctrl Pts',(3.14120871204524,6.27091669228075,16.1254678331017));
#157187=CARTESIAN_POINT('Ctrl Pts',(2.97538145768056,6.3512649022293,16.1338374125817));
#157188=CARTESIAN_POINT('Ctrl Pts',(2.8068238079514,6.42490207502163,16.1422069920616));
#157189=CARTESIAN_POINT('Ctrl Pts',(2.63800617858451,6.49865282418107,16.1505894805982));
#157190=CARTESIAN_POINT('Ctrl Pts',(2.46645004301298,6.56567173289311,16.1589719691348));
#157191=CARTESIAN_POINT('Ctrl Pts',(2.29272383294703,6.62578629208162,16.1673544576714));
#157192=CARTESIAN_POINT('Ctrl Pts',(2.23587777034313,6.64545676088272,16.1700973452756));
#157193=CARTESIAN_POINT('Ctrl Pts',(2.17879945109119,6.66438838201481,16.1728402328799));
#157194=CARTESIAN_POINT('Ctrl Pts',(2.12150903618929,6.68257629749689,16.1755831204842));
#157195=CARTESIAN_POINT('Ctrl Pts',(1.94627098386213,6.73820890009591,16.183972975617));
#157196=CARTESIAN_POINT('Ctrl Pts',(1.76869389559647,6.78699188517103,16.1923628307498));
#157197=CARTESIAN_POINT('Ctrl Pts',(1.58933985198005,6.82873527070775,16.2007526858825));
#157198=CARTESIAN_POINT('Ctrl Pts',(1.41015131376065,6.87044013603351,16.2091347989746));
#157199=CARTESIAN_POINT('Ctrl Pts',(1.22918940765239,6.90511827751886,16.2175169120667));
#157200=CARTESIAN_POINT('Ctrl Pts',(1.04703124785331,6.93262952482814,16.2258990251588));
#157201=CARTESIAN_POINT('Ctrl Pts',(0.865014404179025,6.96011942924032,
16.2342746355077));
#157202=CARTESIAN_POINT('Ctrl Pts',(0.681803480915807,6.98045347548991,
16.2426502458566));
#157203=CARTESIAN_POINT('Ctrl Pts',(0.497986110754245,6.99354247831497,
16.2510258562055));
#157204=CARTESIAN_POINT('Ctrl Pts',(0.314284364448098,7.00662324796289,
16.259396198171));
#157205=CARTESIAN_POINT('Ctrl Pts',(0.129977258900353,7.01246803762569,
16.2677665401366));
#157206=CARTESIAN_POINT('Ctrl Pts',(-0.0543416578270789,7.0110394055892,
16.2761368821022));
#157207=CARTESIAN_POINT('Ctrl Pts',(-0.238571654301916,7.00961146276208,
16.2845031859966));
#157208=CARTESIAN_POINT('Ctrl Pts',(-0.422813122465848,7.00091709807057,
16.2928694898909));
#157209=CARTESIAN_POINT('Ctrl Pts',(-0.606471251806126,6.98497095077945,
16.3012357937852));
#157210=CARTESIAN_POINT('Ctrl Pts',(-0.790078017115247,6.96902926317877,
16.3095997578588));
#157211=CARTESIAN_POINT('Ctrl Pts',(-0.973101441647726,6.94583986398603,
16.3179637219324));
#157212=CARTESIAN_POINT('Ctrl Pts',(-1.15495001680441,6.91546939991665,
16.326327686006));
#157213=CARTESIAN_POINT('Ctrl Pts',(-1.33677060848736,6.88510360935699,
16.3346903630046));
#157214=CARTESIAN_POINT('Ctrl Pts',(-1.51741638717926,6.84755901128605,
16.3430530400031));
#157215=CARTESIAN_POINT('Ctrl Pts',(-1.69630382237542,6.80295376323363,
16.3514157170017));
#157216=CARTESIAN_POINT('Ctrl Pts',(-1.87518757460608,6.75834943352178,
16.359778221828));
#157217=CARTESIAN_POINT('Ctrl Pts',(-2.05231273673844,6.70668482359164,
16.3681407266543));
#157218=CARTESIAN_POINT('Ctrl Pts',(-2.22710835418925,6.64812867965118,
16.3765032314806));
#157219=CARTESIAN_POINT('Ctrl Pts',(-2.40192367192968,6.58956593615741,
16.3848666788005));
#157220=CARTESIAN_POINT('Ctrl Pts',(-2.57440861009297,6.52411021501942,
16.3932301261205));
#157221=CARTESIAN_POINT('Ctrl Pts',(-2.74400928376474,6.45197951121305,
16.4015935734405));
#157222=CARTESIAN_POINT('Ctrl Pts',(-2.91370982307943,6.3798063348212,16.4099619453933));
#157223=CARTESIAN_POINT('Ctrl Pts',(-3.0805224010897,6.30095044972884,16.4183303173461));
#157224=CARTESIAN_POINT('Ctrl Pts',(-3.24391401049165,6.21567763442056,
16.4266986892989));
#157225=CARTESIAN_POINT('Ctrl Pts',(-3.40735457629014,6.13037926914814,
16.4350695686347));
#157226=CARTESIAN_POINT('Ctrl Pts',(-3.56737184065868,6.03866029666453,
16.4434404479705));
#157227=CARTESIAN_POINT('Ctrl Pts',(-3.72345854630337,5.94083184549609,
16.4518113273062));
#157228=CARTESIAN_POINT('Ctrl Pts',(-3.87967750252577,5.84292050533892,
16.4601892991975));
#157229=CARTESIAN_POINT('Ctrl Pts',(-4.03195896960979,5.73888952217155,
16.4685672710888));
#157230=CARTESIAN_POINT('Ctrl Pts',(-4.17982480036675,5.62909328406797,
16.4769452429801));
#157231=CARTESIAN_POINT('Ctrl Pts',(-4.27379473988855,5.55931688067919,
16.4822695123391));
#157232=CARTESIAN_POINT('Ctrl Pts',(-4.36598195812697,5.48721290535029,
16.4875937816981));
#157233=CARTESIAN_POINT('Ctrl Pts',(-4.45627082729048,5.41288064493758,
16.4929180510571));
#157234=CARTESIAN_POINT('Ctrl Pts',(-4.58960858476225,5.30310745802027,
16.5007808822463));
#157235=CARTESIAN_POINT('Ctrl Pts',(-4.71908165106864,5.18824423112787,
16.5086437134356));
#157236=CARTESIAN_POINT('Ctrl Pts',(-4.84426095490537,5.06860556398694,
16.5165065446249));
#157237=CARTESIAN_POINT('Ctrl Pts',(-4.96934407497058,4.94905882336958,
16.5243633342663));
#157238=CARTESIAN_POINT('Ctrl Pts',(-5.09013971963034,4.82474420115351,
16.5322201239076));
#157239=CARTESIAN_POINT('Ctrl Pts',(-5.20625085837897,4.69601730854223,
16.540076913549));
#157240=CARTESIAN_POINT('Ctrl Pts',(-5.32229651594179,4.56736301180475,
16.547929272333));
#157241=CARTESIAN_POINT('Ctrl Pts',(-5.43366266824448,4.43430167672755,
16.5557816311169));
#157242=CARTESIAN_POINT('Ctrl Pts',(-5.53998841533902,4.29722642182251,
16.5636339899009));
#157243=CARTESIAN_POINT('Ctrl Pts',(-5.64628905768406,4.16018353198454,
16.5714844946513));
#157244=CARTESIAN_POINT('Ctrl Pts',(-5.74755142330952,4.01912890439061,
16.5793349994017));
#157245=CARTESIAN_POINT('Ctrl Pts',(-5.84345432267586,3.87448940394742,
16.5871855041521));
#157246=CARTESIAN_POINT('Ctrl Pts',(-5.93934179428829,3.7298731714412,16.5950347460037));
#157247=CARTESIAN_POINT('Ctrl Pts',(-6.02987130763683,3.5816735337559,16.6028839878554));
#157248=CARTESIAN_POINT('Ctrl Pts',(-6.11476478558777,3.43034665586959,
16.610733229707));
#157249=CARTESIAN_POINT('Ctrl Pts',(-6.19968686581309,3.27896879299615,
16.6185851161218));
#157250=CARTESIAN_POINT('Ctrl Pts',(-6.27896893089106,3.12446191839945,
16.6264370025367));
#157251=CARTESIAN_POINT('Ctrl Pts',(-6.35237860285554,2.96730730604079,
16.6342888889515));
#157252=CARTESIAN_POINT('Ctrl Pts',(-6.40628241126751,2.85191063024941,
16.6400544314155));
#157253=CARTESIAN_POINT('Ctrl Pts',(-6.45702090177214,2.73508688812991,
16.6458199738795));
#157254=CARTESIAN_POINT('Ctrl Pts',(-6.50451862268238,2.61703344450889,
16.6515855163435));
#157255=CARTESIAN_POINT('Ctrl Pts',(-6.5840609995976,2.41933445330072,16.6612408207034));
#157256=CARTESIAN_POINT('Ctrl Pts',(-6.65447352736123,2.21828741597566,
16.6708961250633));
#157257=CARTESIAN_POINT('Ctrl Pts',(-6.71555819057391,2.01467236828117,
16.6805514294232));
#157258=CARTESIAN_POINT('Ctrl Pts',(-6.77698125136142,1.80992933142026,
16.690260222358));
#157259=CARTESIAN_POINT('Ctrl Pts',(-6.82897285094434,1.60258981369847,
16.6999690152927));
#157260=CARTESIAN_POINT('Ctrl Pts',(-6.87138419480713,1.39345104322139,
16.7096778082275));
#157261=CARTESIAN_POINT('Ctrl Pts',(-6.91399962565779,1.18330587922256,
16.7194333206982));
#157262=CARTESIAN_POINT('Ctrl Pts',(-6.94694239185566,0.971344151661304,
16.729188833169));
#157263=CARTESIAN_POINT('Ctrl Pts',(-6.97011401131694,0.758378026938607,
16.7389443456397));
#157264=CARTESIAN_POINT('Ctrl Pts',(-6.99330857424638,0.545201032988176,
16.7487095175686));
#157265=CARTESIAN_POINT('Ctrl Pts',(-7.00671264531666,0.331017691958229,
16.7584746894976));
#157266=CARTESIAN_POINT('Ctrl Pts',(-7.01027962605474,0.116645304328492,
16.7682398614265));
#157267=CARTESIAN_POINT('Ctrl Pts',(-7.01384174329551,-0.0974347914142347,
16.7779917187651));
#157268=CARTESIAN_POINT('Ctrl Pts',(-7.00759357668027,-0.311703380643881,
16.7877435761037));
#157269=CARTESIAN_POINT('Ctrl Pts',(-6.99154059236441,-0.525344370694879,
16.7974954334422));
#157270=CARTESIAN_POINT('Ctrl Pts',(-6.98454032859053,-0.618507314970021,
16.8017479495048));
#157271=CARTESIAN_POINT('Ctrl Pts',(-6.9756762554175,-0.711550891502383,
16.8060004655673));
#157272=CARTESIAN_POINT('Ctrl Pts',(-6.96495193175325,-0.804407328948929,
16.8102529816299));
#157273=CARTESIAN_POINT('Ctrl Pts',(-6.94469357652446,-0.979814072904426,
16.8182860272287));
#157274=CARTESIAN_POINT('Ctrl Pts',(-6.91778355046215,-1.15463820249878,
16.8263190728275));
#157275=CARTESIAN_POINT('Ctrl Pts',(-6.8842694409298,-1.32833008969161,
16.8343521184264));
#157276=CARTESIAN_POINT('Ctrl Pts',(-6.85077687555747,-1.50191032105159,
16.8423800000742));
#157277=CARTESIAN_POINT('Ctrl Pts',(-6.81068874636495,-1.67435940038211,
16.8504078817219));
#157278=CARTESIAN_POINT('Ctrl Pts',(-6.76410433349934,-1.84513390517747,
16.8584357633697));
#157279=CARTESIAN_POINT('Ctrl Pts',(-6.71754095395535,-2.01583130360049,
16.8664600203498));
#157280=CARTESIAN_POINT('Ctrl Pts',(-6.66448722721792,-2.18485528003029,
16.87448427733));
#157281=CARTESIAN_POINT('Ctrl Pts',(-6.60509328167289,-2.35167372373373,
16.8825085343101));
#157282=CARTESIAN_POINT('Ctrl Pts',(-6.54570651746083,-2.51847199738821,
16.8905318210758));
#157283=CARTESIAN_POINT('Ctrl Pts',(-6.4799811769894,-2.68306492176134,
16.8985551078415));
#157284=CARTESIAN_POINT('Ctrl Pts',(-6.40811696210377,-2.8449364777615,
16.9065783946072));
#157285=CARTESIAN_POINT('Ctrl Pts',(-6.33625863584952,-3.00679476983154,
16.9146010239361));
#157286=CARTESIAN_POINT('Ctrl Pts',(-6.25826258960548,-3.16593180423259,
16.922623653265));
#157287=CARTESIAN_POINT('Ctrl Pts',(-6.17437616390429,-3.32185272838977,
16.9306462825939));
#157288=CARTESIAN_POINT('Ctrl Pts',(-6.09045820287907,-3.47783226771412,
16.9386719278603));
#157289=CARTESIAN_POINT('Ctrl Pts',(-6.00064561527444,-3.63059295994871,
16.9466975731267));
#157290=CARTESIAN_POINT('Ctrl Pts',(-5.90523126753579,-3.77966536077172,
16.9547232183931));
#157291=CARTESIAN_POINT('Ctrl Pts',(-5.84896915384572,-3.8675675323207,
16.9594556279009));
#157292=CARTESIAN_POINT('Ctrl Pts',(-5.79076015132948,-3.95418780036338,
16.9641880374086));
#157293=CARTESIAN_POINT('Ctrl Pts',(-5.730671251391,-4.03943480835881,16.9689204469164));
#157294=CARTESIAN_POINT('Ctrl Pts',(-5.61982306083929,-4.19669308061732,
16.977650495751));
#157295=CARTESIAN_POINT('Ctrl Pts',(-5.50252001517797,-4.3493551652282,
16.9863805445857));
#157296=CARTESIAN_POINT('Ctrl Pts',(-5.37916323089467,-4.49691333003994,
16.9951105934203));
#157297=CARTESIAN_POINT('Ctrl Pts',(-5.25577077784348,-4.6445141614789,
17.0038431665595));
#157298=CARTESIAN_POINT('Ctrl Pts',(-5.12632126788788,-4.78700791715897,
17.0125757396987));
#157299=CARTESIAN_POINT('Ctrl Pts',(-4.99125530779404,-4.92392089852364,
17.0213083128378));
#157300=CARTESIAN_POINT('Ctrl Pts',(-4.8542705201311,-5.06277894734296,
17.0301649461182));
#157301=CARTESIAN_POINT('Ctrl Pts',(-4.71150868836064,-5.19589623937759,
17.0390215793986));
#157302=CARTESIAN_POINT('Ctrl Pts',(-4.56346755050197,-5.32281790765151,
17.0478782126791));
#157303=CARTESIAN_POINT('Ctrl Pts',(-4.41740719337916,-5.44804137231043,
17.0566163447858));
#157304=CARTESIAN_POINT('Ctrl Pts',(-4.26620815230103,-5.56723381445818,
17.0653544768926));
#157305=CARTESIAN_POINT('Ctrl Pts',(-4.11038189632529,-5.67999887577993,
17.0740926089993));
#157306=CARTESIAN_POINT('Ctrl Pts',(-3.95138581057447,-5.79505781271802,
17.0830084928666));
#157307=CARTESIAN_POINT('Ctrl Pts',(-3.78757247686869,-5.90342489858532,
17.0919243767338));
#157308=CARTESIAN_POINT('Ctrl Pts',(-3.61951728623572,-6.00472490436829,
17.100840260601));
#157309=CARTESIAN_POINT('Ctrl Pts',(-3.45146209560273,-6.10602491015128,
17.1097561444683));
#157310=CARTESIAN_POINT('Ctrl Pts',(-3.27916531018121,-6.20025768494112,
17.1186720283355));
#157311=CARTESIAN_POINT('Ctrl Pts',(-3.10323089411683,-6.2870966733699,
17.1275879122028));
#157312=CARTESIAN_POINT('Ctrl Pts',(-2.93075363378638,-6.37222925373202,
17.136328596699));
#157313=CARTESIAN_POINT('Ctrl Pts',(-2.75476205771371,-6.45026497194488,
17.1450692811952));
#157314=CARTESIAN_POINT('Ctrl Pts',(-2.5758462836326,-6.52093877333595,
17.1538099656915));
#157315=CARTESIAN_POINT('Ctrl Pts',(-2.39696269947126,-6.59159985933617,
17.1625490775933));
#157316=CARTESIAN_POINT('Ctrl Pts',(-2.21515622254328,-6.65490157315164,
17.1712881894952));
#157317=CARTESIAN_POINT('Ctrl Pts',(-2.03103635227476,-6.71062723582814,
17.1800273013971));
#157318=CARTESIAN_POINT('Ctrl Pts',(-1.84453094409265,-6.76707490466769,
17.1888796410715));
#157319=CARTESIAN_POINT('Ctrl Pts',(-1.65565204428361,-6.81574873246951,
17.1977319807458));
#157320=CARTESIAN_POINT('Ctrl Pts',(-1.46504971957287,-6.85647547079981,
17.2065843204201));
#157321=CARTESIAN_POINT('Ctrl Pts',(-1.27698177936859,-6.89666067735824,
17.2153189530699));
#157322=CARTESIAN_POINT('Ctrl Pts',(-1.08723623906643,-6.92910877720895,
17.2240535857197));
#157323=CARTESIAN_POINT('Ctrl Pts',(-0.896449502418545,-6.95370439780938,
17.2327882183694));
#157324=CARTESIAN_POINT('Ctrl Pts',(-0.701806231672854,-6.97879719054645,
17.2416994115561));
#157325=CARTESIAN_POINT('Ctrl Pts',(-0.506079508319231,-6.99571660669538,
17.2506106047427));
#157326=CARTESIAN_POINT('Ctrl Pts',(-0.309953463721105,-7.00439543521261,
17.2595217979293));
#157327=CARTESIAN_POINT('Ctrl Pts',(-0.113827419122962,-7.01307426372985,
17.2684329911159));
#157328=CARTESIAN_POINT('Ctrl Pts',(0.0826976444819196,-7.01351247775379,
17.2773441843025));
#157329=CARTESIAN_POINT('Ctrl Pts',(0.278933644378881,-7.00569929304231,
17.2862553774892));
#157330=CARTESIAN_POINT('Ctrl Pts',(0.455669164994588,-6.99866252472062,
17.2942810423415));
#157331=CARTESIAN_POINT('Ctrl Pts',(0.632251418391536,-6.98492904811914,
17.3023067071939));
#157332=CARTESIAN_POINT('Ctrl Pts',(0.80812813756787,-6.96452119501198,
17.3103323720463));
#157333=CARTESIAN_POINT('Ctrl Pts',(0.983949037787381,-6.94411981885684,
17.3183554897495));
#157334=CARTESIAN_POINT('Ctrl Pts',(1.15906448589412,-6.91704832570057,
17.3263786074527));
#157335=CARTESIAN_POINT('Ctrl Pts',(1.33292641381189,-6.88338098160073,
17.3344017251559));
#157336=CARTESIAN_POINT('Ctrl Pts',(1.50676641621861,-6.84971788324769,
17.3424238310738));
#157337=CARTESIAN_POINT('Ctrl Pts',(1.67935285364287,-6.80946066104088,
17.3504459369916));
#157338=CARTESIAN_POINT('Ctrl Pts',(1.85014699150703,-6.76273485154619,
17.3584680429094));
#157339=CARTESIAN_POINT('Ctrl Pts',(2.02100459705031,-6.71599167858271,
17.3664931298689));
#157340=CARTESIAN_POINT('Ctrl Pts',(2.19006821782699,-6.66277521032895,
17.3745182168285));
#157341=CARTESIAN_POINT('Ctrl Pts',(2.35681301314129,-6.60326123847814,
17.382543303788));
#157342=CARTESIAN_POINT('Ctrl Pts',(2.52359064800853,-6.54373554564842,
17.3905699712482));
#157343=CARTESIAN_POINT('Ctrl Pts',(2.68804820535844,-6.4779100099314,17.3985966387084));
#157344=CARTESIAN_POINT('Ctrl Pts',(2.84968022419069,-6.40600883408355,
17.4066233061687));
#157345=CARTESIAN_POINT('Ctrl Pts',(3.01144200063807,-6.33404993622512,
17.4146564174093));
#157346=CARTESIAN_POINT('Ctrl Pts',(3.17037337705654,-6.25600581409494,
17.4226895286498));
#157347=CARTESIAN_POINT('Ctrl Pts',(3.32599236708978,-6.17214722252803,
17.4307226398904));
#157348=CARTESIAN_POINT('Ctrl Pts',(3.41768872918733,-6.12273469404635,
17.4354560408521));
#157349=CARTESIAN_POINT('Ctrl Pts',(3.50823552404223,-6.07130424260402,
17.4401894418139));
#157350=CARTESIAN_POINT('Ctrl Pts',(3.59753882558523,-6.01791832454603,
17.4449228427756));
#157351=CARTESIAN_POINT('Ctrl Pts',(3.78150640606299,-5.90794167186893,
17.4546737960697));
#157352=CARTESIAN_POINT('Ctrl Pts',(3.96030414582063,-5.78960001110138,
17.4644247493639));
#157353=CARTESIAN_POINT('Ctrl Pts',(4.13326669071841,-5.6633676400087,17.4741757026581));
#157354=CARTESIAN_POINT('Ctrl Pts',(4.30647842060935,-5.53695340750466,
17.4839407040297));
#157355=CARTESIAN_POINT('Ctrl Pts',(4.47383810857436,-5.40262574800827,
17.4937057054013));
#157356=CARTESIAN_POINT('Ctrl Pts',(4.63471077704827,-5.26090130829429,
17.503470706773));
#157357=CARTESIAN_POINT('Ctrl Pts',(4.7953153041157,-5.11941309385686,17.5132194319106));
#157358=CARTESIAN_POINT('Ctrl Pts',(4.94945439307791,-4.97055276472544,
17.5229681570481));
#157359=CARTESIAN_POINT('Ctrl Pts',(5.09652968086165,-4.81487401440539,
17.5327168821857));
#157360=CARTESIAN_POINT('Ctrl Pts',(5.24320130400896,-4.65962254189043,
17.5424388508529));
#157361=CARTESIAN_POINT('Ctrl Pts',(5.38284780231951,-4.49759003650188,
17.5521608195201));
#157362=CARTESIAN_POINT('Ctrl Pts',(5.51490953229886,-4.32936478170403,
17.5618827881872));
#157363=CARTESIAN_POINT('Ctrl Pts',(5.64609744430358,-4.16225262947914,
17.571540429127));
#157364=CARTESIAN_POINT('Ctrl Pts',(5.76980057754607,-3.9890294274626,17.5811980700667));
#157365=CARTESIAN_POINT('Ctrl Pts',(5.8855044144789,-3.81031026947274,17.5908557110064));
#157366=CARTESIAN_POINT('Ctrl Pts',(5.93636023424994,-3.73175704661254,
17.5951005766916));
#157367=CARTESIAN_POINT('Ctrl Pts',(5.98567111523607,-3.65214255663833,
17.5993454423769));
#157368=CARTESIAN_POINT('Ctrl Pts',(6.03339552127299,-3.57152139100175,
17.6035903080621));
#157369=CARTESIAN_POINT('Ctrl Pts',(6.12167269252395,-3.42239416163723,
17.611442155076));
#157370=CARTESIAN_POINT('Ctrl Pts',(6.20448222130841,-3.26988191299991,
17.6192940020899));
#157371=CARTESIAN_POINT('Ctrl Pts',(6.28155018781221,-3.11444277528041,
17.6271458491038));
#157372=CARTESIAN_POINT('Ctrl Pts',(6.35859629846379,-2.9590477188437,17.6349954693974));
#157373=CARTESIAN_POINT('Ctrl Pts',(6.42990391644197,-2.80072776584618,
17.642845089691));
#157374=CARTESIAN_POINT('Ctrl Pts',(6.49524492938314,-2.63996588421567,
17.6506947099845));
#157375=CARTESIAN_POINT('Ctrl Pts',(6.56058072568014,-2.47921683736524,
17.6585437035863));
#157376=CARTESIAN_POINT('Ctrl Pts',(6.61995072229686,-2.31602660365896,
17.6663926971881));
#157377=CARTESIAN_POINT('Ctrl Pts',(6.67317494277457,-2.15089812534802,
17.6742416907899));
#157378=CARTESIAN_POINT('Ctrl Pts',(6.72642610911662,-1.98568604732373,
17.6820946581073));
#157379=CARTESIAN_POINT('Ctrl Pts',(6.77352516535617,-1.81853412759885,
17.6899476254247));
#157380=CARTESIAN_POINT('Ctrl Pts',(6.81434192970358,-1.64996079577172,
17.6978005927421));
#157381=CARTESIAN_POINT('Ctrl Pts',(6.85516906013767,-1.48134465198247,
17.7056555544494));
#157382=CARTESIAN_POINT('Ctrl Pts',(6.88971064413953,-1.31130675078587,
17.7135105161566));
#157383=CARTESIAN_POINT('Ctrl Pts',(6.91788777553333,-1.14037506445314,
17.7213654778639));
#157384=CARTESIAN_POINT('Ctrl Pts',(6.94609287508533,-0.969273714133762,
17.7292282362772));
#157385=CARTESIAN_POINT('Ctrl Pts',(6.96792085686429,-0.797277185065159,
17.7370909946906));
#157386=CARTESIAN_POINT('Ctrl Pts',(6.98334471739352,-0.624918491126651,
17.7449537531039));
#157387=CARTESIAN_POINT('Ctrl Pts',(6.99465944015861,-0.498478626452574,
17.7507217598521));
#157388=CARTESIAN_POINT('Ctrl Pts',(7.00252888663807,-0.371843959662768,
17.7564897666003));
#157389=CARTESIAN_POINT('Ctrl Pts',(7.00696022589238,-0.245224295823586,
17.7622577733485));
#157390=CARTESIAN_POINT('Ctrl Pts',(7.00984801535904,-0.162709527596158,
17.7660166345358));
#157391=CARTESIAN_POINT('Ctrl Pts',(7.01127732144656,-0.0801718186294929,
17.7697754957232));
#157392=CARTESIAN_POINT('Ctrl Pts',(7.01124960457305,0.00235475566585457,
17.7735343569105));
#157393=CARTESIAN_POINT('Ctrl Pts',(7.01124960457286,0.00235475623571418,
17.7735343569365));
#157394=CARTESIAN_POINT('Ctrl Pts',(7.0111881852894,0.185229705388182,17.7818638138947));
#157395=CARTESIAN_POINT('Ctrl Pts',(7.0039674730019,0.368245297451978,17.790193270853));
#157396=CARTESIAN_POINT('Ctrl Pts',(6.98958012196288,0.550814198402105,
17.7985227278113));
#157397=CARTESIAN_POINT('Ctrl Pts',(6.97520604982793,0.733214596136248,
17.8068444970403));
#157398=CARTESIAN_POINT('Ctrl Pts',(6.95367855695298,0.915168792105551,
17.8151662662693));
#157399=CARTESIAN_POINT('Ctrl Pts',(6.92504233787672,1.09609086353046,17.8234880354983));
#157400=CARTESIAN_POINT('Ctrl Pts',(6.89642175765243,1.27691412954095,17.8318052600311));
#157401=CARTESIAN_POINT('Ctrl Pts',(6.86070024019595,1.45670606423809,17.8401224845638));
#157402=CARTESIAN_POINT('Ctrl Pts',(6.81797423568344,1.63488650494671,17.8484397090966));
#157403=CARTESIAN_POINT('Ctrl Pts',(6.77526708842652,1.81298830516108,17.8567532627963));
#157404=CARTESIAN_POINT('Ctrl Pts',(6.72556169588046,1.98947970414347,17.865066816496));
#157405=CARTESIAN_POINT('Ctrl Pts',(6.66900552753703,2.16379107960555,17.8733803701958));
#157406=CARTESIAN_POINT('Ctrl Pts',(6.63837243453911,2.25820512375897,17.8778833248882));
#157407=CARTESIAN_POINT('Ctrl Pts',(6.60573038066985,2.35197980392451,17.8823862795806));
#157408=CARTESIAN_POINT('Ctrl Pts',(6.57110895151814,2.44502632087637,17.886889234273));
#157409=CARTESIAN_POINT('',(7.01124984869581,-0.00145659295646808,17.2264656431293));
#157410=CARTESIAN_POINT('Ctrl Pts',(6.57110895151813,2.44502632087639,17.3396585048403));
#157411=CARTESIAN_POINT('Ctrl Pts',(6.64521162053806,2.24587234548946,17.3299972645521));
#157412=CARTESIAN_POINT('Ctrl Pts',(6.71031798372647,2.04318290855153,17.3203360242638));
#157413=CARTESIAN_POINT('Ctrl Pts',(6.76612737026639,1.83770154590782,17.3106747839755));
#157414=CARTESIAN_POINT('Ctrl Pts',(6.79678406298721,1.72482843647281,17.3053677613906));
#157415=CARTESIAN_POINT('Ctrl Pts',(6.82463624788957,1.61111333633684,17.3000607388057));
#157416=CARTESIAN_POINT('Ctrl Pts',(6.84963993305301,1.49668278203018,17.2947537162207));
#157417=CARTESIAN_POINT('Ctrl Pts',(6.88499295409668,1.3348879998611,17.287250051065));
#157418=CARTESIAN_POINT('Ctrl Pts',(6.91464614817789,1.17167025084036,17.2797463859093));
#157419=CARTESIAN_POINT('Ctrl Pts',(6.93848291677126,1.00751246948778,17.2722427207536));
#157420=CARTESIAN_POINT('Ctrl Pts',(6.96271946392455,0.840601514559226,
17.2646132078162));
#157421=CARTESIAN_POINT('Ctrl Pts',(6.98094261072084,0.672719122730744,
17.2569836948789));
#157422=CARTESIAN_POINT('Ctrl Pts',(6.99308397869091,0.504383811671779,
17.2493541819415));
#157423=CARTESIAN_POINT('Ctrl Pts',(7.00522534666098,0.336048500612814,
17.2417246690041));
#157424=CARTESIAN_POINT('Ctrl Pts',(7.01128489985525,0.167260710847184,
17.2340951560667));
#157425=CARTESIAN_POINT('Ctrl Pts',(7.01124984869581,-0.00145659295646722,
17.2264656431293));
#157426=CARTESIAN_POINT('Ctrl Pts',(7.01124984869562,-0.00145659383538793,
17.2264656430896));
#157427=CARTESIAN_POINT('Ctrl Pts',(7.01121141547279,-0.186453208016376,
17.2180999685));
#157428=CARTESIAN_POINT('Ctrl Pts',(7.00384680112655,-0.37131131097293,
17.2097342939103));
#157429=CARTESIAN_POINT('Ctrl Pts',(6.98921446351228,-0.555434735617764,
17.2013686193206));
#157430=CARTESIAN_POINT('Ctrl Pts',(6.97456974963572,-0.739713894763606,
17.1929958689113));
#157431=CARTESIAN_POINT('Ctrl Pts',(6.95264508443871,-0.923256813949637,
17.1846231185019));
#157432=CARTESIAN_POINT('Ctrl Pts',(6.92355038038466,-1.10547577665705,
17.1762503680925));
#157433=CARTESIAN_POINT('Ctrl Pts',(6.89440752844861,-1.28799628761518,
17.1678637618901));
#157434=CARTESIAN_POINT('Ctrl Pts',(6.85807098344544,-1.46918814448098,
17.1594771556876));
#157435=CARTESIAN_POINT('Ctrl Pts',(6.81470140781121,-1.64847544260627,
17.1510905494852));
#157436=CARTESIAN_POINT('Ctrl Pts',(6.78883754642982,-1.75539513823031,
17.1460891166349));
#157437=CARTESIAN_POINT('Ctrl Pts',(6.76047337797917,-1.86163779181118,
17.1410876837846));
#157438=CARTESIAN_POINT('Ctrl Pts',(6.72965120968409,-1.96708443095296,
17.1360862509343));
#157439=CARTESIAN_POINT('Ctrl Pts',(6.67801997088463,-2.14372160177126,
17.1277081844933));
#157440=CARTESIAN_POINT('Ctrl Pts',(6.61939583769859,-2.31844204455275,
17.1193301180522));
#157441=CARTESIAN_POINT('Ctrl Pts',(6.55394277257689,-2.49067474718945,
17.1109520516112));
#157442=CARTESIAN_POINT('Ctrl Pts',(6.48853446348344,-2.66278967915043,
17.1025797139925));
#157443=CARTESIAN_POINT('Ctrl Pts',(6.41630664854421,-2.83241995612727,
17.0942073763737));
#157444=CARTESIAN_POINT('Ctrl Pts',(6.33747279090054,-2.99901070139728,
17.085835038755));
#157445=CARTESIAN_POINT('Ctrl Pts',(6.25868127787468,-3.16551196453802,
17.0774671982324));
#157446=CARTESIAN_POINT('Ctrl Pts',(6.1732909375192,-3.32897665484439,17.0690993577098));
#157447=CARTESIAN_POINT('Ctrl Pts',(6.08156311049281,-3.48887040395499,
17.0607315171872));
#157448=CARTESIAN_POINT('Ctrl Pts',(5.98987111645723,-3.64870169141759,
17.0523669455172));
#157449=CARTESIAN_POINT('Ctrl Pts',(5.89184673599072,-3.80496453474687,
17.0440023738473));
#157450=CARTESIAN_POINT('Ctrl Pts',(5.7877971738053,-3.95714928166621,17.0356378021774));
#157451=CARTESIAN_POINT('Ctrl Pts',(5.68377302768726,-4.10929685459174,
17.0272752737118));
#157452=CARTESIAN_POINT('Ctrl Pts',(5.57372682060596,-4.25736804682712,
17.0189127452462));
#157453=CARTESIAN_POINT('Ctrl Pts',(5.45800923434146,-4.40088192983445,
17.0105502167806));
#157454=CARTESIAN_POINT('Ctrl Pts',(5.34228241345161,-4.54440726569856,
17.0021870209591));
#157455=CARTESIAN_POINT('Ctrl Pts',(5.22088351075938,-4.68337430608855,
16.9938238251376));
#157456=CARTESIAN_POINT('Ctrl Pts',(5.09420415672048,-4.81733438450684,
16.9854606293161));
#157457=CARTESIAN_POINT('Ctrl Pts',(4.9675161634036,-4.9513035987339,16.9770968631414));
#157458=CARTESIAN_POINT('Ctrl Pts',(4.83554722643299,-5.08026493103917,
16.9687330969667));
#157459=CARTESIAN_POINT('Ctrl Pts',(4.69872669322736,-5.20380572512586,
16.960369330792));
#157460=CARTESIAN_POINT('Ctrl Pts',(4.56187858774039,-5.32737141534072,
16.9520038791384));
#157461=CARTESIAN_POINT('Ctrl Pts',(4.42017718049494,-5.44551416882182,
16.9436384274849));
#157462=CARTESIAN_POINT('Ctrl Pts',(4.27408614211591,-5.55786057870048,
16.9352729758313));
#157463=CARTESIAN_POINT('Ctrl Pts',(4.12794617813501,-5.67024461317118,
16.9269047226044));
#157464=CARTESIAN_POINT('Ctrl Pts',(3.977413912167,-5.77682823291574,16.9185364693776));
#157465=CARTESIAN_POINT('Ctrl Pts',(3.82298366178426,-5.87728019446331,
16.9101682161507));
#157466=CARTESIAN_POINT('Ctrl Pts',(3.66841023252764,-5.97782528931019,
16.9017922043592));
#157467=CARTESIAN_POINT('Ctrl Pts',(3.50993187292332,-6.07222718633111,
16.8934161925677));
#157468=CARTESIAN_POINT('Ctrl Pts',(3.34807034260579,-6.16019898570359,
16.8850401807763));
#157469=CARTESIAN_POINT('Ctrl Pts',(3.18612943339389,-6.24821392753344,
16.8766600612851));
#157470=CARTESIAN_POINT('Ctrl Pts',(3.02080233661885,-6.3297923320713,16.868279941794));
#157471=CARTESIAN_POINT('Ctrl Pts',(2.8526332423941,-6.40469438356649,16.8598998223028));
#157472=CARTESIAN_POINT('Ctrl Pts',(2.6842719936766,-6.47968202014363,16.8515101274636));
#157473=CARTESIAN_POINT('Ctrl Pts',(2.51306256168837,-6.5479779323654,16.8431204326244));
#157474=CARTESIAN_POINT('Ctrl Pts',(2.33956809462149,-6.60939087156518,
16.8347307377852));
#157475=CARTESIAN_POINT('Ctrl Pts',(2.22941945143073,-6.64838088687561,
16.8294042653106));
#157476=CARTESIAN_POINT('Ctrl Pts',(2.11835009357165,-6.68459753836778,
16.824077792836));
#157477=CARTESIAN_POINT('Ctrl Pts',(2.00650681878506,-6.71800245226727,
16.8187513203614));
#157478=CARTESIAN_POINT('Ctrl Pts',(1.83051941084748,-6.77056568613866,
16.8103700199566));
#157479=CARTESIAN_POINT('Ctrl Pts',(1.65226018973763,-6.81627070874301,
16.8019887195517));
#157480=CARTESIAN_POINT('Ctrl Pts',(1.47228955157064,-6.85492451007565,
16.7936074191468));
#157481=CARTESIAN_POINT('Ctrl Pts',(1.29254699984151,-6.89352932337367,
16.7852367408132));
#157482=CARTESIAN_POINT('Ctrl Pts',(1.11109767133741,-6.92510065645303,
16.7768660624797));
#157483=CARTESIAN_POINT('Ctrl Pts',(0.928517585893615,-6.94949506476451,
16.7684953841461));
#157484=CARTESIAN_POINT('Ctrl Pts',(0.746144697499774,-6.97386178961082,
16.7601342050953));
#157485=CARTESIAN_POINT('Ctrl Pts',(0.562643932545363,-6.99106777960009,
16.7517730260445));
#157486=CARTESIAN_POINT('Ctrl Pts',(0.378602425101677,-7.00102040892663,
16.7434118469937));
#157487=CARTESIAN_POINT('Ctrl Pts',(0.194799733223228,-7.01096012354261,
16.735061517559));
#157488=CARTESIAN_POINT('Ctrl Pts',(0.0104580240532623,-7.01366523329991,
16.7267111881243));
#157489=CARTESIAN_POINT('Ctrl Pts',(-0.173829587183502,-7.00909479441673,
16.7183608586895));
#157490=CARTESIAN_POINT('Ctrl Pts',(-0.357975400127153,-7.00452787221287,
16.7100169543338));
#157491=CARTESIAN_POINT('Ctrl Pts',(-0.542066871929678,-6.99269656545033,
16.7016730499781));
#157492=CARTESIAN_POINT('Ctrl Pts',(-0.725508864308825,-6.97361193717498,
16.6933291456224));
#157493=CARTESIAN_POINT('Ctrl Pts',(-0.908803514935531,-6.95454263779209,
16.6849919431427));
#157494=CARTESIAN_POINT('Ctrl Pts',(-1.09144940157904,-6.92823166965606,
16.676654740663));
#157495=CARTESIAN_POINT('Ctrl Pts',(-1.27285433476826,-6.89474208400588,
16.6683175381833));
#157496=CARTESIAN_POINT('Ctrl Pts',(-1.33257183744352,-6.88371749726781,
16.6655729771472));
#157497=CARTESIAN_POINT('Ctrl Pts',(-1.39215489261315,-6.87191538931628,
16.6628284161111));
#157498=CARTESIAN_POINT('Ctrl Pts',(-1.45158250318175,-6.85933923923847,
16.660083855075));
#157499=CARTESIAN_POINT('Ctrl Pts',(-1.63213081342386,-6.82113136542065,
16.6517455447731));
#157500=CARTESIAN_POINT('Ctrl Pts',(-1.81109548287068,-6.77580649576908,
16.6434072344712));
#157501=CARTESIAN_POINT('Ctrl Pts',(-1.98790383542801,-6.7235306873391,
16.6350689241693));
#157502=CARTESIAN_POINT('Ctrl Pts',(-2.16482342980106,-6.67122198874435,
16.6267253676855));
#157503=CARTESIAN_POINT('Ctrl Pts',(-2.33958368701016,-6.61195372118975,
16.6183818112017));
#157504=CARTESIAN_POINT('Ctrl Pts',(-2.51162909085513,-6.54594117545142,
16.6100382547179));
#157505=CARTESIAN_POINT('Ctrl Pts',(-2.68380538609342,-6.47987840765602,
16.6016883504927));
#157506=CARTESIAN_POINT('Ctrl Pts',(-2.85326240251176,-6.40706124421282,
16.5933384462675));
#157507=CARTESIAN_POINT('Ctrl Pts',(-3.0194661192203,-6.32775243806051,
16.5849885420423));
#157508=CARTESIAN_POINT('Ctrl Pts',(-3.18591912920494,-6.24832467456777,
16.5766261135786));
#157509=CARTESIAN_POINT('Ctrl Pts',(-3.34910879232073,-6.16238595203878,
16.568263685115));
#157510=CARTESIAN_POINT('Ctrl Pts',(-3.50852581953311,-6.07024489919225,
16.5599012566513));
#157511=CARTESIAN_POINT('Ctrl Pts',(-3.66807917003529,-5.97802505318498,
16.5515316771713));
#157512=CARTESIAN_POINT('Ctrl Pts',(-3.82385317136701,-5.8795924689408,
16.5431620976914));
#157513=CARTESIAN_POINT('Ctrl Pts',(-3.97536843563536,-5.77529846531364,
16.5347925182115));
#157514=CARTESIAN_POINT('Ctrl Pts',(-4.12711739373861,-5.6708436008928,
16.5264100296749));
#157515=CARTESIAN_POINT('Ctrl Pts',(-4.27459422694588,-5.56050944732146,
16.5180275411383));
#157516=CARTESIAN_POINT('Ctrl Pts',(-4.41735237280503,-5.44468773916134,
16.5096450526017));
#157517=CARTESIAN_POINT('Ctrl Pts',(-4.4640651773608,-5.40678897840034,
16.5069021649974));
#157518=CARTESIAN_POINT('Ctrl Pts',(-4.51027304346737,-5.36830295603565,
16.504159277393));
#157519=CARTESIAN_POINT('Ctrl Pts',(-4.55596120317526,-5.3292442313767,
16.5014163897886));
#157520=CARTESIAN_POINT('Ctrl Pts',(-4.69571065576761,-5.2097726784636,
16.4930265346558));
#157521=CARTESIAN_POINT('Ctrl Pts',(-4.83087709247391,-5.08469895501282,
16.484636679523));
#157522=CARTESIAN_POINT('Ctrl Pts',(-4.96100246275852,-4.95440017832672,
16.4762468243903));
#157523=CARTESIAN_POINT('Ctrl Pts',(-5.09100775517568,-4.82422163952509,
16.4678647112982));
#157524=CARTESIAN_POINT('Ctrl Pts',(-5.21598102341111,-4.68882789082997,
16.4594825982061));
#157525=CARTESIAN_POINT('Ctrl Pts',(-5.33549858863682,-4.54863511101456,
16.451100485114));
#157526=CARTESIAN_POINT('Ctrl Pts',(-5.45492343356298,-4.40855109108324,
16.4427248747651));
#157527=CARTESIAN_POINT('Ctrl Pts',(-5.5689008012334,-4.26367571188172,
16.4343492644162));
#157528=CARTESIAN_POINT('Ctrl Pts',(-5.67704476441904,-4.11446099814816,
16.4259736540673));
#157529=CARTESIAN_POINT('Ctrl Pts',(-5.7851207034458,-3.96534014268552,
16.4176033121018));
#157530=CARTESIAN_POINT('Ctrl Pts',(-5.88737036182711,-3.81188566056653,
16.4092329701362));
#157531=CARTESIAN_POINT('Ctrl Pts',(-5.98344863786708,-3.65458191322983,
16.4008626281706));
#157532=CARTESIAN_POINT('Ctrl Pts',(-6.07948056324105,-3.49735405332319,
16.3924963242763));
#157533=CARTESIAN_POINT('Ctrl Pts',(-6.16934687232379,-3.33628091136447,
16.384130020382));
#157534=CARTESIAN_POINT('Ctrl Pts',(-6.25274603156381,-3.17187541168676,
16.3757637164876));
#157535=CARTESIAN_POINT('Ctrl Pts',(-6.33612186639654,-3.00751589161928,
16.367399752414));
#157536=CARTESIAN_POINT('Ctrl Pts',(-6.41303400803017,-2.8398261643493,
16.3590357883404));
#157537=CARTESIAN_POINT('Ctrl Pts',(-6.48322683788039,-2.6693438015901,
16.3506718242668));
#157538=CARTESIAN_POINT('Ctrl Pts',(-6.55340886622055,-2.49888767323347,
16.3423091472682));
#157539=CARTESIAN_POINT('Ctrl Pts',(-6.61687351925621,-2.32564007002177,
16.3339464702697));
#157540=CARTESIAN_POINT('Ctrl Pts',(-6.67341313985151,-2.15015897722873,
16.3255837932712));
#157541=CARTESIAN_POINT('Ctrl Pts',(-6.72995159639933,-1.97468149727072,
16.3172212884448));
#157542=CARTESIAN_POINT('Ctrl Pts',(-6.77956520439417,-1.79697093235842,
16.3088587836185));
#157543=CARTESIAN_POINT('Ctrl Pts',(-6.82209591187667,-1.61760128945783,
16.3004962787922));
#157544=CARTESIAN_POINT('Ctrl Pts',(-6.86463141277021,-1.4382114307537,
16.2921328314723));
#157545=CARTESIAN_POINT('Ctrl Pts',(-6.90008234631887,-1.25716244115872,
16.2837693841523));
#157546=CARTESIAN_POINT('Ctrl Pts',(-6.92834149969731,-1.07503982534234,
16.2754059368323));
#157547=CARTESIAN_POINT('Ctrl Pts',(-6.95661729285943,-0.892809970611502,
16.2670375648795));
#157548=CARTESIAN_POINT('Ctrl Pts',(-6.97769279247257,-0.709505551373533,
16.2586691929267));
#157549=CARTESIAN_POINT('Ctrl Pts',(-6.99151239034034,-0.525719562331074,
16.2503008209739));
#157550=CARTESIAN_POINT('Ctrl Pts',(-7.0053361289208,-0.341878506202975,
16.2419299416381));
#157551=CARTESIAN_POINT('Ctrl Pts',(-7.0118996113659,-0.157555920751295,
16.2335590623024));
#157552=CARTESIAN_POINT('Ctrl Pts',(-7.01119933913227,0.0266531321092605,
16.2251881829666));
#157553=CARTESIAN_POINT('Ctrl Pts',(-7.01049847356555,0.211018263308303,
16.2168102110753));
#157554=CARTESIAN_POINT('Ctrl Pts',(-7.00252156216052,0.395269340809793,
16.208432239184));
#157555=CARTESIAN_POINT('Ctrl Pts',(-6.9873172140908,0.578813192809563,
16.2000542672927));
#157556=CARTESIAN_POINT('Ctrl Pts',(-6.97765472708303,0.695456805358571,
16.1947299979337));
#157557=CARTESIAN_POINT('Ctrl Pts',(-6.9650743382028,0.811814874612261,
16.1894057285747));
#157558=CARTESIAN_POINT('Ctrl Pts',(-6.94959934240933,0.92773678513023,
16.1840814592157));
#157559=CARTESIAN_POINT('Ctrl Pts',(-6.92674601336555,1.09892917831777,
16.1762186280265));
#157560=CARTESIAN_POINT('Ctrl Pts',(-6.89752954876172,1.26952587813066,
16.1683557968372));
#157561=CARTESIAN_POINT('Ctrl Pts',(-6.86199066830943,1.43899639698447,
16.1604929656479));
#157562=CARTESIAN_POINT('Ctrl Pts',(-6.82647909479571,1.60833670011434,
16.1526361760065));
#157563=CARTESIAN_POINT('Ctrl Pts',(-6.78465484389676,1.77655217235836,
16.1447793863651));
#157564=CARTESIAN_POINT('Ctrl Pts',(-6.73661038061155,1.94311789203246,
16.1369225967237));
#157565=CARTESIAN_POINT('Ctrl Pts',(-6.68859301212934,2.10958967652546,
16.1290702379398));
#157566=CARTESIAN_POINT('Ctrl Pts',(-6.63436251462591,2.27441319399734,
16.1212178791558));
#157567=CARTESIAN_POINT('Ctrl Pts',(-6.57406228090848,2.43707441192024,
16.1133655203719));
#157568=CARTESIAN_POINT('Ctrl Pts',(-6.5137762847798,2.59969722363173,16.1055150156215));
#157569=CARTESIAN_POINT('Ctrl Pts',(-6.44742352927106,2.76015839181329,
16.097664510871));
#157570=CARTESIAN_POINT('Ctrl Pts',(-6.37519703030243,2.91795979878461,
16.0898140061206));
#157571=CARTESIAN_POINT('Ctrl Pts',(-6.30298215030111,3.07573582048299,
16.081964764269));
#157572=CARTESIAN_POINT('Ctrl Pts',(-6.22489556937921,3.23085258707242,
16.0741155224173));
#157573=CARTESIAN_POINT('Ctrl Pts',(-6.14117794584862,3.38283313214273,
16.0662662805657));
#157574=CARTESIAN_POINT('Ctrl Pts',(-6.05743211621199,3.5348648824335,16.0584143941509));
#157575=CARTESIAN_POINT('Ctrl Pts',(-5.96805163865196,3.68375796612744,
16.050562507736));
#157576=CARTESIAN_POINT('Ctrl Pts',(-5.87332261961546,3.82906097736944,
16.0427106213211));
#157577=CARTESIAN_POINT('Ctrl Pts',(-5.80376428000561,3.93575516997383,
16.0369450788572));
#157578=CARTESIAN_POINT('Ctrl Pts',(-5.73132307943551,4.04051419632107,
16.0311795363932));
#157579=CARTESIAN_POINT('Ctrl Pts',(-5.65612682125047,4.14316979430376,
16.0254139939293));
#157580=CARTESIAN_POINT('Ctrl Pts',(-5.53019890309862,4.3150826800325,16.0157586895694));
#157581=CARTESIAN_POINT('Ctrl Pts',(-5.39660821342972,4.48100845535577,
16.0061033852096));
#157582=CARTESIAN_POINT('Ctrl Pts',(-5.2559127474701,4.64036720028505,15.9964480808497));
#157583=CARTESIAN_POINT('Ctrl Pts',(-5.11443785502317,4.80060876276595,
15.986739287915));
#157584=CARTESIAN_POINT('Ctrl Pts',(-4.9657793222305,4.95421033392937,15.9770304949802));
#157585=CARTESIAN_POINT('Ctrl Pts',(-4.81053572745499,5.10062472422537,
15.9673217020455));
#157586=CARTESIAN_POINT('Ctrl Pts',(-4.65454508731951,5.24774367299968,
15.9575661895748));
#157587=CARTESIAN_POINT('Ctrl Pts',(-4.49190590489966,5.3876060916009,15.9478106771041));
#157588=CARTESIAN_POINT('Ctrl Pts',(-4.32325600339384,5.51969963780812,
15.9380551646334));
#157589=CARTESIAN_POINT('Ctrl Pts',(-4.15443911253939,5.65192397694818,
15.9282899927045));
#157590=CARTESIAN_POINT('Ctrl Pts',(-3.97959963524236,5.77636404233737,
15.9185248207756));
#157591=CARTESIAN_POINT('Ctrl Pts',(-3.79940714174909,5.89254884864996,
15.9087596488467));
#157592=CARTESIAN_POINT('Ctrl Pts',(-3.61946033663232,6.00857523961526,
15.8990077915081));
#157593=CARTESIAN_POINT('Ctrl Pts',(-3.43417513474398,6.11636884739151,
15.8892559341696));
#157594=CARTESIAN_POINT('Ctrl Pts',(-3.24424756249647,6.21550354482529,
15.879504076831));
#157595=CARTESIAN_POINT('Ctrl Pts',(-3.16142538578677,6.25873345258309,
15.8752515607683));
#157596=CARTESIAN_POINT('Ctrl Pts',(-3.07772079202939,6.30031734263474,
15.8709990447056));
#157597=CARTESIAN_POINT('Ctrl Pts',(-2.99319322076793,6.34022246499671,
15.8667465286428));
#157598=CARTESIAN_POINT('Ctrl Pts',(-2.8335197887848,6.41560364235874,15.858713483044));
#157599=CARTESIAN_POINT('Ctrl Pts',(-2.67083014928502,6.48502775193635,
15.8506804374452));
#157600=CARTESIAN_POINT('Ctrl Pts',(-2.50561624272882,6.54824509366239,
15.8426473918463));
#157601=CARTESIAN_POINT('Ctrl Pts',(-2.34050854203324,6.61142179684701,
15.8346195101985));
#157602=CARTESIAN_POINT('Ctrl Pts',(-2.17288014523112,6.66839954381638,
15.8265916285507));
#157603=CARTESIAN_POINT('Ctrl Pts',(-2.00324500790262,6.71897581487039,
15.8185637469029));
#157604=CARTESIAN_POINT('Ctrl Pts',(-1.83368646251062,6.76952925023951,
15.8105394899228));
#157605=CARTESIAN_POINT('Ctrl Pts',(-1.66212333122726,6.81368686015267,
15.8025152329427));
#157606=CARTESIAN_POINT('Ctrl Pts',(-1.48908680202622,6.85129528326807,
15.7944909759626));
#157607=CARTESIAN_POINT('Ctrl Pts',(-1.31607119470399,6.88889915914207,
15.7864676891969));
#157608=CARTESIAN_POINT('Ctrl Pts',(-1.14158290066625,6.91995534013259,
15.7784444024312));
#157609=CARTESIAN_POINT('Ctrl Pts',(-0.966165607655633,6.94436106355966,
15.7704211156655));
#157610=CARTESIAN_POINT('Ctrl Pts',(-0.790762688527433,6.96876478715539,
15.7623984863365));
#157611=CARTESIAN_POINT('Ctrl Pts',(-0.614431285757129,6.98651909212234,
15.7543758570076));
#157612=CARTESIAN_POINT('Ctrl Pts',(-0.437722255297477,6.99757284990427,
15.7463532276787));
#157613=CARTESIAN_POINT('Ctrl Pts',(-0.260946794822806,7.00863076311217,
15.7383275824123));
#157614=CARTESIAN_POINT('Ctrl Pts',(-0.0837937893559116,7.01298307725086,
15.7303019371459));
#157615=CARTESIAN_POINT('Ctrl Pts',(0.0931834548376472,7.01063074239719,
15.7222762918795));
#157616=CARTESIAN_POINT('Ctrl Pts',(0.197540022473344,7.00924366242327,
15.7175438823718));
#157617=CARTESIAN_POINT('Ctrl Pts',(0.301835470615949,7.00552636419604,
15.7128114728641));
#157618=CARTESIAN_POINT('Ctrl Pts',(0.405956845365878,6.99948752425494,
15.7080790633564));
#157619=CARTESIAN_POINT('Ctrl Pts',(0.598033352021251,6.98834745543698,
15.6993490145218));
#157620=CARTESIAN_POINT('Ctrl Pts',(0.789613284952843,6.96929894113871,
15.6906189656871));
#157621=CARTESIAN_POINT('Ctrl Pts',(0.980053679305924,6.94241466265009,
15.6818889168525));
#157622=CARTESIAN_POINT('Ctrl Pts',(1.17054913973635,6.91552261053884,15.6731563437134));
#157623=CARTESIAN_POINT('Ctrl Pts',(1.35990413263774,6.88079031002813,15.6644237705742));
#157624=CARTESIAN_POINT('Ctrl Pts',(1.54748375457549,6.83834194756484,15.6556911974351));
#157625=CARTESIAN_POINT('Ctrl Pts',(1.73772824447685,6.79529053835231,15.6468345641546));
#157626=CARTESIAN_POINT('Ctrl Pts',(1.92614625230624,6.74430222229125,15.6379779308742));
#157627=CARTESIAN_POINT('Ctrl Pts',(2.11208871266556,6.68555964989699,15.6291212975938));
#157628=CARTESIAN_POINT('Ctrl Pts',(2.29554327507376,6.62760304927713,15.6203831654871));
#157629=CARTESIAN_POINT('Ctrl Pts',(2.4765878660588,6.56209851231269,15.6116450333804));
#157630=CARTESIAN_POINT('Ctrl Pts',(2.65461586619075,6.48927123531359,15.6029069012736));
#157631=CARTESIAN_POINT('Ctrl Pts',(2.83626532569898,6.41496250020148,15.5939910174064));
#157632=CARTESIAN_POINT('Ctrl Pts',(3.01477387672386,6.33303002306115,15.5850751335391));
#157633=CARTESIAN_POINT('Ctrl Pts',(3.18951910498039,6.24376444474526,15.5761592496718));
#157634=CARTESIAN_POINT('Ctrl Pts',(3.36426433323694,6.15449886642937,15.5672433658046));
#157635=CARTESIAN_POINT('Ctrl Pts',(3.53524597218369,6.05790032992673,15.5583274819373));
#157636=CARTESIAN_POINT('Ctrl Pts',(3.70186786591409,5.95430943651845,15.54941159807));
#157637=CARTESIAN_POINT('Ctrl Pts',(3.86521559732732,5.85275413034307,15.5406709135738));
#157638=CARTESIAN_POINT('Ctrl Pts',(4.02439068243854,5.74446793341385,15.5319302290776));
#157639=CARTESIAN_POINT('Ctrl Pts',(4.17885650916467,5.62981214946929,15.5231895445813));
#157640=CARTESIAN_POINT('Ctrl Pts',(4.33329454492248,5.51517699400501,15.5144504326795));
#157641=CARTESIAN_POINT('Ctrl Pts',(4.48302479459601,5.39417470329297,15.5057113207776));
#157642=CARTESIAN_POINT('Ctrl Pts',(4.62754150307941,5.2672085775843,15.4969722088757));
#157643=CARTESIAN_POINT('Ctrl Pts',(4.77393063351689,5.13859742298107,15.4881198692014));
#157644=CARTESIAN_POINT('Ctrl Pts',(4.91496995418404,5.00386698717785,15.479267529527));
#157645=CARTESIAN_POINT('Ctrl Pts',(5.05016918409218,4.86347795045333,15.4704151898527));
#157646=CARTESIAN_POINT('Ctrl Pts',(5.18357070857305,4.72495562653051,15.4616805572029));
#157647=CARTESIAN_POINT('Ctrl Pts',(5.31128630095293,4.58092446076588,15.4529459245531));
#157648=CARTESIAN_POINT('Ctrl Pts',(5.43288204854389,4.43186407836585,15.4442112919034));
#157649=CARTESIAN_POINT('Ctrl Pts',(5.55693571409598,4.27979061205085,15.4353000987167));
#157650=CARTESIAN_POINT('Ctrl Pts',(5.67461928824829,4.1224826553152,15.4263889055301));
#157651=CARTESIAN_POINT('Ctrl Pts',(5.78551457111583,3.96048579216066,15.4174777123435));
#157652=CARTESIAN_POINT('Ctrl Pts',(5.89640985398337,3.79848892900611,15.4085665191568));
#157653=CARTESIAN_POINT('Ctrl Pts',(6.00051666321702,3.63180340195692,15.3996553259702));
#157654=CARTESIAN_POINT('Ctrl Pts',(6.09746263884185,3.46100793562047,15.3907441327836));
#157655=CARTESIAN_POINT('Ctrl Pts',(6.18477556157925,3.30718358901897,15.3827184017805));
#157656=CARTESIAN_POINT('Ctrl Pts',(6.26631969761614,3.1499545437622,15.3746926707773));
#157657=CARTESIAN_POINT('Ctrl Pts',(6.34182249675829,2.98980166267102,15.3666669397742));
#157658=CARTESIAN_POINT('Ctrl Pts',(6.41729889345471,2.82970478516913,15.3586440152753));
#157659=CARTESIAN_POINT('Ctrl Pts',(6.4867380049896,2.66668643947756,15.3506210907764));
#157660=CARTESIAN_POINT('Ctrl Pts',(6.54991363018798,2.50125128677182,15.3425981662775));
#157661=CARTESIAN_POINT('Ctrl Pts',(6.55705890610752,2.48254027585327,15.3416907592033));
#157662=CARTESIAN_POINT('Ctrl Pts',(6.56412410946124,2.46379837162001,15.340783352129));
#157663=CARTESIAN_POINT('Ctrl Pts',(6.57110895151815,2.44502632087634,15.3398759450547));
#157664=CARTESIAN_POINT('Origin',(0.,0.,50.));
#157665=CARTESIAN_POINT('',(6.57110895151813,2.44502632087639,13.3398632123397));
#157666=CARTESIAN_POINT('',(6.57110895151813,2.44502632087639,13.8866662636617));
#157667=CARTESIAN_POINT('',(6.57110895151814,2.44502632087636,50.));
#157668=CARTESIAN_POINT('',(7.01124847424792,0.00462545740675339,15.7735343569468));
#157669=CARTESIAN_POINT('Ctrl Pts',(6.57110895151813,2.44502632087638,13.8866662636617));
#157670=CARTESIAN_POINT('Ctrl Pts',(6.50682343305336,2.61779629976374,13.8950331353048));
#157671=CARTESIAN_POINT('Ctrl Pts',(6.43577420808727,2.78788399297637,13.9034000069479));
#157672=CARTESIAN_POINT('Ctrl Pts',(6.35822606708258,2.95475681611392,13.911766878591));
#157673=CARTESIAN_POINT('Ctrl Pts',(6.28054885164576,3.12190738949285,13.920147676412));
#157674=CARTESIAN_POINT('Ctrl Pts',(6.19635124690865,3.28583210487158,13.928528474233));
#157675=CARTESIAN_POINT('Ctrl Pts',(6.10594367300422,3.44602356704067,13.936909272054));
#157676=CARTESIAN_POINT('Ctrl Pts',(6.04363046942621,3.55643514831101,13.9426857168607));
#157677=CARTESIAN_POINT('Ctrl Pts',(5.97836806944462,3.66507378318171,13.9484621616674));
#157678=CARTESIAN_POINT('Ctrl Pts',(5.91026961679952,3.77178202170227,13.9542386064741));
#157679=CARTESIAN_POINT('Ctrl Pts',(5.81136169478537,3.92676777723572,13.9626284616069));
#157680=CARTESIAN_POINT('Ctrl Pts',(5.70626946418082,4.07799285774942,13.9710183167397));
#157681=CARTESIAN_POINT('Ctrl Pts',(5.5953027819797,4.22495128261501,13.9794081718725));
#157682=CARTESIAN_POINT('Ctrl Pts',(5.48443849827716,4.3717740963065,13.9877902849646));
#157683=CARTESIAN_POINT('Ctrl Pts',(5.36771076659184,4.51433784210089,13.9961723980567));
#157684=CARTESIAN_POINT('Ctrl Pts',(5.24547289992488,4.65216515384543,14.0045545111488));
#157685=CARTESIAN_POINT('Ctrl Pts',(5.12332986393521,4.78988554080735,14.0129301214977));
#157686=CARTESIAN_POINT('Ctrl Pts',(4.99568543274421,4.92287657443647,14.0213057318465));
#157687=CARTESIAN_POINT('Ctrl Pts',(4.86293366035222,5.05069329671812,14.0296813421954));
#157688=CARTESIAN_POINT('Ctrl Pts',(4.73026539079616,5.17842962038364,14.038051684161));
#157689=CARTESIAN_POINT('Ctrl Pts',(4.59249642185694,5.30099789490473,14.0464220261266));
#157690=CARTESIAN_POINT('Ctrl Pts',(4.4500585001271,5.41798910186672,14.0547923680922));
#157691=CARTESIAN_POINT('Ctrl Pts',(4.30768929416612,5.53492386921882,14.0631586719865));
#157692=CARTESIAN_POINT('Ctrl Pts',(4.16065588068454,5.64628672608035,14.0715249758808));
#157693=CARTESIAN_POINT('Ctrl Pts',(4.0094243424729,5.75170783372085,14.0798912797751));
#157694=CARTESIAN_POINT('Ctrl Pts',(3.85823509948301,5.85709945803282,14.0882552438488));
#157695=CARTESIAN_POINT('Ctrl Pts',(3.70285034144664,5.95655245764888,14.0966192079224));
#157696=CARTESIAN_POINT('Ctrl Pts',(3.54376693566202,6.04973904133134,14.104983171996));
#157697=CARTESIAN_POINT('Ctrl Pts',(3.38470801016987,6.14291128514716,14.1133458489946));
#157698=CARTESIAN_POINT('Ctrl Pts',(3.22195185522551,6.2298188695767,14.1217085259932));
#157699=CARTESIAN_POINT('Ctrl Pts',(3.05602221401651,6.31017866545296,14.1300712029917));
#157700=CARTESIAN_POINT('Ctrl Pts',(2.89009598899557,6.39053680686788,14.138433707818));
#157701=CARTESIAN_POINT('Ctrl Pts',(2.72099670395211,6.46434728564727,14.1467962126444));
#157702=CARTESIAN_POINT('Ctrl Pts',(2.54927085689975,6.53137387236879,14.1551587174707));
#157703=CARTESIAN_POINT('Ctrl Pts',(2.37752565553506,6.59840801330253,14.1635221647907));
#157704=CARTESIAN_POINT('Ctrl Pts',(2.20315360830886,6.65865661884118,14.1718856121108));
#157705=CARTESIAN_POINT('Ctrl Pts',(2.02671965925461,6.71193220952736,14.1802490594308));
#157706=CARTESIAN_POINT('Ctrl Pts',(1.85018182093351,6.76523917037834,14.1886174313836));
#157707=CARTESIAN_POINT('Ctrl Pts',(1.6715799693897,6.81156481577389,14.1969858033364));
#157708=CARTESIAN_POINT('Ctrl Pts',(1.49149363213397,6.8507717308201,14.2053541752893));
#157709=CARTESIAN_POINT('Ctrl Pts',(1.31135333630524,6.88999039328269,14.213725054625));
#157710=CARTESIAN_POINT('Ctrl Pts',(1.12972799018647,6.92208600757216,14.2220959339608));
#157711=CARTESIAN_POINT('Ctrl Pts',(0.947206404613266,6.94697247652239,
14.2304668132965));
#157712=CARTESIAN_POINT('Ctrl Pts',(0.764530170474379,6.97188003150865,
14.2388447851878));
#157713=CARTESIAN_POINT('Ctrl Pts',(0.58095650614245,6.98956619671621,14.2472227570791));
#157714=CARTESIAN_POINT('Ctrl Pts',(0.397079586526947,6.99999674031807,
14.2556007289704));
#157715=CARTESIAN_POINT('Ctrl Pts',(0.280224306798269,7.00662543571315,
14.2609249983293));
#157716=CARTESIAN_POINT('Ctrl Pts',(0.163246613133867,7.01032484772516,
14.2662492676882));
#157717=CARTESIAN_POINT('Ctrl Pts',(0.0462988965612011,7.01109713059784,
14.2715735370471));
#157718=CARTESIAN_POINT('Ctrl Pts',(-0.126408397416553,7.01223763072076,
14.2794363682364));
#157719=CARTESIAN_POINT('Ctrl Pts',(-0.299409378148574,7.0069939243274,
14.2872991994256));
#157720=CARTESIAN_POINT('Ctrl Pts',(-0.472173043189139,6.99533267113048,
14.2951620306149));
#157721=CARTESIAN_POINT('Ctrl Pts',(-0.644803962157695,6.98368037806738,
14.3030188202563));
#157722=CARTESIAN_POINT('Ctrl Pts',(-0.817197550108498,6.96562036978901,
14.3108756098977));
#157723=CARTESIAN_POINT('Ctrl Pts',(-0.98882113102714,6.94117132286289,
14.3187323995391));
#157724=CARTESIAN_POINT('Ctrl Pts',(-1.16034792437023,6.91673606404191,
14.326584758323));
#157725=CARTESIAN_POINT('Ctrl Pts',(-1.33110519821472,6.88591898759986,
14.334437117107));
#157726=CARTESIAN_POINT('Ctrl Pts',(-1.50056398817736,6.84879071660722,
14.3422894758909));
#157727=CARTESIAN_POINT('Ctrl Pts',(-1.66998276694233,6.81167121203261,
14.3501399806413));
#157728=CARTESIAN_POINT('Ctrl Pts',(-1.83810329811438,6.76824355199754,
14.3579904853917));
#157729=CARTESIAN_POINT('Ctrl Pts',(-2.00440548711609,6.71862971190696,
14.3658409901422));
#157730=CARTESIAN_POINT('Ctrl Pts',(-2.17068092333709,6.66902385311951,
14.3736902319938));
#157731=CARTESIAN_POINT('Ctrl Pts',(-2.33513823495106,6.6132339073058,14.3815394738454));
#157732=CARTESIAN_POINT('Ctrl Pts',(-2.49727165792624,6.5514319678234,14.389388715697));
#157733=CARTESIAN_POINT('Ctrl Pts',(-2.65945970682528,6.48960920605785,
14.3972406021119));
#157734=CARTESIAN_POINT('Ctrl Pts',(-2.81932194634441,6.42177054070639,
14.4050924885267));
#157735=CARTESIAN_POINT('Ctrl Pts',(-2.97637161426586,6.34813662237136,
14.4129443749416));
#157736=CARTESIAN_POINT('Ctrl Pts',(-3.09169123066252,6.29406815264098,
14.4187099174055));
#157737=CARTESIAN_POINT('Ctrl Pts',(-3.20549475449589,6.23687602814435,
14.4244754598695));
#157738=CARTESIAN_POINT('Ctrl Pts',(-3.31759780661679,6.17666344849964,
14.4302410023335));
#157739=CARTESIAN_POINT('Ctrl Pts',(-3.50533193478854,6.07582804811839,
14.4398963066934));
#157740=CARTESIAN_POINT('Ctrl Pts',(-3.68820103973575,5.9665727244977,14.4495516110534));
#157741=CARTESIAN_POINT('Ctrl Pts',(-3.86555333472591,5.84936953687228,
14.4592069154133));
#157742=CARTESIAN_POINT('Ctrl Pts',(-4.0438881281576,5.73151706557566,14.468915708348));
#157743=CARTESIAN_POINT('Ctrl Pts',(-4.21664480894793,5.60562849866783,
14.4786245012827));
#157744=CARTESIAN_POINT('Ctrl Pts',(-4.38319836816824,5.47222063040109,
14.4883332942174));
#157745=CARTESIAN_POINT('Ctrl Pts',(-4.55055339725869,5.3381707921437,14.4980888066882));
#157746=CARTESIAN_POINT('Ctrl Pts',(-4.71164544247583,5.1965291571514,14.5078443191589));
#157747=CARTESIAN_POINT('Ctrl Pts',(-4.86587855491735,5.04785622331852,
14.5175998316297));
#157748=CARTESIAN_POINT('Ctrl Pts',(-5.02026438186789,4.89903608040883,
14.5273650035586));
#157749=CARTESIAN_POINT('Ctrl Pts',(-5.16777767184748,4.743170747589,14.5371301754875));
#157750=CARTESIAN_POINT('Ctrl Pts',(-5.30785902364905,4.5808579051928,14.5468953474164));
#157751=CARTESIAN_POINT('Ctrl Pts',(-5.447749377705,4.41876637267536,14.5566472047549));
#157752=CARTESIAN_POINT('Ctrl Pts',(-5.58022802160503,4.25024492945157,
14.5663990620934));
#157753=CARTESIAN_POINT('Ctrl Pts',(-5.70477630390394,4.07592368487391,
14.5761509194319));
#157754=CARTESIAN_POINT('Ctrl Pts',(-5.75908837520181,3.99990699729316,
14.5804034354945));
#157755=CARTESIAN_POINT('Ctrl Pts',(-5.8118929119634,3.9227878698017,14.5846559515572));
#157756=CARTESIAN_POINT('Ctrl Pts',(-5.86314922750659,3.84462061827808,
14.5889084676199));
#157757=CARTESIAN_POINT('Ctrl Pts',(-5.95997292291815,3.69696189422669,
14.5969415132187));
#157758=CARTESIAN_POINT('Ctrl Pts',(-6.05131610743908,3.54548896452417,
14.6049745588175));
#157759=CARTESIAN_POINT('Ctrl Pts',(-6.1368631875334,3.39065432918153,14.6130076044163));
#157760=CARTESIAN_POINT('Ctrl Pts',(-6.22235527467099,3.23591922750376,
14.6210354860642));
#157761=CARTESIAN_POINT('Ctrl Pts',(-6.30205849745976,3.07782704129155,
14.629063367712));
#157762=CARTESIAN_POINT('Ctrl Pts',(-6.37570092852195,2.9168586240242,14.6370912493598));
#157763=CARTESIAN_POINT('Ctrl Pts',(-6.44931010930046,2.75596288558427,
14.6451155063399));
#157764=CARTESIAN_POINT('Ctrl Pts',(-6.51686379486667,2.59219383449292,
14.65313976332));
#157765=CARTESIAN_POINT('Ctrl Pts',(-6.57813634697585,2.42605621598001,
14.6611640203001));
#157766=CARTESIAN_POINT('Ctrl Pts',(-6.63940149060938,2.2599386851974,14.6691873070659));
#157767=CARTESIAN_POINT('Ctrl Pts',(-6.69438687948556,2.09145349847771,
14.6772105938316));
#157768=CARTESIAN_POINT('Ctrl Pts',(-6.74291524803168,1.9211248060347,14.6852338805973));
#157769=CARTESIAN_POINT('Ctrl Pts',(-6.79143964011083,1.75081007050885,
14.6932565099262));
#157770=CARTESIAN_POINT('Ctrl Pts',(-6.83350796916813,1.57865248386803,
14.7012791392551));
#157771=CARTESIAN_POINT('Ctrl Pts',(-6.86899310809289,1.40519046519408,
14.709301768584));
#157772=CARTESIAN_POINT('Ctrl Pts',(-6.90449158690372,1.2316632371498,14.7173274138504));
#157773=CARTESIAN_POINT('Ctrl Pts',(-6.93340186115936,1.05683095744479,
14.7253530591169));
#157774=CARTESIAN_POINT('Ctrl Pts',(-6.95564803755869,0.881241703567202,
14.7333787043833));
#157775=CARTESIAN_POINT('Ctrl Pts',(-6.96876573877862,0.777703579601446,
14.738111113891));
#157776=CARTESIAN_POINT('Ctrl Pts',(-6.97956731078757,0.673902400168856,
14.7428435233987));
#157777=CARTESIAN_POINT('Ctrl Pts',(-6.98804566086226,0.56995122967162,
14.7475759329064));
#157778=CARTESIAN_POINT('Ctrl Pts',(-7.00368598321158,0.37818870502436,
14.756305981741));
#157779=CARTESIAN_POINT('Ctrl Pts',(-7.01142552498665,0.185819746789846,
14.7650360305757));
#157780=CARTESIAN_POINT('Ctrl Pts',(-7.01124697880516,-0.00650881674804643,
14.7737660794103));
#157781=CARTESIAN_POINT('Ctrl Pts',(-7.01106838099683,-0.198892992329736,
14.7824986525495));
#157782=CARTESIAN_POINT('Ctrl Pts',(-7.00296712547059,-0.39123647595842,
14.7912312256886));
#157783=CARTESIAN_POINT('Ctrl Pts',(-6.98697803043219,-0.582893270468943,
14.7999637988278));
#157784=CARTESIAN_POINT('Ctrl Pts',(-6.97076178477534,-0.777272855687614,
14.8088204321082));
#157785=CARTESIAN_POINT('Ctrl Pts',(-6.94643189688725,-0.970945803216331,
14.8176770653886));
#157786=CARTESIAN_POINT('Ctrl Pts',(-6.91407911602979,-1.1632439725959,
14.826533698669));
#157787=CARTESIAN_POINT('Ctrl Pts',(-6.88215921326288,-1.35296920505414,
14.8352718307758));
#157788=CARTESIAN_POINT('Ctrl Pts',(-6.84242984471826,-1.54135594971283,
14.8440099628825));
#157789=CARTESIAN_POINT('Ctrl Pts',(-6.79502978745293,-1.72777219277527,
14.8527480949893));
#157790=CARTESIAN_POINT('Ctrl Pts',(-6.74666551454929,-1.91798052950098,
14.8616639788565));
#157791=CARTESIAN_POINT('Ctrl Pts',(-6.69031520397961,-2.10613704971201,
14.8705798627238));
#157792=CARTESIAN_POINT('Ctrl Pts',(-6.62618024995159,-2.2915850099116,
14.879495746591));
#157793=CARTESIAN_POINT('Ctrl Pts',(-6.56204529592356,-2.4770329701112,
14.8884116304583));
#157794=CARTESIAN_POINT('Ctrl Pts',(-6.49012580302771,-2.65977208648433,
14.8973275143255));
#157795=CARTESIAN_POINT('Ctrl Pts',(-6.41067628819488,-2.83916468181681,
14.9062433981928));
#157796=CARTESIAN_POINT('Ctrl Pts',(-6.33278797640538,-3.01503216731855,
14.914984082689));
#157797=CARTESIAN_POINT('Ctrl Pts',(-6.24765455686902,-3.18770210982015,
14.9237247671852));
#157798=CARTESIAN_POINT('Ctrl Pts',(-6.15555931687582,-3.35659292421994,
14.9324654516814));
#157799=CARTESIAN_POINT('Ctrl Pts',(-6.06348064634596,-3.525453352357,14.9412045635833));
#157800=CARTESIAN_POINT('Ctrl Pts',(-5.96444278782203,-3.69053576996705,
14.9499436754852));
#157801=CARTESIAN_POINT('Ctrl Pts',(-5.85877490313842,-3.85128331817531,
14.9586827873871));
#157802=CARTESIAN_POINT('Ctrl Pts',(-5.75173793892643,-4.01411358222622,
14.9675351270615));
#157803=CARTESIAN_POINT('Ctrl Pts',(-5.63789808562857,-4.17249561437347,
14.9763874667358));
#157804=CARTESIAN_POINT('Ctrl Pts',(-5.51764347797401,-4.32587991193363,
14.9852398064101));
#157805=CARTESIAN_POINT('Ctrl Pts',(-5.39898786138609,-4.47722470243168,
14.9939744390599));
#157806=CARTESIAN_POINT('Ctrl Pts',(-5.27408720562648,-4.62370362732956,
15.0027090717097));
#157807=CARTESIAN_POINT('Ctrl Pts',(-5.14335623431666,-4.76482037535686,
15.0114437043594));
#157808=CARTESIAN_POINT('Ctrl Pts',(-5.0099826870218,-4.90878963588132,
15.0203548975461));
#157809=CARTESIAN_POINT('Ctrl Pts',(-4.87054078900852,-5.04717740252297,
15.0292660907327));
#157810=CARTESIAN_POINT('Ctrl Pts',(-4.72551276559025,-5.17949376529634,
15.0381772839193));
#157811=CARTESIAN_POINT('Ctrl Pts',(-4.58048474217196,-5.31181012806972,
15.0470884771059));
#157812=CARTESIAN_POINT('Ctrl Pts',(-4.42987080820157,-5.43805487271456,
15.0559996702926));
#157813=CARTESIAN_POINT('Ctrl Pts',(-4.27419237401628,-5.55777888300723,
15.0649108634792));
#157814=CARTESIAN_POINT('Ctrl Pts',(-4.1339841088214,-5.66560560848246,
15.0729365283316));
#157815=CARTESIAN_POINT('Ctrl Pts',(-3.98960312497885,-5.76819231375616,
15.0809621931839));
#157816=CARTESIAN_POINT('Ctrl Pts',(-3.84148776815999,-5.86520232298743,
15.0889878580363));
#157817=CARTESIAN_POINT('Ctrl Pts',(-3.69341941952229,-5.96218154362132,
15.0970109757395));
#157818=CARTESIAN_POINT('Ctrl Pts',(-3.54161936381376,-6.05358739132405,
15.1050340934427));
#157819=CARTESIAN_POINT('Ctrl Pts',(-3.38655599559884,-6.13912575625989,
15.1130572111459));
#157820=CARTESIAN_POINT('Ctrl Pts',(-3.23151218223137,-6.2246533340595,
15.1210793170638));
#157821=CARTESIAN_POINT('Ctrl Pts',(-3.07320619725014,-6.30431472647784,
15.1291014229817));
#157822=CARTESIAN_POINT('Ctrl Pts',(-2.91213211645322,-6.37786116961021,
15.1371235288995));
#157823=CARTESIAN_POINT('Ctrl Pts',(-2.75099817998405,-6.45143494284916,
15.145148615859));
#157824=CARTESIAN_POINT('Ctrl Pts',(-2.58709442533485,-6.51888907226617,
15.1531737028186));
#157825=CARTESIAN_POINT('Ctrl Pts',(-2.42093645748432,-6.58002228197772,
15.1611987897781));
#157826=CARTESIAN_POINT('Ctrl Pts',(-2.25474576565336,-6.64116753156906,
15.1692254572383));
#157827=CARTESIAN_POINT('Ctrl Pts',(-2.08630032324651,-6.69598926315759,
15.1772521246985));
#157828=CARTESIAN_POINT('Ctrl Pts',(-1.91613187089708,-6.74433578759484,
15.1852787921588));
#157829=CARTESIAN_POINT('Ctrl Pts',(-1.74582680791346,-6.79272112445162,
15.1933119033994));
#157830=CARTESIAN_POINT('Ctrl Pts',(-1.57379632742428,-6.83462078068159,
15.20134501464));
#157831=CARTESIAN_POINT('Ctrl Pts',(-1.40058397055772,-6.86993385003937,
15.2093781258806));
#157832=CARTESIAN_POINT('Ctrl Pts',(-1.29852095760964,-6.89074159332224,
15.2141115268423));
#157833=CARTESIAN_POINT('Ctrl Pts',(-1.19604776992183,-6.90926345064929,
15.2188449278039));
#157834=CARTESIAN_POINT('Ctrl Pts',(-1.09327653932694,-6.92548720098863,
15.2235783287656));
#157835=CARTESIAN_POINT('Ctrl Pts',(-0.881564605849781,-6.95890863160409,
15.2333292820597));
#157836=CARTESIAN_POINT('Ctrl Pts',(-0.668462914413408,-6.98259511557152,
15.2430802353539));
#157837=CARTESIAN_POINT('Ctrl Pts',(-0.454786202923141,-6.99648455098207,
15.2528311886481));
#157838=CARTESIAN_POINT('Ctrl Pts',(-0.240801650048419,-7.01039399672971,
15.2625961900196));
#157839=CARTESIAN_POINT('Ctrl Pts',(-0.0262404585796727,-7.01447815828849,
15.2723611913911));
#157840=CARTESIAN_POINT('Ctrl Pts',(0.188078825273883,-7.00872691135727,
15.2821261927625));
#157841=CARTESIAN_POINT('Ctrl Pts',(0.402040883290473,-7.00298525056296,
15.2918749179002));
#157842=CARTESIAN_POINT('Ctrl Pts',(0.615761801649108,-6.98744094642008,
15.3016236430378));
#157843=CARTESIAN_POINT('Ctrl Pts',(0.828427412422822,-6.96213577753597,
15.3113723681754));
#157844=CARTESIAN_POINT('Ctrl Pts',(1.04050933855961,-6.93690006152796,
15.3210943368427));
#157845=CARTESIAN_POINT('Ctrl Pts',(1.25154169966688,-6.90195696693144,
15.33081630551));
#157846=CARTESIAN_POINT('Ctrl Pts',(1.46071789640201,-6.85739963759084,
15.3405382741774));
#157847=CARTESIAN_POINT('Ctrl Pts',(1.66851002887363,-6.81313713246149,
15.3501959151171));
#157848=CARTESIAN_POINT('Ctrl Pts',(1.87447042763027,-6.75938718329948,
15.3598535560568));
#157849=CARTESIAN_POINT('Ctrl Pts',(2.07780996499439,-6.69629243028334,
15.3695111969966));
#157850=CARTESIAN_POINT('Ctrl Pts',(2.16718469221616,-6.66856011411384,
15.3737560626818));
#157851=CARTESIAN_POINT('Ctrl Pts',(2.25605311893811,-6.63902314187182,
15.3780009283669));
#157852=CARTESIAN_POINT('Ctrl Pts',(2.34434837785144,-6.60769681854164,
15.3822457940521));
#157853=CARTESIAN_POINT('Ctrl Pts',(2.50767059260672,-6.5497516404042,15.390097641066));
#157854=CARTESIAN_POINT('Ctrl Pts',(2.66896336522462,-6.48570442701368,
15.3979494880799));
#157855=CARTESIAN_POINT('Ctrl Pts',(2.82772286466298,-6.41573144412718,
15.4058013350938));
#157856=CARTESIAN_POINT('Ctrl Pts',(2.9864373411913,-6.3457783050127,15.4136509553874));
#157857=CARTESIAN_POINT('Ctrl Pts',(3.14261962487296,-6.26990289290201,
15.421500575681));
#157858=CARTESIAN_POINT('Ctrl Pts',(3.2957851434009,-6.18832989190443,15.4293501959745));
#157859=CARTESIAN_POINT('Ctrl Pts',(3.44893843362136,-6.10676340346756,
15.4371991895764));
#157860=CARTESIAN_POINT('Ctrl Pts',(3.59907510181574,-6.01950041166084,
15.4450481831782));
#157861=CARTESIAN_POINT('Ctrl Pts',(3.74573473808917,-5.9268117765264,15.45289717678));
#157862=CARTESIAN_POINT('Ctrl Pts',(3.89246862384126,-5.83407621585055,
15.4607501440974));
#157863=CARTESIAN_POINT('Ctrl Pts',(4.03572163758295,-5.7359097275759,15.4686031114148));
#157864=CARTESIAN_POINT('Ctrl Pts',(4.17506168013776,-5.63262696523969,
15.4764560787322));
#157865=CARTESIAN_POINT('Ctrl Pts',(4.31443711038153,-5.52931797255217,
15.4843110404394));
#157866=CARTESIAN_POINT('Ctrl Pts',(4.44989729178476,-5.42089035557746,
15.4921660021467));
#157867=CARTESIAN_POINT('Ctrl Pts',(4.581043381571,-5.30769894574519,15.5000209638539));
#157868=CARTESIAN_POINT('Ctrl Pts',(4.71231964481388,-5.19439518397696,
15.5078837222672));
#157869=CARTESIAN_POINT('Ctrl Pts',(4.83927298479952,-5.07631844508788,
15.5157464806806));
#157870=CARTESIAN_POINT('Ctrl Pts',(4.96154118034644,-4.95386068417618,
15.5236092390939));
#157871=CARTESIAN_POINT('Ctrl Pts',(5.05123537415605,-4.86402742793507,
15.5293772458421));
#157872=CARTESIAN_POINT('Ctrl Pts',(5.1384090411959,-4.77183730484334,15.5351452525903));
#157873=CARTESIAN_POINT('Ctrl Pts',(5.22293326955531,-4.67745599918079,
15.5409132593385));
#157874=CARTESIAN_POINT('Ctrl Pts',(5.3449247988286,-4.54123801723568,15.5492380672394));
#157875=CARTESIAN_POINT('Ctrl Pts',(5.46167769980065,-4.40014018445398,
15.5575628751404));
#157876=CARTESIAN_POINT('Ctrl Pts',(5.5727950877626,-4.25459533590553,15.5658876830414));
#157877=CARTESIAN_POINT('Ctrl Pts',(5.68827901390729,-4.10333106621026,
15.5745396277859));
#157878=CARTESIAN_POINT('Ctrl Pts',(5.79767526457732,-3.94726343442159,
15.5831915725305));
#157879=CARTESIAN_POINT('Ctrl Pts',(5.90058275068057,-3.78691824111254,
15.591843517275));
#157880=CARTESIAN_POINT('Ctrl Pts',(5.99945449149194,-3.63286134016663,
15.6001561568185));
#157881=CARTESIAN_POINT('Ctrl Pts',(6.09233650382568,-3.4748563019137,15.6084687963619));
#157882=CARTESIAN_POINT('Ctrl Pts',(6.17891585027054,-3.31340089300639,
15.6167814359053));
#157883=CARTESIAN_POINT('Ctrl Pts',(6.2654621520297,-3.15200710668529,15.6250909027688));
#157884=CARTESIAN_POINT('Ctrl Pts',(6.34571042458889,-2.98716586962572,
15.6334003696322));
#157885=CARTESIAN_POINT('Ctrl Pts',(6.41939286279622,-2.81940097105413,
15.6417098364956));
#157886=CARTESIAN_POINT('Ctrl Pts',(6.49305797317401,-2.65167552559558,
15.6500173492296));
#157887=CARTESIAN_POINT('Ctrl Pts',(6.5601601930512,-2.48102809613213,15.6583248619635));
#157888=CARTESIAN_POINT('Ctrl Pts',(6.62047905083359,-2.30800426775462,
15.6666323746975));
#157889=CARTESIAN_POINT('Ctrl Pts',(6.68079255755789,-2.13499578881493,
15.6749391504482));
#157890=CARTESIAN_POINT('Ctrl Pts',(6.73432379269518,-1.95961164803175,
15.683245926199));
#157891=CARTESIAN_POINT('Ctrl Pts',(6.78090141494034,-1.78241481237116,
15.6915527019498));
#157892=CARTESIAN_POINT('Ctrl Pts',(6.82749179049423,-1.60516945886351,
15.6998617521592));
#157893=CARTESIAN_POINT('Ctrl Pts',(6.86712466197352,-1.42611074264509,
15.7081708023686));
#157894=CARTESIAN_POINT('Ctrl Pts',(6.89967912188337,-1.2458148247419,15.716479852578));
#157895=CARTESIAN_POINT('Ctrl Pts',(6.93223858515478,-1.06549119679023,
15.7247901798224));
#157896=CARTESIAN_POINT('Ctrl Pts',(6.95771741333767,-0.883930318812309,
15.7331005070667));
#157897=CARTESIAN_POINT('Ctrl Pts',(6.97604620325943,-0.701716418854346,
15.7414108343111));
#157898=CARTESIAN_POINT('Ctrl Pts',(6.99438495527861,-0.519403481664143,
15.7497256783997));
#157899=CARTESIAN_POINT('Ctrl Pts',(7.00556587828336,-0.336437147572331,
15.7580405224883));
#157900=CARTESIAN_POINT('Ctrl Pts',(7.00957155226553,-0.15340539811163,
15.7663553665769));
#157901=CARTESIAN_POINT('Ctrl Pts',(7.01072437784235,-0.100729198529165,
15.7687483633547));
#157902=CARTESIAN_POINT('Ctrl Pts',(7.01128322367289,-0.0480475808299134,
15.7711413601326));
#157903=CARTESIAN_POINT('Ctrl Pts',(7.01124847424845,0.00462545660806772,
15.7735343569105));
#157904=CARTESIAN_POINT('Ctrl Pts',(7.01124847424792,0.00462545740675822,
15.7735343569468));
#157905=CARTESIAN_POINT('Ctrl Pts',(7.01109761289101,0.233300454373922,
15.7839233255262));
#157906=CARTESIAN_POINT('Ctrl Pts',(6.999755421247,0.461583810249137,15.7943122941056));
#157907=CARTESIAN_POINT('Ctrl Pts',(6.97735941040693,0.688536288445155,
15.804701262685));
#157908=CARTESIAN_POINT('Ctrl Pts',(6.95466206942866,0.918542329264845,
15.8152300110386));
#157909=CARTESIAN_POINT('Ctrl Pts',(6.9206114557263,1.14718165363006,15.8257587593922));
#157910=CARTESIAN_POINT('Ctrl Pts',(6.87540077452587,1.3734958143908,15.8362875077458));
#157911=CARTESIAN_POINT('Ctrl Pts',(6.84396755419799,1.5308432086266,15.8436077351343));
#157912=CARTESIAN_POINT('Ctrl Pts',(6.80714072868335,1.68706705157194,15.8509279625228));
#157913=CARTESIAN_POINT('Ctrl Pts',(6.76499934449847,1.84184973095942,15.8582481899113));
#157914=CARTESIAN_POINT('Ctrl Pts',(6.71673751112402,2.01911243901562,15.8666315783861));
#157915=CARTESIAN_POINT('Ctrl Pts',(6.66144805038815,2.1946837817458,15.8750149668608));
#157916=CARTESIAN_POINT('Ctrl Pts',(6.59926293776704,2.36798548152523,15.8833983553356));
#157917=CARTESIAN_POINT('Ctrl Pts',(6.59003002008751,2.39371640425486,15.8846430766588));
#157918=CARTESIAN_POINT('Ctrl Pts',(6.58064518186825,2.41939730899936,15.885887797982));
#157919=CARTESIAN_POINT('Ctrl Pts',(6.57110895151814,2.44502632087636,15.8871325193051));
#157920=CARTESIAN_POINT('',(7.01124961619472,-0.00231989425524781,15.2264656430654));
#157921=CARTESIAN_POINT('Ctrl Pts',(6.57110895151815,2.44502632087634,15.3398759450547));
#157922=CARTESIAN_POINT('Ctrl Pts',(6.63285964731569,2.27906878232018,15.3318538569744));
#157923=CARTESIAN_POINT('Ctrl Pts',(6.68832544267615,2.11075369790805,15.3238317688941));
#157924=CARTESIAN_POINT('Ctrl Pts',(6.7373341885473,1.9406067593234,15.3158096808138));
#157925=CARTESIAN_POINT('Ctrl Pts',(6.78636192543487,1.7703938883578,15.3077844841535));
#157926=CARTESIAN_POINT('Ctrl Pts',(6.82892751104394,1.59834809721087,15.2997592874933));
#157927=CARTESIAN_POINT('Ctrl Pts',(6.86490897642211,1.42500923082597,15.291734090833));
#157928=CARTESIAN_POINT('Ctrl Pts',(6.90089822560439,1.25163286636344,15.2837071580967));
#157929=CARTESIAN_POINT('Ctrl Pts',(6.93030045155082,1.07696323009593,15.2756802253604));
#157930=CARTESIAN_POINT('Ctrl Pts',(6.95304512735804,0.901548678343343,
15.2676532926241));
#157931=CARTESIAN_POINT('Ctrl Pts',(6.97580772661208,0.725995894970501,
15.2596200344382));
#157932=CARTESIAN_POINT('Ctrl Pts',(6.99190226173688,0.54969738842236,15.2515867762522));
#157933=CARTESIAN_POINT('Ctrl Pts',(7.00131017838675,0.373205504404982,
15.2435535180663));
#157934=CARTESIAN_POINT('Ctrl Pts',(7.00579043828701,0.289156129807543,
15.2397279012099));
#157935=CARTESIAN_POINT('Ctrl Pts',(7.0087550187039,0.205062904514265,15.2359022843535));
#157936=CARTESIAN_POINT('Ctrl Pts',(7.01020606780222,0.120985327412108,
15.2320766674971));
#157937=CARTESIAN_POINT('Ctrl Pts',(7.01091548471569,0.079879857370017,
15.230206326028));
#157938=CARTESIAN_POINT('Ctrl Pts',(7.01126321422435,0.0387764624478537,
15.2283359845588));
#157939=CARTESIAN_POINT('Ctrl Pts',(7.0112496161949,-0.0023198937239668,
15.2264656430896));
#157940=CARTESIAN_POINT('Ctrl Pts',(7.01124961619472,-0.00231989425526735,
15.2264656430654));
#157941=CARTESIAN_POINT('Ctrl Pts',(7.01117905493752,-0.215572108811857,
15.2167602945277));
#157942=CARTESIAN_POINT('Ctrl Pts',(7.00137487997501,-0.428703660272864,
15.2070549459899));
#157943=CARTESIAN_POINT('Ctrl Pts',(6.98189533488068,-0.640908804176824,
15.1973495974522));
#157944=CARTESIAN_POINT('Ctrl Pts',(6.96239982346777,-0.85328788104056,
15.1876362939706));
#157945=CARTESIAN_POINT('Ctrl Pts',(6.93321308995598,-1.06473897836569,
15.1779229904891));
#157946=CARTESIAN_POINT('Ctrl Pts',(6.89444527559506,-1.27446102503178,
15.1682096870075));
#157947=CARTESIAN_POINT('Ctrl Pts',(6.85576051130448,-1.48373379615792,
15.1585171917802));
#157948=CARTESIAN_POINT('Ctrl Pts',(6.80753568172825,-1.69128486360751,
15.1488246965529));
#157949=CARTESIAN_POINT('Ctrl Pts',(6.7499315107308,-1.89632570064939,15.1391322013256));
#157950=CARTESIAN_POINT('Ctrl Pts',(6.69249133156878,-2.10078281219675,
15.1294672994141));
#157951=CARTESIAN_POINT('Ctrl Pts',(6.62572512478436,-2.30274390398725,
15.1198023975026));
#157952=CARTESIAN_POINT('Ctrl Pts',(6.54984332309524,-2.50143538901262,
15.1101374955911));
#157953=CARTESIAN_POINT('Ctrl Pts',(6.47443174862118,-2.69889561513824,
15.1005324855088));
#157954=CARTESIAN_POINT('Ctrl Pts',(6.39001719368613,-2.89312656098337,
15.0909274754265));
#157955=CARTESIAN_POINT('Ctrl Pts',(6.29685686916809,-3.0833780390524,15.0813224653443));
#157956=CARTESIAN_POINT('Ctrl Pts',(6.27127292373383,-3.13562542503873,
15.0786847109664));
#157957=CARTESIAN_POINT('Ctrl Pts',(6.24502968962702,-3.18757274566128,
15.0760469565886));
#157958=CARTESIAN_POINT('Ctrl Pts',(6.21813317189115,-3.239204596676,15.0734092022107));
#157959=CARTESIAN_POINT('Ctrl Pts',(6.13806986340353,-3.39289798019031,
15.0655573551968));
#157960=CARTESIAN_POINT('Ctrl Pts',(6.05224545515072,-3.54373423243102,
15.0577055081829));
#157961=CARTESIAN_POINT('Ctrl Pts',(5.96090446899768,-3.69123888064475,
15.049853661169));
#157962=CARTESIAN_POINT('Ctrl Pts',(5.86958938640981,-3.83870169773283,
15.0420040408754));
#157963=CARTESIAN_POINT('Ctrl Pts',(5.77276103852661,-3.98283446619701,
15.0341544205818));
#157964=CARTESIAN_POINT('Ctrl Pts',(5.67070922212415,-4.12318850898382,
15.0263048002882));
#157965=CARTESIAN_POINT('Ctrl Pts',(5.56866555325388,-4.26353134629557,
15.0184558066864));
#157966=CARTESIAN_POINT('Ctrl Pts',(5.46139947098912,-4.40009575040983,
15.0106068130846));
#157967=CARTESIAN_POINT('Ctrl Pts',(5.34924314538045,-4.5324633847501,15.0027578194828));
#157968=CARTESIAN_POINT('Ctrl Pts',(5.23703003830839,-4.66489803294752,
14.9949048521654));
#157969=CARTESIAN_POINT('Ctrl Pts',(5.1199219880671,-4.79313137469256,14.987051884848));
#157970=CARTESIAN_POINT('Ctrl Pts',(4.99829060257687,-4.9167791911669,14.9791989175306));
#157971=CARTESIAN_POINT('Ctrl Pts',(4.87662832680158,-5.040458410032,14.9713439558233));
#157972=CARTESIAN_POINT('Ctrl Pts',(4.75044070460538,-5.15954952167867,
14.963488994116));
#157973=CARTESIAN_POINT('Ctrl Pts',(4.62013451442953,-5.27370682073596,
14.9556340324088));
#157974=CARTESIAN_POINT('Ctrl Pts',(4.4896989844677,-5.38797743045493,14.9477712739954));
#157975=CARTESIAN_POINT('Ctrl Pts',(4.35513701763923,-5.49730420614854,
14.9399085155821));
#157976=CARTESIAN_POINT('Ctrl Pts',(4.21688707096991,-5.60138286436366,
14.9320457571687));
#157977=CARTESIAN_POINT('Ctrl Pts',(4.1154688938625,-5.67773347459001,14.9262777504206));
#157978=CARTESIAN_POINT('Ctrl Pts',(4.01206669416725,-5.75126069484699,
14.9205097436725));
#157979=CARTESIAN_POINT('Ctrl Pts',(3.9068624521206,-5.82185986972464,14.9147417369243));
#157980=CARTESIAN_POINT('Ctrl Pts',(3.75405262227269,-5.92440561969234,
14.9063636704833));
#157981=CARTESIAN_POINT('Ctrl Pts',(3.59710154621272,-6.02099952136897,
14.8979856040423));
#157982=CARTESIAN_POINT('Ctrl Pts',(3.43650094856787,-6.11130818998618,
14.8896075376013));
#157983=CARTESIAN_POINT('Ctrl Pts',(3.27601016770342,-6.20155510660884,
14.8812351999825));
#157984=CARTESIAN_POINT('Ctrl Pts',(3.11187512615867,-6.28552519804157,
14.8728628623638));
#157985=CARTESIAN_POINT('Ctrl Pts',(2.94461521837787,-6.36292918223969,
14.8644905247451));
#157986=CARTESIAN_POINT('Ctrl Pts',(2.77744515215865,-6.44029158985855,
14.8561226842225));
#157987=CARTESIAN_POINT('Ctrl Pts',(2.60715386409951,-6.51109478480129,
14.8477548436999));
#157988=CARTESIAN_POINT('Ctrl Pts',(2.43428437051971,-6.57509590545594,
14.8393870031773));
#157989=CARTESIAN_POINT('Ctrl Pts',(2.26148240749429,-6.63907202441093,
14.8310224315074));
#157990=CARTESIAN_POINT('Ctrl Pts',(2.08610455518346,-6.69625125394265,
14.8226578598375));
#157991=CARTESIAN_POINT('Ctrl Pts',(1.90871321004138,-6.74643909364885,
14.8142932881676));
#157992=CARTESIAN_POINT('Ctrl Pts',(1.73136519607964,-6.79661467402903,
14.805930759702));
#157993=CARTESIAN_POINT('Ctrl Pts',(1.55200498623125,-6.83980218132074,
14.7975682312364));
#157994=CARTESIAN_POINT('Ctrl Pts',(1.37120995672951,-6.8758570241873,14.7892057027708));
#157995=CARTESIAN_POINT('Ctrl Pts',(1.19040049921894,-6.91191474434309,
14.7808425069493));
#157996=CARTESIAN_POINT('Ctrl Pts',(1.00815631443533,-6.94083859267118,
14.7724793111278));
#157997=CARTESIAN_POINT('Ctrl Pts',(0.825065550162284,-6.96253498378539,
14.7641161153063));
#157998=CARTESIAN_POINT('Ctrl Pts',(0.641962299466072,-6.98423285454999,
14.7557523491316));
#157999=CARTESIAN_POINT('Ctrl Pts',(0.458012680667262,-6.9987022463424,
14.7473885829569));
#158000=CARTESIAN_POINT('Ctrl Pts',(0.273810730400995,-7.00590138714622,
14.7390248167822));
#158001=CARTESIAN_POINT('Ctrl Pts',(0.0895716594778335,-7.01310197873182,
14.7306593651286));
#158002=CARTESIAN_POINT('Ctrl Pts',(-0.0949195157738741,-7.01302938503274,
14.722293913475));
#158003=CARTESIAN_POINT('Ctrl Pts',(-0.279067550926409,-7.00569396023834,
14.7139284618214));
#158004=CARTESIAN_POINT('Ctrl Pts',(-0.463277256893581,-6.99835607882461,
14.7055602085946));
#158005=CARTESIAN_POINT('Ctrl Pts',(-0.647143265221654,-6.9837505293066,
14.6971919553677));
#158006=CARTESIAN_POINT('Ctrl Pts',(-0.830073813274393,-6.96193967418679,
14.6888237021408));
#158007=CARTESIAN_POINT('Ctrl Pts',(-1.01317396404313,-6.94010859729263,
14.6804476903494));
#158008=CARTESIAN_POINT('Ctrl Pts',(-1.19533659459348,-6.91105890443767,
14.6720716785579));
#158009=CARTESIAN_POINT('Ctrl Pts',(-1.37597728166385,-6.87490458718119,
14.6636956667664));
#158010=CARTESIAN_POINT('Ctrl Pts',(-1.55670655715935,-6.83873253940077,
14.6553155472753));
#158011=CARTESIAN_POINT('Ctrl Pts',(-1.73591207984935,-6.79544898995672,
14.6469354277841));
#158012=CARTESIAN_POINT('Ctrl Pts',(-1.91302236952525,-6.745218452815,14.6385553082929));
#158013=CARTESIAN_POINT('Ctrl Pts',(-2.0903350301421,-6.69493052092178,
14.6301656134537));
#158014=CARTESIAN_POINT('Ctrl Pts',(-2.26554735932142,-6.63767983593482,
14.6217759186145));
#158015=CARTESIAN_POINT('Ctrl Pts',(-2.43810443619075,-6.57368034823165,
14.6133862237753));
#158016=CARTESIAN_POINT('Ctrl Pts',(-2.5476579465224,-6.53304817791146,
14.6080597513007));
#158017=CARTESIAN_POINT('Ctrl Pts',(-2.65614157544742,-6.4896967032418,
14.6027332788261));
#158018=CARTESIAN_POINT('Ctrl Pts',(-2.76341802457582,-6.44369050963417,
14.5974068063514));
#158019=CARTESIAN_POINT('Ctrl Pts',(-2.93221945005896,-6.37129893510762,
14.5890255059466));
#158020=CARTESIAN_POINT('Ctrl Pts',(-3.0983713354527,-6.29218604120259,
14.5806442055417));
#158021=CARTESIAN_POINT('Ctrl Pts',(-3.26131974452614,-6.20656266273563,
14.5722629051368));
#158022=CARTESIAN_POINT('Ctrl Pts',(-3.42406164034511,-6.12104779936646,
14.5638922268032));
#158023=CARTESIAN_POINT('Ctrl Pts',(-3.58360786318189,-6.02903904616635,
14.5555215484697));
#158024=CARTESIAN_POINT('Ctrl Pts',(-3.73942423593819,-5.93079530469381,
14.5471508701361));
#158025=CARTESIAN_POINT('Ctrl Pts',(-3.89506378386354,-5.83266305300036,
14.5387896910853));
#158026=CARTESIAN_POINT('Ctrl Pts',(-4.04698164254987,-5.72831008925468,
14.5304285120345));
#158027=CARTESIAN_POINT('Ctrl Pts',(-4.19466765942402,-5.61804145494515,
14.5220673329837));
#158028=CARTESIAN_POINT('Ctrl Pts',(-4.34216203627036,-5.50791590719583,
14.513717003549));
#158029=CARTESIAN_POINT('Ctrl Pts',(-4.48543526300853,-5.39189019513811,
14.5053666741143));
#158030=CARTESIAN_POINT('Ctrl Pts',(-4.62400570592323,-5.27031287440218,
14.4970163446796));
#158031=CARTESIAN_POINT('Ctrl Pts',(-4.76246952717136,-5.14882910014184,
14.4886724403239));
#158032=CARTESIAN_POINT('Ctrl Pts',(-4.89623753038195,-5.02180244495776,
14.4803285359682));
#158033=CARTESIAN_POINT('Ctrl Pts',(-5.02485984787179,-4.88962269216613,
14.4719846316124));
#158034=CARTESIAN_POINT('Ctrl Pts',(-5.15337885511394,-4.7575491069764,
14.4636474291327));
#158035=CARTESIAN_POINT('Ctrl Pts',(-5.27676019156735,-4.62033091296745,
14.455310226653));
#158036=CARTESIAN_POINT('Ctrl Pts',(-5.39458956111235,-4.47839592149217,
14.4469730241733));
#158037=CARTESIAN_POINT('Ctrl Pts',(-5.43337833916447,-4.43167170576036,
14.4442284631372));
#158038=CARTESIAN_POINT('Ctrl Pts',(-5.47156574979355,-4.38443663526283,
14.4414839021011));
#158039=CARTESIAN_POINT('Ctrl Pts',(-5.50913790009358,-4.33670683356075,
14.438739341065));
#158040=CARTESIAN_POINT('Ctrl Pts',(-5.62328666333548,-4.19169788968699,
14.4304010307631));
#158041=CARTESIAN_POINT('Ctrl Pts',(-5.73165981888653,-4.04223901281737,
14.4220627204612));
#158042=CARTESIAN_POINT('Ctrl Pts',(-5.83392404630276,-3.88882460191642,
14.4137244101593));
#158043=CARTESIAN_POINT('Ctrl Pts',(-5.93625261490078,-3.73531366787391,
14.4053808536755));
#158044=CARTESIAN_POINT('Ctrl Pts',(-6.03246440723192,-3.57784250843427,
14.3970372971916));
#158045=CARTESIAN_POINT('Ctrl Pts',(-6.12227082116779,-3.41693233102112,
14.3886937407078));
#158046=CARTESIAN_POINT('Ctrl Pts',(-6.212145559432,-3.25589973384628,14.3803438364826));
#158047=CARTESIAN_POINT('Ctrl Pts',(-6.29560503938939,-3.09142318563735,
14.3719939322574));
#158048=CARTESIAN_POINT('Ctrl Pts',(-6.37240757103098,-2.92404656446629,
14.3636440280321));
#158049=CARTESIAN_POINT('Ctrl Pts',(-6.44932530078655,-2.75641889074953,
14.3552815995685));
#158050=CARTESIAN_POINT('Ctrl Pts',(-6.51956599243058,-2.58588274966744,
14.3469191711048));
#158051=CARTESIAN_POINT('Ctrl Pts',(-6.58293633678555,-2.41300139832708,
14.3385567426412));
#158052=CARTESIAN_POINT('Ctrl Pts',(-6.64636087142363,-2.23997220986405,
14.3301871631612));
#158053=CARTESIAN_POINT('Ctrl Pts',(-6.70290323616088,-2.06459412080513,
14.3218175836812));
#158054=CARTESIAN_POINT('Ctrl Pts',(-6.75242043074529,-1.8874440094884,
14.3134480042012));
#158055=CARTESIAN_POINT('Ctrl Pts',(-6.80201399956923,-1.71002066570872,
14.3050655156647));
#158056=CARTESIAN_POINT('Ctrl Pts',(-6.84456067020032,-1.53082015623563,
14.2966830271281));
#158057=CARTESIAN_POINT('Ctrl Pts',(-6.87996853946572,-1.35042936078195,
14.2883005385915));
#158058=CARTESIAN_POINT('Ctrl Pts',(-6.8915545744813,-1.29140253663311,
14.2855576509872));
#158059=CARTESIAN_POINT('Ctrl Pts',(-6.90237666812968,-1.23224830520003,
14.2828147633829));
#158060=CARTESIAN_POINT('Ctrl Pts',(-6.91243280912787,-1.17298730674829,
14.2800718757786));
#158061=CARTESIAN_POINT('Ctrl Pts',(-6.94319220518833,-0.991721697739546,
14.2716820206458));
#158062=CARTESIAN_POINT('Ctrl Pts',(-6.96684353899493,-0.809090877999625,
14.2632921655131));
#158063=CARTESIAN_POINT('Ctrl Pts',(-6.98327672178247,-0.625677864009183,
14.2549023103803));
#158064=CARTESIAN_POINT('Ctrl Pts',(-6.99969474025931,-0.442434100976752,
14.2465201972882));
#158065=CARTESIAN_POINT('Ctrl Pts',(-7.00890785683722,-0.258409908431101,
14.2381380841961));
#158066=CARTESIAN_POINT('Ctrl Pts',(-7.01085739945251,-0.0741962737743869,
14.229755971104));
#158067=CARTESIAN_POINT('Ctrl Pts',(-7.01280542963592,0.109874450144695,
14.2213803607551));
#158068=CARTESIAN_POINT('Ctrl Pts',(-7.00750111685168,0.294133995638763,
14.2130047504063));
#158069=CARTESIAN_POINT('Ctrl Pts',(-6.99493774077801,0.477988038699149,
14.2046291400574));
#158070=CARTESIAN_POINT('Ctrl Pts',(-6.98238226725445,0.661726434836188,
14.1962587980918));
#158071=CARTESIAN_POINT('Ctrl Pts',(-6.96257685710581,0.845059510003589,
14.1878884561262));
#158072=CARTESIAN_POINT('Ctrl Pts',(-6.93556685367119,1.02739426743462,
14.1795181141607));
#158073=CARTESIAN_POINT('Ctrl Pts',(-6.90856988056661,1.2096410618236,14.1711518102663));
#158074=CARTESIAN_POINT('Ctrl Pts',(-6.87437529333594,1.39089017429796,
14.162785506372));
#158075=CARTESIAN_POINT('Ctrl Pts',(-6.83308018701918,1.57055459003051,
14.1544192024777));
#158076=CARTESIAN_POINT('Ctrl Pts',(-6.79179662978624,1.75016875866163,
14.1460552384041));
#158077=CARTESIAN_POINT('Ctrl Pts',(-6.74341658530399,1.92819879393217,
14.1376912743304));
#158078=CARTESIAN_POINT('Ctrl Pts',(-6.6880881936728,2.10406817288664,14.1293273102568));
#158079=CARTESIAN_POINT('Ctrl Pts',(-6.63276831616165,2.27991048846626,
14.1209646332583));
#158080=CARTESIAN_POINT('Ctrl Pts',(-6.57050232194391,2.45359249722821,
14.1126019562597));
#158081=CARTESIAN_POINT('Ctrl Pts',(-6.50148825500374,2.62455272999962,
14.1042392792612));
#158082=CARTESIAN_POINT('Ctrl Pts',(-6.43247560893708,2.79550944301226,
14.0958767744349));
#158083=CARTESIAN_POINT('Ctrl Pts',(-6.35671529057287,2.96374418716771,
14.0875142696086));
#158084=CARTESIAN_POINT('Ctrl Pts',(-6.27445369610554,3.12871497230534,
14.0791517647823));
#158085=CARTESIAN_POINT('Ctrl Pts',(-6.19218283036907,3.29370435042744,
14.0707883174623));
#158086=CARTESIAN_POINT('Ctrl Pts',(-6.10340937481897,3.45542874225665,
14.0624248701423));
#158087=CARTESIAN_POINT('Ctrl Pts',(-6.00842612691287,3.61336990078941,
14.0540614228224));
#158088=CARTESIAN_POINT('Ctrl Pts',(-5.91338695020106,3.77140405951497,
14.0456930508695));
#158089=CARTESIAN_POINT('Ctrl Pts',(-5.81213084330804,3.9256502510821,14.0373246789167));
#158090=CARTESIAN_POINT('Ctrl Pts',(-5.70499502510663,4.07561753922135,
14.0289563069639));
#158091=CARTESIAN_POINT('Ctrl Pts',(-5.59782710621405,4.22562976147958,
14.0205854276282));
#158092=CARTESIAN_POINT('Ctrl Pts',(-5.48477615858671,4.37136025948855,
14.0122145482924));
#158093=CARTESIAN_POINT('Ctrl Pts',(-5.36622073602281,4.51234989498585,
14.0038436689567));
#158094=CARTESIAN_POINT('Ctrl Pts',(-5.2475648627314,4.65345898947669,13.9954656970654));
#158095=CARTESIAN_POINT('Ctrl Pts',(-5.12339541103834,4.78981894673049,
13.9870877251741));
#158096=CARTESIAN_POINT('Ctrl Pts',(-4.99412973283141,4.92100546373902,
13.9787097532828));
#158097=CARTESIAN_POINT('Ctrl Pts',(-4.91198034171617,5.00437556355413,
13.9733854839238));
#158098=CARTESIAN_POINT('Ctrl Pts',(-4.82777348467621,5.08565699865715,
13.9680612145648));
#158099=CARTESIAN_POINT('Ctrl Pts',(-4.74162354313369,5.16474904886001,
13.9627369452057));
#158100=CARTESIAN_POINT('Ctrl Pts',(-4.61439811526017,5.28155144881852,
13.9548741140165));
#158101=CARTESIAN_POINT('Ctrl Pts',(-4.48266862771123,5.39381977872991,
13.9470112828272));
#158102=CARTESIAN_POINT('Ctrl Pts',(-4.34680621465619,5.5011728108401,13.9391484516379));
#158103=CARTESIAN_POINT('Ctrl Pts',(-4.21104819393207,5.60844335631546,
13.9312916619965));
#158104=CARTESIAN_POINT('Ctrl Pts',(-4.07116386007449,5.71080587976393,
13.9234348723551));
#158105=CARTESIAN_POINT('Ctrl Pts',(-3.92756051208506,5.80791657880949,
13.9155780827138));
#158106=CARTESIAN_POINT('Ctrl Pts',(-3.78403814958601,5.90497251201781,
13.9077257239298));
#158107=CARTESIAN_POINT('Ctrl Pts',(-3.63680125991078,5.99678229956816,
13.8998733651458));
#158108=CARTESIAN_POINT('Ctrl Pts',(-3.48628926875563,6.083043127996,13.8920210063619));
#158109=CARTESIAN_POINT('Ctrl Pts',(-3.33581281523772,6.16928358923578,
13.8841705016115));
#158110=CARTESIAN_POINT('Ctrl Pts',(-3.18206312560092,6.24997750223041,
13.876319996861));
#158111=CARTESIAN_POINT('Ctrl Pts',(-3.02550753064883,6.32486606533982,
13.8684694921106));
#158112=CARTESIAN_POINT('Ctrl Pts',(-2.86897712055763,6.39974258123977,
13.860620250259));
#158113=CARTESIAN_POINT('Ctrl Pts',(-2.70964204919594,6.46881544444567,
13.8527710084073));
#158114=CARTESIAN_POINT('Ctrl Pts',(-2.54799267681535,6.53187261674593,
13.8449217665557));
#158115=CARTESIAN_POINT('Ctrl Pts',(-2.38628884159724,6.59495103424177,
13.8370698801408));
#158116=CARTESIAN_POINT('Ctrl Pts',(-2.22226950364427,6.65200957363986,
13.829217993726));
#158117=CARTESIAN_POINT('Ctrl Pts',(-2.0564435429659,6.70288493986685,13.8213661073111));
#158118=CARTESIAN_POINT('Ctrl Pts',(-1.93467960403471,6.74024208805417,
13.8156005648472));
#158119=CARTESIAN_POINT('Ctrl Pts',(-1.81194197276822,6.77426641776532,
13.8098350223832));
#158120=CARTESIAN_POINT('Ctrl Pts',(-1.68843657932644,6.80491061514348,
13.8040694799193));
#158121=CARTESIAN_POINT('Ctrl Pts',(-1.48160744378032,6.85622912583037,
13.7944141755594));
#158122=CARTESIAN_POINT('Ctrl Pts',(-1.27273050459558,6.89804131974426,
13.7847588711995));
#158123=CARTESIAN_POINT('Ctrl Pts',(-1.0626057372995,6.93025941863349,13.7751035668396));
#158124=CARTESIAN_POINT('Ctrl Pts',(-0.85131691821211,6.96265599974643,
13.7653947739049));
#158125=CARTESIAN_POINT('Ctrl Pts',(-0.638766462176318,6.98535193935877,
13.7556859809701));
#158126=CARTESIAN_POINT('Ctrl Pts',(-0.425764535513677,6.99831059062106,
13.7459771880354));
#158127=CARTESIAN_POINT('Ctrl Pts',(-0.211737625493769,7.01133160001355,
13.7362216755647));
#158128=CARTESIAN_POINT('Ctrl Pts',(0.00274506599505633,7.01452140358415,
13.726466163094));
#158129=CARTESIAN_POINT('Ctrl Pts',(0.216865565637567,7.00789525385053,
13.7167106506233));
#158130=CARTESIAN_POINT('Ctrl Pts',(0.431198077516598,7.00126254320925,
13.7069454786944));
#158131=CARTESIAN_POINT('Ctrl Pts',(0.645167642239691,6.98479445079353,
13.6971803067655));
#158132=CARTESIAN_POINT('Ctrl Pts',(0.857958406906245,6.95855832299471,
13.6874151348366));
#158133=CARTESIAN_POINT('Ctrl Pts',(1.07045903619301,6.93235796756088,13.6776632774981));
#158134=CARTESIAN_POINT('Ctrl Pts',(1.28178404011654,6.89641620031286,13.6679114201595));
#158135=CARTESIAN_POINT('Ctrl Pts',(1.49112599177709,6.85085176012055,13.658159562821));
#158136=CARTESIAN_POINT('Ctrl Pts',(1.58241424396691,6.83098236426286,13.6539070467583));
#158137=CARTESIAN_POINT('Ctrl Pts',(1.67332546937911,6.80928379237649,13.6496545306955));
#158138=CARTESIAN_POINT('Ctrl Pts',(1.76379304747665,6.78576897987052,13.6454020146328));
#158139=CARTESIAN_POINT('Ctrl Pts',(1.93468721209668,6.74134926262031,13.637368969034));
#158140=CARTESIAN_POINT('Ctrl Pts',(2.10408073117804,6.69042322326471,13.6293359234352));
#158141=CARTESIAN_POINT('Ctrl Pts',(2.27143590991143,6.633114311518,13.6213028778363));
#158142=CARTESIAN_POINT('Ctrl Pts',(2.43868350629205,6.57584224014638,13.6132749961885));
#158143=CARTESIAN_POINT('Ctrl Pts',(2.60389502520306,6.51219558207775,13.6052471145407));
#158144=CARTESIAN_POINT('Ctrl Pts',(2.76654609550033,6.44234811726065,13.5972192328929));
#158145=CARTESIAN_POINT('Ctrl Pts',(2.92912372723587,6.37253218926251,13.5891949759128));
#158146=CARTESIAN_POINT('Ctrl Pts',(3.08914287609492,6.29652117343372,13.5811707189327));
#158147=CARTESIAN_POINT('Ctrl Pts',(3.24609743408801,6.21453763452336,13.5731464619526));
#158148=CARTESIAN_POINT('Ctrl Pts',(3.40303301467663,6.13256400825778,13.5651231751869));
#158149=CARTESIAN_POINT('Ctrl Pts',(3.55690441415735,6.04461946007117,13.5570998884212));
#158150=CARTESIAN_POINT('Ctrl Pts',(3.70722834423393,5.95097341333404,13.5490766016555));
#158151=CARTESIAN_POINT('Ctrl Pts',(3.85753995660528,5.85733504005514,13.5410539723266));
#158152=CARTESIAN_POINT('Ctrl Pts',(4.00430436951159,5.75799629609272,13.5330313429976));
#158153=CARTESIAN_POINT('Ctrl Pts',(4.14706587138744,5.65327084269572,13.5250087136687));
#158154=CARTESIAN_POINT('Ctrl Pts',(4.28988104142454,5.54850601998384,13.5169830684023));
#158155=CARTESIAN_POINT('Ctrl Pts',(4.42869000032998,5.43835066191202,13.5089574231359));
#158156=CARTESIAN_POINT('Ctrl Pts',(4.56306852052165,5.32315998627924,13.5009317778695));
#158157=CARTESIAN_POINT('Ctrl Pts',(4.64230628464827,5.2552365445539,13.4961993683618));
#158158=CARTESIAN_POINT('Ctrl Pts',(4.72000421274412,5.18556308634323,13.4914669588541));
#158159=CARTESIAN_POINT('Ctrl Pts',(4.79608113605262,5.11421864011505,13.4867345493464));
#158160=CARTESIAN_POINT('Ctrl Pts',(4.93641825604448,4.98261139739737,13.4780047967217));
#158161=CARTESIAN_POINT('Ctrl Pts',(5.07130774320044,4.84525047187811,13.4692750440971));
#158162=CARTESIAN_POINT('Ctrl Pts',(5.20030252992249,4.70260355120243,13.4605452914724));
#158163=CARTESIAN_POINT('Ctrl Pts',(5.32933520731001,4.55991472971133,13.451812974588));
#158164=CARTESIAN_POINT('Ctrl Pts',(5.45246954423712,4.41193701681353,13.4430806577035));
#158165=CARTESIAN_POINT('Ctrl Pts',(5.5692976497973,4.25917248423474,13.4343483408191));
#158166=CARTESIAN_POINT('Ctrl Pts',(5.68618189330382,4.10633454562842,13.4256118279039));
#158167=CARTESIAN_POINT('Ctrl Pts',(5.79675368208154,3.9487054074843,13.4168753149886));
#158168=CARTESIAN_POINT('Ctrl Pts',(5.90064667843867,3.78681863029255,13.4081388020733));
#158169=CARTESIAN_POINT('Ctrl Pts',(6.00455354455175,3.62491024115225,13.3994011228301));
#158170=CARTESIAN_POINT('Ctrl Pts',(6.10177969345145,3.45874331079357,13.3906634435869));
#158171=CARTESIAN_POINT('Ctrl Pts',(6.19200305242617,3.28887895205113,13.3819257643437));
#158172=CARTESIAN_POINT('Ctrl Pts',(6.28225097168962,3.11896835342424,13.3731857065599));
#158173=CARTESIAN_POINT('Ctrl Pts',(6.365492163762,2.94535855734084,13.3644456487761));
#158174=CARTESIAN_POINT('Ctrl Pts',(6.44145072079951,2.76863489359133,13.3557055909922));
#158175=CARTESIAN_POINT('Ctrl Pts',(6.48734531525382,2.66185744553822,13.3504247981081));
#158176=CARTESIAN_POINT('Ctrl Pts',(6.53058218404267,2.55394367782272,13.3451440052239));
#158177=CARTESIAN_POINT('Ctrl Pts',(6.57110895151813,2.44502632087638,13.3398632123397));
#158178=CARTESIAN_POINT('Origin',(0.,0.,50.));
#158179=CARTESIAN_POINT('',(6.57110895151813,2.44502632087638,11.3397782664936));
#158180=CARTESIAN_POINT('',(6.57110895151814,2.44502632087637,11.8871243640548));
#158181=CARTESIAN_POINT('',(6.57110895151814,2.44502632087636,50.));
#158182=CARTESIAN_POINT('',(7.0112496259069,-0.00229035375306598,13.7735343568827));
#158183=CARTESIAN_POINT('Ctrl Pts',(6.57110895151814,2.44502632087636,11.8871243640548));
#158184=CARTESIAN_POINT('Ctrl Pts',(6.50760538438029,2.61569477336292,11.8953815622089));
#158185=CARTESIAN_POINT('Ctrl Pts',(6.43743464203002,2.78392547564742,11.9036387603629));
#158186=CARTESIAN_POINT('Ctrl Pts',(6.36081519077275,2.9491789825873,11.911895958517));
#158187=CARTESIAN_POINT('Ctrl Pts',(6.28420124408154,3.11442061723063,11.9201525634498));
#158188=CARTESIAN_POINT('Ctrl Pts',(6.20113965574545,3.27668517334573,11.9284091683825));
#158189=CARTESIAN_POINT('Ctrl Pts',(6.11189630149514,3.43545486977635,11.9366657733153));
#158190=CARTESIAN_POINT('Ctrl Pts',(6.02264530226914,3.59423816711294,11.9449230855449));
#158191=CARTESIAN_POINT('Ctrl Pts',(5.92721164966669,3.74952571095857,11.9531803977745));
#158192=CARTESIAN_POINT('Ctrl Pts',(5.82590641104413,3.9008256885248,11.9614377100041));
#158193=CARTESIAN_POINT('Ctrl Pts',(5.72454044241862,4.0522163667123,11.9696999722896));
#158194=CARTESIAN_POINT('Ctrl Pts',(5.6172960445512,4.19961441816603,11.9779622345751));
#158195=CARTESIAN_POINT('Ctrl Pts',(5.50452724491788,4.3425575842419,11.9862244968607));
#158196=CARTESIAN_POINT('Ctrl Pts',(5.3917222526362,4.48554662729581,11.9944894108828));
#158197=CARTESIAN_POINT('Ctrl Pts',(5.27338954081468,4.62407767099775,12.0027543249049));
#158198=CARTESIAN_POINT('Ctrl Pts',(5.14992267951546,4.75772245486349,12.011019238927));
#158199=CARTESIAN_POINT('Ctrl Pts',(5.02634348688269,4.89148883003427,12.0192916724471));
#158200=CARTESIAN_POINT('Ctrl Pts',(4.89762104960985,5.02035981792788,12.0275641059672));
#158201=CARTESIAN_POINT('Ctrl Pts',(4.76418567851758,5.14394414657741,12.0358365394873));
#158202=CARTESIAN_POINT('Ctrl Pts',(4.68680150134963,5.21561533469727,12.0406340340039));
#158203=CARTESIAN_POINT('Ctrl Pts',(4.6078328794217,5.28550920289178,12.0454315285205));
#158204=CARTESIAN_POINT('Ctrl Pts',(4.52736870480114,5.35355575046037,12.050229023037));
#158205=CARTESIAN_POINT('Ctrl Pts',(4.3954923223182,5.46508032119157,12.0580918542263));
#158206=CARTESIAN_POINT('Ctrl Pts',(4.25930025509482,5.57189116622296,12.0659546854156));
#158207=CARTESIAN_POINT('Ctrl Pts',(4.11917885399977,5.67362248755248,12.0738175166048));
#158208=CARTESIAN_POINT('Ctrl Pts',(3.97916511770559,5.77527564178997,12.0816743062462));
#158209=CARTESIAN_POINT('Ctrl Pts',(3.83522835813943,5.87185681133711,12.0895310958876));
#158210=CARTESIAN_POINT('Ctrl Pts',(3.68778953694743,5.96303906524861,12.097387885529));
#158211=CARTESIAN_POINT('Ctrl Pts',(3.54043386427054,6.05416989668566,12.105240244313));
#158212=CARTESIAN_POINT('Ctrl Pts',(3.38958038194864,6.13990766924159,12.1130926030969));
#158213=CARTESIAN_POINT('Ctrl Pts',(3.23568048250117,6.21996771516227,12.1209449618809));
#158214=CARTESIAN_POINT('Ctrl Pts',(3.08181692061632,6.30000885797164,12.1287954666313));
#158215=CARTESIAN_POINT('Ctrl Pts',(2.92490870724261,6.37437475898552,12.1366459713818));
#158216=CARTESIAN_POINT('Ctrl Pts',(2.76543332458663,6.44282586213268,12.1444964761322));
#158217=CARTESIAN_POINT('Ctrl Pts',(2.60598359649338,6.51126595365479,12.1523457179838));
#158218=CARTESIAN_POINT('Ctrl Pts',(2.44396787301681,6.57379299375415,12.1601949598355));
#158219=CARTESIAN_POINT('Ctrl Pts',(2.27988474238346,6.63021508881477,12.1680442016871));
#158220=CARTESIAN_POINT('Ctrl Pts',(2.11574632893181,6.68665619358357,12.1758960881019));
#158221=CARTESIAN_POINT('Ctrl Pts',(1.9495394781173,6.7369881206579,12.1837479745168));
#158222=CARTESIAN_POINT('Ctrl Pts',(1.78177929761831,6.78106843329861,12.1915998609316));
#158223=CARTESIAN_POINT('Ctrl Pts',(1.65859508514715,6.81343605821399,12.1973654033956));
#158224=CARTESIAN_POINT('Ctrl Pts',(1.53457370881477,6.84243397803418,12.2031309458595));
#158225=CARTESIAN_POINT('Ctrl Pts',(1.40992285470066,6.86802330414602,12.2088964883235));
#158226=CARTESIAN_POINT('Ctrl Pts',(1.20117546575607,6.91087664076099,12.2185517926834));
#158227=CARTESIAN_POINT('Ctrl Pts',(0.990769093079809,6.94414815441213,
12.2282070970433));
#158228=CARTESIAN_POINT('Ctrl Pts',(0.779506623166767,6.96778271668536,
12.2378624014033));
#158229=CARTESIAN_POINT('Ctrl Pts',(0.567073798805806,6.99154820999944,
12.2475711943379));
#158230=CARTESIAN_POINT('Ctrl Pts',(0.353775418667275,7.00556973151011,
12.2572799872726));
#158231=CARTESIAN_POINT('Ctrl Pts',(0.14042246938709,7.00984365678659,12.2669887802072));
#158232=CARTESIAN_POINT('Ctrl Pts',(-0.0739571524036458,7.01413814855446,
12.2767442926779));
#158233=CARTESIAN_POINT('Ctrl Pts',(-0.288391826045461,7.0085910289728,
12.2864998051487));
#158234=CARTESIAN_POINT('Ctrl Pts',(-0.502064877858065,6.99325084784761,
12.2962553176194));
#158235=CARTESIAN_POINT('Ctrl Pts',(-0.715949498864964,6.97789547758307,
12.3060204895483));
#158236=CARTESIAN_POINT('Ctrl Pts',(-0.929070952183159,6.95272766417894,
12.3157856614773));
#158237=CARTESIAN_POINT('Ctrl Pts',(-1.14061680418228,6.91784792175407,
12.3255508334062));
#158238=CARTESIAN_POINT('Ctrl Pts',(-1.35187421821159,6.88301573706666,
12.3353026907448));
#158239=CARTESIAN_POINT('Ctrl Pts',(-1.56156028716068,6.83849809556149,
12.3450545480834));
#158240=CARTESIAN_POINT('Ctrl Pts',(-1.76887308924225,6.78444651807755,
12.3548064054219));
#158241=CARTESIAN_POINT('Ctrl Pts',(-1.85927648525571,6.76087611569348,
12.3590589214846));
#158242=CARTESIAN_POINT('Ctrl Pts',(-1.94922867856742,6.73549340807665,
12.3633114375472));
#158243=CARTESIAN_POINT('Ctrl Pts',(-2.03866363066502,6.70831403286278,
12.3675639536099));
#158244=CARTESIAN_POINT('Ctrl Pts',(-2.20760715439131,6.65697191981173,
12.3755969992087));
#158245=CARTESIAN_POINT('Ctrl Pts',(-2.37478632349617,6.59918999176792,
12.3836300448075));
#158246=CARTESIAN_POINT('Ctrl Pts',(-2.53966891637576,6.53511349233468,
12.3916630904063));
#158247=CARTESIAN_POINT('Ctrl Pts',(-2.70444551637603,6.47107818374247,
12.3996909720541));
#158248=CARTESIAN_POINT('Ctrl Pts',(-2.86692813856673,6.40075649043177,
12.4077188537019));
#158249=CARTESIAN_POINT('Ctrl Pts',(-3.02659992353144,6.32434340191767,
12.4157467353497));
#158250=CARTESIAN_POINT('Ctrl Pts',(-3.18619961511134,6.24796481466624,
12.4237709923298));
#158251=CARTESIAN_POINT('Ctrl Pts',(-3.34299066646071,6.16550046633553,
12.4317952493099));
#158252=CARTESIAN_POINT('Ctrl Pts',(-3.49647645280875,6.07719334705207,
12.43981950629));
#158253=CARTESIAN_POINT('Ctrl Pts',(-3.64994368116209,5.98889690499867,
12.4478427930557));
#158254=CARTESIAN_POINT('Ctrl Pts',(-3.80010611913558,5.8947592751385,12.4558660798214));
#158255=CARTESIAN_POINT('Ctrl Pts',(-3.94649185092404,5.7950693380744,12.4638893665871));
#158256=CARTESIAN_POINT('Ctrl Pts',(-4.09286558770762,5.69538756971136,
12.4719119959161));
#158257=CARTESIAN_POINT('Ctrl Pts',(-4.23546293395095,5.59015461008322,
12.479934625245));
#158258=CARTESIAN_POINT('Ctrl Pts',(-4.37384132918284,5.47970241798149,
12.4879572545739));
#158259=CARTESIAN_POINT('Ctrl Pts',(-4.51227174483931,5.3692087037193,12.4959828998403));
#158260=CARTESIAN_POINT('Ctrl Pts',(-4.6464797563193,5.25349206862029,12.5040085451067));
#158261=CARTESIAN_POINT('Ctrl Pts',(-4.77605595330646,5.13292471144726,
12.512034190373));
#158262=CARTESIAN_POINT('Ctrl Pts',(-4.85246197503441,5.06183085064536,
12.5167665998808));
#158263=CARTESIAN_POINT('Ctrl Pts',(-4.92725817294144,4.9890511310218,12.5214990093886));
#158264=CARTESIAN_POINT('Ctrl Pts',(-5.00036666383986,4.91466782088668,
12.5262314188964));
#158265=CARTESIAN_POINT('Ctrl Pts',(-5.13523256982751,4.77745020924604,
12.534961467731));
#158266=CARTESIAN_POINT('Ctrl Pts',(-5.26442067180707,4.63470515361891,
12.5436915165657));
#158267=CARTESIAN_POINT('Ctrl Pts',(-5.38750327559169,4.48691820941599,
12.5524215654003));
#158268=CARTESIAN_POINT('Ctrl Pts',(-5.51062146886518,4.33908853243327,
12.5611541385395));
#158269=CARTESIAN_POINT('Ctrl Pts',(-5.62763046477304,4.18621426739015,
12.5698867116787));
#158270=CARTESIAN_POINT('Ctrl Pts',(-5.73814312435743,4.02881372700321,
12.5786192848179));
#158271=CARTESIAN_POINT('Ctrl Pts',(-5.85022579268221,3.86917706068211,
12.5874759180983));
#158272=CARTESIAN_POINT('Ctrl Pts',(-5.95562596969656,3.70488477013143,
12.5963325513787));
#158273=CARTESIAN_POINT('Ctrl Pts',(-6.05398527447998,3.53650800350849,
12.6051891846591));
#158274=CARTESIAN_POINT('Ctrl Pts',(-6.15102853820277,3.37038410700311,
12.6139273167659));
#158275=CARTESIAN_POINT('Ctrl Pts',(-6.24121805231284,3.20028460720148,
12.6226654488726));
#158276=CARTESIAN_POINT('Ctrl Pts',(-6.32425545767368,3.02678368381104,
12.6314035809794));
#158277=CARTESIAN_POINT('Ctrl Pts',(-6.40898201636928,2.84975339119167,
12.6403194648466));
#158278=CARTESIAN_POINT('Ctrl Pts',(-6.48626224073296,2.66918207419653,
12.6492353487138));
#158279=CARTESIAN_POINT('Ctrl Pts',(-6.5558300063021,2.48570301745182,12.6581512325811));
#158280=CARTESIAN_POINT('Ctrl Pts',(-6.62539777187123,2.30222396070711,
12.6670671164483));
#158281=CARTESIAN_POINT('Ctrl Pts',(-6.68725297711931,2.1158374491383,12.6759830003155));
#158282=CARTESIAN_POINT('Ctrl Pts',(-6.74118250120182,1.92719616230169,
12.6848988841828));
#158283=CARTESIAN_POINT('Ctrl Pts',(-6.79405229650815,1.74226172442096,
12.693639568679));
#158284=CARTESIAN_POINT('Ctrl Pts',(-6.83931061792905,1.55514066064806,
12.7023802531752));
#158285=CARTESIAN_POINT('Ctrl Pts',(-6.87680237159827,1.3664610146215,12.7111209376714));
#158286=CARTESIAN_POINT('Ctrl Pts',(-6.91428737987839,1.17781531519662,
12.7198600495733));
#158287=CARTESIAN_POINT('Ctrl Pts',(-6.9440085576483,0.987611861976033,
12.7285991614752));
#158288=CARTESIAN_POINT('Ctrl Pts',(-6.9658618755799,0.796489104032495,
12.7373382733771));
#158289=CARTESIAN_POINT('Ctrl Pts',(-6.98799833469763,0.60289007568695,
12.7461906130514));
#158290=CARTESIAN_POINT('Ctrl Pts',(-7.00206157913035,0.408348035340911,
12.7550429527258));
#158291=CARTESIAN_POINT('Ctrl Pts',(-7.00799757267363,0.213533566214939,
12.7638952924001));
#158292=CARTESIAN_POINT('Ctrl Pts',(-7.01385463701134,0.0213094892736452,
12.7726299250499));
#158293=CARTESIAN_POINT('Ctrl Pts',(-7.01179924502979,-0.171179535379829,
12.7813645576996));
#158294=CARTESIAN_POINT('Ctrl Pts',(-7.00183185414267,-0.363286730851884,
12.7900991903494));
#158295=CARTESIAN_POINT('Ctrl Pts',(-6.991662983931,-0.5592771519767,12.799010383536));
#158296=CARTESIAN_POINT('Ctrl Pts',(-6.97325883762931,-0.754869851934066,
12.8079215767226));
#158297=CARTESIAN_POINT('Ctrl Pts',(-6.94667580252179,-0.949379722323063,
12.8168327699093));
#158298=CARTESIAN_POINT('Ctrl Pts',(-6.92009276741428,-1.14388959271204,
12.8257439630959));
#158299=CARTESIAN_POINT('Ctrl Pts',(-6.88533087119722,-1.33731633137024,
12.8346551562825));
#158300=CARTESIAN_POINT('Ctrl Pts',(-6.84250272341955,-1.52898104713437,
12.8435663494692));
#158301=CARTESIAN_POINT('Ctrl Pts',(-6.80393051955038,-1.70159954395467,
12.8515920143216));
#158302=CARTESIAN_POINT('Ctrl Pts',(-6.75879730526915,-1.87286802781277,
12.859617679174));
#158303=CARTESIAN_POINT('Ctrl Pts',(-6.7072239494188,-2.04224715811845,
12.8676433440264));
#158304=CARTESIAN_POINT('Ctrl Pts',(-6.65566696168666,-2.21157253164253,
12.8756664617296));
#158305=CARTESIAN_POINT('Ctrl Pts',(-6.59767400833211,-2.37900939517207,
12.8836895794328));
#158306=CARTESIAN_POINT('Ctrl Pts',(-6.53341630104245,-2.54403183937876,
12.891712697136));
#158307=CARTESIAN_POINT('Ctrl Pts',(-6.46916669721183,-2.70903347281152,
12.8997348030539));
#158308=CARTESIAN_POINT('Ctrl Pts',(-6.39865404663914,-2.87162095213325,
12.9077569089718));
#158309=CARTESIAN_POINT('Ctrl Pts',(-6.32209833132922,-3.03128673198435,
12.9157790148897));
#158310=CARTESIAN_POINT('Ctrl Pts',(-6.24551416765691,-3.19101184417854,
12.9238041018492));
#158311=CARTESIAN_POINT('Ctrl Pts',(-6.16288260913011,-3.34781275584398,
12.9318291888088));
#158312=CARTESIAN_POINT('Ctrl Pts',(-6.0744705924461,-3.50120459042421,
12.9398542757683));
#158313=CARTESIAN_POINT('Ctrl Pts',(-5.98604116345816,-3.65462663475809,
12.9478809432285));
#158314=CARTESIAN_POINT('Ctrl Pts',(-5.89182919905072,-3.80463795127912,
12.9559076106888));
#158315=CARTESIAN_POINT('Ctrl Pts',(-5.79214579397796,-3.95078139914163,
12.963934278149));
#158316=CARTESIAN_POINT('Ctrl Pts',(-5.69238236341871,-4.09704217044933,
12.9719673893896));
#158317=CARTESIAN_POINT('Ctrl Pts',(-5.58713893356198,-4.23942857387815,
12.9800005006302));
#158318=CARTESIAN_POINT('Ctrl Pts',(-5.47676819497516,-4.37751490014695,
12.9880336118708));
#158319=CARTESIAN_POINT('Ctrl Pts',(-5.41173374636398,-4.458880379844,12.9927670128324));
#158320=CARTESIAN_POINT('Ctrl Pts',(-5.34491985473411,-4.53875351224123,
12.997500413794));
#158321=CARTESIAN_POINT('Ctrl Pts',(-5.27640478678752,-4.61705307403605,
13.0022338147557));
#158322=CARTESIAN_POINT('Ctrl Pts',(-5.13526161448851,-4.77835260817588,
13.0119847680498));
#158323=CARTESIAN_POINT('Ctrl Pts',(-4.98681445036669,-4.93306789468406,
13.0217357213439));
#158324=CARTESIAN_POINT('Ctrl Pts',(-4.83164907454465,-5.08062927037113,
13.031486674638));
#158325=CARTESIAN_POINT('Ctrl Pts',(-4.67626015388893,-5.22840323590313,
13.0412516760096));
#158326=CARTESIAN_POINT('Ctrl Pts',(-4.5141336889914,-5.36900264785623,
13.0510166773813));
#158327=CARTESIAN_POINT('Ctrl Pts',(-4.34589168468698,-5.50189531229636,
13.0607816787529));
#158328=CARTESIAN_POINT('Ctrl Pts',(-4.17793010494584,-5.63456647219875,
13.0705304038905));
#158329=CARTESIAN_POINT('Ctrl Pts',(-4.0038733878872,-5.75955653413059,
13.080279129028));
#158330=CARTESIAN_POINT('Ctrl Pts',(-3.82437342942543,-5.8763759609818,
13.0900278541656));
#158331=CARTESIAN_POINT('Ctrl Pts',(-3.6453661287486,-5.992874763803,13.0997498228327));
#158332=CARTESIAN_POINT('Ctrl Pts',(-3.46094544458197,-6.10124767805766,
13.1094717914998));
#158333=CARTESIAN_POINT('Ctrl Pts',(-3.27179036988941,-6.20104945456807,
13.1191937601669));
#158334=CARTESIAN_POINT('Ctrl Pts',(-3.08388688492214,-6.30019086878977,
13.1288514011066));
#158335=CARTESIAN_POINT('Ctrl Pts',(-2.89131148259919,-6.39087414900364,
13.1385090420462));
#158336=CARTESIAN_POINT('Ctrl Pts',(-2.69476145185496,-6.47270324362987,
13.1481666829859));
#158337=CARTESIAN_POINT('Ctrl Pts',(-2.60837094653578,-6.50866994792293,
13.1524115486713));
#158338=CARTESIAN_POINT('Ctrl Pts',(-2.52121299160725,-6.54292663910667,
13.1566564143567));
#158339=CARTESIAN_POINT('Ctrl Pts',(-2.43334873421041,-6.57544222849054,
13.1609012800421));
#158340=CARTESIAN_POINT('Ctrl Pts',(-2.27082375504671,-6.63558722537181,
13.168753127056));
#158341=CARTESIAN_POINT('Ctrl Pts',(-2.10594760139337,-6.6897467859166,
13.1766049740699));
#158342=CARTESIAN_POINT('Ctrl Pts',(-1.93922005044379,-6.73773345854945,
13.1844568210838));
#158343=CARTESIAN_POINT('Ctrl Pts',(-1.77253978207964,-6.78570652254993,
13.1923064413773));
#158344=CARTESIAN_POINT('Ctrl Pts',(-1.60400952703719,-6.82751007543977,
13.2001560616709));
#158345=CARTESIAN_POINT('Ctrl Pts',(-1.43414529570925,-6.86300618047915,
13.2080056819645));
#158346=CARTESIAN_POINT('Ctrl Pts',(-1.2642946258674,-6.89849945160859,
13.2158546755663));
#158347=CARTESIAN_POINT('Ctrl Pts',(-1.09311056530598,-6.92768620006069,
13.2237036691681));
#158348=CARTESIAN_POINT('Ctrl Pts',(-0.921120155848448,-6.9504794238232,
13.2315526627699));
#158349=CARTESIAN_POINT('Ctrl Pts',(-0.749042672683,-6.97328418712746,13.2394056300873));
#158350=CARTESIAN_POINT('Ctrl Pts',(-0.576158403606521,-6.98968890816385,
13.2472585974048));
#158351=CARTESIAN_POINT('Ctrl Pts',(-0.40300071038223,-6.9996583480861,
13.2551115647222));
#158352=CARTESIAN_POINT('Ctrl Pts',(-0.229799040923113,-7.00963031991105,
13.2629665264294));
#158353=CARTESIAN_POINT('Ctrl Pts',(-0.0563241904046526,-7.01316374685499,
13.2708214881366));
#158354=CARTESIAN_POINT('Ctrl Pts',(0.116890273251932,-7.01027554569142,
13.2786764498438));
#158355=CARTESIAN_POINT('Ctrl Pts',(0.290276666743483,-7.00738447774676,
13.2865392082572));
#158356=CARTESIAN_POINT('Ctrl Pts',(0.463401776424912,-6.99805907169667,
13.2944019666705));
#158357=CARTESIAN_POINT('Ctrl Pts',(0.63573636881906,-6.982368210848,13.3022647250838));
#158358=CARTESIAN_POINT('Ctrl Pts',(0.762158552946482,-6.97085762047976,
13.3080327318321));
#158359=CARTESIAN_POINT('Ctrl Pts',(0.888155422117685,-6.95592256172403,
13.3138007385803));
#158360=CARTESIAN_POINT('Ctrl Pts',(1.01352184654488,-6.9376076589179,13.3195687453285));
#158361=CARTESIAN_POINT('Ctrl Pts',(1.19561737437144,-6.91100514625302,
13.3279468117695));
#158362=CARTESIAN_POINT('Ctrl Pts',(1.37678580379762,-6.87721132586113,
13.3363248782105));
#158363=CARTESIAN_POINT('Ctrl Pts',(1.55643888652931,-6.83630927877019,
13.3447029446515));
#158364=CARTESIAN_POINT('Ctrl Pts',(1.7359691246174,-6.79543520001312,13.3530752822702));
#158365=CARTESIAN_POINT('Ctrl Pts',(1.91398576233902,-6.74746265773913,
13.361447619889));
#158366=CARTESIAN_POINT('Ctrl Pts',(2.08990965660702,-6.69252599469892,
13.3698199575077));
#158367=CARTESIAN_POINT('Ctrl Pts',(2.26573905556167,-6.63761884019824,
13.3781877980302));
#158368=CARTESIAN_POINT('Ctrl Pts',(2.43947763931422,-6.57575512128009,
13.3865556385528));
#158369=CARTESIAN_POINT('Ctrl Pts',(2.61055992599276,-6.50711944221871,
13.3949234790754));
#158370=CARTESIAN_POINT('Ctrl Pts',(2.78157538028006,-6.43851057532266,
13.4032880507453));
#158371=CARTESIAN_POINT('Ctrl Pts',(2.94993630212466,-6.36313514586109,
13.4116526224152));
#158372=CARTESIAN_POINT('Ctrl Pts',(3.11509531742393,-6.28122660997544,
13.420017194085));
#158373=CARTESIAN_POINT('Ctrl Pts',(3.28021398952132,-6.19933808179322,
13.4283797225507));
#158374=CARTESIAN_POINT('Ctrl Pts',(3.4421320208106,-6.11091977595823,13.4367422510163));
#158375=CARTESIAN_POINT('Ctrl Pts',(3.60032444524996,-6.01625219313782,
13.4451047794819));
#158376=CARTESIAN_POINT('Ctrl Pts',(3.75852949393871,-5.92157705554871,
13.4534679753035));
#158377=CARTESIAN_POINT('Ctrl Pts',(3.91300805665509,-5.82065180820859,
13.461831171125));
#158378=CARTESIAN_POINT('Ctrl Pts',(4.06326143054084,-5.71380198375646,
13.4701943669465));
#158379=CARTESIAN_POINT('Ctrl Pts',(4.21352505140549,-5.60694487236049,
13.4785581331212));
#158380=CARTESIAN_POINT('Ctrl Pts',(4.35956264076597,-5.49416256856747,
13.4869218992959));
#158381=CARTESIAN_POINT('Ctrl Pts',(4.50090591956166,-5.37582295706944,
13.4952856654706));
#158382=CARTESIAN_POINT('Ctrl Pts',(4.64227768206981,-5.25745949759296,
13.5036511171242));
#158383=CARTESIAN_POINT('Ctrl Pts',(4.77895299557132,-5.13353670834518,
13.5120165687777));
#158384=CARTESIAN_POINT('Ctrl Pts',(4.91049768391706,-5.00446191500597,
13.5203820204313));
#158385=CARTESIAN_POINT('Ctrl Pts',(5.04208642632047,-4.87534389477207,
13.5287502736582));
#158386=CARTESIAN_POINT('Ctrl Pts',(5.16854088277218,-4.74107066013836,
13.5371185268851));
#158387=CARTESIAN_POINT('Ctrl Pts',(5.28946437627122,-4.60208574177597,
13.545486780112));
#158388=CARTESIAN_POINT('Ctrl Pts',(5.4104999831,-4.46297196456631,13.5538627919035));
#158389=CARTESIAN_POINT('Ctrl Pts',(5.52599416368704,-4.31913802255477,
13.562238803695));
#158390=CARTESIAN_POINT('Ctrl Pts',(5.6355903443491,-4.17106078032666,13.5706148154865));
#158391=CARTESIAN_POINT('Ctrl Pts',(5.74524027233254,-4.02291091918902,
13.5789949349776));
#158392=CARTESIAN_POINT('Ctrl Pts',(5.84898624206894,-3.87051387598069,
13.5873750544688));
#158393=CARTESIAN_POINT('Ctrl Pts',(5.94651519299269,-3.7143752667181,13.59575517396));
#158394=CARTESIAN_POINT('Ctrl Pts',(6.04415558309701,-3.55805824931611,
13.6041448687992));
#158395=CARTESIAN_POINT('Ctrl Pts',(6.13556459098721,-3.39799140545235,
13.6125345636384));
#158396=CARTESIAN_POINT('Ctrl Pts',(6.22047462004988,-3.23470586975312,
13.6209242584776));
#158397=CARTESIAN_POINT('Ctrl Pts',(6.27438253223083,-3.13103870091497,
13.6262507309522));
#158398=CARTESIAN_POINT('Ctrl Pts',(6.32567180420849,-3.02607461810334,
13.6315772034268));
#158399=CARTESIAN_POINT('Ctrl Pts',(6.37428404911066,-2.91995366808336,
13.6369036759013));
#158400=CARTESIAN_POINT('Ctrl Pts',(6.45225519315827,-2.74974198793713,
13.6454470203491));
#158401=CARTESIAN_POINT('Ctrl Pts',(6.52348723065363,-2.57622528567362,
13.6539903647969));
#158402=CARTESIAN_POINT('Ctrl Pts',(6.58770463527921,-2.3999529580433,13.6625337092447));
#158403=CARTESIAN_POINT('Ctrl Pts',(6.65182696371074,-2.22394160798015,
13.6710644049616));
#158404=CARTESIAN_POINT('Ctrl Pts',(6.70895526197059,-2.04518305176247,
13.6795951006784));
#158405=CARTESIAN_POINT('Ctrl Pts',(6.75886111797927,-1.86424862890337,
13.6881257963953));
#158406=CARTESIAN_POINT('Ctrl Pts',(6.80867084795871,-1.68366271239224,
13.6966400607357));
#158407=CARTESIAN_POINT('Ctrl Pts',(6.85128580808707,-1.50090958292236,
13.7051543250761));
#158408=CARTESIAN_POINT('Ctrl Pts',(6.88652671837764,-1.31657750230319,
13.7136685894165));
#158409=CARTESIAN_POINT('Ctrl Pts',(6.92172656359226,-1.13246021780667,
13.7221729323641));
#158410=CARTESIAN_POINT('Ctrl Pts',(6.9495694307345,-0.946767947700473,
13.7306772753118));
#158411=CARTESIAN_POINT('Ctrl Pts',(6.96992612818737,-0.760102841799044,
13.7391816182595));
#158412=CARTESIAN_POINT('Ctrl Pts',(6.9902529427843,-0.573711753158142,
13.7476734771559));
#158413=CARTESIAN_POINT('Ctrl Pts',(7.00311547628919,-0.386350979474767,
13.7561653360522));
#158414=CARTESIAN_POINT('Ctrl Pts',(7.00843577920027,-0.198631546652243,
13.7646571949486));
#158415=CARTESIAN_POINT('Ctrl Pts',(7.01028967994043,-0.133219256925804,
13.7676162489266));
#158416=CARTESIAN_POINT('Ctrl Pts',(7.01122823789861,-0.0677634995192813,
13.7705753029046));
#158417=CARTESIAN_POINT('Ctrl Pts',(7.0112496259069,-0.0022903537530466,
13.7735343568827));
#158418=CARTESIAN_POINT('Ctrl Pts',(7.01124962590711,-0.00229035313711163,
13.7735343569105));
#158419=CARTESIAN_POINT('Ctrl Pts',(7.01130271976769,0.160241050471527,
13.7808799516696));
#158420=CARTESIAN_POINT('Ctrl Pts',(7.00570090552392,0.322819188341013,
13.7882255464287));
#158421=CARTESIAN_POINT('Ctrl Pts',(6.99445468411544,0.485005396212896,
13.7955711411878));
#158422=CARTESIAN_POINT('Ctrl Pts',(6.98168692844655,0.669134251564195,
13.803910542994));
#158423=CARTESIAN_POINT('Ctrl Pts',(6.96164931566915,0.85268294976881,13.8122499448002));
#158424=CARTESIAN_POINT('Ctrl Pts',(6.93442680677069,1.03506107261361,13.8205893466064));
#158425=CARTESIAN_POINT('Ctrl Pts',(6.90719096826687,1.21752849760224,13.8289328318325));
#158426=CARTESIAN_POINT('Ctrl Pts',(6.87276327240065,1.39882388116677,13.8372763170586));
#158427=CARTESIAN_POINT('Ctrl Pts',(6.8312797859362,1.57836720973272,13.8456198022846));
#158428=CARTESIAN_POINT('Ctrl Pts',(6.78974908017936,1.75811490658233,13.8539727846264));
#158429=CARTESIAN_POINT('Ctrl Pts',(6.74114661530322,1.93610624538186,13.8623257669681));
#158430=CARTESIAN_POINT('Ctrl Pts',(6.6856586632065,2.11177527251172,13.8706787493098));
#158431=CARTESIAN_POINT('Ctrl Pts',(6.65025755758115,2.22385145390847,13.8760079207605));
#158432=CARTESIAN_POINT('Ctrl Pts',(6.61205478698717,2.33498270143529,13.8813370922111));
#158433=CARTESIAN_POINT('Ctrl Pts',(6.57110895151813,2.44502632087638,13.8866662636617));
#158434=CARTESIAN_POINT('',(7.0112498931807,0.00122387650393776,13.2264656430896));
#158435=CARTESIAN_POINT('Ctrl Pts',(6.57110895151813,2.44502632087638,13.3398632123397));
#158436=CARTESIAN_POINT('Ctrl Pts',(6.6012849092065,2.36392719159765,13.3359311695798));
#158437=CARTESIAN_POINT('Ctrl Pts',(6.62995846650225,2.28227170996608,13.3319991268199));
#158438=CARTESIAN_POINT('Ctrl Pts',(6.6571103512001,2.20011552752226,13.32806708406));
#158439=CARTESIAN_POINT('Ctrl Pts',(6.71682758851922,2.01942308945293,13.319419038694));
#158440=CARTESIAN_POINT('Ctrl Pts',(6.76919104950635,1.8362765019726,13.3107709933279));
#158441=CARTESIAN_POINT('Ctrl Pts',(6.81402159556527,1.65128321546308,13.3021229479618));
#158442=CARTESIAN_POINT('Ctrl Pts',(6.85884212225374,1.46633127389431,13.2934768353844));
#158443=CARTESIAN_POINT('Ctrl Pts',(6.89613302745317,1.27953373815494,13.2848307228069));
#158444=CARTESIAN_POINT('Ctrl Pts',(6.92576572928521,1.09151070794493,13.2761846102295));
#158445=CARTESIAN_POINT('Ctrl Pts',(6.95539404940694,0.90351548020988,13.2675397761302));
#158446=CARTESIAN_POINT('Ctrl Pts',(6.97736638061505,0.71429540499206,13.2588949420308));
#158447=CARTESIAN_POINT('Ctrl Pts',(6.99160555274134,0.524479129590983,
13.2502501079315));
#158448=CARTESIAN_POINT('Ctrl Pts',(7.00466426059404,0.350399115376199,
13.2423219529842));
#158449=CARTESIAN_POINT('Ctrl Pts',(7.01121941622546,0.175817921308749,
13.2343937980369));
#158450=CARTESIAN_POINT('Ctrl Pts',(7.0112498931807,0.00122387650393776,
13.2264656430896));
#158451=CARTESIAN_POINT('Ctrl Pts',(7.0112498931807,0.00122387650393776,
13.2264656430896));
#158452=CARTESIAN_POINT('Ctrl Pts',(7.01128645483302,-0.208227714535047,
13.216954639037));
#158453=CARTESIAN_POINT('Ctrl Pts',(7.00193253296366,-0.417672943101247,
13.2074436349843));
#158454=CARTESIAN_POINT('Ctrl Pts',(6.98321925767691,-0.626318897775246,
13.1979326309316));
#158455=CARTESIAN_POINT('Ctrl Pts',(6.96450598239015,-0.834964852449244,
13.1884216268789));
#158456=CARTESIAN_POINT('Ctrl Pts',(6.93643335324898,-1.04281133667803,
13.1789106228262));
#158457=CARTESIAN_POINT('Ctrl Pts',(6.89909079732579,-1.24906874620839,
13.1693996187735));
#158458=CARTESIAN_POINT('Ctrl Pts',(6.86758005073053,-1.42311481253751,
13.1613739539212));
#158459=CARTESIAN_POINT('Ctrl Pts',(6.82945876018241,-1.59607916667199,
13.1533482890688));
#158460=CARTESIAN_POINT('Ctrl Pts',(6.78482573095118,-1.76741799332325,
13.1453226242164));
#158461=CARTESIAN_POINT('Ctrl Pts',(6.74020686714869,-1.93870244123346,
13.1372995065132));
#158462=CARTESIAN_POINT('Ctrl Pts',(6.68908047149763,-2.10836203446348,
13.12927638881));
#158463=CARTESIAN_POINT('Ctrl Pts',(6.63159619730733,-2.27586432775746,
13.1212532711068));
#158464=CARTESIAN_POINT('Ctrl Pts',(6.57411917238709,-2.44334549754637,
13.113231165189));
#158465=CARTESIAN_POINT('Ctrl Pts',(6.51028598550464,-2.60866956286985,
13.1052090592711));
#158466=CARTESIAN_POINT('Ctrl Pts',(6.44029576765884,-2.77132044115719,
13.0971869533533));
#158467=CARTESIAN_POINT('Ctrl Pts',(6.37027954121157,-2.93403176106052,
13.0891618663938));
#158468=CARTESIAN_POINT('Ctrl Pts',(6.29410185542612,-3.09406757127754,
13.0811367794343));
#158469=CARTESIAN_POINT('Ctrl Pts',(6.21200968017546,-3.25093252712301,
13.0731116924748));
#158470=CARTESIAN_POINT('Ctrl Pts',(6.12990133728169,-3.40782837673656,
13.0650850250146));
#158471=CARTESIAN_POINT('Ctrl Pts',(6.04187636216168,-3.56155180721156,
13.0570583575544));
#158472=CARTESIAN_POINT('Ctrl Pts',(5.94822697558419,-3.71163338833897,
13.0490316900942));
#158473=CARTESIAN_POINT('Ctrl Pts',(5.8545024076091,-3.86183545443092,13.0409985788536));
#158474=CARTESIAN_POINT('Ctrl Pts',(5.75514461197914,-4.0083895258752,13.032965467613));
#158475=CARTESIAN_POINT('Ctrl Pts',(5.65048865074503,-4.15085588406797,
13.0249323563724));
#158476=CARTESIAN_POINT('Ctrl Pts',(5.58882155654904,-4.23480223769019,
13.0201989554107));
#158477=CARTESIAN_POINT('Ctrl Pts',(5.52531572324001,-4.3173299453401,13.0154655544489));
#158478=CARTESIAN_POINT('Ctrl Pts',(5.46004604497905,-4.39835466387247,
13.0107321534872));
#158479=CARTESIAN_POINT('Ctrl Pts',(5.32558847643832,-4.56526810570072,
13.000981200193));
#158480=CARTESIAN_POINT('Ctrl Pts',(5.18356484757897,-4.72590019857516,
12.9912302468989));
#158481=CARTESIAN_POINT('Ctrl Pts',(5.03453725449078,-4.87965789739859,
12.9814792936047));
#158482=CARTESIAN_POINT('Ctrl Pts',(4.8852949591962,-5.03363711303312,12.971714292233));
#158483=CARTESIAN_POINT('Ctrl Pts',(4.72902854254238,-5.18072209625207,
12.9619492908613));
#158484=CARTESIAN_POINT('Ctrl Pts',(4.56633782112557,-5.32035576497081,
12.9521842894896));
#158485=CARTESIAN_POINT('Ctrl Pts',(4.40391827143435,-5.45975669329375,
12.942435564352));
#158486=CARTESIAN_POINT('Ctrl Pts',(4.23509584666012,-5.59173110455787,
12.9326868392144));
#158487=CARTESIAN_POINT('Ctrl Pts',(4.06050196677742,-5.71576332087821,
12.9229381140768));
#158488=CARTESIAN_POINT('Ctrl Pts',(3.88638727939536,-5.83945511685885,
12.9132161454096));
#158489=CARTESIAN_POINT('Ctrl Pts',(3.7065327922419,-5.95524821140251,12.9034941767424));
#158490=CARTESIAN_POINT('Ctrl Pts',(3.52159880338043,-6.06267007435911,
12.8937722080752));
#158491=CARTESIAN_POINT('Ctrl Pts',(3.33788847442183,-6.16938115490519,
12.8841145671355));
#158492=CARTESIAN_POINT('Ctrl Pts',(3.14916566690129,-6.26783136979799,
12.8744569261958));
#158493=CARTESIAN_POINT('Ctrl Pts',(2.95611096312666,-6.35759660061743,
12.864799285256));
#158494=CARTESIAN_POINT('Ctrl Pts',(2.8712567743537,-6.3970515099891,12.8605544195709));
#158495=CARTESIAN_POINT('Ctrl Pts',(2.78556613652069,-6.43482907720547,
12.8563095538858));
#158496=CARTESIAN_POINT('Ctrl Pts',(2.69909888003669,-6.47089574929814,
12.8520646882007));
#158497=CARTESIAN_POINT('Ctrl Pts',(2.53915797259935,-6.53760928338389,
12.8442128411868));
#158498=CARTESIAN_POINT('Ctrl Pts',(2.37662409889338,-6.59843809185593,
12.8363609941729));
#158499=CARTESIAN_POINT('Ctrl Pts',(2.21198898804205,-6.6531745264408,12.828509147159));
#158500=CARTESIAN_POINT('Ctrl Pts',(2.04740056637714,-6.70789543821534,
12.8206595268654));
#158501=CARTESIAN_POINT('Ctrl Pts',(1.88071245452658,-6.75652729265902,
12.8128099065718));
#158502=CARTESIAN_POINT('Ctrl Pts',(1.7124346177168,-6.79891125420424,12.8049602862782));
#158503=CARTESIAN_POINT('Ctrl Pts',(1.5441702157396,-6.84129183193233,12.7971112926764));
#158504=CARTESIAN_POINT('Ctrl Pts',(1.37431671155877,-6.8774254173219,12.7892622990746));
#158505=CARTESIAN_POINT('Ctrl Pts',(1.20339716687151,-6.90720361805453,
12.7814133054728));
#158506=CARTESIAN_POINT('Ctrl Pts',(1.03239109062408,-6.93699689461816,
12.7735603381554));
#158507=CARTESIAN_POINT('Ctrl Pts',(0.860318271805542,-6.96042829214932,
12.7657073708379));
#158508=CARTESIAN_POINT('Ctrl Pts',(0.687710194737447,-6.97744088119378,
12.7578544035205));
#158509=CARTESIAN_POINT('Ctrl Pts',(0.515058281017167,-6.99445779086425,
12.7499994418132));
#158510=CARTESIAN_POINT('Ctrl Pts',(0.341871219025297,-7.00505262108919,
12.742144480106));
#158511=CARTESIAN_POINT('Ctrl Pts',(0.168682822978939,-7.00922054637546,
12.7342895183987));
#158512=CARTESIAN_POINT('Ctrl Pts',(-0.00467747702693838,-7.01339260867596,
12.7264267599853));
#158513=CARTESIAN_POINT('Ctrl Pts',(-0.178038732466307,-7.011125030057,
12.718564001572));
#158514=CARTESIAN_POINT('Ctrl Pts',(-0.350869343762094,-7.00246508496172,
12.7107012431586));
#158515=CARTESIAN_POINT('Ctrl Pts',(-0.477655400235681,-6.99611227350271,
12.7049332364105));
#158516=CARTESIAN_POINT('Ctrl Pts',(-0.604155947560724,-6.98632051437413,
12.6991652296624));
#158517=CARTESIAN_POINT('Ctrl Pts',(-0.730164208890093,-6.97312604149358,
12.6933972229143));
#158518=CARTESIAN_POINT('Ctrl Pts',(-0.913192008897945,-6.95396098582093,
12.6850191564733));
#158519=CARTESIAN_POINT('Ctrl Pts',(-1.09558632776216,-6.92757283386555,
12.6766410900323));
#158520=CARTESIAN_POINT('Ctrl Pts',(-1.27675602187481,-6.89402064278215,
12.6682630235912));
#158521=CARTESIAN_POINT('Ctrl Pts',(-1.4578018343029,-6.86049139428842,
12.6598906859725));
#158522=CARTESIAN_POINT('Ctrl Pts',(-1.6376243692774,-6.81980793286507,
12.6515183483538));
#158523=CARTESIAN_POINT('Ctrl Pts',(-1.81563949333761,-6.77208090565469,
12.6431460107351));
#158524=CARTESIAN_POINT('Ctrl Pts',(-1.99355899880669,-6.72437951441835,
12.6347781702125));
#158525=CARTESIAN_POINT('Ctrl Pts',(-2.16967271229991,-6.66964218599894,
12.6264103296899));
#158526=CARTESIAN_POINT('Ctrl Pts',(-2.34340810346346,-6.60803034368955,
12.6180424891673));
#158527=CARTESIAN_POINT('Ctrl Pts',(-2.51707562581395,-6.54644256972099,
12.6096779174974));
#158528=CARTESIAN_POINT('Ctrl Pts',(-2.68836636919932,-6.47798574682312,
12.6013133458275));
#158529=CARTESIAN_POINT('Ctrl Pts',(-2.85672390664315,-6.40287084702741,
12.5929487741577));
#158530=CARTESIAN_POINT('Ctrl Pts',(-3.02504031958462,-6.32777429546202,
12.5845862456921));
#158531=CARTESIAN_POINT('Ctrl Pts',(-3.19042465571586,-6.24602304455298,
12.5762237172265));
#158532=CARTESIAN_POINT('Ctrl Pts',(-3.35234096176165,-6.1578759843468,
12.567861188761));
#158533=CARTESIAN_POINT('Ctrl Pts',(-3.51427018923537,-6.06972188972936,
12.5594979929395));
#158534=CARTESIAN_POINT('Ctrl Pts',(-3.67273054214267,-5.97517111793979,
12.551134797118));
#158535=CARTESIAN_POINT('Ctrl Pts',(-3.82721047479072,-5.8745286231452,
12.5427716012965));
#158536=CARTESIAN_POINT('Ctrl Pts',(-3.98170094266064,-5.77387926473412,
12.5344078351218));
#158537=CARTESIAN_POINT('Ctrl Pts',(-4.13221017335271,-5.66713753422754,
12.5260440689471));
#158538=CARTESIAN_POINT('Ctrl Pts',(-4.27825529505239,-5.5546519416482,
12.5176803027724));
#158539=CARTESIAN_POINT('Ctrl Pts',(-4.4243298479869,-5.44214368080134,
12.5093148511188));
#158540=CARTESIAN_POINT('Ctrl Pts',(-4.56593823760468,-5.32388945041,12.5009493994652));
#158541=CARTESIAN_POINT('Ctrl Pts',(-4.7026300605774,-5.20027855752496,
12.4925839478117));
#158542=CARTESIAN_POINT('Ctrl Pts',(-4.83936766137271,-5.07662626759507,
12.4842156945848));
#158543=CARTESIAN_POINT('Ctrl Pts',(-4.97118516849557,-4.94761395844923,
12.4758474413579));
#158544=CARTESIAN_POINT('Ctrl Pts',(-5.0976681723013,-4.81366863915729,
12.467479188131));
#158545=CARTESIAN_POINT('Ctrl Pts',(-5.22426844389627,-4.67959913344503,
12.4591031763396));
#158546=CARTESIAN_POINT('Ctrl Pts',(-5.34552410293513,-4.54058771745697,
12.4507271645481));
#158547=CARTESIAN_POINT('Ctrl Pts',(-5.46105945238373,-4.39709633963487,
12.4423511527566));
#158548=CARTESIAN_POINT('Ctrl Pts',(-5.57665146179558,-4.2535345918677,
12.4339710332655));
#158549=CARTESIAN_POINT('Ctrl Pts',(-5.68651736631649,-4.10548876099445,
12.4255909137743));
#158550=CARTESIAN_POINT('Ctrl Pts',(-5.79032377510463,-3.95345129500264,
12.4172107942831));
#158551=CARTESIAN_POINT('Ctrl Pts',(-5.89424879586417,-3.80124010694706,
12.4088210994439));
#158552=CARTESIAN_POINT('Ctrl Pts',(-5.99210030578865,-3.64502844530348,
12.4004314046047));
#158553=CARTESIAN_POINT('Ctrl Pts',(-6.0835893010936,-3.48533610690842,
12.3920417097655));
#158554=CARTESIAN_POINT('Ctrl Pts',(-6.14167408541145,-3.38395019702961,
12.3867152372908));
#158555=CARTESIAN_POINT('Ctrl Pts',(-6.19719521531832,-3.28116181132902,
12.3813887648161));
#158556=CARTESIAN_POINT('Ctrl Pts',(-6.25008864931608,-3.17710850274118,
12.3760622923414));
#158557=CARTESIAN_POINT('Ctrl Pts',(-6.3333174206817,-3.01337874697112,
12.3676809919366));
#158558=CARTESIAN_POINT('Ctrl Pts',(-6.41020567117949,-2.84618575687497,
12.3592996915317));
#158559=CARTESIAN_POINT('Ctrl Pts',(-6.48046315699108,-2.67604630628494,
12.3509183911268));
#158560=CARTESIAN_POINT('Ctrl Pts',(-6.55063160172435,-2.50612248254191,
12.3425477127933));
#158561=CARTESIAN_POINT('Ctrl Pts',(-6.61418590507734,-2.33325994058392,
12.3341770344597));
#158562=CARTESIAN_POINT('Ctrl Pts',(-6.67088178962721,-2.15799970141799,
12.3258063561262));
#158563=CARTESIAN_POINT('Ctrl Pts',(-6.72751333408258,-1.982938352532,12.3174451770753));
#158564=CARTESIAN_POINT('Ctrl Pts',(-6.77730187212974,-1.8054850394893,
12.3090839980245));
#158565=CARTESIAN_POINT('Ctrl Pts',(-6.82005113331303,-1.62620081831723,
12.3007228189736));
#158566=CARTESIAN_POINT('Ctrl Pts',(-6.86274492228703,-1.44714923957134,
12.2923724895389));
#158567=CARTESIAN_POINT('Ctrl Pts',(-6.89841757807405,-1.2662718087306,
12.2840221601042));
#158568=CARTESIAN_POINT('Ctrl Pts',(-6.92692260572578,-1.08414472132883,
12.2756718306695));
#158569=CARTESIAN_POINT('Ctrl Pts',(-6.95540570046406,-0.902157769824967,
12.2673279263137));
#158570=CARTESIAN_POINT('Ctrl Pts',(-6.97673210713019,-0.718923400261605,
12.258984021958));
#158571=CARTESIAN_POINT('Ctrl Pts',(-6.99080613463866,-0.535029111729923,
12.2506401176022));
#158572=CARTESIAN_POINT('Ctrl Pts',(-7.00486885780036,-0.351282528239018,
12.2423029151225));
#158573=CARTESIAN_POINT('Ctrl Pts',(-7.01169079431758,-0.166877408640384,
12.2339657126428));
#158574=CARTESIAN_POINT('Ctrl Pts',(-7.01122792897932,0.0175923392535826,
12.2256285101631));
#158575=CARTESIAN_POINT('Ctrl Pts',(-7.01107555626492,0.0783187620109528,
12.2228839491271));
#158576=CARTESIAN_POINT('Ctrl Pts',(-7.01013415446048,0.139052146388286,
12.2201393880911));
#158577=CARTESIAN_POINT('Ctrl Pts',(-7.00840338632723,0.199771211682296,
12.217394827055));
#158578=CARTESIAN_POINT('Ctrl Pts',(-7.00314510219136,0.384243118488874,
12.2090565167531));
#158579=CARTESIAN_POINT('Ctrl Pts',(-6.9906012745149,0.568431470743603,
12.2007182064512));
#158580=CARTESIAN_POINT('Ctrl Pts',(-6.97083272321711,0.751743112655893,
12.1923798961493));
#158581=CARTESIAN_POINT('Ctrl Pts',(-6.95105173421761,0.935170088033341,
12.1840363396655));
#158582=CARTESIAN_POINT('Ctrl Pts',(-6.92403699006066,1.11771892707913,
12.1756927831817));
#158583=CARTESIAN_POINT('Ctrl Pts',(-6.88990082146475,1.2988045399056,12.1673492266979));
#158584=CARTESIAN_POINT('Ctrl Pts',(-6.85573868222082,1.48002792187567,
12.1589993224727));
#158585=CARTESIAN_POINT('Ctrl Pts',(-6.814444372126,1.65978553550783,12.1506494182475));
#158586=CARTESIAN_POINT('Ctrl Pts',(-6.76618076614808,1.83750493939686,
12.1422995140224));
#158587=CARTESIAN_POINT('Ctrl Pts',(-6.71784476833251,2.01549090924115,
12.1339370855587));
#158588=CARTESIAN_POINT('Ctrl Pts',(-6.66251867134186,2.19143224369496,
12.1255746570951));
#158589=CARTESIAN_POINT('Ctrl Pts',(-6.60041491324351,2.36477261814593,
12.1172122286315));
#158590=CARTESIAN_POINT('Ctrl Pts',(-6.53825804796553,2.5382612222481,12.1088426491515));
#158591=CARTESIAN_POINT('Ctrl Pts',(-6.46931207971429,2.70914412541343,
12.1004730696715));
#158592=CARTESIAN_POINT('Ctrl Pts',(-6.39383680120533,2.87688677602237,
12.0921034901915));
#158593=CARTESIAN_POINT('Ctrl Pts',(-6.31824511127568,3.044888149231,12.0837210016549));
#158594=CARTESIAN_POINT('Ctrl Pts',(-6.23610413273646,3.20973929851901,
12.0753385131184));
#158595=CARTESIAN_POINT('Ctrl Pts',(-6.14771929896308,3.37093072958447,
12.0669560245818));
#158596=CARTESIAN_POINT('Ctrl Pts',(-6.11879833308085,3.42367520710767,
12.0642131369774));
#158597=CARTESIAN_POINT('Ctrl Pts',(-6.08920917596683,3.47602807320811,
12.061470249373));
#158598=CARTESIAN_POINT('Ctrl Pts',(-6.05896350698819,3.52797219142744,
12.0587273617686));
#158599=CARTESIAN_POINT('Ctrl Pts',(-5.96644904131399,3.68685716584719,
12.0503375066358));
#158600=CARTESIAN_POINT('Ctrl Pts',(-5.8676022527814,3.84223642542365,12.041947651503));
#158601=CARTESIAN_POINT('Ctrl Pts',(-5.76271213654621,3.9935917910827,12.0335577963702));
#158602=CARTESIAN_POINT('Ctrl Pts',(-5.65791881144004,4.14480748813185,
12.0251756832781));
#158603=CARTESIAN_POINT('Ctrl Pts',(-5.5470934621099,4.29200642462559,12.0167935701861));
#158604=CARTESIAN_POINT('Ctrl Pts',(-5.43056966892561,4.43469724259111,
12.008411457094));
#158605=CARTESIAN_POINT('Ctrl Pts',(-5.31413627350797,4.57727736272478,
12.0000358467451));
#158606=CARTESIAN_POINT('Ctrl Pts',(-5.19201345511139,4.71535608326778,
11.9916602363962));
#158607=CARTESIAN_POINT('Ctrl Pts',(-5.06457682105126,4.8484727684262,11.9832846260474));
#158608=CARTESIAN_POINT('Ctrl Pts',(-4.93722034652608,4.98150572121318,
11.9749142840817));
#158609=CARTESIAN_POINT('Ctrl Pts',(-4.80455694765846,5.10958262515248,
11.9665439421161));
#158610=CARTESIAN_POINT('Ctrl Pts',(-4.66700135664109,5.23227721930043,
11.9581736001505));
#158611=CARTESIAN_POINT('Ctrl Pts',(-4.52951212602849,5.3549126223761,11.9498072962562));
#158612=CARTESIAN_POINT('Ctrl Pts',(-4.38713565460876,5.47217067521171,
11.9414409923618));
#158613=CARTESIAN_POINT('Ctrl Pts',(-4.2403225777862,5.58366286579129,11.9330746884675));
#158614=CARTESIAN_POINT('Ctrl Pts',(-4.09355056046649,5.69512387512997,
11.9247107243939));
#158615=CARTESIAN_POINT('Ctrl Pts',(-3.94234467250142,5.80082203787308,
11.9163467603203));
#158616=CARTESIAN_POINT('Ctrl Pts',(-3.78718802054721,5.90040960099583,
11.9079827962466));
#158617=CARTESIAN_POINT('Ctrl Pts',(-3.63205524462364,5.99998183924736,
11.8996201192481));
#158618=CARTESIAN_POINT('Ctrl Pts',(-3.47297319336155,6.0934451752122,11.8912574422496));
#158619=CARTESIAN_POINT('Ctrl Pts',(-3.31045364576519,6.18049538643465,
11.882894765251));
#158620=CARTESIAN_POINT('Ctrl Pts',(-3.1479374441493,6.26754380545233,11.8745322604248));
#158621=CARTESIAN_POINT('Ctrl Pts',(-2.98198417721538,6.34817920818327,
11.8661697555985));
#158622=CARTESIAN_POINT('Ctrl Pts',(-2.81313026979454,6.42214330637878,
11.8578072507722));
#158623=CARTESIAN_POINT('Ctrl Pts',(-2.64425733174284,6.49611574067661,
11.8494438034522));
#158624=CARTESIAN_POINT('Ctrl Pts',(-2.47248340266625,6.56341524002416,
11.8410803561322));
#158625=CARTESIAN_POINT('Ctrl Pts',(-2.29836532333641,6.62383147453079,
11.8327169088122));
#158626=CARTESIAN_POINT('Ctrl Pts',(-2.12414471838836,6.68428328381413,
11.8243485368594));
#158627=CARTESIAN_POINT('Ctrl Pts',(-1.94757751552225,6.73784362052027,
11.8159801649066));
#158628=CARTESIAN_POINT('Ctrl Pts',(-1.76923716564556,6.7843515839171,11.8076117929538));
#158629=CARTESIAN_POINT('Ctrl Pts',(-1.59084338033919,6.83087348231524,
11.7992409136181));
#158630=CARTESIAN_POINT('Ctrl Pts',(-1.41067570807971,6.87033871615299,
11.7908700342824));
#158631=CARTESIAN_POINT('Ctrl Pts',(-1.22931896518636,6.90263728181723,
11.7824991549466));
#158632=CARTESIAN_POINT('Ctrl Pts',(-1.04780856068579,6.93496321370691,
11.7741211830553));
#158633=CARTESIAN_POINT('Ctrl Pts',(-0.86510739717594,6.96011029163034,
11.7657432111641));
#158634=CARTESIAN_POINT('Ctrl Pts',(-0.681807762688048,6.97802011585223,
11.7573652392728));
#158635=CARTESIAN_POINT('Ctrl Pts',(-0.565319352356048,6.98940195498553,
11.7520409699138));
#158636=CARTESIAN_POINT('Ctrl Pts',(-0.448589341809831,6.99786192559897,
11.7467167005548));
#158637=CARTESIAN_POINT('Ctrl Pts',(-0.331770083393816,7.00339597440162,
11.7413924311957));
#158638=CARTESIAN_POINT('Ctrl Pts',(-0.159252495224037,7.01156860591114,
11.7335296000065));
#158639=CARTESIAN_POINT('Ctrl Pts',(0.0138185171071441,7.01337428630965,
11.7256667688172));
#158640=CARTESIAN_POINT('Ctrl Pts',(0.186913749324534,7.00875807920444,
11.7178039376279));
#158641=CARTESIAN_POINT('Ctrl Pts',(0.359875980703924,7.00414541904506,
11.7099471479865));
#158642=CARTESIAN_POINT('Ctrl Pts',(0.532862016288809,6.99312069419079,
11.7020903583451));
#158643=CARTESIAN_POINT('Ctrl Pts',(0.705338861365815,6.97568087380345,
11.6942335687038));
#158644=CARTESIAN_POINT('Ctrl Pts',(0.8777184376647,6.95825088864945,11.6863812099199));
#158645=CARTESIAN_POINT('Ctrl Pts',(1.04958901652641,6.93441304285293,11.6785288511361));
#158646=CARTESIAN_POINT('Ctrl Pts',(1.22041919639701,6.90421636013572,11.6706764923522));
#158647=CARTESIAN_POINT('Ctrl Pts',(1.3912090412712,6.87402680720722,11.6628259876018));
#158648=CARTESIAN_POINT('Ctrl Pts',(1.56095859948777,6.83748146354932,11.6549754828514));
#158649=CARTESIAN_POINT('Ctrl Pts',(1.72914324074419,6.79468102382214,11.6471249781009));
#158650=CARTESIAN_POINT('Ctrl Pts',(1.8973008263928,6.75188746933669,11.6392757362493));
#158651=CARTESIAN_POINT('Ctrl Pts',(2.06389362723065,6.70284091893477,11.6314264943976));
#158652=CARTESIAN_POINT('Ctrl Pts',(2.228409290684,6.647692727232,11.623577252546));
#158653=CARTESIAN_POINT('Ctrl Pts',(2.39298038268426,6.59252595502409,11.6157253661311));
#158654=CARTESIAN_POINT('Ctrl Pts',(2.55547257737388,6.53125355662401,11.6078734797163));
#158655=CARTESIAN_POINT('Ctrl Pts',(2.71539053085719,6.46407617741554,11.6000215933014));
#158656=CARTESIAN_POINT('Ctrl Pts',(2.8328162936427,6.41474866400218,11.5942560508374));
#158657=CARTESIAN_POINT('Ctrl Pts',(2.94885442458848,6.36223834779299,11.5884905083733));
#158658=CARTESIAN_POINT('Ctrl Pts',(3.06331649493972,6.30664083441655,11.5827249659093));
#158659=CARTESIAN_POINT('Ctrl Pts',(3.25500116881123,6.21353408571868,11.5730696615494));
#158660=CARTESIAN_POINT('Ctrl Pts',(3.44216773557614,6.11181628211994,11.5634143571894));
#158661=CARTESIAN_POINT('Ctrl Pts',(3.62414572571811,6.00193254887617,11.5537590528295));
#158662=CARTESIAN_POINT('Ctrl Pts',(3.80713183978237,5.89144008036685,11.5440502598949));
#158663=CARTESIAN_POINT('Ctrl Pts',(3.98487171840446,5.7726910273947,11.5343414669603));
#158664=CARTESIAN_POINT('Ctrl Pts',(4.15671982593661,5.64617630358507,11.5246326740258));
#158665=CARTESIAN_POINT('Ctrl Pts',(4.32939488115642,5.51905278018019,11.5148771615551));
#158666=CARTESIAN_POINT('Ctrl Pts',(4.49612130483396,5.38408871295277,11.5051216490844));
#158667=CARTESIAN_POINT('Ctrl Pts',(4.65628081751959,5.24181986631543,11.4953661366138));
#158668=CARTESIAN_POINT('Ctrl Pts',(4.8165989127633,5.09941015163187,11.4856009646848));
#158669=CARTESIAN_POINT('Ctrl Pts',(4.97033706978391,4.94968122399424,11.4758357927559));
#158670=CARTESIAN_POINT('Ctrl Pts',(5.11691201234755,4.79320748772608,11.466070620827));
#158671=CARTESIAN_POINT('Ctrl Pts',(5.2632871033026,4.63694709984714,11.4563187634885));
#158672=CARTESIAN_POINT('Ctrl Pts',(5.40251847437296,4.47396031134541,11.44656690615));
#158673=CARTESIAN_POINT('Ctrl Pts',(5.53406224469293,4.30485558809634,11.4368150488114));
#158674=CARTESIAN_POINT('Ctrl Pts',(5.59142485540756,4.23111368161041,11.4325625327485));
#158675=CARTESIAN_POINT('Ctrl Pts',(5.64732607623393,4.15620885907853,11.4283100166857));
#158676=CARTESIAN_POINT('Ctrl Pts',(5.70172304235996,4.08019373445936,11.4240575006228));
#158677=CARTESIAN_POINT('Ctrl Pts',(5.8044781167715,3.9366022744403,11.4160245598985));
#158678=CARTESIAN_POINT('Ctrl Pts',(5.90191268951564,3.78897669783169,11.4079916191741));
#158679=CARTESIAN_POINT('Ctrl Pts',(5.99369301470647,3.63775626010855,11.3999586784497));
#158680=CARTESIAN_POINT('Ctrl Pts',(6.08541671766824,3.48662911512809,11.3919306935044));
#158681=CARTESIAN_POINT('Ctrl Pts',(6.17149292580616,3.33191183475777,11.383902708559));
#158682=CARTESIAN_POINT('Ctrl Pts',(6.25163034420859,3.17407381796177,11.3758747236137));
#158683=CARTESIAN_POINT('Ctrl Pts',(6.33173144170547,3.01630733853015,11.3678503772143));
#158684=CARTESIAN_POINT('Ctrl Pts',(6.40589894333775,2.85542326519043,11.359826030815));
#158685=CARTESIAN_POINT('Ctrl Pts',(6.47388683555362,2.69191675260317,11.3518016844156));
#158686=CARTESIAN_POINT('Ctrl Pts',(6.50784377946204,2.610252484222,11.3477938784416));
#158687=CARTESIAN_POINT('Ctrl Pts',(6.54025990091052,2.52793441510125,11.3437860724676));
#158688=CARTESIAN_POINT('Ctrl Pts',(6.57110895151813,2.44502632087638,11.3397782664936));
#158689=CARTESIAN_POINT('Origin',(0.,0.,50.));
#158690=CARTESIAN_POINT('',(6.57110895151814,2.44502632087636,9.34006375887581));
#158691=CARTESIAN_POINT('',(6.57110895151814,2.44502632087636,9.88705365892876));
#158692=CARTESIAN_POINT('',(6.57110895151814,2.44502632087636,50.));
#158693=CARTESIAN_POINT('',(7.01124965431583,-0.00220167122712491,11.7735343569358));
#158694=CARTESIAN_POINT('Ctrl Pts',(6.57110895151814,2.44502632087636,9.88705365892876));
#158695=CARTESIAN_POINT('Ctrl Pts',(6.51065965303537,2.60748630054266,9.8949044975378));
#158696=CARTESIAN_POINT('Ctrl Pts',(6.44414243043556,2.7678078587859,9.90275533614685));
#158697=CARTESIAN_POINT('Ctrl Pts',(6.37174455141127,2.92549105861918,9.91060617475588));
#158698=CARTESIAN_POINT('Ctrl Pts',(6.29935684248814,3.08315210788516,9.91845591051738));
#158699=CARTESIAN_POINT('Ctrl Pts',(6.2210902739352,3.23817518699505,9.92630564627888));
#158700=CARTESIAN_POINT('Ctrl Pts',(6.13718012638381,3.39008062718567,9.93415538204038));
#158701=CARTESIAN_POINT('Ctrl Pts',(6.05327630085696,3.54197462239677,9.94200452638089));
#158702=CARTESIAN_POINT('Ctrl Pts',(5.96372993185385,3.69075111486342,9.9498536707214));
#158703=CARTESIAN_POINT('Ctrl Pts',(5.8688218592914,3.83595575396842,9.95770281506191));
#158704=CARTESIAN_POINT('Ctrl Pts',(5.77388295702589,3.98120756098849,9.96555450909901));
#158705=CARTESIAN_POINT('Ctrl Pts',(5.67357908796459,4.12288488234006,9.97340620313612));
#158706=CARTESIAN_POINT('Ctrl Pts',(5.56823396672836,4.26056299733645,9.98125789717322));
#158707=CARTESIAN_POINT('Ctrl Pts',(5.5400850383453,4.29735152017898,9.98335592288663));
#158708=CARTESIAN_POINT('Ctrl Pts',(5.51157639205649,4.33385468224104,9.98545394860006));
#158709=CARTESIAN_POINT('Ctrl Pts',(5.4827146855865,4.37006478658545,9.98755197431347));
#158710=CARTESIAN_POINT('Ctrl Pts',(5.34989049828849,4.53670696647608,9.99720727867339));
#158711=CARTESIAN_POINT('Ctrl Pts',(5.20965370605441,4.6970549548862,10.0068625830333));
#158712=CARTESIAN_POINT('Ctrl Pts',(5.0625854570575,4.85055203585014,10.0165178873932));
#158713=CARTESIAN_POINT('Ctrl Pts',(4.91470247755025,5.0048994618475,10.026226680328));
#158714=CARTESIAN_POINT('Ctrl Pts',(4.7599122137965,5.15231986845307,10.0359354732628));
#158715=CARTESIAN_POINT('Ctrl Pts',(4.59883503057595,5.2922908956375,10.0456442661976));
#158716=CARTESIAN_POINT('Ctrl Pts',(4.43698273027387,5.43293547528864,10.0553997786683));
#158717=CARTESIAN_POINT('Ctrl Pts',(4.26878290693983,5.56605879866049,10.065155291139));
#158718=CARTESIAN_POINT('Ctrl Pts',(4.0948937185639,5.69117492229557,10.0749108036097));
#158719=CARTESIAN_POINT('Ctrl Pts',(3.92083235313834,5.81641493014236,10.0846759755387));
#158720=CARTESIAN_POINT('Ctrl Pts',(3.74107039234043,5.93363186640219,10.0944411474676));
#158721=CARTESIAN_POINT('Ctrl Pts',(3.55629603071652,6.04238240302697,10.1042063193966));
#158722=CARTESIAN_POINT('Ctrl Pts',(3.37177360474307,6.15098466076206,10.1139581767351));
#158723=CARTESIAN_POINT('Ctrl Pts',(3.18225246996649,6.25114357144574,10.1237100340737));
#158724=CARTESIAN_POINT('Ctrl Pts',(2.98844542841549,6.34246170535405,10.1334618914122));
#158725=CARTESIAN_POINT('Ctrl Pts',(2.90393152212869,6.38228302531048,10.1377144074748));
#158726=CARTESIAN_POINT('Ctrl Pts',(2.81860296076509,6.42042375869067,10.1419669235373));
#158727=CARTESIAN_POINT('Ctrl Pts',(2.7325204682249,6.45685360320582,10.1462194395999));
#158728=CARTESIAN_POINT('Ctrl Pts',(2.56990977430587,6.52566994577636,10.1542524851987));
#158729=CARTESIAN_POINT('Ctrl Pts',(2.40452796168643,6.58841133439484,10.1622855307975));
#158730=CARTESIAN_POINT('Ctrl Pts',(2.23687673117688,6.64484830918054,10.1703185763963));
#158731=CARTESIAN_POINT('Ctrl Pts',(2.0693332733334,6.70124900410584,10.1783464580441));
#158732=CARTESIAN_POINT('Ctrl Pts',(1.89952364747798,6.75135323577297,10.1863743396919));
#158733=CARTESIAN_POINT('Ctrl Pts',(1.72796962997545,6.79497958204309,10.1944022213397));
#158734=CARTESIAN_POINT('Ctrl Pts',(1.55649307080299,6.83858623058781,10.2024264783198));
#158735=CARTESIAN_POINT('Ctrl Pts',(1.38327404273015,6.87572072725005,10.2104507353));
#158736=CARTESIAN_POINT('Ctrl Pts',(1.20884953836834,6.90625146921879,10.2184749922801));
#158737=CARTESIAN_POINT('Ctrl Pts',(1.03444612370561,6.93677851970986,10.2264982790458));
#158738=CARTESIAN_POINT('Ctrl Pts',(0.858837882611601,6.96070333514612,
10.2345215658114));
#158739=CARTESIAN_POINT('Ctrl Pts',(0.682572236592608,6.9779453784286,10.2425448525771));
#158740=CARTESIAN_POINT('Ctrl Pts',(0.506321033970898,6.99518600887944,
10.2505674819061));
#158741=CARTESIAN_POINT('Ctrl Pts',(0.329412899019472,7.00574492623494,
10.258590111235));
#158742=CARTESIAN_POINT('Ctrl Pts',(0.152400312836698,7.00959347659672,
10.2666127405639));
#158743=CARTESIAN_POINT('Ctrl Pts',(-0.0246788174764194,7.01344347373945,
10.2746383858303));
#158744=CARTESIAN_POINT('Ctrl Pts',(-0.201862110666864,7.01057805956247,
10.2826640310967));
#158745=CARTESIAN_POINT('Ctrl Pts',(-0.378596758129559,7.00102071538385,
10.2906896763631));
#158746=CARTESIAN_POINT('Ctrl Pts',(-0.482810275951469,6.99538512286033,
10.2954220858709));
#158747=CARTESIAN_POINT('Ctrl Pts',(-0.586867832603589,6.98742373395397,
10.3001544953786));
#158748=CARTESIAN_POINT('Ctrl Pts',(-0.690656921212897,6.97714981777522,
10.3048869048864));
#158749=CARTESIAN_POINT('Ctrl Pts',(-0.882120447473759,6.95819714898846,
10.313616953721));
#158750=CARTESIAN_POINT('Ctrl Pts',(-1.07276576003735,6.93136281656233,
10.3223470025557));
#158751=CARTESIAN_POINT('Ctrl Pts',(-1.26195338715803,6.89674562465083,
10.3310770513904));
#158752=CARTESIAN_POINT('Ctrl Pts',(-1.45119571811682,6.86211842313516,
10.3398096245295));
#158753=CARTESIAN_POINT('Ctrl Pts',(-1.63897925284441,6.81970391947392,
10.3485421976687));
#158754=CARTESIAN_POINT('Ctrl Pts',(-1.82467467174844,6.76965205197281,
10.3572747708079));
#158755=CARTESIAN_POINT('Ctrl Pts',(-2.01300819050361,6.71888911779606,
10.3661314040883));
#158756=CARTESIAN_POINT('Ctrl Pts',(-2.19919353136163,6.66027023944923,
10.3749880373687));
#158757=CARTESIAN_POINT('Ctrl Pts',(-2.3825896053187,6.59400434752111,10.3838446706491));
#158758=CARTESIAN_POINT('Ctrl Pts',(-2.56353185180905,6.52862508889005,
10.3925828027558));
#158759=CARTESIAN_POINT('Ctrl Pts',(-2.74175875492087,6.45580229510021,
10.4013209348626));
#158760=CARTESIAN_POINT('Ctrl Pts',(-2.91667336898161,6.37578567873588,
10.4100590669694));
#158761=CARTESIAN_POINT('Ctrl Pts',(-3.09514610967642,6.29414135816064,
10.4189749508366));
#158762=CARTESIAN_POINT('Ctrl Pts',(-3.27017008925038,6.20500752522851,
10.4278908347038));
#158763=CARTESIAN_POINT('Ctrl Pts',(-3.4411352453449,6.10869992598631,10.4368067185711));
#158764=CARTESIAN_POINT('Ctrl Pts',(-3.61210040143944,6.0123923267441,10.4457226024383));
#158765=CARTESIAN_POINT('Ctrl Pts',(-3.77900647355707,5.90891111491626,
10.4546384863055));
#158766=CARTESIAN_POINT('Ctrl Pts',(-3.94127167045108,5.79862088622802,
10.4635543701728));
#158767=CARTESIAN_POINT('Ctrl Pts',(-4.10034831522184,5.69049788840374,
10.472295054669));
#158768=CARTESIAN_POINT('Ctrl Pts',(-4.25498167604603,5.5758195038425,10.4810357391652));
#158769=CARTESIAN_POINT('Ctrl Pts',(-4.40465029916485,5.45496858877914,
10.4897764236614));
#158770=CARTESIAN_POINT('Ctrl Pts',(-4.55429199441221,5.33413941680285,
10.4985155355633));
#158771=CARTESIAN_POINT('Ctrl Pts',(-4.69897052287586,5.20714010410245,
10.5072546474651));
#158772=CARTESIAN_POINT('Ctrl Pts',(-4.8381969723823,5.07439421201495,10.515993759367));
#158773=CARTESIAN_POINT('Ctrl Pts',(-4.979227300924,4.93992840584069,10.5248460990414));
#158774=CARTESIAN_POINT('Ctrl Pts',(-5.11466306480168,4.79956625222048,
10.5336984387157));
#158775=CARTESIAN_POINT('Ctrl Pts',(-5.2440331497828,4.65378801477668,10.54255077839));
#158776=CARTESIAN_POINT('Ctrl Pts',(-5.37168303780633,4.50994814879311,
10.5512854110398));
#158777=CARTESIAN_POINT('Ctrl Pts',(-5.49342737628396,4.3608355561093,10.5600200436895));
#158778=CARTESIAN_POINT('Ctrl Pts',(-5.60885214401144,4.20694713410072,
10.5687546763393));
#158779=CARTESIAN_POINT('Ctrl Pts',(-5.72661009045162,4.04994803491747,
10.5776658695259));
#158780=CARTESIAN_POINT('Ctrl Pts',(-5.83779006784455,3.88797819357438,
10.5865770627126));
#158781=CARTESIAN_POINT('Ctrl Pts',(-5.94199644076384,3.72159977166404,
10.5954882558992));
#158782=CARTESIAN_POINT('Ctrl Pts',(-6.04620281368313,3.55522134975372,
10.6043994490859));
#158783=CARTESIAN_POINT('Ctrl Pts',(-6.14343540980711,3.38443459702493,
10.6133106422725));
#158784=CARTESIAN_POINT('Ctrl Pts',(-6.23334574516419,3.20983292146858,
10.6222218354592));
#158785=CARTESIAN_POINT('Ctrl Pts',(-6.31432145775723,3.05258186638172,
10.6302475003116));
#158786=CARTESIAN_POINT('Ctrl Pts',(-6.389394618327,2.89216390866958,10.638273165164));
#158787=CARTESIAN_POINT('Ctrl Pts',(-6.45831249077014,2.72907059895166,
10.6462988300164));
#158788=CARTESIAN_POINT('Ctrl Pts',(-6.527208490371,2.56602905104989,10.6543219477196));
#158789=CARTESIAN_POINT('Ctrl Pts',(-6.58995294864002,2.40031417886261,
10.6623450654229));
#158790=CARTESIAN_POINT('Ctrl Pts',(-6.64634038845737,2.23243947359392,
10.6703681831261));
#158791=CARTESIAN_POINT('Ctrl Pts',(-6.70272071732504,2.06458593879488,
10.678390289044));
#158792=CARTESIAN_POINT('Ctrl Pts',(-6.75274550846172,1.89457346103339,
10.6864123949619));
#158793=CARTESIAN_POINT('Ctrl Pts',(-6.79625849657452,1.7229326772218,10.6944345008797));
#158794=CARTESIAN_POINT('Ctrl Pts',(-6.83978765426074,1.55122811111492,
10.7024595878393));
#158795=CARTESIAN_POINT('Ctrl Pts',(-6.87680008183852,1.37789438511657,
10.7104846747988));
#158796=CARTESIAN_POINT('Ctrl Pts',(-6.90719008977021,1.20347481331362,
10.7185097617583));
#158797=CARTESIAN_POINT('Ctrl Pts',(-6.93758608286187,1.0290208904489,10.7265364292186));
#158798=CARTESIAN_POINT('Ctrl Pts',(-6.96135700378002,0.853481058385692,
10.7345630966788));
#158799=CARTESIAN_POINT('Ctrl Pts',(-6.97844883767682,0.677405626214464,
10.7425897641391));
#158800=CARTESIAN_POINT('Ctrl Pts',(-6.99555439283766,0.501188841306668,
10.7506228753797));
#158801=CARTESIAN_POINT('Ctrl Pts',(-7.0059701256658,0.324435963199458,
10.7586559866203));
#158802=CARTESIAN_POINT('Ctrl Pts',(-7.00969409651,0.147699816698825,10.7666890978609));
#158803=CARTESIAN_POINT('Ctrl Pts',(-7.011888395412,0.0435604588911374,
10.7714224988225));
#158804=CARTESIAN_POINT('Ctrl Pts',(-7.01176030669969,-0.0605730947154226,
10.7761558997841));
#158805=CARTESIAN_POINT('Ctrl Pts',(-7.00931788707195,-0.16458833638283,
10.7808893007457));
#158806=CARTESIAN_POINT('Ctrl Pts',(-7.00428642662564,-0.378862971387192,
10.7906402540398));
#158807=CARTESIAN_POINT('Ctrl Pts',(-6.98942851048065,-0.592761598645687,
10.8003912073339));
#158808=CARTESIAN_POINT('Ctrl Pts',(-6.96482894103385,-0.80547152937722,
10.810142160628));
#158809=CARTESIAN_POINT('Ctrl Pts',(-6.94019393129247,-1.01848790866763,
10.8199071619996));
#158810=CARTESIAN_POINT('Ctrl Pts',(-6.90578919919927,-1.23031212746868,
10.8296721633712));
#158811=CARTESIAN_POINT('Ctrl Pts',(-6.86175136652627,-1.44013705822569,
10.8394371647427));
#158812=CARTESIAN_POINT('Ctrl Pts',(-6.81778693579589,-1.6496122542979,
10.8491858898803));
#158813=CARTESIAN_POINT('Ctrl Pts',(-6.76422150246063,-1.85709478533727,
10.8589346150178));
#158814=CARTESIAN_POINT('Ctrl Pts',(-6.7012419681505,-2.06179112588993,
10.8686833401554));
#158815=CARTESIAN_POINT('Ctrl Pts',(-6.63843528824183,-2.26592565435847,
10.8784053088225));
#158816=CARTESIAN_POINT('Ctrl Pts',(-6.56626610055865,-2.46728922018291,
10.8881272774896));
#158817=CARTESIAN_POINT('Ctrl Pts',(-6.48497048630068,-2.66510494245707,
10.8978492461567));
#158818=CARTESIAN_POINT('Ctrl Pts',(-6.404212783889,-2.8616117697636,10.9075068870964));
#158819=CARTESIAN_POINT('Ctrl Pts',(-6.3144490211031,-3.05461749449963,
10.9171645280361));
#158820=CARTESIAN_POINT('Ctrl Pts',(-6.2159608466107,-3.24337128862897,
10.9268221689757));
#158821=CARTESIAN_POINT('Ctrl Pts',(-6.17267190317865,-3.32633507954867,
10.9310670346612));
#158822=CARTESIAN_POINT('Ctrl Pts',(-6.12769814221123,-3.40847758269322,
10.9353119003466));
#158823=CARTESIAN_POINT('Ctrl Pts',(-6.08106659565566,-3.48973575241749,
10.9395567660321));
#158824=CARTESIAN_POINT('Ctrl Pts',(-5.99481091721748,-3.64004126608645,
10.947408613046));
#158825=CARTESIAN_POINT('Ctrl Pts',(-5.90291526748711,-3.78725741194914,
10.9552604600599));
#158826=CARTESIAN_POINT('Ctrl Pts',(-5.80564328722662,-3.93092006837845,
10.9631123070738));
#158827=CARTESIAN_POINT('Ctrl Pts',(-5.70839889251332,-4.07454198323987,
10.9709619273674));
#158828=CARTESIAN_POINT('Ctrl Pts',(-5.60578141378705,-4.21461209767843,
10.978811547661));
#158829=CARTESIAN_POINT('Ctrl Pts',(-5.49809867869906,-4.35069390807808,
10.9866611679546));
#158830=CARTESIAN_POINT('Ctrl Pts',(-5.39042454070015,-4.48676485408572,
10.9945101615564));
#158831=CARTESIAN_POINT('Ctrl Pts',(-5.27768618867854,-4.61884783125907,
11.0023591551582));
#158832=CARTESIAN_POINT('Ctrl Pts',(-5.16023255287026,-4.74653837683823,
11.01020814876));
#158833=CARTESIAN_POINT('Ctrl Pts',(-5.0427194537255,-4.87429356840152,
11.0180611160774));
#158834=CARTESIAN_POINT('Ctrl Pts',(-4.92048655961227,-4.99765160406667,
11.0259140833949));
#158835=CARTESIAN_POINT('Ctrl Pts',(-4.79392081656102,-5.11624371654077,
11.0337670507123));
#158836=CARTESIAN_POINT('Ctrl Pts',(-4.66732293006375,-5.23486594742664,
11.0416220124196));
#158837=CARTESIAN_POINT('Ctrl Pts',(-4.5363902902682,-5.34871959341548,
11.0494769741268));
#158838=CARTESIAN_POINT('Ctrl Pts',(-4.40154341618671,-5.45747580094712,
11.0573319358341));
#158839=CARTESIAN_POINT('Ctrl Pts',(-4.2665626953109,-5.56633995810563,
11.0651946942474));
#158840=CARTESIAN_POINT('Ctrl Pts',(-4.12766028588765,-5.67009634324284,
11.0730574526608));
#158841=CARTESIAN_POINT('Ctrl Pts',(-3.98528667243108,-5.76845878038868,
11.0809202110741));
#158842=CARTESIAN_POINT('Ctrl Pts',(-3.88084343254005,-5.84061605286124,
11.0866882178222));
#158843=CARTESIAN_POINT('Ctrl Pts',(-3.77453279139432,-5.90987148297041,
11.0924562245704));
#158844=CARTESIAN_POINT('Ctrl Pts',(-3.66654084010936,-5.97612791281363,
11.0982242313185));
#158845=CARTESIAN_POINT('Ctrl Pts',(-3.50968184488422,-6.07236579803331,
11.1066022977595));
#158846=CARTESIAN_POINT('Ctrl Pts',(-3.34892741293879,-6.16248813004605,
11.1149803642005));
#158847=CARTESIAN_POINT('Ctrl Pts',(-3.18478243728188,-6.24618182489759,
11.1233584306416));
#158848=CARTESIAN_POINT('Ctrl Pts',(-3.02074970200894,-6.32981829099504,
11.1317307682603));
#158849=CARTESIAN_POINT('Ctrl Pts',(-2.85333133717546,-6.40703473506373,
11.140103105879));
#158850=CARTESIAN_POINT('Ctrl Pts',(-2.68305808668067,-6.47756326607448,
11.1484754434978));
#158851=CARTESIAN_POINT('Ctrl Pts',(-2.51287629632694,-6.54805391356932,
11.1568432840204));
#158852=CARTESIAN_POINT('Ctrl Pts',(-2.33984298092115,-6.61186368525468,
11.1652111245429));
#158853=CARTESIAN_POINT('Ctrl Pts',(-2.16451059628573,-6.66877203397048,
11.1735789650655));
#158854=CARTESIAN_POINT('Ctrl Pts',(-1.98924670431963,-6.72565815174066,
11.1819435367354));
#158855=CARTESIAN_POINT('Ctrl Pts',(-1.811685846297,-6.77564812142816,11.1903081084054));
#158856=CARTESIAN_POINT('Ctrl Pts',(-1.63239787270859,-6.81857050617477,
11.1986726800753));
#158857=CARTESIAN_POINT('Ctrl Pts',(-1.45315369358812,-6.86148240631963,
11.2070352085409));
#158858=CARTESIAN_POINT('Ctrl Pts',(-1.27218355970473,-6.8973300883243,
11.2153977370064));
#158859=CARTESIAN_POINT('Ctrl Pts',(-1.09007025647918,-6.92599259301072,
11.223760265472));
#158860=CARTESIAN_POINT('Ctrl Pts',(-0.907942420042187,-6.95465738505472,
11.2321234612935));
#158861=CARTESIAN_POINT('Ctrl Pts',(-0.724671555735195,-6.97613579714141,
11.240486657115));
#158862=CARTESIAN_POINT('Ctrl Pts',(-0.540849134503035,-6.99035827237827,
11.2488498529365));
#158863=CARTESIAN_POINT('Ctrl Pts',(-0.357014176950271,-7.00458171755943,
11.2572136191112));
#158864=CARTESIAN_POINT('Ctrl Pts',(-0.17262791529241,-7.01154821358821,
11.2655773852859));
#158865=CARTESIAN_POINT('Ctrl Pts',(0.0117144055303785,-7.01124021377125,
11.2739411514606));
#158866=CARTESIAN_POINT('Ctrl Pts',(0.196093875297651,-7.01093215188569,
11.2823066031142));
#158867=CARTESIAN_POINT('Ctrl Pts',(0.380429057787402,-7.003346671542,11.2906720547678));
#158868=CARTESIAN_POINT('Ctrl Pts',(0.564125623979578,-6.98851835819794,
11.2990375064214));
#158869=CARTESIAN_POINT('Ctrl Pts',(0.747883709790392,-6.97368507888092,
11.3074057596482));
#158870=CARTESIAN_POINT('Ctrl Pts',(0.931002425250959,-6.95160415627133,
11.3157740128751));
#158871=CARTESIAN_POINT('Ctrl Pts',(1.11289303815448,-6.92236199921149,
11.324142266102));
#158872=CARTESIAN_POINT('Ctrl Pts',(1.29495228960569,-6.89309273050021,
11.3325182778934));
#158873=CARTESIAN_POINT('Ctrl Pts',(1.47578083823409,-6.85664901190681,
11.3408942896849));
#158874=CARTESIAN_POINT('Ctrl Pts',(1.65479938758511,-6.81316853962589,
11.3492703014764));
#158875=CARTESIAN_POINT('Ctrl Pts',(1.83390572984466,-6.76966674398412,
11.3576504209675));
#158876=CARTESIAN_POINT('Ctrl Pts',(2.01119998494268,-6.71912139677779,
11.3660305404587));
#158877=CARTESIAN_POINT('Ctrl Pts',(2.18611784614132,-6.66172014762572,
11.3744106599498));
#158878=CARTESIAN_POINT('Ctrl Pts',(2.36123557315379,-6.6042533102753,11.382800354789));
#158879=CARTESIAN_POINT('Ctrl Pts',(2.53397117006586,-6.53991502628123,
11.3911900496282));
#158880=CARTESIAN_POINT('Ctrl Pts',(2.70377888891536,-6.46894166632809,
11.3995797444674));
#158881=CARTESIAN_POINT('Ctrl Pts',(2.81158687928558,-6.42388190486252,
11.4049062169421));
#158882=CARTESIAN_POINT('Ctrl Pts',(2.91821513877765,-6.37614866300158,
11.4102326894167));
#158883=CARTESIAN_POINT('Ctrl Pts',(3.02352911297256,-6.32581206372015,
11.4155591618913));
#158884=CARTESIAN_POINT('Ctrl Pts',(3.18924254879002,-6.24660651784591,
11.4239404622962));
#158885=CARTESIAN_POINT('Ctrl Pts',(3.35203493321813,-6.16079312393665,
11.4323217627011));
#158886=CARTESIAN_POINT('Ctrl Pts',(3.51136137524599,-6.06860509960325,
11.440703063106));
#158887=CARTESIAN_POINT('Ctrl Pts',(3.67048589433233,-5.97653391009532,
11.4490737414396));
#158888=CARTESIAN_POINT('Ctrl Pts',(3.826152943663,-5.87810435335717,11.4574444197731));
#158889=CARTESIAN_POINT('Ctrl Pts',(3.9778393323686,-5.77359686922817,11.4658150981067));
#158890=CARTESIAN_POINT('Ctrl Pts',(4.12935358306614,-5.66920798315071,
11.4741762771575));
#158891=CARTESIAN_POINT('Ctrl Pts',(4.27689590857438,-5.55875510173029,
11.4825374562083));
#158892=CARTESIAN_POINT('Ctrl Pts',(4.41996900155504,-5.44256378812344,
11.4908986352591));
#158893=CARTESIAN_POINT('Ctrl Pts',(4.56285644032072,-5.32652324645188,
11.4992489646939));
#158894=CARTESIAN_POINT('Ctrl Pts',(4.70128596084793,-5.2047593305936,11.5075992941286));
#158895=CARTESIAN_POINT('Ctrl Pts',(4.83479052300556,-5.07763992039172,
11.5159496235633));
#158896=CARTESIAN_POINT('Ctrl Pts',(4.96819236138863,-4.95061832097192,
11.524293527919));
#158897=CARTESIAN_POINT('Ctrl Pts',(5.09667655682613,-4.81824966405888,
11.5326374322748));
#158898=CARTESIAN_POINT('Ctrl Pts',(5.21980948776443,-4.68094172938998,
11.5409813366305));
#158899=CARTESIAN_POINT('Ctrl Pts',(5.34284351756477,-4.54374408131044,
11.5493185391102));
#158900=CARTESIAN_POINT('Ctrl Pts',(5.46053463683438,-4.40161531083358,
11.5576557415899));
#158901=CARTESIAN_POINT('Ctrl Pts',(5.57248631467415,-4.25499974562506,
11.5659929440696));
#158902=CARTESIAN_POINT('Ctrl Pts',(5.60934018906037,-4.20673471085718,
11.5687375051057));
#158903=CARTESIAN_POINT('Ctrl Pts',(5.64557239156457,-4.15798373428186,
11.5714820661417));
#158904=CARTESIAN_POINT('Ctrl Pts',(5.68116969739712,-4.10876349183994,
11.5742266271778));
#158905=CARTESIAN_POINT('Ctrl Pts',(5.7893186429094,-3.95922640768553,11.5825649374797));
#158906=CARTESIAN_POINT('Ctrl Pts',(5.89151555911645,-3.80547827912205,
11.5909032477815));
#158907=CARTESIAN_POINT('Ctrl Pts',(5.98744753524082,-3.64802666865782,
11.5992415580834));
#158908=CARTESIAN_POINT('Ctrl Pts',(6.08343986850949,-3.49047599498278,
11.6075851145673));
#158909=CARTESIAN_POINT('Ctrl Pts',(6.17315922902922,-3.32921747152846,
11.6159286710511));
#158910=CARTESIAN_POINT('Ctrl Pts',(6.25633847895222,-3.16478362598168,
11.6242722275349));
#158911=CARTESIAN_POINT('Ctrl Pts',(6.33958101128566,-3.00022467988263,
11.63262213176));
#158912=CARTESIAN_POINT('Ctrl Pts',(6.41627336041963,-2.83248588505753,
11.6409720359852));
#158913=CARTESIAN_POINT('Ctrl Pts',(6.48619618491797,-2.66212051065604,
11.6493219402104));
#158914=CARTESIAN_POINT('Ctrl Pts',(6.55622388847894,-2.49149960079956,
11.6576843686741));
#158915=CARTESIAN_POINT('Ctrl Pts',(6.61946165243177,-2.31824454203393,
11.6660467971377));
#158916=CARTESIAN_POINT('Ctrl Pts',(6.67573926520284,-2.14292599627917,
11.6744092256013));
#158917=CARTESIAN_POINT('Ctrl Pts',(6.7320650030048,-1.96745752926772,11.6827788050813));
#158918=CARTESIAN_POINT('Ctrl Pts',(6.78141862654025,-1.78992236943731,
11.6911483845613));
#158919=CARTESIAN_POINT('Ctrl Pts',(6.82368074612044,-1.61090273993349,
11.6995179640413));
#158920=CARTESIAN_POINT('Ctrl Pts',(6.86600804987073,-1.43160699446347,
11.7079004525778));
#158921=CARTESIAN_POINT('Ctrl Pts',(6.90122193019567,-1.25082252497166,
11.7162829411144));
#158922=CARTESIAN_POINT('Ctrl Pts',(6.92925445938158,-1.06913946688002,
11.7246654296509));
#158923=CARTESIAN_POINT('Ctrl Pts',(6.93842716227157,-1.00968979321814,
11.7274083172554));
#158924=CARTESIAN_POINT('Ctrl Pts',(6.94683136914179,-0.950143927580071,
11.7301512048598));
#158925=CARTESIAN_POINT('Ctrl Pts',(6.95446591090137,-0.890522575014692,
11.7328940924642));
#158926=CARTESIAN_POINT('Ctrl Pts',(6.99217189097099,-0.596060693431332,
11.7464408472796));
#158927=CARTESIAN_POINT('Ctrl Pts',(7.01115634495759,-0.299346418725676,
11.7599876020951));
#158928=CARTESIAN_POINT('Ctrl Pts',(7.01124965431565,-0.00220167178196738,
11.7735343569105));
#158929=CARTESIAN_POINT('Ctrl Pts',(7.01124965431583,-0.00220167122712958,
11.7735343569358));
#158930=CARTESIAN_POINT('Ctrl Pts',(7.01130668446778,0.179411563396666,
11.781814058953));
#158931=CARTESIAN_POINT('Ctrl Pts',(7.00430291895196,0.361201757753028,
11.7900937609703));
#158932=CARTESIAN_POINT('Ctrl Pts',(6.99022344746899,0.542588902351294,
11.7983734629875));
#158933=CARTESIAN_POINT('Ctrl Pts',(6.97615945174002,0.723776671367002,
11.8066440641922));
#158934=CARTESIAN_POINT('Ctrl Pts',(6.95503528430813,0.904561935256292,
11.8149146653968));
#158935=CARTESIAN_POINT('Ctrl Pts',(6.92688806918397,1.08436536254937,11.8231852666014));
#158936=CARTESIAN_POINT('Ctrl Pts',(6.89875892534549,1.26405335110059,11.8314505578528));
#158937=CARTESIAN_POINT('Ctrl Pts',(6.86361576914439,1.44276042284829,11.8397158491041));
#158938=CARTESIAN_POINT('Ctrl Pts',(6.82154754427712,1.61991223949535,11.8479811403555));
#158939=CARTESIAN_POINT('Ctrl Pts',(6.77950291415879,1.79696469724027,11.856241795864));
#158940=CARTESIAN_POINT('Ctrl Pts',(6.73054103683612,1.97246330740118,11.8645024513725));
#158941=CARTESIAN_POINT('Ctrl Pts',(6.67480198863536,2.14584365111008,11.8727631068811));
#158942=CARTESIAN_POINT('Ctrl Pts',(6.64250096825414,2.24631831288892,11.8775501926056));
#158943=CARTESIAN_POINT('Ctrl Pts',(6.60792495302767,2.34608180031525,11.8823372783302));
#158944=CARTESIAN_POINT('Ctrl Pts',(6.57110895151814,2.44502632087636,11.8871243640548));
#158945=CARTESIAN_POINT('',(7.0112498809707,-0.00129193205168586,11.2264656430533));
#158946=CARTESIAN_POINT('Ctrl Pts',(6.57110895151813,2.44502632087638,11.3397782664936));
#158947=CARTESIAN_POINT('Ctrl Pts',(6.63286227697798,2.27906171499445,11.3317554799954));
#158948=CARTESIAN_POINT('Ctrl Pts',(6.68833298419261,2.11073178541639,11.3237326934973));
#158949=CARTESIAN_POINT('Ctrl Pts',(6.7373471412283,1.94056179007081,11.3157099069992));
#158950=CARTESIAN_POINT('Ctrl Pts',(6.78858424553279,1.76267404644062,11.3073232617221));
#158951=CARTESIAN_POINT('Ctrl Pts',(6.83276533325641,1.58277584443963,11.298936616445));
#158952=CARTESIAN_POINT('Ctrl Pts',(6.8697504549464,1.40148323188821,11.2905499711678));
#158953=CARTESIAN_POINT('Ctrl Pts',(6.90673557663638,1.22019061933677,11.2821633258907));
#158954=CARTESIAN_POINT('Ctrl Pts',(6.93652466649385,1.03750404859929,11.2737766806136));
#158955=CARTESIAN_POINT('Ctrl Pts',(6.95903917973925,0.854049329578839,
11.2653900353364));
#158956=CARTESIAN_POINT('Ctrl Pts',(6.98457816243644,0.645950364981519,
11.2558767766536));
#158957=CARTESIAN_POINT('Ctrl Pts',(7.00076663815956,0.436802360120021,
11.2463635179709));
#158958=CARTESIAN_POINT('Ctrl Pts',(7.00756193005895,0.227381527148892,
11.2368502592881));
#158959=CARTESIAN_POINT('Ctrl Pts',(7.01003449670461,0.151180684833668,
11.2333887205553));
#158960=CARTESIAN_POINT('Ctrl Pts',(7.01126392857063,0.0749437292480127,
11.2299271818224));
#158961=CARTESIAN_POINT('Ctrl Pts',(7.01124988097084,-0.0012919312519414,
11.2264656430896));
#158962=CARTESIAN_POINT('Ctrl Pts',(7.0112498809707,-0.00129193205166578,
11.2264656430533));
#158963=CARTESIAN_POINT('Ctrl Pts',(7.01121483285703,-0.19149627172734,
11.2178292688864));
#158964=CARTESIAN_POINT('Ctrl Pts',(7.00343552236527,-0.381688380886737,
11.2091928947195));
#158965=CARTESIAN_POINT('Ctrl Pts',(6.98794071515853,-0.57123648686839,
11.2005565205526));
#158966=CARTESIAN_POINT('Ctrl Pts',(6.97244167909753,-0.760836324459489,
11.1919177893401));
#158967=CARTESIAN_POINT('Ctrl Pts',(6.94922296039208,-0.949791518269339,
11.1832790581275));
#158968=CARTESIAN_POINT('Ctrl Pts',(6.91836528355355,-1.13747455612029,
11.174640326915));
#158969=CARTESIAN_POINT('Ctrl Pts',(6.88750581762904,-1.32516847557757,
11.1660010948406));
#158970=CARTESIAN_POINT('Ctrl Pts',(6.84900656005112,-1.51158980612792,
11.1573618627662));
#158971=CARTESIAN_POINT('Ctrl Pts',(6.80299959257456,-1.69612001519068,
11.1487226306918));
#158972=CARTESIAN_POINT('Ctrl Pts',(6.75698038588684,-1.88069931473509,
11.1400811003267));
#158973=CARTESIAN_POINT('Ctrl Pts',(6.70344954877135,-2.06338620598536,
11.1314395699616));
#158974=CARTESIAN_POINT('Ctrl Pts',(6.64258968814643,-2.24357500374531,
11.1227980395966));
#158975=CARTESIAN_POINT('Ctrl Pts',(6.60485135574661,-2.35530750978073,
11.1174395497477));
#158976=CARTESIAN_POINT('Ctrl Pts',(6.56429595901887,-2.46607976288995,
11.1120810598989));
#158977=CARTESIAN_POINT('Ctrl Pts',(6.5209765531919,-2.57575063917715,11.10672257005));
#158978=CARTESIAN_POINT('Ctrl Pts',(6.45031461865842,-2.75464405039773,
11.0979818855538));
#158979=CARTESIAN_POINT('Ctrl Pts',(6.37228337420837,-2.9306376100954,11.0892412010576));
#158980=CARTESIAN_POINT('Ctrl Pts',(6.28714218852822,-3.1031386794226,11.0805005165614));
#158981=CARTESIAN_POINT('Ctrl Pts',(6.2020163211615,-3.27560871294231,11.0717614046595));
#158982=CARTESIAN_POINT('Ctrl Pts',(6.10978318835428,-3.44458726553878,
11.0630222927576));
#158983=CARTESIAN_POINT('Ctrl Pts',(6.01074900219863,-3.60950453595341,
11.0542831808556));
#158984=CARTESIAN_POINT('Ctrl Pts',(5.91043168562665,-3.77655854696298,
11.0454308411813));
#158985=CARTESIAN_POINT('Ctrl Pts',(5.8031359797634,-3.93944504673891,11.036578501507));
#158986=CARTESIAN_POINT('Ctrl Pts',(5.68922732024001,-4.09759918258664,
11.0277261618326));
#158987=CARTESIAN_POINT('Ctrl Pts',(5.57683327152893,-4.25365038819914,
11.0189915291829));
#158988=CARTESIAN_POINT('Ctrl Pts',(5.45800121360134,-4.40509407825301,
11.0102568965331));
#158989=CARTESIAN_POINT('Ctrl Pts',(5.33312531501383,-4.55141746457724,
11.0015222638833));
#158990=CARTESIAN_POINT('Ctrl Pts',(5.20572519399149,-4.70069860959371,
10.9926110706967));
#158991=CARTESIAN_POINT('Ctrl Pts',(5.0720344634497,-4.8446500091867,10.9836998775101));
#158992=CARTESIAN_POINT('Ctrl Pts',(4.93251499832045,-4.98276252232071,
10.9747886843235));
#158993=CARTESIAN_POINT('Ctrl Pts',(4.79299553319121,-5.12087503545471,
10.9658774911369));
#158994=CARTESIAN_POINT('Ctrl Pts',(4.64764753942393,-5.25314843929787,
10.9569662979502));
#158995=CARTESIAN_POINT('Ctrl Pts',(4.49697370569523,-5.37911275702469,
10.9480551047636));
#158996=CARTESIAN_POINT('Ctrl Pts',(4.36127272085424,-5.49255967443127,
10.9400294399112));
#158997=CARTESIAN_POINT('Ctrl Pts',(4.22118909179728,-5.60094084191295,
10.9320037750588));
#158998=CARTESIAN_POINT('Ctrl Pts',(4.07714709029428,-5.70390201236004,
10.9239781102064));
#158999=CARTESIAN_POINT('Ctrl Pts',(3.93315080418942,-5.80683050545712,
10.9159549925032));
#159000=CARTESIAN_POINT('Ctrl Pts',(3.78519894465811,-5.90434221331194,
10.9079318747999));
#159001=CARTESIAN_POINT('Ctrl Pts',(3.63374754083289,-5.99612419584442,
10.8999087570967));
#159002=CARTESIAN_POINT('Ctrl Pts',(3.48231523635535,-6.08789460386554,
10.8918866511788));
#159003=CARTESIAN_POINT('Ctrl Pts',(3.327384580363,-6.17393653641374,10.883864545261));
#159004=CARTESIAN_POINT('Ctrl Pts',(3.16943910852018,-6.25398131592051,
10.8758424393431));
#159005=CARTESIAN_POINT('Ctrl Pts',(3.0114349436063,-6.33405584033783,10.8678173523836));
#159006=CARTESIAN_POINT('Ctrl Pts',(2.85041405073292,-6.40812859121088,
10.859792265424));
#159007=CARTESIAN_POINT('Ctrl Pts',(2.68688341071867,-6.47597746287808,
10.8517671784645));
#159008=CARTESIAN_POINT('Ctrl Pts',(2.5233205641631,-6.54383969704107,10.8437405110042));
#159009=CARTESIAN_POINT('Ctrl Pts',(2.35724732772862,-6.6054754777394,10.835713843544));
#159010=CARTESIAN_POINT('Ctrl Pts',(2.18918882380095,-6.66071158782941,
10.8276871760837));
#159011=CARTESIAN_POINT('Ctrl Pts',(2.02099540309858,-6.71599204127395,
10.8196540648431));
#159012=CARTESIAN_POINT('Ctrl Pts',(1.85081388283077,-6.7648624573645,10.8116209536025));
#159013=CARTESIAN_POINT('Ctrl Pts',(1.67918324409768,-6.8071998791898,10.8035878423619));
#159014=CARTESIAN_POINT('Ctrl Pts',(1.57805223693432,-6.83214662611971,
10.7988544414003));
#159015=CARTESIAN_POINT('Ctrl Pts',(1.4764183082212,-6.8548260866022,10.7941210404387));
#159016=CARTESIAN_POINT('Ctrl Pts',(1.37439299910562,-6.87522148345124,
10.7893876394771));
#159017=CARTESIAN_POINT('Ctrl Pts',(1.16421768708872,-6.91723663570723,
10.779636686183));
#159018=CARTESIAN_POINT('Ctrl Pts',(0.952257338297864,-6.94958151096932,
10.7698857328889));
#159019=CARTESIAN_POINT('Ctrl Pts',(0.739323485861614,-6.97216088065626,
10.7601347795948));
#159020=CARTESIAN_POINT('Ctrl Pts',(0.526082862265363,-6.99477278016103,
10.7503697782232));
#159021=CARTESIAN_POINT('Ctrl Pts',(0.31186596799987,-7.00759102779102,
10.7406047768516));
#159022=CARTESIAN_POINT('Ctrl Pts',(0.0974902579981229,-7.01057217437318,
10.73083977548));
#159023=CARTESIAN_POINT('Ctrl Pts',(-0.116528132112505,-7.01354835200166,
10.7210910503425));
#159024=CARTESIAN_POINT('Ctrl Pts',(-0.330704771000217,-7.00672019781832,
10.711342325205));
#159025=CARTESIAN_POINT('Ctrl Pts',(-0.544224464764906,-6.99009630079954,
10.7015936000674));
#159026=CARTESIAN_POINT('Ctrl Pts',(-0.757158129762107,-6.97351802993218,
10.6918716314003));
#159027=CARTESIAN_POINT('Ctrl Pts',(-0.969438409336941,-6.94719769186674,
10.6821496627332));
#159028=CARTESIAN_POINT('Ctrl Pts',(-1.1802555801732,-6.91119550642073,
10.6724276940662));
#159029=CARTESIAN_POINT('Ctrl Pts',(-1.3896778288526,-6.87543153803253,
10.6627700531265));
#159030=CARTESIAN_POINT('Ctrl Pts',(-1.59765621594698,-6.83011340267927,
10.6531124121868));
#159031=CARTESIAN_POINT('Ctrl Pts',(-1.80339645969658,-6.77535148694545,
10.6434547712472));
#159032=CARTESIAN_POINT('Ctrl Pts',(-1.89382638003329,-6.75128173964155,
10.6392099055617));
#159033=CARTESIAN_POINT('Ctrl Pts',(-1.98382391000512,-6.72538821540239,
10.6349650398762));
#159034=CARTESIAN_POINT('Ctrl Pts',(-2.07332161451241,-6.69768348351097,
10.6307201741907));
#159035=CARTESIAN_POINT('Ctrl Pts',(-2.23886802656795,-6.64643726455113,
10.6228683271768));
#159036=CARTESIAN_POINT('Ctrl Pts',(-2.40263517021604,-6.58901142800171,
10.6150164801629));
#159037=CARTESIAN_POINT('Ctrl Pts',(-2.5641124543584,-6.52556157613306,
10.607164633149));
#159038=CARTESIAN_POINT('Ctrl Pts',(-2.72554394484851,-6.46212971812941,
10.5993150128554));
#159039=CARTESIAN_POINT('Ctrl Pts',(-2.88468651288333,-6.39267738239986,
10.5914653925618));
#159040=CARTESIAN_POINT('Ctrl Pts',(-3.04104683840681,-6.31740933366803,
10.5836157722682));
#159041=CARTESIAN_POINT('Ctrl Pts',(-3.1973946805583,-6.24214729412714,
10.5757667786664));
#159042=CARTESIAN_POINT('Ctrl Pts',(-3.35096037900238,-6.16107063202908,
10.5679177850646));
#159043=CARTESIAN_POINT('Ctrl Pts',(-3.50127287565162,-6.07443123368157,
10.5600687914628));
#159044=CARTESIAN_POINT('Ctrl Pts',(-3.65166147111628,-5.98774797234377,
10.5522158241453));
#159045=CARTESIAN_POINT('Ctrl Pts',(-3.79879324307088,-5.89549653849056,
10.5443628568279));
#159046=CARTESIAN_POINT('Ctrl Pts',(-3.94222363728072,-5.7979737284818,
10.5365098895105));
#159047=CARTESIAN_POINT('Ctrl Pts',(-4.08569045799139,-5.70042615095609,
10.5286549278032));
#159048=CARTESIAN_POINT('Ctrl Pts',(-4.22545372090009,-5.5976047562469,
10.5207999660959));
#159049=CARTESIAN_POINT('Ctrl Pts',(-4.36110046444042,-5.48984783956327,
10.5129450043887));
#159050=CARTESIAN_POINT('Ctrl Pts',(-4.49688184871228,-5.38198396513256,
10.5050822459753));
#159051=CARTESIAN_POINT('Ctrl Pts',(-4.62853826330783,-5.26917503243585,
10.4972194875619));
#159052=CARTESIAN_POINT('Ctrl Pts',(-4.75569182610824,-5.15179792088037,
10.4893567291486));
#159053=CARTESIAN_POINT('Ctrl Pts',(-4.84896985523238,-5.06569175610569,
10.4835887224005));
#159054=CARTESIAN_POINT('Ctrl Pts',(-4.93982542595319,-4.97712803729662,
10.4778207156524));
#159055=CARTESIAN_POINT('Ctrl Pts',(-5.02812298621066,-4.88626706167807,
10.4720527089043));
#159056=CARTESIAN_POINT('Ctrl Pts',(-5.15637575336667,-4.75429091742679,
10.4636746424633));
#159057=CARTESIAN_POINT('Ctrl Pts',(-5.27951448298945,-4.61717463325744,
10.4552965760223));
#159058=CARTESIAN_POINT('Ctrl Pts',(-5.39712312308619,-4.4753422837531,
10.4469185095812));
#159059=CARTESIAN_POINT('Ctrl Pts',(-5.51465134379223,-4.33360691752412,
10.4385461719625));
#159060=CARTESIAN_POINT('Ctrl Pts',(-5.62665680482521,-4.1871621674751,
10.4301738343438));
#159061=CARTESIAN_POINT('Ctrl Pts',(-5.73276188898709,-4.03646722849042,
10.421801496725));
#159062=CARTESIAN_POINT('Ctrl Pts',(-5.83880998013379,-3.88585323340221,
10.4134336562024));
#159063=CARTESIAN_POINT('Ctrl Pts',(-5.93896382489256,-3.73099386951696,
10.4050658156798));
#159064=CARTESIAN_POINT('Ctrl Pts',(-6.03288724599517,-3.57237988455999,
10.3966979751572));
#159065=CARTESIAN_POINT('Ctrl Pts',(-6.12677397640972,-3.41382786131795,
10.3883334034873));
#159066=CARTESIAN_POINT('Ctrl Pts',(-6.21443496943698,-3.25152442428541,
10.3799688318174));
#159067=CARTESIAN_POINT('Ctrl Pts',(-6.29557815673927,-3.0859880484032,
10.3716042601475));
#159068=CARTESIAN_POINT('Ctrl Pts',(-6.37670152328819,-2.92049210790181,
10.3632417316819));
#159069=CARTESIAN_POINT('Ctrl Pts',(-6.4513101149823,-2.75176509848021,
10.3548792032163));
#159070=CARTESIAN_POINT('Ctrl Pts',(-6.5191582832499,-2.58034917025472,
10.3465166747507));
#159071=CARTESIAN_POINT('Ctrl Pts',(-6.58701186601356,-2.40891956250198,
10.3381534789292));
#159072=CARTESIAN_POINT('Ctrl Pts',(-6.6481038209225,-2.23480091061489,
10.3297902831077));
#159073=CARTESIAN_POINT('Ctrl Pts',(-6.70223675191998,-2.05855509610823,
10.3214270872862));
#159074=CARTESIAN_POINT('Ctrl Pts',(-6.75637337467483,-1.88229726199034,
10.3130633211115));
#159075=CARTESIAN_POINT('Ctrl Pts',(-6.80354993042206,-1.70391229024975,
10.3046995549368));
#159076=CARTESIAN_POINT('Ctrl Pts',(-6.84361894436408,-1.52397713461885,
10.2963357887621));
#159077=CARTESIAN_POINT('Ctrl Pts',(-6.88369603307462,-1.3440057181822,
10.2879703371085));
#159078=CARTESIAN_POINT('Ctrl Pts',(-6.91666265244109,-1.16248381585892,
10.279604885455));
#159079=CARTESIAN_POINT('Ctrl Pts',(-6.94242239497191,-0.979998904230274,
10.2712394338014));
#159080=CARTESIAN_POINT('Ctrl Pts',(-6.96819076438986,-0.79745287876346,
10.2628711805746));
#159081=CARTESIAN_POINT('Ctrl Pts',(-6.98674739831039,-0.613943526323872,
10.2545029273477));
#159082=CARTESIAN_POINT('Ctrl Pts',(-6.99804768035543,-0.430064211452212,
10.2461346741208));
#159083=CARTESIAN_POINT('Ctrl Pts',(-7.00935843937408,-0.246014414222441,
10.2377586623293));
#159084=CARTESIAN_POINT('Ctrl Pts',(-7.0133993824308,-0.0615942976320604,
10.2293826505379));
#159085=CARTESIAN_POINT('Ctrl Pts',(-7.01017800193792,0.122600748960567,
10.2210066387464));
#159086=CARTESIAN_POINT('Ctrl Pts',(-7.00695504164024,0.306886127079898,
10.2126265192552));
#159087=CARTESIAN_POINT('Ctrl Pts',(-6.99646266769307,0.490945886679691,
10.2042463997641));
#159088=CARTESIAN_POINT('Ctrl Pts',(-6.97876039602519,0.674188324854724,
10.195866280273));
#159089=CARTESIAN_POINT('Ctrl Pts',(-6.96103789726951,0.857640140727379,
10.1874765854337));
#159090=CARTESIAN_POINT('Ctrl Pts',(-6.93608907723435,1.04027244237954,
10.1790868905945));
#159091=CARTESIAN_POINT('Ctrl Pts',(-6.90402505451619,1.22150096566184,
10.1706971957553));
#159092=CARTESIAN_POINT('Ctrl Pts',(-6.88366815981293,1.33655982768021,
10.1653707232807));
#159093=CARTESIAN_POINT('Ctrl Pts',(-6.86044432726521,1.45105306635647,
10.1600442508061));
#159094=CARTESIAN_POINT('Ctrl Pts',(-6.83439251135145,1.5648340369775,10.1547177783314));
#159095=CARTESIAN_POINT('Ctrl Pts',(-6.79339950964048,1.74387044422,10.1463364779266));
#159096=CARTESIAN_POINT('Ctrl Pts',(-6.74531936724476,1.92150377135524,
10.1379551775217));
#159097=CARTESIAN_POINT('Ctrl Pts',(-6.69026031388856,2.09715128088266,
10.1295738771168));
#159098=CARTESIAN_POINT('Ctrl Pts',(-6.63527103982242,2.2725761829047,10.1212031987833));
#159099=CARTESIAN_POINT('Ctrl Pts',(-6.57332057867011,2.44601997279038,
10.1128325204497));
#159100=CARTESIAN_POINT('Ctrl Pts',(-6.50456798830298,2.61691074514286,
10.1044618421162));
#159101=CARTESIAN_POINT('Ctrl Pts',(-6.43589342032166,2.78760758580926,
10.0961006630653));
#159102=CARTESIAN_POINT('Ctrl Pts',(-6.36043222998785,2.95575688132914,
10.0877394840145));
#159103=CARTESIAN_POINT('Ctrl Pts',(-6.27839317148616,3.12080209989932,
10.0793783049637));
#159104=CARTESIAN_POINT('Ctrl Pts',(-6.19646056834021,3.28563315282965,
10.071027975529));
#159105=CARTESIAN_POINT('Ctrl Pts',(-6.10796726725877,3.44736787087806,
10.0626776460943));
#159106=CARTESIAN_POINT('Ctrl Pts',(-6.01316994022668,3.60546998773451,
10.0543273166596));
#159107=CARTESIAN_POINT('Ctrl Pts',(-5.91844555406709,3.7634504544695,10.0459834123038));
#159108=CARTESIAN_POINT('Ctrl Pts',(-5.81742697603724,3.91780361026158,
10.0376395079481));
#159109=CARTESIAN_POINT('Ctrl Pts',(-5.71041712791927,4.06801705842862,
10.0292956035924));
#159110=CARTESIAN_POINT('Ctrl Pts',(-5.60349323077875,4.21810985421718,
10.0209584011127));
#159111=CARTESIAN_POINT('Ctrl Pts',(-5.49058785040465,4.36406930760973,
10.012621198633));
#159112=CARTESIAN_POINT('Ctrl Pts',(-5.3720476919304,4.5054112085497,10.0042839961533));
#159113=CARTESIAN_POINT('Ctrl Pts',(-5.33302492608617,4.55194018215114,
10.0015394351172));
#159114=CARTESIAN_POINT('Ctrl Pts',(-5.29339187257674,4.59796899144473,
9.99879487408112));
#159115=CARTESIAN_POINT('Ctrl Pts',(-5.25316190643485,4.64348108074985,
9.99605031304502));
#159116=CARTESIAN_POINT('Ctrl Pts',(-5.1309383753438,4.78175234457802,9.98771200274311));
#159117=CARTESIAN_POINT('Ctrl Pts',(-5.00330256798266,4.91513824112804,
9.97937369244119));
#159118=CARTESIAN_POINT('Ctrl Pts',(-4.87068120156059,5.04322230278066,
9.97103538213927));
#159119=CARTESIAN_POINT('Ctrl Pts',(-4.73797639427498,5.17138695057864,
9.96269182565545));
#159120=CARTESIAN_POINT('Ctrl Pts',(-4.60028000698162,5.29424288232457,
9.95434826917163));
#159121=CARTESIAN_POINT('Ctrl Pts',(-4.45805313999478,5.41141282508391,
9.94600471268782));
#159122=CARTESIAN_POINT('Ctrl Pts',(-4.31571806742758,5.52867191022492,
9.9376548084626));
#159123=CARTESIAN_POINT('Ctrl Pts',(-4.16884589258824,5.6402361695705,9.9293049042374));
#159124=CARTESIAN_POINT('Ctrl Pts',(-4.01792842083125,5.74577042419696,
9.92095500001219));
#159125=CARTESIAN_POINT('Ctrl Pts',(-3.86678458403449,5.85146297239585,
9.91259257154852));
#159126=CARTESIAN_POINT('Ctrl Pts',(-3.71158359400024,5.95110725406904,
9.90423014308485));
#159127=CARTESIAN_POINT('Ctrl Pts',(-3.55284498573029,6.04441221872492,
9.89586771462119));
#159128=CARTESIAN_POINT('Ctrl Pts',(-3.39397063431105,6.1377969718449,9.88749813514123));
#159129=CARTESIAN_POINT('Ctrl Pts',(-3.23155291681996,6.22483143729944,
9.87912855566126));
#159130=CARTESIAN_POINT('Ctrl Pts',(-3.06613377845246,6.30527162104321,
9.87075897618129));
#159131=CARTESIAN_POINT('Ctrl Pts',(-2.90045950121834,6.38583587396974,
9.86237648764471));
#159132=CARTESIAN_POINT('Ctrl Pts',(-2.73177485183306,6.45978538944467,
9.85399399910813));
#159133=CARTESIAN_POINT('Ctrl Pts',(-2.56064076548373,6.52692465351355,
9.84561151057155));
#159134=CARTESIAN_POINT('Ctrl Pts',(-2.50464288823322,6.54889372085846,
9.84286862296723));
#159135=CARTESIAN_POINT('Ctrl Pts',(-2.44838285924885,6.57013401149062,
9.8401257353629));
#159136=CARTESIAN_POINT('Ctrl Pts',(-2.39188062497575,6.59063985045197,
9.83738284775858));
#159137=CARTESIAN_POINT('Ctrl Pts',(-2.21905343384968,6.65336244177899,
9.82899299262579));
#159138=CARTESIAN_POINT('Ctrl Pts',(-2.04361021329538,6.70933634883603,
9.82060313749299));
#159139=CARTESIAN_POINT('Ctrl Pts',(-1.86610484110358,6.75834885785795,
9.8122132823602));
#159140=CARTESIAN_POINT('Ctrl Pts',(-1.68876326838071,6.80731613882366,
9.8038311692681));
#159141=CARTESIAN_POINT('Ctrl Pts',(-1.50936365283739,6.84933474068126,
9.79544905617602));
#159142=CARTESIAN_POINT('Ctrl Pts',(-1.32847692186159,6.88424110781872,
9.78706694308393));
#159143=CARTESIAN_POINT('Ctrl Pts',(-1.1477305206512,6.91912039501348,9.77869133273506));
#159144=CARTESIAN_POINT('Ctrl Pts',(-0.965499625721145,6.94689838581222,
9.77031572238618));
#159145=CARTESIAN_POINT('Ctrl Pts',(-0.782367750467858,6.96746203904462,
9.76194011203731));
#159146=CARTESIAN_POINT('Ctrl Pts',(-0.599351067883436,6.9880127574338,
9.75356977007172));
#159147=CARTESIAN_POINT('Ctrl Pts',(-0.415434860816468,7.00135814988574,
9.74519942810614));
#159148=CARTESIAN_POINT('Ctrl Pts',(-0.231210660255876,7.00743663496746,
9.73682908614055));
#159149=CARTESIAN_POINT('Ctrl Pts',(-0.0470753342545793,7.01351218762943,
9.72846278224624));
#159150=CARTESIAN_POINT('Ctrl Pts',(0.137367360980391,7.01232781312478,
9.72009647835192));
#159151=CARTESIAN_POINT('Ctrl Pts',(0.3215225121874,7.00387391638775,9.71173017445761));
#159152=CARTESIAN_POINT('Ctrl Pts',(0.505626160360471,6.99542238396868,
9.70336621038399));
#159153=CARTESIAN_POINT('Ctrl Pts',(0.689442096772502,6.97970539686829,
9.69500224631038));
#159154=CARTESIAN_POINT('Ctrl Pts',(0.872376589461687,6.95676545879328,
9.68663828223676));
#159155=CARTESIAN_POINT('Ctrl Pts',(1.05528293157237,6.93382905079353,9.67827560523823));
#159156=CARTESIAN_POINT('Ctrl Pts',(1.23730777438916,6.9036719487937,9.66991292823969));
#159157=CARTESIAN_POINT('Ctrl Pts',(1.4178632597763,6.86638844947448,9.66155025124115));
#159158=CARTESIAN_POINT('Ctrl Pts',(1.59841502785603,6.82910571775436,9.65318774641485));
#159159=CARTESIAN_POINT('Ctrl Pts',(1.77749717705043,6.784696948129,9.64482524158854));
#159160=CARTESIAN_POINT('Ctrl Pts',(1.95453235461456,6.73330749611696,9.63646273676223));
#159161=CARTESIAN_POINT('Ctrl Pts',(2.13158748487691,6.68191225227167,9.62809928944225));
#159162=CARTESIAN_POINT('Ctrl Pts',(2.30659486809438,6.62353484960426,9.61973584212229));
#159163=CARTESIAN_POINT('Ctrl Pts',(2.47899220149725,6.55837054666903,9.61137239480231));
#159164=CARTESIAN_POINT('Ctrl Pts',(2.65149104729497,6.4931678731609,9.60300402284951));
#159165=CARTESIAN_POINT('Ctrl Pts',(2.82137646415526,6.42117042921805,9.59463565089669));
#159166=CARTESIAN_POINT('Ctrl Pts',(2.98810506373554,6.34262206745586,9.58626727894389));
#159167=CARTESIAN_POINT('Ctrl Pts',(3.15488361956161,6.26405017055167,9.57789639960814));
#159168=CARTESIAN_POINT('Ctrl Pts',(3.31850317695768,6.17892358688459,9.56952552027242));
#159169=CARTESIAN_POINT('Ctrl Pts',(3.47844422946308,6.08753253009912,9.56115464093668));
#159170=CARTESIAN_POINT('Ctrl Pts',(3.63852079829292,5.9960640386594,9.55277666904538));
#159171=CARTESIAN_POINT('Ctrl Pts',(3.79491235148339,5.89832063598326,9.54439869715408));
#159172=CARTESIAN_POINT('Ctrl Pts',(3.94712670689393,5.79463694481584,9.53602072526279));
#159173=CARTESIAN_POINT('Ctrl Pts',(4.0438601692439,5.7287451147792,9.53069645590377));
#159174=CARTESIAN_POINT('Ctrl Pts',(4.13890717369984,5.66045504662206,9.52537218654476));
#159175=CARTESIAN_POINT('Ctrl Pts',(4.23214814517252,5.58986123618582,9.52004791718574));
#159176=CARTESIAN_POINT('Ctrl Pts',(4.36984553972143,5.48560895722712,9.51218508599645));
#159177=CARTESIAN_POINT('Ctrl Pts',(4.50388872818022,5.37611348052248,9.50432225480718));
#159178=CARTESIAN_POINT('Ctrl Pts',(4.63383618386604,5.26167167196832,9.49645942361791));
#159179=CARTESIAN_POINT('Ctrl Pts',(4.76368379208507,5.14731779683784,9.48860263397651));
#159180=CARTESIAN_POINT('Ctrl Pts',(4.88944164157285,5.02802539826285,9.48074584433512));
#159181=CARTESIAN_POINT('Ctrl Pts',(5.01069854977613,4.90413362437968,9.47288905469373));
#159182=CARTESIAN_POINT('Ctrl Pts',(5.13188707482306,4.78031171959238,9.46503669590978));
#159183=CARTESIAN_POINT('Ctrl Pts',(5.2485794420259,4.65189587085154,9.45718433712582));
#159184=CARTESIAN_POINT('Ctrl Pts',(5.36039904202615,4.51926417381692,9.44933197834187));
#159185=CARTESIAN_POINT('Ctrl Pts',(5.47219224011429,4.38666379267334,9.44148147359145));
#159186=CARTESIAN_POINT('Ctrl Pts',(5.5791147088633,4.24984983017525,9.43363096884102));
#159187=CARTESIAN_POINT('Ctrl Pts',(5.68082814214468,4.10923571749261,9.42578046409059));
#159188=CARTESIAN_POINT('Ctrl Pts',(5.78252521294037,3.96864422518894,9.41793122223895));
#159189=CARTESIAN_POINT('Ctrl Pts',(5.87901469524553,3.82425411056282,9.41008198038731));
#159190=CARTESIAN_POINT('Ctrl Pts',(5.9700001664025,3.67650983619711,9.40223273853567));
#159191=CARTESIAN_POINT('Ctrl Pts',(6.06101629234551,3.52871578389365,9.39438085212082));
#159192=CARTESIAN_POINT('Ctrl Pts',(6.14652450283271,3.37756563973237,9.38652896570598));
#159193=CARTESIAN_POINT('Ctrl Pts',(6.226273013965,3.22353081543688,9.37867707929113));
#159194=CARTESIAN_POINT('Ctrl Pts',(6.28483135307956,3.11042496118986,9.37291153682718));
#159195=CARTESIAN_POINT('Ctrl Pts',(6.34028511368452,2.99576432463116,9.36714599436324));
#159196=CARTESIAN_POINT('Ctrl Pts',(6.39255086948598,2.87974303428865,9.36138045189929));
#159197=CARTESIAN_POINT('Ctrl Pts',(6.45696418237184,2.7367561863678,9.35427488755813));
#159198=CARTESIAN_POINT('Ctrl Pts',(6.51651601396806,2.59174708930409,9.34716932321697));
#159199=CARTESIAN_POINT('Ctrl Pts',(6.57110895151814,2.44502632087636,9.34006375887581));
#159200=CARTESIAN_POINT('Origin',(0.,0.,50.));
#159201=CARTESIAN_POINT('',(6.57110895151814,2.44502632087637,7.33978485479521));
#159202=CARTESIAN_POINT('',(6.57110895151813,2.44502632087637,7.88693503181338));
#159203=CARTESIAN_POINT('',(6.57110895151814,2.44502632087636,50.));
#159204=CARTESIAN_POINT('',(7.01124998073505,0.000519752639607968,9.77353435687236));
#159205=CARTESIAN_POINT('Ctrl Pts',(6.57110895151814,2.44502632087637,7.88693503181337));
#159206=CARTESIAN_POINT('Ctrl Pts',(6.49628307728171,2.64612394007251,7.89670751236697));
#159207=CARTESIAN_POINT('Ctrl Pts',(6.41220863601586,2.84382046692177,7.90647999292057));
#159208=CARTESIAN_POINT('Ctrl Pts',(6.31918628001434,3.03735268300844,7.91625247347417));
#159209=CARTESIAN_POINT('Ctrl Pts',(6.29182779425026,3.09427177865692,7.91912662417941));
#159210=CARTESIAN_POINT('Ctrl Pts',(6.26369565058952,3.15083077630124,7.92200077488466));
#159211=CARTESIAN_POINT('Ctrl Pts',(6.23479831148065,3.20701053594434,7.9248749255899));
#159212=CARTESIAN_POINT('Ctrl Pts',(6.15403231604373,3.36402894493653,7.93290797118868));
#159213=CARTESIAN_POINT('Ctrl Pts',(6.06724655878222,3.51815830011378,7.94094101678745));
#159214=CARTESIAN_POINT('Ctrl Pts',(5.97467924385627,3.66890099287689,7.94897406238623));
#159215=CARTESIAN_POINT('Ctrl Pts',(5.88217143476448,3.81954678243306,7.95700194403399));
#159216=CARTESIAN_POINT('Ctrl Pts',(5.78388965702759,3.9668099320284,7.96502982568177));
#159217=CARTESIAN_POINT('Ctrl Pts',(5.68011830557492,4.11021685524896,7.97305770732953));
#159218=CARTESIAN_POINT('Ctrl Pts',(5.5763938079104,4.25355902883001,7.9810819643096));
#159219=CARTESIAN_POINT('Ctrl Pts',(5.46718488614912,4.39304814645702,7.98910622128966));
#159220=CARTESIAN_POINT('Ctrl Pts',(5.35281953635889,4.52823912505453,7.99713047826972));
#159221=CARTESIAN_POINT('Ctrl Pts',(5.2384680145043,4.66341375768576,8.00515376503539));
#159222=CARTESIAN_POINT('Ctrl Pts',(5.11896153718186,4.79429100174109,8.01317705180106));
#159223=CARTESIAN_POINT('Ctrl Pts',(4.99466882432703,4.92045830160115,8.02120033856673));
#159224=CARTESIAN_POINT('Ctrl Pts',(4.87038629615114,5.04661526317659,8.02922296789562));
#159225=CARTESIAN_POINT('Ctrl Pts',(4.7413185738181,5.16806279093765,8.03724559722452));
#159226=CARTESIAN_POINT('Ctrl Pts',(4.60787150224812,5.28442492436685,8.04526822655342));
#159227=CARTESIAN_POINT('Ctrl Pts',(4.47437426407975,5.40083080167404,8.05329387181978));
#159228=CARTESIAN_POINT('Ctrl Pts',(4.33649466631384,5.5121472268049,8.06131951708615));
#159229=CARTESIAN_POINT('Ctrl Pts',(4.1946722069539,5.6180380595639,8.06934516235251));
#159230=CARTESIAN_POINT('Ctrl Pts',(4.11104504267748,5.68047774723022,8.07407757186045));
#159231=CARTESIAN_POINT('Ctrl Pts',(4.02604755290439,5.7410317358922,8.0788099813684));
#159232=CARTESIAN_POINT('Ctrl Pts',(3.93977462314065,5.79963813365601,8.08354239087634));
#159233=CARTESIAN_POINT('Ctrl Pts',(3.78062379549445,5.90775149824227,8.09227243971103));
#159234=CARTESIAN_POINT('Ctrl Pts',(3.61705163562554,6.00928900419594,8.10100248854573));
#159235=CARTESIAN_POINT('Ctrl Pts',(3.44961244000387,6.10391682252228,8.10973253738042));
#159236=CARTESIAN_POINT('Ctrl Pts',(3.28212482912982,6.1985720026004,8.11846511051963));
#159237=CARTESIAN_POINT('Ctrl Pts',(3.11076818908985,6.28631337226274,8.12719768365884));
#159238=CARTESIAN_POINT('Ctrl Pts',(2.93612178165304,6.36685286823896,8.13593025679805));
#159239=CARTESIAN_POINT('Ctrl Pts',(2.75899424321187,6.44853655632009,8.14478689007845));
#159240=CARTESIAN_POINT('Ctrl Pts',(2.57848301538312,6.5228120615465,8.15364352335883));
#159241=CARTESIAN_POINT('Ctrl Pts',(2.39521419140986,6.58942907540318,8.16250015663922));
#159242=CARTESIAN_POINT('Ctrl Pts',(2.21439749230609,6.65515475797466,8.171238288746));
#159243=CARTESIAN_POINT('Ctrl Pts',(2.03089680065212,6.71342554354389,8.1799764208528));
#159244=CARTESIAN_POINT('Ctrl Pts',(1.84533044374377,6.76405071801598,8.18871455295959));
#159245=CARTESIAN_POINT('Ctrl Pts',(1.6559892816241,6.81570571371,8.19763043682679));
#159246=CARTESIAN_POINT('Ctrl Pts',(1.46449779898592,6.85940062961301,8.20654632069398));
#159247=CARTESIAN_POINT('Ctrl Pts',(1.27152670014793,6.89498704953903,8.21546220456118));
#159248=CARTESIAN_POINT('Ctrl Pts',(1.07855560130995,6.93057346946505,8.22437808842837));
#159249=CARTESIAN_POINT('Ctrl Pts',(0.884105184772854,6.95805134455219,
8.23329397229557));
#159250=CARTESIAN_POINT('Ctrl Pts',(0.688855744565208,6.97732787861367,
8.24220985616277));
#159251=CARTESIAN_POINT('Ctrl Pts',(0.497443005196463,6.99622562390973,
8.25095054065896));
#159252=CARTESIAN_POINT('Ctrl Pts',(0.305242022758536,7.00724336029941,
8.25969122515517));
#159253=CARTESIAN_POINT('Ctrl Pts',(0.112898462328194,7.01034096886192,
8.26843190965136));
#159254=CARTESIAN_POINT('Ctrl Pts',(-0.0794104923005177,7.01343802011321,
8.27717102155322));
#159255=CARTESIAN_POINT('Ctrl Pts',(-0.271861700031282,7.00861778488913,
8.28591013345508));
#159256=CARTESIAN_POINT('Ctrl Pts',(-0.463808403015683,6.99589224672536,
8.29464924535694));
#159257=CARTESIAN_POINT('Ctrl Pts',(-0.658242051797386,6.9830018308994,
8.30350158503129));
#159258=CARTESIAN_POINT('Ctrl Pts',(-0.852157745652109,6.96199983140085,
8.31235392470564));
#159259=CARTESIAN_POINT('Ctrl Pts',(-1.04488606462257,6.93295317122924,
8.32120626438));
#159260=CARTESIAN_POINT('Ctrl Pts',(-1.2350517303488,6.9042927361766,8.32994089702973));
#159261=CARTESIAN_POINT('Ctrl Pts',(-1.4240611257198,6.8678003025821,8.33867552967946));
#159262=CARTESIAN_POINT('Ctrl Pts',(-1.61127801080753,6.82359214302761,
8.3474101623292));
#159263=CARTESIAN_POINT('Ctrl Pts',(-1.80227926955795,6.77849036645446,
8.35632135551586));
#159264=CARTESIAN_POINT('Ctrl Pts',(-1.99141449157405,6.72535765834676,
8.36523254870253));
#159265=CARTESIAN_POINT('Ctrl Pts',(-2.17801974077083,6.66437218133206,
8.37414374188919));
#159266=CARTESIAN_POINT('Ctrl Pts',(-2.36462498996762,6.60338670431735,
8.38305493507585));
#159267=CARTESIAN_POINT('Ctrl Pts',(-2.54869997402684,6.53454853975444,
8.39196612826252));
#159268=CARTESIAN_POINT('Ctrl Pts',(-2.7295969416885,6.45809005034962,8.40087732144918));
#159269=CARTESIAN_POINT('Ctrl Pts',(-2.892517709408,6.38922943895561,8.40890298630158));
#159270=CARTESIAN_POINT('Ctrl Pts',(-3.05293536394447,6.31415563055696,
8.41692865115397));
#159271=CARTESIAN_POINT('Ctrl Pts',(-3.21034092784216,6.23308412341126,
8.42495431600637));
#159272=CARTESIAN_POINT('Ctrl Pts',(-3.36769653507477,6.15203834637339,
8.4329774337096));
#159273=CARTESIAN_POINT('Ctrl Pts',(-3.52204162940454,6.06499882797018,
8.44100055141283));
#159274=CARTESIAN_POINT('Ctrl Pts',(-3.6728894627452,5.97222819029509,8.44902366911607));
#159275=CARTESIAN_POINT('Ctrl Pts',(-3.82371827285366,5.87946925180945,
8.45704577503393));
#159276=CARTESIAN_POINT('Ctrl Pts',(-3.97105038861594,5.78098082615529,
8.46506788095178));
#159277=CARTESIAN_POINT('Ctrl Pts',(-4.11442586268289,5.6770702288228,8.47308998686965));
#159278=CARTESIAN_POINT('Ctrl Pts',(-4.2578546155606,5.57312101796113,8.48111507382918));
#159279=CARTESIAN_POINT('Ctrl Pts',(-4.3973234906917,5.46374582318037,8.48914016078872));
#159280=CARTESIAN_POINT('Ctrl Pts',(-4.53240325157572,5.3492940961968,8.49716524774825));
#159281=CARTESIAN_POINT('Ctrl Pts',(-4.66750961574264,5.23481982851836,
8.5051919152085));
#159282=CARTESIAN_POINT('Ctrl Pts',(-4.79822486962966,5.11526728056,8.51321858266876));
#159283=CARTESIAN_POINT('Ctrl Pts',(-4.92415497177501,4.99102438147155,
8.52124525012901));
#159284=CARTESIAN_POINT('Ctrl Pts',(-5.05018617016269,4.86668174062144,
8.52927836136961));
#159285=CARTESIAN_POINT('Ctrl Pts',(-5.17142428999715,4.73764149221596,
8.53731147261022));
#159286=CARTESIAN_POINT('Ctrl Pts',(-5.28751366212846,4.60432686017239,
8.54534458385083));
#159287=CARTESIAN_POINT('Ctrl Pts',(-5.35591773736397,4.52577303605498,
8.55007798481243));
#159288=CARTESIAN_POINT('Ctrl Pts',(-5.42253493239236,4.44573577773099,
8.55481138577402));
#159289=CARTESIAN_POINT('Ctrl Pts',(-5.4872993526033,4.36430663191984,8.55954478673562));
#159290=CARTESIAN_POINT('Ctrl Pts',(-5.62071607384052,4.19656005730543,
8.56929574002974));
#159291=CARTESIAN_POINT('Ctrl Pts',(-5.74634700732665,4.02280664304624,
8.57904669332387));
#159292=CARTESIAN_POINT('Ctrl Pts',(-5.8637365978661,3.84372471352278,8.58879764661799));
#159293=CARTESIAN_POINT('Ctrl Pts',(-5.98129531013271,3.66438478288451,
8.59856264798959));
#159294=CARTESIAN_POINT('Ctrl Pts',(-6.09058890837765,3.47970101358163,
8.60832764936119));
#159295=CARTESIAN_POINT('Ctrl Pts',(-6.19120518797151,3.29038065927556,
8.61809265073278));
#159296=CARTESIAN_POINT('Ctrl Pts',(-6.29165376107438,3.10137586277407,
8.62784137587034));
#159297=CARTESIAN_POINT('Ctrl Pts',(-6.38345390398281,2.90774996033089,
8.63759010100791));
#159298=CARTESIAN_POINT('Ctrl Pts',(-6.46624073214091,2.71023197466597,
8.64733882614547));
#159299=CARTESIAN_POINT('Ctrl Pts',(-6.54880034255623,2.5132560992843,8.65706079481259));
#159300=CARTESIAN_POINT('Ctrl Pts',(-6.62239600826602,2.31240950289493,
8.66678276347969));
#159301=CARTESIAN_POINT('Ctrl Pts',(-6.68671126918446,2.10843993631821,
8.6765047321468));
#159302=CARTESIAN_POINT('Ctrl Pts',(-6.75060097281963,1.90581998308961,
8.68616237308649));
#159303=CARTESIAN_POINT('Ctrl Pts',(-6.80533263618958,1.70011828665719,
8.69582001402617));
#159304=CARTESIAN_POINT('Ctrl Pts',(-6.85064147791335,1.49209178792499,
8.70547765496585));
#159305=CARTESIAN_POINT('Ctrl Pts',(-6.87055627373975,1.40065697981429,
8.70972252065125));
#159306=CARTESIAN_POINT('Ctrl Pts',(-6.88865126635412,1.30877335101945,
8.71396738633665));
#159307=CARTESIAN_POINT('Ctrl Pts',(-6.90490681962792,1.21650662750181,
8.71821225202205));
#159308=CARTESIAN_POINT('Ctrl Pts',(-6.93497517205461,1.04583828338241,
8.72606409903597));
#159309=CARTESIAN_POINT('Ctrl Pts',(-6.95873380167368,0.873928622337296,
8.73391594604989));
#159310=CARTESIAN_POINT('Ctrl Pts',(-6.97608778540275,0.701302910912703,
8.74176779306381));
#159311=CARTESIAN_POINT('Ctrl Pts',(-6.99343684768233,0.528726154744227,
8.7496174133574));
#159312=CARTESIAN_POINT('Ctrl Pts',(-7.00438483889631,0.355434131305913,
8.75746703365098));
#159313=CARTESIAN_POINT('Ctrl Pts',(-7.00888845738292,0.181959210991192,
8.76531665394457));
#159314=CARTESIAN_POINT('Ctrl Pts',(-7.01339171631319,0.00849814043011765,
8.77316564754637));
#159315=CARTESIAN_POINT('Ctrl Pts',(-7.01145161759505,-0.16514541658381,
8.78101464114818));
#159316=CARTESIAN_POINT('Ctrl Pts',(-7.00307694641226,-0.338437357762359,
8.78886363474999));
#159317=CARTESIAN_POINT('Ctrl Pts',(-6.99469803537867,-0.511817031576421,
8.79671660206742));
#159318=CARTESIAN_POINT('Ctrl Pts',(-6.97987806139873,-0.684844352360426,
8.80456956938485));
#159319=CARTESIAN_POINT('Ctrl Pts',(-6.95867786783105,-0.856988269615363,
8.81242253670229));
#159320=CARTESIAN_POINT('Ctrl Pts',(-6.93747229012655,-1.02917590564115,
8.82027749840955));
#159321=CARTESIAN_POINT('Ctrl Pts',(-6.90988332535711,-1.20047931451484,
8.8281324601168));
#159322=CARTESIAN_POINT('Ctrl Pts',(-6.87602316633129,-1.37037658275942,
8.83598742182406));
#159323=CARTESIAN_POINT('Ctrl Pts',(-6.8421293982673,-1.54044248824431,
8.84385018023741));
#159324=CARTESIAN_POINT('Ctrl Pts',(-6.80195209202671,-1.70909909458856,
8.85171293865077));
#159325=CARTESIAN_POINT('Ctrl Pts',(-6.75565379072281,-1.87583805868005,
8.85957569706412));
#159326=CARTESIAN_POINT('Ctrl Pts',(-6.72169002122761,-1.99815537017491,
8.86534370381225));
#159327=CARTESIAN_POINT('Ctrl Pts',(-6.68443330330044,-2.11944099994925,
8.87111171056036));
#159328=CARTESIAN_POINT('Ctrl Pts',(-6.64396427386324,-2.23950112527966,
8.87687971730848));
#159329=CARTESIAN_POINT('Ctrl Pts',(-6.58518275153944,-2.41388921996474,
8.88525778374951));
#159330=CARTESIAN_POINT('Ctrl Pts',(-6.51949218948711,-2.58607740822038,
8.89363585019053));
#159331=CARTESIAN_POINT('Ctrl Pts',(-6.44707966720527,-2.75550182856199,
8.90201391663155));
#159332=CARTESIAN_POINT('Ctrl Pts',(-6.37471665974576,-2.92481039849804,
8.91038625425029));
#159333=CARTESIAN_POINT('Ctrl Pts',(-6.29564098469207,-3.09135866697574,
8.91875859186902));
#159334=CARTESIAN_POINT('Ctrl Pts',(-6.21008852409888,-3.25460091030458,
8.92713092948775));
#159335=CARTESIAN_POINT('Ctrl Pts',(-6.12458201693686,-3.41775547010987,
8.93549877001035));
#159336=CARTESIAN_POINT('Ctrl Pts',(-6.03260581313219,-3.57760725501266,
8.94386661053294));
#159337=CARTESIAN_POINT('Ctrl Pts',(-5.93444279738993,-3.73363298236541,
8.95223445105553));
#159338=CARTESIAN_POINT('Ctrl Pts',(-5.83631812851099,-3.88959775909232,
8.96059902272545));
#159339=CARTESIAN_POINT('Ctrl Pts',(-5.73201164201706,-4.04173918095498,
8.96896359439538));
#159340=CARTESIAN_POINT('Ctrl Pts',(-5.62185104212056,-4.18956052858864,
8.9773281660653));
#159341=CARTESIAN_POINT('Ctrl Pts',(-5.51171735102767,-4.33734576807097,
8.98569069453087));
#159342=CARTESIAN_POINT('Ctrl Pts',(-5.39573259483072,-4.48081277470594,
8.99405322299644));
#159343=CARTESIAN_POINT('Ctrl Pts',(-5.27426674904245,-4.61949529953708,
9.00241575146201));
#159344=CARTESIAN_POINT('Ctrl Pts',(-5.15279120989962,-4.75818889166765,
9.01077894728352));
#159345=CARTESIAN_POINT('Ctrl Pts',(-5.02583391929153,-4.89209698795397,
9.01914214310503));
#159346=CARTESIAN_POINT('Ctrl Pts',(-4.89380445364757,-5.02078724225188,
9.02750533892654));
#159347=CARTESIAN_POINT('Ctrl Pts',(-4.76176598385867,-5.14948627296721,
9.03586910510124));
#159348=CARTESIAN_POINT('Ctrl Pts',(-4.6246548845979,-5.27296652245916,
9.04423287127595));
#159349=CARTESIAN_POINT('Ctrl Pts',(-4.48291695154482,-5.3908331608437,
9.05259663745066));
#159350=CARTESIAN_POINT('Ctrl Pts',(-4.34115045524832,-5.50872355189213,
9.06096208910422));
#159351=CARTESIAN_POINT('Ctrl Pts',(-4.19475551872438,-5.62099786585431,
9.06932754075776));
#159352=CARTESIAN_POINT('Ctrl Pts',(-4.04421063405157,-5.7273018874444,
9.07769299241132));
#159353=CARTESIAN_POINT('Ctrl Pts',(-3.89361533219282,-5.83364151004235,
9.0860612456382));
#159354=CARTESIAN_POINT('Ctrl Pts',(-3.7388675793336,-5.93400666375764,
9.09442949886508));
#159355=CARTESIAN_POINT('Ctrl Pts',(-3.58047477207803,-6.02808650974858,
9.10279775209195));
#159356=CARTESIAN_POINT('Ctrl Pts',(-3.421935112093,-6.12225358117866,9.11117376388342));
#159357=CARTESIAN_POINT('Ctrl Pts',(-3.25974392746319,-6.21012353197168,
9.11954977567489));
#159358=CARTESIAN_POINT('Ctrl Pts',(-3.09443422830602,-6.29143094766112,
9.12792578746637));
#159359=CARTESIAN_POINT('Ctrl Pts',(-2.92904345922981,-6.37277823751186,
9.13630590695752));
#159360=CARTESIAN_POINT('Ctrl Pts',(-2.76053142351737,-6.44755643510344,
9.14468602644866));
#159361=CARTESIAN_POINT('Ctrl Pts',(-2.58945162577646,-6.51554808441037,
9.15306614593981));
#159362=CARTESIAN_POINT('Ctrl Pts',(-2.41817634769534,-6.58361742278939,
9.16145584077902));
#159363=CARTESIAN_POINT('Ctrl Pts',(-2.24432775285461,-6.64488460241941,
9.16984553561824));
#159364=CARTESIAN_POINT('Ctrl Pts',(-2.06847631044044,-6.6991814660932,
9.17823523045745));
#159365=CARTESIAN_POINT('Ctrl Pts',(-1.95683126427435,-6.73365360785283,
9.18356170293207));
#159366=CARTESIAN_POINT('Ctrl Pts',(-1.84437920556129,-6.76531719248854,
9.1888881754067));
#159367=CARTESIAN_POINT('Ctrl Pts',(-1.73126837294955,-6.79413985603216,
9.19421464788132));
#159368=CARTESIAN_POINT('Ctrl Pts',(-1.55328643993816,-6.8394928364106,
9.20259594828622));
#159369=CARTESIAN_POINT('Ctrl Pts',(-1.37331386193084,-6.87790078047717,
9.21097724869112));
#159370=CARTESIAN_POINT('Ctrl Pts',(-1.1919184300458,-6.90919365907609,
9.21935854909601));
#159371=CARTESIAN_POINT('Ctrl Pts',(-1.01075289031636,-6.94044687853232,
9.22772922742957));
#159372=CARTESIAN_POINT('Ctrl Pts',(-0.828168410681715,-6.96460294782168,
9.23609990576311));
#159373=CARTESIAN_POINT('Ctrl Pts',(-0.644746374589701,-6.98154199836637,
9.24447058409667));
#159374=CARTESIAN_POINT('Ctrl Pts',(-0.46153249101654,-6.99846182599699,
9.2528317631475));
#159375=CARTESIAN_POINT('Ctrl Pts',(-0.277483269681747,-7.00818092866042,
9.26119294219835));
#159376=CARTESIAN_POINT('Ctrl Pts',(-0.0931891295821639,-7.01063066696768,
9.26955412124917));
#159377=CARTESIAN_POINT('Ctrl Pts',(0.0908658671312361,-7.01307722645052,
9.27790445068389));
#159378=CARTESIAN_POINT('Ctrl Pts',(0.275164822626464,-7.00827323207764,
9.28625478011861));
#159379=CARTESIAN_POINT('Ctrl Pts',(0.459113446337256,-6.99620192718109,
9.29460510955333));
#159380=CARTESIAN_POINT('Ctrl Pts',(0.64292053258566,-6.98413991043156,
9.30294901390906));
#159381=CARTESIAN_POINT('Ctrl Pts',(0.826377498673072,-6.96482174788353,
9.31129291826479));
#159382=CARTESIAN_POINT('Ctrl Pts',(1.00889015050328,-6.93828272894075,
9.31963682262052));
#159383=CARTESIAN_POINT('Ctrl Pts',(1.19125620703326,-6.9117650263035,9.32797402510024));
#159384=CARTESIAN_POINT('Ctrl Pts',(1.37267913868257,-6.87803808123059,
9.33631122757996));
#159385=CARTESIAN_POINT('Ctrl Pts',(1.55256981481071,-6.83718900811135,
9.34464843005967));
#159386=CARTESIAN_POINT('Ctrl Pts',(1.61178883241873,-6.82374171872212,
9.34739299109571));
#159387=CARTESIAN_POINT('Ctrl Pts',(1.67084185141757,-6.80952302812026,
9.35013755213173));
#159388=CARTESIAN_POINT('Ctrl Pts',(1.72970803380628,-6.79453726756179,
9.35288211316777));
#159389=CARTESIAN_POINT('Ctrl Pts',(1.90855065694367,-6.74900870397519,
9.36122042346967));
#159390=CARTESIAN_POINT('Ctrl Pts',(2.08552113087069,-6.69643353800162,
9.36955873377158));
#159391=CARTESIAN_POINT('Ctrl Pts',(2.26005401679439,-6.63700100976876,
9.37789704407349));
#159392=CARTESIAN_POINT('Ctrl Pts',(2.43469671288792,-6.57753108860572,
9.38624060055731));
#159393=CARTESIAN_POINT('Ctrl Pts',(2.60689845176619,-6.5111953051539,9.39458415704114));
#159394=CARTESIAN_POINT('Ctrl Pts',(2.77611294521756,-6.43823139362787,
9.40292771352497));
#159395=CARTESIAN_POINT('Ctrl Pts',(2.94545617631766,-6.36521197147612,
9.41127761775018));
#159396=CARTESIAN_POINT('Ctrl Pts',(3.11180732819729,-6.28555449239434,
9.41962752197539));
#159397=CARTESIAN_POINT('Ctrl Pts',(3.27464352290386,-6.19954323804615,
9.42797742620061));
#159398=CARTESIAN_POINT('Ctrl Pts',(3.43772395985251,-6.11340297318133,
9.43633985466426));
#159399=CARTESIAN_POINT('Ctrl Pts',(3.59727861419359,-6.02089004189167,
9.4447022831279));
#159400=CARTESIAN_POINT('Ctrl Pts',(3.75281118749222,-5.92233355642295,
9.45306471159156));
#159401=CARTESIAN_POINT('Ctrl Pts',(3.90847676234316,-5.82369279172396,
9.46143429107151));
#159402=CARTESIAN_POINT('Ctrl Pts',(4.06011312461653,-5.71899834694114,
9.46980387055147));
#159403=CARTESIAN_POINT('Ctrl Pts',(4.20725559066611,-5.60862077139369,
9.47817345003142));
#159404=CARTESIAN_POINT('Ctrl Pts',(4.35462500604198,-5.49807295188418,
9.48655593856799));
#159405=CARTESIAN_POINT('Ctrl Pts',(4.49748642076467,-5.38182469185198,
9.49493842710455));
#159406=CARTESIAN_POINT('Ctrl Pts',(4.63540959522959,-5.26028558606408,
9.50332091564112));
#159407=CARTESIAN_POINT('Ctrl Pts',(4.68054031791934,-5.22051599911428,
9.50606380324548));
#159408=CARTESIAN_POINT('Ctrl Pts',(4.72514260623293,-5.18018020006754,
9.50880669084984));
#159409=CARTESIAN_POINT('Ctrl Pts',(4.76920229736288,-5.13929333754444,
9.5115495784542));
#159410=CARTESIAN_POINT('Ctrl Pts',(4.90163784191209,-5.0163947478293,9.51979420759718));
#159411=CARTESIAN_POINT('Ctrl Pts',(5.02946326007933,-4.88824085956467,
9.52803883674016));
#159412=CARTESIAN_POINT('Ctrl Pts',(5.15224421891428,-4.75520830996544,
9.53628346588314));
#159413=CARTESIAN_POINT('Ctrl Pts',(5.27490518171818,-4.62230577546061,
9.54452003740233));
#159414=CARTESIAN_POINT('Ctrl Pts',(5.39253127495641,-4.48453433245291,
9.55275660892152));
#159415=CARTESIAN_POINT('Ctrl Pts',(5.50472345142624,-4.34230886577843,
9.56099318044071));
#159416=CARTESIAN_POINT('Ctrl Pts',(5.61682639527973,-4.20019651884993,
9.56922320096099));
#159417=CARTESIAN_POINT('Ctrl Pts',(5.72350382148417,-4.05363747813611,
9.57745322148126));
#159418=CARTESIAN_POINT('Ctrl Pts',(5.82439541115204,-3.90308143100437,
9.58568324200154));
#159419=CARTESIAN_POINT('Ctrl Pts',(5.92521986830862,-3.75262556274348,
9.59390778632754));
#159420=CARTESIAN_POINT('Ctrl Pts',(6.02026597205407,-3.5981782768221,9.60213233065354));
#159421=CARTESIAN_POINT('Ctrl Pts',(6.1092152791352,-3.44022023069469,9.61035687497954));
#159422=CARTESIAN_POINT('Ctrl Pts',(6.19813176112689,-3.28232047604994,
9.61857838419024));
#159423=CARTESIAN_POINT('Ctrl Pts',(6.2809557596573,-3.12091284334057,9.62679989340093));
#159424=CARTESIAN_POINT('Ctrl Pts',(6.35741332620368,-2.95650509255571,
9.63502140261163));
#159425=CARTESIAN_POINT('Ctrl Pts',(6.4338552822269,-2.79213090929226,9.64324123321724));
#159426=CARTESIAN_POINT('Ctrl Pts',(6.50393325101697,-2.62475814206892,
9.65146106382287));
#159427=CARTESIAN_POINT('Ctrl Pts',(6.56742014076435,-2.45491736259751,
9.65968089442848));
#159428=CARTESIAN_POINT('Ctrl Pts',(6.63090453343465,-2.28508326333237,
9.66790040173033));
#159429=CARTESIAN_POINT('Ctrl Pts',(6.68779824362939,-2.11278166948833,
9.67611990903217));
#159430=CARTESIAN_POINT('Ctrl Pts',(6.73792297411684,-1.93856146597638,
9.68433941633402));
#159431=CARTESIAN_POINT('Ctrl Pts',(6.78806944695646,-1.76426569184326,
9.6925624889702));
#159432=CARTESIAN_POINT('Ctrl Pts',(6.83144097603342,-1.58804997731326,
9.70078556160637));
#159433=CARTESIAN_POINT('Ctrl Pts',(6.86790944372065,-1.41047737853278,
9.70900863424255));
#159434=CARTESIAN_POINT('Ctrl Pts',(6.90438617357222,-1.2328645495456,9.71723356986837));
#159435=CARTESIAN_POINT('Ctrl Pts',(6.9339566615384,-1.05389456364962,9.72545850549418));
#159436=CARTESIAN_POINT('Ctrl Pts',(6.95654419597645,-0.874139240582622,
9.73368344112));
#159437=CARTESIAN_POINT('Ctrl Pts',(6.97914965908088,-0.694241238232732,
9.74191490521962));
#159438=CARTESIAN_POINT('Ctrl Pts',(6.99476105883144,-0.513556997444592,
9.75014636931923));
#159439=CARTESIAN_POINT('Ctrl Pts',(7.00335362096458,-0.332662925830885,
9.75837783341885));
#159440=CARTESIAN_POINT('Ctrl Pts',(7.0086274243415,-0.221636697453453,
9.76343000790335));
#159441=CARTESIAN_POINT('Ctrl Pts',(7.01125821309936,-0.110531466213418,
9.76848218238786));
#159442=CARTESIAN_POINT('Ctrl Pts',(7.01124998073505,0.000519752639607109,
9.77353435687236));
#159443=CARTESIAN_POINT('Ctrl Pts',(7.01124998073499,0.000519753478595656,
9.77353435691053));
#159444=CARTESIAN_POINT('Ctrl Pts',(7.01122549278315,0.330851649082017,
9.78856250690858));
#159445=CARTESIAN_POINT('Ctrl Pts',(6.98785181828166,0.660634656774128,
9.80359065690662));
#159446=CARTESIAN_POINT('Ctrl Pts',(6.94138454713677,0.987323215198966,
9.81861880690467));
#159447=CARTESIAN_POINT('Ctrl Pts',(6.93080397747084,1.06171000328255,9.82204070761214));
#159448=CARTESIAN_POINT('Ctrl Pts',(6.91902627410213,1.13593643056938,9.82546260831958));
#159449=CARTESIAN_POINT('Ctrl Pts',(6.90605482080883,1.20997246848147,9.82888450902704));
#159450=CARTESIAN_POINT('Ctrl Pts',(6.87624591910682,1.38011014901938,9.83674816929057));
#159451=CARTESIAN_POINT('Ctrl Pts',(6.84010208160346,1.54939332710809,9.8446118295541));
#159452=CARTESIAN_POINT('Ctrl Pts',(6.79768561947328,1.71729344647505,9.85247548981762));
#159453=CARTESIAN_POINT('Ctrl Pts',(6.75530637964033,1.88504622615753,9.86033224937598));
#159454=CARTESIAN_POINT('Ctrl Pts',(6.706665562064,2.05141799498684,9.86818900893433));
#159455=CARTESIAN_POINT('Ctrl Pts',(6.65187693518678,2.2158880390557,9.87604576849268));
#159456=CARTESIAN_POINT('Ctrl Pts',(6.62628932079653,2.29269952907191,9.87971506530471));
#159457=CARTESIAN_POINT('Ctrl Pts',(6.59936152799537,2.36909635782941,9.88338436211673));
#159458=CARTESIAN_POINT('Ctrl Pts',(6.57110895151814,2.44502632087636,9.88705365892876));
#159459=CARTESIAN_POINT('',(7.01124990260052,0.0011686677202812,9.22646564312219));
#159460=CARTESIAN_POINT('Ctrl Pts',(6.57110895151814,2.44502632087636,9.34006375887581));
#159461=CARTESIAN_POINT('Ctrl Pts',(6.6443561952353,2.24817133622682,9.33053023629209));
#159462=CARTESIAN_POINT('Ctrl Pts',(6.70867476342362,2.04823487019919,9.32099671370838));
#159463=CARTESIAN_POINT('Ctrl Pts',(6.76387515396249,1.84597385249871,9.31146319112466));
#159464=CARTESIAN_POINT('Ctrl Pts',(6.8192203234386,1.64318234697191,9.30190466412966));
#159465=CARTESIAN_POINT('Ctrl Pts',(6.86539944347675,1.43805418440369,9.29234613713465));
#159466=CARTESIAN_POINT('Ctrl Pts',(6.90227373070976,1.23135856226121,9.28278761013965));
#159467=CARTESIAN_POINT('Ctrl Pts',(6.93922415287218,1.02423617236859,9.2732093475014));
#159468=CARTESIAN_POINT('Ctrl Pts',(6.96683128480148,0.815539939704676,
9.26363108486317));
#159469=CARTESIAN_POINT('Ctrl Pts',(6.98500763070788,0.606048646110736,
9.25405282222492));
#159470=CARTESIAN_POINT('Ctrl Pts',(7.00245805043746,0.404924007432989,
9.24485709585735));
#159471=CARTESIAN_POINT('Ctrl Pts',(7.01121624930699,0.203066646850565,
9.23566136948977));
#159472=CARTESIAN_POINT('Ctrl Pts',(7.01124990260052,0.00116866772027653,
9.2264656431222));
#159473=CARTESIAN_POINT('Ctrl Pts',(7.01124990260064,0.00116866700544844,
9.22646564308963));
#159474=CARTESIAN_POINT('Ctrl Pts',(7.01127887818486,-0.172666190258528,
9.21854809093071));
#159475=CARTESIAN_POINT('Ctrl Pts',(7.00484218383645,-0.346555053651323,
9.21063053877179));
#159476=CARTESIAN_POINT('Ctrl Pts',(6.99193196050225,-0.520109625182228,
9.20271298661287));
#159477=CARTESIAN_POINT('Ctrl Pts',(6.97883341556641,-0.696195839585311,
9.19467994101399));
#159478=CARTESIAN_POINT('Ctrl Pts',(6.9590649918697,-0.871970795754378,
9.1866468954151));
#159479=CARTESIAN_POINT('Ctrl Pts',(6.93265185505888,-1.04688338369119,
9.17861384981622));
#159480=CARTESIAN_POINT('Ctrl Pts',(6.90625569762941,-1.22168353108165,
9.17058596816835));
#159481=CARTESIAN_POINT('Ctrl Pts',(6.8732233840713,-1.39562205276577,9.16255808652047));
#159482=CARTESIAN_POINT('Ctrl Pts',(6.83363198264051,-1.56815193407168,
9.15453020487261));
#159483=CARTESIAN_POINT('Ctrl Pts',(6.79405845711781,-1.74060391643517,
9.14650594789245));
#159484=CARTESIAN_POINT('Ctrl Pts',(6.74793182221218,-1.9116481682579,9.1384816909123));
#159485=CARTESIAN_POINT('Ctrl Pts',(6.69538041288335,-2.0807469065886,9.13045743393214));
#159486=CARTESIAN_POINT('Ctrl Pts',(6.64283535755508,-2.24982519915979,
9.12243414716638));
#159487=CARTESIAN_POINT('Ctrl Pts',(6.58386717645966,-2.41695809464307,
9.11441086040061));
#159488=CARTESIAN_POINT('Ctrl Pts',(6.518654392187,-2.58162186962405,9.10638757363485));
#159489=CARTESIAN_POINT('Ctrl Pts',(6.45344695152034,-2.74627215187738,
9.09836494430587));
#159490=CARTESIAN_POINT('Ctrl Pts',(6.38199606565139,-2.9084533772295,9.09034231497688));
#159491=CARTESIAN_POINT('Ctrl Pts',(6.30452871829496,-3.06766103125723,
9.0823196856479));
#159492=CARTESIAN_POINT('Ctrl Pts',(6.22703224873098,-3.22692853602856,
9.07429404038144));
#159493=CARTESIAN_POINT('Ctrl Pts',(6.14351496262899,-3.38321990785342,
9.06626839511497));
#159494=CARTESIAN_POINT('Ctrl Pts',(6.05425036654084,-3.53605416555518,
9.05824274984851));
#159495=CARTESIAN_POINT('Ctrl Pts',(6.00161452117611,-3.62617455714782,
9.05351034034116));
#159496=CARTESIAN_POINT('Ctrl Pts',(5.94698119959167,-3.71509339081393,
9.0487779308338));
#159497=CARTESIAN_POINT('Ctrl Pts',(5.89041361735245,-3.80271665773416,
9.04404552132645));
#159498=CARTESIAN_POINT('Ctrl Pts',(5.78606133029057,-3.96435850171983,
9.03531547249181));
#159499=CARTESIAN_POINT('Ctrl Pts',(5.67507237408558,-4.12167082863513,
9.02658542365718));
#159500=CARTESIAN_POINT('Ctrl Pts',(5.55782685636029,-4.27412999301851,
9.01785537482254));
#159501=CARTESIAN_POINT('Ctrl Pts',(5.44054743694793,-4.4266332411586,9.00912280168344));
#159502=CARTESIAN_POINT('Ctrl Pts',(5.31700801196676,-4.5742803085538,9.00039022854433));
#159503=CARTESIAN_POINT('Ctrl Pts',(5.18762953249469,-4.71657994696251,
8.99165765540523));
#159504=CARTESIAN_POINT('Ctrl Pts',(5.05641302519356,-4.86090117888916,
8.9828010221248));
#159505=CARTESIAN_POINT('Ctrl Pts',(4.91919048775539,-4.99972167185865,
8.97394438884436));
#159506=CARTESIAN_POINT('Ctrl Pts',(4.77644072199006,-5.13256666705997,
8.96508775556393));
#159507=CARTESIAN_POINT('Ctrl Pts',(4.63560093874928,-5.26363420491874,
8.95634962345722));
#159508=CARTESIAN_POINT('Ctrl Pts',(4.48938113564619,-5.38888498323262,
8.9476114913505));
#159509=CARTESIAN_POINT('Ctrl Pts',(4.33827621675964,-5.50790214415595,
8.93887335924379));
#159510=CARTESIAN_POINT('Ctrl Pts',(4.18409750990132,-5.6293403613915,8.92995747537649));
#159511=CARTESIAN_POINT('Ctrl Pts',(4.02483304193899,-5.74428844899757,
8.92104159150919));
#159512=CARTESIAN_POINT('Ctrl Pts',(3.86104244633639,-5.85234805783873,
8.91212570764189));
#159513=CARTESIAN_POINT('Ctrl Pts',(3.69725185073379,-5.96040766667988,
8.90320982377459));
#159514=CARTESIAN_POINT('Ctrl Pts',(3.52893538326675,-6.06157863529755,
8.89429393990729));
#159515=CARTESIAN_POINT('Ctrl Pts',(3.35668320892921,-6.15551008425725,
8.88537805604));
#159516=CARTESIAN_POINT('Ctrl Pts',(3.18781583334579,-6.24759575650828,
8.87663737154375));
#159517=CARTESIAN_POINT('Ctrl Pts',(3.01514805500628,-6.33273356531839,
8.86789668704751));
#159518=CARTESIAN_POINT('Ctrl Pts',(2.83925870844214,-6.41063464479419,
8.85915600255126));
#159519=CARTESIAN_POINT('Ctrl Pts',(2.66340100729269,-6.48852170857198,
8.85041689064932));
#159520=CARTESIAN_POINT('Ctrl Pts',(2.48432314570172,-6.55917453238893,
8.84167777874739));
#159521=CARTESIAN_POINT('Ctrl Pts',(2.30262529379728,-6.6223517966705,8.83293866684545));
#159522=CARTESIAN_POINT('Ctrl Pts',(2.11857328471429,-6.6863476133382,8.82408632717113));
#159523=CARTESIAN_POINT('Ctrl Pts',(1.93183318237887,-6.74267269199388,
8.81523398749681));
#159524=CARTESIAN_POINT('Ctrl Pts',(1.7430474591679,-6.79112745555466,8.80638164782249));
#159525=CARTESIAN_POINT('Ctrl Pts',(1.55677196563332,-6.83893793000617,
8.79764701517271));
#159526=CARTESIAN_POINT('Ctrl Pts',(1.36850518904379,-6.87908603184273,
8.78891238252292));
#159527=CARTESIAN_POINT('Ctrl Pts',(1.17887830698919,-6.91143056825505,
8.78017774987315));
#159528=CARTESIAN_POINT('Ctrl Pts',(0.985418335961838,-6.94442891221042,
8.77126655668655));
#159529=CARTESIAN_POINT('Ctrl Pts',(0.790542970508542,-6.96930478037182,
8.76235536349997));
#159530=CARTESIAN_POINT('Ctrl Pts',(0.594933037498019,-6.98596315788978,
8.75344417031337));
#159531=CARTESIAN_POINT('Ctrl Pts',(0.399323104487497,-7.00262153540775,
8.74453297712678));
#159532=CARTESIAN_POINT('Ctrl Pts',(0.202978904812929,-7.01106238313507,
8.73562178394019));
#159533=CARTESIAN_POINT('Ctrl Pts',(0.00658751125854588,-7.01124690530832,
8.72671059075359));
#159534=CARTESIAN_POINT('Ctrl Pts',(-0.170287961144563,-7.01141309103556,
8.71868492590123));
#159535=CARTESIAN_POINT('Ctrl Pts',(-0.347283000348599,-7.00488188201524,
8.71065926104888));
#159536=CARTESIAN_POINT('Ctrl Pts',(-0.523844888054318,-6.99165310178926,
8.70263359619653));
#159537=CARTESIAN_POINT('Ctrl Pts',(-0.700350739347519,-6.97842852005365,
8.69461047849335));
#159538=CARTESIAN_POINT('Ctrl Pts',(-0.876423347724347,-6.95851062642729,
8.68658736079017));
#159539=CARTESIAN_POINT('Ctrl Pts',(-1.05151207543291,-6.93195130664655,
8.67856424308699));
#159540=CARTESIAN_POINT('Ctrl Pts',(-1.22657872291956,-6.90539533622863,
8.67054213716921));
#159541=CARTESIAN_POINT('Ctrl Pts',(-1.40066137465016,-6.87219966348944,
8.66252003125144));
#159542=CARTESIAN_POINT('Ctrl Pts',(-1.57321663076453,-6.83246778222817,
8.65449792533366));
#159543=CARTESIAN_POINT('Ctrl Pts',(-1.74583600899621,-6.79272113646532,
8.64647283837417));
#159544=CARTESIAN_POINT('Ctrl Pts',(-1.91692649952479,-6.74643350945737,
8.63844775141469));
#159545=CARTESIAN_POINT('Ctrl Pts',(-2.08595653833109,-6.69375917423788,
8.6304226644552));
#159546=CARTESIAN_POINT('Ctrl Pts',(-2.2550198667579,-6.64107446507159,
8.62239599699498));
#159547=CARTESIAN_POINT('Ctrl Pts',(-2.42202158770787,-6.58200065935708,
8.61436932953476));
#159548=CARTESIAN_POINT('Ctrl Pts',(-2.5864475293609,-6.51674119022406,
8.60634266207454));
#159549=CARTESIAN_POINT('Ctrl Pts',(-2.75100547158014,-6.45142933101932,
8.59830955083399));
#159550=CARTESIAN_POINT('Ctrl Pts',(-2.91298316731429,-6.37992203423224,
8.59027643959342));
#159551=CARTESIAN_POINT('Ctrl Pts',(-3.07188800419658,-6.30247020240264,
8.58224332835287));
#159552=CARTESIAN_POINT('Ctrl Pts',(-3.16552050662644,-6.25683276949458,
8.57750992739096));
#159553=CARTESIAN_POINT('Ctrl Pts',(-3.25808657030887,-6.20913227422216,
8.57277652642905));
#159554=CARTESIAN_POINT('Ctrl Pts',(-3.34948980370665,-6.15942729621555,
8.56804312546714));
#159555=CARTESIAN_POINT('Ctrl Pts',(-3.53778330915515,-6.0570334946049,
8.55829217217283));
#159556=CARTESIAN_POINT('Ctrl Pts',(-3.72125190656563,-5.94607109475091,
8.54854121887851));
#159557=CARTESIAN_POINT('Ctrl Pts',(-3.89921147911015,-5.82698690608411,
8.5387902655842));
#159558=CARTESIAN_POINT('Ctrl Pts',(-4.07742743580522,-5.70773115430261,
8.52902526421232));
#159559=CARTESIAN_POINT('Ctrl Pts',(-4.250118459623,-5.58033022982944,8.51926026284045));
#159560=CARTESIAN_POINT('Ctrl Pts',(-4.41662906055381,-5.44527449298671,
8.50949526146857));
#159561=CARTESIAN_POINT('Ctrl Pts',(-4.5828621228114,-5.31044386607573,
8.49974653633082));
#159562=CARTESIAN_POINT('Ctrl Pts',(-4.74293532122369,-5.1679839507073,
8.48999781119308));
#159563=CARTESIAN_POINT('Ctrl Pts',(-4.89622824126452,-5.01842361423821,
8.48024908605532));
#159564=CARTESIAN_POINT('Ctrl Pts',(-5.0491004316789,-4.86927376290099,
8.47052711738802));
#159565=CARTESIAN_POINT('Ctrl Pts',(-5.19522946543464,-4.71306242276272,
8.46080514872073));
#159566=CARTESIAN_POINT('Ctrl Pts',(-5.33403220687575,-4.55035459920568,
8.45108318005343));
#159567=CARTESIAN_POINT('Ctrl Pts',(-5.47191652683011,-4.38872337082007,
8.44142553911356));
#159568=CARTESIAN_POINT('Ctrl Pts',(-5.60257113408197,-4.22068136269092,
8.43176789817369));
#159569=CARTESIAN_POINT('Ctrl Pts',(-5.72545688970472,-4.04682220595776,
8.42211025723382));
#159570=CARTESIAN_POINT('Ctrl Pts',(-5.77946940998658,-3.97040512098604,
8.41786539154946));
#159571=CARTESIAN_POINT('Ctrl Pts',(-5.83198149049903,-3.89286473541701,
8.4136205258651));
#159572=CARTESIAN_POINT('Ctrl Pts',(-5.88294940643042,-3.81425390396077,
8.40937566018074));
#159573=CARTESIAN_POINT('Ctrl Pts',(-5.97722618884602,-3.6688452460379,
8.40152381316689));
#159574=CARTESIAN_POINT('Ctrl Pts',(-6.06617771077686,-3.51983172051869,
8.39367196615304));
#159575=CARTESIAN_POINT('Ctrl Pts',(-6.14951162340794,-3.36765992286494,
8.3858201191392));
#159576=CARTESIAN_POINT('Ctrl Pts',(-6.23282190321506,-3.21553127990284,
8.37797049884569));
#159577=CARTESIAN_POINT('Ctrl Pts',(-6.31051755964291,-3.06024648067694,
8.37012087855218));
#159578=CARTESIAN_POINT('Ctrl Pts',(-6.38235100187401,-2.90227880317827,
8.36227125825867));
#159579=CARTESIAN_POINT('Ctrl Pts',(-6.45417870912356,-2.74432373737807,
8.35442226465694));
#159580=CARTESIAN_POINT('Ctrl Pts',(-6.520144976658,-2.5836865672631,8.34657327105521));
#159581=CARTESIAN_POINT('Ctrl Pts',(-6.58004949623077,-2.42086248879468,
8.33872427745347));
#159582=CARTESIAN_POINT('Ctrl Pts',(-6.63998434370778,-2.25795597726288,
8.3308713101361));
#159583=CARTESIAN_POINT('Ctrl Pts',(-6.69385117955146,-2.09286070367149,
8.32301834281873));
#159584=CARTESIAN_POINT('Ctrl Pts',(-6.74149881819546,-1.92608936624686,
8.31516537550136));
#159585=CARTESIAN_POINT('Ctrl Pts',(-6.78915855773862,-1.75927567450637,
8.30731041379416));
#159586=CARTESIAN_POINT('Ctrl Pts',(-6.8305958623034,-1.59078544138089,
8.29945545208697));
#159587=CARTESIAN_POINT('Ctrl Pts',(-6.86571039080206,-1.42114298792651,
8.29160049037977));
#159588=CARTESIAN_POINT('Ctrl Pts',(-6.90085977340539,-1.25133215015704,
8.2837377319665));
#159589=CARTESIAN_POINT('Ctrl Pts',(-6.92967378203492,-1.08036718384407,
8.27587497355323));
#159590=CARTESIAN_POINT('Ctrl Pts',(-6.95210372994142,-0.908779561078822,
8.26801221513996));
#159591=CARTESIAN_POINT('Ctrl Pts',(-6.96855801787632,-0.7829053431442,
8.2622442083914));
#159592=CARTESIAN_POINT('Ctrl Pts',(-6.98157782023741,-0.656696184326862,
8.25647620164285));
#159593=CARTESIAN_POINT('Ctrl Pts',(-6.99116175634591,-0.530362007600873,
8.25070819489429));
#159594=CARTESIAN_POINT('Ctrl Pts',(-7.00508248442126,-0.346860813423779,
8.24233012845327));
#159595=CARTESIAN_POINT('Ctrl Pts',(-7.0117834348992,-0.162689373237821,
8.23395206201226));
#159596=CARTESIAN_POINT('Ctrl Pts',(-7.01121685033776,0.0215601493483096,
8.22557399557124));
#159597=CARTESIAN_POINT('Ctrl Pts',(-7.01065065320011,0.205683684299958,
8.21720165795251));
#159598=CARTESIAN_POINT('Ctrl Pts',(-7.00282682965187,0.389884867529372,
8.20882932033377));
#159599=CARTESIAN_POINT('Ctrl Pts',(-6.98774963364724,0.573569193701026,
8.20045698271505));
#159600=CARTESIAN_POINT('Ctrl Pts',(-6.97268053616941,0.757154856139826,
8.1920891421925));
#159601=CARTESIAN_POINT('Ctrl Pts',(-6.95036586143784,0.940223888185467,
8.18372130166996));
#159602=CARTESIAN_POINT('Ctrl Pts',(-6.92086189661233,1.12218410722998,
8.17535346114742));
#159603=CARTESIAN_POINT('Ctrl Pts',(-6.89136945735466,1.30407324447717,
8.16698888947752));
#159604=CARTESIAN_POINT('Ctrl Pts',(-6.85469338100372,1.48485410849331,
8.15862431780762));
#159605=CARTESIAN_POINT('Ctrl Pts',(-6.81094158624654,1.66394148672285,
8.15025974613773));
#159606=CARTESIAN_POINT('Ctrl Pts',(-6.76720047869017,1.84298511948361,
8.14189721767218));
#159607=CARTESIAN_POINT('Ctrl Pts',(-6.71638717788505,2.02033577249617,
8.13353468920663));
#159608=CARTESIAN_POINT('Ctrl Pts',(-6.65866041230502,2.19541979495995,
8.12517216074108));
#159609=CARTESIAN_POINT('Ctrl Pts',(-6.60092903994836,2.37051778967687,
8.11680896491957));
#159610=CARTESIAN_POINT('Ctrl Pts',(-6.53628319774413,2.54334847843099,
8.10844576909806));
#159611=CARTESIAN_POINT('Ctrl Pts',(-6.46493130449214,2.71335397445626,
8.10008257327656));
#159612=CARTESIAN_POINT('Ctrl Pts',(-6.39357454518413,2.88337106451541,
8.09171880710187));
#159613=CARTESIAN_POINT('Ctrl Pts',(-6.31551094993941,3.05056227436935,
8.08335504092719));
#159614=CARTESIAN_POINT('Ctrl Pts',(-6.23099692415811,3.21439012778974,
8.0749912747525));
#159615=CARTESIAN_POINT('Ctrl Pts',(-6.14646586698207,3.3782509960478,8.06662582309896));
#159616=CARTESIAN_POINT('Ctrl Pts',(-6.05548193798342,3.53874686415457,
8.05826037144542));
#159617=CARTESIAN_POINT('Ctrl Pts',(-5.95834749445622,3.69536489372934,
8.04989491979188));
#159618=CARTESIAN_POINT('Ctrl Pts',(-5.8611805207953,3.85203537437359,8.04152666656507));
#159619=CARTESIAN_POINT('Ctrl Pts',(-5.7578590985367,4.00482514758256,8.03315841333824));
#159620=CARTESIAN_POINT('Ctrl Pts',(-5.64872912316993,4.15325003527983,
8.02479016011143));
#159621=CARTESIAN_POINT('Ctrl Pts',(-5.53949796874631,4.30181253402392,
8.01641414831997));
#159622=CARTESIAN_POINT('Ctrl Pts',(-5.4244476946266,4.44600179523599,8.0080381365285));
#159623=CARTESIAN_POINT('Ctrl Pts',(-5.30396550340238,4.585365470845,7.99966212473704));
#159624=CARTESIAN_POINT('Ctrl Pts',(-5.18342422622279,4.72479749212263,
7.99128200524589));
#159625=CARTESIAN_POINT('Ctrl Pts',(-5.05744593948409,4.85939896419983,
7.98290188575475));
#159626=CARTESIAN_POINT('Ctrl Pts',(-4.9264554283491,4.98875369957164,7.97452176626361));
#159627=CARTESIAN_POINT('Ctrl Pts',(-4.79531524396207,5.11825623911446,
7.9661320714244));
#159628=CARTESIAN_POINT('Ctrl Pts',(-4.65915162980593,5.24249983616411,
7.95774237658519));
#159629=CARTESIAN_POINT('Ctrl Pts',(-4.51842422648261,5.36110707522569,
7.94935268174598));
#159630=CARTESIAN_POINT('Ctrl Pts',(-4.42907882660513,5.43640876453474,
7.94402620927113));
#159631=CARTESIAN_POINT('Ctrl Pts',(-4.33789453138378,5.50943939103424,
7.93869973679628));
#159632=CARTESIAN_POINT('Ctrl Pts',(-4.24499520190079,5.58011131594516,
7.93337326432143));
#159633=CARTESIAN_POINT('Ctrl Pts',(-4.09881643320985,5.69131486307507,
7.92499196391622));
#159634=CARTESIAN_POINT('Ctrl Pts',(-3.94809497438731,5.79690056691332,
7.916610663511));
#159635=CARTESIAN_POINT('Ctrl Pts',(-3.79328726983628,5.89649033332524,
7.90822936310578));
#159636=CARTESIAN_POINT('Ctrl Pts',(-3.63867576138863,5.99595388428708,
7.8998586847719));
#159637=CARTESIAN_POINT('Ctrl Pts',(-3.47998860118254,6.08943646595476,
7.89148800643802));
#159638=CARTESIAN_POINT('Ctrl Pts',(-3.31771432034658,6.17660086544916,
7.88311732810414));
#159639=CARTESIAN_POINT('Ctrl Pts',(-3.15562419295871,6.26366634831526,
7.87475614905302));
#159640=CARTESIAN_POINT('Ctrl Pts',(-2.98995534531653,6.34442778560906,
7.86639497000189));
#159641=CARTESIAN_POINT('Ctrl Pts',(-2.82122461662683,6.41859160759109,
7.85803379095077));
#159642=CARTESIAN_POINT('Ctrl Pts',(-2.65271283596032,6.49265919326608,
7.84968346151571));
#159643=CARTESIAN_POINT('Ctrl Pts',(-2.48114739765742,6.56014610859907,
7.84133313208065));
#159644=CARTESIAN_POINT('Ctrl Pts',(-2.30706894932868,6.62080504361391,
7.8329828026456));
#159645=CARTESIAN_POINT('Ctrl Pts',(-2.13312444395439,6.68141730520625,
7.82463889828961));
#159646=CARTESIAN_POINT('Ctrl Pts',(-1.95667108997936,6.73521194883618,
7.81629499393363));
#159647=CARTESIAN_POINT('Ctrl Pts',(-1.77826975363068,6.78198962295154,
7.80795108957764));
#159648=CARTESIAN_POINT('Ctrl Pts',(-1.60001171034735,6.82872972494747,
7.79961388709764));
#159649=CARTESIAN_POINT('Ctrl Pts',(-1.41980912114422,6.8684640149127,7.79127668461763));
#159650=CARTESIAN_POINT('Ctrl Pts',(-1.23823841130986,6.90104283418505,
7.78293948213764));
#159651=CARTESIAN_POINT('Ctrl Pts',(-1.17846633592108,6.91176760165113,
7.78019492110342));
#159652=CARTESIAN_POINT('Ctrl Pts',(-1.11854611485407,6.92171734123032,
7.7774503600692));
#159653=CARTESIAN_POINT('Ctrl Pts',(-1.0584986244211,6.93088791026075,7.77470579903499));
#159654=CARTESIAN_POINT('Ctrl Pts',(-0.876067043632634,6.95874921458652,
7.76636748873373));
#159655=CARTESIAN_POINT('Ctrl Pts',(-0.692609763917193,6.97939196714889,
7.75802917843247));
#159656=CARTESIAN_POINT('Ctrl Pts',(-0.508721244209177,6.99276978444095,
7.74969086813121));
#159657=CARTESIAN_POINT('Ctrl Pts',(-0.324717028084998,7.00615601860165,
7.74134731164808));
#159658=CARTESIAN_POINT('Ctrl Pts',(-0.140281357570403,7.01226817658823,
7.73300375516494));
#159659=CARTESIAN_POINT('Ctrl Pts',(0.0439900195438079,7.01111199744239,
7.7246601986818));
#159660=CARTESIAN_POINT('Ctrl Pts',(0.228401589516582,7.0099549386805,7.71631029445735));
#159661=CARTESIAN_POINT('Ctrl Pts',(0.41264828949352,7.0015185148547,7.7079603902329));
#159662=CARTESIAN_POINT('Ctrl Pts',(0.596137764416577,6.98586045726197,
7.69961048600845));
#159663=CARTESIAN_POINT('Ctrl Pts',(0.779902459975568,6.97017891374139,
7.69124805754548));
#159664=CARTESIAN_POINT('Ctrl Pts',(0.962907334084302,6.94725411876133,
7.6828856290825));
#159665=CARTESIAN_POINT('Ctrl Pts',(1.14456701236412,6.9171954516775,7.67452320061952));
#159666=CARTESIAN_POINT('Ctrl Pts',(1.32638203443264,6.88711108033573,7.66615362114024));
#159667=CARTESIAN_POINT('Ctrl Pts',(1.50684924534435,6.84988073099078,7.65778404166098));
#159668=CARTESIAN_POINT('Ctrl Pts',(1.68539621165002,6.80566427119762,7.6494144621817));
#159669=CARTESIAN_POINT('Ctrl Pts',(1.86421856489746,6.76137961290245,7.64103197364581));
#159670=CARTESIAN_POINT('Ctrl Pts',(2.04111444101417,6.71008740311691,7.63264948510993));
#159671=CARTESIAN_POINT('Ctrl Pts',(2.21552788564968,6.65199689945874,7.62426699657404));
#159672=CARTESIAN_POINT('Ctrl Pts',(2.27259882275809,6.63298873476249,7.62152410896555));
#159673=CARTESIAN_POINT('Ctrl Pts',(2.32940413615168,6.61325305163047,7.61878122135707));
#159674=CARTESIAN_POINT('Ctrl Pts',(2.38592487487982,6.59279827189713,7.61603833374858));
#159675=CARTESIAN_POINT('Ctrl Pts',(2.5588208641615,6.53022744467304,7.60764788668033));
#159676=CARTESIAN_POINT('Ctrl Pts',(2.7294014515115,6.46079789610722,7.59925743961206));
#159677=CARTESIAN_POINT('Ctrl Pts',(2.89710496355616,6.38470119838339,7.5908669925438));
#159678=CARTESIAN_POINT('Ctrl Pts',(3.06465158322805,6.30867569172359,7.58248439502582));
#159679=CARTESIAN_POINT('Ctrl Pts',(3.22932619550739,6.22599560575943,7.57410179750785));
#159680=CARTESIAN_POINT('Ctrl Pts',(3.39058555648328,6.13690118436552,7.56571919998986));
#159681=CARTESIAN_POINT('Ctrl Pts',(3.55171776280078,6.04787701483576,7.55734321223591));
#159682=CARTESIAN_POINT('Ctrl Pts',(3.70943980023771,5.95244875244961,7.54896722448196));
#159683=CARTESIAN_POINT('Ctrl Pts',(3.86323114988645,5.85090348963705,7.54059123672801));
#159684=CARTESIAN_POINT('Ctrl Pts',(4.01690928358334,5.74943298098728,7.53222141509086));
#159685=CARTESIAN_POINT('Ctrl Pts',(4.16666222802708,5.64185463528875,7.52385159345374));
#159686=CARTESIAN_POINT('Ctrl Pts',(4.3119964399461,5.52850009174208,7.5154817718166));
#159687=CARTESIAN_POINT('Ctrl Pts',(4.45726703110845,5.41519516969702,7.5071156141095));
#159688=CARTESIAN_POINT('Ctrl Pts',(4.59812248720092,5.29611929235213,7.4987494564024));
#159689=CARTESIAN_POINT('Ctrl Pts',(4.73409990577678,5.17164622191274,7.49038329869531));
#159690=CARTESIAN_POINT('Ctrl Pts',(4.8700359395881,5.04721103488638,7.4820196872306));
#159691=CARTESIAN_POINT('Ctrl Pts',(5.00109665387081,4.91738215166125,7.47365607576589));
#159692=CARTESIAN_POINT('Ctrl Pts',(5.12685346072713,4.782572545684,7.46529246430118));
#159693=CARTESIAN_POINT('Ctrl Pts',(5.25258876091069,4.64778599457074,7.45693028316425));
#159694=CARTESIAN_POINT('Ctrl Pts',(5.37302173875201,4.50802065980671,7.44856810202733));
#159695=CARTESIAN_POINT('Ctrl Pts',(5.48776151230319,4.36372548937073,7.44020592089041));
#159696=CARTESIAN_POINT('Ctrl Pts',(5.60258692083858,4.21932262554947,7.43183749871581));
#159697=CARTESIAN_POINT('Ctrl Pts',(5.71171041313554,4.0703834153163,7.4234690765412));
#159698=CARTESIAN_POINT('Ctrl Pts',(5.81478108593368,3.91739039223408,7.4151006543666));
#159699=CARTESIAN_POINT('Ctrl Pts',(5.91780065474847,3.76447322538423,7.40673638138106));
#159700=CARTESIAN_POINT('Ctrl Pts',(6.01477323009914,3.60750654362712,7.39837210839551));
#159701=CARTESIAN_POINT('Ctrl Pts',(6.105392107819,3.44700069223688,7.39000783540997));
#159702=CARTESIAN_POINT('Ctrl Pts',(6.19607841426631,3.2863754098232,7.38163733864084));
#159703=CARTESIAN_POINT('Ctrl Pts',(6.28040140896109,3.1222059794816,7.37326684187171));
#159704=CARTESIAN_POINT('Ctrl Pts',(6.35809994547922,2.95502819712388,7.36489634510259));
#159705=CARTESIAN_POINT('Ctrl Pts',(6.43579848199734,2.78785041476615,7.35652584833346));
#159706=CARTESIAN_POINT('Ctrl Pts',(6.50687244152518,2.61766458747699,7.34815535156433));
#159707=CARTESIAN_POINT('Ctrl Pts',(6.57110895151815,2.44502632087633,7.33978485479521));
#159708=CARTESIAN_POINT('Origin',(0.,0.,50.));
#159709=CARTESIAN_POINT('',(6.57110895151814,2.44502632087637,5.33975062352345));
#159710=CARTESIAN_POINT('',(6.57110895151814,2.44502632087637,5.88692100032223));
#159711=CARTESIAN_POINT('',(6.57110895151814,2.44502632087636,50.));
#159712=CARTESIAN_POINT('',(7.01125,3.55178126493216E-12,7.77353435691053));
#159713=CARTESIAN_POINT('Ctrl Pts',(6.57110895151814,2.44502632087637,5.88692100032223));
#159714=CARTESIAN_POINT('Ctrl Pts',(6.5044983873315,2.62404495591324,5.895592809261));
#159715=CARTESIAN_POINT('Ctrl Pts',(6.43056821795877,2.80033990715955,5.90426461819976));
#159716=CARTESIAN_POINT('Ctrl Pts',(6.34956511459265,2.97332295892123,5.91293642713853));
#159717=CARTESIAN_POINT('Ctrl Pts',(6.26856213015506,3.14630575670966,5.92160822334536));
#159718=CARTESIAN_POINT('Ctrl Pts',(6.18048635294248,3.3159764075473,5.9302800195522));
#159719=CARTESIAN_POINT('Ctrl Pts',(6.08563165071504,3.48176879966423,5.93895181575904));
#159720=CARTESIAN_POINT('Ctrl Pts',(5.99077708581898,3.64756095174566,5.94762359941078));
#159721=CARTESIAN_POINT('Ctrl Pts',(5.88914375658023,3.80947460983867,5.95629538306252));
#159722=CARTESIAN_POINT('Ctrl Pts',(5.78107076500129,3.96696954520039,5.96496716671427));
#159723=CARTESIAN_POINT('Ctrl Pts',(5.6729979276878,4.12446425575084,5.97363893798774));
#159724=CARTESIAN_POINT('Ctrl Pts',(5.55848560711296,4.27754002202603,5.98231070926122));
#159725=CARTESIAN_POINT('Ctrl Pts',(5.43791587524826,4.4256861045744,5.99098248053469));
#159726=CARTESIAN_POINT('Ctrl Pts',(5.31734631302827,4.57383197867744,5.99965423960676));
#159727=CARTESIAN_POINT('Ctrl Pts',(5.19071953583751,4.7170479626693,6.00832599867883));
#159728=CARTESIAN_POINT('Ctrl Pts',(5.05845803451497,4.85485621574429,6.0169977577509));
#159729=CARTESIAN_POINT('Ctrl Pts',(4.92619671659114,4.99266427772924,6.02566950479839));
#159730=CARTESIAN_POINT('Ctrl Pts',(4.78830088681692,5.12506441890981,6.03434125184587));
#159731=CARTESIAN_POINT('Ctrl Pts',(4.64523063400368,5.25161488681471,6.04301299889335));
#159732=CARTESIAN_POINT('Ctrl Pts',(4.49652806262298,5.38314733060966,6.05202613096636));
#159733=CARTESIAN_POINT('Ctrl Pts',(4.34223563523867,5.50835996364338,6.06103926303936));
#159734=CARTESIAN_POINT('Ctrl Pts',(4.18290943344465,5.62680151010321,6.07005239511237));
#159735=CARTESIAN_POINT('Ctrl Pts',(4.02607270355366,5.7433924073996,6.07892469699674));
#159736=CARTESIAN_POINT('Ctrl Pts',(3.86435862820312,5.85342208902684,6.0877969988811));
#159737=CARTESIAN_POINT('Ctrl Pts',(3.69833198496378,5.9565062823348,6.09666930076547));
#159738=CARTESIAN_POINT('Ctrl Pts',(3.53489950802504,6.05797978512232,6.10540297293289));
#159739=CARTESIAN_POINT('Ctrl Pts',(3.36728850947003,6.15272311279952,6.11413664510032));
#159740=CARTESIAN_POINT('Ctrl Pts',(3.19606623000888,6.24041562845752,6.12287031726774));
#159741=CARTESIAN_POINT('Ctrl Pts',(3.02603797481024,6.32749661743998,6.13154308488173));
#159742=CARTESIAN_POINT('Ctrl Pts',(2.85244891335276,6.40762471321634,6.14021585249571));
#159743=CARTESIAN_POINT('Ctrl Pts',(2.6758783609508,6.48053250588987,6.1488886201097));
#159744=CARTESIAN_POINT('Ctrl Pts',(2.49930871513386,6.55343992422515,6.15756134319417));
#159745=CARTESIAN_POINT('Ctrl Pts',(2.3197578716491,6.61912700519444,6.16623406627865));
#159746=CARTESIAN_POINT('Ctrl Pts',(2.13782503580022,6.67737453486068,6.17490678936312));
#159747=CARTESIAN_POINT('Ctrl Pts',(1.95589311921758,6.73562177021507,6.18357946862625));
#159748=CARTESIAN_POINT('Ctrl Pts',(1.77157950496959,6.78642944284913,6.19225214788937));
#159749=CARTESIAN_POINT('Ctrl Pts',(1.58549928668711,6.82962799678099,6.2009248271525));
#159750=CARTESIAN_POINT('Ctrl Pts',(1.39941999343791,6.87282633596621,6.20959746330241));
#159751=CARTESIAN_POINT('Ctrl Pts',(1.21157439050561,6.90841556788932,6.21827009945232));
#159752=CARTESIAN_POINT('Ctrl Pts',(1.02258935229021,6.93627692491316,6.22694273560223));
#159753=CARTESIAN_POINT('Ctrl Pts',(0.833605238123156,6.96413814570801,
6.23561532934701));
#159754=CARTESIAN_POINT('Ctrl Pts',(0.643481980914484,6.98427152577633,
6.24428792309178));
#159755=CARTESIAN_POINT('Ctrl Pts',(0.452854049805853,6.9966098770815,6.25296051683656));
#159756=CARTESIAN_POINT('Ctrl Pts',(0.262227035219643,7.00894816906496,
6.26163306888427));
#159757=CARTESIAN_POINT('Ctrl Pts',(0.0710956351198641,7.01349148893089,
6.27030562093198));
#159758=CARTESIAN_POINT('Ctrl Pts',(-0.119902323158553,7.01022467510145,
6.27897817297969));
#159759=CARTESIAN_POINT('Ctrl Pts',(-0.310899378724106,7.00695787671193,
6.28765068403835));
#159760=CARTESIAN_POINT('Ctrl Pts',(-0.501762709654535,6.99588102335271,
6.29632319509701));
#159761=CARTESIAN_POINT('Ctrl Pts',(-0.69185538920701,6.97703107940084,
6.30499570615567));
#159762=CARTESIAN_POINT('Ctrl Pts',(-0.881947185839014,6.958181223001,6.31366817693325));
#159763=CARTESIAN_POINT('Ctrl Pts',(-1.07126805553177,6.93155837629103,
6.32234064771084));
#159764=CARTESIAN_POINT('Ctrl Pts',(-1.25918622472626,6.89725138109085,
6.33101311848842));
#159765=CARTESIAN_POINT('Ctrl Pts',(-1.44710353643658,6.86294454243597,
6.33968554969289));
#159766=CARTESIAN_POINT('Ctrl Pts',(-1.6336178809721,6.82095367648008,6.34835798089736));
#159767=CARTESIAN_POINT('Ctrl Pts',(-1.81810685596831,6.7714189076427,6.35703041210184));
#159768=CARTESIAN_POINT('Ctrl Pts',(-2.00259500418343,6.7218843607937,6.3657028044411));
#159769=CARTESIAN_POINT('Ctrl Pts',(-2.18505752664271,6.66480605238633,
6.37437519678037));
#159770=CARTESIAN_POINT('Ctrl Pts',(-2.36488554745062,6.60037445225339,
6.38304758911964));
#159771=CARTESIAN_POINT('Ctrl Pts',(-2.54471277704031,6.5359431356105,6.39171994330159));
#159772=CARTESIAN_POINT('Ctrl Pts',(-2.7219052607312,6.4641586878085,6.40039229748355));
#159773=CARTESIAN_POINT('Ctrl Pts',(-2.89587171390055,6.38526065083726,
6.4090646516655));
#159774=CARTESIAN_POINT('Ctrl Pts',(-3.06983741583796,6.30636295456807,
6.41773696839799));
#159775=CARTESIAN_POINT('Ctrl Pts',(-3.24057685640968,6.22035184793667,
6.42640928513048));
#159776=CARTESIAN_POINT('Ctrl Pts',(-3.40752028946975,6.12751434427958,
6.43508160186297));
#159777=CARTESIAN_POINT('Ctrl Pts',(-3.57446301524744,6.03467723394333,
6.44375388185381));
#159778=CARTESIAN_POINT('Ctrl Pts',(-3.73760951742361,5.93501392252033,
6.45242616184466));
#159779=CARTESIAN_POINT('Ctrl Pts',(-3.89641539159055,5.82885697703043,
6.4610984418355));
#159780=CARTESIAN_POINT('Ctrl Pts',(-4.05522060590922,5.72270047262923,
6.46977068579249));
#159781=CARTESIAN_POINT('Ctrl Pts',(-4.20968499214316,5.61005054602417,
6.47844292974947));
#159782=CARTESIAN_POINT('Ctrl Pts',(-4.3592931215613,5.49128309621789,6.48711517370645));
#159783=CARTESIAN_POINT('Ctrl Pts',(-4.50890064155567,5.37251613020689,
6.49578738233733));
#159784=CARTESIAN_POINT('Ctrl Pts',(-4.65365172183509,5.24763186748229,
6.50445959096822));
#159785=CARTESIAN_POINT('Ctrl Pts',(-4.7930633497115,5.1170470281357,6.5131317995991));
#159786=CARTESIAN_POINT('Ctrl Pts',(-4.93247442107403,4.98646271006755,
6.52180397361161));
#159787=CARTESIAN_POINT('Ctrl Pts',(-5.06654587536807,4.85017805510629,
6.53047614762413));
#159788=CARTESIAN_POINT('Ctrl Pts',(-5.19483033978703,4.70864782111894,
6.53914832163663));
#159789=CARTESIAN_POINT('Ctrl Pts',(-5.32311430257712,4.56711814055521,
6.54782046173846));
#159790=CARTESIAN_POINT('Ctrl Pts',(-5.44561113000693,4.42034313247674,
6.55649260184028));
#159791=CARTESIAN_POINT('Ctrl Pts',(-5.56191207495262,4.26881255538308,
6.56516474194211));
#159792=CARTESIAN_POINT('Ctrl Pts',(-5.67821257461712,4.11728255845425,
6.57383684884094));
#159793=CARTESIAN_POINT('Ctrl Pts',(-5.78831706632323,3.96099725427861,
6.58250895573975));
#159794=CARTESIAN_POINT('Ctrl Pts',(-5.89185815647412,3.80047813129998,
6.59118106263858));
#159795=CARTESIAN_POINT('Ctrl Pts',(-5.99539885864469,3.63995960980488,
6.59985313704202));
#159796=CARTESIAN_POINT('Ctrl Pts',(-6.09237605450686,3.47520753994929,
6.60852521144547));
#159797=CARTESIAN_POINT('Ctrl Pts',(-6.18246615568102,3.30677165772885,
6.61719728584892));
#159798=CARTESIAN_POINT('Ctrl Pts',(-6.27255592662724,3.13833639291513,
6.62586932846462));
#159799=CARTESIAN_POINT('Ctrl Pts',(-6.35575851943897,2.96621759322222,
6.63454137108032));
#159800=CARTESIAN_POINT('Ctrl Pts',(-6.43179631013701,2.79098957135421,
6.64321341369602));
#159801=CARTESIAN_POINT('Ctrl Pts',(-6.50783382831931,2.6157621774949,6.65188542523155));
#159802=CARTESIAN_POINT('Ctrl Pts',(-6.57670648270626,2.43742584432008,
6.66055743676707));
#159803=CARTESIAN_POINT('Ctrl Pts',(-6.63818446599492,2.25657562645787,
6.66922944830259));
#159804=CARTESIAN_POINT('Ctrl Pts',(-6.6996622339648,2.07572604200044,6.6779014294655));
#159805=CARTESIAN_POINT('Ctrl Pts',(-6.75374529124758,1.89236285939144,
6.68657341062841));
#159806=CARTESIAN_POINT('Ctrl Pts',(-6.80025318023397,1.70709790206002,
6.69524539179132));
#159807=CARTESIAN_POINT('Ctrl Pts',(-6.84676091012636,1.52183357848227,
6.70391734328915));
#159808=CARTESIAN_POINT('Ctrl Pts',(-6.88569345442288,1.3346677686782,6.71258929478698));
#159809=CARTESIAN_POINT('Ctrl Pts',(-6.91692090874678,1.14622497994137,
6.72126124628481));
#159810=CARTESIAN_POINT('Ctrl Pts',(-6.9481482587953,0.957782820456753,
6.72993316882507));
#159811=CARTESIAN_POINT('Ctrl Pts',(-6.97167052392502,0.768063970771554,
6.73860509136533));
#159812=CARTESIAN_POINT('Ctrl Pts',(-6.9874092190315,0.57770145256321,6.7472770139056));
#159813=CARTESIAN_POINT('Ctrl Pts',(-7.00314786286682,0.387339554489333,
6.75594890819577));
#159814=CARTESIAN_POINT('Ctrl Pts',(-7.01110296401743,0.196334275138324,
6.76462080248594));
#159815=CARTESIAN_POINT('Ctrl Pts',(-7.01124797942392,0.00532292437979963,
6.77329269677612));
#159816=CARTESIAN_POINT('Ctrl Pts',(-7.01139299436984,-0.185687819711539,
6.78196456352367));
#159817=CARTESIAN_POINT('Ctrl Pts',(-7.0037279729944,-0.376704351160677,
6.79063643027122));
#159818=CARTESIAN_POINT('Ctrl Pts',(-6.98827849031204,-0.567089326598627,
6.79930829701877));
#159819=CARTESIAN_POINT('Ctrl Pts',(-6.97282905543828,-0.757473712888125,
6.80798013693113));
#159820=CARTESIAN_POINT('Ctrl Pts',(-6.94959523043374,-0.947226264001047,
6.81665197684349));
#159821=CARTESIAN_POINT('Ctrl Pts',(-6.91865453650896,-1.13571385786388,
6.82532381675585));
#159822=CARTESIAN_POINT('Ctrl Pts',(-6.88771393580682,-1.3242008838237,
6.83399563054043));
#159823=CARTESIAN_POINT('Ctrl Pts',(-6.84906655865494,-1.51142267990842,
6.842667444325));
#159824=CARTESIAN_POINT('Ctrl Pts',(-6.80284135383486,-1.69675457183835,
6.85133925810957));
#159825=CARTESIAN_POINT('Ctrl Pts',(-6.75661628451852,-1.88208592048964,
6.86001104647374));
#159826=CARTESIAN_POINT('Ctrl Pts',(-6.70281350071451,-2.06552710051589,
6.86868283483791));
#159827=CARTESIAN_POINT('Ctrl Pts',(-6.64161251687612,-2.2464660554245,
6.87735462320208));
#159828=CARTESIAN_POINT('Ctrl Pts',(-6.58041170744941,-2.42740449468997,
6.88602638685323));
#159829=CARTESIAN_POINT('Ctrl Pts',(-6.51181283117298,-2.60584045408564,
6.89469815050438));
#159830=CARTESIAN_POINT('Ctrl Pts',(-6.43604476876237,-2.78117858056374,
6.90336991415553));
#159831=CARTESIAN_POINT('Ctrl Pts',(-6.35684774728261,-2.96445180845298,
6.91243412710089));
#159832=CARTESIAN_POINT('Ctrl Pts',(-6.26981768815679,-3.14433998862217,
6.92149834004625));
#159833=CARTESIAN_POINT('Ctrl Pts',(-6.17527181578122,-3.3201874290043,
6.93056255299162));
#159834=CARTESIAN_POINT('Ctrl Pts',(-6.08368050191737,-3.4905396368745,
6.93934350928244));
#159835=CARTESIAN_POINT('Ctrl Pts',(-5.98503618716623,-3.65709956718604,
6.94812446557326));
#159836=CARTESIAN_POINT('Ctrl Pts',(-5.87967633130112,-3.819297422516,6.95690542186409));
#159837=CARTESIAN_POINT('Ctrl Pts',(-5.77561495477707,-3.97949631379482,
6.96557815960957));
#159838=CARTESIAN_POINT('Ctrl Pts',(-5.66500279405234,-4.13543980257606,
6.97425089735506));
#159839=CARTESIAN_POINT('Ctrl Pts',(-5.54820899034585,-4.2866074653443,
6.98292363510055));
#159840=CARTESIAN_POINT('Ctrl Pts',(-5.4314163636836,-4.43777360464965,
6.99159628544246));
#159841=CARTESIAN_POINT('Ctrl Pts',(-5.30844239242685,-4.58416378940594,
7.00026893578438));
#159842=CARTESIAN_POINT('Ctrl Pts',(-5.17969746407092,-4.72528948776657,
7.00894158612629));
#159843=CARTESIAN_POINT('Ctrl Pts',(-5.05095379116799,-4.86641380994343,
7.01761415189707));
#159844=CARTESIAN_POINT('Ctrl Pts',(-4.91643946526928,-5.00227353854876,
7.02628671766785));
#159845=CARTESIAN_POINT('Ctrl Pts',(-4.77660337747906,-5.13241529270145,
7.03495928343862));
#159846=CARTESIAN_POINT('Ctrl Pts',(-4.63676860764499,-5.26255582026714,
7.0436317674704));
#159847=CARTESIAN_POINT('Ctrl Pts',(-4.49161238426941,-5.38697828766251,
7.05230425150218));
#159848=CARTESIAN_POINT('Ctrl Pts',(-4.34161910267562,-5.50526748939433,
7.06097673553396));
#159849=CARTESIAN_POINT('Ctrl Pts',(-4.19162718580484,-5.62355561486465,
7.06964914065862));
#159850=CARTESIAN_POINT('Ctrl Pts',(-4.03679852186307,-5.73571041041457,
7.07832154578328));
#159851=CARTESIAN_POINT('Ctrl Pts',(-3.87764977431538,-5.84135761533669,
7.08699395090793));
#159852=CARTESIAN_POINT('Ctrl Pts',(-3.7185024228424,-5.94700389350699,
7.09566627995706));
#159853=CARTESIAN_POINT('Ctrl Pts',(-3.55503530028438,-6.04614253816465,
7.10433860900618));
#159854=CARTESIAN_POINT('Ctrl Pts',(-3.38779388709407,-6.13844272931401,
7.1130109380553));
#159855=CARTESIAN_POINT('Ctrl Pts',(-3.22055388638018,-6.23074214092055,
7.12168319386025));
#159856=CARTESIAN_POINT('Ctrl Pts',(-3.04953990753581,-6.31620307732962,
7.1303554496652));
#159857=CARTESIAN_POINT('Ctrl Pts',(-2.87532260481251,-6.39454036508913,
7.13902770547014));
#159858=CARTESIAN_POINT('Ctrl Pts',(-2.70110671662093,-6.47287701680057,
7.14769989086198));
#159859=CARTESIAN_POINT('Ctrl Pts',(-2.52368781567603,-6.54409001910946,
7.15637207625383));
#159860=CARTESIAN_POINT('Ctrl Pts',(-2.34365791912392,-6.60794174615877,
7.16504426164567));
#159861=CARTESIAN_POINT('Ctrl Pts',(-2.16362942554292,-6.67179297561222,
7.17371637945526));
#159862=CARTESIAN_POINT('Ctrl Pts',(-1.98099024478671,-6.72828294965095,
7.18238849726485));
#159863=CARTESIAN_POINT('Ctrl Pts',(-1.79634980371134,-6.77722317363138,
7.19106061507444));
#159864=CARTESIAN_POINT('Ctrl Pts',(-1.61171074128092,-6.82616303219246,
7.19973266813239));
#159865=CARTESIAN_POINT('Ctrl Pts',(-1.42507072299576,-6.8675531807254,
7.20840472119034));
#159866=CARTESIAN_POINT('Ctrl Pts',(-1.2370525163378,-6.90125551145024,
7.21707677424829));
#159867=CARTESIAN_POINT('Ctrl Pts',(-1.04903565219027,-6.93495760152961,
7.225748765385));
#159868=CARTESIAN_POINT('Ctrl Pts',(-0.859640898939492,-6.96097193353415,
7.2344207565217));
#159869=CARTESIAN_POINT('Ctrl Pts',(-0.669500206860438,-6.97921170588154,
7.24309274765841));
#159870=CARTESIAN_POINT('Ctrl Pts',(-0.479360810402781,-6.99745135394286,
7.25176467970404));
#159871=CARTESIAN_POINT('Ctrl Pts',(-0.288475768013728,-7.00791652123622,
7.26043661174968));
#159872=CARTESIAN_POINT('Ctrl Pts',(-0.0974819939195787,-7.01057228929005,
7.26910854379531));
#159873=CARTESIAN_POINT('Ctrl Pts',(0.0935105410598241,-7.01322804011398,
7.27778041957985));
#159874=CARTESIAN_POINT('Ctrl Pts',(0.284611522346058,-7.00807448913595,
7.28645229536439));
#159875=CARTESIAN_POINT('Ctrl Pts',(0.475183323468245,-6.99512883166548,
7.29512417114893));
#159876=CARTESIAN_POINT('Ctrl Pts',(0.665753950392636,-6.98218325395897,
7.30379599350217));
#159877=CARTESIAN_POINT('Ctrl Pts',(0.855795120325422,-6.96144568508264,
7.31246781585542));
#159878=CARTESIAN_POINT('Ctrl Pts',(1.04467275076238,-6.93298531704161,
7.32113963820866));
#159879=CARTESIAN_POINT('Ctrl Pts',(1.23354927906265,-6.90452511507221,
7.32981140996019));
#159880=CARTESIAN_POINT('Ctrl Pts',(1.42126200062692,-6.86834224643129,
7.3384831817117));
#159881=CARTESIAN_POINT('Ctrl Pts',(1.60718460924519,-6.82455743578332,
7.34715495346322));
#159882=CARTESIAN_POINT('Ctrl Pts',(1.79763389405661,-6.77970659200761,
7.35603785770171));
#159883=CARTESIAN_POINT('Ctrl Pts',(1.98620448431676,-6.72687898190926,
7.3649207619402));
#159884=CARTESIAN_POINT('Ctrl Pts',(2.17223623427651,-6.66625954377687,
7.37380366617869));
#159885=CARTESIAN_POINT('Ctrl Pts',(2.35386532185837,-6.60707473666683,
7.38247634593503));
#159886=CARTESIAN_POINT('Ctrl Pts',(2.53307410227486,-6.54046283696597,
7.39114902569138));
#159887=CARTESIAN_POINT('Ctrl Pts',(2.70926451774061,-6.46664614273982,
7.39982170544772));
#159888=CARTESIAN_POINT('Ctrl Pts',(2.88545151535976,-6.39283088045386,
7.40849421696626));
#159889=CARTESIAN_POINT('Ctrl Pts',(3.05862000314199,-6.31181121311119,
7.4171667284848));
#159890=CARTESIAN_POINT('Ctrl Pts',(3.22819210344032,-6.22385751008051,
7.42583924000333));
#159891=CARTESIAN_POINT('Ctrl Pts',(3.39776113570901,-6.13590539837628,
7.43451159461208));
#159892=CARTESIAN_POINT('Ctrl Pts',(3.56373365851006,-6.04101963284017,
7.44318394922084));
#159893=CARTESIAN_POINT('Ctrl Pts',(3.7255558277518,-5.93951684371756,7.45185630382959));
#159894=CARTESIAN_POINT('Ctrl Pts',(3.88737528046406,-5.83801575853528,
7.46052851285441));
#159895=CARTESIAN_POINT('Ctrl Pts',(4.04504427838839,-5.72989802299715,
7.46920072187921));
#159896=CARTESIAN_POINT('Ctrl Pts',(4.19803670363139,-5.61552440983598,
7.47787293090403));
#159897=CARTESIAN_POINT('Ctrl Pts',(4.35102676029996,-5.5011525673665,7.48654500566879));
#159898=CARTESIAN_POINT('Ctrl Pts',(4.49934016166387,-5.38052521115996,
7.49521708043356));
#159899=CARTESIAN_POINT('Ctrl Pts',(4.64248202336615,-5.25404484423402,
7.50388915519832));
#159900=CARTESIAN_POINT('Ctrl Pts',(4.78562185584448,-5.12756627033347,
7.51256110702502));
#159901=CARTESIAN_POINT('Ctrl Pts',(4.92359008252393,-4.99523503982244,
7.52123305885172));
#159902=CARTESIAN_POINT('Ctrl Pts',(5.05592635132172,-4.85749269608413,
7.52990501067843));
#159903=CARTESIAN_POINT('Ctrl Pts',(5.18826091680305,-4.71975212524454,
7.53857685088737));
#159904=CARTESIAN_POINT('Ctrl Pts',(5.31496347269478,-4.57660078535332,
7.54724869109631));
#159905=CARTESIAN_POINT('Ctrl Pts',(5.43561126741903,-4.42851631045966,
7.55592053130525));
#159906=CARTESIAN_POINT('Ctrl Pts',(5.56176013705625,-4.27367975367592,
7.56498777403881));
#159907=CARTESIAN_POINT('Ctrl Pts',(5.68128895686563,-4.11344992041037,
7.57405501677237));
#159908=CARTESIAN_POINT('Ctrl Pts',(5.79376175354059,-3.9484112381704,7.58312225950592));
#159909=CARTESIAN_POINT('Ctrl Pts',(5.90133874236365,-3.79055649462729,
7.59179481588435));
#159910=CARTESIAN_POINT('Ctrl Pts',(6.00246078174245,-3.62830291661641,
7.60046737226278));
#159911=CARTESIAN_POINT('Ctrl Pts',(6.09679041553322,-3.46219196341887,
7.60913992864121));
#159912=CARTESIAN_POINT('Ctrl Pts',(6.1911166917875,-3.29608692271739,7.61781217633166));
#159913=CARTESIAN_POINT('Ctrl Pts',(6.27865090596307,-3.12612502860771,
7.6264844240221));
#159914=CARTESIAN_POINT('Ctrl Pts',(6.35910096686113,-2.95287342359368,
7.63515667171254));
#159915=CARTESIAN_POINT('Ctrl Pts',(6.43954858437068,-2.77962708048965,
7.64382865601387));
#159916=CARTESIAN_POINT('Ctrl Pts',(6.51291235952014,-2.60309148403811,
7.65250064031521));
#159917=CARTESIAN_POINT('Ctrl Pts',(6.57894750102532,-2.42385567665501,
7.66117262461654));
#159918=CARTESIAN_POINT('Ctrl Pts',(6.64498098171195,-2.24462437714676,
7.6698443908129));
#159919=CARTESIAN_POINT('Ctrl Pts',(6.70368609940955,-2.06269326909702,
7.67851615700926));
#159920=CARTESIAN_POINT('Ctrl Pts',(6.75486698389468,-1.8786693675018,7.68718792320563));
#159921=CARTESIAN_POINT('Ctrl Pts',(6.80605126222577,-1.69463326313241,
7.69586026443384));
#159922=CARTESIAN_POINT('Ctrl Pts',(6.84971023276689,-1.50850436117643,
7.70453260566205));
#159923=CARTESIAN_POINT('Ctrl Pts',(6.88569820761782,-1.32090376489309,
7.71320494689027));
#159924=CARTESIAN_POINT('Ctrl Pts',(6.92168406448288,-1.13331420939253,
7.72187677772865));
#159925=CARTESIAN_POINT('Ctrl Pts',(6.94999977553846,-0.944253411824701,
7.73054860856705));
#159926=CARTESIAN_POINT('Ctrl Pts',(6.97055086371898,-0.754352184862346,
7.73922043940544));
#159927=CARTESIAN_POINT('Ctrl Pts',(6.99110229108047,-0.564447823716458,
7.74789241336617));
#159928=CARTESIAN_POINT('Ctrl Pts',(7.00388880856509,-0.373703287790729,
7.7565643873269));
#159929=CARTESIAN_POINT('Ctrl Pts',(7.00886775178469,-0.182755028638574,
7.76523636128763));
#159930=CARTESIAN_POINT('Ctrl Pts',(7.01045582731897,-0.12185048618891,
7.7680023598286));
#159931=CARTESIAN_POINT('Ctrl Pts',(7.01125000000003,-0.0609252433271523,
7.77076835836956));
#159932=CARTESIAN_POINT('Ctrl Pts',(7.01125,3.55178232870534E-12,7.77353435691052));
#159933=CARTESIAN_POINT('Ctrl Pts',(7.01124860966183,0.00441542920857962,
7.77353435691052));
#159934=CARTESIAN_POINT('Ctrl Pts',(7.01111374519947,0.218566359853513,
7.7832434407798));
#159935=CARTESIAN_POINT('Ctrl Pts',(7.00116331493674,0.432422285858829,
7.79295252464907));
#159936=CARTESIAN_POINT('Ctrl Pts',(6.98150240916137,0.645174916882285,
7.80266160851835));
#159937=CARTESIAN_POINT('Ctrl Pts',(6.96175963902393,0.858813410368804,
7.81241111921059));
#159938=CARTESIAN_POINT('Ctrl Pts',(6.93222542281991,1.07133937000862,7.82216062990284));
#159939=CARTESIAN_POINT('Ctrl Pts',(6.89305680462996,1.28194947273466,7.83191014059508));
#159940=CARTESIAN_POINT('Ctrl Pts',(6.85375143361006,1.493294896973,7.84169369060858));
#159941=CARTESIAN_POINT('Ctrl Pts',(6.80474430104216,1.70271103413845,7.85147724062208));
#159942=CARTESIAN_POINT('Ctrl Pts',(6.74624425403649,1.90940174593501,7.86126079063558));
#159943=CARTESIAN_POINT('Ctrl Pts',(6.6950718161633,2.09020275635724,7.86981887102818));
#159944=CARTESIAN_POINT('Ctrl Pts',(6.63663641341989,2.26891856784468,7.87837695142078));
#159945=CARTESIAN_POINT('Ctrl Pts',(6.57110895151814,2.44502632087637,7.88693503181337));
#159946=CARTESIAN_POINT('',(7.01124941011649,0.0028760461125263,7.22646564306228));
#159947=CARTESIAN_POINT('Ctrl Pts',(6.57110895151815,2.44502632087633,7.33978485479521));
#159948=CARTESIAN_POINT('Ctrl Pts',(6.63540283922006,2.27223384931942,7.33140688128228));
#159949=CARTESIAN_POINT('Ctrl Pts',(6.69284696259494,2.09698487088329,7.32302890776936));
#159950=CARTESIAN_POINT('Ctrl Pts',(6.74327785184177,1.91985165451923,7.31465093425643));
#159951=CARTESIAN_POINT('Ctrl Pts',(6.77527636844613,1.80746021646097,7.30933509056286));
#159952=CARTESIAN_POINT('Ctrl Pts',(6.80445241352737,1.69431048651665,7.3040192468693));
#159953=CARTESIAN_POINT('Ctrl Pts',(6.83077487139492,1.58055092256459,7.29870340317573));
#159954=CARTESIAN_POINT('Ctrl Pts',(6.87364674711721,1.39526860916829,7.29004538988013));
#159955=CARTESIAN_POINT('Ctrl Pts',(6.90902110269817,1.20804545734485,7.28138737658453));
#159956=CARTESIAN_POINT('Ctrl Pts',(6.93673266435705,1.0194932592921,7.27272936328893));
#159957=CARTESIAN_POINT('Ctrl Pts',(6.9643773710318,0.83139594914365,7.26409223771336));
#159958=CARTESIAN_POINT('Ctrl Pts',(6.9843961214186,0.641976267544519,7.2554551121378));
#159959=CARTESIAN_POINT('Ctrl Pts',(6.99667434903633,0.451856853480315,
7.24681798656223));
#159960=CARTESIAN_POINT('Ctrl Pts',(7.00631840262508,0.302525706136942,
7.24003387207136));
#159961=CARTESIAN_POINT('Ctrl Pts',(7.01118792571456,0.152763206930641,
7.2332497575805));
#159962=CARTESIAN_POINT('Ctrl Pts',(7.01124941011624,0.00287604671680145,
7.22646564308963));
#159963=CARTESIAN_POINT('Ctrl Pts',(7.01124941011649,0.00287604611253946,
7.22646564306228));
#159964=CARTESIAN_POINT('Ctrl Pts',(7.01131757022025,-0.163285228295573,
7.21894493810047));
#159965=CARTESIAN_POINT('Ctrl Pts',(7.0054745942836,-0.329575821312576,
7.21142423313868));
#159966=CARTESIAN_POINT('Ctrl Pts',(6.99371928995505,-0.495496776791375,
7.20390352817687));
#159967=CARTESIAN_POINT('Ctrl Pts',(6.98196648505361,-0.661382453954761,
7.1963844222765));
#159968=CARTESIAN_POINT('Ctrl Pts',(6.96430388228091,-0.826898246025481,
7.18886531637613));
#159969=CARTESIAN_POINT('Ctrl Pts',(6.94078235372499,-0.991547719839916,
7.18134621047576));
#159970=CARTESIAN_POINT('Ctrl Pts',(6.91725260803397,-1.15625471317179,
7.17382447781119));
#159971=CARTESIAN_POINT('Ctrl Pts',(6.88785990483266,-1.32009438218466,
7.16630274514664));
#159972=CARTESIAN_POINT('Ctrl Pts',(6.85270668800832,-1.48257802851186,
7.15878101248207));
#159973=CARTESIAN_POINT('Ctrl Pts',(6.82350465433979,-1.61755437887948,
7.15253265428448));
#159974=CARTESIAN_POINT('Ctrl Pts',(6.79032839184365,-1.75159501383976,
7.14628429608688));
#159975=CARTESIAN_POINT('Ctrl Pts',(6.75326300162647,-1.8844270729755,7.14003593788929));
#159976=CARTESIAN_POINT('Ctrl Pts',(6.6959875362354,-2.08968642573767,7.13038063353122));
#159977=CARTESIAN_POINT('Ctrl Pts',(6.62943112543927,-2.29204274376962,
7.12072532917314));
#159978=CARTESIAN_POINT('Ctrl Pts',(6.55391163375439,-2.49075668411005,
7.11107002481508));
#159979=CARTESIAN_POINT('Ctrl Pts',(6.47797377825457,-2.69057146239716,
7.1013612318824));
#159980=CARTESIAN_POINT('Ctrl Pts',(6.39297332712872,-2.88670337037012,
7.09165243894973));
#159981=CARTESIAN_POINT('Ctrl Pts',(6.29927765817105,-3.07842939626152,
7.08194364601705));
#159982=CARTESIAN_POINT('Ctrl Pts',(6.20513111770013,-3.27107802406593,
7.07218813354855));
#159983=CARTESIAN_POINT('Ctrl Pts',(6.10220551435119,-3.45927823647201,
7.06243262108007));
#159984=CARTESIAN_POINT('Ctrl Pts',(5.99091723264469,-3.64232580559467,
7.05267710861158));
#159985=CARTESIAN_POINT('Ctrl Pts',(5.87951875841874,-3.82555461997077,
7.04291193668496));
#159986=CARTESIAN_POINT('Ctrl Pts',(5.75974107273603,-4.00362055912466,
7.03314676475832));
#159987=CARTESIAN_POINT('Ctrl Pts',(5.63204484367387,-4.17584691306405,
7.0233815928317));
#159988=CARTESIAN_POINT('Ctrl Pts',(5.50452272552154,-4.34783844027911,
7.01362973549534));
#159989=CARTESIAN_POINT('Ctrl Pts',(5.36910366545502,-4.51400626528277,
7.003877878159));
#159990=CARTESIAN_POINT('Ctrl Pts',(5.2262888972894,-4.67370633700595,6.99412602082265));
#159991=CARTESIAN_POINT('Ctrl Pts',(5.16401131506322,-4.743347134495,6.98987350474939));
#159992=CARTESIAN_POINT('Ctrl Pts',(5.10032791452013,-4.81175841621377,
6.98562098867613));
#159993=CARTESIAN_POINT('Ctrl Pts',(5.03528278304038,-4.87888858832799,
6.98136847260287));
#159994=CARTESIAN_POINT('Ctrl Pts',(4.912411875898,-5.00569815818591,6.97333542699789));
#159995=CARTESIAN_POINT('Ctrl Pts',(4.78461915748462,-5.12799552920953,
6.9653023813929));
#159996=CARTESIAN_POINT('Ctrl Pts',(4.65227703156344,-5.24537367439988,
6.95726933578793));
#159997=CARTESIAN_POINT('Ctrl Pts',(4.52001998025667,-5.36267636439883,
6.94924145413398));
#159998=CARTESIAN_POINT('Ctrl Pts',(4.38321961589875,-5.4750658809148,6.94121357248004));
#159999=CARTESIAN_POINT('Ctrl Pts',(4.24228557003584,-5.58217159399151,
6.93318569082609));
#160000=CARTESIAN_POINT('Ctrl Pts',(4.10141515728416,-5.68922894778277,
6.92516143383985));
#160001=CARTESIAN_POINT('Ctrl Pts',(3.95641507048716,-5.79100702697689,
6.91713717685362));
#160002=CARTESIAN_POINT('Ctrl Pts',(3.80772838996846,-5.88717513504806,
6.90911291986739));
#160003=CARTESIAN_POINT('Ctrl Pts',(3.65905968718424,-5.98333161541522,
6.90108963309558));
#160004=CARTESIAN_POINT('Ctrl Pts',(3.50670558196251,-6.0738792702854,6.89306634632377));
#160005=CARTESIAN_POINT('Ctrl Pts',(3.3511386818256,-6.15853035209475,6.88504305955196));
#160006=CARTESIAN_POINT('Ctrl Pts',(3.19558452900869,-6.24317449750292,
6.87702043021694));
#160007=CARTESIAN_POINT('Ctrl Pts',(3.03681842963845,-6.32192286056721,
6.86899780088192));
#160008=CARTESIAN_POINT('Ctrl Pts',(2.87533789368541,-6.39453349038355,
6.8609751715469));
#160009=CARTESIAN_POINT('Ctrl Pts',(2.71379665254778,-6.46717141662704,
6.85294952627444));
#160010=CARTESIAN_POINT('Ctrl Pts',(2.54953927212061,-6.5336668526107,6.84492388100198));
#160011=CARTESIAN_POINT('Ctrl Pts',(2.38308390614504,-6.5938257225053,6.83689823572952));
#160012=CARTESIAN_POINT('Ctrl Pts',(2.28493167991229,-6.62929905779368,
6.83216582625849));
#160013=CARTESIAN_POINT('Ctrl Pts',(2.18601556915375,-6.6625700913399,6.82743341678746));
#160014=CARTESIAN_POINT('Ctrl Pts',(2.08644434056026,-6.69360714235935,
6.82270100731643));
#160015=CARTESIAN_POINT('Ctrl Pts',(1.90276165401132,-6.75086232535084,
6.81397095850849));
#160016=CARTESIAN_POINT('Ctrl Pts',(1.71675704446272,-6.80054131086613,
6.80524090970055));
#160017=CARTESIAN_POINT('Ctrl Pts',(1.52905784929066,-6.84248556125788,
6.7965108608926));
#160018=CARTESIAN_POINT('Ctrl Pts',(1.3413043806691,-6.88444193988042,6.78777828778048));
#160019=CARTESIAN_POINT('Ctrl Pts',(1.15185561572288,-6.91865905944544,
6.77904571466835));
#160020=CARTESIAN_POINT('Ctrl Pts',(0.961349495982859,-6.94502942463698,
6.77031314155622));
#160021=CARTESIAN_POINT('Ctrl Pts',(0.768136931815597,-6.97177442308448,
6.76145650826237));
#160022=CARTESIAN_POINT('Ctrl Pts',(0.573837028153697,-6.99044797678349,
6.75259987496852));
#160023=CARTESIAN_POINT('Ctrl Pts',(0.379121580805413,-7.00099231462709,
6.74374324167466));
#160024=CARTESIAN_POINT('Ctrl Pts',(0.187011414285745,-7.01139556987243,
6.73500510959497));
#160025=CARTESIAN_POINT('Ctrl Pts',(-0.00550296647739609,-7.01388580322923,
6.72626697751529));
#160026=CARTESIAN_POINT('Ctrl Pts',(-0.197774497716119,-7.00846001704748,
6.7175288454356));
#160027=CARTESIAN_POINT('Ctrl Pts',(-0.393957232692518,-7.00292385906468,
6.70861296153466));
#160028=CARTESIAN_POINT('Ctrl Pts',(-0.589886835983756,-6.98914617974144,
6.69969707763373));
#160029=CARTESIAN_POINT('Ctrl Pts',(-0.78487840171196,-6.96717966303626,
6.6907811937328));
#160030=CARTESIAN_POINT('Ctrl Pts',(-0.979869967440173,-6.94521314633108,
6.68186530983186));
#160031=CARTESIAN_POINT('Ctrl Pts',(-1.17392319577496,-6.91505783214244,
6.67294942593093));
#160032=CARTESIAN_POINT('Ctrl Pts',(-1.36636015085385,-6.87682241305231,
6.66403354203));
#160033=CARTESIAN_POINT('Ctrl Pts',(-1.55501567164087,-6.83933832950921,
6.65529285747741));
#160034=CARTESIAN_POINT('Ctrl Pts',(-1.74213788700388,-6.79408476441464,
6.6465521729248));
#160035=CARTESIAN_POINT('Ctrl Pts',(-1.9270972911631,-6.74121076609327,
6.6378114883722));
#160036=CARTESIAN_POINT('Ctrl Pts',(-2.11202341805838,-6.688346280681,6.6290723764137));
#160037=CARTESIAN_POINT('Ctrl Pts',(-2.29478724770831,-6.62786417534572,
6.6203332644552));
#160038=CARTESIAN_POINT('Ctrl Pts',(-2.47477335420135,-6.55996367427709,
6.6115941524967));
#160039=CARTESIAN_POINT('Ctrl Pts',(-2.65709143798604,-6.49118342515641,
6.60274181285061));
#160040=CARTESIAN_POINT('Ctrl Pts',(-2.8365590434985,-6.41479128798384,
6.5938894732045));
#160041=CARTESIAN_POINT('Ctrl Pts',(-3.01255500787018,-6.33104563931238,
6.58503713355841));
#160042=CARTESIAN_POINT('Ctrl Pts',(-3.18621080598725,-6.2484135317479,
6.57630250085286));
#160043=CARTESIAN_POINT('Ctrl Pts',(-3.35648646466823,-6.15862238645124,
6.56756786814732));
#160044=CARTESIAN_POINT('Ctrl Pts',(-3.52280689854241,-6.06196817197864,
6.55883323544177));
#160045=CARTESIAN_POINT('Ctrl Pts',(-3.69248930596735,-5.9633602053118,
6.5499220423254));
#160046=CARTESIAN_POINT('Ctrl Pts',(-3.85805462311256,-5.85760888370049,
6.54101084920905));
#160047=CARTESIAN_POINT('Ctrl Pts',(-4.01891922818866,-5.74507744071352,
6.53209965609268));
#160048=CARTESIAN_POINT('Ctrl Pts',(-4.17978383326477,-5.63254599772656,
6.52318846297632));
#160049=CARTESIAN_POINT('Ctrl Pts',(-4.33594747016127,-5.51323459608025,
6.51427726985994));
#160050=CARTESIAN_POINT('Ctrl Pts',(-4.48685773942913,-5.38755363672836,
6.50536607674358));
#160051=CARTESIAN_POINT('Ctrl Pts',(-4.62277166467131,-5.2743619195802,
6.49734041195011));
#160052=CARTESIAN_POINT('Ctrl Pts',(-4.75448655588241,-5.15595124616252,
6.48931474715665));
#160053=CARTESIAN_POINT('Ctrl Pts',(-4.88157791519271,-5.03267559260507,
6.48128908236318));
#160054=CARTESIAN_POINT('Ctrl Pts',(-5.00862893882244,-4.90943906371678,
6.47326596471888));
#160055=CARTESIAN_POINT('Ctrl Pts',(-5.13105908918682,-4.78134088361919,
6.46524284707458));
#160056=CARTESIAN_POINT('Ctrl Pts',(-5.24847882072518,-4.64877366957128,
6.45721972943029));
#160057=CARTESIAN_POINT('Ctrl Pts',(-5.36588374460855,-4.51622317340838,
6.4491976235713));
#160058=CARTESIAN_POINT('Ctrl Pts',(-5.47827926571286,-4.37920504061177,
6.44117551771231));
#160059=CARTESIAN_POINT('Ctrl Pts',(-5.58531445971767,-4.23814687671024,
6.43315341185331));
#160060=CARTESIAN_POINT('Ctrl Pts',(-5.69238942836389,-4.09703629511619,
6.42512832495255));
#160061=CARTESIAN_POINT('Ctrl Pts',(-5.79409986651127,-3.95188297379347,
6.41710323805178));
#160062=CARTESIAN_POINT('Ctrl Pts',(-5.89013647044135,-3.80314592437323,
6.40907815115102));
#160063=CARTESIAN_POINT('Ctrl Pts',(-5.98619198830061,-3.65437958193445,
6.4010514837495));
#160064=CARTESIAN_POINT('Ctrl Pts',(-6.07657125439554,-3.50202841806052,
6.39302481634798));
#160065=CARTESIAN_POINT('Ctrl Pts',(-6.16100981452104,-3.34657804748005,
6.38499814894646));
#160066=CARTESIAN_POINT('Ctrl Pts',(-6.24551616162911,-3.19100288188241,
6.37696503776425));
#160067=CARTESIAN_POINT('Ctrl Pts',(-6.32407211075625,-3.03232386684494,
6.36893192658205));
#160068=CARTESIAN_POINT('Ctrl Pts',(-6.39646017371002,-2.87104925221453,
6.36089881539984));
#160069=CARTESIAN_POINT('Ctrl Pts',(-6.43911385352952,-2.77602038288491,
6.35616541408561));
#160070=CARTESIAN_POINT('Ctrl Pts',(-6.47962695838208,-2.68009070373161,
6.35143201277137));
#160071=CARTESIAN_POINT('Ctrl Pts',(-6.51796300787284,-2.58336694848045,
6.34669861145713));
#160072=CARTESIAN_POINT('Ctrl Pts',(-6.59693645836743,-2.38411301390853,
6.33694765799879));
#160073=CARTESIAN_POINT('Ctrl Pts',(-6.66671560835717,-2.18137117766495,
6.32719670454047));
#160074=CARTESIAN_POINT('Ctrl Pts',(-6.72706144207423,-1.97592280139134,
6.31744575108213));
#160075=CARTESIAN_POINT('Ctrl Pts',(-6.78749421530973,-1.77017843810756,
6.30768074954217));
#160076=CARTESIAN_POINT('Ctrl Pts',(-6.83846647645426,-1.56171977215431,
6.2979157480022));
#160077=CARTESIAN_POINT('Ctrl Pts',(-6.87978909168529,-1.35134326372988,
6.28815074646224));
#160078=CARTESIAN_POINT('Ctrl Pts',(-6.92104283065413,-1.14131740948047,
6.27840202116236));
#160079=CARTESIAN_POINT('Ctrl Pts',(-6.95267906171902,-0.92938013875767,
6.26865329586247));
#160080=CARTESIAN_POINT('Ctrl Pts',(-6.974560252916,-0.716335006086056,
6.25890457056258));
#160081=CARTESIAN_POINT('Ctrl Pts',(-6.99638138870826,-0.503874599883472,
6.24918260174219));
#160082=CARTESIAN_POINT('Ctrl Pts',(-7.00850093008893,-0.290312441622313,
6.2394606329218));
#160083=CARTESIAN_POINT('Ctrl Pts',(-7.0108331209835,-0.0764559495448779,
6.2297386641014));
#160084=CARTESIAN_POINT('Ctrl Pts',(-7.01314988037575,0.135985509585613,
6.22008102302742));
#160085=CARTESIAN_POINT('Ctrl Pts',(-7.00580835251575,0.348717373991946,
6.21042338195344));
#160086=CARTESIAN_POINT('Ctrl Pts',(-6.98877490237801,0.560938433690608,
6.20076574087945));
#160087=CARTESIAN_POINT('Ctrl Pts',(-6.98128811610057,0.654216877264134,
6.19652087597655));
#160088=CARTESIAN_POINT('Ctrl Pts',(-6.97192960369691,0.747396515675602,
6.19227601107363));
#160089=CARTESIAN_POINT('Ctrl Pts',(-6.96069965522493,0.840408753078836,
6.18803114617072));
#160090=CARTESIAN_POINT('Ctrl Pts',(-6.93992730107203,1.01245612628937,
6.18017929918189));
#160091=CARTESIAN_POINT('Ctrl Pts',(-6.91275659676435,1.18385961718861,
6.17232745219306));
#160092=CARTESIAN_POINT('Ctrl Pts',(-6.87924919440166,1.35408902359633,
6.16447560520423));
#160093=CARTESIAN_POINT('Ctrl Pts',(-6.84575129446697,1.52427015432279,
6.15662598493563));
#160094=CARTESIAN_POINT('Ctrl Pts',(-6.80592034468947,1.69327748896089,
6.14877636466701));
#160095=CARTESIAN_POINT('Ctrl Pts',(-6.75986945775669,1.86058901334718,
6.14092674439841));
#160096=CARTESIAN_POINT('Ctrl Pts',(-6.71382224739759,2.02788718005055,
6.13307775082147));
#160097=CARTESIAN_POINT('Ctrl Pts',(-6.66155619039472,2.19348943843572,
6.12522875724454));
#160098=CARTESIAN_POINT('Ctrl Pts',(-6.6032347459023,2.35688723807666,6.11737976366761));
#160099=CARTESIAN_POINT('Ctrl Pts',(-6.54488377496868,2.5203677612435,6.10952679637484));
#160100=CARTESIAN_POINT('Ctrl Pts',(-6.48047141959149,2.68164123600291,
6.10167382908207));
#160101=CARTESIAN_POINT('Ctrl Pts',(-6.41021006923064,2.84021714501446,
6.0938208617893));
#160102=CARTESIAN_POINT('Ctrl Pts',(-6.33993087484643,2.99883332698135,
6.08596590010658));
#160103=CARTESIAN_POINT('Ctrl Pts',(-6.26379989351225,3.15475023551417,
6.07811093842385));
#160104=CARTESIAN_POINT('Ctrl Pts',(-6.18207600021978,3.30750100378014,
6.07025597674112));
#160105=CARTESIAN_POINT('Ctrl Pts',(-6.10027098912941,3.46040338995675,
6.06239321835208));
#160106=CARTESIAN_POINT('Ctrl Pts',(-6.01286217068981,3.61013302988238,
6.05453045996305));
#160107=CARTESIAN_POINT('Ctrl Pts',(-5.9201526622887,3.75625065959342,6.04666770157402));
#160108=CARTESIAN_POINT('Ctrl Pts',(-5.85214229526773,3.86344045917565,
6.04089969467744));
#160109=CARTESIAN_POINT('Ctrl Pts',(-5.7812802946199,3.9686870491885,6.03513168778086));
#160110=CARTESIAN_POINT('Ctrl Pts',(-5.70770009220788,4.07182836326757,
6.02936368088429));
#160111=CARTESIAN_POINT('Ctrl Pts',(-5.60082438494124,4.22164177134821,
6.02098561455147));
#160112=CARTESIAN_POINT('Ctrl Pts',(-5.4879758233974,4.36734428812648,6.01260754821865));
#160113=CARTESIAN_POINT('Ctrl Pts',(-5.36949712189324,4.5084506452306,6.00422948188583));
#160114=CARTESIAN_POINT('Ctrl Pts',(-5.25109943473175,4.64946051546728,
5.99585714437624));
#160115=CARTESIAN_POINT('Ctrl Pts',(-5.12707949372502,4.78588024089517,
5.98748480686666));
#160116=CARTESIAN_POINT('Ctrl Pts',(-4.99782144854695,4.91725607742205,
5.97911246935706));
#160117=CARTESIAN_POINT('Ctrl Pts',(-4.86863283271904,5.0485613470535,5.97074462894436));
#160118=CARTESIAN_POINT('Ctrl Pts',(-4.73421195276814,5.17482789599584,
5.96237678853165));
#160119=CARTESIAN_POINT('Ctrl Pts',(-4.59498142208136,5.29563709984239,
5.95400894811894));
#160120=CARTESIAN_POINT('Ctrl Pts',(-4.45580528107472,5.41639911020401,
5.94564437655942));
#160121=CARTESIAN_POINT('Ctrl Pts',(-4.31182348396954,5.53170781163764,
5.93727980499988));
#160122=CARTESIAN_POINT('Ctrl Pts',(-4.16349382203681,5.64118301035885,
5.92891523344036));
#160123=CARTESIAN_POINT('Ctrl Pts',(-4.0152003924244,5.75063146769593,5.92055270508536));
#160124=CARTESIAN_POINT('Ctrl Pts',(-3.86256148044464,5.85424906933691,
5.91219017673037));
#160125=CARTESIAN_POINT('Ctrl Pts',(-3.7060664825293,5.95169705122605,5.90382764837537));
#160126=CARTESIAN_POINT('Ctrl Pts',(-3.54955899581676,6.04915280977324,
5.89546445266408));
#160127=CARTESIAN_POINT('Ctrl Pts',(-3.38919508417895,6.14043778605301,
5.88710125695277));
#160128=CARTESIAN_POINT('Ctrl Pts',(-3.22549219738419,6.2252571550992,5.87873806124149));
#160129=CARTESIAN_POINT('Ctrl Pts',(-3.06177814637302,6.31008230866031,
5.87037429517662));
#160130=CARTESIAN_POINT('Ctrl Pts',(-2.89472495800337,6.38844082427623,
5.86201052911176));
#160131=CARTESIAN_POINT('Ctrl Pts',(-2.72487385034697,6.46008429218964,
5.8536467630469));
#160132=CARTESIAN_POINT('Ctrl Pts',(-2.5549885140255,6.53174219780852,5.84528131150261));
#160133=CARTESIAN_POINT('Ctrl Pts',(-2.38230443704883,6.59668222958885,
5.83691585995833));
#160134=CARTESIAN_POINT('Ctrl Pts',(-2.20738233519328,6.65470433518851,
5.82855040841404));
#160135=CARTESIAN_POINT('Ctrl Pts',(-2.0324016522518,6.7127458722832,5.82018215529562));
#160136=CARTESIAN_POINT('Ctrl Pts',(-1.85518176182634,6.76386475996052,
5.8118139021772));
#160137=CARTESIAN_POINT('Ctrl Pts',(-1.67629844704744,6.80791084540084,
5.80344564905878));
#160138=CARTESIAN_POINT('Ctrl Pts',(-1.49724928186962,6.85199776785745,
5.79506963737372));
#160139=CARTESIAN_POINT('Ctrl Pts',(-1.31653393007678,6.88899870554986,
5.78669362568866));
#160140=CARTESIAN_POINT('Ctrl Pts',(-1.13473949834754,6.91881440952061,
5.7783176140036));
#160141=CARTESIAN_POINT('Ctrl Pts',(-0.95285591235669,6.94864473548526,
5.76993749461772));
#160142=CARTESIAN_POINT('Ctrl Pts',(-0.769892516413647,6.97128275400953,
5.76155737523184));
#160143=CARTESIAN_POINT('Ctrl Pts',(-0.586442106525143,6.98668105885723,
5.75317725584596));
#160144=CARTESIAN_POINT('Ctrl Pts',(-0.402782081242819,7.00209695822399,
5.74478756110929));
#160145=CARTESIAN_POINT('Ctrl Pts',(-0.218634258290256,7.01025659315712,
5.73639786637262));
#160146=CARTESIAN_POINT('Ctrl Pts',(-0.034593355991068,7.01116465804514,
5.72800817163596));
#160147=CARTESIAN_POINT('Ctrl Pts',(0.0822510668830052,7.01174117292009,
5.72268169786111));
#160148=CARTESIAN_POINT('Ctrl Pts',(0.199052410907578,7.00939580229304,
5.71735522408627));
#160149=CARTESIAN_POINT('Ctrl Pts',(0.31565942591468,7.00414061033409,5.71202875031143));
#160150=CARTESIAN_POINT('Ctrl Pts',(0.499142634924632,6.99587147245648,
5.70364744923058));
#160151=CARTESIAN_POINT('Ctrl Pts',(0.68251458485407,6.98037849663042,5.69526614814971));
#160152=CARTESIAN_POINT('Ctrl Pts',(0.865182576578385,6.95766380846942,
5.68688484706885));
#160153=CARTESIAN_POINT('Ctrl Pts',(1.04761906322664,6.93497790786754,5.67851416806646));
#160154=CARTESIAN_POINT('Ctrl Pts',(1.2293530471497,6.90508857495438,5.67014348906408));
#160155=CARTESIAN_POINT('Ctrl Pts',(1.40979338410086,6.86804988163638,5.6617728100617));
#160156=CARTESIAN_POINT('Ctrl Pts',(1.59002895208051,6.83105322091078,5.65341163035066));
#160157=CARTESIAN_POINT('Ctrl Pts',(1.76897348010267,6.78692343596839,5.64505045063961));
#160158=CARTESIAN_POINT('Ctrl Pts',(1.9460420495598,6.73576624474492,5.63668927092857));
#160159=CARTESIAN_POINT('Ctrl Pts',(2.12288085134853,6.68467543610186,5.62833894084925));
#160160=CARTESIAN_POINT('Ctrl Pts',(2.29784823671262,6.62657550030596,5.61998861076992));
#160161=CARTESIAN_POINT('Ctrl Pts',(2.47037064399661,6.56162292758276,5.6116382806906));
#160162=CARTESIAN_POINT('Ctrl Pts',(2.64276030541287,6.49672033205246,5.60329437570022));
#160163=CARTESIAN_POINT('Ctrl Pts',(2.81270843243529,6.42497572208527,5.59495047070984));
#160164=CARTESIAN_POINT('Ctrl Pts',(2.9796566649325,6.3465953645733,5.58660656571946));
#160165=CARTESIAN_POINT('Ctrl Pts',(3.14647080324813,6.26827796280358,5.5782693626216));
#160166=CARTESIAN_POINT('Ctrl Pts',(3.31028955679106,6.18333558203062,5.56993215952376));
#160167=CARTESIAN_POINT('Ctrl Pts',(3.470574455851,6.09202261230985,5.5615949564259));
#160168=CARTESIAN_POINT('Ctrl Pts',(3.52333928093263,6.0619629316833,5.55885039929227));
#160169=CARTESIAN_POINT('Ctrl Pts',(3.57572131606705,6.03121326287636,5.55610584215863));
#160170=CARTESIAN_POINT('Ctrl Pts',(3.62770187811974,5.999783799937,5.553361285025));
#160171=CARTESIAN_POINT('Ctrl Pts',(3.78562535409301,5.90429714416894,5.54502297575256));
#160172=CARTESIAN_POINT('Ctrl Pts',(3.93971164680453,5.80261084754989,5.53668466648012));
#160173=CARTESIAN_POINT('Ctrl Pts',(4.08947460581958,5.69507014977488,5.52834635720769));
#160174=CARTESIAN_POINT('Ctrl Pts',(4.23933179035228,5.58746179122458,5.52000280176816));
#160175=CARTESIAN_POINT('Ctrl Pts',(4.38485994949304,5.47399187566745,5.51165924632863));
#160176=CARTESIAN_POINT('Ctrl Pts',(4.52560533670533,5.3550464889564,5.5033156908891));
#160177=CARTESIAN_POINT('Ctrl Pts',(4.66645780219709,5.23601060928062,5.49496578772067));
#160178=CARTESIAN_POINT('Ctrl Pts',(4.80251998776095,5.11149116047744,5.48661588455225));
#160179=CARTESIAN_POINT('Ctrl Pts',(4.93337406187388,4.9819119751487,5.47826598138382));
#160180=CARTESIAN_POINT('Ctrl Pts',(5.0644244072465,4.85213843079747,5.46990355398927));
#160181=CARTESIAN_POINT('Ctrl Pts',(5.19025079776716,4.71729021501192,5.46154112659473));
#160182=CARTESIAN_POINT('Ctrl Pts',(5.31047385128612,4.5778263441623,5.45317869920018));
#160183=CARTESIAN_POINT('Ctrl Pts',(5.43079971181987,4.43824321278974,5.44480912079614));
#160184=CARTESIAN_POINT('Ctrl Pts',(5.54551247135562,4.29403680685261,5.43643954239211));
#160185=CARTESIAN_POINT('Ctrl Pts',(5.65427503038995,4.14569661736224,5.42806996398807));
#160186=CARTESIAN_POINT('Ctrl Pts',(5.76320534240702,3.997127631221,5.41968747653009));
#160187=CARTESIAN_POINT('Ctrl Pts',(5.86616693181532,3.84441239180857,5.41130498907212));
#160188=CARTESIAN_POINT('Ctrl Pts',(5.96286699486789,3.68806775480266,5.40292250161414));
#160189=CARTESIAN_POINT('Ctrl Pts',(5.99450891739559,3.63690910261986,5.40017960765562));
#160190=CARTESIAN_POINT('Ctrl Pts',(6.02548078590298,3.58536202772556,5.3974367136971));
#160191=CARTESIAN_POINT('Ctrl Pts',(6.05577344516303,3.5334451380145,5.39469381973858));
#160192=CARTESIAN_POINT('Ctrl Pts',(6.15138017468945,3.36959012648025,5.38603696599194));
#160193=CARTESIAN_POINT('Ctrl Pts',(6.24039807521569,3.20174082998824,5.3773801122453));
#160194=CARTESIAN_POINT('Ctrl Pts',(6.32250483875401,3.03043876797273,5.36872325849865));
#160195=CARTESIAN_POINT('Ctrl Pts',(6.40450656935418,2.85935583965718,5.36007747880662));
#160196=CARTESIAN_POINT('Ctrl Pts',(6.47961467772508,2.68482922005942,5.3514316991146));
#160197=CARTESIAN_POINT('Ctrl Pts',(6.5475526276583,2.50742520337994,5.34278591942257));
#160198=CARTESIAN_POINT('Ctrl Pts',(6.55550301070338,2.48666464337298,5.34177415412287));
#160199=CARTESIAN_POINT('Ctrl Pts',(6.56335525258107,2.4658647061558,5.34076238882317));
#160200=CARTESIAN_POINT('Ctrl Pts',(6.57110895151813,2.44502632087638,5.33975062352347));
#160201=CARTESIAN_POINT('Origin',(0.,0.,50.));
#160202=CARTESIAN_POINT('',(6.57110895151814,2.44502632087637,3.33981554959538));
#160203=CARTESIAN_POINT('',(6.57110895151814,2.44502632087637,3.88698101089639));
#160204=CARTESIAN_POINT('',(6.57110895151814,2.44502632087636,50.));
#160205=CARTESIAN_POINT('',(7.01124963752017,-0.002254522849646,5.77353435691053));
#160206=CARTESIAN_POINT('Ctrl Pts',(6.57110895151813,2.44502632087638,3.88698101089636));
#160207=CARTESIAN_POINT('Ctrl Pts',(6.50404475006846,2.62526412474361,3.8957147867161));
#160208=CARTESIAN_POINT('Ctrl Pts',(6.4295520875458,2.8027648898791,3.90444856253583));
#160209=CARTESIAN_POINT('Ctrl Pts',(6.34787495986428,2.9769296357872,3.91318233835557));
#160210=CARTESIAN_POINT('Ctrl Pts',(6.26622791776542,3.15103022851057,3.92191289710902));
#160211=CARTESIAN_POINT('Ctrl Pts',(6.17740181137757,3.32179700819347,3.93064345586247));
#160212=CARTESIAN_POINT('Ctrl Pts',(6.0816880179526,3.48865266468185,3.93937401461591));
#160213=CARTESIAN_POINT('Ctrl Pts',(6.01293388485033,3.608510164887,3.94564544088701));
#160214=CARTESIAN_POINT('Ctrl Pts',(5.9406267137465,3.72634995895831,3.9519168671581));
#160215=CARTESIAN_POINT('Ctrl Pts',(5.86488917672598,3.84196583889321,3.9581882934292));
#160216=CARTESIAN_POINT('Ctrl Pts',(5.76796621207628,3.98992198170838,3.9662139733059));
#160217=CARTESIAN_POINT('Ctrl Pts',(5.66537871576642,4.1343028176686,3.97423965318258));
#160218=CARTESIAN_POINT('Ctrl Pts',(5.55742985037872,4.27464618660066,3.98226533305928));
#160219=CARTESIAN_POINT('Ctrl Pts',(5.44951524390886,4.41494501581543,3.99028846588645));
#160220=CARTESIAN_POINT('Ctrl Pts',(5.33624287910824,4.55120863881733,3.99831159871363));
#160221=CARTESIAN_POINT('Ctrl Pts',(5.21795829982202,4.68300520433392,4.0063347315408));
#160222=CARTESIAN_POINT('Ctrl Pts',(5.09968863589183,4.81478515067062,4.01435685267326));
#160223=CARTESIAN_POINT('Ctrl Pts',(4.97640826161214,4.94209888918038,4.0223789738057));
#160224=CARTESIAN_POINT('Ctrl Pts',(4.84850189231907,5.06454893970612,4.03040109493816));
#160225=CARTESIAN_POINT('Ctrl Pts',(4.72054799115267,5.18704449445752,4.0384261972079));
#160226=CARTESIAN_POINT('Ctrl Pts',(4.58796492374278,5.30467249467776,4.04645129947765));
#160227=CARTESIAN_POINT('Ctrl Pts',(4.45117336088422,5.41707322027815,4.05447640174739));
#160228=CARTESIAN_POINT('Ctrl Pts',(4.31435485656344,5.52949608350048,4.06250308458238));
#160229=CARTESIAN_POINT('Ctrl Pts',(4.17332649434682,5.63668939520866,4.07052976741736));
#160230=CARTESIAN_POINT('Ctrl Pts',(4.02854049783307,5.73833495186704,4.07855645025234));
#160231=CARTESIAN_POINT('Ctrl Pts',(3.88363826722259,5.84006210950721,4.08658957690268));
#160232=CARTESIAN_POINT('Ctrl Pts',(3.73497268265571,5.93623241389945,4.09462270355302));
#160233=CARTESIAN_POINT('Ctrl Pts',(3.58302382035294,6.02657173401956,4.10265583020336));
#160234=CARTESIAN_POINT('Ctrl Pts',(3.49349193253668,6.07980181255923,4.10738913970745));
#160235=CARTESIAN_POINT('Ctrl Pts',(3.4028206236895,6.13100832511276,4.11212244921153));
#160236=CARTESIAN_POINT('Ctrl Pts',(3.31111175468872,6.18014283900156,4.11685575871562));
#160237=CARTESIAN_POINT('Ctrl Pts',(3.12218526897848,6.28136326770418,4.12660669709408));
#160238=CARTESIAN_POINT('Ctrl Pts',(2.92874330649919,6.37384810930519,4.13635763547254));
#160239=CARTESIAN_POINT('Ctrl Pts',(2.73153480289983,6.45727064502078,4.14610857385101));
#160240=CARTESIAN_POINT('Ctrl Pts',(2.53404219874635,6.54081336008051,4.15587355952939));
#160241=CARTESIAN_POINT('Ctrl Pts',(2.33277223522788,6.6152676398631,4.16563854520778));
#160242=CARTESIAN_POINT('Ctrl Pts',(2.12849454649652,6.68035459598026,4.17540353088616));
#160243=CARTESIAN_POINT('Ctrl Pts',(1.92455734720968,6.74533306535238,4.18515224031543));
#160244=CARTESIAN_POINT('Ctrl Pts',(1.71762247832009,6.80097540444875,4.1949009497447));
#160245=CARTESIAN_POINT('Ctrl Pts',(1.50847251728717,6.84705317834536,4.20464965917397));
#160246=CARTESIAN_POINT('Ctrl Pts',(1.29989658111883,6.89300448897231,4.21437161267375));
#160247=CARTESIAN_POINT('Ctrl Pts',(1.08911772845036,6.92944363070854,4.22409356617353));
#160248=CARTESIAN_POINT('Ctrl Pts',(0.876928290547881,6.95619316406156,
4.23381551967331));
#160249=CARTESIAN_POINT('Ctrl Pts',(0.666142826683952,6.98276570627524,
4.24347314683125));
#160250=CARTESIAN_POINT('Ctrl Pts',(0.453965425161636,6.99977640646201,
4.25313077398921));
#160251=CARTESIAN_POINT('Ctrl Pts',(0.241188204621614,7.00710031414218,
4.26278840114715));
#160252=CARTESIAN_POINT('Ctrl Pts',(0.147663498990188,7.01031948538674,
4.26703334209878));
#160253=CARTESIAN_POINT('Ctrl Pts',(0.0540231068225535,7.0116678307699,
4.27127828305041));
#160254=CARTESIAN_POINT('Ctrl Pts',(-0.0396647883018845,7.01113780117528,
4.27552322400204));
#160255=CARTESIAN_POINT('Ctrl Pts',(-0.212958871141432,7.01015740779197,
4.28337507239659));
#160256=CARTESIAN_POINT('Ctrl Pts',(-0.386344281526877,7.00274699430319,
4.29122692079114));
#160257=CARTESIAN_POINT('Ctrl Pts',(-0.559287245113946,6.98890723503702,
4.29907876918568));
#160258=CARTESIAN_POINT('Ctrl Pts',(-0.732181163610055,6.97507140060387,
4.30692839086565));
#160259=CARTESIAN_POINT('Ctrl Pts',(-0.904632505023892,6.95480987765904,
4.31477801254561));
#160260=CARTESIAN_POINT('Ctrl Pts',(-1.07610975018993,6.92817539963057,
4.32262763422557));
#160261=CARTESIAN_POINT('Ctrl Pts',(-1.24757330521086,6.90154304800591,
4.33047662921912));
#160262=CARTESIAN_POINT('Ctrl Pts',(-1.41806254197057,6.86853881345669,
4.33832562421267));
#160263=CARTESIAN_POINT('Ctrl Pts',(-1.58705356494276,6.82926698442099,
4.34617461920622));
#160264=CARTESIAN_POINT('Ctrl Pts',(-1.75613014321767,6.78997527318585,
4.35402758792056));
#160265=CARTESIAN_POINT('Ctrl Pts',(-1.92370662013163,6.74440971390524,
4.36188055663491));
#160266=CARTESIAN_POINT('Ctrl Pts',(-2.0892714250179,6.69272526517439,4.36973352534925));
#160267=CARTESIAN_POINT('Ctrl Pts',(-2.25487827788404,6.64102769030444,
4.3775884884577));
#160268=CARTESIAN_POINT('Ctrl Pts',(-2.41847208118997,6.58320825719328,
4.38544345156615));
#160269=CARTESIAN_POINT('Ctrl Pts',(-2.57955944907681,6.5194708076023,4.3932984146746));
#160270=CARTESIAN_POINT('Ctrl Pts',(-2.74080670963018,6.4556700932693,4.40116117448998));
#160271=CARTESIAN_POINT('Ctrl Pts',(-2.89954221680159,6.38593978368614,
4.40902393430535));
#160272=CARTESIAN_POINT('Ctrl Pts',(-3.05529495229387,6.3105308268788,4.41688669412072));
#160273=CARTESIAN_POINT('Ctrl Pts',(-3.16955273817767,6.25521198825049,
4.42265469250997));
#160274=CARTESIAN_POINT('Ctrl Pts',(-3.28220583408499,6.1968381901427,4.42842269089923));
#160275=CARTESIAN_POINT('Ctrl Pts',(-3.39307799138927,6.1355234745578,4.43419068928848));
#160276=CARTESIAN_POINT('Ctrl Pts',(-3.55412074152026,6.04646332941971,
4.44256875593696));
#160277=CARTESIAN_POINT('Ctrl Pts',(-3.71176189921157,5.95099977948684,
4.45094682258544));
#160278=CARTESIAN_POINT('Ctrl Pts',(-3.86548021925234,5.84941785454492,
4.45932488923393));
#160279=CARTESIAN_POINT('Ctrl Pts',(-4.01909342862745,5.74790539005344,
4.46769722706517));
#160280=CARTESIAN_POINT('Ctrl Pts',(-4.16878887486146,5.64028307220609,
4.4760695648964));
#160281=CARTESIAN_POINT('Ctrl Pts',(-4.31407189673789,5.52688069640338,
4.48444190272764));
#160282=CARTESIAN_POINT('Ctrl Pts',(-4.45927688174176,5.41353923320171,
4.49280974346726));
#160283=CARTESIAN_POINT('Ctrl Pts',(-4.60007390954522,5.29442410430156,
4.50117758420688));
#160284=CARTESIAN_POINT('Ctrl Pts',(-4.73599881429248,5.16990732929714,
4.5095454249465));
#160285=CARTESIAN_POINT('Ctrl Pts',(-4.87187062076033,5.04543919605208,
4.51790999683743));
#160286=CARTESIAN_POINT('Ctrl Pts',(-5.00287385753078,4.91557384630014,
4.52627456872838));
#160287=CARTESIAN_POINT('Ctrl Pts',(-5.12857851876306,4.78072263778,4.53463914061932));
#160288=CARTESIAN_POINT('Ctrl Pts',(-5.25425247431509,4.64590436915284,
4.54300166930941));
#160289=CARTESIAN_POINT('Ctrl Pts',(-5.37463021181935,4.50610291102831,
4.5513641979995));
#160290=CARTESIAN_POINT('Ctrl Pts',(-5.48931927309304,4.36176575259944,
4.55972672668959));
#160291=CARTESIAN_POINT('Ctrl Pts',(-5.60401748696586,4.21741707554675,
4.56808992273952));
#160292=CARTESIAN_POINT('Ctrl Pts',(-5.71302590842811,4.0685322286015,4.57645311878946));
#160293=CARTESIAN_POINT('Ctrl Pts',(-5.81599252567112,3.91559159053107,
4.58481631483939));
#160294=CARTESIAN_POINT('Ctrl Pts',(-5.91896616505678,3.76264052217747,
4.59318008124461));
#160295=CARTESIAN_POINT('Ctrl Pts',(-6.01589699478896,3.60563338380146,
4.60154384764983));
#160296=CARTESIAN_POINT('Ctrl Pts',(-6.10647639889291,3.44507946965871,
4.60990761405506));
#160297=CARTESIAN_POINT('Ctrl Pts',(-6.19707405671325,3.28449320041665,
4.61827306594079));
#160298=CARTESIAN_POINT('Ctrl Pts',(-6.28131757511131,3.12035901653803,
4.62663851782652));
#160299=CARTESIAN_POINT('Ctrl Pts',(-6.35894415133984,2.95321110702247,
4.63500396971225));
#160300=CARTESIAN_POINT('Ctrl Pts',(-6.43659672456651,2.78600721997828,
4.64337222317249));
#160301=CARTESIAN_POINT('Ctrl Pts',(-6.50762779842177,2.61578789281798,
4.65174047663273));
#160302=CARTESIAN_POINT('Ctrl Pts',(-6.57182242155123,2.44310798412525,
4.66010873009297));
#160303=CARTESIAN_POINT('Ctrl Pts',(-6.63607656225491,2.2702679765211,4.66848474211806));
#160304=CARTESIAN_POINT('Ctrl Pts',(-6.69348147160369,2.09496313714209,
4.67686075414315));
#160305=CARTESIAN_POINT('Ctrl Pts',(-6.74387147511934,1.91776538960629,
4.68523676616824));
#160306=CARTESIAN_POINT('Ctrl Pts',(-6.79428619051588,1.74048074210371,
4.69361688589321));
#160307=CARTESIAN_POINT('Ctrl Pts',(-6.83767905608054,1.56130165305553,
4.70199700561819));
#160308=CARTESIAN_POINT('Ctrl Pts',(-6.87393525061726,1.38081162104809,
4.71037712534316));
#160309=CARTESIAN_POINT('Ctrl Pts',(-6.91023287244005,1.20011535636002,
4.7187668204144));
#160310=CARTESIAN_POINT('Ctrl Pts',(-6.93937747039207,1.01810547924149,
4.72715651548564));
#160311=CARTESIAN_POINT('Ctrl Pts',(-6.96130576314523,0.835373350365624,
4.73554621055688));
#160312=CARTESIAN_POINT('Ctrl Pts',(-6.97522765034435,0.71935993726033,
4.74087268032504));
#160313=CARTESIAN_POINT('Ctrl Pts',(-6.98624186628859,0.603055503857434,
4.74619915009319));
#160314=CARTESIAN_POINT('Ctrl Pts',(-6.99434311623759,0.486611687939976,
4.75152561986134));
#160315=CARTESIAN_POINT('Ctrl Pts',(-7.00709058383346,0.303385176044988,
4.75990691919134));
#160316=CARTESIAN_POINT('Ctrl Pts',(-7.01264880468849,0.119443890517566,
4.76828821852136));
#160317=CARTESIAN_POINT('Ctrl Pts',(-7.01095217616347,-0.0646231076991999,
4.77666951785137));
#160318=CARTESIAN_POINT('Ctrl Pts',(-7.00925769786622,-0.248456827997147,
4.78504019511396));
#160319=CARTESIAN_POINT('Ctrl Pts',(-7.000326696783,-0.432415618489877,
4.79341087237654));
#160320=CARTESIAN_POINT('Ctrl Pts',(-6.98414535408082,-0.615906028198585,
4.80178154963913));
#160321=CARTESIAN_POINT('Ctrl Pts',(-6.96798237441494,-0.799188207903296,
4.8101427276251));
#160322=CARTESIAN_POINT('Ctrl Pts',(-6.94458548082489,-0.982002741824664,
4.81850390561106));
#160323=CARTESIAN_POINT('Ctrl Pts',(-6.91399287360902,-1.16375646343372,
4.82686508359703));
#160324=CARTESIAN_POINT('Ctrl Pts',(-6.88343996386488,-1.34527433841562,
4.83521541198052));
#160325=CARTESIAN_POINT('Ctrl Pts',(-6.84571001881127,-1.52573382513473,
4.84356574036403));
#160326=CARTESIAN_POINT('Ctrl Pts',(-6.80089297609878,-1.70454723904923,
4.85191606874752));
#160327=CARTESIAN_POINT('Ctrl Pts',(-6.75611041737426,-1.8832230669196,
4.86025997206131));
#160328=CARTESIAN_POINT('Ctrl Pts',(-6.70425170732621,-2.06025502952368,
4.8686038753751));
#160329=CARTESIAN_POINT('Ctrl Pts',(-6.64545797108466,-2.2350648574588,
4.87694777868888));
#160330=CARTESIAN_POINT('Ctrl Pts',(-6.58671145822536,-2.40973427738703,
4.88528498014358));
#160331=CARTESIAN_POINT('Ctrl Pts',(-6.52104113237506,-2.58218481257427,
4.89362218159826));
#160332=CARTESIAN_POINT('Ctrl Pts',(-6.44863819916045,-2.75185245586108,
4.90195938305295));
#160333=CARTESIAN_POINT('Ctrl Pts',(-6.42480349530858,-2.80770624315171,
4.90470395041789));
#160334=CARTESIAN_POINT('Ctrl Pts',(-6.40023958290911,-2.86325857395826,
4.90744851778282));
#160335=CARTESIAN_POINT('Ctrl Pts',(-6.37495445485824,-2.91848972261049,
4.91019308514775));
#160336=CARTESIAN_POINT('Ctrl Pts',(-6.29813533133291,-3.08628829662708,
4.91853139607132));
#160337=CARTESIAN_POINT('Ctrl Pts',(-6.21471876977992,-3.25098310266247,
4.92686970699488));
#160338=CARTESIAN_POINT('Ctrl Pts',(-6.12499220819046,-3.412051730573,4.93520801791844));
#160339=CARTESIAN_POINT('Ctrl Pts',(-6.03520919354579,-3.57322169766318,
4.94355157503799));
#160340=CARTESIAN_POINT('Ctrl Pts',(-5.93910841956194,-3.73076064971087,
4.95189513215755));
#160341=CARTESIAN_POINT('Ctrl Pts',(-5.83702160499504,-3.88417370174419,
4.9602386892771));
#160342=CARTESIAN_POINT('Ctrl Pts',(-5.73485712307548,-4.03770346998288,
4.96858859415072));
#160343=CARTESIAN_POINT('Ctrl Pts',(-5.62669769781581,-4.18710080451296,
4.97693849902432));
#160344=CARTESIAN_POINT('Ctrl Pts',(-5.51291665075828,-4.3319021877568,
4.98528840389795));
#160345=CARTESIAN_POINT('Ctrl Pts',(-5.39896494036342,-4.4769207625976,
4.99365083302468));
#160346=CARTESIAN_POINT('Ctrl Pts',(-5.27937496094569,-4.61732935272852,
5.00201326215141));
#160347=CARTESIAN_POINT('Ctrl Pts',(-5.15455938018053,-4.7526986185422,
5.01037569127813));
#160348=CARTESIAN_POINT('Ctrl Pts',(-5.02963706496323,-4.88818364365719,
5.01874527142949));
#160349=CARTESIAN_POINT('Ctrl Pts',(-4.89948046325721,-5.0186205148773,
5.02711485158085));
#160350=CARTESIAN_POINT('Ctrl Pts',(-4.76453734851883,-5.14361841674411,
5.0354844317322));
#160351=CARTESIAN_POINT('Ctrl Pts',(-4.62938610036217,-5.2688091127423,
5.04386692094771));
#160352=CARTESIAN_POINT('Ctrl Pts',(-4.48943383498774,-5.38854386317103,
5.05224941016321));
#160353=CARTESIAN_POINT('Ctrl Pts',(-4.34516057201549,-5.50247273195443,
5.06063189937873));
#160354=CARTESIAN_POINT('Ctrl Pts',(-4.297952067592,-5.53975206836868,5.06337478306388));
#160355=CARTESIAN_POINT('Ctrl Pts',(-4.25028113534252,-5.57641011894061,
5.06611766674903));
#160356=CARTESIAN_POINT('Ctrl Pts',(-4.20216521516231,-5.61243566261386,
5.06886055043419));
#160357=CARTESIAN_POINT('Ctrl Pts',(-4.05498959952626,-5.72262957657989,
5.07725040546489));
#160358=CARTESIAN_POINT('Ctrl Pts',(-3.90335144205631,-5.82712488836407,
5.08564026049558));
#160359=CARTESIAN_POINT('Ctrl Pts',(-3.74771901562778,-5.92555725163481,
5.09403011552628));
#160360=CARTESIAN_POINT('Ctrl Pts',(-3.59223020465912,-6.02389878287626,
5.10241222851429));
#160361=CARTESIAN_POINT('Ctrl Pts',(-3.43275474896385,-6.1161883439764,
5.1107943415023));
#160362=CARTESIAN_POINT('Ctrl Pts',(-3.26979150759739,-6.20210368015112,
5.11917645449031));
#160363=CARTESIAN_POINT('Ctrl Pts',(-3.10695469120247,-6.28795236421557,
5.12755206473336));
#160364=CARTESIAN_POINT('Ctrl Pts',(-2.94063577338977,-6.36743652951964,
5.13592767497642));
#160365=CARTESIAN_POINT('Ctrl Pts',(-2.77136032177016,-6.44027860650593,
5.14430328521948));
#160366=CARTESIAN_POINT('Ctrl Pts',(-2.60219134695455,-6.51307486473068,
5.15267362707777));
#160367=CARTESIAN_POINT('Ctrl Pts',(-2.43006984759372,-6.57923723553984,
5.16104396893607));
#160368=CARTESIAN_POINT('Ctrl Pts',(-2.25554400260356,-6.63853506542062,
5.16941431079436));
#160369=CARTESIAN_POINT('Ctrl Pts',(-2.08110235345898,-6.69780428847283,
5.17778061458018));
#160370=CARTESIAN_POINT('Ctrl Pts',(-1.90425898244624,-6.75021546896936,
5.18614691836599));
#160371=CARTESIAN_POINT('Ctrl Pts',(-1.72558039697261,-6.7955867190467,
5.19451322215181));
#160372=CARTESIAN_POINT('Ctrl Pts',(-1.54695178291753,-6.8409452800504,
5.20287718611573));
#160373=CARTESIAN_POINT('Ctrl Pts',(-1.36648929574014,-6.8792677543224,
5.21124115007965));
#160374=CARTESIAN_POINT('Ctrl Pts',(-1.1847734369315,-6.91042245203877,
5.21960511404357));
#160375=CARTESIAN_POINT('Ctrl Pts',(-1.00308554118659,-6.94157235556269,
5.22796779093183));
#160376=CARTESIAN_POINT('Ctrl Pts',(-0.820144982198395,-6.96555662617578,
5.23633046782008));
#160377=CARTESIAN_POINT('Ctrl Pts',(-0.636541676327658,-6.98229484172632,
5.24469314470834));
#160378=CARTESIAN_POINT('Ctrl Pts',(-0.452942150520935,-6.99903271266691,
5.25305564942403));
#160379=CARTESIAN_POINT('Ctrl Pts',(-0.268680232367219,-7.00852479657953,
5.26141815413972));
#160380=CARTESIAN_POINT('Ctrl Pts',(-0.0843506078705089,-7.01074258102891,
5.2697806588554));
#160381=CARTESIAN_POINT('Ctrl Pts',(0.0999997914405822,-7.01296061543302,
5.27814410606465));
#160382=CARTESIAN_POINT('Ctrl Pts',(0.28441758368971,-7.00790271241602,
5.28650755327388));
#160383=CARTESIAN_POINT('Ctrl Pts',(0.468307997633091,-6.99559248254591,
5.29487100048313));
#160384=CARTESIAN_POINT('Ctrl Pts',(0.652306691433842,-6.98327500406558,
5.30323937232575));
#160385=CARTESIAN_POINT('Ctrl Pts',(0.835777058075314,-6.96369668652385,
5.31160774416838));
#160386=CARTESIAN_POINT('Ctrl Pts',(1.018128319102,-6.93693313275705,5.319976116011));
#160387=CARTESIAN_POINT('Ctrl Pts',(1.20053421733961,-6.910161559929,5.32834699523687));
#160388=CARTESIAN_POINT('Ctrl Pts',(1.38182001688646,-6.87620051104627,
5.33671787446275));
#160389=CARTESIAN_POINT('Ctrl Pts',(1.56140433386273,-6.83517688642326,
5.34508875368862));
#160390=CARTESIAN_POINT('Ctrl Pts',(1.74114081072128,-6.7941185029193,5.35346672547146));
#160391=CARTESIAN_POINT('Ctrl Pts',(1.91917260488283,-6.74598566497967,
5.36184469725429));
#160392=CARTESIAN_POINT('Ctrl Pts',(2.09493158788415,-6.69095570188484,
5.37022266903713));
#160393=CARTESIAN_POINT('Ctrl Pts',(2.20662788146104,-6.65598370325123,
5.37554693969376));
#160394=CARTESIAN_POINT('Ctrl Pts',(2.31740656455883,-6.61822716054181,
5.38087121035041));
#160395=CARTESIAN_POINT('Ctrl Pts',(2.42712577899576,-6.5777417869231,5.38619548100704));
#160396=CARTESIAN_POINT('Ctrl Pts',(2.58915804863588,-6.51795338059578,
5.39405831217204));
#160397=CARTESIAN_POINT('Ctrl Pts',(2.74921560712769,-6.45208674590007,
5.40192114333703));
#160398=CARTESIAN_POINT('Ctrl Pts',(2.90678976092643,-6.38029778680222,
5.40978397450203));
#160399=CARTESIAN_POINT('Ctrl Pts',(3.06424283978368,-6.30856398804516,
5.41764076411896));
#160400=CARTESIAN_POINT('Ctrl Pts',(3.21921596389816,-6.23091707130824,
5.42549755373589));
#160401=CARTESIAN_POINT('Ctrl Pts',(3.3712172023382,-6.14756221092223,5.43335434335282));
#160402=CARTESIAN_POINT('Ctrl Pts',(3.52313271927187,-6.06425435873344,
5.44120670211217));
#160403=CARTESIAN_POINT('Ctrl Pts',(3.67207935122264,-5.97524514899978,
5.44905906087151));
#160404=CARTESIAN_POINT('Ctrl Pts',(3.81758694489274,-5.8807870630286,5.45691141963085));
#160405=CARTESIAN_POINT('Ctrl Pts',(3.96306018251841,-5.78635127971612,
5.46476192435646));
#160406=CARTESIAN_POINT('Ctrl Pts',(4.10509567386234,-5.68646938107938,
5.47261242908209));
#160407=CARTESIAN_POINT('Ctrl Pts',(4.24324966124329,-5.58143878178904,
5.4804629338077));
#160408=CARTESIAN_POINT('Ctrl Pts',(4.3813814239992,-5.47642507861391,5.48831217563438));
#160409=CARTESIAN_POINT('Ctrl Pts',(4.51563262390902,-5.36626455691305,
5.49616141746104));
#160410=CARTESIAN_POINT('Ctrl Pts',(4.64559057446229,-5.25129648534218,
5.50401065928772));
#160411=CARTESIAN_POINT('Ctrl Pts',(4.77559231039103,-5.13628967877926,
5.51186254567749));
#160412=CARTESIAN_POINT('Ctrl Pts',(4.90129762170006,-5.01647233999805,
5.51971443206726));
#160413=CARTESIAN_POINT('Ctrl Pts',(5.02232871478114,-4.89222248504551,
5.52756631845704));
#160414=CARTESIAN_POINT('Ctrl Pts',(5.11120034255486,-4.80098736042441,
5.53333186106919));
#160415=CARTESIAN_POINT('Ctrl Pts',(5.19755245283155,-4.70736313794122,
5.53909740368134));
#160416=CARTESIAN_POINT('Ctrl Pts',(5.28124885572657,-4.61151136682832,
5.54486294629348));
#160417=CARTESIAN_POINT('Ctrl Pts',(5.42141159660048,-4.45099255727263,
5.55451825078916));
#160418=CARTESIAN_POINT('Ctrl Pts',(5.55405446686134,-4.28430810827498,
5.56417355528482));
#160419=CARTESIAN_POINT('Ctrl Pts',(5.67873381976766,-4.11212946862413,
5.57382885978049));
#160420=CARTESIAN_POINT('Ctrl Pts',(5.80410387309668,-3.93899699133767,
5.58353765286702));
#160421=CARTESIAN_POINT('Ctrl Pts',(5.92142194851332,-3.76030935149879,
5.59324644595356));
#160422=CARTESIAN_POINT('Ctrl Pts',(6.03028522262628,-3.57677042823203,
5.60295523904009));
#160423=CARTESIAN_POINT('Ctrl Pts',(6.13967235620445,-3.39234829983506,
5.6127107516764));
#160424=CARTESIAN_POINT('Ctrl Pts',(6.24052312079776,-3.20302813553686,
5.62246626431272));
#160425=CARTESIAN_POINT('Ctrl Pts',(6.33247728879412,-3.00954447539935,
5.63222177694904));
#160426=CARTESIAN_POINT('Ctrl Pts',(6.42452250558758,-2.8158692366211,5.64198694904626));
#160427=CARTESIAN_POINT('Ctrl Pts',(6.50765349940626,-2.61802229548323,
5.65175212114348));
#160428=CARTESIAN_POINT('Ctrl Pts',(6.58155734801784,-2.41676011164792,
5.6615172932407));
#160429=CARTESIAN_POINT('Ctrl Pts',(6.65536043037557,-2.21577234432387,
5.67126915074296));
#160430=CARTESIAN_POINT('Ctrl Pts',(6.71996149939726,-2.01137867682215,
5.6810210082452));
#160431=CARTESIAN_POINT('Ctrl Pts',(6.77509719585795,-1.80435155919731,
5.69077286574746));
#160432=CARTESIAN_POINT('Ctrl Pts',(6.7991403477887,-1.71407276048134,5.69502538102494));
#160433=CARTESIAN_POINT('Ctrl Pts',(6.82138419463603,-1.62329342927667,
5.69927789630243));
#160434=CARTESIAN_POINT('Ctrl Pts',(6.84180979817911,-1.53207873428241,
5.70353041157991));
#160435=CARTESIAN_POINT('Ctrl Pts',(6.88098123745258,-1.35715068976807,
5.71168572232018));
#160436=CARTESIAN_POINT('Ctrl Pts',(6.91347900255069,-1.18054410539551,
5.71984103306045));
#160437=CARTESIAN_POINT('Ctrl Pts',(6.93916435907318,-1.00280833675662,
5.72799634380073));
#160438=CARTESIAN_POINT('Ctrl Pts',(6.96482790339024,-0.825223502720967,
5.73614472898741));
#160439=CARTESIAN_POINT('Ctrl Pts',(6.98369051605902,-0.646511743554583,
5.74429311417409));
#160440=CARTESIAN_POINT('Ctrl Pts',(6.995664336616,-0.467233401951416,5.75244149936078));
#160441=CARTESIAN_POINT('Ctrl Pts',(7.00599612160768,-0.312540480816032,
5.75947245187736));
#160442=CARTESIAN_POINT('Ctrl Pts',(7.01119974088769,-0.157426046806037,
5.76650340439395));
#160443=CARTESIAN_POINT('Ctrl Pts',(7.01124963752017,-0.002254522849646,
5.77353435691053));
#160444=CARTESIAN_POINT('Ctrl Pts',(7.01125,3.556613210152E-12,5.77353435691053));
#160445=CARTESIAN_POINT('Ctrl Pts',(7.0112499999999,0.191008754743661,5.78220613084263));
#160446=CARTESIAN_POINT('Ctrl Pts',(7.00344012880999,0.382017367486429,
5.79087790477474));
#160447=CARTESIAN_POINT('Ctrl Pts',(6.98784644419152,0.572388534913077,
5.79954967870684));
#160448=CARTESIAN_POINT('Ctrl Pts',(6.97225169663171,0.762772678963806,
5.8082220437492));
#160449=CARTESIAN_POINT('Ctrl Pts',(6.94887209704284,0.952519007630189,
5.81689440879155));
#160450=CARTESIAN_POINT('Ctrl Pts',(6.91778566246054,1.14099434299889,5.82556677383391));
#160451=CARTESIAN_POINT('Ctrl Pts',(6.88670108297145,1.32945843103985,5.83423862135003));
#160452=CARTESIAN_POINT('Ctrl Pts',(6.84791063501108,1.51665139731098,5.84291046886614));
#160453=CARTESIAN_POINT('Ctrl Pts',(6.80154374572927,1.70194865887049,5.85158231638226));
#160454=CARTESIAN_POINT('Ctrl Pts',(6.75517597619852,1.88724943819281,5.86025432852846));
#160455=CARTESIAN_POINT('Ctrl Pts',(6.70123154646085,2.07065416525472,5.86892634067466));
#160456=CARTESIAN_POINT('Ctrl Pts',(6.6398904528553,2.25155087363823,5.87759835282085));
#160457=CARTESIAN_POINT('Ctrl Pts',(6.61790934153639,2.31637382429788,5.88070590198798));
#160458=CARTESIAN_POINT('Ctrl Pts',(6.59497889661513,2.38087486019071,5.88381345115511));
#160459=CARTESIAN_POINT('Ctrl Pts',(6.57110895151814,2.44502632087637,5.88692100032223));
#160460=CARTESIAN_POINT('',(7.01124988024546,0.00129586190515713,5.22646564305715));
#160461=CARTESIAN_POINT('Ctrl Pts',(6.57110895151813,2.44502632087638,5.33975062352347));
#160462=CARTESIAN_POINT('Ctrl Pts',(6.63727736514693,2.26719598367653,5.33111643416571));
#160463=CARTESIAN_POINT('Ctrl Pts',(6.6962654193017,2.08656392115047,5.32248224480796));
#160464=CARTESIAN_POINT('Ctrl Pts',(6.74784989526467,1.90371960999422,5.3138480554502));
#160465=CARTESIAN_POINT('Ctrl Pts',(6.79935992125682,1.72113919128581,5.30522632749937));
#160466=CARTESIAN_POINT('Ctrl Pts',(6.84348761691352,1.53635317540665,5.29660459954852));
#160467=CARTESIAN_POINT('Ctrl Pts',(6.88005927097208,1.34996703308311,5.28798287159768));
#160468=CARTESIAN_POINT('Ctrl Pts',(6.91659744670839,1.1637515118456,5.27936903612517));
#160469=CARTESIAN_POINT('Ctrl Pts',(6.94559332009529,0.975939069717269,
5.27075520065265));
#160470=CARTESIAN_POINT('Ctrl Pts',(6.96692361721662,0.78714793677513,5.26214136518013));
#160471=CARTESIAN_POINT('Ctrl Pts',(6.98822860751318,0.598580790591932,
5.25353774938826));
#160472=CARTESIAN_POINT('Ctrl Pts',(7.00188613807103,0.409037558786854,
5.24493413359641));
#160473=CARTESIAN_POINT('Ctrl Pts',(7.00782436062502,0.219144457220791,
5.23633051780455));
#160474=CARTESIAN_POINT('Ctrl Pts',(7.0100939421181,0.146567542991075,5.23304222623291));
#160475=CARTESIAN_POINT('Ctrl Pts',(7.01123645377904,0.0739396047210392,
5.22975393466127));
#160476=CARTESIAN_POINT('Ctrl Pts',(7.01124988024532,0.00129586262259841,
5.22646564308963));
#160477=CARTESIAN_POINT('Ctrl Pts',(7.01124988024546,0.00129586190516873,
5.22646564305716));
#160478=CARTESIAN_POINT('Ctrl Pts',(7.01128652420434,-0.196965967775037,
5.21749112323366));
#160479=CARTESIAN_POINT('Ctrl Pts',(7.00290926625389,-0.395057195486619,
5.20851660341015));
#160480=CARTESIAN_POINT('Ctrl Pts',(6.98618743385599,-0.592293594033082,
5.19954208358664));
#160481=CARTESIAN_POINT('Ctrl Pts',(6.96943444002355,-0.789897546145331,
5.19055083958451));
#160482=CARTESIAN_POINT('Ctrl Pts',(6.94430580230218,-0.986643262615029,
5.18155959558237));
#160483=CARTESIAN_POINT('Ctrl Pts',(6.91092245162695,-1.18185338773412,
5.17256835158023));
#160484=CARTESIAN_POINT('Ctrl Pts',(6.87746142153865,-1.37751774550624,
5.16355618593474));
#160485=CARTESIAN_POINT('Ctrl Pts',(6.83570728321723,-1.57163914238257,
5.15454402028925));
#160486=CARTESIAN_POINT('Ctrl Pts',(6.78583228453984,-1.76354948005347,
5.14553185464376));
#160487=CARTESIAN_POINT('Ctrl Pts',(6.73590749769426,-1.95565139395338,
5.13651069252246));
#160488=CARTESIAN_POINT('Ctrl Pts',(6.6778457133722,-2.14553762481288,5.12748953040116));
#160489=CARTESIAN_POINT('Ctrl Pts',(6.61186906878772,-2.33255524687159,
5.11846836827986));
#160490=CARTESIAN_POINT('Ctrl Pts',(6.54581642848924,-2.51978828664077,
5.10943681506243));
#160491=CARTESIAN_POINT('Ctrl Pts',(6.47183077497929,-2.70414590213013,
5.100405261845));
#160492=CARTESIAN_POINT('Ctrl Pts',(6.39018315943529,-2.884993197803,5.09137370862757));
#160493=CARTESIAN_POINT('Ctrl Pts',(6.3479506085923,-2.97853717405308,5.08670210214029));
#160494=CARTESIAN_POINT('Ctrl Pts',(6.30366886474925,-3.07114230857741,
5.082030495653));
#160495=CARTESIAN_POINT('Ctrl Pts',(6.25738035770964,-3.16272313385943,
5.07735888916572));
#160496=CARTESIAN_POINT('Ctrl Pts',(6.17947165912919,-3.31686383462863,
5.06949605657549));
#160497=CARTESIAN_POINT('Ctrl Pts',(6.09575013385041,-3.4683483313541,5.06163322398526));
#160498=CARTESIAN_POINT('Ctrl Pts',(6.00642878203436,-3.61668907273617,
5.05377039139503));
#160499=CARTESIAN_POINT('Ctrl Pts',(5.91717606189674,-3.76491583382291,
5.04591360035463));
#160500=CARTESIAN_POINT('Ctrl Pts',(5.8223322672198,-3.9100033187394,5.03805680931422));
#160501=CARTESIAN_POINT('Ctrl Pts',(5.72215743083715,-4.05148625805583,
5.03020001827382));
#160502=CARTESIAN_POINT('Ctrl Pts',(5.62203908833992,-4.19288940766408,
5.0223476580932));
#160503=CARTESIAN_POINT('Ctrl Pts',(5.51659590430043,-4.3306917451642,5.01449529791258));
#160504=CARTESIAN_POINT('Ctrl Pts',(5.40613242074016,-4.46445504086693,
5.00664293773195));
#160505=CARTESIAN_POINT('Ctrl Pts',(5.29569501897807,-4.59818675339694,
4.99879243159093));
#160506=CARTESIAN_POINT('Ctrl Pts',(5.1802399129313,-4.72788102310245,4.99094192544991));
#160507=CARTESIAN_POINT('Ctrl Pts',(5.06011326814566,-4.85313097660019,
4.98309141930889));
#160508=CARTESIAN_POINT('Ctrl Pts',(4.9400059479837,-4.97836078129396,4.97524217606901));
#160509=CARTESIAN_POINT('Ctrl Pts',(4.81522885136987,-5.09914741976571,
4.96739293282913));
#160510=CARTESIAN_POINT('Ctrl Pts',(4.68616617399064,-5.21511966806572,
4.95954368958925));
#160511=CARTESIAN_POINT('Ctrl Pts',(4.55706001301264,-5.33113098955728,
4.95169180179441));
#160512=CARTESIAN_POINT('Ctrl Pts',(4.4236656712221,-5.44232442568857,4.94383991399956));
#160513=CARTESIAN_POINT('Ctrl Pts',(4.28640185157114,-5.54836784373094,
4.93598802620472));
#160514=CARTESIAN_POINT('Ctrl Pts',(4.18561090107159,-5.62623407917368,
4.93022249209624));
#160515=CARTESIAN_POINT('Ctrl Pts',(4.08273435008407,-5.7013243541646,4.92445695798776));
#160516=CARTESIAN_POINT('Ctrl Pts',(3.97794824856842,-5.77352182763791,
4.91869142387928));
#160517=CARTESIAN_POINT('Ctrl Pts',(3.802467499896,-5.894427811486,4.90903613346177));
#160518=CARTESIAN_POINT('Ctrl Pts',(3.62172062104522,-6.00715877938123,
4.89938084304426));
#160519=CARTESIAN_POINT('Ctrl Pts',(3.43642534724975,-6.11135070138177,
4.88972555262675));
#160520=CARTESIAN_POINT('Ctrl Pts',(3.25010359379651,-6.21611981505184,
4.88001677482664));
#160521=CARTESIAN_POINT('Ctrl Pts',(3.05918298030223,-6.31225503789554,
4.87030799702654));
#160522=CARTESIAN_POINT('Ctrl Pts',(2.8644087958511,-6.39943660119787,4.86059921922643));
#160523=CARTESIAN_POINT('Ctrl Pts',(2.66869735532569,-6.48703768339075,
4.85084372265302));
#160524=CARTESIAN_POINT('Ctrl Pts',(2.46909521703533,-6.5655987326719,4.84108822607961));
#160525=CARTESIAN_POINT('Ctrl Pts',(2.2663732636386,-6.63484580019492,4.83133272950621));
#160526=CARTESIAN_POINT('Ctrl Pts',(2.06345058237605,-6.70416143363221,
4.8215675733968));
#160527=CARTESIAN_POINT('Ctrl Pts',(1.85740194694757,-6.76414463665865,
4.81180241728738));
#160528=CARTESIAN_POINT('Ctrl Pts',(1.64901461157417,-6.81457096032574,
4.80203726117797));
#160529=CARTESIAN_POINT('Ctrl Pts',(1.44091138821088,-6.86492853353756,
4.79228541872856));
#160530=CARTESIAN_POINT('Ctrl Pts',(1.23047587455813,-6.90575526019108,
4.78253357627916));
#160531=CARTESIAN_POINT('Ctrl Pts',(1.01850554823742,-6.93687775665029,
4.77278173382975));
#160532=CARTESIAN_POINT('Ctrl Pts',(0.926069348134061,-6.95044968136426,
4.76852914208412));
#160533=CARTESIAN_POINT('Ctrl Pts',(0.833341447452034,-6.96217683157803,
4.76427655033848));
#160534=CARTESIAN_POINT('Ctrl Pts',(0.740388755513583,-6.97204783784571,
4.76002395859285));
#160535=CARTESIAN_POINT('Ctrl Pts',(0.56480297425954,-6.99069397182128,
4.75199089759764));
#160536=CARTESIAN_POINT('Ctrl Pts',(0.388329000813756,-7.00272228021521,
4.74395783660243));
#160537=CARTESIAN_POINT('Ctrl Pts',(0.211513544990063,-7.00805883128743,
4.73592477560721));
#160538=CARTESIAN_POINT('Ctrl Pts',(0.0348117535483582,-7.01339195180107,
4.72789687860011));
#160539=CARTESIAN_POINT('Ctrl Pts',(-0.142230718440287,-7.01204186670302,
4.71986898159302));
#160540=CARTESIAN_POINT('Ctrl Pts',(-0.319061895795209,-7.00398644124556,
4.71184108458592));
#160541=CARTESIAN_POINT('Ctrl Pts',(-0.495813231268391,-6.99593465293136,
4.70381681229259));
#160542=CARTESIAN_POINT('Ctrl Pts',(-0.672353096637324,-6.9811835691244,
4.69579253999928));
#160543=CARTESIAN_POINT('Ctrl Pts',(-0.848129418575118,-6.95976314624625,
4.68776826770595));
#160544=CARTESIAN_POINT('Ctrl Pts',(-1.02388448507122,-6.93834531359495,
4.67974496573359));
#160545=CARTESIAN_POINT('Ctrl Pts',(-1.19887582744569,-6.91025978490329,
4.67172166376123));
#160546=CARTESIAN_POINT('Ctrl Pts',(-1.3725562172269,-6.87558841067816,
4.66369836178887));
#160547=CARTESIAN_POINT('Ctrl Pts',(-1.54622237433824,-6.84091987768469,
4.65567571730588));
#160548=CARTESIAN_POINT('Ctrl Pts',(-1.71857743408248,-6.7996666498913,
4.64765307282289));
#160549=CARTESIAN_POINT('Ctrl Pts',(-1.88908438820088,-6.75196169544494,
4.6396304283399));
#160550=CARTESIAN_POINT('Ctrl Pts',(-2.05965543780748,-6.70423880816786,
4.63160476805431));
#160551=CARTESIAN_POINT('Ctrl Pts',(-2.22837664152133,-6.65005945106735,
4.62357910776871));
#160552=CARTESIAN_POINT('Ctrl Pts',(-2.39472581274701,-6.58960657735067,
4.61555344748312));
#160553=CARTESIAN_POINT('Ctrl Pts',(-2.49281334188007,-6.55396063473387,
4.61082112942422));
#160554=CARTESIAN_POINT('Ctrl Pts',(-2.59007646853187,-6.51613441841434,
4.60608881136533));
#160555=CARTESIAN_POINT('Ctrl Pts',(-2.6864113892892,-6.4761732844325,4.60135649330643));
#160556=CARTESIAN_POINT('Ctrl Pts',(-2.864126479334,-6.40245446608456,4.59262648840947));
#160557=CARTESIAN_POINT('Ctrl Pts',(-3.03877054673932,-6.32143101450485,
4.58389648351253));
#160558=CARTESIAN_POINT('Ctrl Pts',(-3.20976034755821,-6.23338311623335,
4.57516647861559));
#160559=CARTESIAN_POINT('Ctrl Pts',(-3.38079958204756,-6.1453097630472,
4.56643394984773));
#160560=CARTESIAN_POINT('Ctrl Pts',(-3.54818219764428,-6.05020803502009,
4.55770142107988));
#160561=CARTESIAN_POINT('Ctrl Pts',(-3.71134950974166,-5.94840410354243,
4.54896889231202));
#160562=CARTESIAN_POINT('Ctrl Pts',(-3.87683612734117,-5.84515310270155,
4.54011223695435));
#160563=CARTESIAN_POINT('Ctrl Pts',(-4.03798644674918,-5.73500806499387,
4.53125558159669));
#160564=CARTESIAN_POINT('Ctrl Pts',(-4.19424763424862,-5.61835503907504,
4.52239892623902));
#160565=CARTESIAN_POINT('Ctrl Pts',(-4.34841689211665,-5.50326369283764,
4.5136608383905));
#160566=CARTESIAN_POINT('Ctrl Pts',(-4.49782690134713,-5.38183771029516,
4.50492275054197));
#160567=CARTESIAN_POINT('Ctrl Pts',(-4.64197892218068,-5.2544893423177,
4.49618466269344));
#160568=CARTESIAN_POINT('Ctrl Pts',(-4.78906495094792,-5.12454898069474,
4.4872687235812));
#160569=CARTESIAN_POINT('Ctrl Pts',(-4.93067643526651,-4.98844275983394,
4.47835278446896));
#160570=CARTESIAN_POINT('Ctrl Pts',(-5.06632123745495,-4.84664994417928,
4.46943684535672));
#160571=CARTESIAN_POINT('Ctrl Pts',(-5.20196603964339,-4.70485712852462,
4.46052090624448));
#160572=CARTESIAN_POINT('Ctrl Pts',(-5.33164395503506,-4.55737794082467,
4.45160496713224));
#160573=CARTESIAN_POINT('Ctrl Pts',(-5.45490408292047,-4.40473018567967,
4.44268902802));
#160574=CARTESIAN_POINT('Ctrl Pts',(-5.57574224718921,-4.2550818376866,
4.43394828003006));
#160575=CARTESIAN_POINT('Ctrl Pts',(-5.69042532874889,-4.10045025632596,
4.4252075320401));
#160576=CARTESIAN_POINT('Ctrl Pts',(-5.79856547132975,-3.94135319873803,
4.41646678405016));
#160577=CARTESIAN_POINT('Ctrl Pts',(-5.90668616011713,-3.78228476180128,
4.40772760847081));
#160578=CARTESIAN_POINT('Ctrl Pts',(-6.00826610670791,-3.61875267926487,
4.39898843289146));
#160579=CARTESIAN_POINT('Ctrl Pts',(-6.10296041194863,-3.4513042132921,
4.39024925731211));
#160580=CARTESIAN_POINT('Ctrl Pts',(-6.19888057478418,-3.28168805652492,
4.38139694943056));
#160581=CARTESIAN_POINT('Ctrl Pts',(-6.28773541961175,-3.10805364858808,
4.37254464154902));
#160582=CARTESIAN_POINT('Ctrl Pts',(-6.36921354941784,-2.93099732589646,
4.36369233366747));
#160583=CARTESIAN_POINT('Ctrl Pts',(-6.44960915198586,-2.75629339264287,
4.35495763850513));
#160584=CARTESIAN_POINT('Ctrl Pts',(-6.52282273410569,-2.57825816930568,
4.34622294334278));
#160585=CARTESIAN_POINT('Ctrl Pts',(-6.58860235168398,-2.39748735426996,
4.33748824818043));
#160586=CARTESIAN_POINT('Ctrl Pts',(-6.65571055363997,-2.21306541918152,
4.32857713393929));
#160587=CARTESIAN_POINT('Ctrl Pts',(-6.71508118046617,-2.02579647754138,
4.31966601969815));
#160588=CARTESIAN_POINT('Ctrl Pts',(-6.76649883806085,-1.83633331315999,
4.31075490545701));
#160589=CARTESIAN_POINT('Ctrl Pts',(-6.81791649565554,-1.6468701487786,
4.30184379121587));
#160590=CARTESIAN_POINT('Ctrl Pts',(-6.86138109162614,-1.4552130506391,
4.29293267697472));
#160591=CARTESIAN_POINT('Ctrl Pts',(-6.89673142008012,-1.26203101458707,
4.28402156273358));
#160592=CARTESIAN_POINT('Ctrl Pts',(-6.92856904036456,-1.08804518252878,
4.27599593231008));
#160593=CARTESIAN_POINT('Ctrl Pts',(-6.95383899451739,-0.912742376751788,
4.26797030188659));
#160594=CARTESIAN_POINT('Ctrl Pts',(-6.97244213013839,-0.736666345349977,
4.2599446714631));
#160595=CARTESIAN_POINT('Ctrl Pts',(-6.99103936169988,-0.560646195031204,
4.25192158812632));
#160596=CARTESIAN_POINT('Ctrl Pts',(-7.00297394870145,-0.383853671762903,
4.24389850478953));
#160597=CARTESIAN_POINT('Ctrl Pts',(-7.0081983319312,-0.206839799885826,
4.23587542145275));
#160598=CARTESIAN_POINT('Ctrl Pts',(-7.01342205637091,-0.0298482492990209,
4.22785334981958));
#160599=CARTESIAN_POINT('Ctrl Pts',(-7.01193725225357,0.147364227971745,
4.21983127818641));
#160600=CARTESIAN_POINT('Ctrl Pts',(-7.00374843033031,0.324244486685203,
4.21180920655323));
#160601=CARTESIAN_POINT('Ctrl Pts',(-6.99555656518028,0.501190479730516,
4.203784153663));
#160602=CARTESIAN_POINT('Ctrl Pts',(-6.9806557191138,0.67780364091553,4.19575910077279));
#160603=CARTESIAN_POINT('Ctrl Pts',(-6.95910248079907,0.853533376170037,
4.18773404788256));
#160604=CARTESIAN_POINT('Ctrl Pts',(-6.93754499739822,1.02929772282963,
4.17970741439269));
#160605=CARTESIAN_POINT('Ctrl Pts',(-6.90933256489879,1.20417793415915,
4.1716807809028));
#160606=CARTESIAN_POINT('Ctrl Pts',(-6.87457325192067,1.37763172382061,
4.16365414741293));
#160607=CARTESIAN_POINT('Ctrl Pts',(-6.83978603290037,1.55122476850053,
4.15562106984942));
#160608=CARTESIAN_POINT('Ctrl Pts',(-6.7984415168326,1.72338874676363,4.14758799228592));
#160609=CARTESIAN_POINT('Ctrl Pts',(-6.75069833517884,1.89359408266756,
4.1395549147224));
#160610=CARTESIAN_POINT('Ctrl Pts',(-6.72256498307134,1.9938900093255,4.13482130896399));
#160611=CARTESIAN_POINT('Ctrl Pts',(-6.69221075140437,2.09350612363944,
4.13008770320556));
#160612=CARTESIAN_POINT('Ctrl Pts',(-6.65967601729574,2.19233708793971,
4.12535409744714));
#160613=CARTESIAN_POINT('Ctrl Pts',(-6.59265675514161,2.39592191771794,
4.11560320278182));
#160614=CARTESIAN_POINT('Ctrl Pts',(-6.51634348769467,2.59629432247953,
4.10585230811651));
#160615=CARTESIAN_POINT('Ctrl Pts',(-6.43105328435768,2.79270124006353,
4.09610141345119));
#160616=CARTESIAN_POINT('Ctrl Pts',(-6.34564023879427,2.98939103964446,
4.08633647471558));
#160617=CARTESIAN_POINT('Ctrl Pts',(-6.25122441024143,3.18210389205048,
4.07657153597996));
#160618=CARTESIAN_POINT('Ctrl Pts',(-6.14817084124316,3.37010710058113,
4.06680659724435));
#160619=CARTESIAN_POINT('Ctrl Pts',(-6.0452890566934,3.55779691843731,4.0570579361072));
#160620=CARTESIAN_POINT('Ctrl Pts',(-5.93379832692504,3.7407927495352,4.04730927497005));
#160621=CARTESIAN_POINT('Ctrl Pts',(-5.81410786029961,3.91838950990101,
4.03756061383289));
#160622=CARTESIAN_POINT('Ctrl Pts',(-5.6947458817172,4.0954988595824,4.02783870769728));
#160623=CARTESIAN_POINT('Ctrl Pts',(-5.56722911418537,4.26723868639639,
4.01811680156166));
#160624=CARTESIAN_POINT('Ctrl Pts',(-5.4320089959831,4.43293411072832,4.00839489542604));
#160625=CARTESIAN_POINT('Ctrl Pts',(-5.29768353520315,4.59753324374508,
3.99873731237784));
#160626=CARTESIAN_POINT('Ctrl Pts',(-5.15575632941792,4.75616763870949,
3.98907972932964));
#160627=CARTESIAN_POINT('Ctrl Pts',(-5.00671485939788,4.9082005744656,3.97942214628144));
#160628=CARTESIAN_POINT('Ctrl Pts',(-4.94120089189194,4.97502949672207,
3.97517697490786));
#160629=CARTESIAN_POINT('Ctrl Pts',(-4.87431288738266,5.04058320983856,
3.97093180353428));
#160630=CARTESIAN_POINT('Ctrl Pts',(-4.80609502587596,5.10480921923144,
3.9666866321607));
#160631=CARTESIAN_POINT('Ctrl Pts',(-4.67991776677176,5.22360306074756,
3.95883466969053));
#160632=CARTESIAN_POINT('Ctrl Pts',(-4.54924017819576,5.33780310879715,
3.95098270722035));
#160633=CARTESIAN_POINT('Ctrl Pts',(-4.41444929813602,5.44704176197378,
3.94313074475017));
#160634=CARTESIAN_POINT('Ctrl Pts',(-4.27969663339582,5.55624944428624,
3.93528100843398));
#160635=CARTESIAN_POINT('Ctrl Pts',(-4.14083329296949,5.66049828982512,
3.92743127211779));
#160636=CARTESIAN_POINT('Ctrl Pts',(-3.99828058058831,5.75945995397055,
3.9195815358016));
#160637=CARTESIAN_POINT('Ctrl Pts',(-3.85573923930518,5.85841372417438,
3.9117324256406));
#160638=CARTESIAN_POINT('Ctrl Pts',(-3.70950942570064,5.95208093565143,
3.9038833154796));
#160639=CARTESIAN_POINT('Ctrl Pts',(-3.56004247386272,6.04017583740684,
3.89603420531861));
#160640=CARTESIAN_POINT('Ctrl Pts',(-3.41049984156261,6.12831534476102,
3.88818112087248));
#160641=CARTESIAN_POINT('Ctrl Pts',(-3.25771712511903,6.21087671103691,
3.88032803642635));
#160642=CARTESIAN_POINT('Ctrl Pts',(-3.10217167427491,6.28761937984691,
3.87247495198022));
#160643=CARTESIAN_POINT('Ctrl Pts',(-2.94658671212205,6.3643815426586,3.86461987271108));
#160644=CARTESIAN_POINT('Ctrl Pts',(-2.78823796560874,6.43532190740176,
3.85676479344193));
#160645=CARTESIAN_POINT('Ctrl Pts',(-2.62762332414846,6.50024785903515,
3.84890971417279));
#160646=CARTESIAN_POINT('Ctrl Pts',(-2.46684925761971,6.56523825575394,
3.84104683800208));
#160647=CARTESIAN_POINT('Ctrl Pts',(-2.30380516265391,6.62420218634343,
3.83318396183138));
#160648=CARTESIAN_POINT('Ctrl Pts',(-2.13900521393938,6.6769965746015,3.82532108566067));
#160649=CARTESIAN_POINT('Ctrl Pts',(-2.01812682852617,6.71572049691636,
3.81955377939854));
#160650=CARTESIAN_POINT('Ctrl Pts',(-1.8963041239431,6.75112623947487,3.81378647313642));
#160651=CARTESIAN_POINT('Ctrl Pts',(-1.77374330284059,6.78317486566049,
3.80801916687429));
#160652=CARTESIAN_POINT('Ctrl Pts',(-1.5957060076044,6.82973012427246,3.79964132150356));
#160653=CARTESIAN_POINT('Ctrl Pts',(-1.41571643005527,6.86930273055416,
3.7912634761328));
#160654=CARTESIAN_POINT('Ctrl Pts',(-1.23434857655566,6.90173964693359,
3.78288563076206));
#160655=CARTESIAN_POINT('Ctrl Pts',(-1.05310478568828,6.93415437520664,
3.77451351616185));
#160656=CARTESIAN_POINT('Ctrl Pts',(-0.870484921105781,6.95944308732074,
3.76614140156164));
#160657=CARTESIAN_POINT('Ctrl Pts',(-0.687074608834716,6.97750349655195,
3.75776928696143));
#160658=CARTESIAN_POINT('Ctrl Pts',(-0.503762847088566,6.99555420151523,
3.74940167088847));
#160659=CARTESIAN_POINT('Ctrl Pts',(-0.319661810952985,7.00638431563537,
3.74103405481551));
#160660=CARTESIAN_POINT('Ctrl Pts',(-0.135364160697066,7.00994316000485,
3.73266643874256));
#160661=CARTESIAN_POINT('Ctrl Pts',(0.0488614725731419,7.01350061370416,
3.7243020924372));
#160662=CARTESIAN_POINT('Ctrl Pts',(0.233283238559968,7.00979245737618,
3.71593774613184));
#160663=CARTESIAN_POINT('Ctrl Pts',(0.417306087178902,6.99882005713131,
3.70757339982649));
#160664=CARTESIAN_POINT('Ctrl Pts',(0.601283974752137,6.98785033769804,
3.69921109712475));
#160665=CARTESIAN_POINT('Ctrl Pts',(0.784862811510427,6.9696199337488,3.69084879442301));
#160666=CARTESIAN_POINT('Ctrl Pts',(0.967449822494202,6.94418227032211,
3.68248649172126));
#160667=CARTESIAN_POINT('Ctrl Pts',(1.15005142104003,6.91874257458496,3.67412352092375));
#160668=CARTESIAN_POINT('Ctrl Pts',(1.33166070911257,6.88609450834275,3.66576055012623));
#160669=CARTESIAN_POINT('Ctrl Pts',(1.51169152188426,6.84634320679027,3.65739757932871));
#160670=CARTESIAN_POINT('Ctrl Pts',(1.69173462933279,6.80658919053913,3.64903403740661));
#160671=CARTESIAN_POINT('Ctrl Pts',(1.87019872536886,6.75973104238083,3.64067049548451));
#160672=CARTESIAN_POINT('Ctrl Pts',(2.04650913219775,6.70592476354539,3.63230695356241));
#160673=CARTESIAN_POINT('Ctrl Pts',(2.22285509621616,6.65210763339329,3.62394172493303));
#160674=CARTESIAN_POINT('Ctrl Pts',(2.39704619044741,6.59133967441651,3.61557649630364));
#160675=CARTESIAN_POINT('Ctrl Pts',(2.56852374778743,6.5238265090016,3.60721126767427));
#160676=CARTESIAN_POINT('Ctrl Pts',(2.7400587687183,6.45629071934959,3.59884323578549));
#160677=CARTESIAN_POINT('Ctrl Pts',(2.90887813370036,6.38200533641811,3.59047520389672));
#160678=CARTESIAN_POINT('Ctrl Pts',(3.07444357628501,6.30122394926096,3.58210717200794));
#160679=CARTESIAN_POINT('Ctrl Pts',(3.24016260788494,6.22036762416076,3.57373137740155));
#160680=CARTESIAN_POINT('Ctrl Pts',(3.4026213893167,6.13300339721256,3.56535558279515));
#160681=CARTESIAN_POINT('Ctrl Pts',(3.56130557270496,6.0394311967536,3.55697978818876));
#160682=CARTESIAN_POINT('Ctrl Pts',(3.72006762203486,5.94581308064417,3.54859988360038));
#160683=CARTESIAN_POINT('Ctrl Pts',(3.87505109997757,5.84598108878888,3.540219979012));
#160684=CARTESIAN_POINT('Ctrl Pts',(4.02577050542334,5.7402785995249,3.53184007442363));
#160685=CARTESIAN_POINT('Ctrl Pts',(4.17666223258766,5.63445525764376,3.52345058885558));
#160686=CARTESIAN_POINT('Ctrl Pts',(4.32327988002905,5.52274820075145,3.51506110328756));
#160687=CARTESIAN_POINT('Ctrl Pts',(4.46516985074383,5.4055420418778,3.50667161771951));
#160688=CARTESIAN_POINT('Ctrl Pts',(4.55530048957808,5.33109093077125,3.50134249058015));
#160689=CARTESIAN_POINT('Ctrl Pts',(4.64352420715157,5.25442173762314,3.49601336344078));
#160690=CARTESIAN_POINT('Ctrl Pts',(4.72973243973347,5.17564079231093,3.49068423630143));
#160691=CARTESIAN_POINT('Ctrl Pts',(4.86533391691881,5.05172208711947,3.48230177107087));
#160692=CARTESIAN_POINT('Ctrl Pts',(4.99622050371155,4.92232668016906,3.4739193058403));
#160693=CARTESIAN_POINT('Ctrl Pts',(5.12193835131295,4.78783605482159,3.46553684060975));
#160694=CARTESIAN_POINT('Ctrl Pts',(5.24749632646853,4.65351645805617,3.45716503516414));
#160695=CARTESIAN_POINT('Ctrl Pts',(5.36789843988125,4.51411479332084,3.44879322971853));
#160696=CARTESIAN_POINT('Ctrl Pts',(5.48272532811655,4.37005143435741,3.44042142427291));
#160697=CARTESIAN_POINT('Ctrl Pts',(5.59771704647468,4.2257812773041,3.43203760138312));
#160698=CARTESIAN_POINT('Ctrl Pts',(5.70711726478799,4.07683624319286,3.42365377849332));
#160699=CARTESIAN_POINT('Ctrl Pts',(5.81054159026457,3.92367595378437,3.41526995560352));
#160700=CARTESIAN_POINT('Ctrl Pts',(5.91356675244229,3.77110678224002,3.40691848984428));
#160701=CARTESIAN_POINT('Ctrl Pts',(6.01066186247285,3.61435509316714,3.39856702408504));
#160702=CARTESIAN_POINT('Ctrl Pts',(6.10148678868888,3.45390873214031,3.39021555832579));
#160703=CARTESIAN_POINT('Ctrl Pts',(6.19283955649819,3.29252991494346,3.38181555687072));
#160704=CARTESIAN_POINT('Ctrl Pts',(6.27784880476541,3.12741359563608,3.37341555541566));
#160705=CARTESIAN_POINT('Ctrl Pts',(6.35621222836559,2.95908645876996,3.36501555396059));
#160706=CARTESIAN_POINT('Ctrl Pts',(6.43457565196577,2.79075932190384,3.35661555250552));
#160707=CARTESIAN_POINT('Ctrl Pts',(6.50629307529157,2.61922165809476,3.34821555105044));
#160708=CARTESIAN_POINT('Ctrl Pts',(6.57110895151814,2.44502632087637,3.33981554959537));
#160709=CARTESIAN_POINT('Origin',(0.,0.,50.));
#160710=CARTESIAN_POINT('',(6.57110895151814,2.44502632087636,1.34015432832236));
#160711=CARTESIAN_POINT('',(6.57110895151814,2.44502632087635,1.88679067599786));
#160712=CARTESIAN_POINT('',(6.57110895151814,2.44502632087636,50.));
#160713=CARTESIAN_POINT('',(7.01124672537777,0.00677631016985116,1.22646564305006));
#160714=CARTESIAN_POINT('Ctrl Pts',(6.57110895151814,2.44502632087636,1.34015432832236));
#160715=CARTESIAN_POINT('Ctrl Pts',(6.63376189300869,2.27664395985542,1.33198913246426));
#160716=CARTESIAN_POINT('Ctrl Pts',(6.68988070270378,2.10600776687022,1.32382393660616));
#160717=CARTESIAN_POINT('Ctrl Pts',(6.73932882506234,1.93366841784827,1.31565874074806));
#160718=CARTESIAN_POINT('Ctrl Pts',(6.78885956678129,1.76104111923176,1.30747990224335));
#160719=CARTESIAN_POINT('Ctrl Pts',(6.8316972634231,1.58670532059054,1.29930106373863));
#160720=CARTESIAN_POINT('Ctrl Pts',(6.86775650424132,1.41122186808137,1.29112222523392));
#160721=CARTESIAN_POINT('Ctrl Pts',(6.8997684057998,1.25543492195056,1.28386139091976));
#160722=CARTESIAN_POINT('Ctrl Pts',(6.92643882991178,1.09874375883881,1.27660055660559));
#160723=CARTESIAN_POINT('Ctrl Pts',(6.94774241808982,0.94154227434327,1.26933972229143));
#160724=CARTESIAN_POINT('Ctrl Pts',(6.9896738586244,0.632125633165928,1.2550483625575));
#160725=CARTESIAN_POINT('Ctrl Pts',(7.01094414743398,0.319844675254871,
1.24075700282355));
#160726=CARTESIAN_POINT('Ctrl Pts',(7.01124672537693,0.00677631103669551,
1.22646564308963));
#160727=CARTESIAN_POINT('',(-5.31037376991255,4.57794244025903,0.));
#160728=CARTESIAN_POINT('Ctrl Pts',(7.01124672537777,0.00677631016984748,
1.22646564305006));
#160729=CARTESIAN_POINT('Ctrl Pts',(7.01141682993229,-0.169225816498521,
1.21843126464065));
#160730=CARTESIAN_POINT('Ctrl Pts',(7.00495567967284,-0.345511762794221,
1.21039688623124));
#160731=CARTESIAN_POINT('Ctrl Pts',(6.99182592907262,-0.52153306707037,
1.20236250782184));
#160732=CARTESIAN_POINT('Ctrl Pts',(6.97871089679715,-0.697357053149192,
1.19433713587373));
#160733=CARTESIAN_POINT('Ctrl Pts',(6.95894217120697,-0.87291662569608,
1.18631176392561));
#160734=CARTESIAN_POINT('Ctrl Pts',(6.93253436434061,-1.0476611330657,1.17828639197751));
#160735=CARTESIAN_POINT('Ctrl Pts',(6.90615057214422,-1.22224673168184,
1.17026831812347));
#160736=CARTESIAN_POINT('Ctrl Pts',(6.87313977264274,-1.39601838056077,
1.16225024426945));
#160737=CARTESIAN_POINT('Ctrl Pts',(6.8335685390142,-1.5684283806076,1.15423217041541));
#160738=CARTESIAN_POINT('Ctrl Pts',(6.7919833913311,-1.74961290928045,1.14580602963638));
#160739=CARTESIAN_POINT('Ctrl Pts',(6.74315260201287,-1.92929316192643,
1.13737988885733));
#160740=CARTESIAN_POINT('Ctrl Pts',(6.68721496429928,-2.1068418506741,1.1289537480783));
#160741=CARTESIAN_POINT('Ctrl Pts',(6.63404803922703,-2.27559616739471,
1.12094497234592));
#160742=CARTESIAN_POINT('Ctrl Pts',(6.57446140310177,-2.44242457829185,
1.11293619661355));
#160743=CARTESIAN_POINT('Ctrl Pts',(6.50862608358455,-2.60680130937954,
1.10492742088118));
#160744=CARTESIAN_POINT('Ctrl Pts',(6.44280441263479,-2.77114396290947,
1.09692030547819));
#160745=CARTESIAN_POINT('Ctrl Pts',(6.37073677303487,-2.93303560808939,
1.08891319007519));
#160746=CARTESIAN_POINT('Ctrl Pts',(6.29264303487681,-3.09196866059738,
1.0809060746722));
#160747=CARTESIAN_POINT('Ctrl Pts',(6.21455054475987,-3.25089917314522,
1.07289908723349));
#160748=CARTESIAN_POINT('Ctrl Pts',(6.1304323099791,-3.40687085824795,1.06489209979479));
#160749=CARTESIAN_POINT('Ctrl Pts',(6.04055500235253,-3.55939908215612,
1.05688511235608));
#160750=CARTESIAN_POINT('Ctrl Pts',(5.95066193371926,-3.71195405362074,
1.04887672080119));
#160751=CARTESIAN_POINT('Ctrl Pts',(5.8550079687018,-3.86106404641347,1.0408683292463));
#160752=CARTESIAN_POINT('Ctrl Pts',(5.75390406474699,-4.00627190492458,
1.03285993769141));
#160753=CARTESIAN_POINT('Ctrl Pts',(5.65272073837281,-4.1515938318246,1.02484525512491));
#160754=CARTESIAN_POINT('Ctrl Pts',(5.54607913401669,-4.29300720248875,
1.01683057255842));
#160755=CARTESIAN_POINT('Ctrl Pts',(5.43433198097541,-4.43008605819886,
1.00881588999193));
#160756=CARTESIAN_POINT('Ctrl Pts',(5.32253372883842,-4.56722759654004,
1.00079754251747));
#160757=CARTESIAN_POINT('Ctrl Pts',(5.20562551800962,-4.70003039580051,
0.992779195042993));
#160758=CARTESIAN_POINT('Ctrl Pts',(5.0839979594269,-4.82810431857506,0.984760847568531));
#160759=CARTESIAN_POINT('Ctrl Pts',(4.96223719035818,-4.95631851210481,
0.976733718137279));
#160760=CARTESIAN_POINT('Ctrl Pts',(4.83574701523879,-5.07979323295038,
0.96870658870603));
#160761=CARTESIAN_POINT('Ctrl Pts',(4.70495270924007,-5.19817723498483,
0.960679459274779));
#160762=CARTESIAN_POINT('Ctrl Pts',(4.6578376048721,-5.24082186365395,0.957787903422705));
#160763=CARTESIAN_POINT('Ctrl Pts',(4.61016428687613,-5.28280631233251,
0.954896347570646));
#160764=CARTESIAN_POINT('Ctrl Pts',(4.56195357994032,-5.32411552250416,
0.952004791718572));
#160765=CARTESIAN_POINT('Ctrl Pts',(4.42499058165173,-5.44147188671545,
0.943790098668195));
#160766=CARTESIAN_POINT('Ctrl Pts',(4.28336273305126,-5.55365432817702,
0.935575405617811));
#160767=CARTESIAN_POINT('Ctrl Pts',(4.13749531642573,-5.66027906282501,
0.927360712567442));
#160768=CARTESIAN_POINT('Ctrl Pts',(3.99174322317756,-5.76681949952082,
0.919152514087063));
#160769=CARTESIAN_POINT('Ctrl Pts',(3.84175851848875,-5.86781077799396,
0.910944315606697));
#160770=CARTESIAN_POINT('Ctrl Pts',(3.688000133595,-5.96290881844619,0.902736117126317));
#160771=CARTESIAN_POINT('Ctrl Pts',(3.53433743432414,-6.05794767828694,
0.894533026702872));
#160772=CARTESIAN_POINT('Ctrl Pts',(3.37690602898616,-6.14710042473106,
0.886329936279438));
#160773=CARTESIAN_POINT('Ctrl Pts',(3.21619461364133,-6.23006571150614,
0.878126845855995));
#160774=CARTESIAN_POINT('Ctrl Pts',(3.05555571771255,-6.31299356102677,
0.869927456994921));
#160775=CARTESIAN_POINT('Ctrl Pts',(2.89164007017492,-6.38973935584501,
0.861728068133851));
#160776=CARTESIAN_POINT('Ctrl Pts',(2.72496197649438,-6.46004711973217,
0.853528679272777));
#160777=CARTESIAN_POINT('Ctrl Pts',(2.55832821219312,-6.53033618470417,
0.845331471105103));
#160778=CARTESIAN_POINT('Ctrl Pts',(2.38893378670014,-6.59419049688694,
0.83713426293742));
#160779=CARTESIAN_POINT('Ctrl Pts',(2.21731424712931,-6.65140166370799,
0.828937054769746));
#160780=CARTESIAN_POINT('Ctrl Pts',(2.04569290397268,-6.70861343177321,
0.820739760455888));
#160781=CARTESIAN_POINT('Ctrl Pts',(1.87184672901308,-6.75918180167349,
0.81254246614204));
#160782=CARTESIAN_POINT('Ctrl Pts',(1.69632810358554,-6.80294770871318,
0.804345171828182));
#160783=CARTESIAN_POINT('Ctrl Pts',(1.61776226552343,-6.8225382516356,0.800675890029505));
#160784=CARTESIAN_POINT('Ctrl Pts',(1.53886152203894,-6.84076649049403,
0.797006608230821));
#160785=CARTESIAN_POINT('Ctrl Pts',(1.45967623572252,-6.85762144255331,
0.793337326432145));
#160786=CARTESIAN_POINT('Ctrl Pts',(1.2603658835866,-6.9000455668628,0.784101698433557));
#160787=CARTESIAN_POINT('Ctrl Pts',(1.05939543448741,-6.93373583637711,
0.774866070434961));
#160788=CARTESIAN_POINT('Ctrl Pts',(0.857490139534536,-6.95861604222428,
0.765630442436375));
#160789=CARTESIAN_POINT('Ctrl Pts',(0.655095352696672,-6.98355656674144,
0.756372423915742));
#160790=CARTESIAN_POINT('Ctrl Pts',(0.451761352159633,-6.99964427887868,
0.747114405395103));
#160791=CARTESIAN_POINT('Ctrl Pts',(0.248218246281154,-7.00685480545395,
0.737856386874469));
#160792=CARTESIAN_POINT('Ctrl Pts',(0.0441803191657221,-7.01408286110083,
0.728575861749368));
#160793=CARTESIAN_POINT('Ctrl Pts',(-0.160067563697973,-7.01239053413776,
0.719295336624267));
#160794=CARTESIAN_POINT('Ctrl Pts',(-0.363792928561735,-7.00180557196703,
0.710014811499164));
#160795=CARTESIAN_POINT('Ctrl Pts',(-0.567660667977806,-6.99121321243931,
0.70072780062983));
#160796=CARTESIAN_POINT('Ctrl Pts',(-0.771004994509795,-6.97171581173367,
0.691440789760502));
#160797=CARTESIAN_POINT('Ctrl Pts',(-0.973097359689014,-6.9433931251994,
0.68215377889117));
#160798=CARTESIAN_POINT('Ctrl Pts',(-1.17520208409502,-6.91506870655365,
0.672866200062363));
#160799=CARTESIAN_POINT('Ctrl Pts',(-1.37605453130155,-6.87791795119954,
0.663578621233559));
#160800=CARTESIAN_POINT('Ctrl Pts',(-1.57493393023453,-6.83207213646753,
0.654291042404751));
#160801=CARTESIAN_POINT('Ctrl Pts',(-1.71498653192544,-6.79978711517168,
0.647750648651738));
#160802=CARTESIAN_POINT('Ctrl Pts',(-1.85406084050494,-6.76319120099541,
0.641210254898729));
#160803=CARTESIAN_POINT('Ctrl Pts',(-1.9919081624325,-6.72234545638163,
0.634669861145717));
#160804=CARTESIAN_POINT('Ctrl Pts',(-2.16187146483775,-6.67198337791189,
0.62660567168053));
#160805=CARTESIAN_POINT('Ctrl Pts',(-2.33009322388277,-6.61512101676497,
0.618541482215349));
#160806=CARTESIAN_POINT('Ctrl Pts',(-2.49603703497435,-6.55190244757479,
0.610477292750161));
#160807=CARTESIAN_POINT('Ctrl Pts',(-2.66187495730633,-6.48872421815883,
0.602418249044939));
#160808=CARTESIAN_POINT('Ctrl Pts',(-2.82543748714466,-6.41919798424768,
0.594359205339728));
#160809=CARTESIAN_POINT('Ctrl Pts',(-2.98620339036206,-6.34351762619843,
0.586300161634504));
#160810=CARTESIAN_POINT('Ctrl Pts',(-3.14689695606165,-6.2678713209498,
0.578244744141095));
#160811=CARTESIAN_POINT('Ctrl Pts',(-3.30479607282164,-6.18607656046966,
0.570189326647669));
#160812=CARTESIAN_POINT('Ctrl Pts',(-3.45939951677418,-6.09837532018509,
0.562133909154262));
#160813=CARTESIAN_POINT('Ctrl Pts',(-3.61398280253898,-6.01068551495023,
0.554079541977809));
#160814=CARTESIAN_POINT('Ctrl Pts',(-3.76527095204614,-5.91709093718653,
0.546025174801362));
#160815=CARTESIAN_POINT('Ctrl Pts',(-3.9127872078451,-5.81787958182565,
0.537970807624909));
#160816=CARTESIAN_POINT('Ctrl Pts',(-4.0602908570555,-5.71867670496585,
0.529917128766447));
#160817=CARTESIAN_POINT('Ctrl Pts',(-4.20402295515093,-5.61385821280352,
0.521863449907972));
#160818=CARTESIAN_POINT('Ctrl Pts',(-4.34353582518329,-5.50375536319061,
0.513809771049509));
#160819=CARTESIAN_POINT('Ctrl Pts',(-4.48309818947319,-5.3936134529606,
0.505753235029154));
#160820=CARTESIAN_POINT('Ctrl Pts',(-4.61843805165705,-5.27818366768537,
0.497696699008806));
#160821=CARTESIAN_POINT('Ctrl Pts',(-4.74914061076898,-5.15783772734708,
0.489640162988451));
#160822=CARTESIAN_POINT('Ctrl Pts',(-4.82288988547179,-5.08993220297417,
0.485094240612061));
#160823=CARTESIAN_POINT('Ctrl Pts',(-4.89516335785953,-5.02046217445374,
0.480548318235672));
#160824=CARTESIAN_POINT('Ctrl Pts',(-4.96589168557297,-4.94949960396577,
0.476002395859283));
#160825=CARTESIAN_POINT('Ctrl Pts',(-5.10456501020033,-4.81036701180917,
0.467089444149383));
#160826=CARTESIAN_POINT('Ctrl Pts',(-5.23733419343256,-4.66545741061707,
0.458176492439488));
#160827=CARTESIAN_POINT('Ctrl Pts',(-5.36375573086079,-4.51527972800779,
0.449263540729589));
#160828=CARTESIAN_POINT('Ctrl Pts',(-5.49025725910387,-4.36500702333621,
0.440344949519613));
#160829=CARTESIAN_POINT('Ctrl Pts',(-5.61040296415482,-4.20945976339479,
0.431426358309636));
#160830=CARTESIAN_POINT('Ctrl Pts',(-5.72378996120478,-4.04917955177483,
0.42250776709966));
#160831=CARTESIAN_POINT('Ctrl Pts',(-5.83725514330947,-3.88878882027654,
0.413583026149766));
#160832=CARTESIAN_POINT('Ctrl Pts',(-5.94395216188509,-3.72365880956333,
0.40465828519986));
#160833=CARTESIAN_POINT('Ctrl Pts',(-6.04352085891127,-3.55436101014013,
0.395733544249964));
#160834=CARTESIAN_POINT('Ctrl Pts',(-6.14310049497154,-3.3850446109516,
0.386807822790647));
#160835=CARTESIAN_POINT('Ctrl Pts',(-6.23555012739648,-3.21155971820321,
0.377882101331347));
#160836=CARTESIAN_POINT('Ctrl Pts',(-6.32055488330501,-3.0345036710522,
0.368956379872031));
#160837=CARTESIAN_POINT('Ctrl Pts',(-6.40555790762161,-2.85745123062667,
0.360030840234392));
#160838=CARTESIAN_POINT('Ctrl Pts',(-6.48311625587417,-2.67682799855142,
0.35110530059676));
#160839=CARTESIAN_POINT('Ctrl Pts',(-6.55296211181921,-2.49325372225973,
0.34217976095912));
#160840=CARTESIAN_POINT('Ctrl Pts',(-6.61776896625368,-2.32292333915279,
0.333898150830369));
#160841=CARTESIAN_POINT('Ctrl Pts',(-6.67593642861803,-2.15005271925837,
0.325616540701606));
#160842=CARTESIAN_POINT('Ctrl Pts',(-6.72728788244206,-1.97515171803289,
0.317334930572855));
#160843=CARTESIAN_POINT('Ctrl Pts',(-6.77907180886242,-1.79877773241324,
0.308983574231145));
#160844=CARTESIAN_POINT('Ctrl Pts',(-6.82393755001756,-1.62029056482357,
0.300632217889427));
#160845=CARTESIAN_POINT('Ctrl Pts',(-6.86172539517146,-1.4402607971333,
0.292280861547717));
#160846=CARTESIAN_POINT('Ctrl Pts',(-6.89949937822051,-1.2602970716189,
0.283932568820159));
#160847=CARTESIAN_POINT('Ctrl Pts',(-6.93020057416922,-1.07879219770202,
0.275584276092606));
#160848=CARTESIAN_POINT('Ctrl Pts',(-6.95371995337483,-0.896328830584341,
0.267235983365048));
#160849=CARTESIAN_POINT('Ctrl Pts',(-6.97723395162932,-0.713907208890815,
0.258889600626471));
#160850=CARTESIAN_POINT('Ctrl Pts',(-6.99356936789201,-0.530527859304366,
0.250543217887913));
#160851=CARTESIAN_POINT('Ctrl Pts',(-7.00266874717422,-0.346780881608981,
0.242196835149336));
#160852=CARTESIAN_POINT('Ctrl Pts',(-7.01176860716355,-0.163024196824893,
0.233850011483357));
#160853=CARTESIAN_POINT('Ctrl Pts',(-7.01363164572049,0.0210998245950316,
0.225503187817363));
#160854=CARTESIAN_POINT('Ctrl Pts',(-7.00825244637512,0.20499807408169,
0.217156364151386));
#160855=CARTESIAN_POINT('Ctrl Pts',(-7.00287315096108,0.38889960785984,
0.208809391417094));
#160856=CARTESIAN_POINT('Ctrl Pts',(-6.99025137322777,0.572575031013105,
0.200462418682822));
#160857=CARTESIAN_POINT('Ctrl Pts',(-6.97043378629731,0.755433248768528,
0.192115445948531));
#160858=CARTESIAN_POINT('Ctrl Pts',(-6.95060935228489,0.938354645013201,
0.183765589290653));
#160859=CARTESIAN_POINT('Ctrl Pts',(-6.92358418101607,1.12045794309435,
0.175415732632769));
#160860=CARTESIAN_POINT('Ctrl Pts',(-6.88945667745427,1.30115842693376,
0.167065875974892));
#160861=CARTESIAN_POINT('Ctrl Pts',(-6.87801469298165,1.3617421765345,0.164266405745402));
#160862=CARTESIAN_POINT('Ctrl Pts',(-6.86577478234028,1.42216831972826,
0.16146693551591));
#160863=CARTESIAN_POINT('Ctrl Pts',(-6.85274193659805,1.48241509466492,
0.15866746528642));
#160864=CARTESIAN_POINT('Ctrl Pts',(-6.81252228002286,1.66833800403104,
0.150028236874645));
#160865=CARTESIAN_POINT('Ctrl Pts',(-6.76472908610749,1.85263628174639,
0.141389008462876));
#160866=CARTESIAN_POINT('Ctrl Pts',(-6.7095182968688,2.03469673083801,0.1327497800511));
#160867=CARTESIAN_POINT('Ctrl Pts',(-6.65431427480331,2.21673486482398,
0.12411161054748));
#160868=CARTESIAN_POINT('Ctrl Pts',(-6.59169455695899,2.39653544070573,
0.115473441043872));
#160869=CARTESIAN_POINT('Ctrl Pts',(-6.52186501817855,2.57350019373594,
0.106835271540255));
#160870=CARTESIAN_POINT('Ctrl Pts',(-6.44989512403592,2.75588911918205,
0.0979323322452363));
#160871=CARTESIAN_POINT('Ctrl Pts',(-6.37026650450594,2.93526531039644,
0.0890293929502093));
#160872=CARTESIAN_POINT('Ctrl Pts',(-6.28325856614943,3.11099475303475,
0.0801264536551898));
#160873=CARTESIAN_POINT('Ctrl Pts',(-6.19884731143077,3.28147968836712,
0.0714892155965488));
#160874=CARTESIAN_POINT('Ctrl Pts',(-6.1074910014181,3.44853214205245,0.0628519775378872));
#160875=CARTESIAN_POINT('Ctrl Pts',(-6.00949230903563,3.6115964268093,0.0542147394792423));
#160876=CARTESIAN_POINT('Ctrl Pts',(-5.90697162011571,3.78218505819899,
0.0451789495660293));
#160877=CARTESIAN_POINT('Ctrl Pts',(-5.79718119022459,3.94840845108158,
0.0361431596528352));
#160878=CARTESIAN_POINT('Ctrl Pts',(-5.68051992566802,4.10966177885585,
0.0271073697396247));
#160879=CARTESIAN_POINT('Ctrl Pts',(-5.56385866111145,4.27091510663012,
0.0180715798264141));
#160880=CARTESIAN_POINT('Ctrl Pts',(-5.44032677458003,4.42719807500911,
0.00903578991321001));
#160881=CARTESIAN_POINT('Ctrl Pts',(-5.31037376991255,4.57794244025903,
0.));
#160882=CARTESIAN_POINT('',(5.30919883249355,4.57930500398795,2.57697863048634E-7));
#160883=CARTESIAN_POINT('Origin',(0.,0.,0.));
#160884=CARTESIAN_POINT('',(7.01124999980813,-5.18702183968693E-5,1.77353435693496));
#160885=CARTESIAN_POINT('Ctrl Pts',(5.30919883249355,4.57930500398795,2.57697855943206E-7));
#160886=CARTESIAN_POINT('Ctrl Pts',(5.17711001830684,4.73244740822939,0.00920421453633651));
#160887=CARTESIAN_POINT('Ctrl Pts',(5.03841024185807,4.87985060242885,0.0184081713748201));
#160888=CARTESIAN_POINT('Ctrl Pts',(4.89359335575129,5.02099299253115,0.0276121282132991));
#160889=CARTESIAN_POINT('Ctrl Pts',(4.74881129473298,5.16210144117568,0.0368138717145086));
#160890=CARTESIAN_POINT('Ctrl Pts',(4.59791519661176,5.29695196575731,0.0460156152156967));
#160891=CARTESIAN_POINT('Ctrl Pts',(4.44143525766802,5.42506031435996,0.0552173587169094));
#160892=CARTESIAN_POINT('Ctrl Pts',(4.28516511765998,5.55299690295701,0.0644067650712253));
#160893=CARTESIAN_POINT('Ctrl Pts',(4.12332623735365,5.67420925882696,0.0735961714255482));
#160894=CARTESIAN_POINT('Ctrl Pts',(3.95648126927498,5.78825384104535,0.082785577779859));
#160895=CARTESIAN_POINT('Ctrl Pts',(3.78985279998986,5.90215043849234,0.0919630599184624));
#160896=CARTESIAN_POINT('Ctrl Pts',(3.61823136491426,6.00889772774248,0.101140542057079));
#160897=CARTESIAN_POINT('Ctrl Pts',(3.44220988242581,6.10809443998946,0.110318024195685));
#160898=CARTESIAN_POINT('Ctrl Pts',(3.26664748986962,6.20703243261163,0.119471570110178));
#160899=CARTESIAN_POINT('Ctrl Pts',(3.08670811918591,6.29845906723639,0.128625116024664));
#160900=CARTESIAN_POINT('Ctrl Pts',(2.90301021948285,6.38201835065351,0.137778661939159));
#160901=CARTESIAN_POINT('Ctrl Pts',(2.82012422289691,6.41972098357,0.141908816811068));
#160902=CARTESIAN_POINT('Ctrl Pts',(2.73647342649563,6.45582249259887,0.146038971682991));
#160903=CARTESIAN_POINT('Ctrl Pts',(2.65211653575299,6.49029309378903,0.1501691265549));
#160904=CARTESIAN_POINT('Ctrl Pts',(2.48468518033815,6.55871026076169,0.158366648087392));
#160905=CARTESIAN_POINT('Ctrl Pts',(2.31456968522649,6.62065883490012,0.166564169619877));
#160906=CARTESIAN_POINT('Ctrl Pts',(2.14230841566705,6.67593747833682,0.174761691152369));
#160907=CARTESIAN_POINT('Ctrl Pts',(1.97005289242181,6.73121427778122,0.182958939230855));
#160908=CARTESIAN_POINT('Ctrl Pts',(1.79565206881785,6.77982148391414,0.19115618730935));
#160909=CARTESIAN_POINT('Ctrl Pts',(1.6196603517921,6.82160735511307,0.199353435387835));
#160910=CARTESIAN_POINT('Ctrl Pts',(1.44364490628013,6.86339886018776,0.20755178867906));
#160911=CARTESIAN_POINT('Ctrl Pts',(1.26603847869501,6.89836711822185,0.215750141970292));
#160912=CARTESIAN_POINT('Ctrl Pts',(1.08740676178002,6.9264112711371,0.223948495261517));
#160913=CARTESIAN_POINT('Ctrl Pts',(0.90865370707236,6.95447447338845,0.232152417385136));
#160914=CARTESIAN_POINT('Ctrl Pts',(0.728874315852634,6.97560412070426,
0.240356339508754));
#160915=CARTESIAN_POINT('Ctrl Pts',(0.548641355408434,6.98975101313599,
0.248560261632377));
#160916=CARTESIAN_POINT('Ctrl Pts',(0.368339379111189,7.00390332277801,
0.256767325249556));
#160917=CARTESIAN_POINT('Ctrl Pts',(0.187583834733879,7.01106752899879,
0.264974388866734));
#160918=CARTESIAN_POINT('Ctrl Pts',(0.00694885283989022,7.01124655649366,
0.273181452483911));
#160919=CARTESIAN_POINT('Ctrl Pts',(-0.173861858901962,7.01142575815454,
0.281396500302297));
#160920=CARTESIAN_POINT('Ctrl Pts',(-0.354551426171415,7.00460621641048,
0.289611548120658));
#160921=CARTESIAN_POINT('Ctrl Pts',(-0.534548563057438,6.99084289597708,
0.297826595939043));
#160922=CARTESIAN_POINT('Ctrl Pts',(-0.614960663037309,6.98469425651597,
0.30149659457313));
#160923=CARTESIAN_POINT('Ctrl Pts',(-0.695234661285935,6.97716048410052,
0.305166593207232));
#160924=CARTESIAN_POINT('Ctrl Pts',(-0.775320191888788,6.96824979191687,
0.30883659184132));
#160925=CARTESIAN_POINT('Ctrl Pts',(-0.953332438724452,6.94844331346151,
0.31699417908361));
#160926=CARTESIAN_POINT('Ctrl Pts',(-1.13078883931233,6.92178858772017,
0.325151766325908));
#160927=CARTESIAN_POINT('Ctrl Pts',(-1.30712494444465,6.88832715121099,
0.333309353568197));
#160928=CARTESIAN_POINT('Ctrl Pts',(-1.48330105598897,6.85489607499181,
0.341459539253945));
#160929=CARTESIAN_POINT('Ctrl Pts',(-1.6583585512607,6.81467065416905,0.349609724939691));
#160930=CARTESIAN_POINT('Ctrl Pts',(-1.83173834330004,6.7677441739611,0.35775991062544));
#160931=CARTESIAN_POINT('Ctrl Pts',(-2.00499456597701,6.72085113868448,
0.365904287599363));
#160932=CARTESIAN_POINT('Ctrl Pts',(-2.17657512720709,6.66726664954513,
0.374048664573273));
#160933=CARTESIAN_POINT('Ctrl Pts',(-2.34593121972405,6.60713502774266,
0.382193041547197));
#160934=CARTESIAN_POINT('Ctrl Pts',(-2.51519956181275,6.54703456263192,
0.390333198581012));
#160935=CARTESIAN_POINT('Ctrl Pts',(-2.68224539890916,6.48039384135878,
0.398473355614832));
#160936=CARTESIAN_POINT('Ctrl Pts',(-2.8465350287286,6.4074070334825,0.406613512648647));
#160937=CARTESIAN_POINT('Ctrl Pts',(-3.01077149323455,6.3344438446656,0.41475103546872));
#160938=CARTESIAN_POINT('Ctrl Pts',(-3.17225320489948,6.25513880485553,
0.422888558288796));
#160939=CARTESIAN_POINT('Ctrl Pts',(-3.33046625360608,6.16973428083342,
0.431026081108868));
#160940=CARTESIAN_POINT('Ctrl Pts',(-3.48869526370463,6.08432114073891,
0.439164424886455));
#160941=CARTESIAN_POINT('Ctrl Pts',(-3.64365463637829,5.99280744701559,
0.447302768664046));
#160942=CARTESIAN_POINT('Ctrl Pts',(-3.79485442334125,5.89548186903729,
0.455441112441633));
#160943=CARTESIAN_POINT('Ctrl Pts',(-3.94606937134013,5.79814653207312,
0.463580272263508));
#160944=CARTESIAN_POINT('Ctrl Pts',(-4.09352368425078,5.69499834042374,
0.471719432085371));
#160945=CARTESIAN_POINT('Ctrl Pts',(-4.236755969054,5.58636961014802,0.479858591907245));
#160946=CARTESIAN_POINT('Ctrl Pts',(-4.38002786946516,5.47771083501756,
0.488000002881957));
#160947=CARTESIAN_POINT('Ctrl Pts',(-4.5190751328444,5.36356871457753,0.496141413856687));
#160948=CARTESIAN_POINT('Ctrl Pts',(-4.65346897011614,5.24431626684225,
0.5042828248314));
#160949=CARTESIAN_POINT('Ctrl Pts',(-4.78792367425065,5.12500980976756,
0.512427923044713));
#160950=CARTESIAN_POINT('Ctrl Pts',(-4.9177204885028,5.00058864848786,0.520573021258008));
#160951=CARTESIAN_POINT('Ctrl Pts',(-5.04246696641261,4.87146317394863,
0.528718119471321));
#160952=CARTESIAN_POINT('Ctrl Pts',(-5.16737490010896,4.74217057601317,
0.536873759651514));
#160953=CARTESIAN_POINT('Ctrl Pts',(-5.287219191426,4.60816175451188,0.545029399831718));
#160954=CARTESIAN_POINT('Ctrl Pts',(-5.40164643869375,4.46988168902121,
0.553185040011911));
#160955=CARTESIAN_POINT('Ctrl Pts',(-5.516149875366,4.33150955213938,0.561346110484132));
#160956=CARTESIAN_POINT('Ctrl Pts',(-5.62522886350364,4.18886078260095,
0.569507180956342));
#160957=CARTESIAN_POINT('Ctrl Pts',(-5.72857299043574,4.04240993168062,
0.577668251428562));
#160958=CARTESIAN_POINT('Ctrl Pts',(-5.83209280458033,3.89571011120075,
0.585843195894058));
#160959=CARTESIAN_POINT('Ctrl Pts',(-5.92985807979805,3.74519558773208,
0.594018140359565));
#160960=CARTESIAN_POINT('Ctrl Pts',(-6.02160329609183,3.59136747033718,
0.602193084825061));
#160961=CARTESIAN_POINT('Ctrl Pts',(-6.11130449436035,3.44096653375286,
0.610185897354768));
#160962=CARTESIAN_POINT('Ctrl Pts',(-6.19525095685086,3.28739838638717,
0.618178709884468));
#160963=CARTESIAN_POINT('Ctrl Pts',(-6.27323931727954,3.13114915496502,
0.626171522414175));
#160964=CARTESIAN_POINT('Ctrl Pts',(-6.35305293962011,2.97124302180383,
0.634351401016297));
#160965=CARTESIAN_POINT('Ctrl Pts',(-6.42687058601084,2.80803900398711,
0.642531279618431));
#160966=CARTESIAN_POINT('Ctrl Pts',(-6.4944077485214,2.64202470814435,0.650711158220552));
#160967=CARTESIAN_POINT('Ctrl Pts',(-6.56185810388352,2.4762237944913,0.658880523026866));
#160968=CARTESIAN_POINT('Ctrl Pts',(-6.62304391942665,2.30762011976076,
0.667049887833166));
#160969=CARTESIAN_POINT('Ctrl Pts',(-6.67772617467052,2.13672639769818,
0.675219252639479));
#160970=CARTESIAN_POINT('Ctrl Pts',(-6.73234876599132,1.96601913813318,
0.683379703834765));
#160971=CARTESIAN_POINT('Ctrl Pts',(-6.78048182329104,1.79302714164442,
0.691540155030056));
#160972=CARTESIAN_POINT('Ctrl Pts',(-6.8219340456616,1.61828379437696,0.699700606225342));
#160973=CARTESIAN_POINT('Ctrl Pts',(-6.8633490868576,1.44369718569983,0.707853737785077));
#160974=CARTESIAN_POINT('Ctrl Pts',(-6.89809514877191,1.26736269732015,
0.716006869344827));
#160975=CARTESIAN_POINT('Ctrl Pts',(-6.92603044060034,1.08982975660305,
0.724160000904561));
#160976=CARTESIAN_POINT('Ctrl Pts',(-6.9539460969969,0.912421601980324,
0.73230740171123));
#160977=CARTESIAN_POINT('Ctrl Pts',(-6.975060465986,0.733817021089351,0.74045480251789));
#160978=CARTESIAN_POINT('Ctrl Pts',(-6.98928259890422,0.554576699072976,
0.748602203324559));
#160979=CARTESIAN_POINT('Ctrl Pts',(-7.00349787038227,0.375422851198931,
0.756745673433665));
#160980=CARTESIAN_POINT('Ctrl Pts',(-7.01082750234475,0.195634224786323,
0.764889143542771));
#160981=CARTESIAN_POINT('Ctrl Pts',(-7.01123224688893,0.0157779176322022,
0.773032613651878));
#160982=CARTESIAN_POINT('Ctrl Pts',(-7.01163688829273,-0.164032557039414,
0.781174008574092));
#160983=CARTESIAN_POINT('Ctrl Pts',(-7.00512015578681,-0.343910325027825,
0.789315403496302));
#160984=CARTESIAN_POINT('Ctrl Pts',(-6.99169489609768,-0.523286768781423,
0.797456798418516));
#160985=CARTESIAN_POINT('Ctrl Pts',(-6.97827069719901,-0.702649039191136,
0.805597550052304));
#160986=CARTESIAN_POINT('Ctrl Pts',(-6.95793908487309,-0.881509711923539,
0.813738301686094));
#160987=CARTESIAN_POINT('Ctrl Pts',(-6.93076491788837,-1.05930364649039,
0.821879053319883));
#160988=CARTESIAN_POINT('Ctrl Pts',(-6.90358812056928,-1.23711479069232,
0.830020592940985));
#160989=CARTESIAN_POINT('Ctrl Pts',(-6.86956750309537,-1.41385864180084,
0.838162132562087));
#160990=CARTESIAN_POINT('Ctrl Pts',(-6.82881936249476,-1.588978501087,0.84630367218319));
#160991=CARTESIAN_POINT('Ctrl Pts',(-6.78804138159968,-1.76422660249885,
0.854451173939893));
#160992=CARTESIAN_POINT('Ctrl Pts',(-6.74052611273859,-1.93784799086778,
0.862598675696589));
#160993=CARTESIAN_POINT('Ctrl Pts',(-6.68644047313306,-2.1092985473252,
0.870746177453292));
#160994=CARTESIAN_POINT('Ctrl Pts',(-6.6323353760226,-2.28081078374184,
0.878896610303287));
#160995=CARTESIAN_POINT('Ctrl Pts',(-6.57165531205661,-2.45015029749233,
0.88704704315328));
#160996=CARTESIAN_POINT('Ctrl Pts',(-6.50461607235799,-2.61679122471055,
0.895197476003275));
#160997=CARTESIAN_POINT('Ctrl Pts',(-6.43749721470135,-2.78363006005553,
0.90335758856956));
#160998=CARTESIAN_POINT('Ctrl Pts',(-6.36400422904425,-2.94776357937369,
0.911517701135838));
#160999=CARTESIAN_POINT('Ctrl Pts',(-6.28440028099749,-3.10868777311243,
0.919677813702123));
#161000=CARTESIAN_POINT('Ctrl Pts',(-6.20691549353275,-3.2653279556126,
0.927620693463757));
#161001=CARTESIAN_POINT('Ctrl Pts',(-6.12364114321043,-3.41892726396892,
0.935563573225403));
#161002=CARTESIAN_POINT('Ctrl Pts',(-6.0348598328842,-3.56904656175019,
0.943506452987037));
#161003=CARTESIAN_POINT('Ctrl Pts',(-5.94312944520624,-3.72415242054883,
0.951713173941446));
#161004=CARTESIAN_POINT('Ctrl Pts',(-5.84532617622802,-3.87587088288704,
0.959919894895858));
#161005=CARTESIAN_POINT('Ctrl Pts',(-5.74172845038914,-4.02370239511969,
0.968126615850267));
#161006=CARTESIAN_POINT('Ctrl Pts',(-5.63821157389144,-4.17141853724869,
0.976326932146879));
#161007=CARTESIAN_POINT('Ctrl Pts',(-5.52890944776105,-4.31525348751679,
0.984527248443485));
#161008=CARTESIAN_POINT('Ctrl Pts',(-5.4141451452014,-4.45473443756102,
0.9927275647401));
#161009=CARTESIAN_POINT('Ctrl Pts',(-5.2994509438435,-4.59413018879342,
1.00092287205732));
#161010=CARTESIAN_POINT('Ctrl Pts',(-5.17930143457965,-4.72917697002963,
1.00911817937454));
#161011=CARTESIAN_POINT('Ctrl Pts',(-5.05406163145324,-4.85943284632808,
1.01731348669176));
#161012=CARTESIAN_POINT('Ctrl Pts',(-4.92887574014346,-4.98963265154735,
1.0255052661856));
#161013=CARTESIAN_POINT('Ctrl Pts',(-4.79860416296257,-5.11504541049285,
1.03369704567944));
#161014=CARTESIAN_POINT('Ctrl Pts',(-4.66365077157032,-5.23526389433537,
1.04188882517328));
#161015=CARTESIAN_POINT('Ctrl Pts',(-4.52873164262145,-5.35545185668486,
1.05007852490923));
#161016=CARTESIAN_POINT('Ctrl Pts',(-4.38913332933796,-5.47044794098969,
1.05826822464517));
#161017=CARTESIAN_POINT('Ctrl Pts',(-4.24529511770079,-5.57988314627877,
1.06645792438111));
#161018=CARTESIAN_POINT('Ctrl Pts',(-4.10145226326054,-5.6893218839123,
1.0746478884638));
#161019=CARTESIAN_POINT('Ctrl Pts',(-3.95336951282026,-5.79319917026139,
1.0828378525465));
#161020=CARTESIAN_POINT('Ctrl Pts',(-3.8015179559582,-5.89118729909578,
1.09102781662919));
#161021=CARTESIAN_POINT('Ctrl Pts',(-3.73263068243912,-5.93563949420083,
1.09474318384395));
#161022=CARTESIAN_POINT('Ctrl Pts',(-3.66296820625712,-5.97888029959006,
1.09845855105871));
#161023=CARTESIAN_POINT('Ctrl Pts',(-3.59257642105979,-6.02088209661551,
1.10217391827347));
#161024=CARTESIAN_POINT('Ctrl Pts',(-3.41746583716016,-6.12536814113538,
1.11141647577581));
#161025=CARTESIAN_POINT('Ctrl Pts',(-3.23796122535349,-6.22211184220953,
1.12065903327815));
#161026=CARTESIAN_POINT('Ctrl Pts',(-3.05472541606613,-6.3108065407632,
1.12990159078048));
#161027=CARTESIAN_POINT('Ctrl Pts',(-2.87104650153154,-6.39971572297312,
1.13916649885798));
#161028=CARTESIAN_POINT('Ctrl Pts',(-2.68361848851216,-6.48053689192567,
1.14843140693547));
#161029=CARTESIAN_POINT('Ctrl Pts',(-2.49312555262666,-6.5530108760279,
1.15769631501296));
#161030=CARTESIAN_POINT('Ctrl Pts',(-2.30217615922385,-6.62565852166094,
1.16698342358267));
#161031=CARTESIAN_POINT('Ctrl Pts',(-2.10814729959598,-6.68991889389765,
1.17627053215238));
#161032=CARTESIAN_POINT('Ctrl Pts',(-1.91174218981668,-6.74558139541544,
1.18555764072208));
#161033=CARTESIAN_POINT('Ctrl Pts',(-1.71520558877797,-6.80128116242207,
1.19485096691822));
#161034=CARTESIAN_POINT('Ctrl Pts',(-1.51628971763685,-6.84837151554262,
1.20414429311435));
#161035=CARTESIAN_POINT('Ctrl Pts',(-1.31571086991073,-6.88669234606126,
1.21343761931049));
#161036=CARTESIAN_POINT('Ctrl Pts',(-1.11513281857241,-6.92501302442905,
1.22273090860796));
#161037=CARTESIAN_POINT('Ctrl Pts',(-0.91289196553951,-6.9545642242027,
1.23202419790545));
#161038=CARTESIAN_POINT('Ctrl Pts',(-0.709713821382708,-6.97523711813716,
1.24131748720293));
#161039=CARTESIAN_POINT('Ctrl Pts',(-0.56743090082418,-6.98971406760236,
1.24782545265525));
#161040=CARTESIAN_POINT('Ctrl Pts',(-0.424688526390375,-6.99983815160022,
1.25433341810757));
#161041=CARTESIAN_POINT('Ctrl Pts',(-0.281737904202462,-7.00558707859917,
1.26084138355989));
#161042=CARTESIAN_POINT('Ctrl Pts',(-0.104003942047775,-7.01273485842708,
1.26893289423473));
#161043=CARTESIAN_POINT('Ctrl Pts',(0.0741727825111977,-7.01312142222494,
1.27702440490957));
#161044=CARTESIAN_POINT('Ctrl Pts',(0.252234662990571,-7.00671137105604,
1.2851159155844));
#161045=CARTESIAN_POINT('Ctrl Pts',(0.430183508079656,-7.00030538904913,
1.29320228969061));
#161046=CARTESIAN_POINT('Ctrl Pts',(0.608017295106995,-6.98711139578564,
1.30128866379682));
#161047=CARTESIAN_POINT('Ctrl Pts',(0.785176856287711,-6.96714603455749,
1.30937503790304));
#161048=CARTESIAN_POINT('Ctrl Pts',(0.962256743144636,-6.94718965239118,
1.31745777530806));
#161049=CARTESIAN_POINT('Ctrl Pts',(1.13866265029188,-6.92046800781922,
1.32554051271306));
#161050=CARTESIAN_POINT('Ctrl Pts',(1.3138389435012,-6.88704971617308,1.33362325011807));
#161051=CARTESIAN_POINT('Ctrl Pts',(1.48899055768737,-6.85363613253152,
1.34170484881842));
#161052=CARTESIAN_POINT('Ctrl Pts',(1.66291254770987,-6.81352784264098,
1.34978644751877));
#161053=CARTESIAN_POINT('Ctrl Pts',(1.83505767291986,-6.76684489991887,
1.35786804621912));
#161054=CARTESIAN_POINT('Ctrl Pts',(2.00718729145277,-6.72016616235398,
1.36594891693636));
#161055=CARTESIAN_POINT('Ctrl Pts',(2.17754001679949,-6.6669140498178,1.37402978765361));
#161056=CARTESIAN_POINT('Ctrl Pts',(2.34558220662477,-6.60725893805179,
1.38211065837086));
#161057=CARTESIAN_POINT('Ctrl Pts',(2.51368048924321,-6.54758391329936,
1.39019422649766));
#161058=CARTESIAN_POINT('Ctrl Pts',(2.67946635625044,-6.48150174261075,
1.39827779462447));
#161059=CARTESIAN_POINT('Ctrl Pts',(2.84242424131525,-6.40923170082682,
1.40636136275128));
#161060=CARTESIAN_POINT('Ctrl Pts',(2.93077163503861,-6.37005059686643,
1.4107438581163));
#161061=CARTESIAN_POINT('Ctrl Pts',(3.01828816610743,-6.32905155411584,
1.41512635348131));
#161062=CARTESIAN_POINT('Ctrl Pts',(3.10489448994163,-6.28627526988996,
1.41950884884632));
#161063=CARTESIAN_POINT('Ctrl Pts',(3.27771823665414,-6.20091478600073,
1.42825416022083));
#161064=CARTESIAN_POINT('Ctrl Pts',(3.44697940375194,-6.10844346605245,
1.43699947159534));
#161065=CARTESIAN_POINT('Ctrl Pts',(3.61211310649541,-6.00918176363339,
1.44574478296985));
#161066=CARTESIAN_POINT('Ctrl Pts',(3.77730538342889,-5.90988485232771,
1.45449319637334));
#161067=CARTESIAN_POINT('Ctrl Pts',(3.93836704090803,-5.80379289000895,
1.46324160977681));
#161068=CARTESIAN_POINT('Ctrl Pts',(4.09476082786269,-5.69127053698041,
1.47199002318029));
#161069=CARTESIAN_POINT('Ctrl Pts',(4.25295023698565,-5.57745626797834,
1.48083888075966));
#161070=CARTESIAN_POINT('Ctrl Pts',(4.40636368954346,-5.45706319406896,
1.48968773833904));
#161071=CARTESIAN_POINT('Ctrl Pts',(4.55447803406386,-5.33051183281022,
1.49853659591841));
#161072=CARTESIAN_POINT('Ctrl Pts',(4.70102050150528,-5.20530350949099,
1.50729154418434));
#161073=CARTESIAN_POINT('Ctrl Pts',(4.84237559824804,-5.07406717295695,
1.51604649245028));
#161074=CARTESIAN_POINT('Ctrl Pts',(4.97807157499556,-4.93724922975549,
1.52480144071622));
#161075=CARTESIAN_POINT('Ctrl Pts',(5.11595085122566,-4.79822993503458,
1.53369725295231));
#161076=CARTESIAN_POINT('Ctrl Pts',(5.24798713546572,-4.65344808564039,
1.54259306518839));
#161077=CARTESIAN_POINT('Ctrl Pts',(5.37372534685965,-4.50341009225432,
1.55148887742448));
#161078=CARTESIAN_POINT('Ctrl Pts',(5.49946355825359,-4.35337209886826,
1.56038468966057));
#161079=CARTESIAN_POINT('Ctrl Pts',(5.61890351354897,-4.19807819035687,
1.56928050189667));
#161080=CARTESIAN_POINT('Ctrl Pts',(5.73163312037252,-4.03806987754654,
1.57817631413276));
#161081=CARTESIAN_POINT('Ctrl Pts',(5.84190041495611,-3.88155656873942,
1.58687781834303));
#161082=CARTESIAN_POINT('Ctrl Pts',(5.94576623752495,-3.72050582006927,
1.5955793225533));
#161083=CARTESIAN_POINT('Ctrl Pts',(6.04287839307084,-3.55545317632754,
1.60428082676357));
#161084=CARTESIAN_POINT('Ctrl Pts',(6.13996557177791,-3.39044298343305,
1.61298009298348));
#161085=CARTESIAN_POINT('Ctrl Pts',(6.23030240926093,-3.22143319194772,
1.62167935920339));
#161086=CARTESIAN_POINT('Ctrl Pts',(6.31358137924273,-3.04898618071311,
1.6303786254233));
#161087=CARTESIAN_POINT('Ctrl Pts',(6.39851486807195,-2.87311313250504,
1.63925072158962));
#161088=CARTESIAN_POINT('Ctrl Pts',(6.47610696232078,-2.69366511636206,
1.64812281775594));
#161089=CARTESIAN_POINT('Ctrl Pts',(6.54608126140386,-2.51126396095617,
1.65699491392227));
#161090=CARTESIAN_POINT('Ctrl Pts',(6.61465203606897,-2.33252135560124,
1.66568905612877));
#161091=CARTESIAN_POINT('Ctrl Pts',(6.67590759491925,-2.1509432230381,1.67438319833527));
#161092=CARTESIAN_POINT('Ctrl Pts',(6.729636539265,-1.96713461966621,1.68307734054176));
#161093=CARTESIAN_POINT('Ctrl Pts',(6.78501509058346,-1.77768265297394,
1.692038413688));
#161094=CARTESIAN_POINT('Ctrl Pts',(6.83239738946693,-1.58586136081559,
1.70099948683424));
#161095=CARTESIAN_POINT('Ctrl Pts',(6.87160723836469,-1.39235071880399,
1.70996055998047));
#161096=CARTESIAN_POINT('Ctrl Pts',(6.91081708726246,-1.19884007679238,
1.71892163312671));
#161097=CARTESIAN_POINT('Ctrl Pts',(6.94185440853548,-1.00364040257306,
1.72788270627295));
#161098=CARTESIAN_POINT('Ctrl Pts',(6.9646004601257,-0.80744473081255,1.73684377941919));
#161099=CARTESIAN_POINT('Ctrl Pts',(6.98611826354928,-0.621843292217489,
1.74532096983004));
#161100=CARTESIAN_POINT('Ctrl Pts',(7.00022244399467,-0.435295819209708,
1.75379816024087));
#161101=CARTESIAN_POINT('Ctrl Pts',(7.00684800478492,-0.248410145408003,
1.76227535065171));
#161102=CARTESIAN_POINT('Ctrl Pts',(7.00978125769814,-0.165672553153999,
1.76602835273798));
#161103=CARTESIAN_POINT('Ctrl Pts',(7.01124938711065,-0.0828687677121652,
1.76978135482426));
#161104=CARTESIAN_POINT('Ctrl Pts',(7.01124999980813,-5.18707572911836E-5,
1.77353435691053));
#161105=CARTESIAN_POINT('Ctrl Pts',(7.01124999980813,-5.18702183956429E-5,
1.77353435693495));
#161106=CARTESIAN_POINT('Ctrl Pts',(7.01125130796046,0.176769884228194,
1.78154736439763));
#161107=CARTESIAN_POINT('Ctrl Pts',(7.00455917992508,0.353638611934562,
1.78956037186032));
#161108=CARTESIAN_POINT('Ctrl Pts',(6.99118901390433,0.530002579581904,
1.797573379323));
#161109=CARTESIAN_POINT('Ctrl Pts',(6.97781578052973,0.706407008259656,
1.80558822511209));
#161110=CARTESIAN_POINT('Ctrl Pts',(6.95776147010324,0.882306078325773,
1.8136030709012));
#161111=CARTESIAN_POINT('Ctrl Pts',(6.93109350035504,1.05715157467423,1.82161791669029));
#161112=CARTESIAN_POINT('Ctrl Pts',(6.90442269778751,1.23201564407883,1.82963361386064));
#161113=CARTESIAN_POINT('Ctrl Pts',(6.87113689907918,1.40582555445287,1.83764931103099));
#161114=CARTESIAN_POINT('Ctrl Pts',(6.83135485206238,1.57804228324331,1.84566500820135));
#161115=CARTESIAN_POINT('Ctrl Pts',(6.79154449996455,1.7503815449055,1.8536864085714));
#161116=CARTESIAN_POINT('Ctrl Pts',(6.74522875642327,1.92112500394349,1.86170780894145));
#161117=CARTESIAN_POINT('Ctrl Pts',(6.69257671255988,2.08974723567258,1.86972920931149));
#161118=CARTESIAN_POINT('Ctrl Pts',(6.65524652701859,2.20930003429072,1.87541636487362));
#161119=CARTESIAN_POINT('Ctrl Pts',(6.6147322762983,2.32778683862197,1.88110352043573));
#161120=CARTESIAN_POINT('Ctrl Pts',(6.57110895151814,2.44502632087635,1.88679067599786));
#161121=CARTESIAN_POINT('Origin',(0.,0.,50.));
#161122=CARTESIAN_POINT('',(7.01124998147128,0.000509724478514493,3.77353435695081));
#161123=CARTESIAN_POINT('Ctrl Pts',(6.57110895151814,2.44502632087635,1.88679067599786));
#161124=CARTESIAN_POINT('Ctrl Pts',(6.54881191176188,2.50495053366855,1.88969753223378));
#161125=CARTESIAN_POINT('Ctrl Pts',(6.52570281864319,2.5645489697426,1.89260438846969));
#161126=CARTESIAN_POINT('Ctrl Pts',(6.50179287697683,2.62379800049344,1.89551124470561));
#161127=CARTESIAN_POINT('Ctrl Pts',(6.42183274031803,2.82193987226578,1.90523241530129));
#161128=CARTESIAN_POINT('Ctrl Pts',(6.33286264442998,3.01629711353528,1.91495358589697));
#161129=CARTESIAN_POINT('Ctrl Pts',(6.23524423677873,3.20614345752302,1.92467475649266));
#161130=CARTESIAN_POINT('Ctrl Pts',(6.1375012290525,3.39623212126647,1.93440833518446));
#161131=CARTESIAN_POINT('Ctrl Pts',(6.03108785351913,3.58179832928602,1.94414191387626));
#161132=CARTESIAN_POINT('Ctrl Pts',(5.9164122242712,3.76213941195622,1.95387549256807));
#161133=CARTESIAN_POINT('Ctrl Pts',(5.80193074154801,3.94217517609713,1.96359259225305));
#161134=CARTESIAN_POINT('Ctrl Pts',(5.67921498599119,4.11700345412605,1.97330969193804));
#161135=CARTESIAN_POINT('Ctrl Pts',(5.54871539223631,4.285951943088,1.98302679162303));
#161136=CARTESIAN_POINT('Ctrl Pts',(5.41856219452529,4.45445197787085,1.99271809839332));
#161137=CARTESIAN_POINT('Ctrl Pts',(5.28066643653707,4.61710334255045,2.00240940516362));
#161138=CARTESIAN_POINT('Ctrl Pts',(5.13551887243857,4.77326643644865,2.01210071193392));
#161139=CARTESIAN_POINT('Ctrl Pts',(4.99129585024135,4.92843482316981,2.02173028829046));
#161140=CARTESIAN_POINT('Ctrl Pts',(4.83991312762028,5.07719727207463,2.03135986464701));
#161141=CARTESIAN_POINT('Ctrl Pts',(4.68189530183761,5.21895420032893,2.04098944100355));
#161142=CARTESIAN_POINT('Ctrl Pts',(4.60975160855841,5.28367391344689,2.04538586399972));
#161143=CARTESIAN_POINT('Ctrl Pts',(4.53622547746523,5.34693377424892,2.04978228699588));
#161144=CARTESIAN_POINT('Ctrl Pts',(4.46136984459352,5.40867873627669,2.05417870999204));
#161145=CARTESIAN_POINT('Ctrl Pts',(4.32760616633295,5.51901423032092,2.06203492185741));
#161146=CARTESIAN_POINT('Ctrl Pts',(4.18964934262517,5.62446438578487,2.06989113372279));
#161147=CARTESIAN_POINT('Ctrl Pts',(4.0479102567175,5.72468768720716,2.07774734558816));
#161148=CARTESIAN_POINT('Ctrl Pts',(3.9062107971707,5.82488296894325,2.08560136107217));
#161149=CARTESIAN_POINT('Ctrl Pts',(3.76073148972948,5.91985408365099,2.09345537655617));
#161150=CARTESIAN_POINT('Ctrl Pts',(3.6119148097489,6.00930095515415,2.10130939204018));
#161151=CARTESIAN_POINT('Ctrl Pts',(3.46310945214693,6.09874102129555,2.10916280996928));
#161152=CARTESIAN_POINT('Ctrl Pts',(3.31096755453269,6.1826574852981,2.11701622789838));
#161153=CARTESIAN_POINT('Ctrl Pts',(3.15595874177207,6.26079475647721,2.12486964582749));
#161154=CARTESIAN_POINT('Ctrl Pts',(3.0008708088336,6.33897191077445,2.13272707232754));
#161155=CARTESIAN_POINT('Ctrl Pts',(2.84291337771074,6.41136380665686,2.14058449882761));
#161156=CARTESIAN_POINT('Ctrl Pts',(2.68257905108324,6.47776166566735,2.14844192532766));
#161157=CARTESIAN_POINT('Ctrl Pts',(2.52220354053244,6.54417657981748,2.15630137010825));
#161158=CARTESIAN_POINT('Ctrl Pts',(2.35945027544116,6.60459425709277,2.16416081488881));
#161159=CARTESIAN_POINT('Ctrl Pts',(2.19482919393369,6.65885510969839,2.1720202596694));
#161160=CARTESIAN_POINT('Ctrl Pts',(2.03004440777395,6.71316992109183,2.17988752014201));
#161161=CARTESIAN_POINT('Ctrl Pts',(1.86338846141331,6.76131557379169,2.18775478061465));
#161162=CARTESIAN_POINT('Ctrl Pts',(1.69538428261545,6.80318298274863,2.19562204108727));
#161163=CARTESIAN_POINT('Ctrl Pts',(1.5727780068827,6.83373702684158,2.20136341915101));
#161164=CARTESIAN_POINT('Ctrl Pts',(1.44945394977381,6.86094846313475,2.20710479721472));
#161165=CARTESIAN_POINT('Ctrl Pts',(1.32561746232475,6.8847922921523,2.21284617527846));
#161166=CARTESIAN_POINT('Ctrl Pts',(1.14492041564138,6.91958421474189,2.22122375511282));
#161167=CARTESIAN_POINT('Ctrl Pts',(0.962732557221327,6.94728122495448,
2.22960133494719));
#161168=CARTESIAN_POINT('Ctrl Pts',(0.779636631868518,6.96776817099627,
2.23797891478154));
#161169=CARTESIAN_POINT('Ctrl Pts',(0.596666158168134,6.98824108001769,
2.24635075455788));
#161170=CARTESIAN_POINT('Ctrl Pts',(0.412789183680431,7.00151373752131,
2.25472259433422));
#161171=CARTESIAN_POINT('Ctrl Pts',(0.228596728856126,7.00752239368925,
2.26309443411056));
#161172=CARTESIAN_POINT('Ctrl Pts',(0.0445034355987655,7.01352781504629,
2.27146176683611));
#161173=CARTESIAN_POINT('Ctrl Pts',(-0.139904671468852,7.01227702179103,
2.27982909956166));
#161174=CARTESIAN_POINT('Ctrl Pts',(-0.324032928336835,7.00375822140181,
2.2881964322872));
#161175=CARTESIAN_POINT('Ctrl Pts',(-0.508089061088417,6.99524275787659,
2.29656048747952));
#161176=CARTESIAN_POINT('Ctrl Pts',(-0.691865234292956,6.97946497954218,
2.30492454267182));
#161177=CARTESIAN_POINT('Ctrl Pts',(-0.874767803901157,6.95646518368043,
2.31328859786414));
#161178=CARTESIAN_POINT('Ctrl Pts',(-1.05762553125399,6.9334710266827,2.32165060243957));
#161179=CARTESIAN_POINT('Ctrl Pts',(-1.23960975629789,6.9032584246089,2.33001260701502));
#161180=CARTESIAN_POINT('Ctrl Pts',(-1.42013251124371,6.86591947323945,
2.33837461159045));
#161181=CARTESIAN_POINT('Ctrl Pts',(-1.60066950234422,6.82857757729336,
2.34673727559959));
#161182=CARTESIAN_POINT('Ctrl Pts',(-1.77974446994,6.78410826993319,2.35509993960872));
#161183=CARTESIAN_POINT('Ctrl Pts',(-1.95677942634572,6.73265481360289,
2.36346260361786));
#161184=CARTESIAN_POINT('Ctrl Pts',(-2.13382636961676,6.68119787340892,
2.37182583385488));
#161185=CARTESIAN_POINT('Ctrl Pts',(-2.30883271038909,6.62275593287524,
2.38018906409187));
#161186=CARTESIAN_POINT('Ctrl Pts',(-2.4812352520754,6.55752225969217,2.38855229432889));
#161187=CARTESIAN_POINT('Ctrl Pts',(-2.65367247665255,6.49227546319697,
2.39691720702951));
#161188=CARTESIAN_POINT('Ctrl Pts',(-2.82350455007629,6.42023432597462,
2.40528211973014));
#161189=CARTESIAN_POINT('Ctrl Pts',(-2.99018749978493,6.34164058258034,
2.41364703243076));
#161190=CARTESIAN_POINT('Ctrl Pts',(-3.15692623686185,6.26302053452734,
2.42201474479665));
#161191=CARTESIAN_POINT('Ctrl Pts',(-3.32051345122711,6.17784364739914,
2.43038245716253));
#161192=CARTESIAN_POINT('Ctrl Pts',(-3.48042866702708,6.08639818416739,
2.43875016952842));
#161193=CARTESIAN_POINT('Ctrl Pts',(-3.64049217405539,5.99486792250042,
2.44712564137072));
#161194=CARTESIAN_POINT('Ctrl Pts',(-3.79687659237451,5.8970576321919,2.45550111321302));
#161195=CARTESIAN_POINT('Ctrl Pts',(-3.94908834715754,5.7933002501894,2.46387658505532));
#161196=CARTESIAN_POINT('Ctrl Pts',(-4.1013747601314,5.68949197633274,2.4722561649744));
#161197=CARTESIAN_POINT('Ctrl Pts',(-4.24948416030648,5.57973098428019,
2.48063574489348));
#161198=CARTESIAN_POINT('Ctrl Pts',(-4.39295460257362,5.46439167906431,
2.48901532481256));
#161199=CARTESIAN_POINT('Ctrl Pts',(-4.53658908447272,5.34892049848178,
2.49740448568214));
#161200=CARTESIAN_POINT('Ctrl Pts',(-4.67557375764741,5.22785847119752,
2.50579364655172));
#161201=CARTESIAN_POINT('Ctrl Pts',(-4.80948121262479,5.10161905946624,
2.51418280742131));
#161202=CARTESIAN_POINT('Ctrl Pts',(-4.89460261550951,5.02137202745653,
2.51951557356465));
#161203=CARTESIAN_POINT('Ctrl Pts',(-4.97767315107139,4.9390336635969,2.52484833970799));
#161204=CARTESIAN_POINT('Ctrl Pts',(-5.05859124150601,4.85471741853826,
2.53018110585133));
#161205=CARTESIAN_POINT('Ctrl Pts',(-5.1857527666769,4.72221574603521,2.53856146520638));
#161206=CARTESIAN_POINT('Ctrl Pts',(-5.30785359630183,4.58456025632525,
2.54694182456144));
#161207=CARTESIAN_POINT('Ctrl Pts',(-5.42446601166464,4.44216107888887,
2.55532218391649));
#161208=CARTESIAN_POINT('Ctrl Pts',(-5.54093063954313,4.29994236951103,
2.56369192251369));
#161209=CARTESIAN_POINT('Ctrl Pts',(-5.65192050908317,4.15299220491027,
2.57206166111089));
#161210=CARTESIAN_POINT('Ctrl Pts',(-5.75704484462818,4.00175726643186,
2.58043139970809));
#161211=CARTESIAN_POINT('Ctrl Pts',(-5.86204990942763,3.85069391433041,
2.58879164226465));
#161212=CARTESIAN_POINT('Ctrl Pts',(-5.96120251809666,3.69535574506099,
2.59715188482121));
#161213=CARTESIAN_POINT('Ctrl Pts',(-6.05415201487855,3.53622255284392,
2.60551212737776));
#161214=CARTESIAN_POINT('Ctrl Pts',(-6.14698098335738,3.37729570981951,
2.61386152914569));
#161215=CARTESIAN_POINT('Ctrl Pts',(-6.23362271923093,3.21458394103671,
2.62221093091362));
#161216=CARTESIAN_POINT('Ctrl Pts',(-6.31376980097288,3.04859598222245,
2.63056033268154));
#161217=CARTESIAN_POINT('Ctrl Pts',(-6.39385526816211,2.88273562972421,
2.63890331569229));
#161218=CARTESIAN_POINT('Ctrl Pts',(-6.46745588918847,2.7136044002636,2.64724629870304));
#161219=CARTESIAN_POINT('Ctrl Pts',(-6.53430957592106,2.54173659699946,
2.65558928171379));
#161220=CARTESIAN_POINT('Ctrl Pts',(-6.60110965729342,2.37000660267236,
2.66392557506191));
#161221=CARTESIAN_POINT('Ctrl Pts',(-6.66117347514114,2.19554471527738,
2.67226186841003));
#161222=CARTESIAN_POINT('Ctrl Pts',(-6.71428653058669,2.01890637417445,
2.68059816175815));
#161223=CARTESIAN_POINT('Ctrl Pts',(-6.73180848479055,1.9606335277436,2.68334829821801));
#161224=CARTESIAN_POINT('Ctrl Pts',(-6.74857435224345,1.9021239724077,2.68609843467789));
#161225=CARTESIAN_POINT('Ctrl Pts',(-6.7645775924045,1.84339810101858,2.68884857113775));
#161226=CARTESIAN_POINT('Ctrl Pts',(-6.81310307226829,1.66532784393962,
2.69718761311069));
#161227=CARTESIAN_POINT('Ctrl Pts',(-6.8545730863525,1.4854138533272,2.70552665508362));
#161228=CARTESIAN_POINT('Ctrl Pts',(-6.88887368500057,1.30424150930977,
2.71386569705655));
#161229=CARTESIAN_POINT('Ctrl Pts',(-6.92319593805141,1.12295478889478,
2.72221000357239));
#161230=CARTESIAN_POINT('Ctrl Pts',(-6.95033968674414,0.940408452339989,
2.73055431008823));
#161231=CARTESIAN_POINT('Ctrl Pts',(-6.97024261627548,0.757195108777878,
2.73889861660408));
#161232=CARTESIAN_POINT('Ctrl Pts',(-6.99016072631762,0.573842023368403,
2.7472492875516));
#161233=CARTESIAN_POINT('Ctrl Pts',(-7.00282696569165,0.389821241431179,
2.75559995849914));
#161234=CARTESIAN_POINT('Ctrl Pts',(-7.00823105916826,0.205727936385168,
2.76395062944666));
#161235=CARTESIAN_POINT('Ctrl Pts',(-7.01364327047901,0.021358093021924,
2.77231384447063));
#161236=CARTESIAN_POINT('Ctrl Pts',(-7.01177152674733,-0.163084163458303,
2.78067705949459));
#161237=CARTESIAN_POINT('Ctrl Pts',(-7.00265765997846,-0.347004696863131,
2.78904027451856));
#161238=CARTESIAN_POINT('Ctrl Pts',(-6.99353598803923,-0.531082740919804,
2.79741065185022));
#161239=CARTESIAN_POINT('Ctrl Pts',(-6.97715984707679,-0.714637844927594,
2.80578102918187));
#161240=CARTESIAN_POINT('Ctrl Pts',(-6.95362270461438,-0.897082964040355,
2.81415140651352));
#161241=CARTESIAN_POINT('Ctrl Pts',(-6.93004923143481,-1.07980969601372,
2.82253470392721));
#161242=CARTESIAN_POINT('Ctrl Pts',(-6.89929272341551,-1.26142269704876,
2.83091800134089));
#161243=CARTESIAN_POINT('Ctrl Pts',(-6.86149759690809,-1.4413456525499,
2.83930129875458));
#161244=CARTESIAN_POINT('Ctrl Pts',(-6.84915253210731,-1.50011409044292,
2.84203954464445));
#161245=CARTESIAN_POINT('Ctrl Pts',(-6.83605692651416,-1.5587023478056,
2.84477779053431));
#161246=CARTESIAN_POINT('Ctrl Pts',(-6.82221694956083,-1.61709073821631,
2.84751603642418));
#161247=CARTESIAN_POINT('Ctrl Pts',(-6.77981297178162,-1.79598554547567,
2.85590568318875));
#161248=CARTESIAN_POINT('Ctrl Pts',(-6.73033202143927,-1.9733641316168,
2.86429532995331));
#161249=CARTESIAN_POINT('Ctrl Pts',(-6.67390018366921,-2.14864676038666,
2.87268497671788));
#161250=CARTESIAN_POINT('Ctrl Pts',(-6.61752044903777,-2.32376755187697,
2.88106687737766));
#161251=CARTESIAN_POINT('Ctrl Pts',(-6.55420272092,-2.49679593235451,2.88944877803744));
#161252=CARTESIAN_POINT('Ctrl Pts',(-6.48412353651385,-2.66716488536557,
2.89783067869723));
#161253=CARTESIAN_POINT('Ctrl Pts',(-6.41409874967245,-2.83740159288559,
2.90620607307433));
#161254=CARTESIAN_POINT('Ctrl Pts',(-6.33732309494566,-3.00498268562944,
2.91458146745144));
#161255=CARTESIAN_POINT('Ctrl Pts',(-6.25402224617957,-3.16935834307057,
2.92295686182855));
#161256=CARTESIAN_POINT('Ctrl Pts',(-6.17077382624258,-3.33363054390376,
2.93132698480533));
#161257=CARTESIAN_POINT('Ctrl Pts',(-6.08100854927558,-3.4947010395989,
2.93969710778212));
#161258=CARTESIAN_POINT('Ctrl Pts',(-5.9849995091868,-3.65204154378531,
2.9480672307589));
#161259=CARTESIAN_POINT('Ctrl Pts',(-5.88903681621201,-3.80930609389201,
2.95643331316781));
#161260=CARTESIAN_POINT('Ctrl Pts',(-5.78683654163941,-3.96284396305371,
2.96479939557671));
#161261=CARTESIAN_POINT('Ctrl Pts',(-5.67871709607945,-4.11215256346296,
2.97316547798562));
#161262=CARTESIAN_POINT('Ctrl Pts',(-5.57062792117543,-4.26141936131535,
2.98152921810724));
#161263=CARTESIAN_POINT('Ctrl Pts',(-5.45662307118149,-4.40645898463984,
2.98989295822887));
#161264=CARTESIAN_POINT('Ctrl Pts',(-5.33706386300932,-4.5467984213796,
2.9982566983505));
#161265=CARTESIAN_POINT('Ctrl Pts',(-5.2175230703903,-4.68711624181399,
3.00661915021584));
#161266=CARTESIAN_POINT('Ctrl Pts',(-5.09242983843877,-4.82273506897357,
3.01498160208117));
#161267=CARTESIAN_POINT('Ctrl Pts',(-4.96218555970055,-4.95321522181294,
3.02334405394652));
#161268=CARTESIAN_POINT('Ctrl Pts',(-4.83194397380087,-5.08369267693699,
3.03170633291572));
#161269=CARTESIAN_POINT('Ctrl Pts',(-4.69655178595717,-5.2090314372549,
3.04006861188495));
#161270=CARTESIAN_POINT('Ctrl Pts',(-4.55644730890227,-5.3288286220986,
3.04843089085416));
#161271=CARTESIAN_POINT('Ctrl Pts',(-4.4163270454667,-5.44863930518307,
3.05679411204964));
#161272=CARTESIAN_POINT('Ctrl Pts',(-4.27149368438351,-5.56290695473472,
3.0651573332451));
#161273=CARTESIAN_POINT('Ctrl Pts',(-4.12241899829919,-5.6712686556856,
3.07352055444058));
#161274=CARTESIAN_POINT('Ctrl Pts',(-3.97325651111114,-5.77969417885334,
3.08188870135532));
#161275=CARTESIAN_POINT('Ctrl Pts',(-3.81984797284376,-5.88220660841301,
3.09025684827006));
#161276=CARTESIAN_POINT('Ctrl Pts',(-3.66269540106451,-5.97848550734389,
3.09862499518479));
#161277=CARTESIAN_POINT('Ctrl Pts',(-3.50549572969042,-6.07479326165448,
3.10699565008476));
#161278=CARTESIAN_POINT('Ctrl Pts',(-3.34455007043597,-6.16486359291279,
3.11536630498472));
#161279=CARTESIAN_POINT('Ctrl Pts',(-3.18038609269,-6.24842146977331,3.12373695988469));
#161280=CARTESIAN_POINT('Ctrl Pts',(-3.01608296101485,-6.33205017463787,
3.13211471018728));
#161281=CARTESIAN_POINT('Ctrl Pts',(-2.84855635538395,-6.40915525015496,
3.14049246048987));
#161282=CARTESIAN_POINT('Ctrl Pts',(-2.67835607621456,-6.4795088773382,
3.14887021079247));
#161283=CARTESIAN_POINT('Ctrl Pts',(-2.57013572790641,-6.52424261147582,
3.15419712952732));
#161284=CARTESIAN_POINT('Ctrl Pts',(-2.4608348332046,-6.5662477458062,3.15952404826219));
#161285=CARTESIAN_POINT('Ctrl Pts',(-2.35059822772696,-6.60547610201618,
3.16485096699704));
#161286=CARTESIAN_POINT('Ctrl Pts',(-2.18788037255686,-6.66338022521263,
3.17271391585551));
#161287=CARTESIAN_POINT('Ctrl Pts',(-2.0227845315506,-6.7153520709923,3.18057686471396));
#161288=CARTESIAN_POINT('Ctrl Pts',(-1.85580118382156,-6.76118543811856,
3.18843981357243));
#161289=CARTESIAN_POINT('Ctrl Pts',(-1.68894614423762,-6.80698358739587,
3.19629672062854));
#161290=CARTESIAN_POINT('Ctrl Pts',(-1.52020684742823,-6.84665253767507,
3.20415362768465));
#161291=CARTESIAN_POINT('Ctrl Pts',(-1.35009246772126,-6.88003465769631,
3.21201053474076));
#161292=CARTESIAN_POINT('Ctrl Pts',(-1.18007402925903,-6.91339795084263,
3.21986301065211));
#161293=CARTESIAN_POINT('Ctrl Pts',(-1.00868242354859,-6.94048139366133,
3.22771548656349));
#161294=CARTESIAN_POINT('Ctrl Pts',(-0.836440411758605,-6.96117763026322,
3.23556796247484));
#161295=CARTESIAN_POINT('Ctrl Pts',(-0.664239081800378,-6.98186897862208,
3.24341858371031));
#161296=CARTESIAN_POINT('Ctrl Pts',(-0.49118812271401,-6.99617606946939,
3.25126920494577));
#161297=CARTESIAN_POINT('Ctrl Pts',(-0.317818816115003,-7.00404295836507,
3.25911982618125));
#161298=CARTESIAN_POINT('Ctrl Pts',(-0.144477404799089,-7.01190858147098,
3.26696918424445));
#161299=CARTESIAN_POINT('Ctrl Pts',(0.0291818707969171,-7.0133360511738,
3.27481854230764));
#161300=CARTESIAN_POINT('Ctrl Pts',(0.202624771223616,-7.00832146555697,
3.28266790037083));
#161301=CARTESIAN_POINT('Ctrl Pts',(0.376126089262714,-7.00330519096862,
3.29051990219031));
#161302=CARTESIAN_POINT('Ctrl Pts',(0.549410504870092,-6.99184253813095,
3.29837190400979));
#161303=CARTESIAN_POINT('Ctrl Pts',(0.721945745408626,-6.97398171084399,
3.30622390582927));
#161304=CARTESIAN_POINT('Ctrl Pts',(0.848618974748946,-6.96086851342375,
3.31198874798067));
#161305=CARTESIAN_POINT('Ctrl Pts',(0.974888403198217,-6.9443075883769,
3.31775359013207));
#161306=CARTESIAN_POINT('Ctrl Pts',(1.10054604165771,-6.92433570623865,
3.32351843228348));
#161307=CARTESIAN_POINT('Ctrl Pts',(1.31100373558767,-6.89088579973248,
3.33317367807616));
#161308=CARTESIAN_POINT('Ctrl Pts',(1.51963775258519,-6.84788416589423,
3.34282892386885));
#161309=CARTESIAN_POINT('Ctrl Pts',(1.72567728556939,-6.79556211571713,
3.35248416966154));
#161310=CARTESIAN_POINT('Ctrl Pts',(1.93285815865867,-6.74295023157767,
3.36219289994376));
#161311=CARTESIAN_POINT('Ctrl Pts',(2.13741569195809,-6.68091445029618,
3.37190163022599));
#161312=CARTESIAN_POINT('Ctrl Pts',(2.33858964665929,-6.60973713751447,
3.38161036050822));
#161313=CARTESIAN_POINT('Ctrl Pts',(2.54073163563352,-6.53821732473898,
3.39136580848646));
#161314=CARTESIAN_POINT('Ctrl Pts',(2.73945737179978,-6.45746782909917,
3.40112125646469));
#161315=CARTESIAN_POINT('Ctrl Pts',(2.93401967882751,-6.36782184791259,
3.41087670444293));
#161316=CARTESIAN_POINT('Ctrl Pts',(3.12877465504619,-6.27808709301166,
3.42064181294739));
#161317=CARTESIAN_POINT('Ctrl Pts',(3.31935792518545,-6.17943825691252,
3.43040692145185));
#161318=CARTESIAN_POINT('Ctrl Pts',(3.50504459134553,-6.07225567439147,
3.44017202995631));
#161319=CARTESIAN_POINT('Ctrl Pts',(3.69047816886052,-5.96521918041382,
3.44992382873783));
#161320=CARTESIAN_POINT('Ctrl Pts',(3.87102844849001,-5.84967220600856,
3.45967562751936));
#161321=CARTESIAN_POINT('Ctrl Pts',(4.04599834227271,-5.72603911764725,
3.46942742630088));
#161322=CARTESIAN_POINT('Ctrl Pts',(4.12230386678096,-5.67212191252108,
3.47368025005722));
#161323=CARTESIAN_POINT('Ctrl Pts',(4.19754838569729,-5.6166674017912,3.47793307381355));
#161324=CARTESIAN_POINT('Ctrl Pts',(4.27167559387015,-5.55971349830493,
3.48218589756989));
#161325=CARTESIAN_POINT('Ctrl Pts',(4.41169191776097,-5.45213523663908,
3.4902189095124));
#161326=CARTESIAN_POINT('Ctrl Pts',(4.54778793700469,-5.33915192181211,
3.49825192145491));
#161327=CARTESIAN_POINT('Ctrl Pts',(4.67951674515051,-5.22108701271642,
3.50628493339742));
#161328=CARTESIAN_POINT('Ctrl Pts',(4.81116086930135,-5.10309800355718,
3.51431278118828));
#161329=CARTESIAN_POINT('Ctrl Pts',(4.9384430989766,-4.9800341463838,3.52234062897914));
#161330=CARTESIAN_POINT('Ctrl Pts',(5.06094843303202,-4.85226004256684,
3.53036847677));
#161331=CARTESIAN_POINT('Ctrl Pts',(5.18339845173464,-4.72454363313262,
3.53839269971271));
#161332=CARTESIAN_POINT('Ctrl Pts',(5.30107561634916,-4.59212147588672,
3.54641692265544));
#161333=CARTESIAN_POINT('Ctrl Pts',(5.41360077606581,-4.4553959644323,3.55444114559815));
#161334=CARTESIAN_POINT('Ctrl Pts',(5.5261123275988,-4.31868698782107,3.56246439813478));
#161335=CARTESIAN_POINT('Ctrl Pts',(5.63347287649328,-4.17767597157517,
3.5704876506714));
#161336=CARTESIAN_POINT('Ctrl Pts',(5.73534256614378,-4.03279955012387,
3.57851090320803));
#161337=CARTESIAN_POINT('Ctrl Pts',(5.83720390685092,-3.88793500232253,
3.58653349818222));
#161338=CARTESIAN_POINT('Ctrl Pts',(5.93357507709479,-3.7392059825822,3.59455609315643));
#161339=CARTESIAN_POINT('Ctrl Pts',(6.02415887192994,-3.58707909701583,
3.60257868813062));
#161340=CARTESIAN_POINT('Ctrl Pts',(6.11477671915454,-3.43489502369349,
3.61060429897017));
#161341=CARTESIAN_POINT('Ctrl Pts',(6.19960265975807,-3.27931084957656,
3.61862990980972));
#161342=CARTESIAN_POINT('Ctrl Pts',(6.27838469183871,-3.12081915909675,
3.62665552064927));
#161343=CARTESIAN_POINT('Ctrl Pts',(6.32484158600727,-3.02735835976525,
3.63138813471829));
#161344=CARTESIAN_POINT('Ctrl Pts',(6.36919768915796,-2.93288697902556,
3.63612074878732));
#161345=CARTESIAN_POINT('Ctrl Pts',(6.41140909568868,-2.83750946610236,
3.64085336285634));
#161346=CARTESIAN_POINT('Ctrl Pts',(6.48937692854863,-2.66133959645394,
3.64959487831509));
#161347=CARTESIAN_POINT('Ctrl Pts',(6.56006375811123,-2.48199048378617,
3.65833639377386));
#161348=CARTESIAN_POINT('Ctrl Pts',(6.62324011041767,-2.30006891250123,
3.66707790923261));
#161349=CARTESIAN_POINT('Ctrl Pts',(6.68735494721308,-2.11544489692144,
3.67594927987243));
#161350=CARTESIAN_POINT('Ctrl Pts',(6.74373430442291,-1.9281716611185,3.68482065051225));
#161351=CARTESIAN_POINT('Ctrl Pts',(6.79219060571534,-1.73890003684293,
3.69369202115208));
#161352=CARTESIAN_POINT('Ctrl Pts',(6.839973679427,-1.5522580577181,3.70244013741148));
#161353=CARTESIAN_POINT('Ctrl Pts',(6.88005238733607,-1.36367313327642,
3.71118825367088));
#161354=CARTESIAN_POINT('Ctrl Pts',(6.91229803400266,-1.17378126225587,
3.71993636993028));
#161355=CARTESIAN_POINT('Ctrl Pts',(6.94522515604355,-0.979876240709369,
3.72886936776033));
#161356=CARTESIAN_POINT('Ctrl Pts',(6.96998440141852,-0.78460870798043,
3.73780236559036));
#161357=CARTESIAN_POINT('Ctrl Pts',(6.98649418571502,-0.588664212832904,
3.74673536342041));
#161358=CARTESIAN_POINT('Ctrl Pts',(7.00300397001153,-0.392719717685374,
3.75566836125045));
#161359=CARTESIAN_POINT('Ctrl Pts',(7.01126427505398,-0.196098560856857,
3.76460135908049));
#161360=CARTESIAN_POINT('Ctrl Pts',(7.01124998147134,0.000509723592105507,
3.77353435691053));
#161361=CARTESIAN_POINT('Ctrl Pts',(7.01124998147128,0.000509724478513097,
3.77353435695083));
#161362=CARTESIAN_POINT('Ctrl Pts',(7.0112361212336,0.191157015833389,3.78219651401479));
#161363=CARTESIAN_POINT('Ctrl Pts',(7.00344264641733,0.381774601939896,
3.79085867107877));
#161364=CARTESIAN_POINT('Ctrl Pts',(6.9878983077323,0.571755020347058,3.79952082814276));
#161365=CARTESIAN_POINT('Ctrl Pts',(6.97221302745539,0.763458004322272,
3.80826152558279));
#161366=CARTESIAN_POINT('Ctrl Pts',(6.94863393904671,0.954525375757643,
3.81700222302283));
#161367=CARTESIAN_POINT('Ctrl Pts',(6.91723719363269,1.14431471611814,3.82574292046287));
#161368=CARTESIAN_POINT('Ctrl Pts',(6.88584628000161,1.3340688040911,3.8344819943636));
#161369=CARTESIAN_POINT('Ctrl Pts',(6.84664065413371,1.52254506505955,3.84322106826431));
#161370=CARTESIAN_POINT('Ctrl Pts',(6.79974792207753,1.70910934661956,3.85196014216504));
#161371=CARTESIAN_POINT('Ctrl Pts',(6.75286578113278,1.89563149109329,3.86069724227364));
#161372=CARTESIAN_POINT('Ctrl Pts',(6.69830006769018,2.08024225306533,3.86943434238223));
#161373=CARTESIAN_POINT('Ctrl Pts',(6.63622901049916,2.26231984535992,3.87817144249082));
#161374=CARTESIAN_POINT('Ctrl Pts',(6.61536704571558,2.32351577934635,3.88110796529267));
#161375=CARTESIAN_POINT('Ctrl Pts',(6.59365768196524,2.38442567898503,3.88404448809452));
#161376=CARTESIAN_POINT('Ctrl Pts',(6.57110895151813,2.44502632087638,3.88698101089636));
#161377=CARTESIAN_POINT('',(7.01124720379832,-0.00626176734468637,3.22646564312318));
#161378=CARTESIAN_POINT('Ctrl Pts',(6.57110895151814,2.44502632087637,3.33981554959537));
#161379=CARTESIAN_POINT('Ctrl Pts',(6.59116786340787,2.39111716891718,3.33721595673525));
#161380=CARTESIAN_POINT('Ctrl Pts',(6.61056612747059,2.33695364996059,3.33461636387513));
#161381=CARTESIAN_POINT('Ctrl Pts',(6.62929711484677,2.28255258988358,3.33201677101501));
#161382=CARTESIAN_POINT('Ctrl Pts',(6.68657087311147,2.11621041573025,3.32406799340565));
#161383=CARTESIAN_POINT('Ctrl Pts',(6.73757578283827,1.9477226746472,3.3161192157963));
#161384=CARTESIAN_POINT('Ctrl Pts',(6.78216126708799,1.77761500604361,3.30817043818693));
#161385=CARTESIAN_POINT('Ctrl Pts',(6.82677318622039,1.60740648003458,3.30021694772075));
#161386=CARTESIAN_POINT('Ctrl Pts',(6.86495798444076,1.43557646827349,3.29226345725457));
#161387=CARTESIAN_POINT('Ctrl Pts',(6.89661578464712,1.26266277424189,3.28430996678838));
#161388=CARTESIAN_POINT('Ctrl Pts',(6.92828431387039,1.0896904787302,3.27635378083694));
#161389=CARTESIAN_POINT('Ctrl Pts',(6.95342138408542,0.915634136736148,
3.26839759488551));
#161390=CARTESIAN_POINT('Ctrl Pts',(6.97197888062657,0.7410378199506,3.26044140893407));
#161391=CARTESIAN_POINT('Ctrl Pts',(6.99055419794468,0.566273838199409,
3.25247758265168));
#161392=CARTESIAN_POINT('Ctrl Pts',(7.00253730037618,0.390969216493217,
3.24451375636926));
#161393=CARTESIAN_POINT('Ctrl Pts',(7.00793215743723,0.215669745808578,
3.23654993008687));
#161394=CARTESIAN_POINT('Ctrl Pts',(7.01020925744765,0.141678086343953,
3.23318850109897));
#161395=CARTESIAN_POINT('Ctrl Pts',(7.01131324795972,0.0676873138780279,
3.22982707211106));
#161396=CARTESIAN_POINT('Ctrl Pts',(7.01124720379832,-0.00626176734468154,
3.22646564312316));
#161397=CARTESIAN_POINT('Ctrl Pts',(7.01124720379766,-0.00626176808276841,
3.22646564308963));
#161398=CARTESIAN_POINT('Ctrl Pts',(7.01104753157552,-0.229833016754554,
3.21630298976489));
#161399=CARTESIAN_POINT('Ctrl Pts',(7.00015032087287,-0.453038581422552,
3.20614033644017));
#161400=CARTESIAN_POINT('Ctrl Pts',(6.97868319966023,-0.674986934155092,
3.19597768311544));
#161401=CARTESIAN_POINT('Ctrl Pts',(6.96275015197123,-0.839718555761688,
3.18843489065315));
#161402=CARTESIAN_POINT('Ctrl Pts',(6.94099549368847,-1.00375802951733,
3.18089209819085));
#161403=CARTESIAN_POINT('Ctrl Pts',(6.91348882294048,-1.16674712666332,
3.17334930572856));
#161404=CARTESIAN_POINT('Ctrl Pts',(6.88289506747146,-1.34802855573501,
3.16495998263458));
#161405=CARTESIAN_POINT('Ctrl Pts',(6.8451407420748,-1.52826072867804,3.1565706595406));
#161406=CARTESIAN_POINT('Ctrl Pts',(6.80031366703914,-1.70685693377642,
3.14818133644661));
#161407=CARTESIAN_POINT('Ctrl Pts',(6.75552797832865,-1.88528825101159,
3.13979975874429));
#161408=CARTESIAN_POINT('Ctrl Pts',(6.70368263690095,-2.0620862940113,3.13141818104197));
#161409=CARTESIAN_POINT('Ctrl Pts',(6.64491664019896,-2.2366737373401,3.12303660333965));
#161410=CARTESIAN_POINT('Ctrl Pts',(6.58619625109565,-2.41112568540812,
3.11466153048118));
#161411=CARTESIAN_POINT('Ctrl Pts',(6.52056601942359,-2.58337014372758,
3.1062864576227));
#161412=CARTESIAN_POINT('Ctrl Pts',(6.44821510041239,-2.75284372627901,
3.09791138476423));
#161413=CARTESIAN_POINT('Ctrl Pts',(6.37590970147637,-2.9222106833677,3.08954158114009));
#161414=CARTESIAN_POINT('Ctrl Pts',(6.29689217492977,-3.08880993908589,
3.08117177751596));
#161415=CARTESIAN_POINT('Ctrl Pts',(6.2114004049943,-3.25209648862648,3.07280197389181));
#161416=CARTESIAN_POINT('Ctrl Pts',(6.12594987710188,-3.4153042671823,3.06443620794056));
#161417=CARTESIAN_POINT('Ctrl Pts',(6.03403148628287,-3.57520223562449,
3.0560704419893));
#161418=CARTESIAN_POINT('Ctrl Pts',(5.93593001954654,-3.73126806401606,
3.04770467603804));
#161419=CARTESIAN_POINT('Ctrl Pts',(5.83785594686929,-3.88729031225879,
3.0393412461608));
#161420=CARTESIAN_POINT('Ctrl Pts',(5.73360241458621,-4.03948227536512,
3.03097781628356));
#161421=CARTESIAN_POINT('Ctrl Pts',(5.62349896132917,-4.1873483249462,3.02261438640632));
#161422=CARTESIAN_POINT('Ctrl Pts',(5.5134124108012,-4.33519167460552,3.01425224045601));
#161423=CARTESIAN_POINT('Ctrl Pts',(5.39747792611674,-4.47871017123534,
3.0058900945057));
#161424=CARTESIAN_POINT('Ctrl Pts',(5.27606721836805,-4.61743882144226,
2.99752794855539));
#161425=CARTESIAN_POINT('Ctrl Pts',(5.15465894855081,-4.75616468597281,
2.98916597051727));
#161426=CARTESIAN_POINT('Ctrl Pts',(5.02777489172064,-4.89010064876383,
2.98080399247916));
#161427=CARTESIAN_POINT('Ctrl Pts',(4.89582600964123,-5.01881602031998,
2.97244201444104));
#161428=CARTESIAN_POINT('Ctrl Pts',(4.76386217056269,-5.14754598234231,
2.96407908853512));
#161429=CARTESIAN_POINT('Ctrl Pts',(4.62683259727144,-5.27105394415241,
2.95571616262919));
#161430=CARTESIAN_POINT('Ctrl Pts',(4.48518425625931,-5.38894690546341,
2.94735323672326));
#161431=CARTESIAN_POINT('Ctrl Pts',(4.34345230361911,-5.50690945616997,
2.93898537438218));
#161432=CARTESIAN_POINT('Ctrl Pts',(4.19709638768098,-5.61925017217225,
2.93061751204111));
#161433=CARTESIAN_POINT('Ctrl Pts',(4.04659643642701,-5.72561645966582,
2.92224964970003));
#161434=CARTESIAN_POINT('Ctrl Pts',(3.89605126911981,-5.8320147037393,2.91387927332684));
#161435=CARTESIAN_POINT('Ctrl Pts',(3.74135985549983,-5.93243475478525,
2.90550889695365));
#161436=CARTESIAN_POINT('Ctrl Pts',(3.58303069217646,-6.02656764845642,
2.89713852058046));
#161437=CARTESIAN_POINT('Ctrl Pts',(3.42456708812255,-6.1207804724116,2.88876103673894));
#161438=CARTESIAN_POINT('Ctrl Pts',(3.26245984774095,-6.20869530810382,
2.88038355289741));
#161439=CARTESIAN_POINT('Ctrl Pts',(3.09724264181671,-6.29004885356324,
2.87200606905589));
#161440=CARTESIAN_POINT('Ctrl Pts',(2.99211549249737,-6.3418138393789,2.8666755044225));
#161441=CARTESIAN_POINT('Ctrl Pts',(2.88572966766815,-6.39092327569232,
2.86134493978911));
#161442=CARTESIAN_POINT('Ctrl Pts',(2.77822683336806,-6.43731949066175,
2.85601437515572));
#161443=CARTESIAN_POINT('Ctrl Pts',(2.61956441318462,-6.50579522716049,
2.84814704504126));
#161444=CARTESIAN_POINT('Ctrl Pts',(2.4581382896286,-6.56850053935805,2.84027971492681));
#161445=CARTESIAN_POINT('Ctrl Pts',(2.29442486448226,-6.62519743885008,
2.83241238481235));
#161446=CARTESIAN_POINT('Ctrl Pts',(2.13083753904616,-6.68185066774764,
2.82455111448222));
#161447=CARTESIAN_POINT('Ctrl Pts',(1.96496677326853,-6.73250456367311,
2.81668984415209));
#161448=CARTESIAN_POINT('Ctrl Pts',(1.79731079744992,-6.77696838268189,
2.80882857382196));
#161449=CARTESIAN_POINT('Ctrl Pts',(1.6297497338721,-6.82140703014116,2.80097175385979));
#161450=CARTESIAN_POINT('Ctrl Pts',(1.46040583769453,-6.85966247432036,
2.79311493389762));
#161451=CARTESIAN_POINT('Ctrl Pts',(1.28979418668937,-6.89159324963991,
2.78525811393544));
#161452=CARTESIAN_POINT('Ctrl Pts',(1.1192236155632,-6.92351633666631,2.77740318573864));
#161453=CARTESIAN_POINT('Ctrl Pts',(0.947386269685783,-6.94911770765619,
2.76954825754183));
#161454=CARTESIAN_POINT('Ctrl Pts',(0.77480909498942,-6.96830663998232,
2.76169332934503));
#161455=CARTESIAN_POINT('Ctrl Pts',(0.602260058155004,-6.98749244364714,
2.75383968185574));
#161456=CARTESIAN_POINT('Ctrl Pts',(0.428971811777411,-7.00026785080396,
2.74598603436646));
#161457=CARTESIAN_POINT('Ctrl Pts',(0.2554776700235,-7.00659387453129,2.73813238687718));
#161458=CARTESIAN_POINT('Ctrl Pts',(0.0819260470773751,-7.01292199416446,
2.73027613735755));
#161459=CARTESIAN_POINT('Ctrl Pts',(-0.0918312262740901,-7.0127964482853,
2.72241988783793));
#161460=CARTESIAN_POINT('Ctrl Pts',(-0.265259376653958,-7.00623037200442,
2.7145636383183));
#161461=CARTESIAN_POINT('Ctrl Pts',(-0.391946857028583,-7.0014339208046,
2.7088247288353));
#161462=CARTESIAN_POINT('Ctrl Pts',(-0.518458670811295,-6.99320179469858,
2.70308581935229));
#161463=CARTESIAN_POINT('Ctrl Pts',(-0.644587821142319,-6.98155663898353,
2.69734690986928));
#161464=CARTESIAN_POINT('Ctrl Pts',(-0.856167445565318,-6.96202207725794,
2.68771998136127));
#161465=CARTESIAN_POINT('Ctrl Pts',(-1.06656328868496,-6.93289256428452,
2.67809305285326));
#161466=CARTESIAN_POINT('Ctrl Pts',(-1.27499597528205,-6.8943463668077,
2.66846612434526));
#161467=CARTESIAN_POINT('Ctrl Pts',(-1.48453805740377,-6.85559500487386,
2.65878795593061));
#161468=CARTESIAN_POINT('Ctrl Pts',(-1.6920959842416,-6.80732651379863,
2.64910978751596));
#161469=CARTESIAN_POINT('Ctrl Pts',(-1.8968979678959,-6.74977071180143,
2.63943161910131));
#161470=CARTESIAN_POINT('Ctrl Pts',(-2.10266028244323,-6.69194502660416,
2.62970806907487));
#161471=CARTESIAN_POINT('Ctrl Pts',(-2.30564070360076,-6.62474476636611,
2.61998451904842));
#161472=CARTESIAN_POINT('Ctrl Pts',(-2.50507743212523,-6.54845123838888,
2.61026096902198));
#161473=CARTESIAN_POINT('Ctrl Pts',(-2.70471732197539,-6.47207999205757,
2.60052751385254));
#161474=CARTESIAN_POINT('Ctrl Pts',(-2.90080625793617,-6.38659697746056,
2.59079405868311));
#161475=CARTESIAN_POINT('Ctrl Pts',(-3.09260159054713,-6.29233199733178,
2.58106060351368));
#161476=CARTESIAN_POINT('Ctrl Pts',(-3.28417339240915,-6.19817687973886,
2.57133849234566));
#161477=CARTESIAN_POINT('Ctrl Pts',(-3.47146155099836,-6.09526027644286,
2.56161638117764));
#161478=CARTESIAN_POINT('Ctrl Pts',(-3.65374801202568,-5.98395788981828,
2.55189427000961));
#161479=CARTESIAN_POINT('Ctrl Pts',(-3.73633925578969,-5.93352845861741,
2.54748932820069));
#161480=CARTESIAN_POINT('Ctrl Pts',(-3.81790402458919,-5.88137818228995,
2.54308438639177));
#161481=CARTESIAN_POINT('Ctrl Pts',(-3.89837706152768,-5.82754518203461,
2.53867944458285));
#161482=CARTESIAN_POINT('Ctrl Pts',(-4.04553163005916,-5.72910510537409,
2.53062448187785));
#161483=CARTESIAN_POINT('Ctrl Pts',(-4.18910593294209,-5.62498673949934,
2.52256951917284));
#161484=CARTESIAN_POINT('Ctrl Pts',(-4.32863101602867,-5.51548548085974,
2.51451455646784));
#161485=CARTESIAN_POINT('Ctrl Pts',(-4.46806543240845,-5.40605537873403,
2.50646482806857));
#161486=CARTESIAN_POINT('Ctrl Pts',(-4.60345558165775,-5.29124957136967,
2.49841509966931));
#161487=CARTESIAN_POINT('Ctrl Pts',(-4.73436169629557,-5.17140656796092,
2.49036537127004));
#161488=CARTESIAN_POINT('Ctrl Pts',(-4.86520750588745,-5.0516187731102,
2.4823193511715));
#161489=CARTESIAN_POINT('Ctrl Pts',(-4.99157312601222,-4.92679864862529,
2.47427333107296));
#161490=CARTESIAN_POINT('Ctrl Pts',(-5.11305210604816,-4.79732474649533,
2.46622731097442));
#161491=CARTESIAN_POINT('Ctrl Pts',(-5.23451372403499,-4.66786934906674,
2.45818244083118));
#161492=CARTESIAN_POINT('Ctrl Pts',(-5.35108983886226,-4.53376175975606,
2.45013757068795));
#161493=CARTESIAN_POINT('Ctrl Pts',(-5.46241097456368,-4.39541726204309,
2.44209270054471));
#161494=CARTESIAN_POINT('Ctrl Pts',(-5.57372174642829,-4.25708564400284,
2.43404857936724));
#161495=CARTESIAN_POINT('Ctrl Pts',(-5.67977828813721,-4.11451818964834,
2.42600445818977));
#161496=CARTESIAN_POINT('Ctrl Pts',(-5.7802516956113,-3.96816291221552,
2.41796033701231));
#161497=CARTESIAN_POINT('Ctrl Pts',(-5.88076006096164,-3.82175671315272,
2.40991341703067));
#161498=CARTESIAN_POINT('Ctrl Pts',(-5.97568120715722,-3.67156036033681,
2.40186649704902));
#161499=CARTESIAN_POINT('Ctrl Pts',(-6.06472960808963,-3.51805078747607,
2.39381957706738));
#161500=CARTESIAN_POINT('Ctrl Pts',(-6.1156619111748,-3.43024914242068,
2.38921704447706));
#161501=CARTESIAN_POINT('Ctrl Pts',(-6.16467382062123,-3.34136410659353,
2.38461451188674));
#161502=CARTESIAN_POINT('Ctrl Pts',(-6.21171869217826,-3.2514884978642,
2.38001197929643));
#161503=CARTESIAN_POINT('Ctrl Pts',(-6.30054239512107,-3.08179764512375,
2.37132210569158));
#161504=CARTESIAN_POINT('Ctrl Pts',(-6.38239382465608,-2.90849380649929,
2.36263223208672));
#161505=CARTESIAN_POINT('Ctrl Pts',(-6.45700612407809,-2.73216003852595,
2.35394235848187));
#161506=CARTESIAN_POINT('Ctrl Pts',(-6.53163751284605,-2.5557811560564,
2.34525026159742));
#161507=CARTESIAN_POINT('Ctrl Pts',(-6.59902596574914,-2.37637105548189,
2.33655816471299));
#161508=CARTESIAN_POINT('Ctrl Pts',(-6.65895292056474,-2.19453242496034,
2.32786606782853));
#161509=CARTESIAN_POINT('Ctrl Pts',(-6.7201532694509,-2.00882988654265,
2.31898927167699));
#161510=CARTESIAN_POINT('Ctrl Pts',(-6.77357138147548,-1.82059474689036,
2.31011247552542));
#161511=CARTESIAN_POINT('Ctrl Pts',(-6.81902811021397,-1.63048526353711,
2.30123567937387));
#161512=CARTESIAN_POINT('Ctrl Pts',(-6.863568952766,-1.44420620649368,2.29253773760101));
#161513=CARTESIAN_POINT('Ctrl Pts',(-6.9004661194254,-1.25612789758659,
2.28383979582816));
#161514=CARTESIAN_POINT('Ctrl Pts',(-6.9296025805661,-1.06688079836111,
2.2751418540553));
#161515=CARTESIAN_POINT('Ctrl Pts',(-6.95963773425792,-0.871796512609358,
2.26617563071442));
#161516=CARTESIAN_POINT('Ctrl Pts',(-6.98142572935617,-0.675470495382184,
2.25720940737353));
#161517=CARTESIAN_POINT('Ctrl Pts',(-6.99489582811723,-0.47860099904643,
2.24824318403265));
#161518=CARTESIAN_POINT('Ctrl Pts',(-7.00836592687828,-0.281731502710676,
2.23927696069177));
#161519=CARTESIAN_POINT('Ctrl Pts',(-7.01351811730095,-0.084318853007292,
2.23031073735089));
#161520=CARTESIAN_POINT('Ctrl Pts',(-7.01034036778413,0.112935779610404,
2.22134451401001));
#161521=CARTESIAN_POINT('Ctrl Pts',(-7.00723646838226,0.305606263221481,
2.21258666348793));
#161522=CARTESIAN_POINT('Ctrl Pts',(-6.99618509540164,0.498159174276181,
2.20382881296585));
#161523=CARTESIAN_POINT('Ctrl Pts',(-6.97722014547274,0.689946087828103,
2.19507096244377));
#161524=CARTESIAN_POINT('Ctrl Pts',(-6.95825895554909,0.881694977562244,
2.18631484825973));
#161525=CARTESIAN_POINT('Ctrl Pts',(-6.93138734864916,1.07267790347401,
2.17755873407569));
#161526=CARTESIAN_POINT('Ctrl Pts',(-6.89669110777299,1.26225129291475,
2.16880261989165));
#161527=CARTESIAN_POINT('Ctrl Pts',(-6.86164741998548,1.45372306347608,
2.15995882229431));
#161528=CARTESIAN_POINT('Ctrl Pts',(-6.81862155666545,1.64375663391736,
2.15111502469697));
#161529=CARTESIAN_POINT('Ctrl Pts',(-6.76775516826714,1.83169772203097,
2.14227122709963));
#161530=CARTESIAN_POINT('Ctrl Pts',(-6.71742360909971,2.01766272356223,
2.13352041667153));
#161531=CARTESIAN_POINT('Ctrl Pts',(-6.65941568650613,2.20157876791965,
2.12476960624344));
#161532=CARTESIAN_POINT('Ctrl Pts',(-6.59391944734918,2.38282456013242,
2.11601879581534));
#161533=CARTESIAN_POINT('Ctrl Pts',(-6.52737925176231,2.56695926188584,
2.10712850463338));
#161534=CARTESIAN_POINT('Ctrl Pts',(-6.45311007030879,2.74833759050299,
2.09823821345143));
#161535=CARTESIAN_POINT('Ctrl Pts',(-6.37136138372236,2.92632545703848,
2.08934792226946));
#161536=CARTESIAN_POINT('Ctrl Pts',(-6.28961269713594,3.10431332357397,
2.0804576310875));
#161537=CARTESIAN_POINT('Ctrl Pts',(-6.20038461379614,3.27891045438438,
2.07156733990554));
#161538=CARTESIAN_POINT('Ctrl Pts',(-6.10397786506047,3.44950442605193,
2.06267704872357));
#161539=CARTESIAN_POINT('Ctrl Pts',(-6.01631887157887,3.60461904247164,
2.05459344475404));
#161540=CARTESIAN_POINT('Ctrl Pts',(-5.92269477699021,3.75647621605263,
2.0465098407845));
#161541=CARTESIAN_POINT('Ctrl Pts',(-5.82338398339379,3.90459031710788,
2.03842623681497));
#161542=CARTESIAN_POINT('Ctrl Pts',(-5.72410160994942,4.05266203178077,
2.0303449461615));
#161543=CARTESIAN_POINT('Ctrl Pts',(-5.61913597921042,4.19699250786548,
2.02226365550803));
#161544=CARTESIAN_POINT('Ctrl Pts',(-5.50880960625082,4.33712384934749,
2.01418236485456));
#161545=CARTESIAN_POINT('Ctrl Pts',(-5.39849438982538,4.47724102032739,
2.00610189140547));
#161546=CARTESIAN_POINT('Ctrl Pts',(-5.28281973493344,4.61315961981969,
1.99802141795639));
#161547=CARTESIAN_POINT('Ctrl Pts',(-5.16214935538897,4.74445366666777,
1.9899409445073));
#161548=CARTESIAN_POINT('Ctrl Pts',(-5.04143258982531,4.87579818330139,
1.98185736490244));
#161549=CARTESIAN_POINT('Ctrl Pts',(-4.91571650574492,5.00251432843386,
1.97377378529757));
#161550=CARTESIAN_POINT('Ctrl Pts',(-4.7854030638399,5.1242115568243,1.9656902056927));
#161551=CARTESIAN_POINT('Ctrl Pts',(-4.65506242599418,5.24593418298307,
1.95760493907422));
#161552=CARTESIAN_POINT('Ctrl Pts',(-4.52012278784488,5.3626355651621,1.94951967245572));
#161553=CARTESIAN_POINT('Ctrl Pts',(-4.38102025938351,5.47396456413185,
1.94143440583724));
#161554=CARTESIAN_POINT('Ctrl Pts',(-4.24180835108692,5.58538110390836,
1.93334278156918));
#161555=CARTESIAN_POINT('Ctrl Pts',(-4.09842730155014,5.69141660436618,
1.92525115730112));
#161556=CARTESIAN_POINT('Ctrl Pts',(-3.95134388299007,5.79176208772917,
1.91715953303306));
#161557=CARTESIAN_POINT('Ctrl Pts',(-3.87166727433948,5.8461202736215,1.91277621650108));
#161558=CARTESIAN_POINT('Ctrl Pts',(-3.79090469083633,5.89880948512212,
1.90839289996912));
#161559=CARTESIAN_POINT('Ctrl Pts',(-3.70913347285415,5.94978616784275,
1.90400958343714));
#161560=CARTESIAN_POINT('Ctrl Pts',(-3.53577909345671,6.05785635946815,
1.8947169846982));
#161561=CARTESIAN_POINT('Ctrl Pts',(-3.35775526832687,6.15831162868173,
1.88542438595926));
#161562=CARTESIAN_POINT('Ctrl Pts',(-3.17570664580314,6.25080105764868,
1.87613178722032));
#161563=CARTESIAN_POINT('Ctrl Pts',(-2.99361604881069,6.34331181165829,
1.86683704591149));
#161564=CARTESIAN_POINT('Ctrl Pts',(-2.80749894707798,6.42785298311857,
1.85754230460267));
#161565=CARTESIAN_POINT('Ctrl Pts',(-2.61802323834685,6.50412030069985,
1.84824756329385));
#161566=CARTESIAN_POINT('Ctrl Pts',(-2.4287389281723,6.58031057698335,1.83896221105174));
#161567=CARTESIAN_POINT('Ctrl Pts',(-2.23610294376896,6.64824364362018,
1.82967685880963));
#161568=CARTESIAN_POINT('Ctrl Pts',(-2.04080166488643,6.70766390981963,
1.82039150656752));
#161569=CARTESIAN_POINT('Ctrl Pts',(-1.84574325221575,6.76701028415805,
1.81111770109223));
#161570=CARTESIAN_POINT('Ctrl Pts',(-1.64802632048138,6.81786495122889,
1.80184389561693));
#161571=CARTESIAN_POINT('Ctrl Pts',(-1.44835289833174,6.8600218982445,1.79257009014163));
#161572=CARTESIAN_POINT('Ctrl Pts',(-1.24927025242264,6.90205411497602,
1.78332372319007));
#161573=CARTESIAN_POINT('Ctrl Pts',(-1.04824283211687,6.93543994730127,
1.77407735623852));
#161574=CARTESIAN_POINT('Ctrl Pts',(-0.845982265906969,6.96002446606841,
1.76483098928696));
#161575=CARTESIAN_POINT('Ctrl Pts',(-0.703878521035723,6.97729699846627,
1.75833469890821));
#161576=CARTESIAN_POINT('Ctrl Pts',(-0.561166409073024,6.9902260899788,
1.75183840852947));
#161577=CARTESIAN_POINT('Ctrl Pts',(-0.418096783377079,6.99877286688386,
1.74534211815072));
#161578=CARTESIAN_POINT('Ctrl Pts',(-0.237722289166465,7.009548183824,1.7371519444111));
#161579=CARTESIAN_POINT('Ctrl Pts',(-0.056889423869269,7.01334864684188,
1.72896177067148));
#161580=CARTESIAN_POINT('Ctrl Pts',(0.123828300585204,7.01015642582063,
1.72077159693185));
#161581=CARTESIAN_POINT('Ctrl Pts',(0.304536860524118,7.00696436668254,
1.71258183853043));
#161582=CARTESIAN_POINT('Ctrl Pts',(0.485129942468523,6.99678033663585,
1.70439208012902));
#161583=CARTESIAN_POINT('Ctrl Pts',(0.665034749126982,6.97963862567065,
1.6962023217276));
#161584=CARTESIAN_POINT('Ctrl Pts',(0.84496092534677,6.96249487856838,1.68801159052535));
#161585=CARTESIAN_POINT('Ctrl Pts',(1.02419831620835,6.93839183785307,1.67982085932311));
#161586=CARTESIAN_POINT('Ctrl Pts',(1.20217976786569,6.90741560702948,1.67163012812087));
#161587=CARTESIAN_POINT('Ctrl Pts',(1.38027861073457,6.87641894521585,1.66343399455871));
#161588=CARTESIAN_POINT('Ctrl Pts',(1.55711951550437,6.83854009680515,1.65523786099655));
#161589=CARTESIAN_POINT('Ctrl Pts',(1.73214522940835,6.79391635706077,1.64704172743439));
#161590=CARTESIAN_POINT('Ctrl Pts',(1.90723594944459,6.74927604365608,1.63884254975414));
#161591=CARTESIAN_POINT('Ctrl Pts',(2.08050979909328,6.69788594002075,1.6306433720739));
#161592=CARTESIAN_POINT('Ctrl Pts',(2.25142498318926,6.63993314029375,1.62244419439365));
#161593=CARTESIAN_POINT('Ctrl Pts',(2.42250439563771,6.58192465509404,1.61423713831776));
#161594=CARTESIAN_POINT('Ctrl Pts',(2.59122028843721,6.51734099885884,1.60603008224185));
#161595=CARTESIAN_POINT('Ctrl Pts',(2.75705029625068,6.44641762736825,1.59782302616596));
#161596=CARTESIAN_POINT('Ctrl Pts',(2.83213750635506,6.41430378882573,1.59410690173206));
#161597=CARTESIAN_POINT('Ctrl Pts',(2.90663335369555,6.38089078951445,1.59039077729817));
#161598=CARTESIAN_POINT('Ctrl Pts',(2.98049102249514,6.34620357594412,1.58667465286428));
#161599=CARTESIAN_POINT('Ctrl Pts',(3.14270627245884,6.27001927292849,1.57851284565132));
#161600=CARTESIAN_POINT('Ctrl Pts',(3.30218226723319,6.18752525781849,1.57035103843836));
#161601=CARTESIAN_POINT('Ctrl Pts',(3.4583976801335,6.09894351904879,1.5621892312254));
#161602=CARTESIAN_POINT('Ctrl Pts',(3.61446761511558,6.01044427333602,1.55403502481636));
#161603=CARTESIAN_POINT('Ctrl Pts',(3.76728271123916,5.91586877054678,1.54588081840732));
#161604=CARTESIAN_POINT('Ctrl Pts',(3.91634350483618,5.81548623200395,1.53772661199827));
#161605=CARTESIAN_POINT('Ctrl Pts',(4.06682964618143,5.71414381647522,1.52949443351178));
#161606=CARTESIAN_POINT('Ctrl Pts',(4.21348897605338,5.60688287115958,1.52126225502529));
#161607=CARTESIAN_POINT('Ctrl Pts',(4.35583367523542,5.49402762608499,1.51303007653879));
#161608=CARTESIAN_POINT('Ctrl Pts',(4.49664671805326,5.38238672517176,1.50488647787748));
#161609=CARTESIAN_POINT('Ctrl Pts',(4.63323723830541,5.265271544388,1.49674287921618));
#161610=CARTESIAN_POINT('Ctrl Pts',(4.76516285886654,5.14303893539402,1.48859928055487));
#161611=CARTESIAN_POINT('Ctrl Pts',(4.89705026642743,5.02084173176481,1.48045804073286));
#161612=CARTESIAN_POINT('Ctrl Pts',(5.02427520692485,4.89353029247951,1.47231680091084));
#161613=CARTESIAN_POINT('Ctrl Pts',(5.14642961380638,4.7615006870352,1.46417556108882));
#161614=CARTESIAN_POINT('Ctrl Pts',(5.26857011421174,4.62948611229351,1.45603524809344));
#161615=CARTESIAN_POINT('Ctrl Pts',(5.38564099163647,4.49275470124292,1.44789493509806));
#161616=CARTESIAN_POINT('Ctrl Pts',(5.49727209523096,4.35173828182429,1.43975462210268));
#161617=CARTESIAN_POINT('Ctrl Pts',(5.61109338112971,4.20795514545604,1.43145459762098));
#161618=CARTESIAN_POINT('Ctrl Pts',(5.71925897298525,4.0597173999367,1.42315457313929));
#161619=CARTESIAN_POINT('Ctrl Pts',(5.82142064820782,3.90751688404793,1.4148545486576));
#161620=CARTESIAN_POINT('Ctrl Pts',(5.92167666008053,3.75815542639042,1.4067093479141));
#161621=CARTESIAN_POINT('Ctrl Pts',(6.01615060709697,3.60497805767956,1.39856414717059));
#161622=CARTESIAN_POINT('Ctrl Pts',(6.10455816450969,3.44847737104626,1.39041894642709));
#161623=CARTESIAN_POINT('Ctrl Pts',(6.19548639433195,3.28751454368182,1.3820415100763));
#161624=CARTESIAN_POINT('Ctrl Pts',(6.27999697204131,3.12303642653392,1.3736640737255));
#161625=CARTESIAN_POINT('Ctrl Pts',(6.35783226829758,2.95560406866246,1.36528663737471));
#161626=CARTESIAN_POINT('Ctrl Pts',(6.43566756455385,2.788171710791,1.35690920102392));
#161627=CARTESIAN_POINT('Ctrl Pts',(6.50682745250105,2.61778549733251,1.34853176467315));
#161628=CARTESIAN_POINT('Ctrl Pts',(6.57110895151814,2.44502632087636,1.34015432832236));
#161629=CARTESIAN_POINT('Origin',(0.,0.,-4.41670255678778));
#161630=CARTESIAN_POINT('',(2.10208451021623,-7.84862588447233,0.));
#161631=CARTESIAN_POINT('',(8.12525,4.45453136183049E-13,0.416702556787629));
#161632=CARTESIAN_POINT('Ctrl Pts',(2.10208451021623,-7.84862588447233,
1.77635683940025E-15));
#161633=CARTESIAN_POINT('Ctrl Pts',(2.30734049756823,-7.79365251231869,
0.00832438836227722));
#161634=CARTESIAN_POINT('Ctrl Pts',(2.5104411573911,-7.73062260289495,0.0166487767245511));
#161635=CARTESIAN_POINT('Ctrl Pts',(2.71075935410536,-7.65973049699728,
0.024973165086827));
#161636=CARTESIAN_POINT('Ctrl Pts',(2.91107282461945,-7.58884006368997,
0.0332973570479451));
#161637=CARTESIAN_POINT('Ctrl Pts',(3.10860370015948,-7.51008789831038,
0.0416215490090642));
#161638=CARTESIAN_POINT('Ctrl Pts',(3.30274228536127,-7.42371746222784,
0.0499457409701822));
#161639=CARTESIAN_POINT('Ctrl Pts',(3.49688087431976,-7.33734702447398,
0.0582699330923786));
#161640=CARTESIAN_POINT('Ctrl Pts',(3.68762691807514,-7.24335843006386,
0.0665941252145752));
#161641=CARTESIAN_POINT('Ctrl Pts',(3.87439200321211,-7.14204271675451,
0.0749183173367713));
#161642=CARTESIAN_POINT('Ctrl Pts',(4.06118273642806,-7.04071308995904,
0.0832436526037741));
#161643=CARTESIAN_POINT('Ctrl Pts',(4.24399117233817,-6.93205446539553,
0.0915689878707773));
#161644=CARTESIAN_POINT('Ctrl Pts',(4.42225369533016,-6.81640373046071,
0.0998943231377805));
#161645=CARTESIAN_POINT('Ctrl Pts',(4.60051640598431,-6.70075287377699,
0.108219667169107));
#161646=CARTESIAN_POINT('Ctrl Pts',(4.77423296131069,-6.57811004621418,
0.116545011200433));
#161647=CARTESIAN_POINT('Ctrl Pts',(4.94286836885875,-6.44885570086939,
0.124870355231759));
#161648=CARTESIAN_POINT('Ctrl Pts',(5.11152549662714,-6.31958470758037,
0.133196771566401));
#161649=CARTESIAN_POINT('Ctrl Pts',(5.27509994743933,-6.18370066507483,
0.141523187901042));
#161650=CARTESIAN_POINT('Ctrl Pts',(5.43308855487239,-6.04162530428813,
0.149849604235683));
#161651=CARTESIAN_POINT('Ctrl Pts',(5.48885971067159,-5.99147164314507,
0.152788891252597));
#161652=CARTESIAN_POINT('Ctrl Pts',(5.54393509745807,-5.9405468168862,0.155728178269512));
#161653=CARTESIAN_POINT('Ctrl Pts',(5.5982936114802,-5.88887053705207,0.158667465286427));
#161654=CARTESIAN_POINT('Ctrl Pts',(5.74712452149839,-5.74738345094562,
0.166715087069352));
#161655=CARTESIAN_POINT('Ctrl Pts',(5.89064187191427,-5.60020048953742,
0.174762708852277));
#161656=CARTESIAN_POINT('Ctrl Pts',(6.02840651757392,-5.44775205211951,
0.182810330635203));
#161657=CARTESIAN_POINT('Ctrl Pts',(6.16613103580062,-5.29534801915979,
0.190855608345004));
#161658=CARTESIAN_POINT('Ctrl Pts',(6.29810597726349,-5.13768180517975,
0.198900886054805));
#161659=CARTESIAN_POINT('Ctrl Pts',(6.42393006636541,-4.9752195996706,0.206946163764606));
#161660=CARTESIAN_POINT('Ctrl Pts',(6.54973363839208,-4.81278388550598,
0.214990129598681));
#161661=CARTESIAN_POINT('Ctrl Pts',(6.66938816373354,-4.64555399194908,
0.223034095432758));
#161662=CARTESIAN_POINT('Ctrl Pts',(6.78253321612534,-4.47402846824386,
0.231078061266833));
#161663=CARTESIAN_POINT('Ctrl Pts',(6.89569459095891,-4.30247820005963,
0.239123187533125));
#161664=CARTESIAN_POINT('Ctrl Pts',(7.00234443755863,-4.12663132763536,
0.247168313799416));
#161665=CARTESIAN_POINT('Ctrl Pts',(7.10216567530887,-3.94701536391291,
0.255213440065709));
#161666=CARTESIAN_POINT('Ctrl Pts',(7.20199262453546,-3.76738912309559,
0.263259026650361));
#161667=CARTESIAN_POINT('Ctrl Pts',(7.29499003409692,-3.58399364156959,
0.271304613235014));
#161668=CARTESIAN_POINT('Ctrl Pts',(7.38088672132661,-3.39738116340285,
0.279350199819667));
#161669=CARTESIAN_POINT('Ctrl Pts',(7.46682099106362,-3.21068703639666,
0.287399306601971));
#161670=CARTESIAN_POINT('Ctrl Pts',(7.54564819953609,-3.02077339122527,
0.295448413384275));
#161671=CARTESIAN_POINT('Ctrl Pts',(7.61714485605674,-2.82821353584703,
0.303497520166579));
#161672=CARTESIAN_POINT('Ctrl Pts',(7.65811538880073,-2.71786879745113,
0.308109990302005));
#161673=CARTESIAN_POINT('Ctrl Pts',(7.69667963643193,-2.60665545684858,
0.31272246043743));
#161674=CARTESIAN_POINT('Ctrl Pts',(7.73280286670624,-2.49468382508883,
0.317334930572856));
#161675=CARTESIAN_POINT('Ctrl Pts',(7.80025255645084,-2.2856091724334,0.325947385140962));
#161676=CARTESIAN_POINT('Ctrl Pts',(7.85920825178188,-2.07383061034273,
0.33455983970907));
#161677=CARTESIAN_POINT('Ctrl Pts',(7.90948727930528,-1.86002648932964,
0.343172294277177));
#161678=CARTESIAN_POINT('Ctrl Pts',(7.95976819968273,-1.64621431923495,
0.351785073078274));
#161679=CARTESIAN_POINT('Ctrl Pts',(8.001371750913,-1.4303766624732,0.360397851879371));
#161680=CARTESIAN_POINT('Ctrl Pts',(8.03416612107553,-1.21320332239168,
0.369010630680469));
#161681=CARTESIAN_POINT('Ctrl Pts',(8.0669557889288,-0.996061122295518,
0.377622174515039));
#161682=CARTESIAN_POINT('Ctrl Pts',(8.09093876693625,-0.777583848880212,
0.386233718349605));
#161683=CARTESIAN_POINT('Ctrl Pts',(8.1060347856621,-0.558468992994177,
0.394845262184174));
#161684=CARTESIAN_POINT('Ctrl Pts',(8.11880671657131,-0.373087678133646,
0.402131027051992));
#161685=CARTESIAN_POINT('Ctrl Pts',(8.12521827829703,-0.187250194103663,
0.40941679191981));
#161686=CARTESIAN_POINT('Ctrl Pts',(8.12524988254124,-0.0013815801172392,
0.416702556787628));
#161687=CARTESIAN_POINT('',(-2.1020845102162,-7.84862588447233,0.));
#161688=CARTESIAN_POINT('Origin',(0.,0.,0.));
#161689=CARTESIAN_POINT('',(8.13159794993462,0.00671758913419385,0.583297443212405));
#161690=CARTESIAN_POINT('Ctrl Pts',(-2.1020845102162,-7.84862588447233,
0.));
#161691=CARTESIAN_POINT('Ctrl Pts',(0.0676884603301917,-8.42975259623151,
0.0879975931412002));
#161692=CARTESIAN_POINT('Ctrl Pts',(2.47476766063835,-8.05858769184727,
0.175995186282401));
#161693=CARTESIAN_POINT('Ctrl Pts',(6.26263734649459,-5.64310942899612,
0.351990372564801));
#161694=CARTESIAN_POINT('Ctrl Pts',(7.61452387219173,-3.61722777291617,
0.439987965706001));
#161695=CARTESIAN_POINT('Ctrl Pts',(8.08425694621335,-0.941261955081332,
0.546422853635602));
#161696=CARTESIAN_POINT('Ctrl Pts',(8.12525000000002,-0.470634548223924,
0.564860148424005));
#161697=CARTESIAN_POINT('Ctrl Pts',(8.12525,4.45453585155269E-13,0.583297443212406));
#161698=CARTESIAN_POINT('',(8.13064101234911,-0.00726150239757081,2.58329744321241));
#161699=CARTESIAN_POINT('Ctrl Pts',(8.1326776545346,0.00786016460551604,
0.583297443212405));
#161700=CARTESIAN_POINT('Ctrl Pts',(8.13566645843386,0.371006238495569,
0.597588802946333));
#161701=CARTESIAN_POINT('Ctrl Pts',(7.9488919173957,3.41866176301992,0.717658472871213));
#161702=CARTESIAN_POINT('Ctrl Pts',(4.99171475646078,7.44423893657555,0.890617297891568));
#161703=CARTESIAN_POINT('Ctrl Pts',(-0.510988490918925,8.4371067902629,
1.10217391827347));
#161704=CARTESIAN_POINT('Ctrl Pts',(-4.47752894352082,7.19508636046628,
1.2608413835599));
#161705=CARTESIAN_POINT('Ctrl Pts',(-7.3764386431641,4.16414405786186,1.41950884884633));
#161706=CARTESIAN_POINT('Ctrl Pts',(-8.46487839372028,0.136812730728797,
1.57817631413276));
#161707=CARTESIAN_POINT('Ctrl Pts',(-7.50785040472005,-3.92613790885581,
1.73684377941919));
#161708=CARTESIAN_POINT('Ctrl Pts',(-4.70369331913998,-7.04503919375124,
1.89551124470561));
#161709=CARTESIAN_POINT('Ctrl Pts',(-0.787795848183251,-8.4201070003184,
2.05417870999205));
#161710=CARTESIAN_POINT('Ctrl Pts',(4.76217654495408,-7.59287955017986,
2.26573533037394));
#161711=CARTESIAN_POINT('Ctrl Pts',(7.88034319623104,-3.60392890592102,
2.44210824144741));
#161712=CARTESIAN_POINT('Ctrl Pts',(8.13264513995538,-0.45895858051545,
2.56559199742538));
#161713=CARTESIAN_POINT('Ctrl Pts',(8.13064101234911,-0.00726150239757081,
2.58329744321241));
#161714=CARTESIAN_POINT('',(8.1252498612179,0.00150175848002178,4.58329744319216));
#161715=CARTESIAN_POINT('Ctrl Pts',(8.12524675951605,-0.00725668477251276,
2.58329744321241));
#161716=CARTESIAN_POINT('Ctrl Pts',(8.12542154448592,0.188448524219183,
2.59097374895978));
#161717=CARTESIAN_POINT('Ctrl Pts',(8.11852158023305,0.384406059005546,
2.59865005470714));
#161718=CARTESIAN_POINT('Ctrl Pts',(8.10451899472242,0.580051227637208,
2.6063263604545));
#161719=CARTESIAN_POINT('Ctrl Pts',(8.0905296202666,0.775511810426265,2.61399542381825));
#161720=CARTESIAN_POINT('Ctrl Pts',(8.06945100009161,0.970660258994976,
2.621664487182));
#161721=CARTESIAN_POINT('Ctrl Pts',(8.04130730329936,1.16493107796317,2.62933355054574));
#161722=CARTESIAN_POINT('Ctrl Pts',(8.0131790158619,1.35909552895852,2.63699841491178));
#161723=CARTESIAN_POINT('Ctrl Pts',(7.97799340247663,1.55238295358604,2.64466327927782));
#161724=CARTESIAN_POINT('Ctrl Pts',(7.93582655914097,1.74423174656718,2.65232814364386));
#161725=CARTESIAN_POINT('Ctrl Pts',(7.89367489297021,1.93601148717118,2.65999024918563));
#161726=CARTESIAN_POINT('Ctrl Pts',(7.8445470758866,2.12635327763722,2.66765235472741));
#161727=CARTESIAN_POINT('Ctrl Pts',(7.78857053785034,2.31470441729168,2.67531446026918));
#161728=CARTESIAN_POINT('Ctrl Pts',(7.75561211810127,2.42560366434635,2.67982583055871));
#161729=CARTESIAN_POINT('Ctrl Pts',(7.72028039636842,2.53581298880038,2.68433720084825));
#161730=CARTESIAN_POINT('Ctrl Pts',(7.68260957495565,2.64522166959591,2.68884857113778));
#161731=CARTESIAN_POINT('Ctrl Pts',(7.61549722361775,2.84013841283621,2.69688579083545));
#161732=CARTESIAN_POINT('Ctrl Pts',(7.54098955720979,3.0324221846715,2.70492301053312));
#161733=CARTESIAN_POINT('Ctrl Pts',(7.45932971704242,3.22150395544501,2.7129602302308));
#161734=CARTESIAN_POINT('Ctrl Pts',(7.37762037695026,3.41070034233108,2.7210023218676));
#161735=CARTESIAN_POINT('Ctrl Pts',(7.28875033878966,3.5966905659627,2.7290444135044));
#161736=CARTESIAN_POINT('Ctrl Pts',(7.19300957783444,3.7789285221716,2.7370865051412));
#161737=CARTESIAN_POINT('Ctrl Pts',(7.09719909448777,3.96129919161561,2.74513445336255));
#161738=CARTESIAN_POINT('Ctrl Pts',(6.99450805242976,4.13991186269587,2.7531824015839));
#161739=CARTESIAN_POINT('Ctrl Pts',(6.88527107355487,4.31424730470665,2.76123034980525));
#161740=CARTESIAN_POINT('Ctrl Pts',(6.77587284440087,4.48884009216008,2.76929017801368));
#161741=CARTESIAN_POINT('Ctrl Pts',(6.6599095335933,4.65914276345852,2.7773500062221));
#161742=CARTESIAN_POINT('Ctrl Pts',(6.53775860245799,4.82466579345,2.78540983443052));
#161743=CARTESIAN_POINT('Ctrl Pts',(6.41550865653361,4.99032299538556,2.79347619588583));
#161744=CARTESIAN_POINT('Ctrl Pts',(6.28706127770004,5.1511925781628,2.80154255734113));
#161745=CARTESIAN_POINT('Ctrl Pts',(6.1528330915265,5.30681943449336,2.80960891879644));
#161746=CARTESIAN_POINT('Ctrl Pts',(6.01839397508925,5.46269084761026,2.81768795597804));
#161747=CARTESIAN_POINT('Ctrl Pts',(5.87815610848054,5.61330283573933,2.82576699315964));
#161748=CARTESIAN_POINT('Ctrl Pts',(5.73257296564144,5.75823712225338,2.83384603034124));
#161749=CARTESIAN_POINT('Ctrl Pts',(5.65046242022818,5.83998170533265,2.83840269903555));
#161750=CARTESIAN_POINT('Ctrl Pts',(5.56665210613339,5.91992088417901,2.84295936772987));
#161751=CARTESIAN_POINT('Ctrl Pts',(5.48122781329227,5.99798543023332,2.84751603642419));
#161752=CARTESIAN_POINT('Ctrl Pts',(5.32963895041481,6.13651412475151,2.85560202932981));
#161753=CARTESIAN_POINT('Ctrl Pts',(5.17267087758265,6.26940683553619,2.86368802223543));
#161754=CARTESIAN_POINT('Ctrl Pts',(5.0107695065041,6.39623924780716,2.87177401514105));
#161755=CARTESIAN_POINT('Ctrl Pts',(4.84901262311636,6.52295846942231,2.87985279176162));
#161756=CARTESIAN_POINT('Ctrl Pts',(4.68233146822159,6.64362798204878,2.8879315683822));
#161757=CARTESIAN_POINT('Ctrl Pts',(4.51120663100571,6.75786225776097,2.89601034500277));
#161758=CARTESIAN_POINT('Ctrl Pts',(4.34021113449181,6.87201019217021,2.90408301546917));
#161759=CARTESIAN_POINT('Ctrl Pts',(4.16477891564455,6.97973241345168,2.91215568593557));
#161760=CARTESIAN_POINT('Ctrl Pts',(3.98542178030168,7.08068505129249,2.92022835640197));
#161761=CARTESIAN_POINT('Ctrl Pts',(3.80617574113922,7.18157515773501,2.92829602654958));
#161762=CARTESIAN_POINT('Ctrl Pts',(3.62300990922674,7.27570388805911,2.93636369669719));
#161763=CARTESIAN_POINT('Ctrl Pts',(3.43646360804606,7.3627715863712,2.94443136684479));
#161764=CARTESIAN_POINT('Ctrl Pts',(3.25000744004199,7.44979721637006,2.9524951389535));
#161765=CARTESIAN_POINT('Ctrl Pts',(3.06017434701721,7.52976848513044,2.96055891106221));
#161766=CARTESIAN_POINT('Ctrl Pts',(2.8675272614942,7.60243217444836,2.96862268317092));
#161767=CARTESIAN_POINT('Ctrl Pts',(2.67219473769384,7.67610877217409,2.97679886166368));
#161768=CARTESIAN_POINT('Ctrl Pts',(2.47396947892957,7.74227239099172,2.98497504015643));
#161769=CARTESIAN_POINT('Ctrl Pts',(2.27345940018541,7.80070957786589,2.99315121864919));
#161770=CARTESIAN_POINT('Ctrl Pts',(2.07579972660383,7.85831603513186,3.00121116646899));
#161771=CARTESIAN_POINT('Ctrl Pts',(1.87592007785936,7.9084141940002,3.0092711142888));
#161772=CARTESIAN_POINT('Ctrl Pts',(1.67441853426039,7.9508496485989,3.0173310621086));
#161773=CARTESIAN_POINT('Ctrl Pts',(1.47292674455366,7.99328304906519,3.02539061977823));
#161774=CARTESIAN_POINT('Ctrl Pts',(1.26981352658252,8.02805441989696,3.03345017744786));
#161775=CARTESIAN_POINT('Ctrl Pts',(1.06568788024979,8.0550603290347,3.04150973511749));
#161776=CARTESIAN_POINT('Ctrl Pts',(0.861546829722573,8.08206827615388,
3.04956990099582));
#161777=CARTESIAN_POINT('Ctrl Pts',(0.656393512582881,8.10130955180625,
3.05763006687415));
#161778=CARTESIAN_POINT('Ctrl Pts',(0.45084339107128,8.11273244962678,3.06569023275248));
#161779=CARTESIAN_POINT('Ctrl Pts',(0.240110538496967,8.12444336385385,
3.07395362727286));
#161780=CARTESIAN_POINT('Ctrl Pts',(0.0289609577969593,8.12793642602925,
3.08221702179324));
#161781=CARTESIAN_POINT('Ctrl Pts',(-0.181940457436845,8.12321274080937,
3.09048041631362));
#161782=CARTESIAN_POINT('Ctrl Pts',(-0.387824207660257,8.11860143923576,
3.09854721212694));
#161783=CARTESIAN_POINT('Ctrl Pts',(-0.593471145601391,8.1061599576421,
3.10661400794026));
#161784=CARTESIAN_POINT('Ctrl Pts',(-0.798266002813213,8.08594205712931,
3.11468080375358));
#161785=CARTESIAN_POINT('Ctrl Pts',(-1.01054755085099,8.06498505031108,
3.12304249762749));
#161786=CARTESIAN_POINT('Ctrl Pts',(-1.22191317306984,8.0356723877964,3.1314041915014));
#161787=CARTESIAN_POINT('Ctrl Pts',(-1.4316867562105,7.99812231680608,3.13976588537531));
#161788=CARTESIAN_POINT('Ctrl Pts',(-1.64146033935117,7.96057224581576,
3.14812757924922));
#161789=CARTESIAN_POINT('Ctrl Pts',(-1.84964152006452,7.91478487093404,
3.15648927312313));
#161790=CARTESIAN_POINT('Ctrl Pts',(-2.05556894582339,7.86093657724488,
3.16485096699704));
#161791=CARTESIAN_POINT('Ctrl Pts',(-2.24220479106239,7.81213286996637,
3.17242932523678));
#161792=CARTESIAN_POINT('Ctrl Pts',(-2.42736339181452,7.75660979140615,
3.18000768347651));
#161793=CARTESIAN_POINT('Ctrl Pts',(-2.6105035175124,7.69447587217969,3.18758604171625));
#161794=CARTESIAN_POINT('Ctrl Pts',(-2.79350736016814,7.6323881896777,3.19515876054894));
#161795=CARTESIAN_POINT('Ctrl Pts',(-2.97449537018565,7.56369957030046,
3.20273147938162));
#161796=CARTESIAN_POINT('Ctrl Pts',(-3.15293799653857,7.48856925937681,
3.21030419821431));
#161797=CARTESIAN_POINT('Ctrl Pts',(-3.33128172004362,7.41348058985838,
3.21787271982421));
#161798=CARTESIAN_POINT('Ctrl Pts',(-3.50708252961938,7.33195747540202,
3.2254412414341));
#161799=CARTESIAN_POINT('Ctrl Pts',(-3.67982755711192,7.24420849454374,
3.233009763044));
#161800=CARTESIAN_POINT('Ctrl Pts',(-3.85253083465313,7.15648072133313,
3.24057645545271));
#161801=CARTESIAN_POINT('Ctrl Pts',(-4.02217946920668,7.06253023576544,
3.24814314786142));
#161802=CARTESIAN_POINT('Ctrl Pts',(-4.18828193421433,6.96261315901105,
3.25570984027014));
#161803=CARTESIAN_POINT('Ctrl Pts',(-4.35435492833486,6.86271381013861,
3.26327519015128));
#161804=CARTESIAN_POINT('Ctrl Pts',(-4.51688269178376,6.75685016943834,
3.27084054003243));
#161805=CARTESIAN_POINT('Ctrl Pts',(-4.67539985699655,6.64532344883954,
3.27840588991358));
#161806=CARTESIAN_POINT('Ctrl Pts',(-4.8339721285435,6.53375795749484,3.2859738697856));
#161807=CARTESIAN_POINT('Ctrl Pts',(-4.98853071348142,6.41652566237355,
3.29354184965763));
#161808=CARTESIAN_POINT('Ctrl Pts',(-5.13864032618363,6.29397038129505,
3.30110982952966));
#161809=CARTESIAN_POINT('Ctrl Pts',(-5.28679728649344,6.17300932098956,
3.30857936378094));
#161810=CARTESIAN_POINT('Ctrl Pts',(-5.4306200820621,6.04686317803796,3.31604889803221));
#161811=CARTESIAN_POINT('Ctrl Pts',(-5.56972346001078,5.9158996054282,3.32351843228349));
#161812=CARTESIAN_POINT('Ctrl Pts',(-5.74302290330132,5.75274099232116,
3.33282421727933));
#161813=CARTESIAN_POINT('Ctrl Pts',(-5.90891371658913,5.58218701785903,
3.34213000227518));
#161814=CARTESIAN_POINT('Ctrl Pts',(-6.06686896837867,5.40488561239032,
3.35143578727102));
#161815=CARTESIAN_POINT('Ctrl Pts',(-6.22567219020883,5.22663237861395,
3.36079152962372));
#161816=CARTESIAN_POINT('Ctrl Pts',(-6.37645442877942,5.04155914313817,
3.37014727197641));
#161817=CARTESIAN_POINT('Ctrl Pts',(-6.51872615786608,4.85035017717819,
3.37950301432911));
#161818=CARTESIAN_POINT('Ctrl Pts',(-6.66168851444334,4.65821302844297,
3.38890417211962));
#161819=CARTESIAN_POINT('Ctrl Pts',(-6.79605753013016,4.45988048359757,
3.39830532991012));
#161820=CARTESIAN_POINT('Ctrl Pts',(-6.92138273540747,4.25607196749578,
3.40770648770062));
#161821=CARTESIAN_POINT('Ctrl Pts',(-7.04684359176357,4.05204285055782,
3.41711782123505));
#161822=CARTESIAN_POINT('Ctrl Pts',(-7.16324104757251,3.84252594413645,
3.42652915476948));
#161823=CARTESIAN_POINT('Ctrl Pts',(-7.27016938693719,3.62826744435155,
3.4359404883039));
#161824=CARTESIAN_POINT('Ctrl Pts',(-7.37697234794513,3.41426017243366,
3.44534078662035));
#161825=CARTESIAN_POINT('Ctrl Pts',(-7.47432837298677,3.19552245461012,
3.4547410849368));
#161826=CARTESIAN_POINT('Ctrl Pts',(-7.56187933311759,2.97282164178563,
3.46414138325324));
#161827=CARTESIAN_POINT('Ctrl Pts',(-7.61789934795596,2.83032517092681,
3.47015622135879));
#161828=CARTESIAN_POINT('Ctrl Pts',(-7.66990594206708,2.68620662287665,
3.47617105946434));
#161829=CARTESIAN_POINT('Ctrl Pts',(-7.71781530533523,2.54067205188572,
3.48218589756989));
#161830=CARTESIAN_POINT('Ctrl Pts',(-7.77948397067406,2.35334076335584,
3.489928163651));
#161831=CARTESIAN_POINT('Ctrl Pts',(-7.8343900712243,2.16357430055282,3.49767042973211));
#161832=CARTESIAN_POINT('Ctrl Pts',(-7.88233822795875,1.97191065278325,
3.50541269581321));
#161833=CARTESIAN_POINT('Ctrl Pts',(-7.93025651605203,1.78036639923259,
3.51315013895673));
#161834=CARTESIAN_POINT('Ctrl Pts',(-7.97122540513269,1.58692765514176,
3.52088758210024));
#161835=CARTESIAN_POINT('Ctrl Pts',(-8.00509898102066,1.39214865102903,
3.52862502524376));
#161836=CARTESIAN_POINT('Ctrl Pts',(-8.03895747624439,1.19745636338144,
3.53635902364373));
#161837=CARTESIAN_POINT('Ctrl Pts',(-8.06572688911408,1.0014253514074,3.54409302204369));
#161838=CARTESIAN_POINT('Ctrl Pts',(-8.08531212440768,0.804621285702891,
3.55182702044366));
#161839=CARTESIAN_POINT('Ctrl Pts',(-8.10489485293535,0.607842409469903,
3.55956002894876));
#161840=CARTESIAN_POINT('Ctrl Pts',(-8.11729519281468,0.410291027156225,
3.56729303745387));
#161841=CARTESIAN_POINT('Ctrl Pts',(-8.12246972851236,0.212539577256358,
3.57502604595898));
#161842=CARTESIAN_POINT('Ctrl Pts',(-8.12764374719607,0.0148078857019956,
3.58275828182018));
#161843=CARTESIAN_POINT('Ctrl Pts',(-8.12559339413814,-0.183123480250224,
3.59049051768137));
#161844=CARTESIAN_POINT('Ctrl Pts',(-8.11632736431311,-0.380680545605153,
3.59822275354257));
#161845=CARTESIAN_POINT('Ctrl Pts',(-8.10705777033334,-0.578313600781254,
3.60595796358856));
#161846=CARTESIAN_POINT('Ctrl Pts',(-8.09056697090893,-0.775571714409861,
3.61369317363456));
#161847=CARTESIAN_POINT('Ctrl Pts',(-8.06691572793074,-0.971883841291524,
3.62142838368055));
#161848=CARTESIAN_POINT('Ctrl Pts',(-8.04711773496089,-1.13621288359535,
3.62790337673915));
#161849=CARTESIAN_POINT('Ctrl Pts',(-8.02230332607686,-1.29987903084078,
3.63437836979774));
#161850=CARTESIAN_POINT('Ctrl Pts',(-7.99253584895792,-1.46255197022961,
3.64085336285634));
#161851=CARTESIAN_POINT('Ctrl Pts',(-7.95385356750799,-1.67394242164687,
3.64926749559853));
#161852=CARTESIAN_POINT('Ctrl Pts',(-7.90678791254452,-1.88375739966851,
3.65768162834072));
#161853=CARTESIAN_POINT('Ctrl Pts',(-7.85149466753507,-2.09134383786319,
3.66609576108292));
#161854=CARTESIAN_POINT('Ctrl Pts',(-7.79618597220823,-2.29898828090738,
3.67451224494451));
#161855=CARTESIAN_POINT('Ctrl Pts',(-7.7326451652376,-2.50440268585466,
3.68292872880611));
#161856=CARTESIAN_POINT('Ctrl Pts',(-7.66107820026736,-2.70694816571879,
3.69134521266771));
#161857=CARTESIAN_POINT('Ctrl Pts',(-7.58949347906698,-2.90954389843566,
3.69976378471378));
#161858=CARTESIAN_POINT('Ctrl Pts',(-7.50987871227754,-3.10926903617535,
3.70818235675984));
#161859=CARTESIAN_POINT('Ctrl Pts',(-7.42248876835383,-3.30550269190046,
3.7166009288059));
#161860=CARTESIAN_POINT('Ctrl Pts',(-7.33506525103029,-3.50181173651689,
3.72502273509235));
#161861=CARTESIAN_POINT('Ctrl Pts',(-7.2398606936539,-3.69462637691134,
3.73344454137879));
#161862=CARTESIAN_POINT('Ctrl Pts',(-7.13717749240084,-3.88334713932026,
3.74186634766523));
#161863=CARTESIAN_POINT('Ctrl Pts',(-7.03448315831298,-4.0720883626911,
3.75028906703752));
#161864=CARTESIAN_POINT('Ctrl Pts',(-6.92430869024064,-4.25673459147822,
3.75871178640981));
#161865=CARTESIAN_POINT('Ctrl Pts',(-6.80700198349754,-4.43671179581913,
3.76713450578211));
#161866=CARTESIAN_POINT('Ctrl Pts',(-6.68967297221502,-4.61672322078355,
3.77555882663893));
#161867=CARTESIAN_POINT('Ctrl Pts',(-6.56520915723441,-4.79206362670022,
3.78398314749575));
#161868=CARTESIAN_POINT('Ctrl Pts',(-6.43400195451774,-4.96218766390005,
3.79240746835257));
#161869=CARTESIAN_POINT('Ctrl Pts',(-6.39707221043305,-5.01007098910143,
3.79477858828264));
#161870=CARTESIAN_POINT('Ctrl Pts',(-6.35960850789623,-5.05754125858306,
3.79714970821271));
#161871=CARTESIAN_POINT('Ctrl Pts',(-6.32162016755184,-5.10458676287335,
3.79952082814277));
#161872=CARTESIAN_POINT('Ctrl Pts',(-6.18665249013186,-5.27173337653293,
3.80794511167146));
#161873=CARTESIAN_POINT('Ctrl Pts',(-6.04504535410084,-5.43353292673586,
3.81636939520014));
#161874=CARTESIAN_POINT('Ctrl Pts',(-5.89723839174989,-5.58947823265921,
3.82479367872883));
#161875=CARTESIAN_POINT('Ctrl Pts',(-5.74945698348554,-5.74539657747201,
3.8332165057979));
#161876=CARTESIAN_POINT('Ctrl Pts',(-5.59547807123916,-5.89546250807257,
3.84163933286698));
#161877=CARTESIAN_POINT('Ctrl Pts',(-5.43577928233965,-6.03920451352552,
3.85006215993605));
#161878=CARTESIAN_POINT('Ctrl Pts',(-5.27611313587101,-6.18291713811398,
3.85848326537936));
#161879=CARTESIAN_POINT('Ctrl Pts',(-5.11072964350834,-6.32030824234214,
3.86690437082266));
#161880=CARTESIAN_POINT('Ctrl Pts',(-4.94014156378475,-6.45094480617114,
3.87532547626597));
#161881=CARTESIAN_POINT('Ctrl Pts',(-4.76960134775628,-6.58154471592282,
3.88374421891098));
#161882=CARTESIAN_POINT('Ctrl Pts',(-4.59385967038434,-6.70539371012401,
3.89216296155599));
#161883=CARTESIAN_POINT('Ctrl Pts',(-4.41346127678764,-6.82209990551267,
3.90058170420101));
#161884=CARTESIAN_POINT('Ctrl Pts',(-4.23311327418162,-6.93877350116091,
3.90899809522429));
#161885=CARTESIAN_POINT('Ctrl Pts',(-4.04811137390595,-7.04830813839393,
3.91741448624758));
#161886=CARTESIAN_POINT('Ctrl Pts',(-3.85902909530774,-7.15035537606826,
3.92583087727086));
#161887=CARTESIAN_POINT('Ctrl Pts',(-3.67001543178216,-7.25236558235776,
3.93424421411432));
#161888=CARTESIAN_POINT('Ctrl Pts',(-3.47692457894577,-7.34689368975686,
3.94265755095777));
#161889=CARTESIAN_POINT('Ctrl Pts',(-3.28035530375629,-7.43363683829241,
3.95107088780122));
#161890=CARTESIAN_POINT('Ctrl Pts',(-3.2249249280901,-7.4580974530307,3.95344335634387));
#161891=CARTESIAN_POINT('Ctrl Pts',(-3.16921810209201,-7.48193930733348,
3.95581582488653));
#161892=CARTESIAN_POINT('Ctrl Pts',(-3.11324858489207,-7.50515628159518,
3.95818829342918));
#161893=CARTESIAN_POINT('Ctrl Pts',(-2.93076550130723,-7.58085293339315,
3.96592349282039));
#161894=CARTESIAN_POINT('Ctrl Pts',(-2.74540735442137,-7.64993685540819,
3.97365869221159));
#161895=CARTESIAN_POINT('Ctrl Pts',(-2.5577036049958,-7.7121877461257,3.9813938916028));
#161896=CARTESIAN_POINT('Ctrl Pts',(-2.37005789584823,-7.7744193881121,
3.98912669917645));
#161897=CARTESIAN_POINT('Ctrl Pts',(-2.1800683634462,-7.82982209529938,
3.99685950675011));
#161898=CARTESIAN_POINT('Ctrl Pts',(-1.98828263028762,-7.87822440303629,
4.00459231432376));
#161899=CARTESIAN_POINT('Ctrl Pts',(-1.79652212509887,-7.92662034381389,
4.01232410470477));
#161900=CARTESIAN_POINT('Ctrl Pts',(-1.60296623243336,-7.96801763365407,
4.02005589508579));
#161901=CARTESIAN_POINT('Ctrl Pts',(-1.40817598455326,-8.0022951682019,
4.0277876854668));
#161902=CARTESIAN_POINT('Ctrl Pts',(-1.2133160332439,-8.0365849685676,4.03552224257926));
#161903=CARTESIAN_POINT('Ctrl Pts',(-1.0172211918205,-8.06374985805016,
4.04325679969172));
#161904=CARTESIAN_POINT('Ctrl Pts',(-0.820461557063465,-8.08372008396388,
4.05099135680417));
#161905=CARTESIAN_POINT('Ctrl Pts',(-0.623668690312049,-8.1036936827769,
4.0587272202555));
#161906=CARTESIAN_POINT('Ctrl Pts',(-0.426211158872913,-8.11647016867068,
4.06646308370682));
#161907=CARTESIAN_POINT('Ctrl Pts',(-0.22866254125838,-8.1220318273647,
4.07419894715815));
#161908=CARTESIAN_POINT('Ctrl Pts',(-0.0309522798858196,-8.12759803687474,
4.08194114046414));
#161909=CARTESIAN_POINT('Ctrl Pts',(0.166848862963725,-8.1259376218865,
4.08968333377014));
#161910=CARTESIAN_POINT('Ctrl Pts',(0.36416801257101,-8.11708501995144,
4.09742552707613));
#161911=CARTESIAN_POINT('Ctrl Pts',(0.529235654785898,-8.10967936200189,
4.10390227095596));
#161912=CARTESIAN_POINT('Ctrl Pts',(0.693965924963077,-8.09724141428031,
4.1103790148358));
#161913=CARTESIAN_POINT('Ctrl Pts',(0.858027275555607,-8.07981910421902,
4.11685575871563));
#161914=CARTESIAN_POINT('Ctrl Pts',(1.09608684901361,-8.05453863635218,
4.12625377281134));
#161915=CARTESIAN_POINT('Ctrl Pts',(1.33287327577442,-8.01874928881438,
4.13565178690704));
#161916=CARTESIAN_POINT('Ctrl Pts',(1.56755319678678,-7.97260713554503,
4.14504980100275));
#161917=CARTESIAN_POINT('Ctrl Pts',(1.80256702990828,-7.9263993293487,4.15446118697405));
#161918=CARTESIAN_POINT('Ctrl Pts',(2.0354683253152,-7.86980925921721,4.16387257294536));
#161919=CARTESIAN_POINT('Ctrl Pts',(2.26543342217421,-7.80304421185707,
4.17328395891666));
#161920=CARTESIAN_POINT('Ctrl Pts',(2.49505226591476,-7.7363796910819,4.18268117438215));
#161921=CARTESIAN_POINT('Ctrl Pts',(2.72174371303819,-7.65957082634099,
4.19207838984764));
#161922=CARTESIAN_POINT('Ctrl Pts',(2.94470151255391,-7.57287399634133,
4.20147560531313));
#161923=CARTESIAN_POINT('Ctrl Pts',(3.16709693949201,-7.48639584413569,
4.2108491179241));
#161924=CARTESIAN_POINT('Ctrl Pts',(3.38577748706466,-7.39007953936429,
4.22022263053508));
#161925=CARTESIAN_POINT('Ctrl Pts',(3.59995718815401,-7.28422925270466,
4.22959614314606));
#161926=CARTESIAN_POINT('Ctrl Pts',(3.81274604645226,-7.17906633794529,
4.23890878592495));
#161927=CARTESIAN_POINT('Ctrl Pts',(4.02109227437145,-7.0644928636502,4.24822142870384));
#161928=CARTESIAN_POINT('Ctrl Pts',(4.22423981990064,-6.94085625167859,
4.25753407148273));
#161929=CARTESIAN_POINT('Ctrl Pts',(4.35504594612473,-6.86124698921201,
4.26353045565584));
#161930=CARTESIAN_POINT('Ctrl Pts',(4.48369697723611,-6.77788110845369,
4.26952683982893));
#161931=CARTESIAN_POINT('Ctrl Pts',(4.60999450977774,-6.69086228989352,
4.27552322400203));
#161932=CARTESIAN_POINT('Ctrl Pts',(4.76938668679867,-6.58104130881041,
4.28309088354668));
#161933=CARTESIAN_POINT('Ctrl Pts',(4.9249653082953,-6.46544311001104,4.29065854309133));
#161934=CARTESIAN_POINT('Ctrl Pts',(5.07627240430222,-6.34437909017263,
4.29822620263598));
#161935=CARTESIAN_POINT('Ctrl Pts',(5.22753760620868,-6.22334859069344,
4.30579176683747));
#161936=CARTESIAN_POINT('Ctrl Pts',(5.37453334913977,-6.09685551090348,
4.31335733103895));
#161937=CARTESIAN_POINT('Ctrl Pts',(5.51683266023166,-5.96525313473798,
4.32092289524044));
#161938=CARTESIAN_POINT('Ctrl Pts',(5.65911950465485,-5.83366228809579,
4.32848779663209));
#161939=CARTESIAN_POINT('Ctrl Pts',(5.7967104668374,-5.69696328627307,4.33605269802375));
#161940=CARTESIAN_POINT('Ctrl Pts',(5.92921359509749,-5.55554801133166,
4.34361759941541));
#161941=CARTESIAN_POINT('Ctrl Pts',(6.06178175514736,-5.41406333056902,
4.3511862136181));
#161942=CARTESIAN_POINT('Ctrl Pts',(6.18925683847888,-5.26785801880553,
4.35875482782079));
#161943=CARTESIAN_POINT('Ctrl Pts',(6.31128517599999,-5.11735937664171,
4.36632344202348));
#161944=CARTESIAN_POINT('Ctrl Pts',(6.43334065053819,-4.96682726615152,
4.37389373935664));
#161945=CARTESIAN_POINT('Ctrl Pts',(6.54994674376694,-4.81200021614064,
4.3814640366898));
#161946=CARTESIAN_POINT('Ctrl Pts',(6.66079187115985,-4.65333635272488,
4.38903433402297));
#161947=CARTESIAN_POINT('Ctrl Pts',(6.77174931625615,-4.49451171759845,
4.39661230222476));
#161948=CARTESIAN_POINT('Ctrl Pts',(6.87693393149166,-4.33184280958211,
4.40419027042654));
#161949=CARTESIAN_POINT('Ctrl Pts',(6.97607856849142,-4.16581509055967,
4.41176823862833));
#161950=CARTESIAN_POINT('Ctrl Pts',(7.07386492635362,-4.00206194728666,
4.41924238884839));
#161951=CARTESIAN_POINT('Ctrl Pts',(7.16577564216525,-3.83504176562554,
4.42671653906844));
#161952=CARTESIAN_POINT('Ctrl Pts',(7.25159989324019,-3.66524031283883,
4.43419068928849));
#161953=CARTESIAN_POINT('Ctrl Pts',(7.35155880230678,-3.46747374026879,
4.44289578013214));
#161954=CARTESIAN_POINT('Ctrl Pts',(7.44343978347571,-3.26558398144789,
4.4516008709758));
#161955=CARTESIAN_POINT('Ctrl Pts',(7.52693546046989,-3.0602173348344,4.46030596181945));
#161956=CARTESIAN_POINT('Ctrl Pts',(7.61036495209151,-2.85501347830184,
4.46900415230968));
#161957=CARTESIAN_POINT('Ctrl Pts',(7.6854223337838,-2.64633843566982,4.47770234279992));
#161958=CARTESIAN_POINT('Ctrl Pts',(7.75184816053937,-2.4348588580126,4.48640053329015));
#161959=CARTESIAN_POINT('Ctrl Pts',(7.81816189742858,-2.22373614031112,
4.49508404607056));
#161960=CARTESIAN_POINT('Ctrl Pts',(7.87587310579198,-2.00981854287022,
4.50376755885097));
#161961=CARTESIAN_POINT('Ctrl Pts',(7.92477200248283,-1.79378824590983,
4.51245107163138));
#161962=CARTESIAN_POINT('Ctrl Pts',(7.97360943000941,-1.57802951339587,
4.52112366865889));
#161963=CARTESIAN_POINT('Ctrl Pts',(8.01365661180745,-1.36016359039827,
4.5297962656864));
#161964=CARTESIAN_POINT('Ctrl Pts',(8.04475399050408,-1.14088596922243,
4.53846886271391));
#161965=CARTESIAN_POINT('Ctrl Pts',(8.07577958197994,-0.922114542834185,
4.54712143935181));
#161966=CARTESIAN_POINT('Ctrl Pts',(8.09789658457935,-0.701938135039435,
4.5557740159897));
#161967=CARTESIAN_POINT('Ctrl Pts',(8.1109967727298,-0.481060199212926,
4.56442659262759));
#161968=CARTESIAN_POINT('Ctrl Pts',(8.1205203980151,-0.320485505899887,
4.57071687614912));
#161969=CARTESIAN_POINT('Ctrl Pts',(8.12527962600337,-0.159540328021134,
4.57700715967064));
#161970=CARTESIAN_POINT('Ctrl Pts',(8.1252498612179,0.00150175848001979,
4.58329744319216));
#161971=CARTESIAN_POINT('',(8.12524931639108,0.00333301459649942,6.58329744321241));
#161972=CARTESIAN_POINT('Ctrl Pts',(8.1252498612178,0.00150175899845503,
4.58329744321241));
#161973=CARTESIAN_POINT('Ctrl Pts',(8.12521061695668,0.213832384326663,
4.59159105057079));
#161974=CARTESIAN_POINT('Ctrl Pts',(8.11684406997655,0.426046074186561,
4.59988465792917));
#161975=CARTESIAN_POINT('Ctrl Pts',(8.10020335251704,0.637489772758512,
4.60817826528755));
#161976=CARTESIAN_POINT('Ctrl Pts',(8.08354769346874,0.849123325211606,
4.61647931942044));
#161977=CARTESIAN_POINT('Ctrl Pts',(8.05860305086515,1.05998522618361,4.62478037355333));
#161978=CARTESIAN_POINT('Ctrl Pts',(8.02547427528377,1.26942909185918,4.63308142768623));
#161979=CARTESIAN_POINT('Ctrl Pts',(7.99231477745251,1.47906718707278,4.64139017987179));
#161980=CARTESIAN_POINT('Ctrl Pts',(7.95095603491722,1.68728434421521,4.64969893205735));
#161981=CARTESIAN_POINT('Ctrl Pts',(7.90155388575722,1.89344494321196,4.65800768424292));
#161982=CARTESIAN_POINT('Ctrl Pts',(7.85207263488596,2.09993564234511,4.66632974023261));
#161983=CARTESIAN_POINT('Ctrl Pts',(7.79452229016653,2.3043629254726,4.67465179622231));
#161984=CARTESIAN_POINT('Ctrl Pts',(7.72910903618032,2.50610476024761,4.68297385221201));
#161985=CARTESIAN_POINT('Ctrl Pts',(7.66364328559863,2.70800850042935,4.69130258696451));
#161986=CARTESIAN_POINT('Ctrl Pts',(7.59030211941962,2.90722222466709,4.699631321717));
#161987=CARTESIAN_POINT('Ctrl Pts',(7.50934026374922,3.10314298183871,4.70796005646949));
#161988=CARTESIAN_POINT('Ctrl Pts',(7.42826014781913,3.29934991871097,4.71630095693047));
#161989=CARTESIAN_POINT('Ctrl Pts',(7.33953719817232,3.49225401381393,4.72464185739145));
#161990=CARTESIAN_POINT('Ctrl Pts',(7.24347352182253,3.68127408666564,4.73298275785243));
#161991=CARTESIAN_POINT('Ctrl Pts',(7.17228634393308,3.82134581889641,4.7391637118554));
#161992=CARTESIAN_POINT('Ctrl Pts',(7.0970690304504,3.95928515739477,4.74534466585837));
#161993=CARTESIAN_POINT('Ctrl Pts',(7.01796016192712,4.09486541025513,4.75152561986133));
#161994=CARTESIAN_POINT('Ctrl Pts',(6.91457202894797,4.27205653273904,4.75960356745843));
#161995=CARTESIAN_POINT('Ctrl Pts',(6.8043534006649,4.44552896342827,4.76768151505552));
#161996=CARTESIAN_POINT('Ctrl Pts',(6.68759103205316,4.61473875213994,4.77575946265262));
#161997=CARTESIAN_POINT('Ctrl Pts',(6.57097155683386,4.78374146248355,4.78382752448472));
#161998=CARTESIAN_POINT('Ctrl Pts',(6.44782448223716,4.9484916715378,4.79189558631683));
#161999=CARTESIAN_POINT('Ctrl Pts',(6.31848192230606,5.10847078488186,4.79996364814893));
#162000=CARTESIAN_POINT('Ctrl Pts',(6.18928172762075,5.26827381182556,4.80802282959699));
#162001=CARTESIAN_POINT('Ctrl Pts',(6.05389983934316,5.42331596799718,4.81608201104505));
#162002=CARTESIAN_POINT('Ctrl Pts',(5.91271140304813,5.57310787862254,4.8241411924931));
#162003=CARTESIAN_POINT('Ctrl Pts',(5.77170431816329,5.72270738698792,4.83219002221577));
#162004=CARTESIAN_POINT('Ctrl Pts',(5.62490577983017,5.86706987465934,4.84023885193844));
#162005=CARTESIAN_POINT('Ctrl Pts',(5.47273091592304,6.00573924545515,4.84828768166111));
#162006=CARTESIAN_POINT('Ctrl Pts',(5.32067115625161,6.14430372749645,4.85633042329295));
#162007=CARTESIAN_POINT('Ctrl Pts',(5.16324340916897,6.27718346434961,4.86437316492479));
#162008=CARTESIAN_POINT('Ctrl Pts',(5.00090029161773,6.40395845050526,4.87241590655662));
#162009=CARTESIAN_POINT('Ctrl Pts',(4.83868940833045,6.53063017390954,4.88045209708832));
#162010=CARTESIAN_POINT('Ctrl Pts',(4.67157138921698,6.65120687193072,4.88848828762003));
#162011=CARTESIAN_POINT('Ctrl Pts',(4.50003284081094,6.76530797481704,4.89652447815172));
#162012=CARTESIAN_POINT('Ctrl Pts',(4.40277726539928,6.82999878932741,4.90108068048374));
#162013=CARTESIAN_POINT('Ctrl Pts',(4.30410135635659,6.89260877847994,4.90563688281576));
#162014=CARTESIAN_POINT('Ctrl Pts',(4.20409836836367,6.95307446182061,4.91019308514777));
#162015=CARTESIAN_POINT('Ctrl Pts',(4.02770683320637,7.05972762211968,4.91822960025558));
#162016=CARTESIAN_POINT('Ctrl Pts',(3.84732439917407,7.15962256640634,4.9262661153634));
#162017=CARTESIAN_POINT('Ctrl Pts',(3.66350218994938,7.25247814658797,4.93430263047121));
#162018=CARTESIAN_POINT('Ctrl Pts',(3.47956893352285,7.34538982092926,4.94234400044677));
#162019=CARTESIAN_POINT('Ctrl Pts',(3.29219203813748,7.43125350482278,4.95038537042233));
#162020=CARTESIAN_POINT('Ctrl Pts',(3.10194390534103,7.50983565536674,4.9584267403979));
#162021=CARTESIAN_POINT('Ctrl Pts',(2.91155758205264,7.58847488560911,4.9664739513815));
#162022=CARTESIAN_POINT('Ctrl Pts',(2.71829615201036,7.6598219098172,4.97452116236509));
#162023=CARTESIAN_POINT('Ctrl Pts',(2.52274908496553,7.72369242116784,4.98256837334869));
#162024=CARTESIAN_POINT('Ctrl Pts',(2.32691379518903,7.78765707319537,4.99062744535975));
#162025=CARTESIAN_POINT('Ctrl Pts',(2.12878643574662,7.84412308924679,4.99868651737081));
#162026=CARTESIAN_POINT('Ctrl Pts',(1.92897034042226,7.89295641621511,5.00674558938187));
#162027=CARTESIAN_POINT('Ctrl Pts',(1.72899252394641,7.94182926643532,5.01481118400265));
#162028=CARTESIAN_POINT('Ctrl Pts',(1.52732355286919,7.98305703666817,5.02287677862344));
#162029=CARTESIAN_POINT('Ctrl Pts',(1.32457478472854,8.0165571913485,5.03094237324422));
#162030=CARTESIAN_POINT('Ctrl Pts',(1.12150765453683,8.0501099489524,5.03902063269778));
#162031=CARTESIAN_POINT('Ctrl Pts',(0.917357651253059,8.07591079719502,
5.04709889215135));
#162032=CARTESIAN_POINT('Ctrl Pts',(0.712740830625026,8.09392908733823,
5.05517715160492));
#162033=CARTESIAN_POINT('Ctrl Pts',(0.597210433682415,8.10410254329402,
5.05973828454801));
#162034=CARTESIAN_POINT('Ctrl Pts',(0.481531224403746,8.11179591523572,
5.06429941749109));
#162035=CARTESIAN_POINT('Ctrl Pts',(0.365813763653463,8.11701101716769,
5.06886055043418));
#162036=CARTESIAN_POINT('Ctrl Pts',(0.160664340009819,8.12625659815997,
5.07694674406796));
#162037=CARTESIAN_POINT('Ctrl Pts',(-0.0450043799496586,8.12772803245504,
5.08503293770174));
#162038=CARTESIAN_POINT('Ctrl Pts',(-0.250578138511302,8.1213852364606,
5.09311913133552));
#162039=CARTESIAN_POINT('Ctrl Pts',(-0.455968534985882,8.11504809794073,
5.10119811246635));
#162040=CARTESIAN_POINT('Ctrl Pts',(-0.661263823822632,8.10091063622865,
5.10927709359718));
#162041=CARTESIAN_POINT('Ctrl Pts',(-0.865847974163694,8.07898476593047,
5.117356074728));
#162042=CARTESIAN_POINT('Ctrl Pts',(-1.07027758216294,8.0570754583784,5.12542895301723));
#162043=CARTESIAN_POINT('Ctrl Pts',(-1.27399680900844,8.02738950775516,
5.13350183130646));
#162044=CARTESIAN_POINT('Ctrl Pts',(-1.47639234688607,7.98999081354642,
5.14157470959568));
#162045=CARTESIAN_POINT('Ctrl Pts',(-1.67866259284557,7.95261527080724,
5.14964259041107));
#162046=CARTESIAN_POINT('Ctrl Pts',(-1.87961047327186,7.90753656362804,
5.15771047122645));
#162047=CARTESIAN_POINT('Ctrl Pts',(-2.07862988130234,7.85487016945901,
5.16577835204184));
#162048=CARTESIAN_POINT('Ctrl Pts',(-2.27755319075201,7.80222920580345,
5.17384233719748));
#162049=CARTESIAN_POINT('Ctrl Pts',(-2.47454957933523,7.74200794346335,
5.18190632235312));
#162050=CARTESIAN_POINT('Ctrl Pts',(-2.66902456627974,7.6743726406199,5.18997030750876));
#162051=CARTESIAN_POINT('Ctrl Pts',(-2.86620213686945,7.60579742223165,
5.19814635640453));
#162052=CARTESIAN_POINT('Ctrl Pts',(-3.06078738364896,7.52960064206599,
5.20632240530029));
#162053=CARTESIAN_POINT('Ctrl Pts',(-3.25217684153511,7.44600788032639,
5.21449845419605));
#162054=CARTESIAN_POINT('Ctrl Pts',(-3.44085361458228,7.36359993210748,
5.22255861873681));
#162055=CARTESIAN_POINT('Ctrl Pts',(-3.626424296388,7.27400440932727,5.23061878327756));
#162056=CARTESIAN_POINT('Ctrl Pts',(-3.8083307277502,7.17748595474583,5.23867894781831));
#162057=CARTESIAN_POINT('Ctrl Pts',(-3.9902283702988,7.08097216345584,5.24673872293202));
#162058=CARTESIAN_POINT('Ctrl Pts',(-4.16846183575713,6.9775362560542,5.25479849804573));
#162059=CARTESIAN_POINT('Ctrl Pts',(-4.34249723919958,6.86748900909525,
5.26285827315944));
#162060=CARTESIAN_POINT('Ctrl Pts',(-4.51654578253325,6.75743345343113,
5.27091865679628));
#162061=CARTESIAN_POINT('Ctrl Pts',(-4.68639536425903,6.64076573241742,
5.27897904043312));
#162062=CARTESIAN_POINT('Ctrl Pts',(-4.85154027747262,6.51784047814618,
5.28703942406996));
#162063=CARTESIAN_POINT('Ctrl Pts',(-5.02083658679712,6.39182514127668,
5.29530242881472));
#162064=CARTESIAN_POINT('Ctrl Pts',(-5.18518831100657,6.25923374809879,
5.30356543355948));
#162065=CARTESIAN_POINT('Ctrl Pts',(-5.34408573461268,6.12049305396299,
5.31182843830423));
#162066=CARTESIAN_POINT('Ctrl Pts',(-5.49921422051319,5.98504319375995,
5.31989545025416));
#162067=CARTESIAN_POINT('Ctrl Pts',(-5.64914399369161,5.84373267320644,
5.32796246220408));
#162068=CARTESIAN_POINT('Ctrl Pts',(-5.79343706396068,5.69699697633996,
5.33602947415401));
#162069=CARTESIAN_POINT('Ctrl Pts',(-5.94298866160503,5.54491373452579,
5.34439047529618));
#162070=CARTESIAN_POINT('Ctrl Pts',(-6.08648473877691,5.38700273511236,
5.35275147643835));
#162071=CARTESIAN_POINT('Ctrl Pts',(-6.22348204251012,5.22378778560672,
5.36111247758053));
#162072=CARTESIAN_POINT('Ctrl Pts',(-6.36047934624334,5.06057283610108,
5.3694734787227));
#162073=CARTESIAN_POINT('Ctrl Pts',(-6.49097766467865,4.89205424938621,
5.37783447986487));
#162074=CARTESIAN_POINT('Ctrl Pts',(-6.61458230332845,4.71879100141065,
5.38619548100704));
#162075=CARTESIAN_POINT('Ctrl Pts',(-6.72661508444199,4.56174864646745,
5.39377372581309));
#162076=CARTESIAN_POINT('Ctrl Pts',(-6.83320887724693,4.40049359157615,
5.40135197061913));
#162077=CARTESIAN_POINT('Ctrl Pts',(-6.93401765419816,4.23545590624767,
5.40893021542518));
#162078=CARTESIAN_POINT('Ctrl Pts',(-7.03475141668576,4.07054102980367,
5.41650282105985));
#162079=CARTESIAN_POINT('Ctrl Pts',(-7.1297085367821,3.90184943399813,5.42407542669452));
#162080=CARTESIAN_POINT('Ctrl Pts',(-7.21858444593699,3.72984264539091,
5.43164803232919));
#162081=CARTESIAN_POINT('Ctrl Pts',(-7.30741109748623,3.55793118793294,
5.43921644100627));
#162082=CARTESIAN_POINT('Ctrl Pts',(-7.39016307655815,3.38270851918058,
5.44678484968334));
#162083=CARTESIAN_POINT('Ctrl Pts',(-7.46658023023578,3.20466335641549,
5.45435325836042));
#162084=CARTESIAN_POINT('Ctrl Pts',(-7.54297892091693,3.02666121078799,
5.46191983844933));
#162085=CARTESIAN_POINT('Ctrl Pts',(-7.61304568045102,2.84583826262366,
5.46948641853824));
#162086=CARTESIAN_POINT('Ctrl Pts',(-7.6765672014734,2.66270606033839,5.47705299862715));
#162087=CARTESIAN_POINT('Ctrl Pts',(-7.7400774540643,2.47960634488027,5.48461823643886));
#162088=CARTESIAN_POINT('Ctrl Pts',(-7.79704466169135,2.29419853912275,
5.49218347425057));
#162089=CARTESIAN_POINT('Ctrl Pts',(-7.84730449065638,2.10701205345965,
5.49974871206228));
#162090=CARTESIAN_POINT('Ctrl Pts',(-7.89758179737495,1.91976047407596,
5.50731658067009));
#162091=CARTESIAN_POINT('Ctrl Pts',(-7.94114696698577,1.73072933381126,
5.5148844492779));
#162092=CARTESIAN_POINT('Ctrl Pts',(-7.97788605957186,1.5404614837733,5.52245231788571));
#162093=CARTESIAN_POINT('Ctrl Pts',(-8.0141510545858,1.35264893459905,5.52992252735497));
#162094=CARTESIAN_POINT('Ctrl Pts',(-8.04376507047298,1.16363175200847,
5.53739273682422));
#162095=CARTESIAN_POINT('Ctrl Pts',(-8.06666783720681,0.9739392007067,5.54486294629347));
#162096=CARTESIAN_POINT('Ctrl Pts',(-8.09519843192592,0.737634069308306,
5.5541687878676));
#162097=CARTESIAN_POINT('Ctrl Pts',(-8.11330244404707,0.500397178607468,
5.56347462944173));
#162098=CARTESIAN_POINT('Ctrl Pts',(-8.12099040105428,0.263063620601914,
5.57278047101585));
#162099=CARTESIAN_POINT('Ctrl Pts',(-8.12871963316337,0.0244558662428032,
5.58213627379016));
#162100=CARTESIAN_POINT('Ctrl Pts',(-8.12592071876027,-0.214249548839692,
5.59149207656446));
#162101=CARTESIAN_POINT('Ctrl Pts',(-8.11265618823322,-0.452213593361826,
5.60084787933876));
#162102=CARTESIAN_POINT('Ctrl Pts',(-8.09932726561922,-0.691332823995937,
5.61024909945102));
#162103=CARTESIAN_POINT('Ctrl Pts',(-8.07543089672325,-0.92970342792701,
5.61965031956329));
#162104=CARTESIAN_POINT('Ctrl Pts',(-8.04108212224408,-1.16648440445067,
5.62905153967555));
#162105=CARTESIAN_POINT('Ctrl Pts',(-8.00669617218807,-1.40352164832363,
5.63846293470048));
#162106=CARTESIAN_POINT('Ctrl Pts',(-7.96183520505301,-1.63896578837552,
5.64787432972541));
#162107=CARTESIAN_POINT('Ctrl Pts',(-7.90666577561126,-1.8719839409775,
5.65728572475034));
#162108=CARTESIAN_POINT('Ctrl Pts',(-7.85156106085704,-2.10472875928746,
5.66668608004739));
#162109=CARTESIAN_POINT('Ctrl Pts',(-7.78617206616532,-2.33505324380799,
5.67608643534444));
#162110=CARTESIAN_POINT('Ctrl Pts',(-7.71071543733702,-2.56213875637376,
5.68548679064149));
#162111=CARTESIAN_POINT('Ctrl Pts',(-7.66243673705226,-2.70743272948673,
5.6915013309543));
#162112=CARTESIAN_POINT('Ctrl Pts',(-7.61003766399274,-2.85140099218548,
5.69751587126711));
#162113=CARTESIAN_POINT('Ctrl Pts',(-7.55358586981176,-2.99383167026474,
5.70353041157992));
#162114=CARTESIAN_POINT('Ctrl Pts',(-7.48091753331546,-3.17717748933431,
5.71127271004293));
#162115=CARTESIAN_POINT('Ctrl Pts',(-7.40149660188222,-3.35806044101228,
5.71901500850595));
#162116=CARTESIAN_POINT('Ctrl Pts',(-7.31551774020827,-3.53594227260543,
5.72675730696896));
#162117=CARTESIAN_POINT('Ctrl Pts',(-7.22959243558202,-3.71371329992003,
5.7344947826809));
#162118=CARTESIAN_POINT('Ctrl Pts',(-7.13711748749244,-3.88848661264783,
5.74223225839283));
#162119=CARTESIAN_POINT('Ctrl Pts',(-7.03833594562911,-4.05974317894189,
5.74996973410476));
#162120=CARTESIAN_POINT('Ctrl Pts',(-6.93959837940351,-4.2309235051148,
5.7577037652417));
#162121=CARTESIAN_POINT('Ctrl Pts',(-6.83455998714991,-4.39858989752977,
5.76543779637864));
#162122=CARTESIAN_POINT('Ctrl Pts',(-6.72351016729135,-4.56224709905435,
5.77317182751558));
#162123=CARTESIAN_POINT('Ctrl Pts',(-6.61247455831453,-4.72588335760812,
5.78090486893996));
#162124=CARTESIAN_POINT('Ctrl Pts',(-6.49542924588141,-4.88551115071757,
5.78863791036433));
#162125=CARTESIAN_POINT('Ctrl Pts',(-6.37270764469657,-5.04066313472006,
5.79637095178871));
#162126=CARTESIAN_POINT('Ctrl Pts',(-6.24999830330982,-5.19579961915296,
5.80410322068791));
#162127=CARTESIAN_POINT('Ctrl Pts',(-6.12161402475157,-5.34646091018045,
5.81183548958711));
#162128=CARTESIAN_POINT('Ctrl Pts',(-5.98792921918407,-5.49221187032525,
5.81956775848631));
#162129=CARTESIAN_POINT('Ctrl Pts',(-5.85419299115056,-5.63801889423708,
5.82730300163777));
#162130=CARTESIAN_POINT('Ctrl Pts',(-5.71515240164898,-5.77891155295762,
5.83503824478923));
#162131=CARTESIAN_POINT('Ctrl Pts',(-5.57121996140689,-5.91449031651261,
5.84277348794069));
#162132=CARTESIAN_POINT('Ctrl Pts',(-5.45074110708877,-6.02797671384943,
5.84924828424924));
#162133=CARTESIAN_POINT('Ctrl Pts',(-5.32683549395849,-6.13774047173051,
5.85572308055778));
#162134=CARTESIAN_POINT('Ctrl Pts',(-5.1997633585022,-6.24356857719029,
5.86219787686633));
#162135=CARTESIAN_POINT('Ctrl Pts',(-5.03463161213713,-6.38109345474372,
5.87061195142287));
#162136=CARTESIAN_POINT('Ctrl Pts',(-4.86407241924091,-6.51203776821705,
5.87902602597942));
#162137=CARTESIAN_POINT('Ctrl Pts',(-4.6886237841604,-6.63599989248835,
5.88744010053596));
#162138=CARTESIAN_POINT('Ctrl Pts',(-4.51312615108145,-6.75999663598578,
5.89585652491308));
#162139=CARTESIAN_POINT('Ctrl Pts',(-4.33273656549878,-6.87700714520411,
5.90427294929019));
#162140=CARTESIAN_POINT('Ctrl Pts',(-4.14802246900494,-6.98667282468058,
5.9126893736673));
#162141=CARTESIAN_POINT('Ctrl Pts',(-3.96326256468477,-7.0963657004918,
5.92110788525982));
#162142=CARTESIAN_POINT('Ctrl Pts',(-3.7741762353731,-7.19870997543418,
5.92952639685233));
#162143=CARTESIAN_POINT('Ctrl Pts',(-3.58135694828023,-7.29339221292156,
5.93794490844484));
#162144=CARTESIAN_POINT('Ctrl Pts',(-3.38846360009358,-7.38811081746629,
5.94636665355297));
#162145=CARTESIAN_POINT('Ctrl Pts',(-3.1918346653308,-7.4751613859921,5.9547883986611));
#162146=CARTESIAN_POINT('Ctrl Pts',(-2.9920863848915,-7.55427737297532,
5.96321014376923));
#162147=CARTESIAN_POINT('Ctrl Pts',(-2.79231645228214,-7.63340193591624,
5.97163280177162));
#162148=CARTESIAN_POINT('Ctrl Pts',(-2.58942674539637,-7.704590105673,5.980055459774));
#162149=CARTESIAN_POINT('Ctrl Pts',(-2.38405213892045,-7.76762402291774,
5.98847811777639));
#162150=CARTESIAN_POINT('Ctrl Pts',(-2.17863847611245,-7.83066992739716,
5.99690237752562));
#162151=CARTESIAN_POINT('Ctrl Pts',(-1.97073922199153,-7.88555840405078,
6.00532663727485));
#162152=CARTESIAN_POINT('Ctrl Pts',(-1.7610042924744,-7.93212149707673,
6.01375089702408));
#162153=CARTESIAN_POINT('Ctrl Pts',(-1.70196260050231,-7.94522929844312,
6.01612237873364));
#162154=CARTESIAN_POINT('Ctrl Pts',(-1.64277551537179,-7.95767765612669,
6.01849386044321));
#162155=CARTESIAN_POINT('Ctrl Pts',(-1.58345770236731,-7.96946354953165,
6.02086534215277));
#162156=CARTESIAN_POINT('Ctrl Pts',(-1.37274026585278,-8.0113311289237,
6.02928966734735));
#162157=CARTESIAN_POINT('Ctrl Pts',(-1.16035067532255,-8.04483934999749,
6.03771399254192));
#162158=CARTESIAN_POINT('Ctrl Pts',(-0.946951430774239,-8.06988045452066,
6.0461383177365));
#162159=CARTESIAN_POINT('Ctrl Pts',(-0.733589064234515,-8.09491723163364,
6.05456118710428));
#162160=CARTESIAN_POINT('Ctrl Pts',(-0.519217654164309,-8.11148978395286,
6.06298405647207));
#162161=CARTESIAN_POINT('Ctrl Pts',(-0.304506020712815,-8.11954208350752,
6.07140692583985));
#162162=CARTESIAN_POINT('Ctrl Pts',(-0.0898382639491243,-8.12759273756106,
6.07982807397994));
#162163=CARTESIAN_POINT('Ctrl Pts',(0.125169313769842,-8.1271266058822,
6.08824922212004));
#162164=CARTESIAN_POINT('Ctrl Pts',(0.339845578329916,-8.11813972196769,
6.09667037026013));
#162165=CARTESIAN_POINT('Ctrl Pts',(0.554461611973064,-8.10915535946959,
6.10508915571017));
#162166=CARTESIAN_POINT('Ctrl Pts',(0.76874625460702,-8.09165503050455,
6.11350794116021));
#162167=CARTESIAN_POINT('Ctrl Pts',(0.982030167741453,-8.06568684689318,
6.12192672661026));
#162168=CARTESIAN_POINT('Ctrl Pts',(1.19525450144443,-8.03972591731983,
6.13034316032902));
#162169=CARTESIAN_POINT('Ctrl Pts',(1.40747840200391,-8.00530188782437,
6.13875959404778));
#162170=CARTESIAN_POINT('Ctrl Pts',(1.61803826996039,-7.96251466054811,
6.14717602776654));
#162171=CARTESIAN_POINT('Ctrl Pts',(1.82852171693458,-7.91974296254611,
6.1555894068095));
#162172=CARTESIAN_POINT('Ctrl Pts',(2.03734207895128,-7.86861418081482,
6.16400278585247));
#162173=CARTESIAN_POINT('Ctrl Pts',(2.2438455737859,-7.80927939079538,6.17241616489543));
#162174=CARTESIAN_POINT('Ctrl Pts',(2.30207075494353,-7.79254950978005,
6.17478837907668));
#162175=CARTESIAN_POINT('Ctrl Pts',(2.3601118139356,-7.7751675618776,6.17716059325793));
#162176=CARTESIAN_POINT('Ctrl Pts',(2.41795427037059,-7.75713766210814,
6.17953280743918));
#162177=CARTESIAN_POINT('Ctrl Pts',(2.60656375600892,-7.69834676125057,
6.18726799235569));
#162178=CARTESIAN_POINT('Ctrl Pts',(2.79314417217995,-7.63263656410289,
6.19500317727219));
#162179=CARTESIAN_POINT('Ctrl Pts',(2.97714785180455,-7.56017712960454,
6.2027383621887));
#162180=CARTESIAN_POINT('Ctrl Pts',(3.1610946329462,-7.48774010135321,6.21047115519495));
#162181=CARTESIAN_POINT('Ctrl Pts',(3.34246593595063,-7.40855812119425,
6.21820394820121));
#162182=CARTESIAN_POINT('Ctrl Pts',(3.52073143724983,-7.32285038146081,
6.22593674120747));
#162183=CARTESIAN_POINT('Ctrl Pts',(3.69897348706952,-7.23715391689439,
6.23366851693649));
#162184=CARTESIAN_POINT('Ctrl Pts',(3.87411023102477,-7.14493355647251,
6.24140029266551));
#162185=CARTESIAN_POINT('Ctrl Pts',(4.04563331373399,-7.04645575117773,
6.24913206839453));
#162186=CARTESIAN_POINT('Ctrl Pts',(4.21721777208604,-6.94794270783505,
6.25686661076403));
#162187=CARTESIAN_POINT('Ctrl Pts',(4.38518567693939,-6.84316791854296,
6.26460115313354));
#162188=CARTESIAN_POINT('Ctrl Pts',(4.54905461260978,-6.73244307023785,
6.27233569550305));
#162189=CARTESIAN_POINT('Ctrl Pts',(4.71295122391648,-6.6216995217403,6.28007154415053));
#162190=CARTESIAN_POINT('Ctrl Pts',(4.87274719809861,-6.50500411610102,
6.28780739279802));
#162191=CARTESIAN_POINT('Ctrl Pts',(5.02799078569935,-6.38271072675414,
6.29554324144551));
#162192=CARTESIAN_POINT('Ctrl Pts',(5.18336140063324,-6.26031727141839,
6.30328541991465));
#162193=CARTESIAN_POINT('Ctrl Pts',(5.33417191366276,-6.13231690544928,
6.31102759838379));
#162194=CARTESIAN_POINT('Ctrl Pts',(5.4800045279485,-5.99910309431034,6.31876977685294));
#162195=CARTESIAN_POINT('Ctrl Pts',(5.60200292160804,-5.88766114388099,
6.3252466088105));
#162196=CARTESIAN_POINT('Ctrl Pts',(5.72051813165079,-5.77257137445318,
6.33172344076807));
#162197=CARTESIAN_POINT('Ctrl Pts',(5.8353262874522,-5.6540830097788,6.33820027272563));
#162198=CARTESIAN_POINT('Ctrl Pts',(6.00191549708611,-5.48215373450969,
6.34759830119504));
#162199=CARTESIAN_POINT('Ctrl Pts',(6.16079438656214,-5.3029712452053,6.35699632966446));
#162200=CARTESIAN_POINT('Ctrl Pts',(6.3114230822179,-5.11718929098261,6.36639435813387));
#162201=CARTESIAN_POINT('Ctrl Pts',(6.46226610989966,-4.93114298458938,
6.37580575921115));
#162202=CARTESIAN_POINT('Ctrl Pts',(6.60483543793473,-4.73847845832144,
6.38521716028845));
#162203=CARTESIAN_POINT('Ctrl Pts',(6.73863144967037,-4.53988256984841,
6.39462856136573));
#162204=CARTESIAN_POINT('Ctrl Pts',(6.87222600892987,-4.3415857010021,6.40402579199036));
#162205=CARTESIAN_POINT('Ctrl Pts',(6.9970736359882,-4.13737535138648,6.41342302261498));
#162206=CARTESIAN_POINT('Ctrl Pts',(7.1127195336528,-3.92796491813431,6.4228202532396));
#162207=CARTESIAN_POINT('Ctrl Pts',(7.22807372922396,-3.71908269611144,
6.43219378054313));
#162208=CARTESIAN_POINT('Ctrl Pts',(7.33427252055881,-3.5050266135619,6.44156730784666));
#162209=CARTESIAN_POINT('Ctrl Pts',(7.4309073037858,-3.28653376751903,6.45094083515019));
#162210=CARTESIAN_POINT('Ctrl Pts',(7.52691454640957,-3.06945980117793,
6.46025349131827));
#162211=CARTESIAN_POINT('Ctrl Pts',(7.61348155627842,-2.84800654052336,
6.46956614748636));
#162212=CARTESIAN_POINT('Ctrl Pts',(7.69025040874438,-2.62292512537186,
6.47887880365445));
#162213=CARTESIAN_POINT('Ctrl Pts',(7.73968098375228,-2.47799780892583,
6.48487511510698));
#162214=CARTESIAN_POINT('Ctrl Pts',(7.78505018096513,-2.33156685795491,
6.49087142655951));
#162215=CARTESIAN_POINT('Ctrl Pts',(7.82627209184742,-2.18383898373259,
6.49686773801204));
#162216=CARTESIAN_POINT('Ctrl Pts',(7.87610976657735,-2.00523460595254,
6.50411733448523));
#162217=CARTESIAN_POINT('Ctrl Pts',(7.91987916280345,-1.82474445529073,
6.51136693095843));
#162218=CARTESIAN_POINT('Ctrl Pts',(7.9574296753959,-1.64286351339015,6.51861652743162));
#162219=CARTESIAN_POINT('Ctrl Pts',(7.99496808093457,-1.46104121362771,
6.52586378648654));
#162220=CARTESIAN_POINT('Ctrl Pts',(8.02629151042615,-1.27782939594045,
6.53311104554146));
#162221=CARTESIAN_POINT('Ctrl Pts',(8.05129984720199,-1.0937359521133,6.54035830459638));
#162222=CARTESIAN_POINT('Ctrl Pts',(8.07631239206426,-0.909611531371167,
6.54760678312834));
#162223=CARTESIAN_POINT('Ctrl Pts',(8.09500765887235,-0.724605573874979,
6.5548552616603));
#162224=CARTESIAN_POINT('Ctrl Pts',(8.10733706991169,-0.539233898540962,
6.56210374019226));
#162225=CARTESIAN_POINT('Ctrl Pts',(8.11935365494763,-0.35856553629746,
6.56916830786564));
#162226=CARTESIAN_POINT('Ctrl Pts',(8.1253235154935,-0.177550143507737,
6.57623287553903));
#162227=CARTESIAN_POINT('Ctrl Pts',(8.12524931639108,0.00333301459649942,
6.58329744321241));
#162228=CARTESIAN_POINT('',(8.1252500832311,-0.00151305119605756,10.5836787518598));
#162229=CARTESIAN_POINT('Ctrl Pts',(8.1252493577062,0.00323072670080068,
6.5857174746832));
#162230=CARTESIAN_POINT('Ctrl Pts',(8.12506851487489,0.458048863603974,
6.60495129592261));
#162231=CARTESIAN_POINT('Ctrl Pts',(8.08669999959761,0.91206338244344,6.6243674061125));
#162232=CARTESIAN_POINT('Ctrl Pts',(8.00331728191846,1.40301841636916,6.64449536413657));
#162233=CARTESIAN_POINT('Ctrl Pts',(7.99575615035507,1.4454867178715,6.64622858465563));
#162234=CARTESIAN_POINT('Ctrl Pts',(7.98533186637207,1.50145020413107,6.64850049919071));
#162235=CARTESIAN_POINT('Ctrl Pts',(7.98277209453259,1.51500079901468,6.64904966738446));
#162236=CARTESIAN_POINT('Ctrl Pts',(7.97758522937364,1.54208021779063,6.65014516253916));
#162237=CARTESIAN_POINT('Ctrl Pts',(7.97495818822034,1.55560900901587,6.65069148943679));
#162238=CARTESIAN_POINT('Ctrl Pts',(7.97057719053874,1.57786757842396,6.65158866374817));
#162239=CARTESIAN_POINT('Ctrl Pts',(7.96884328695497,1.58660124609189,6.65194026390858));
#162240=CARTESIAN_POINT('Ctrl Pts',(7.96572449629611,1.60217649970945,6.65256650971597));
#162241=CARTESIAN_POINT('Ctrl Pts',(7.96434514416166,1.6090191770655,6.6528413684856));
#162242=CARTESIAN_POINT('Ctrl Pts',(7.96166200618667,1.62224167850085,6.65337196125073));
#162243=CARTESIAN_POINT('Ctrl Pts',(7.96035936555062,1.62862172889939,6.65362774010539));
#162244=CARTESIAN_POINT('Ctrl Pts',(7.95766572554249,1.64173415097857,6.65415291961192));
#162245=CARTESIAN_POINT('Ctrl Pts',(7.95627384865523,1.64846633799888,6.65442228483655));
#162246=CARTESIAN_POINT('Ctrl Pts',(7.95291096889975,1.66462833359493,6.65506828295408));
#162247=CARTESIAN_POINT('Ctrl Pts',(7.95093173341598,1.67405643269761,6.65544457922563));
#162248=CARTESIAN_POINT('Ctrl Pts',(7.94367465385001,1.70832237244617,6.65681016453348));
#162249=CARTESIAN_POINT('Ctrl Pts',(7.93829711754992,1.73313912534099,6.65779526868028));
#162250=CARTESIAN_POINT('Ctrl Pts',(7.85527509273323,2.10778272548637,6.6726033866534));
#162251=CARTESIAN_POINT('Ctrl Pts',(7.75468717983921,2.45212727384615,6.68527878474658));
#162252=CARTESIAN_POINT('Ctrl Pts',(7.60886089427707,2.85120154610489,6.69979572936306));
#162253=CARTESIAN_POINT('Ctrl Pts',(7.58525845803258,2.91341185007144,6.70205371008332));
#162254=CARTESIAN_POINT('Ctrl Pts',(7.52305042414752,3.07149484230334,6.70779144781689));
#162255=CARTESIAN_POINT('Ctrl Pts',(7.4833747926049,3.1669338838541,6.71125550356128));
#162256=CARTESIAN_POINT('Ctrl Pts',(7.38259362292187,3.39688374256376,6.71964568119447));
#162257=CARTESIAN_POINT('Ctrl Pts',(7.31961965685809,3.53053478886467,6.72455970264925));
#162258=CARTESIAN_POINT('Ctrl Pts',(7.10028125540747,3.96491440246287,6.74081570347696));
#162259=CARTESIAN_POINT('Ctrl Pts',(6.92875210910965,4.25757238634734,6.75224253116121));
#162260=CARTESIAN_POINT('Ctrl Pts',(6.61099920012536,4.72940411045619,6.77226320482249));
#162261=CARTESIAN_POINT('Ctrl Pts',(6.47450707693038,4.91460309634165,6.7805744202096));
#162262=CARTESIAN_POINT('Ctrl Pts',(6.25761448044106,5.18414984621858,6.79350908661515));
#162263=CARTESIAN_POINT('Ctrl Pts',(6.18295404121457,5.27297133140727,6.79791721325621));
#162264=CARTESIAN_POINT('Ctrl Pts',(6.09226463307138,5.37628678244633,6.80322894855996));
#162265=CARTESIAN_POINT('Ctrl Pts',(6.07804647112951,5.39235560890253,6.80406050199459));
#162266=CARTESIAN_POINT('Ctrl Pts',(6.05608061211405,5.41698333546571,6.80534337514342));
#162267=CARTESIAN_POINT('Ctrl Pts',(6.04837799741681,5.42558240525059,6.80579289271527));
#162268=CARTESIAN_POINT('Ctrl Pts',(6.03487703792565,5.44059016940609,6.80658021394662));
#162269=CARTESIAN_POINT('Ctrl Pts',(6.02908673732833,5.44700609211496,6.80691769456274));
#162270=CARTESIAN_POINT('Ctrl Pts',(6.01692205815316,5.4604419620549,6.80762631208383));
#162271=CARTESIAN_POINT('Ctrl Pts',(6.01054560751961,5.4674600111999,6.80799753225109));
#162272=CARTESIAN_POINT('Ctrl Pts',(5.99277641454043,5.48694848837617,6.80903140040465));
#162273=CARTESIAN_POINT('Ctrl Pts',(5.98135707903818,5.49939454464192,6.80969512200837));
#162274=CARTESIAN_POINT('Ctrl Pts',(5.93567853747192,5.5488694969207,6.81234737819525));
#162275=CARTESIAN_POINT('Ctrl Pts',(5.90111397066161,5.5856142175783,6.81434830590851));
#162276=CARTESIAN_POINT('Ctrl Pts',(5.25270631991151,6.26218343549144,6.85177831546235));
#162277=CARTESIAN_POINT('Ctrl Pts',(4.53861672800915,6.7975172662044,6.89209952473709));
#162278=CARTESIAN_POINT('Ctrl Pts',(3.52519598912004,7.3251848441121,6.94297758991279));
#162279=CARTESIAN_POINT('Ctrl Pts',(3.29244869271108,7.43270704362022,6.95422539958008));
#162280=CARTESIAN_POINT('Ctrl Pts',(2.96263572692282,7.56653241722902,6.96924913864206));
#162281=CARTESIAN_POINT('Ctrl Pts',(2.86958686411492,7.60230857997144,6.97338962316836));
#162282=CARTESIAN_POINT('Ctrl Pts',(2.72155291514907,7.65612050878128,6.97979943098742));
#162283=CARTESIAN_POINT('Ctrl Pts',(2.66699560334524,7.67529583024132,6.98212381510126));
#162284=CARTESIAN_POINT('Ctrl Pts',(2.59849408190045,7.69855354794333,6.98499969329111));
#162285=CARTESIAN_POINT('Ctrl Pts',(2.58473789961544,7.70318299264376,6.98557507933486));
#162286=CARTESIAN_POINT('Ctrl Pts',(2.56418191238656,7.71003955095519,6.98643178749436));
#162287=CARTESIAN_POINT('Ctrl Pts',(2.5573914955036,7.7122945675236,6.98671428690972));
#162288=CARTESIAN_POINT('Ctrl Pts',(2.54348585076419,7.71689208184667,6.9872917829858));
#162289=CARTESIAN_POINT('Ctrl Pts',(2.53637034312827,7.71923371578307,6.98758674361304));
#162290=CARTESIAN_POINT('Ctrl Pts',(2.52105188895716,7.72425138021242,6.98822059083882));
#162291=CARTESIAN_POINT('Ctrl Pts',(2.51284789275766,7.7269241927241,6.98855934604577));
#162292=CARTESIAN_POINT('Ctrl Pts',(2.49075974945243,7.73408147824269,6.9894695224137));
#162293=CARTESIAN_POINT('Ctrl Pts',(2.47686771996339,7.73854164185578,6.99003997287339));
#162294=CARTESIAN_POINT('Ctrl Pts',(2.41276687533607,7.75893151395074,6.9926632530704));
#162295=CARTESIAN_POINT('Ctrl Pts',(2.36241530647571,7.77441035037212,6.99469871348262));
#162296=CARTESIAN_POINT('Ctrl Pts',(1.92559200941377,7.9040607741543,7.0121643302506));
#162297=CARTESIAN_POINT('Ctrl Pts',(1.53125007587217,7.9898304307067,7.02665820915452));
#162298=CARTESIAN_POINT('Ctrl Pts',(0.659928805305274,8.11243461975554,
7.058258914541));
#162299=CARTESIAN_POINT('Ctrl Pts',(0.182783245919793,8.13717883820747,
7.07532819278513));
#162300=CARTESIAN_POINT('Ctrl Pts',(-0.466511668410448,8.1136879827477,
7.09956678266333));
#162301=CARTESIAN_POINT('Ctrl Pts',(-0.639004929851296,8.10192794173982,
7.10609483435487));
#162302=CARTESIAN_POINT('Ctrl Pts',(-0.892807870939498,8.07646849664879,
7.11585423782745));
#162303=CARTESIAN_POINT('Ctrl Pts',(-0.974496814572122,8.06701958598615,
7.11901886368915));
#162304=CARTESIAN_POINT('Ctrl Pts',(-1.08840127526852,8.05208893954448,
7.1234648236591));
#162305=CARTESIAN_POINT('Ctrl Pts',(-1.12074898971591,8.0476502977396,7.12473118787188));
#162306=CARTESIAN_POINT('Ctrl Pts',(-1.17560882179874,8.03978544162671,
7.12688522083534));
#162307=CARTESIAN_POINT('Ctrl Pts',(-1.1981349425908,8.03645933879725,7.12777151478346));
#162308=CARTESIAN_POINT('Ctrl Pts',(-1.24260074708423,8.02970261300227,
7.12952460616806));
#162309=CARTESIAN_POINT('Ctrl Pts',(-1.26454095244713,8.02627664898215,
7.13039132853214));
#162310=CARTESIAN_POINT('Ctrl Pts',(-1.31510141256166,8.01816917141084,
7.13239279191779));
#162311=CARTESIAN_POINT('Ctrl Pts',(-1.34371115593501,8.01342429342372,
7.13352838330375));
#162312=CARTESIAN_POINT('Ctrl Pts',(-1.42057873243792,8.00025270968165,
7.13658810675044));
#162313=CARTESIAN_POINT('Ctrl Pts',(-1.4687865936428,7.99154260746225,7.13851622905903));
#162314=CARTESIAN_POINT('Ctrl Pts',(-1.92540643512068,7.90477013406925,
7.15687310397061));
#162315=CARTESIAN_POINT('Ctrl Pts',(-2.32731471100886,7.79590624444567,
7.17379111161773));
#162316=CARTESIAN_POINT('Ctrl Pts',(-3.22132822465334,7.47842005584968,
7.21342263100111));
#162317=CARTESIAN_POINT('Ctrl Pts',(-3.7047640348543,7.2510978483851,7.23637391631977));
#162318=CARTESIAN_POINT('Ctrl Pts',(-4.31022689168872,6.88993764755602,
7.26572644660342));
#162319=CARTESIAN_POINT('Ctrl Pts',(-4.45517323706194,6.79711201938735,
7.27279269848444));
#162320=CARTESIAN_POINT('Ctrl Pts',(-4.62354053657463,6.68158598845901,
7.28096824325882));
#162321=CARTESIAN_POINT('Ctrl Pts',(-4.64990688479634,6.66326379565898,
7.28224752677352));
#162322=CARTESIAN_POINT('Ctrl Pts',(-4.68574312931519,6.63804459817739,
7.28398424347574));
#162323=CARTESIAN_POINT('Ctrl Pts',(-4.69530755491471,6.63128281162708,
7.28444756009791));
#162324=CARTESIAN_POINT('Ctrl Pts',(-4.71059955764046,6.62042211455746,
7.2851879708793));
#162325=CARTESIAN_POINT('Ctrl Pts',(-4.71633646639644,6.61633641099674,
7.28546566027693));
#162326=CARTESIAN_POINT('Ctrl Pts',(-4.72823132082869,6.60784181843816,
7.2860412393571));
#162327=CARTESIAN_POINT('Ctrl Pts',(-4.73438843127363,6.60343176712427,
7.28633907508634));
#162328=CARTESIAN_POINT('Ctrl Pts',(-4.74847081582593,6.59331539101312,
7.28702003277565));
#162329=CARTESIAN_POINT('Ctrl Pts',(-4.75639199526871,6.58760336712136,
7.28740288588776));
#162330=CARTESIAN_POINT('Ctrl Pts',(-4.7812657306256,6.56959847157609,7.28860450010607));
#162331=CARTESIAN_POINT('Ctrl Pts',(-4.79818115619207,6.55725427809367,
7.28942077550516));
#162332=CARTESIAN_POINT('Ctrl Pts',(-4.9836946525188,6.42077181501787,7.29836166164221));
#162333=CARTESIAN_POINT('Ctrl Pts',(-5.14747592292401,6.29023160081385,
7.30611111194316));
#162334=CARTESIAN_POINT('Ctrl Pts',(-5.83512534767394,5.69728655314435,
7.33859483463413));
#162335=CARTESIAN_POINT('Ctrl Pts',(-6.30319005430231,5.17471520366987,
7.36088202334357));
#162336=CARTESIAN_POINT('Ctrl Pts',(-6.92858383190715,4.2637394856707,7.39923867065006));
#162337=CARTESIAN_POINT('Ctrl Pts',(-7.13306093305325,3.91205172482726,
7.41390827205031));
#162338=CARTESIAN_POINT('Ctrl Pts',(-7.32446622966944,3.51751680673151,
7.43077356318846));
#162339=CARTESIAN_POINT('Ctrl Pts',(-7.33838586369557,3.48838399871033,
7.43202097217626));
#162340=CARTESIAN_POINT('Ctrl Pts',(-7.35793632868408,3.44683136587635,
7.43380328280909));
#162341=CARTESIAN_POINT('Ctrl Pts',(-7.36371017945046,3.4344789812522,7.43433350030101));
#162342=CARTESIAN_POINT('Ctrl Pts',(-7.37359982794669,3.41318181290075,
7.43524835003641));
#162343=CARTESIAN_POINT('Ctrl Pts',(-7.37773051756353,3.40424395717882,
7.43563249491743));
#162344=CARTESIAN_POINT('Ctrl Pts',(-7.38558937038807,3.38715773319133,
7.4363672534548));
#162345=CARTESIAN_POINT('Ctrl Pts',(-7.38932032210059,3.37901065909877,
7.43671777546324));
#162346=CARTESIAN_POINT('Ctrl Pts',(-7.39800051083408,3.35997308058562,
7.43753726377785));
#162347=CARTESIAN_POINT('Ctrl Pts',(-7.40293918386998,3.34907779829207,
7.43800657306172));
#162348=CARTESIAN_POINT('Ctrl Pts',(-7.41981616146235,3.31162550581032,
7.43962090391658));
#162349=CARTESIAN_POINT('Ctrl Pts',(-7.43163570069759,3.28501539591612,
7.44076977750974));
#162350=CARTESIAN_POINT('Ctrl Pts',(-7.55477318034031,3.00372186510362,
7.4529348925732));
#162351=CARTESIAN_POINT('Ctrl Pts',(-7.65308820831105,2.74356796448362,
7.46437073609428));
#162352=CARTESIAN_POINT('Ctrl Pts',(-7.83492931251577,2.17595230680987,
7.48970513956059));
#162353=CARTESIAN_POINT('Ctrl Pts',(-7.91410156959003,1.86758154772862,
7.50370154779696));
#162354=CARTESIAN_POINT('Ctrl Pts',(-8.04804951627489,1.18078267618282,
7.53501007428641));
#162355=CARTESIAN_POINT('Ctrl Pts',(-8.09462380115126,0.801506318363753,
7.55239154354304));
#162356=CARTESIAN_POINT('Ctrl Pts',(-8.13214650837807,0.077198212269558,
7.58465864371618));
#162357=CARTESIAN_POINT('Ctrl Pts',(-8.12813840593303,-0.266780047999812,
7.5995790610305));
#162358=CARTESIAN_POINT('Ctrl Pts',(-8.098824885156,-0.656461255678929,
7.61537839712574));
#162359=CARTESIAN_POINT('Ctrl Pts',(-8.09488351424861,-0.703396675891562,
7.61726282406029));
#162360=CARTESIAN_POINT('Ctrl Pts',(-8.08931697511869,-0.7634213810071,
7.61965197660907));
#162361=CARTESIAN_POINT('Ctrl Pts',(-8.08806778321992,-0.776544181494922,
7.62017302712088));
#162362=CARTESIAN_POINT('Ctrl Pts',(-8.08600943193197,-0.797623335483167,
7.62100802328078));
#162363=CARTESIAN_POINT('Ctrl Pts',(-8.08522045480616,-0.805581601330433,
7.62132281863089));
#162364=CARTESIAN_POINT('Ctrl Pts',(-8.08369928627636,-0.820697986996388,
7.62191992348114));
#162365=CARTESIAN_POINT('Ctrl Pts',(-8.08296933370346,-0.827856320658696,
7.62220232520776));
#162366=CARTESIAN_POINT('Ctrl Pts',(-8.0812888746549,-0.844121750168679,
7.62284321776499));
#162367=CARTESIAN_POINT('Ctrl Pts',(-8.08033247961804,-0.853228237017915,
7.62320146897822));
#162368=CARTESIAN_POINT('Ctrl Pts',(-8.07782203535444,-0.87674906026654,
7.6241253692235));
#162369=CARTESIAN_POINT('Ctrl Pts',(-8.07624479327208,-0.891160923783693,
7.62469009609325));
#162370=CARTESIAN_POINT('Ctrl Pts',(-8.06652146504213,-0.977860343993965,
7.62807952882937));
#162371=CARTESIAN_POINT('Ctrl Pts',(-8.05744332515673,-1.05004135050398,
7.63086846506619));
#162372=CARTESIAN_POINT('Ctrl Pts',(-8.00424884755594,-1.43154046959468,
7.64547641591087));
#162373=CARTESIAN_POINT('Ctrl Pts',(-7.94328554737833,-1.7382576791047,
7.65677186848395));
#162374=CARTESIAN_POINT('Ctrl Pts',(-7.72260550019974,-2.5887480965958,
7.68831684905884));
#162375=CARTESIAN_POINT('Ctrl Pts',(-7.5235178714004,-3.12040490831959,
7.7084419970786));
#162376=CARTESIAN_POINT('Ctrl Pts',(-7.09285591318382,-3.9837105863508,
7.74444849594742));
#162377=CARTESIAN_POINT('Ctrl Pts',(-6.88893313626673,-4.32679253032133,
7.75969780275065));
#162378=CARTESIAN_POINT('Ctrl Pts',(-6.60591985710963,-4.73187593007761,
7.77882716238859));
#162379=CARTESIAN_POINT('Ctrl Pts',(-6.54978895402285,-4.80927140458512,
7.78253981052386));
#162380=CARTESIAN_POINT('Ctrl Pts',(-6.46411244913894,-4.92312261383116,
7.78809415863395));
#162381=CARTESIAN_POINT('Ctrl Pts',(-6.43559546286425,-4.9603424317168,
7.78992515087991));
#162382=CARTESIAN_POINT('Ctrl Pts',(-6.38367713808798,-5.02690382729935,
7.79322779586642));
#162383=CARTESIAN_POINT('Ctrl Pts',(-6.36039160390264,-5.05633409936315,
7.79469817683162));
#162384=CARTESIAN_POINT('Ctrl Pts',(-6.3100251200391,-5.11909314556633,
7.79785589629071));
#162385=CARTESIAN_POINT('Ctrl Pts',(-6.2828821535919,-5.15237066532803,
7.79954387529148));
#162386=CARTESIAN_POINT('Ctrl Pts',(-6.20871267845345,-5.24184546388572,
7.80412017936905));
#162387=CARTESIAN_POINT('Ctrl Pts',(-6.16118783837029,-5.29762411961881,
7.8070139542251));
#162388=CARTESIAN_POINT('Ctrl Pts',(-5.85225311734252,-5.65043175104563,
7.82558857621375));
#162389=CARTESIAN_POINT('Ctrl Pts',(-5.57020058014652,-5.92866748899128,
7.84150606354376));
#162390=CARTESIAN_POINT('Ctrl Pts',(-4.96505118080151,-6.44417510396032,
7.87375733276426));
#162391=CARTESIAN_POINT('Ctrl Pts',(-4.64241597843746,-6.68035203775207,
7.89004798921172));
#162392=CARTESIAN_POINT('Ctrl Pts',(-4.23425855980627,-6.93523250203518,
7.90937004372964));
#162393=CARTESIAN_POINT('Ctrl Pts',(-4.16413716740915,-6.97756098145358,
7.91264608714295));
#162394=CARTESIAN_POINT('Ctrl Pts',(-4.04427514789393,-7.04746468475808,
7.91816819050737));
#162395=CARTESIAN_POINT('Ctrl Pts',(-3.99486335153644,-7.07559091785973,
7.92042267801759));
#162396=CARTESIAN_POINT('Ctrl Pts',(-3.92423133490674,-7.11482038596776,
7.92361292894792));
#162397=CARTESIAN_POINT('Ctrl Pts',(-3.90325119953369,-7.12635185592349,
7.92455651855231));
#162398=CARTESIAN_POINT('Ctrl Pts',(-3.86756672387046,-7.14576052281125,
7.92615449538628));
#162399=CARTESIAN_POINT('Ctrl Pts',(-3.85288856488585,-7.15368545028408,
7.92680981025561));
#162400=CARTESIAN_POINT('Ctrl Pts',(-3.82184520004718,-7.17032290431969,
7.92819172803375));
#162401=CARTESIAN_POINT('Ctrl Pts',(-3.80547436039207,-7.1790247374264,
7.92891813331191));
#162402=CARTESIAN_POINT('Ctrl Pts',(-3.75880206958781,-7.20362864170807,
7.93098265723723));
#162403=CARTESIAN_POINT('Ctrl Pts',(-3.72842967365028,-7.21939545879472,
7.93231850007248));
#162404=CARTESIAN_POINT('Ctrl Pts',(-3.55079425523386,-7.31018898023141,
7.94009018230389));
#162405=CARTESIAN_POINT('Ctrl Pts',(-3.40136773590529,-7.38090112204373,
7.94646480033873));
#162406=CARTESIAN_POINT('Ctrl Pts',(-3.11776657953699,-7.50466518170462,
7.95837279081931));
#162407=CARTESIAN_POINT('Ctrl Pts',(-2.9841345834056,-7.55879678061377,
7.96390724988982));
#162408=CARTESIAN_POINT('Ctrl Pts',(-2.73010354713418,-7.65391250092677,
7.97434329094935));
#162409=CARTESIAN_POINT('Ctrl Pts',(-2.61004491476187,-7.69568107732392,
7.97924072030386));
#162410=CARTESIAN_POINT('Ctrl Pts',(-2.40315601994212,-7.76225944872292,
7.98764799393247));
#162411=CARTESIAN_POINT('Ctrl Pts',(-2.31680143967154,-7.78846978246094,
7.99114765230988));
#162412=CARTESIAN_POINT('Ctrl Pts',(-2.1880979538327,-7.82520391507167,
7.99635556931798));
#162413=CARTESIAN_POINT('Ctrl Pts',(-2.14607174852429,-7.83683386323641,
7.99805486431949));
#162414=CARTESIAN_POINT('Ctrl Pts',(-2.07333671835877,-7.85633293644145,
8.00099425411069));
#162415=CARTESIAN_POINT('Ctrl Pts',(-2.04267165781704,-7.86436169355199,
8.00223301234753));
#162416=CARTESIAN_POINT('Ctrl Pts',(-1.97377900531381,-7.88196910985819,
8.00501518301959));
#162417=CARTESIAN_POINT('Ctrl Pts',(-1.93552715516518,-7.89144950107877,
8.00655937131698));
#162418=CARTESIAN_POINT('Ctrl Pts',(-1.83128521837362,-7.91648144142791,
8.01076639455341));
#162419=CARTESIAN_POINT('Ctrl Pts',(-1.76516722070955,-7.93148589959464,
8.01343361128471));
#162420=CARTESIAN_POINT('Ctrl Pts',(-1.39418490061335,-8.01080598686902,
8.02839540584334));
#162421=CARTESIAN_POINT('Ctrl Pts',(-1.08600913143585,-8.05837101056055,
8.0408249113099));
#162422=CARTESIAN_POINT('Ctrl Pts',(-0.62364412205684,-8.10272432042586,
8.05938033546882));
#162423=CARTESIAN_POINT('Ctrl Pts',(-0.471036062616764,-8.11302648903253,
8.06548696029151));
#162424=CARTESIAN_POINT('Ctrl Pts',(-0.235710951945573,-8.12225014445922,
8.07484021313481));
#162425=CARTESIAN_POINT('Ctrl Pts',(-0.153148991548546,-8.12422627825285,
8.07810958130518));
#162426=CARTESIAN_POINT('Ctrl Pts',(-0.0432080940608028,-8.12518119167401,
8.08244047333058));
#162427=CARTESIAN_POINT('Ctrl Pts',(-0.015844260820631,-8.12528062942543,
8.08351653896995));
#162428=CARTESIAN_POINT('Ctrl Pts',(0.0312397680984873,-8.12521387554218,
8.0853645286597));
#162429=CARTESIAN_POINT('Ctrl Pts',(0.050959761725058,-8.1251141254933,
8.08613744895639));
#162430=CARTESIAN_POINT('Ctrl Pts',(0.092861406918647,-8.12474962122101,
8.08777770398095));
#162431=CARTESIAN_POINT('Ctrl Pts',(0.115042742060254,-8.12446581752494,
8.08864476788495));
#162432=CARTESIAN_POINT('Ctrl Pts',(0.174884321978119,-8.1234550432774,
8.09098098206213));
#162433=CARTESIAN_POINT('Ctrl Pts',(0.212541205609717,-8.12255702475901,
8.09244792117921));
#162434=CARTESIAN_POINT('Ctrl Pts',(0.411886184091409,-8.11641593371033,
8.10019985312173));
#162435=CARTESIAN_POINT('Ctrl Pts',(0.573398458324473,-8.10660674880811,
8.10643363746578));
#162436=CARTESIAN_POINT('Ctrl Pts',(0.743539928098192,-8.09116296498737,
8.11299755615427));
#162437=CARTESIAN_POINT('Ctrl Pts',(0.752567202775413,-8.09032832189467,
8.1133458104373));
#162438=CARTESIAN_POINT('Ctrl Pts',(0.763852227499174,-8.08926588054208,
8.11378115986181));
#162439=CARTESIAN_POINT('Ctrl Pts',(0.766111302016934,-8.08905224265988,
8.11386830936705));
#162440=CARTESIAN_POINT('Ctrl Pts',(0.782018752425672,-8.0875411711376,
8.11448197868131));
#162441=CARTESIAN_POINT('Ctrl Pts',(0.795663919412676,-8.08621014144403,
8.11500837088762));
#162442=CARTESIAN_POINT('Ctrl Pts',(1.12918536632948,-8.05282412012167,
8.12787518608451));
#162443=CARTESIAN_POINT('Ctrl Pts',(1.44688185475672,-8.00184780213221,
8.14015402965942));
#162444=CARTESIAN_POINT('Ctrl Pts',(1.93827387127676,-7.89277266798919,
8.15955983397255));
#162445=CARTESIAN_POINT('Ctrl Pts',(2.1144522820973,-7.84741082013793,8.16660053198384));
#162446=CARTESIAN_POINT('Ctrl Pts',(2.35772781314247,-7.77598508202863,
8.17647147745223));
#162447=CARTESIAN_POINT('Ctrl Pts',(2.42622669512594,-7.75488545357596,
8.17926739528149));
#162448=CARTESIAN_POINT('Ctrl Pts',(2.54659238679437,-7.71605844868456,
8.18421098540876));
#162449=CARTESIAN_POINT('Ctrl Pts',(2.59857587805192,-7.69870730368207,
8.18635620305781));
#162450=CARTESIAN_POINT('Ctrl Pts',(2.71067135570806,-7.66002717155188,
8.19100455456611));
#162451=CARTESIAN_POINT('Ctrl Pts',(2.77071577958751,-7.6385135661183,8.19350858723749));
#162452=CARTESIAN_POINT('Ctrl Pts',(3.03093282318446,-7.54180716851412,
8.20442233573992));
#162453=CARTESIAN_POINT('Ctrl Pts',(3.22834592373732,-7.45943637626475,
8.21286489215665));
#162454=CARTESIAN_POINT('Ctrl Pts',(3.54045059601038,-7.31449747615005,
8.2264494520932));
#162455=CARTESIAN_POINT('Ctrl Pts',(3.65728570375875,-7.25678477187633,
8.23158986546695));
#162456=CARTESIAN_POINT('Ctrl Pts',(3.81195006038744,-7.17570136056437,
8.2384567579603));
#162457=CARTESIAN_POINT('Ctrl Pts',(3.85104839795112,-7.15479416422231,
8.24019807116571));
#162458=CARTESIAN_POINT('Ctrl Pts',(3.92888215815467,-7.11235098792857,
8.243674437032));
#162459=CARTESIAN_POINT('Ctrl Pts',(3.96761643292707,-7.09081599298028,
8.24540943304662));
#162460=CARTESIAN_POINT('Ctrl Pts',(4.10405026020627,-7.01349527370921,
8.2515414770699));
#162461=CARTESIAN_POINT('Ctrl Pts',(4.20076555097384,-6.95599837799962,
8.25592667111853));
#162462=CARTESIAN_POINT('Ctrl Pts',(4.42753395751192,-6.81473056543669,
8.26633276062376));
#162463=CARTESIAN_POINT('Ctrl Pts',(4.55645002556714,-6.72921784053184,
8.27234891134538));
#162464=CARTESIAN_POINT('Ctrl Pts',(4.74299424650599,-6.5976594491307,8.28124780044818));
#162465=CARTESIAN_POINT('Ctrl Pts',(4.80256263212642,-6.55442573802253,
8.28411960099532));
#162466=CARTESIAN_POINT('Ctrl Pts',(4.91349663191918,-6.47158743553914,
8.28952971157284));
#162467=CARTESIAN_POINT('Ctrl Pts',(4.96499146371565,-6.43216548429352,
8.29206687621601));
#162468=CARTESIAN_POINT('Ctrl Pts',(5.05903338116241,-6.35836927304515,
8.296751040562));
#162469=CARTESIAN_POINT('Ctrl Pts',(5.10171596297473,-6.32417368297417,
8.29889676889834));
#162470=CARTESIAN_POINT('Ctrl Pts',(5.19745840068094,-6.24586857462188,
8.3037565424415));
#162471=CARTESIAN_POINT('Ctrl Pts',(5.25030812133242,-6.20150890148645,
8.30647223130618));
#162472=CARTESIAN_POINT('Ctrl Pts',(5.42107177510248,-6.05442992635263,
8.31535998394037));
#162473=CARTESIAN_POINT('Ctrl Pts',(5.53658565480808,-5.94897970908474,
8.32155244944679));
#162474=CARTESIAN_POINT('Ctrl Pts',(5.70878421389509,-5.78242095659344,
8.33107799120264));
#162475=CARTESIAN_POINT('Ctrl Pts',(5.76769248563614,-5.723664266293,8.33439237140566));
#162476=CARTESIAN_POINT('Ctrl Pts',(6.0559574272559,-5.42717105058736,8.35089274022879));
#162477=CARTESIAN_POINT('Ctrl Pts',(6.2715688575507,-5.17650744042051,8.36415444487014));
#162478=CARTESIAN_POINT('Ctrl Pts',(6.52492715487124,-4.84281645342351,
8.38085641292913));
#162479=CARTESIAN_POINT('Ctrl Pts',(6.5773732338078,-4.77134227228956,8.38438142795461));
#162480=CARTESIAN_POINT('Ctrl Pts',(6.66361502264975,-4.64968600124284,
8.39028776082471));
#162481=CARTESIAN_POINT('Ctrl Pts',(6.69803878443076,-4.59995886886304,
8.39267637007353));
#162482=CARTESIAN_POINT('Ctrl Pts',(6.74680944483229,-4.5277984047061,8.39610391506119));
#162483=CARTESIAN_POINT('Ctrl Pts',(6.76160614123683,-4.50567181191829,
8.397149745348));
#162484=CARTESIAN_POINT('Ctrl Pts',(6.78729471156454,-4.46684626137138,
8.39897564398917));
#162485=CARTESIAN_POINT('Ctrl Pts',(6.79823433660271,-4.45017920227608,
8.39975651910052));
#162486=CARTESIAN_POINT('Ctrl Pts',(6.82102753639908,-4.41517244868763,
8.40139035447707));
#162487=CARTESIAN_POINT('Ctrl Pts',(6.83286870460551,-4.39682495375392,
8.40224305178656));
#162488=CARTESIAN_POINT('Ctrl Pts',(6.86781577781336,-4.34219349938828,
8.40477146175581));
#162489=CARTESIAN_POINT('Ctrl Pts',(6.89070769428885,-4.30577350163387,
8.40644334798275));
#162490=CARTESIAN_POINT('Ctrl Pts',(7.0112870914248,-4.11051258713604,8.41534049658046));
#162491=CARTESIAN_POINT('Ctrl Pts',(7.10377488535658,-3.9485243079388,8.42249021582988));
#162492=CARTESIAN_POINT('Ctrl Pts',(7.29946044159808,-3.57662010723258,
8.43857951931458));
#162493=CARTESIAN_POINT('Ctrl Pts',(7.3993338569666,-3.3651436925088,8.44750749987546));
#162494=CARTESIAN_POINT('Ctrl Pts',(7.51517549881037,-3.08966980570351,
8.45900823862386));
#162495=CARTESIAN_POINT('Ctrl Pts',(7.53967931607756,-3.02938245285457,
8.46151716705563));
#162496=CARTESIAN_POINT('Ctrl Pts',(7.59557544302184,-2.88697917594726,
8.46742875446918));
#162497=CARTESIAN_POINT('Ctrl Pts',(7.62636445055141,-2.80463548270725,
8.4708357836797));
#162498=CARTESIAN_POINT('Ctrl Pts',(7.67031490234861,-2.68101314961786,
8.47593878056291));
#162499=CARTESIAN_POINT('Ctrl Pts',(7.68449231014864,-2.64010229452998,
8.47762558520713));
#162500=CARTESIAN_POINT('Ctrl Pts',(7.70955205412459,-2.56587661997485,
8.48068298548938));
#162501=CARTESIAN_POINT('Ctrl Pts',(7.7205471384761,-2.53260095087661,8.48205254031005));
#162502=CARTESIAN_POINT('Ctrl Pts',(7.74389349668088,-2.46038010874637,
8.48502288731742));
#162503=CARTESIAN_POINT('Ctrl Pts',(7.75616699032932,-2.4214108220697,8.48662432381654));
#162504=CARTESIAN_POINT('Ctrl Pts',(7.7896006527893,-2.31239346806226,8.49110106700274));
#162505=CARTESIAN_POINT('Ctrl Pts',(7.81010919421641,-2.24214989816937,
8.49398182492996));
#162506=CARTESIAN_POINT('Ctrl Pts',(7.90802503056263,-1.88912242516791,
8.5084425888189));
#162507=CARTESIAN_POINT('Ctrl Pts',(7.97103478925703,-1.60257423112907,
8.52013667610983));
#162508=CARTESIAN_POINT('Ctrl Pts',(8.03709931868304,-1.19919940431071,
8.53643679629225));
#162509=CARTESIAN_POINT('Ctrl Pts',(8.05334343877357,-1.0847600246756,8.54104175269497));
#162510=CARTESIAN_POINT('Ctrl Pts',(8.0754214269259,-0.901147769265471,
8.54838203796153));
#162511=CARTESIAN_POINT('Ctrl Pts',(8.0828198330413,-0.832179165420568,
8.55112833007654));
#162512=CARTESIAN_POINT('Ctrl Pts',(8.0918512957371,-0.736443058255913,
8.55492142841022));
#162513=CARTESIAN_POINT('Ctrl Pts',(8.09423628599722,-0.709749761455962,
8.55597697178944));
#162514=CARTESIAN_POINT('Ctrl Pts',(8.09808970663029,-0.664073159925274,
8.55777935247312));
#162515=CARTESIAN_POINT('Ctrl Pts',(8.09962355278008,-0.645095624269162,
8.55852706959161));
#162516=CARTESIAN_POINT('Ctrl Pts',(8.10263537568373,-0.606126529499454,
8.56005999836525));
#162517=CARTESIAN_POINT('Ctrl Pts',(8.10410609618441,-0.586134613668799,
8.56084507042151));
#162518=CARTESIAN_POINT('Ctrl Pts',(8.10797637599208,-0.530723036553506,
8.5630173824105));
#162519=CARTESIAN_POINT('Ctrl Pts',(8.11021781218605,-0.495292754225757,
8.56440225631748));
#162520=CARTESIAN_POINT('Ctrl Pts',(8.1209324651045,-0.306274760923921,
8.5717709197774));
#162521=CARTESIAN_POINT('Ctrl Pts',(8.12527528680076,-0.152482634129329,
8.57769777076142));
#162522=CARTESIAN_POINT('Ctrl Pts',(8.125182719626,0.408164825321524,8.59918056248831));
#162523=CARTESIAN_POINT('Ctrl Pts',(8.09456184005172,0.814411360073113,
8.61452497607626));
#162524=CARTESIAN_POINT('Ctrl Pts',(8.01329831772904,1.35099982553224,8.6351925936212));
#162525=CARTESIAN_POINT('Ctrl Pts',(7.98958556626881,1.4848139978795,8.64037875206134));
#162526=CARTESIAN_POINT('Ctrl Pts',(7.91719876941115,1.84105174360256,8.65430843227127));
#162527=CARTESIAN_POINT('Ctrl Pts',(7.86251460153513,2.06212749641007,8.66308426533485));
#162528=CARTESIAN_POINT('Ctrl Pts',(7.77992147013455,2.34455711414634,8.6745246926588));
#162529=CARTESIAN_POINT('Ctrl Pts',(7.76043598271661,2.40826897182255,8.67712067203412));
#162530=CARTESIAN_POINT('Ctrl Pts',(7.72766479468173,2.51089108503831,8.68132786711606));
#162531=CARTESIAN_POINT('Ctrl Pts',(7.71486341604042,2.54995287755799,8.68293537427143));
#162532=CARTESIAN_POINT('Ctrl Pts',(7.68968758118228,2.62484847548354,8.68602953626025));
#162533=CARTESIAN_POINT('Ctrl Pts',(7.67735765786065,2.66069614914523,8.6875158289862));
#162534=CARTESIAN_POINT('Ctrl Pts',(7.64810768996246,2.74384027551099,8.69097567914695));
#162535=CARTESIAN_POINT('Ctrl Pts',(7.6309990348167,2.79106868453185,8.69295050739298));
#162536=CARTESIAN_POINT('Ctrl Pts',(7.57333148275497,2.94576505567647,8.69945091666786));
#162537=CARTESIAN_POINT('Ctrl Pts',(7.53093177068594,3.05253139720528,8.70398826968992));
#162538=CARTESIAN_POINT('Ctrl Pts',(7.24063133272663,3.74063206243468,8.73356875176072));
#162539=CARTESIAN_POINT('Ctrl Pts',(6.9279019071613,4.29222491871825,8.7589090755481));
#162540=CARTESIAN_POINT('Ctrl Pts',(6.30402989153378,5.14377470095022,8.80307618079208));
#162541=CARTESIAN_POINT('Ctrl Pts',(6.0272806678017,5.46544475055119,8.82116457929401));
#162542=CARTESIAN_POINT('Ctrl Pts',(5.54484101561906,5.94475867454676,8.84969961406211));
#162543=CARTESIAN_POINT('Ctrl Pts',(5.35450696844494,6.11675429558451,8.86031290433557));
#162544=CARTESIAN_POINT('Ctrl Pts',(5.14095158526736,6.29211423259743,8.87130511686792));
#162545=CARTESIAN_POINT('Ctrl Pts',(5.12550340556368,6.30470455818851,8.87209529929975));
#162546=CARTESIAN_POINT('Ctrl Pts',(5.10250147071666,6.32331080571663,8.87326430691714));
#162547=CARTESIAN_POINT('Ctrl Pts',(5.0949831202747,6.32937025378214,8.87364521461099));
#162548=CARTESIAN_POINT('Ctrl Pts',(5.08208854913336,6.33972482781171,8.87429643918843));
#162549=CARTESIAN_POINT('Ctrl Pts',(5.07671764987614,6.344026546085,8.87456707919515));
#162550=CARTESIAN_POINT('Ctrl Pts',(5.06568701150684,6.35283834495498,8.87512165091374));
#162551=CARTESIAN_POINT('Ctrl Pts',(5.06002669774812,6.35734769807042,8.87540554630125));
#162552=CARTESIAN_POINT('Ctrl Pts',(5.04694262300288,6.36774273001224,8.87606019979413));
#162553=CARTESIAN_POINT('Ctrl Pts',(5.03951456873107,6.37362300642583,8.87643068373376));
#162554=CARTESIAN_POINT('Ctrl Pts',(5.01621366716805,6.39200251754911,8.87758912836506));
#162555=CARTESIAN_POINT('Ctrl Pts',(5.00030439788749,6.40445561132186,8.87837469463885));
#162556=CARTESIAN_POINT('Ctrl Pts',(4.71661439390168,6.62481452093798,8.89228460660483));
#162557=CARTESIAN_POINT('Ctrl Pts',(4.43612901921814,6.81581818506839,8.90437727330124));
#162558=CARTESIAN_POINT('Ctrl Pts',(3.9577308585481,7.09952262867376,8.92349279391847));
#162559=CARTESIAN_POINT('Ctrl Pts',(3.76655789947534,7.20277030241508,8.93077367961808));
#162560=CARTESIAN_POINT('Ctrl Pts',(3.32598231856728,7.41837101108538,8.94714853350188));
#162561=CARTESIAN_POINT('Ctrl Pts',(3.07458504197616,7.52604224706054,8.95621727660027));
#162562=CARTESIAN_POINT('Ctrl Pts',(2.32875672476372,7.80185513908871,8.98317481311338));
#162563=CARTESIAN_POINT('Ctrl Pts',(1.82302384374018,7.93527320198415,9.00159640601862));
#162564=CARTESIAN_POINT('Ctrl Pts',(1.27586993043952,8.02451894916715,9.02290721311776));
#162565=CARTESIAN_POINT('Ctrl Pts',(1.2436925431829,8.02956893449013,9.0241650507121));
#162566=CARTESIAN_POINT('Ctrl Pts',(1.19896070351345,8.0363139088088,9.02592017373139));
#162567=CARTESIAN_POINT('Ctrl Pts',(1.18643116178892,8.03817324434369,9.02641249913906));
#162568=CARTESIAN_POINT('Ctrl Pts',(1.16485239355959,8.04132389716677,9.02726162938249));
#162569=CARTESIAN_POINT('Ctrl Pts',(1.15580522569965,8.04262925898584,9.02761801037268));
#162570=CARTESIAN_POINT('Ctrl Pts',(1.13713608099941,8.04529076648824,9.02835418797354));
#162571=CARTESIAN_POINT('Ctrl Pts',(1.12751383727057,8.04664492382057,9.02873404383304));
#162572=CARTESIAN_POINT('Ctrl Pts',(1.10512450230696,8.04975487069735,9.02961889481034));
#162573=CARTESIAN_POINT('Ctrl Pts',(1.09235563325358,8.05149755092593,9.0301242833098));
#162574=CARTESIAN_POINT('Ctrl Pts',(1.05170670195827,8.05694679218192,9.03173555755846));
#162575=CARTESIAN_POINT('Ctrl Pts',(1.02381165509941,8.06053895683023,9.032844875136));
#162576=CARTESIAN_POINT('Ctrl Pts',(0.48231095226244,8.12741405139886,9.05444963470158));
#162577=CARTESIAN_POINT('Ctrl Pts',(-0.0360949400586856,8.14162538617692,
9.07646773667047));
#162578=CARTESIAN_POINT('Ctrl Pts',(-1.32616395195673,8.05373575201676,
9.13370019919003));
#162579=CARTESIAN_POINT('Ctrl Pts',(-2.08855332663799,7.89046719957832,
9.16985986382854));
#162580=CARTESIAN_POINT('Ctrl Pts',(-2.85440477111827,7.60747762210895,
9.20281494154776));
#162581=CARTESIAN_POINT('Ctrl Pts',(-2.89245649901079,7.59309145573709,
9.20444316449478));
#162582=CARTESIAN_POINT('Ctrl Pts',(-2.94287120840034,7.57359725797457,
9.20658994141164));
#162583=CARTESIAN_POINT('Ctrl Pts',(-2.95533147876041,7.56874376820314,
9.20711967626199));
#162584=CARTESIAN_POINT('Ctrl Pts',(-2.97470799783421,7.56114113611318,
9.20794219173996));
#162585=CARTESIAN_POINT('Ctrl Pts',(-2.98163251263289,7.55841322717335,
9.20823588082018));
#162586=CARTESIAN_POINT('Ctrl Pts',(-2.99552710024956,7.55291739641583,
9.2088247046404));
#162587=CARTESIAN_POINT('Ctrl Pts',(-3.0024971079398,7.55014933115094,9.2091198328891));
#162588=CARTESIAN_POINT('Ctrl Pts',(-3.01810397376515,7.54392619916122,
9.20978013448992));
#162589=CARTESIAN_POINT('Ctrl Pts',(-3.0267387593589,7.54046593907381,9.2101450918043));
#162590=CARTESIAN_POINT('Ctrl Pts',(-3.05215445956522,7.530230290043,9.21121827508495));
#162591=CARTESIAN_POINT('Ctrl Pts',(-3.06891876179363,7.52341363384642,
9.21192482032293));
#162592=CARTESIAN_POINT('Ctrl Pts',(-3.19928010648258,7.46989821802504,
9.21740951179803));
#162593=CARTESIAN_POINT('Ctrl Pts',(-3.31183101789318,7.4206838984056,9.22208881726159));
#162594=CARTESIAN_POINT('Ctrl Pts',(-3.72771333181943,7.2274865252283,9.23929557784815));
#162595=CARTESIAN_POINT('Ctrl Pts',(-4.02315264457134,7.06729559820798,
9.25136337991569));
#162596=CARTESIAN_POINT('Ctrl Pts',(-4.84462103407879,6.55363455182756,
9.2861515482775));
#162597=CARTESIAN_POINT('Ctrl Pts',(-5.34030882697556,6.15642318869333,
9.30890778908585));
#162598=CARTESIAN_POINT('Ctrl Pts',(-5.84624108327607,5.64347368663516,
9.33644066665696));
#162599=CARTESIAN_POINT('Ctrl Pts',(-5.9066210350818,5.58024710267164,9.33980240538738));
#162600=CARTESIAN_POINT('Ctrl Pts',(-5.98906341417004,5.49108043051823,
9.34450029453073));
#162601=CARTESIAN_POINT('Ctrl Pts',(-6.01200119246856,5.46595705431438,
9.34581932250214));
#162602=CARTESIAN_POINT('Ctrl Pts',(-6.04866028798457,5.42529501067237,
9.34794671475477));
#162603=CARTESIAN_POINT('Ctrl Pts',(-6.06248114301694,5.40984654305795,
9.34875325234681));
#162604=CARTESIAN_POINT('Ctrl Pts',(-6.09077359222066,5.37797765523366,
9.35041355318815));
#162605=CARTESIAN_POINT('Ctrl Pts',(-6.10523826906305,5.36155129479687,
9.35126741735504));
#162606=CARTESIAN_POINT('Ctrl Pts',(-6.13757949360315,5.32452340645861,
9.35318802353218));
#162607=CARTESIAN_POINT('Ctrl Pts',(-6.1554190126457,5.30388992316072,9.35425541150572));
#162608=CARTESIAN_POINT('Ctrl Pts',(-6.20822369417321,5.24218991622258,
9.35743914425395));
#162609=CARTESIAN_POINT('Ctrl Pts',(-6.24288405600679,5.20086484658591,
9.35956099384458));
#162610=CARTESIAN_POINT('Ctrl Pts',(-6.65761041079696,4.69627259410928,
9.3853540921076));
#162611=CARTESIAN_POINT('Ctrl Pts',(-6.98568565628412,4.19271383247046,
9.41012990363884));
#162612=CARTESIAN_POINT('Ctrl Pts',(-7.33118660057727,3.50738292618752,
9.44263593248867));
#162613=CARTESIAN_POINT('Ctrl Pts',(-7.40228494005331,3.35472942106161,
9.44979119382671));
#162614=CARTESIAN_POINT('Ctrl Pts',(-7.61299214213051,2.86294930949839,
9.47246190222982));
#162615=CARTESIAN_POINT('Ctrl Pts',(-7.73442249284311,2.51651720664905,
9.48789027845702));
#162616=CARTESIAN_POINT('Ctrl Pts',(-7.83824832364922,2.14058273843573,
9.50344609326389));
#162617=CARTESIAN_POINT('Ctrl Pts',(-7.84435889627673,2.11808044292194,
9.50437270577527));
#162618=CARTESIAN_POINT('Ctrl Pts',(-7.85276810773991,2.08657779247594,
9.50566337810948));
#162619=CARTESIAN_POINT('Ctrl Pts',(-7.85514827453566,2.07759943778976,
9.50603047996719));
#162620=CARTESIAN_POINT('Ctrl Pts',(-7.85946989663317,2.06118402496943,
9.50670028345169));
#162621=CARTESIAN_POINT('Ctrl Pts',(-7.86141620305199,2.05374826202169,
9.50700317026875));
#162622=CARTESIAN_POINT('Ctrl Pts',(-7.86532383065232,2.03873242612407,
9.50761376504513));
#162623=CARTESIAN_POINT('Ctrl Pts',(-7.86728475257214,2.03115225643798,
9.5079214572226));
#162624=CARTESIAN_POINT('Ctrl Pts',(-7.87205877013605,2.01258710735715,
9.50867370150504));
#162625=CARTESIAN_POINT('Ctrl Pts',(-7.87485983766816,2.0015990317497,9.50911777541884));
#162626=CARTESIAN_POINT('Ctrl Pts',(-7.88485054513738,1.96206171915785,
9.51071141632596));
#162627=CARTESIAN_POINT('Ctrl Pts',(-7.89190806413483,1.93347910414778,
9.5118555859956));
#162628=CARTESIAN_POINT('Ctrl Pts',(-7.93008327903596,1.77517927702798,
9.5181464593863));
#162629=CARTESIAN_POINT('Ctrl Pts',(-7.95815733801256,1.64475346712227,
9.52314819155498));
#162630=CARTESIAN_POINT('Ctrl Pts',(-7.99856259789834,1.43166158392886,
9.53108050670572));
#162631=CARTESIAN_POINT('Ctrl Pts',(-8.01285176661908,1.34939453128148,
9.53408679184817));
#162632=CARTESIAN_POINT('Ctrl Pts',(-8.10241914036645,0.78199017682363,
9.55451076146514));
#162633=CARTESIAN_POINT('Ctrl Pts',(-8.13486373541702,0.291100010976691,
9.57066610291255));
#162634=CARTESIAN_POINT('Ctrl Pts',(-8.10837268012976,-0.786262068619116,
9.60708870836392));
#162635=CARTESIAN_POINT('Ctrl Pts',(-8.03047078835915,-1.36944161749787,
9.62751658244886));
#162636=CARTESIAN_POINT('Ctrl Pts',(-7.88168299525032,-1.97487099089194,
9.65144491329839));
#162637=CARTESIAN_POINT('Ctrl Pts',(-7.87265630206983,-2.01055340043818,
9.65286487400218));
#162638=CARTESIAN_POINT('Ctrl Pts',(-7.86002757618888,-2.05908525329603,
9.65480966336704));
#162639=CARTESIAN_POINT('Ctrl Pts',(-7.85663581582393,-2.07198919743552,
9.65532805910014));
#162640=CARTESIAN_POINT('Ctrl Pts',(-7.85081990499647,-2.09389620389514,
9.65621036854512));
#162641=CARTESIAN_POINT('Ctrl Pts',(-7.84841200861653,-2.10290357260312,
9.65657378365717));
#162642=CARTESIAN_POINT('Ctrl Pts',(-7.84373325546249,-2.12028570552623,
9.65727633463989));
#162643=CARTESIAN_POINT('Ctrl Pts',(-7.84146447564054,-2.12866101872184,
9.65761540639882));
#162644=CARTESIAN_POINT('Ctrl Pts',(-7.8360621465402,-2.14847814330986,
9.65841902335726));
#162645=CARTESIAN_POINT('Ctrl Pts',(-7.8329169505939,-2.15991674385787,
9.658883925919));
#162646=CARTESIAN_POINT('Ctrl Pts',(-7.82361092763713,-2.19347368165725,
9.66025088530729));
#162647=CARTESIAN_POINT('Ctrl Pts',(-7.81738140832054,-2.21557275790414,
9.66115505425801));
#162648=CARTESIAN_POINT('Ctrl Pts',(-7.76978174448922,-2.38173126239937,
9.6679833466699));
#162649=CARTESIAN_POINT('Ctrl Pts',(-7.72452776439988,-2.52464255814885,
9.67402720316051));
#162650=CARTESIAN_POINT('Ctrl Pts',(-7.55909379323849,-3.00088429411161,
9.69476095408454));
#162651=CARTESIAN_POINT('Ctrl Pts',(-7.42108433541074,-3.32756334259877,
9.70999610653406));
#162652=CARTESIAN_POINT('Ctrl Pts',(-7.0424348097251,-4.08214664848373,
9.74732285693284));
#162653=CARTESIAN_POINT('Ctrl Pts',(-6.78349995443966,-4.49932380980036,
9.76975394677767));
#162654=CARTESIAN_POINT('Ctrl Pts',(-6.26862024336325,-5.18243370737129,
9.80777817620634));
#162655=CARTESIAN_POINT('Ctrl Pts',(-6.02920071011497,-5.45912507791164,
9.82358536800317));
#162656=CARTESIAN_POINT('Ctrl Pts',(-5.75455485135851,-5.73632241861889,
9.83917321402805));
#162657=CARTESIAN_POINT('Ctrl Pts',(-5.73710781529798,-5.75377183790873,
9.84015380791609));
#162658=CARTESIAN_POINT('Ctrl Pts',(-5.71282150511364,-5.77784117065954,
9.8415059651135));
#162659=CARTESIAN_POINT('Ctrl Pts',(-5.70604979967101,-5.78452883365565,
9.84188161316139));
#162660=CARTESIAN_POINT('Ctrl Pts',(-5.69438876068727,-5.79600474782677,
9.84252616691749));
#162661=CARTESIAN_POINT('Ctrl Pts',(-5.68950510908996,-5.80079873885671,
9.84279540958758));
#162662=CARTESIAN_POINT('Ctrl Pts',(-5.6794335687255,-5.81066041825461,
9.84334924853374));
#162663=CARTESIAN_POINT('Ctrl Pts',(-5.67424493946721,-5.81572734274852,
9.8436338008379));
#162664=CARTESIAN_POINT('Ctrl Pts',(-5.6621888395409,-5.82746916111994,
9.84429320334781));
#162665=CARTESIAN_POINT('Ctrl Pts',(-5.65531632918775,-5.83413888215379,
9.84466776187203));
#162666=CARTESIAN_POINT('Ctrl Pts',(-5.63381755770509,-5.85492959969573,
9.84583537805118));
#162667=CARTESIAN_POINT('Ctrl Pts',(-5.6191500153604,-5.86900792340847,
9.84662609561483));
#162668=CARTESIAN_POINT('Ctrl Pts',(-5.47792635059363,-6.00354368998127,
9.8541847864595));
#162669=CARTESIAN_POINT('Ctrl Pts',(-5.34756372359454,-6.11994939718079,
9.8607446446613));
#162670=CARTESIAN_POINT('Ctrl Pts',(-5.06320898874539,-6.35783143124494,
9.87441729713133));
#162671=CARTESIAN_POINT('Ctrl Pts',(-4.90836798574893,-6.47811951448859,
9.88149629424793));
#162672=CARTESIAN_POINT('Ctrl Pts',(-4.503555850863,-6.7697431564852,9.8994161294254));
#162673=CARTESIAN_POINT('Ctrl Pts',(-4.24807861511865,-6.93291179475225,
9.91019819615098));
#162674=CARTESIAN_POINT('Ctrl Pts',(-3.43354064838567,-7.39117918649344,
9.94400062722491));
#162675=CARTESIAN_POINT('Ctrl Pts',(-2.84878029242084,-7.63564635039871,
9.96770957252968));
#162676=CARTESIAN_POINT('Ctrl Pts',(-2.12767790626376,-7.84262312616943,
9.99667905926199));
#162677=CARTESIAN_POINT('Ctrl Pts',(-2.01299010490966,-7.87284073630419,
10.0012752615384));
#162678=CARTESIAN_POINT('Ctrl Pts',(-1.85187288485123,-7.91154055837685,
10.0077272668261));
#162679=CARTESIAN_POINT('Ctrl Pts',(-1.8059682307994,-7.9221452847949,10.0095649703947));
#162680=CARTESIAN_POINT('Ctrl Pts',(-1.72237421614428,-7.9406925369856,
10.0129112107143));
#162681=CARTESIAN_POINT('Ctrl Pts',(-1.68471560644113,-7.94876746539863,
10.0144185674137));
#162682=CARTESIAN_POINT('Ctrl Pts',(-1.61263541033176,-7.96368797734493,
10.0173039002247));
#162683=CARTESIAN_POINT('Ctrl Pts',(-1.5782240700626,-7.97057889623961,
10.0186814493681));
#162684=CARTESIAN_POINT('Ctrl Pts',(-1.49382579057793,-7.9869117832368,
10.0220606065234));
#162685=CARTESIAN_POINT('Ctrl Pts',(-1.44379283484209,-7.99610764953757,
10.0240643017052));
#162686=CARTESIAN_POINT('Ctrl Pts',(-1.26794720997423,-8.02672315391913,
10.0311094126743));
#162687=CARTESIAN_POINT('Ctrl Pts',(-1.14172019073502,-8.04564784278232,
10.036172023216));
#162688=CARTESIAN_POINT('Ctrl Pts',(-0.831905031029516,-8.08465920321975,
10.0486211603613));
#162689=CARTESIAN_POINT('Ctrl Pts',(-0.647977991701629,-8.10147539601015,
10.0560321969358));
#162690=CARTESIAN_POINT('Ctrl Pts',(-0.179355597340776,-8.12825939199799,
10.0749737423686));
#162691=CARTESIAN_POINT('Ctrl Pts',(0.105584676168758,-8.12955219632266,
10.0865490769958));
#162692=CARTESIAN_POINT('Ctrl Pts',(0.495020917070936,-8.11083821153645,
10.1023925010561));
#162693=CARTESIAN_POINT('Ctrl Pts',(0.599933168815925,-8.1037536052002,
10.1066623410405));
#162694=CARTESIAN_POINT('Ctrl Pts',(0.865215571781854,-8.08065944319061,
10.1174530550649));
#162695=CARTESIAN_POINT('Ctrl Pts',(1.02530286659011,-8.06191106427882,
10.1239594023143));
#162696=CARTESIAN_POINT('Ctrl Pts',(1.28238060144516,-8.0240221059192,10.1343683114038));
#162697=CARTESIAN_POINT('Ctrl Pts',(1.37976393642195,-8.00785131075567,
10.138301999353));
#162698=CARTESIAN_POINT('Ctrl Pts',(1.5072753911121,-7.9842825032573,10.1434336478598));
#162699=CARTESIAN_POINT('Ctrl Pts',(1.53768918019316,-7.97848094536262,
10.1446562050728));
#162700=CARTESIAN_POINT('Ctrl Pts',(1.58505001863631,-7.96916579729514,
10.1465574892036));
#162701=CARTESIAN_POINT('Ctrl Pts',(1.6020201298794,-7.9657716871767,10.1472382321943));
#162702=CARTESIAN_POINT('Ctrl Pts',(1.63425463311115,-7.95921744504413,
10.1485303651622));
#162703=CARTESIAN_POINT('Ctrl Pts',(1.64952096862422,-7.9560675662774,10.1491419362434));
#162704=CARTESIAN_POINT('Ctrl Pts',(1.66482904541191,-7.95286312058463,
10.1497548497821));
#162705=CARTESIAN_POINT('Ctrl Pts',(1.66487991835834,-7.95285247082126,
10.1497568866586));
#162706=CARTESIAN_POINT('Ctrl Pts',(1.66498154272579,-7.95283119571714,
10.1497609555386));
#162707=CARTESIAN_POINT('Ctrl Pts',(1.6650323007612,-7.95282056899382,10.1497629878069));
#162708=CARTESIAN_POINT('Ctrl Pts',(1.66513370577417,-7.95279933778493,
10.1497670478897));
#162709=CARTESIAN_POINT('Ctrl Pts',(1.66518435252817,-7.95278873334837,
10.1497690756953));
#162710=CARTESIAN_POINT('Ctrl Pts',(1.66528553548582,-7.95276754661342,
10.149773126873));
#162711=CARTESIAN_POINT('Ctrl Pts',(1.66533607193129,-7.95275696426656,
10.1497751502548));
#162712=CARTESIAN_POINT('Ctrl Pts',(1.665437035628,-7.95273582143359,10.1497791926392));
#162713=CARTESIAN_POINT('Ctrl Pts',(1.66548746296985,-7.95272526093066,
10.1497812116456));
#162714=CARTESIAN_POINT('Ctrl Pts',(1.66558820962998,-7.95270416154685,
10.149785245326));
#162715=CARTESIAN_POINT('Ctrl Pts',(1.66563852899509,-7.95269362265831,
10.149787260002));
#162716=CARTESIAN_POINT('Ctrl Pts',(1.66573906108083,-7.95267256622083,
10.1497912850771));
#162717=CARTESIAN_POINT('Ctrl Pts',(1.6657892737062,-7.95266204869396,10.1497932954724));
#162718=CARTESIAN_POINT('Ctrl Pts',(1.66588959330177,-7.95264103477893,
10.1497973120257));
#162719=CARTESIAN_POINT('Ctrl Pts',(1.66593970029281,-7.95263053838849,
10.1497993181845));
#162720=CARTESIAN_POINT('Ctrl Pts',(1.66603980961057,-7.95260956654498,
10.1498033263047));
#162721=CARTESIAN_POINT('Ctrl Pts',(1.66608981196689,-7.95259909108778,
10.1498053282672));
#162722=CARTESIAN_POINT('Ctrl Pts',(1.66618971384362,-7.95257816073385,
10.1498093280679));
#162723=CARTESIAN_POINT('Ctrl Pts',(1.66623961300413,-7.95256770591455,
10.1498113258917));
#162724=CARTESIAN_POINT('Ctrl Pts',(1.66633930880072,-7.95254681677726,
10.1498153174276));
#162725=CARTESIAN_POINT('Ctrl Pts',(1.66638910563149,-7.95253638242047,
10.1498173111474));
#162726=CARTESIAN_POINT('Ctrl Pts',(1.6664885980956,-7.95251553393613,10.1498212945285));
#162727=CARTESIAN_POINT('Ctrl Pts',(1.66653829373343,-7.95250511980962,
10.1498232841899));
#162728=CARTESIAN_POINT('Ctrl Pts',(1.66663758511132,-7.95248431151939,
10.1498272595062));
#162729=CARTESIAN_POINT('Ctrl Pts',(1.6666871807584,-7.95247391737712,10.1498292451574));
#162730=CARTESIAN_POINT('Ctrl Pts',(1.66678627291365,-7.95245314890218,
10.1498332124837));
#162731=CARTESIAN_POINT('Ctrl Pts',(1.66683576954283,-7.95244277454608,
10.1498351941636));
#162732=CARTESIAN_POINT('Ctrl Pts',(1.66693466489529,-7.95242204539082,
10.1498391535969));
#162733=CARTESIAN_POINT('Ctrl Pts',(1.66698406360673,-7.95241169059605,
10.1498411313497));
#162734=CARTESIAN_POINT('Ctrl Pts',(1.66708276439456,-7.95239100030275,
10.1498450829795));
#162735=CARTESIAN_POINT('Ctrl Pts',(1.66713206638249,-7.95238066482464,
10.149847056853));
#162736=CARTESIAN_POINT('Ctrl Pts',(1.66723057429436,-7.95236001305058,
10.1498510007472));
#162737=CARTESIAN_POINT('Ctrl Pts',(1.66727978041752,-7.95234969671471,
10.1498529707758));
#162738=CARTESIAN_POINT('Ctrl Pts',(1.66737809812419,-7.9523290829111,10.1498569070413));
#162739=CARTESIAN_POINT('Ctrl Pts',(1.66742720957816,-7.95231878547235,
10.149858873273));
#162740=CARTESIAN_POINT('Ctrl Pts',(1.66752533900274,-7.95229820924695,
10.149862801987));
#162741=CARTESIAN_POINT('Ctrl Pts',(1.66757435693084,-7.95228793047102,
10.1498647644675));
#162742=CARTESIAN_POINT('Ctrl Pts',(1.66767229972826,-7.95226739148766,
10.1498686856962));
#162743=CARTESIAN_POINT('Ctrl Pts',(1.66772122492586,-7.95225713121317,
10.1498706444575));
#162744=CARTESIAN_POINT('Ctrl Pts',(1.66781898376004,-7.95223662892392,
10.1498745583077));
#162745=CARTESIAN_POINT('Ctrl Pts',(1.66786781735956,-7.95222638691869,
10.1498765133951));
#162746=CARTESIAN_POINT('Ctrl Pts',(1.66796539419119,-7.95220592092289,
10.1498804199454));
#162747=CARTESIAN_POINT('Ctrl Pts',(1.66801413731788,-7.95219569695616,
10.149882371404));
#162748=CARTESIAN_POINT('Ctrl Pts',(1.66811153371643,-7.95217526693505,
10.1498862707173));
#162749=CARTESIAN_POINT('Ctrl Pts',(1.66816018711285,-7.95216506085626,
10.1498882185769));
#162750=CARTESIAN_POINT('Ctrl Pts',(1.66825740605545,-7.95214466619563,
10.1498921107724));
#162751=CARTESIAN_POINT('Ctrl Pts',(1.66830597113018,-7.95213447771438,
10.1498940550894));
#162752=CARTESIAN_POINT('Ctrl Pts',(1.66840301361363,-7.95211411821526,
10.1498979402072));
#162753=CARTESIAN_POINT('Ctrl Pts',(1.66845149114522,-7.95210394717328,
10.1498998810129));
#162754=CARTESIAN_POINT('Ctrl Pts',(1.6685483596427,-7.95208362232682,10.149903759152));
#162755=CARTESIAN_POINT('Ctrl Pts',(1.66859675065309,-7.95207346851466,
10.1499056964872));
#162756=CARTESIAN_POINT('Ctrl Pts',(1.66869344705058,-7.95205317793503,
10.1499095677233));
#162757=CARTESIAN_POINT('Ctrl Pts',(1.66874175247925,-7.95204304116047,
10.1499115016258));
#162758=CARTESIAN_POINT('Ctrl Pts',(1.66883827893448,-7.95202278440465,
10.1499153660452));
#162759=CARTESIAN_POINT('Ctrl Pts',(1.66888649985005,-7.95201266444829,
10.1499172965577));
#162760=CARTESIAN_POINT('Ctrl Pts',(1.66898285814562,-7.9519924411518,10.149921154232));
#162761=CARTESIAN_POINT('Ctrl Pts',(1.66903099552138,-7.95198233781415,
10.1499230813935));
#162762=CARTESIAN_POINT('Ctrl Pts',(1.6691271875952,-7.95196214757977,10.1499269324003));
#162763=CARTESIAN_POINT('Ctrl Pts',(1.66917524238861,-7.95195206066459,
10.1499288562493));
#162764=CARTESIAN_POINT('Ctrl Pts',(1.66927127014065,-7.95193190310291,
10.1499327006647));
#162765=CARTESIAN_POINT('Ctrl Pts',(1.66931924326078,-7.95192183242404,
10.1499346212375));
#162766=CARTESIAN_POINT('Ctrl Pts',(1.66941510872256,-7.95190170711784,
10.1499384591429));
#162767=CARTESIAN_POINT('Ctrl Pts',(1.66946300113413,-7.95189165247735,
10.1499403764783));
#162768=CARTESIAN_POINT('Ctrl Pts',(1.66955870621739,-7.95187155903442,
10.1499442079503));
#162769=CARTESIAN_POINT('Ctrl Pts',(1.66960651889522,-7.95186152023219,
10.1499461220872));
#162770=CARTESIAN_POINT('Ctrl Pts',(1.66970206540729,-7.95184145828207,
10.1499499471983));
#162771=CARTESIAN_POINT('Ctrl Pts',(1.66974979926172,-7.95183143513143,
10.1499518581733));
#162772=CARTESIAN_POINT('Ctrl Pts',(1.66984518921076,-7.95181140426135,
10.1499556770039));
#162773=CARTESIAN_POINT('Ctrl Pts',(1.66989284524425,-7.95180139655621,
10.1499575848571));
#162774=CARTESIAN_POINT('Ctrl Pts',(1.66998808035551,-7.95178139641264,
10.1499613974764));
#162775=CARTESIAN_POINT('Ctrl Pts',(1.67003565949024,-7.95177140396368,
10.1499633022447));
#162776=CARTESIAN_POINT('Ctrl Pts',(1.67013074144333,-7.95175143420253,
10.14996710872));
#162777=CARTESIAN_POINT('Ctrl Pts',(1.67017824441422,-7.95174145685972,
10.1499690104329));
#162778=CARTESIAN_POINT('Ctrl Pts',(1.67027317558942,-7.95172151698958,
10.1499728108595));
#162779=CARTESIAN_POINT('Ctrl Pts',(1.67032060347758,-7.95171155453007,
10.1499747095604));
#162780=CARTESIAN_POINT('Ctrl Pts',(1.67041538549919,-7.95169164421816,
10.1499785040034));
#162781=CARTESIAN_POINT('Ctrl Pts',(1.67046273933832,-7.95168169642898,
10.1499803997337));
#162782=CARTESIAN_POINT('Ctrl Pts',(1.67055737356861,-7.95166181539744,
10.1499841882477));
#162783=CARTESIAN_POINT('Ctrl Pts',(1.67060465405356,-7.95165188213674,
10.1499860810352));
#162784=CARTESIAN_POINT('Ctrl Pts',(1.67069914295218,-7.951632029877,10.1499898637188));
#162785=CARTESIAN_POINT('Ctrl Pts',(1.67074635121749,-7.95162211091048,
10.1499917536089));
#162786=CARTESIAN_POINT('Ctrl Pts',(1.67084069584218,-7.95160228720838,
10.1499955305044));
#162787=CARTESIAN_POINT('Ctrl Pts',(1.67088783251507,-7.95159238240826,
10.1499974175224));
#162788=CARTESIAN_POINT('Ctrl Pts',(1.67098203531661,-7.9515725867568,10.150001188728));
#162789=CARTESIAN_POINT('Ctrl Pts',(1.67102910142358,-7.95156269591132,
10.1500030729149));
#162790=CARTESIAN_POINT('Ctrl Pts',(1.67112316386047,-7.95154292801185,
10.1500068384891));
#162791=CARTESIAN_POINT('Ctrl Pts',(1.67117016024723,-7.95153305094719,
10.1500087198788));
#162792=CARTESIAN_POINT('Ctrl Pts',(1.67126408417501,-7.95151331041747,
10.150012479896));
#162793=CARTESIAN_POINT('Ctrl Pts',(1.67131101174322,-7.95150344694796,
10.1500143585246));
#162794=CARTESIAN_POINT('Ctrl Pts',(1.6714047987701,-7.95148373345762,10.1500181130491));
#162795=CARTESIAN_POINT('Ctrl Pts',(1.67145165830128,-7.95147388342279,
10.1500199889479));
#162796=CARTESIAN_POINT('Ctrl Pts',(1.6715453104418,-7.95145419655589,10.1500237380606));
#162797=CARTESIAN_POINT('Ctrl Pts',(1.67159210289913,-7.95144435975701,
10.1500256112682));
#162798=CARTESIAN_POINT('Ctrl Pts',(1.67168562172243,-7.9514246991911,10.1500293550318));
#162799=CARTESIAN_POINT('Ctrl Pts',(1.6717323480043,-7.95141487544298,10.1500312255843));
#162800=CARTESIAN_POINT('Ctrl Pts',(1.67182573506276,-7.95139524085901,
10.150034964061));
#162801=CARTESIAN_POINT('Ctrl Pts',(1.67187239593607,-7.95138543000404,
10.1500368319891));
#162802=CARTESIAN_POINT('Ctrl Pts',(1.67196565308732,-7.95136582101864,
10.1500405652534));
#162803=CARTESIAN_POINT('Ctrl Pts',(1.67201224938012,-7.95135602288629,
10.1500424305902));
#162804=CARTESIAN_POINT('Ctrl Pts',(1.67210537853235,-7.95133643910533,
10.1500461587185));
#162805=CARTESIAN_POINT('Ctrl Pts',(1.67215191125789,-7.95132665348604,
10.1500480215047));
#162806=CARTESIAN_POINT('Ctrl Pts',(1.67224491351611,-7.95130709468415,
10.1500517445413));
#162807=CARTESIAN_POINT('Ctrl Pts',(1.67229138327103,-7.95129732145594,
10.1500536048007));
#162808=CARTESIAN_POINT('Ctrl Pts',(1.69057088484334,-7.94745272368089,
10.1507853616201));
#162809=CARTESIAN_POINT('Ctrl Pts',(1.70879070887859,-7.94355518819029,
10.1515142731423));
#162810=CARTESIAN_POINT('Ctrl Pts',(1.75281277139888,-7.93397964059079,
10.1532745713825));
#162811=CARTESIAN_POINT('Ctrl Pts',(1.77860106717169,-7.92823837934945,
10.1543050367159));
#162812=CARTESIAN_POINT('Ctrl Pts',(1.84850786305649,-7.91231674593432,
10.1570971787407));
#162813=CARTESIAN_POINT('Ctrl Pts',(1.89257010973498,-7.90189319194668,
10.1588557273213));
#162814=CARTESIAN_POINT('Ctrl Pts',(2.03849354505676,-7.86608234785184,
10.1646794663983));
#162815=CARTESIAN_POINT('Ctrl Pts',(2.13995013157618,-7.83908930294379,
10.1687284611599));
#162816=CARTESIAN_POINT('Ctrl Pts',(2.51647609251735,-7.73105787905047,
10.1838095159714));
#162817=CARTESIAN_POINT('Ctrl Pts',(2.78771618458517,-7.63744368176316,
10.1947921950815));
#162818=CARTESIAN_POINT('Ctrl Pts',(3.13505678288803,-7.49659012125501,
10.2092938959108));
#162819=CARTESIAN_POINT('Ctrl Pts',(3.21613064380215,-7.46216778335393,
10.2127101160946));
#162820=CARTESIAN_POINT('Ctrl Pts',(3.33613636829626,-7.40889668818547,
10.217819418823));
#162821=CARTESIAN_POINT('Ctrl Pts',(3.37550354160689,-7.39104402820663,
10.2195040381777));
#162822=CARTESIAN_POINT('Ctrl Pts',(3.44435470487714,-7.359155819407,10.2224659927665));
#162823=CARTESIAN_POINT('Ctrl Pts',(3.47390007818522,-7.34525506338436,
10.2237421270038));
#162824=CARTESIAN_POINT('Ctrl Pts',(3.5040818945928,-7.33083203171378,10.2250511143772));
#162825=CARTESIAN_POINT('Ctrl Pts',(3.50480293477164,-7.33048733643472,
10.2250823890818));
#162826=CARTESIAN_POINT('Ctrl Pts',(3.5061965566879,-7.32982085894873,10.2251428427155));
#162827=CARTESIAN_POINT('Ctrl Pts',(3.50686914502705,-7.32949909052912,
10.225172021523));
#162828=CARTESIAN_POINT('Ctrl Pts',(3.50816912171393,-7.32887695761007,
10.2252284235291));
#162829=CARTESIAN_POINT('Ctrl Pts',(3.5087965157786,-7.32857660512563,10.2252556466205));
#162830=CARTESIAN_POINT('Ctrl Pts',(3.51000915279073,-7.32799588775397,
10.2253082684474));
#162831=CARTESIAN_POINT('Ctrl Pts',(3.51059440075626,-7.3277155333018,10.2253336670913));
#162832=CARTESIAN_POINT('Ctrl Pts',(3.51172559532561,-7.32717348451479,
10.2253827627916));
#162833=CARTESIAN_POINT('Ctrl Pts',(3.51227154628423,-7.32691179926467,
10.2254064597676));
#162834=CARTESIAN_POINT('Ctrl Pts',(3.51332680799275,-7.32640584610242,
10.2254522668507));
#162835=CARTESIAN_POINT('Ctrl Pts',(3.51383612252943,-7.32616158609483,
10.2254743768878));
#162836=CARTESIAN_POINT('Ctrl Pts',(3.51482059463394,-7.32568932099896,
10.2255171172076));
#162837=CARTESIAN_POINT('Ctrl Pts',(3.5152957555056,-7.3254613227827,10.2255377474297));
#162838=CARTESIAN_POINT('Ctrl Pts',(3.51621423624747,-7.32502049479315,
10.2255776280752));
#162839=CARTESIAN_POINT('Ctrl Pts',(3.51665755898457,-7.32480767100172,
10.2255968784455));
#162840=CARTESIAN_POINT('Ctrl Pts',(3.51751452244458,-7.32439617698688,
10.2256340926169));
#162841=CARTESIAN_POINT('Ctrl Pts',(3.51792816566473,-7.32419751196616,
10.2256520563719));
#162842=CARTESIAN_POINT('Ctrl Pts',(3.51872778212257,-7.32381338792771,
10.2256867842389));
#162843=CARTESIAN_POINT('Ctrl Pts',(3.51911375752603,-7.32362793343991,
10.2257035483105));
#162844=CARTESIAN_POINT('Ctrl Pts',(3.51985991292835,-7.32326934610251,
10.2257359578351));
#162845=CARTESIAN_POINT('Ctrl Pts',(3.52022009482751,-7.32309621718691,
10.2257516032536));
#162846=CARTESIAN_POINT('Ctrl Pts',(3.52091640953461,-7.32276145580888,
10.2257818509848));
#162847=CARTESIAN_POINT('Ctrl Pts',(3.52125254398466,-7.32259982677545,
10.2257964532668));
#162848=CARTESIAN_POINT('Ctrl Pts',(3.52190239037642,-7.32228729539804,
10.2258246850882));
#162849=CARTESIAN_POINT('Ctrl Pts',(3.52221610375679,-7.32213639603381,
10.2258383146013));
#162850=CARTESIAN_POINT('Ctrl Pts',(3.52282262305852,-7.32184460600965,
10.2258646664471));
#162851=CARTESIAN_POINT('Ctrl Pts',(3.52311543022188,-7.3217037179483,10.2258773887566));
#162852=CARTESIAN_POINT('Ctrl Pts',(3.52368154816212,-7.32143128094813,
10.2259019872793));
#162853=CARTESIAN_POINT('Ctrl Pts',(3.52395486003317,-7.32129973426526,
10.2259138634728));
#162854=CARTESIAN_POINT('Ctrl Pts',(3.52448330174721,-7.32104535557484,
10.225936826679));
#162855=CARTESIAN_POINT('Ctrl Pts',(3.52473843252175,-7.32092252554165,
10.2259479136737));
#162856=CARTESIAN_POINT('Ctrl Pts',(3.5252317362463,-7.32068499787717,10.2259693515096));
#162857=CARTESIAN_POINT('Ctrl Pts',(3.52546991002964,-7.32057030195445,
10.2259797023362));
#162858=CARTESIAN_POINT('Ctrl Pts',(3.52593044019454,-7.3203484995131,10.2259997172483));
#162859=CARTESIAN_POINT('Ctrl Pts',(3.52615279729178,-7.32024139448731,
10.2260093813205));
#162860=CARTESIAN_POINT('Ctrl Pts',(3.52675068213241,-7.3199533715954,10.226035367371));
#162861=CARTESIAN_POINT('Ctrl Pts',(3.52712620082542,-7.31977243496631,
10.2260516895154));
#162862=CARTESIAN_POINT('Ctrl Pts',(3.52787186354028,-7.3194130806903,10.2260841019011));
#162863=CARTESIAN_POINT('Ctrl Pts',(3.52824201365148,-7.31923466111413,
10.2261001923827));
#162864=CARTESIAN_POINT('Ctrl Pts',(3.52897706204733,-7.31888028472595,
10.2261321467115));
#162865=CARTESIAN_POINT('Ctrl Pts',(3.52934195494318,-7.3187043314841,10.2261480103007));
#162866=CARTESIAN_POINT('Ctrl Pts',(3.53006658476145,-7.31835484444252,
10.2261795149417));
#162867=CARTESIAN_POINT('Ctrl Pts',(3.53042632206502,-7.31818131139801,
10.2261951559874));
#162868=CARTESIAN_POINT('Ctrl Pts',(3.53114074206643,-7.31783661865404,
10.2262262198812));
#162869=CARTESIAN_POINT('Ctrl Pts',(3.53149542509341,-7.31766545970364,
10.2262416427217));
#162870=CARTESIAN_POINT('Ctrl Pts',(3.56685255137686,-7.30060004562135,
10.2277791691853));
#162871=CARTESIAN_POINT('Ctrl Pts',(3.60173325761103,-7.28345492721995,
10.2293034803997));
#162872=CARTESIAN_POINT('Ctrl Pts',(3.71118441605843,-7.22867723777756,
10.2341107426513));
#162873=CARTESIAN_POINT('Ctrl Pts',(3.78529804408404,-7.19014485005422,
10.2374015663014));
#162874=CARTESIAN_POINT('Ctrl Pts',(3.95757713078065,-7.09717325481907,
10.2451371065078));
#162875=CARTESIAN_POINT('Ctrl Pts',(4.05523457613207,-7.04182911029313,
10.2495889123754));
#162876=CARTESIAN_POINT('Ctrl Pts',(4.30830254769003,-6.89140048273695,
10.2613001709367));
#162877=CARTESIAN_POINT('Ctrl Pts',(4.46171639275852,-6.79308161000347,
10.2685786282759));
#162878=CARTESIAN_POINT('Ctrl Pts',(4.63177606156879,-6.67584698457957,
10.2768294992151));
#162879=CARTESIAN_POINT('Ctrl Pts',(4.65179462951999,-6.66191332662261,
10.2778036733782));
#162880=CARTESIAN_POINT('Ctrl Pts',(4.82552668531783,-6.53982454489698,
10.2862829172916));
#162881=CARTESIAN_POINT('Ctrl Pts',(4.97550869415378,-6.42645526630782,
10.293774749702));
#162882=CARTESIAN_POINT('Ctrl Pts',(5.14773201326787,-6.28662794470906,
10.3025267626075));
#162883=CARTESIAN_POINT('Ctrl Pts',(5.17390509734162,-6.26510509525038,
10.3038609860312));
#162884=CARTESIAN_POINT('Ctrl Pts',(5.21405163519809,-6.23166833564856,
10.3059134209709));
#162885=CARTESIAN_POINT('Ctrl Pts',(5.22812050297963,-6.21986983043301,
10.3066337790557));
#162886=CARTESIAN_POINT('Ctrl Pts',(5.2563838979688,-6.19600379122663,10.3080832652032));
#162887=CARTESIAN_POINT('Ctrl Pts',(5.27057712280001,-6.18393494944108,
10.3088123683506));
#162888=CARTESIAN_POINT('Ctrl Pts',(5.30429008782234,-6.15506762167589,
10.3105472561971));
#162889=CARTESIAN_POINT('Ctrl Pts',(5.3237717419084,-6.13822492333912,10.3115522541191));
#162890=CARTESIAN_POINT('Ctrl Pts',(5.38847419393348,-6.0817472192066,10.3148989536424));
#162891=CARTESIAN_POINT('Ctrl Pts',(5.43333521065963,-6.04170273454323,
10.3172339862031));
#162892=CARTESIAN_POINT('Ctrl Pts',(5.54351828268168,-5.94112972933677,
10.3230117213443));
#162893=CARTESIAN_POINT('Ctrl Pts',(5.60829774390473,-5.88001819535284,
10.3264467278162));
#162894=CARTESIAN_POINT('Ctrl Pts',(5.91129756648928,-5.58461147961954,
10.3427326787712));
#162895=CARTESIAN_POINT('Ctrl Pts',(6.13592099468687,-5.33683417118405,
10.3554772539437));
#162896=CARTESIAN_POINT('Ctrl Pts',(6.48224024490431,-4.90395316903533,
10.3768056122942));
#162897=CARTESIAN_POINT('Ctrl Pts',(6.61277875294917,-4.72645224784754,
10.3853151448662));
#162898=CARTESIAN_POINT('Ctrl Pts',(6.77395761074221,-4.48751674341049,
10.3965297098054));
#162899=CARTESIAN_POINT('Ctrl Pts',(6.81126266711804,-4.43068945654746,
10.3991796890481));
#162900=CARTESIAN_POINT('Ctrl Pts',(6.87497336751892,-4.33093154833192,
10.403803019197));
#162901=CARTESIAN_POINT('Ctrl Pts',(6.90170085040494,-4.28821084265929,
10.4057739727337));
#162902=CARTESIAN_POINT('Ctrl Pts',(6.95545264356238,-4.20049057090326,
10.4098031666068));
#162903=CARTESIAN_POINT('Ctrl Pts',(6.98244179159792,-4.15547218959073,
10.4118615336058));
#162904=CARTESIAN_POINT('Ctrl Pts',(7.03894928240731,-4.05911166605496,
10.4162476134647));
#162905=CARTESIAN_POINT('Ctrl Pts',(7.06834634013845,-4.00770189850069,
10.4185758832597));
#162906=CARTESIAN_POINT('Ctrl Pts',(7.1107659305653,-3.93159945137952,10.42200514909));
#162907=CARTESIAN_POINT('Ctrl Pts',(7.12422746798997,-3.90715361195838,
10.4231041098016));
#162908=CARTESIAN_POINT('Ctrl Pts',(7.17337663564569,-3.81680133433638,
10.4271562674272));
#162909=CARTESIAN_POINT('Ctrl Pts',(7.20827778092115,-3.7504714616891,10.4301123142812));
#162910=CARTESIAN_POINT('Ctrl Pts',(7.33593554461111,-3.49949060674241,
10.4412249285254));
#162911=CARTESIAN_POINT('Ctrl Pts',(7.42255521428859,-3.3118060388286,10.4493910383001));
#162912=CARTESIAN_POINT('Ctrl Pts',(7.5148724022378,-3.08990554796304,10.4588440320815));
#162913=CARTESIAN_POINT('Ctrl Pts',(7.52762483364334,-3.05870689803732,
10.4601685037238));
#162914=CARTESIAN_POINT('Ctrl Pts',(7.55371688170796,-2.99372147230505,
10.4629173778105));
#162915=CARTESIAN_POINT('Ctrl Pts',(7.56702476633594,-2.95992283287973,
10.464341400777));
#162916=CARTESIAN_POINT('Ctrl Pts',(7.59471510713539,-2.88818902293506,
10.4673522393804));
#162917=CARTESIAN_POINT('Ctrl Pts',(7.60904097186529,-2.85023312918963,
10.4689386855553));
#162918=CARTESIAN_POINT('Ctrl Pts',(7.64556271482043,-2.75123196816582,
10.4730611587756));
#162919=CARTESIAN_POINT('Ctrl Pts',(7.66731193345125,-2.69002496553027,
10.4755946481013));
#162920=CARTESIAN_POINT('Ctrl Pts',(7.74695149019609,-2.4570860423642,10.4851890236454));
#162921=CARTESIAN_POINT('Ctrl Pts',(7.79982475366788,-2.28369504403652,
10.4922346519436));
#162922=CARTESIAN_POINT('Ctrl Pts',(7.87331385630181,-2.01022633545768,
10.503272909895));
#162923=CARTESIAN_POINT('Ctrl Pts',(7.89791625943527,-1.91128220100265,
10.5072515897117));
#162924=CARTESIAN_POINT('Ctrl Pts',(7.93237398500466,-1.76065173256889,
10.5132956950265));
#162925=CARTESIAN_POINT('Ctrl Pts',(7.9436000317772,-1.70928934836631,10.5153543432748));
#162926=CARTESIAN_POINT('Ctrl Pts',(7.96475263439291,-1.60779790912964,
10.5194191440834));
#162927=CARTESIAN_POINT('Ctrl Pts',(7.97470633569509,-1.55767695060615,
10.5214250577235));
#162928=CARTESIAN_POINT('Ctrl Pts',(7.99408052241681,-1.45506291582417,
10.525529997864));
#162929=CARTESIAN_POINT('Ctrl Pts',(8.00345830989705,-1.40256427466893,
10.5276291684506));
#162930=CARTESIAN_POINT('Ctrl Pts',(8.02429097204558,-1.27891928218496,
10.5325721218566));
#162931=CARTESIAN_POINT('Ctrl Pts',(8.03531752175575,-1.20770542584511,
10.5354182603425));
#162932=CARTESIAN_POINT('Ctrl Pts',(8.09849714336799,-0.760393423566754,
10.5532968006508));
#162933=CARTESIAN_POINT('Ctrl Pts',(8.12517915088166,-0.381183041305498,
10.5684829774549));
#162934=CARTESIAN_POINT('Ctrl Pts',(8.12524985909245,-0.00151321448057171,
10.5836791336291));
#162935=CARTESIAN_POINT('',(8.12631724021387,-0.0026888491199863,14.5832974432124));
#162936=CARTESIAN_POINT('Ctrl Pts',(8.12524985911998,-0.00151306667137495,
10.5836791395451));
#162937=CARTESIAN_POINT('Ctrl Pts',(8.12529265115791,0.228282491430003,
10.5928766288908));
#162938=CARTESIAN_POINT('Ctrl Pts',(8.11558692129937,0.457979970419391,
10.6020610450867));
#162939=CARTESIAN_POINT('Ctrl Pts',(8.09315866316021,0.722308052229391,
10.6125517107936));
#162940=CARTESIAN_POINT('Ctrl Pts',(8.0899278691087,0.757636559940404,10.6139521386737));
#162941=CARTESIAN_POINT('Ctrl Pts',(8.08419352636532,0.816115635688944,
10.6162669789118));
#162942=CARTESIAN_POINT('Ctrl Pts',(8.08182165012504,0.839278572863596,
10.6171830084473));
#162943=CARTESIAN_POINT('Ctrl Pts',(8.07734109287788,0.881252933032226,
10.6188412735829));
#162944=CARTESIAN_POINT('Ctrl Pts',(8.07526617865032,0.900067780436113,
10.6195839632212));
#162945=CARTESIAN_POINT('Ctrl Pts',(8.07108472871043,0.93680548842099,10.6210328256588));
#162946=CARTESIAN_POINT('Ctrl Pts',(8.06898419304009,0.954728922878413,
10.6217390820601));
#162947=CARTESIAN_POINT('Ctrl Pts',(8.06393028238987,0.996644521322071,
10.623389204976));
#162948=CARTESIAN_POINT('Ctrl Pts',(8.06092952216192,1.02063075704632,10.6243322776981));
#162949=CARTESIAN_POINT('Ctrl Pts',(8.05228363369517,1.08732308727048,10.6269515234829));
#162950=CARTESIAN_POINT('Ctrl Pts',(8.04640584367617,1.12999833755841,10.6286242518605));
#162951=CARTESIAN_POINT('Ctrl Pts',(8.02962009212361,1.2450910696279,10.6331297389549));
#162952=CARTESIAN_POINT('Ctrl Pts',(8.01807196723447,1.31741133804886,10.6359546758437));
#162953=CARTESIAN_POINT('Ctrl Pts',(7.96625029425089,1.61596563119189,10.6476130340297));
#162954=CARTESIAN_POINT('Ctrl Pts',(7.91736642247098,1.84059735638636,10.6563797654729));
#162955=CARTESIAN_POINT('Ctrl Pts',(7.80968269373701,2.25084876072845,10.6726264459083));
#162956=CARTESIAN_POINT('Ctrl Pts',(7.75360875783441,2.43700925418768,10.6800904127697));
#162957=CARTESIAN_POINT('Ctrl Pts',(7.66672913416935,2.69194599507781,10.6905122411309));
#162958=CARTESIAN_POINT('Ctrl Pts',(7.64156319577322,2.76257501026842,10.6934210417988));
#162959=CARTESIAN_POINT('Ctrl Pts',(7.61403276671079,2.83658394930537,10.6964937659909));
#162960=CARTESIAN_POINT('Ctrl Pts',(7.61263928763962,2.84032155754824,10.6966490117158));
#162961=CARTESIAN_POINT('Ctrl Pts',(7.60992488073863,2.84758582912157,10.696950871385));
#162962=CARTESIAN_POINT('Ctrl Pts',(7.60860425227359,2.85111260334811,10.6970974826651));
#162963=CARTESIAN_POINT('Ctrl Pts',(7.60601412460523,2.85801499387517,10.6973845386176));
#162964=CARTESIAN_POINT('Ctrl Pts',(7.60474482890162,2.86139068569684,10.6975249814674));
#162965=CARTESIAN_POINT('Ctrl Pts',(7.60223710546207,2.86804652121934,10.6978020006031));
#162966=CARTESIAN_POINT('Ctrl Pts',(7.60099880122183,2.87132671066121,10.6979385757707));
#162967=CARTESIAN_POINT('Ctrl Pts',(7.58815796127725,2.90527476393036,10.6993525901106));
#162968=CARTESIAN_POINT('Ctrl Pts',(7.57637203371379,2.93587286808058,10.7006316431492));
#162969=CARTESIAN_POINT('Ctrl Pts',(7.55209785131115,2.9977727244565,10.7032286783329));
#162970=CARTESIAN_POINT('Ctrl Pts',(7.53959941775076,3.02906980340426,10.7045467295308));
#162971=CARTESIAN_POINT('Ctrl Pts',(7.50984075115534,3.1022624880415,10.7076410795414));
#162972=CARTESIAN_POINT('Ctrl Pts',(7.49242407357638,3.1440932129875,10.709418748656));
#162973=CARTESIAN_POINT('Ctrl Pts',(7.43526071153168,3.27821331877689,10.715148624682));
#162974=CARTESIAN_POINT('Ctrl Pts',(7.39415185960124,3.36991134389192,10.7191126189783));
#162975=CARTESIAN_POINT('Ctrl Pts',(7.2178994729735,3.74430021180341,10.735490817272));
#162976=CARTESIAN_POINT('Ctrl Pts',(7.06816124149337,4.01981968477365,10.7480196970835));
#162977=CARTESIAN_POINT('Ctrl Pts',(6.862123225813,4.35165777445126,10.7635699358125));
#162978=CARTESIAN_POINT('Ctrl Pts',(6.8204211224188,4.41673141052762,10.766641694564));
#162979=CARTESIAN_POINT('Ctrl Pts',(6.75719266075966,4.51236419446143,10.7711841388713));
#162980=CARTESIAN_POINT('Ctrl Pts',(6.73637369886617,4.54338559694112,10.7726620863151));
#162981=CARTESIAN_POINT('Ctrl Pts',(6.69836453311552,4.5991857468792,10.7753278451495));
#162982=CARTESIAN_POINT('Ctrl Pts',(6.68124892407901,4.62401446548007,10.7765166325493));
#162983=CARTESIAN_POINT('Ctrl Pts',(6.65288023759654,4.66468107558776,10.7784676584035));
#162984=CARTESIAN_POINT('Ctrl Pts',(6.64170789764263,4.68057487901611,10.7792311762396));
#162985=CARTESIAN_POINT('Ctrl Pts',(6.61971775452888,4.71162084821153,10.7807243962234));
#162986=CARTESIAN_POINT('Ctrl Pts',(6.60890466668478,4.7267762034841,10.7814541679662));
#162987=CARTESIAN_POINT('Ctrl Pts',(6.58440445999246,4.76086665791639,10.7830975369568));
#162988=CARTESIAN_POINT('Ctrl Pts',(6.57068757961514,4.77978013759346,10.7840105872908));
#162989=CARTESIAN_POINT('Ctrl Pts',(6.51864108322602,4.85089685484496,10.7874491675334));
#162990=CARTESIAN_POINT('Ctrl Pts',(6.47976917033216,4.90270063014863,10.7899650087921));
#162991=CARTESIAN_POINT('Ctrl Pts',(6.17837103672735,5.29452046066359,10.8090991282585));
#162992=CARTESIAN_POINT('Ctrl Pts',(5.88986677228204,5.61370616202336,10.8253168143115));
#162993=CARTESIAN_POINT('Ctrl Pts',(5.30859019482285,6.16240905196027,10.8556902447381));
#162994=CARTESIAN_POINT('Ctrl Pts',(5.02269081090321,6.39757655641904,10.8697827030386));
#162995=CARTESIAN_POINT('Ctrl Pts',(4.63055603046021,6.67758956403809,10.8884167132347));
#162996=CARTESIAN_POINT('Ctrl Pts',(4.53799862327918,6.74083227399317,10.8927672121003));
#162997=CARTESIAN_POINT('Ctrl Pts',(4.41062536777149,6.8240513137138,10.8986958469211));
#162998=CARTESIAN_POINT('Ctrl Pts',(4.37692613319178,6.84571472371547,10.900258962277));
#162999=CARTESIAN_POINT('Ctrl Pts',(4.31356226024147,6.88578877191805,10.9031882058082));
#163000=CARTESIAN_POINT('Ctrl Pts',(4.28393647181853,6.90425916962392,10.90455379719));
#163001=CARTESIAN_POINT('Ctrl Pts',(4.22187352931657,6.94239947464928,10.9074064677361));
#163002=CARTESIAN_POINT('Ctrl Pts',(4.18941580722701,6.96203431093546,10.9088937939024));
#163003=CARTESIAN_POINT('Ctrl Pts',(4.11424812518309,7.00678992200614,10.9123279440105));
#163004=CARTESIAN_POINT('Ctrl Pts',(4.07144353127451,7.03174872955914,10.914275954168));
#163005=CARTESIAN_POINT('Ctrl Pts',(3.93338203666808,7.11056732350726,10.9205352733369));
#163006=CARTESIAN_POINT('Ctrl Pts',(3.83726479815657,7.16289470562214,10.9248570928374));
#163007=CARTESIAN_POINT('Ctrl Pts',(3.36121053052287,7.40973167124872,10.9460910605371));
#163008=CARTESIAN_POINT('Ctrl Pts',(2.96742000936151,7.57603226117489,10.9630780234009));
#163009=CARTESIAN_POINT('Ctrl Pts',(2.00833633791254,7.89475521907546,11.0044517423284));
#163010=CARTESIAN_POINT('Ctrl Pts',(1.43605565189704,8.01861883388864,11.0292861957511));
#163011=CARTESIAN_POINT('Ctrl Pts',(0.635130703420006,8.10341941460139,
11.0632324896176));
#163012=CARTESIAN_POINT('Ctrl Pts',(0.413886850961786,8.11772751179484,
11.0724984861625));
#163013=CARTESIAN_POINT('Ctrl Pts',(0.129590859632434,8.12445888940698,
11.0840878714626));
#163014=CARTESIAN_POINT('Ctrl Pts',(0.0668351667036395,8.12521749339648,
11.0866260193365));
#163015=CARTESIAN_POINT('Ctrl Pts',(-0.0220465098795425,8.12526208246541,
11.0901870086564));
#163016=CARTESIAN_POINT('Ctrl Pts',(-0.0481692811329664,8.12514921066762,
11.0912294606377));
#163017=CARTESIAN_POINT('Ctrl Pts',(-0.0935171110648323,8.12473456663143,
11.0930314186847));
#163018=CARTESIAN_POINT('Ctrl Pts',(-0.112742417193487,8.1244905306867,
11.093792963717));
#163019=CARTESIAN_POINT('Ctrl Pts',(-0.141589131703196,8.12402195310369,
11.0949318525471));
#163020=CARTESIAN_POINT('Ctrl Pts',(-0.151211231384496,8.12384855479316,
11.0953111094605));
#163021=CARTESIAN_POINT('Ctrl Pts',(-0.168091093588086,8.12351436552898,
11.0959753002843));
#163022=CARTESIAN_POINT('Ctrl Pts',(-0.175348981507235,8.12336094223565,
11.0962605172744));
#163023=CARTESIAN_POINT('Ctrl Pts',(-0.189434441725192,8.12304430597555,
11.0968133156299));
#163024=CARTESIAN_POINT('Ctrl Pts',(-0.196262030954958,8.12288221138896,
11.0970809406237));
#163025=CARTESIAN_POINT('Ctrl Pts',(-0.212551508866258,8.12247493105734,
11.0977186466833));
#163026=CARTESIAN_POINT('Ctrl Pts',(-0.222013202487022,8.12222181970473,
11.0980884105787));
#163027=CARTESIAN_POINT('Ctrl Pts',(-0.255822710572896,8.12125825363165,
11.09940732992));
#163028=CARTESIAN_POINT('Ctrl Pts',(-0.280167902308072,8.12045484227611,
11.1003526707005));
#163029=CARTESIAN_POINT('Ctrl Pts',(-0.719717783733941,8.10397028905207,
11.1173371884553));
#163030=CARTESIAN_POINT('Ctrl Pts',(-1.13312688033432,8.05657256933183,
11.131825676582));
#163031=CARTESIAN_POINT('Ctrl Pts',(-1.89297623454167,7.90978937642664,
11.1580067482654));
#163032=CARTESIAN_POINT('Ctrl Pts',(-2.23997418020351,7.81860901940375,
11.1697960761293));
#163033=CARTESIAN_POINT('Ctrl Pts',(-3.12792621930284,7.52129418690696,
11.2013369051586));
#163034=CARTESIAN_POINT('Ctrl Pts',(-3.6548209486279,7.2798338754045,11.2215530013828));
#163035=CARTESIAN_POINT('Ctrl Pts',(-4.17601726727558,6.97003392361174,
11.2449069805585));
#163036=CARTESIAN_POINT('Ctrl Pts',(-4.20033856836218,6.95540430202424,
11.2460045988469));
#163037=CARTESIAN_POINT('Ctrl Pts',(-4.23563207237819,6.93392211046934,
11.2476089261183));
#163038=CARTESIAN_POINT('Ctrl Pts',(-4.24666546278597,6.92717022541985,
11.2481121188675));
#163039=CARTESIAN_POINT('Ctrl Pts',(-4.26596529626576,6.91529624982362,
11.2489952220247));
#163040=CARTESIAN_POINT('Ctrl Pts',(-4.27423876756105,6.91018560451417,
11.2493747311537));
#163041=CARTESIAN_POINT('Ctrl Pts',(-4.29025952257052,6.90024956767657,
11.2501114415699));
#163042=CARTESIAN_POINT('Ctrl Pts',(-4.29800789232975,6.8954259494295,11.250468580315));
#163043=CARTESIAN_POINT('Ctrl Pts',(-4.31644599173505,6.88390446583105,
11.251320420033));
#163044=CARTESIAN_POINT('Ctrl Pts',(-4.3271282683962,6.87719475086799,11.2518155374269));
#163045=CARTESIAN_POINT('Ctrl Pts',(-4.36507270314597,6.85323781514009,
11.253579945961));
#163046=CARTESIAN_POINT('Ctrl Pts',(-4.39224755367537,6.83585324979259,
11.2548540774218));
#163047=CARTESIAN_POINT('Ctrl Pts',(-4.84284466526236,6.54379661686656,
11.2761577162981));
#163048=CARTESIAN_POINT('Ctrl Pts',(-5.23982019050381,6.2304570818495,11.297628900543));
#163049=CARTESIAN_POINT('Ctrl Pts',(-5.79100952472595,5.70524468651953,
11.3313031969452));
#163050=CARTESIAN_POINT('Ctrl Pts',(-5.96838379670385,5.51942010774735,
11.3428413712309));
#163051=CARTESIAN_POINT('Ctrl Pts',(-6.49110043748582,4.91708699120388,
11.3786662859981));
#163052=CARTESIAN_POINT('Ctrl Pts',(-6.80394575591562,4.47422117943838,
11.4028777576027));
#163053=CARTESIAN_POINT('Ctrl Pts',(-7.08429012982834,3.97910859437228,
11.4256860842845));
#163054=CARTESIAN_POINT('Ctrl Pts',(-7.09796286858158,3.95466749460866,
11.4268024466376));
#163055=CARTESIAN_POINT('Ctrl Pts',(-7.11694028075076,3.92032838958783,
11.4283581489933));
#163056=CARTESIAN_POINT('Ctrl Pts',(-7.12235111468058,3.91048951447941,
11.4288024306939));
#163057=CARTESIAN_POINT('Ctrl Pts',(-7.13151191494472,3.89374974193561,
11.4295558964342));
#163058=CARTESIAN_POINT('Ctrl Pts',(-7.13527229326003,3.88685458274594,
11.4298655520171));
#163059=CARTESIAN_POINT('Ctrl Pts',(-7.14268325889419,3.87321858289333,
11.4304765711139));
#163060=CARTESIAN_POINT('Ctrl Pts',(-7.14633431529943,3.86647800746843,
11.4307779553236));
#163061=CARTESIAN_POINT('Ctrl Pts',(-7.15435109770708,3.85162728813988,
11.4314405358723));
#163062=CARTESIAN_POINT('Ctrl Pts',(-7.15871258727613,3.84351486137858,
11.4318015473707));
#163063=CARTESIAN_POINT('Ctrl Pts',(-7.17384226158204,3.8152583796623,11.4330557989328));
#163064=CARTESIAN_POINT('Ctrl Pts',(-7.1845393447092,3.79507624620174,11.4339460105105));
#163065=CARTESIAN_POINT('Ctrl Pts',(-7.30939040062601,3.55710058317286,
11.4443793829554));
#163066=CARTESIAN_POINT('Ctrl Pts',(-7.4136915840685,3.33426762328105,11.4535284661577));
#163067=CARTESIAN_POINT('Ctrl Pts',(-7.82054910795897,2.35115279212803,
11.4924060625655));
#163068=CARTESIAN_POINT('Ctrl Pts',(-8.01742843781844,1.55236406007379,
11.5208665305891));
#163069=CARTESIAN_POINT('Ctrl Pts',(-8.09801399738059,0.668353344859133,
11.5546854401877));
#163070=CARTESIAN_POINT('Ctrl Pts',(-8.10343931057638,0.598997574237792,
11.557349112804));
#163071=CARTESIAN_POINT('Ctrl Pts',(-8.11154474092193,0.47490213009185,
11.5621344235867));
#163072=CARTESIAN_POINT('Ctrl Pts',(-8.11456292977148,0.420188659166743,
11.5642509465442));
#163073=CARTESIAN_POINT('Ctrl Pts',(-8.11825794597017,0.338118285954926,
11.5674357836876));
#163074=CARTESIAN_POINT('Ctrl Pts',(-8.11935040071199,0.310781458755766,
11.5684982883157));
#163075=CARTESIAN_POINT('Ctrl Pts',(-8.1210710357293,0.261486739850709,
11.5704172138061));
#163076=CARTESIAN_POINT('Ctrl Pts',(-8.12174827740896,0.239530782974643,
11.5712729687722));
#163077=CARTESIAN_POINT('Ctrl Pts',(-8.12288624877459,0.197048441890887,
11.572930810875));
#163078=CARTESIAN_POINT('Ctrl Pts',(-8.12335822854482,0.176522481287602,
11.573732757641));
#163079=CARTESIAN_POINT('Ctrl Pts',(-8.12438472758666,0.12306548295282,
11.5758239082714));
#163080=CARTESIAN_POINT('Ctrl Pts',(-8.12481682408881,0.0901325447555323,
11.5771147536032));
#163081=CARTESIAN_POINT('Ctrl Pts',(-8.12561658356266,-0.0234743099147386,
11.5815773309753));
#163082=CARTESIAN_POINT('Ctrl Pts',(-8.12498298390104,-0.104149851407131,
11.5847631281905));
#163083=CARTESIAN_POINT('Ctrl Pts',(-8.10433610808371,-1.01170351500131,
11.6208219477433));
#163084=CARTESIAN_POINT('Ctrl Pts',(-7.95936508962477,-1.83085476222711,
11.6561536426617));
#163085=CARTESIAN_POINT('Ctrl Pts',(-7.61448465331733,-2.84594486187559,
11.7012645010144));
#163086=CARTESIAN_POINT('Ctrl Pts',(-7.52515977387297,-3.07437113449255,
11.7114510975381));
#163087=CARTESIAN_POINT('Ctrl Pts',(-7.4096944074711,-3.3343154378054,11.7228700119843));
#163088=CARTESIAN_POINT('Ctrl Pts',(-7.39348766625363,-3.37009952968905,
11.7244379287296));
#163089=CARTESIAN_POINT('Ctrl Pts',(-7.37170466490312,-3.41728237323068,
11.7264987936629));
#163090=CARTESIAN_POINT('Ctrl Pts',(-7.36636044210507,-3.42878729642047,
11.7270007944998));
#163091=CARTESIAN_POINT('Ctrl Pts',(-7.35755157994219,-3.44763516511162,
11.7278223000871));
#163092=CARTESIAN_POINT('Ctrl Pts',(-7.35410284912168,-3.4549854946647,
11.7281424488936));
#163093=CARTESIAN_POINT('Ctrl Pts',(-7.34740518124786,-3.46920486623594,
11.7287613350122));
#163094=CARTESIAN_POINT('Ctrl Pts',(-7.34415761505196,-3.47607454279973,
11.7290601287303));
#163095=CARTESIAN_POINT('Ctrl Pts',(-7.33664634520981,-3.49190584885813,
11.7297482207586));
#163096=CARTESIAN_POINT('Ctrl Pts',(-7.33237584494681,-3.50086425351041,
11.7301372306741));
#163097=CARTESIAN_POINT('Ctrl Pts',(-7.32091098261479,-3.52480156492575,
11.7311756862282));
#163098=CARTESIAN_POINT('Ctrl Pts',(-7.31368704248173,-3.53976631112827,
11.7318238435214));
#163099=CARTESIAN_POINT('Ctrl Pts',(-7.25729415643373,-3.65567733766896,
11.7368355291189));
#163100=CARTESIAN_POINT('Ctrl Pts',(-7.20608706340845,-3.75560987903254,
11.7410983140621));
#163101=CARTESIAN_POINT('Ctrl Pts',(-6.82713873912917,-4.45883393915177,
11.7707338083873));
#163102=CARTESIAN_POINT('Ctrl Pts',(-6.42614615297047,-5.01954530813275,
11.7927778355634));
#163103=CARTESIAN_POINT('Ctrl Pts',(-5.61179172038431,-5.89821701954696,
11.8336009652055));
#163104=CARTESIAN_POINT('Ctrl Pts',(-5.22960669425561,-6.2395766536831,
11.8516698324195));
#163105=CARTESIAN_POINT('Ctrl Pts',(-4.78720361993821,-6.56535011823596,
11.8727520685766));
#163106=CARTESIAN_POINT('Ctrl Pts',(-4.7563498213442,-6.58773686514507,
11.8742226524467));
#163107=CARTESIAN_POINT('Ctrl Pts',(-4.71347846809473,-6.61838506657224,
11.8762667188977));
#163108=CARTESIAN_POINT('Ctrl Pts',(-4.70159429560587,-6.62683266994992,
11.8768334175325));
#163109=CARTESIAN_POINT('Ctrl Pts',(-4.6814943471707,-6.64103899254882,
11.8777920269946));
#163110=CARTESIAN_POINT('Ctrl Pts',(-4.67329050777977,-6.64681457934395,
11.8781833248629));
#163111=CARTESIAN_POINT('Ctrl Pts',(-4.65703564395792,-6.658213199561,11.8789587159831));
#163112=CARTESIAN_POINT('Ctrl Pts',(-4.64898508032753,-6.66383686189753,
11.879342785471));
#163113=CARTESIAN_POINT('Ctrl Pts',(-4.63121871570784,-6.6761995612146,
11.8801904643422));
#163114=CARTESIAN_POINT('Ctrl Pts',(-4.62149836737635,-6.68293200719578,
11.8806543102977));
#163115=CARTESIAN_POINT('Ctrl Pts',(-4.58749229554157,-6.70637540354939,
11.8822772857245));
#163116=CARTESIAN_POINT('Ctrl Pts',(-4.56313048606076,-6.72297529074886,
11.883440401352));
#163117=CARTESIAN_POINT('Ctrl Pts',(-4.30886999711988,-6.89420708232514,
11.8955847305446));
#163118=CARTESIAN_POINT('Ctrl Pts',(-4.07131186355975,-7.03710546185362,
11.9069827030973));
#163119=CARTESIAN_POINT('Ctrl Pts',(-3.70578840531833,-7.23226655614917,
11.924591624839));
#163120=CARTESIAN_POINT('Ctrl Pts',(-3.58302699048722,-7.2938647448299,
11.9305153698488));
#163121=CARTESIAN_POINT('Ctrl Pts',(-2.9154949321715,-7.60789314700132,
11.9627271364486));
#163122=CARTESIAN_POINT('Ctrl Pts',(-2.34561218264704,-7.80244741272736,
11.9903756857371));
#163123=CARTESIAN_POINT('Ctrl Pts',(-1.4305579981823,-8.0054192632853,12.0318452353692));
#163124=CARTESIAN_POINT('Ctrl Pts',(-1.09731261015582,-8.0578666042927,
12.0463258643458));
#163125=CARTESIAN_POINT('Ctrl Pts',(-0.738091934923298,-8.09169148247531,
12.0607265603345));
#163126=CARTESIAN_POINT('Ctrl Pts',(-0.714455018619491,-8.09381274774334,
12.061669047209));
#163127=CARTESIAN_POINT('Ctrl Pts',(-0.680727215952277,-8.09669070681349,
12.0630070578546));
#163128=CARTESIAN_POINT('Ctrl Pts',(-0.670643831490075,-8.09753214238101,
12.0634062034579));
#163129=CARTESIAN_POINT('Ctrl Pts',(-0.653239222353201,-8.09895178492797,
12.0640936920894));
#163130=CARTESIAN_POINT('Ctrl Pts',(-0.645918751949548,-8.09953890431957,
12.0643824066605));
#163131=CARTESIAN_POINT('Ctrl Pts',(-0.631905802522059,-8.10064365813612,
12.0649342295564));
#163132=CARTESIAN_POINT('Ctrl Pts',(-0.625213461827286,-8.10116292558314,
12.065197404548));
#163133=CARTESIAN_POINT('Ctrl Pts',(-0.609541213024148,-8.1023594198958,
12.0658128709066));
#163134=CARTESIAN_POINT('Ctrl Pts',(-0.600560796162926,-8.10303001293335,
12.0661648947441));
#163135=CARTESIAN_POINT('Ctrl Pts',(-0.569493237913271,-8.10529798381146,
12.0673805300424));
#163136=CARTESIAN_POINT('Ctrl Pts',(-0.547400581031609,-8.10682000356397,
12.068241172011));
#163137=CARTESIAN_POINT('Ctrl Pts',(-0.210674478157437,-8.12863516795831,
12.0813040481688));
#163138=CARTESIAN_POINT('Ctrl Pts',(0.104892474832877,-8.13068960530555,
12.0928329131821));
#163139=CARTESIAN_POINT('Ctrl Pts',(0.825502891211111,-8.09340922295008,
12.1188609473769));
#163140=CARTESIAN_POINT('Ctrl Pts',(1.22906490512882,-8.04202287321422,
12.1332444810864));
#163141=CARTESIAN_POINT('Ctrl Pts',(2.20786328258949,-7.84196480575918,
12.1695562714419));
#163142=CARTESIAN_POINT('Ctrl Pts',(2.77386969966544,-7.66006811214229,
12.1919170142696));
#163143=CARTESIAN_POINT('Ctrl Pts',(3.41806590246757,-7.37219469490929,
12.2191842372807));
#163144=CARTESIAN_POINT('Ctrl Pts',(3.52015105456113,-7.32399927498181,
12.2235620969215));
#163145=CARTESIAN_POINT('Ctrl Pts',(3.66587450289509,-7.25145105203742,
12.229903523818));
#163146=CARTESIAN_POINT('Ctrl Pts',(3.7103446981521,-7.22879799293918,12.231851331262));
#163147=CARTESIAN_POINT('Ctrl Pts',(3.78818133192683,-7.18824063046671,
12.2352837101963));
#163148=CARTESIAN_POINT('Ctrl Pts',(3.8216366418659,-7.17051006061672,12.2367665956087));
#163149=CARTESIAN_POINT('Ctrl Pts',(3.89127750408656,-7.13297612606508,
12.2398697126844));
#163150=CARTESIAN_POINT('Ctrl Pts',(3.92743864147188,-7.11312974216804,
12.2414903227027));
#163151=CARTESIAN_POINT('Ctrl Pts',(4.02219228751627,-7.0601830931749,12.2457620127695));
#163152=CARTESIAN_POINT('Ctrl Pts',(4.0805272593001,-7.02662887284802,12.2484174582775));
#163153=CARTESIAN_POINT('Ctrl Pts',(4.34092770662842,-6.87251035812182,
12.2603904851186));
#163154=CARTESIAN_POINT('Ctrl Pts',(4.5381126687349,-6.74392929621897,12.2697862865433));
#163155=CARTESIAN_POINT('Ctrl Pts',(5.090629043771,-6.34842435634939,12.2971340719851));
#163156=CARTESIAN_POINT('Ctrl Pts',(5.43000998420353,-6.0606914236517,12.315251763597));
#163157=CARTESIAN_POINT('Ctrl Pts',(5.85951213597909,-5.63137666391457,
12.3398516028791));
#163158=CARTESIAN_POINT('Ctrl Pts',(5.97136237091782,-5.51263258995273,
12.3464323664701));
#163159=CARTESIAN_POINT('Ctrl Pts',(6.12108115104263,-5.34377855151213,
12.3554625739321));
#163160=CARTESIAN_POINT('Ctrl Pts',(6.16205623417064,-5.29647682188468,
12.357958266947));
#163161=CARTESIAN_POINT('Ctrl Pts',(6.23241039838118,-5.21333816802961,
12.3622839555946));
#163162=CARTESIAN_POINT('Ctrl Pts',(6.2620368721053,-5.17771460055728,12.3641184790684));
#163163=CARTESIAN_POINT('Ctrl Pts',(6.30533136637005,-5.1247411204932,12.3668178522994));
#163164=CARTESIAN_POINT('Ctrl Pts',(6.31923584674851,-5.1075858791526,12.3676876564034));
#163165=CARTESIAN_POINT('Ctrl Pts',(6.34468522661543,-5.07592362634966,
12.3692848753012));
#163166=CARTESIAN_POINT('Ctrl Pts',(6.35625070560465,-5.06143341909078,
12.3700127568318));
#163167=CARTESIAN_POINT('Ctrl Pts',(6.382341256541,-5.02851451560522,12.3716596122835));
#163168=CARTESIAN_POINT('Ctrl Pts',(6.39683631066451,-5.01006221206307,
12.3725779796894));
#163169=CARTESIAN_POINT('Ctrl Pts',(6.43448041616303,-4.96171130944181,
12.374972516524));
#163170=CARTESIAN_POINT('Ctrl Pts',(6.45750109633736,-4.93171338940285,
12.3764463681937));
#163171=CARTESIAN_POINT('Ctrl Pts',(6.63112928979315,-4.70216080404274,
12.3876415538274));
#163172=CARTESIAN_POINT('Ctrl Pts',(6.77266538859039,-4.49590905071219,
12.3972309915625));
#163173=CARTESIAN_POINT('Ctrl Pts',(6.96773722830066,-4.18147452923651,
12.4114560571119));
#163174=CARTESIAN_POINT('Ctrl Pts',(7.02873944284768,-4.07810164525169,
12.4160720620689));
#163175=CARTESIAN_POINT('Ctrl Pts',(7.15011457969925,-3.86160336246185,
12.4256466546382));
#163176=CARTESIAN_POINT('Ctrl Pts',(7.21014471885082,-3.74832386558068,
12.4306058753737));
#163177=CARTESIAN_POINT('Ctrl Pts',(7.28947857508346,-3.5896534274096,12.4375012634681));
#163178=CARTESIAN_POINT('Ctrl Pts',(7.31108720016794,-3.54543559400808,
12.4394174298225));
#163179=CARTESIAN_POINT('Ctrl Pts',(7.34769540319897,-3.46876601457286,
12.4427314809984));
#163180=CARTESIAN_POINT('Ctrl Pts',(7.36288501303784,-3.43640650629159,
12.4441276655105));
#163181=CARTESIAN_POINT('Ctrl Pts',(7.39178592285411,-3.37376545243903,
12.4468257733171));
#163182=CARTESIAN_POINT('Ctrl Pts',(7.40552591923626,-3.34349791512338,
12.4481274148966));
#163183=CARTESIAN_POINT('Ctrl Pts',(7.44176488958444,-3.26234853847497,
12.4516120073448));
#163184=CARTESIAN_POINT('Ctrl Pts',(7.4639276068279,-3.21131862306415,12.4537978337567));
#163185=CARTESIAN_POINT('Ctrl Pts',(7.55328028810477,-2.9996599415525,12.4628432180989));
#163186=CARTESIAN_POINT('Ctrl Pts',(7.61582209448657,-2.8371210124757,12.4697415681784));
#163187=CARTESIAN_POINT('Ctrl Pts',(7.76489656313638,-2.40914095653798,
12.4877789786306));
#163188=CARTESIAN_POINT('Ctrl Pts',(7.84305907362351,-2.14102831124228,
12.4989609756006));
#163189=CARTESIAN_POINT('Ctrl Pts',(7.92042105107633,-1.81380396183036,
12.512346261099));
#163190=CARTESIAN_POINT('Ctrl Pts',(7.93298418642574,-1.75804333802678,
12.5146177882177));
#163191=CARTESIAN_POINT('Ctrl Pts',(7.95865504449285,-1.63822232793874,
12.5194757383592));
#163192=CARTESIAN_POINT('Ctrl Pts',(7.97158001161698,-1.57412665431497,
12.5220602645463));
#163193=CARTESIAN_POINT('Ctrl Pts',(7.98841825203901,-1.48509188440374,
12.5256274314229));
#163194=CARTESIAN_POINT('Ctrl Pts',(7.99299102021141,-1.46028032789587,
12.526619029474));
#163195=CARTESIAN_POINT('Ctrl Pts',(8.00058106963645,-1.41799315544178,
12.5283046120188));
#163196=CARTESIAN_POINT('Ctrl Pts',(8.00365682013918,-1.40052831047807,
12.528999502148));
#163197=CARTESIAN_POINT('Ctrl Pts',(8.01049901803404,-1.3609179431206,12.5305728006465));
#163198=CARTESIAN_POINT('Ctrl Pts',(8.01423085740361,-1.33876657204445,
12.5314507173465));
#163199=CARTESIAN_POINT('Ctrl Pts',(8.02418580735126,-1.27814261285496,
12.5338485135776));
#163200=CARTESIAN_POINT('Ctrl Pts',(8.03022407002165,-1.23964019581819,
12.5353659830407));
#163201=CARTESIAN_POINT('Ctrl Pts',(8.06845771197173,-0.983836286024178,
12.5454166505161));
#163202=CARTESIAN_POINT('Ctrl Pts',(8.09210663306075,-0.765346949249157,
12.5538541972457));
#163203=CARTESIAN_POINT('Ctrl Pts',(8.10736665149593,-0.538839006894385,
12.5625610443669));
#163204=CARTESIAN_POINT('Ctrl Pts',(8.10785037039943,-0.531510929684908,
12.5628426859488));
#163205=CARTESIAN_POINT('Ctrl Pts',(8.11963563174591,-0.349210351509505,
12.5698480294779));
#163206=CARTESIAN_POINT('Ctrl Pts',(8.12528048587414,-0.173918382653126,
12.576560895722));
#163207=CARTESIAN_POINT('Ctrl Pts',(8.12522641224824,0.135823389154046,
12.5884549462431));
#163208=CARTESIAN_POINT('Ctrl Pts',(8.12186803869165,0.270206438898749,
12.5936257863592));
#163209=CARTESIAN_POINT('Ctrl Pts',(8.10741118415194,0.560283777379415,
12.6048397644352));
#163210=CARTESIAN_POINT('Ctrl Pts',(8.09515708609359,0.715866712459239,
12.6108872219502));
#163211=CARTESIAN_POINT('Ctrl Pts',(8.07103413390869,0.939604708174832,
12.6196507742779));
#163212=CARTESIAN_POINT('Ctrl Pts',(8.06276361071442,1.0081130394713,12.622343154546));
#163213=CARTESIAN_POINT('Ctrl Pts',(8.0463755951845,1.13071587734183,12.627178718226));
#163214=CARTESIAN_POINT('Ctrl Pts',(8.03858258780985,1.18484959679853,12.6293198543425));
#163215=CARTESIAN_POINT('Ctrl Pts',(8.02035646582059,1.30298677889777,12.6340061135323));
#163216=CARTESIAN_POINT('Ctrl Pts',(8.00970246524742,1.36695236380762,12.636552271451));
#163217=CARTESIAN_POINT('Ctrl Pts',(7.9853252457818,1.50322450858034,12.6419954437753));
#163218=CARTESIAN_POINT('Ctrl Pts',(7.97138299263149,1.57548606664267,12.6448932154794));
#163219=CARTESIAN_POINT('Ctrl Pts',(7.92510995838367,1.79895122553601,12.653888771948));
#163220=CARTESIAN_POINT('Ctrl Pts',(7.88944369472393,1.94942848893371,12.659995758361));
#163221=CARTESIAN_POINT('Ctrl Pts',(7.820432934825,2.20752902130431,12.6705405833494));
#163222=CARTESIAN_POINT('Ctrl Pts',(7.78910373554606,2.31564651979451,12.6749792416968));
#163223=CARTESIAN_POINT('Ctrl Pts',(7.74231925136006,2.46538945028468,12.6811482070504));
#163224=CARTESIAN_POINT('Ctrl Pts',(7.72875389267594,2.507591636382,12.6828891870632));
#163225=CARTESIAN_POINT('Ctrl Pts',(7.70093454293506,2.5917676400348,12.6863655488141));
#163226=CARTESIAN_POINT('Ctrl Pts',(7.6866810535198,2.63374006556882,12.6881008722784));
#163227=CARTESIAN_POINT('Ctrl Pts',(7.62927067352579,2.79836045644615,12.6949181143822));
#163228=CARTESIAN_POINT('Ctrl Pts',(7.5835158515422,2.92008215772154,12.6999834793816));
#163229=CARTESIAN_POINT('Ctrl Pts',(7.45466117616743,3.23938912228191,12.7133915839555));
#163230=CARTESIAN_POINT('Ctrl Pts',(7.36663157493395,3.43487321047026,12.7217264267388));
#163231=CARTESIAN_POINT('Ctrl Pts',(7.24253407197357,3.68367326433715,12.7325923283225));
#163232=CARTESIAN_POINT('Ctrl Pts',(7.21342082468294,3.74036207792905,12.7350858325704));
#163233=CARTESIAN_POINT('Ctrl Pts',(7.15803331728252,3.84515936778576,12.7397311063965));
#163234=CARTESIAN_POINT('Ctrl Pts',(7.13193324719649,3.89335583621992,12.7418817495222));
#163235=CARTESIAN_POINT('Ctrl Pts',(7.07054271093535,4.00403069526038,12.7468551348575));
#163236=CARTESIAN_POINT('Ctrl Pts',(7.03490830119401,4.06631296981573,12.749679898323));
#163237=CARTESIAN_POINT('Ctrl Pts',(6.90569743345405,4.2853660497278,12.7597122306441));
#163238=CARTESIAN_POINT('Ctrl Pts',(6.8076682124996,4.43944498129916,12.7669491890796));
#163239=CARTESIAN_POINT('Ctrl Pts',(6.5213797708074,4.85761335604164,12.7871282773802));
#163240=CARTESIAN_POINT('Ctrl Pts',(6.32237899041786,5.11393424234623,12.8001312462778));
#163241=CARTESIAN_POINT('Ctrl Pts',(6.10601221395583,5.36062662406682,12.8132451629552));
#163242=CARTESIAN_POINT('Ctrl Pts',(6.10342270025719,5.363574768904,12.8134019727042));
#163243=CARTESIAN_POINT('Ctrl Pts',(5.98322556172651,5.50021868215928,12.8206741013764));
#163244=CARTESIAN_POINT('Ctrl Pts',(5.86125578380425,5.63001558501365,12.8277665808182));
#163245=CARTESIAN_POINT('Ctrl Pts',(5.70797719928455,5.78274605810582,12.8363063478163));
#163246=CARTESIAN_POINT('Ctrl Pts',(5.68064413497349,5.80959877378475,12.8378153842299));
#163247=CARTESIAN_POINT('Ctrl Pts',(5.63708802386881,5.85178814322042,12.8401978025678));
#163248=CARTESIAN_POINT('Ctrl Pts',(5.62099001452248,5.86725294521716,12.8410735806017));
#163249=CARTESIAN_POINT('Ctrl Pts',(5.59197786867657,5.89489492048746,12.8426432995449));
#163250=CARTESIAN_POINT('Ctrl Pts',(5.57908718359271,5.90709647861592,12.8433377316474));
#163251=CARTESIAN_POINT('Ctrl Pts',(5.54756603271848,5.93673731017992,12.8450283510913));
#163252=CARTESIAN_POINT('Ctrl Pts',(5.52889320415729,5.95413123113358,12.8460235201225));
#163253=CARTESIAN_POINT('Ctrl Pts',(5.46051063987603,6.01723118837448,12.8496457863755));
#163254=CARTESIAN_POINT('Ctrl Pts',(5.41031330004677,6.06240527570437,12.8522624192402));
#163255=CARTESIAN_POINT('Ctrl Pts',(5.27619003327776,6.18011405732958,12.8591547037826));
#163256=CARTESIAN_POINT('Ctrl Pts',(5.19133168771568,6.25156513372939,12.8634153933824));
#163257=CARTESIAN_POINT('Ctrl Pts',(4.81391014043049,6.55637016173753,12.8820118466904));
#163258=CARTESIAN_POINT('Ctrl Pts',(4.50689160434748,6.77108906724472,12.8962618687067));
#163259=CARTESIAN_POINT('Ctrl Pts',(4.1286791668259,6.99844236261406,12.9133565198978));
#163260=CARTESIAN_POINT('Ctrl Pts',(4.07076238092081,7.03228844221481,12.9159613342482));
#163261=CARTESIAN_POINT('Ctrl Pts',(3.97829228913194,7.0848020126076,12.9201018620056));
#163262=CARTESIAN_POINT('Ctrl Pts',(3.94401120632091,7.10394289712026,12.9216329242276));
#163263=CARTESIAN_POINT('Ctrl Pts',(3.88178116706388,7.13809982075457,12.9244055000265));
#163264=CARTESIAN_POINT('Ctrl Pts',(3.85388040109641,7.15320207504099,12.9256461548602));
#163265=CARTESIAN_POINT('Ctrl Pts',(3.78721485060061,7.18878385432034,12.9286049810804));
#163266=CARTESIAN_POINT('Ctrl Pts',(3.74837140701687,7.20911377380686,12.9303245258839));
#163267=CARTESIAN_POINT('Ctrl Pts',(3.62786248225703,7.2709485653715,12.9356460555939));
#163268=CARTESIAN_POINT('Ctrl Pts',(3.54565856797332,7.3113873087351,12.939257552339));
#163269=CARTESIAN_POINT('Ctrl Pts',(3.34521591942216,7.40581591237887,12.948019966004));
#163270=CARTESIAN_POINT('Ctrl Pts',(3.22633159949039,7.45837535378336,12.9531811865184));
#163271=CARTESIAN_POINT('Ctrl Pts',(2.97358353615235,7.56294241038155,12.9640708603669));
#163272=CARTESIAN_POINT('Ctrl Pts',(2.83949751547102,7.61429909300117,12.9698004062699));
#163273=CARTESIAN_POINT('Ctrl Pts',(2.55189027818813,7.71580225734242,12.9819613538924));
#163274=CARTESIAN_POINT('Ctrl Pts',(2.39809040965023,7.76497981508553,12.988388873169));
#163275=CARTESIAN_POINT('Ctrl Pts',(2.21029081637543,7.81891648814228,12.9961084248972));
#163276=CARTESIAN_POINT('Ctrl Pts',(2.17759608140437,7.82808506987927,12.9974476363544));
#163277=CARTESIAN_POINT('Ctrl Pts',(2.12701176194575,7.84192899495319,12.9995117913366));
#163278=CARTESIAN_POINT('Ctrl Pts',(2.10916214084377,7.84674865555616,13.0002386655092));
#163279=CARTESIAN_POINT('Ctrl Pts',(2.07516901176752,7.8558029298737,13.0016199651753));
#163280=CARTESIAN_POINT('Ctrl Pts',(2.05902860106362,7.86004881172323,13.0022745537269));
#163281=CARTESIAN_POINT('Ctrl Pts',(2.01957599720585,7.87029731570946,13.0038713705553));
#163282=CARTESIAN_POINT('Ctrl Pts',(1.99624996112023,7.87624613282752,13.0048127409227));
#163283=CARTESIAN_POINT('Ctrl Pts',(1.91697599265494,7.89608851115254,13.0080032020417));
#163284=CARTESIAN_POINT('Ctrl Pts',(1.86090652234849,7.90949035783482,13.0102449219928));
#163285=CARTESIAN_POINT('Ctrl Pts',(1.72335358951067,7.94082491959504,13.0157127795035));
#163286=CARTESIAN_POINT('Ctrl Pts',(1.6417271886123,7.9581015331882,13.0189304841876));
#163287=CARTESIAN_POINT('Ctrl Pts',(1.16626462801893,8.05110864238313,13.0375488955238));
#163288=CARTESIAN_POINT('Ctrl Pts',(0.767516496533518,8.09885474919749,
13.0526844958605));
#163289=CARTESIAN_POINT('Ctrl Pts',(-0.0243256322105377,8.13464477912087,
13.0828320313359));
#163290=CARTESIAN_POINT('Ctrl Pts',(-0.416285256848256,8.12402210800684,
13.0978017719164));
#163291=CARTESIAN_POINT('Ctrl Pts',(-0.878679891243662,8.07792996870312,
13.1158512736093));
#163292=CARTESIAN_POINT('Ctrl Pts',(-0.951316316782368,8.06969814280534,
13.1186975124839));
#163293=CARTESIAN_POINT('Ctrl Pts',(-1.06639269489724,8.05508130715052,
13.1232255901971));
#163294=CARTESIAN_POINT('Ctrl Pts',(-1.10891032474857,8.0493382411396,13.1249026847915));
#163295=CARTESIAN_POINT('Ctrl Pts',(-1.18853383091524,8.03794025607925,
13.1280513735352));
#163296=CARTESIAN_POINT('Ctrl Pts',(-1.22564991694263,8.03236444007877,
13.1295223727827));
#163297=CARTESIAN_POINT('Ctrl Pts',(-1.30910066704185,8.01923605120664,
13.1328372422107));
#163298=CARTESIAN_POINT('Ctrl Pts',(-1.35541116447638,8.01153867600735,
13.1346820409557));
#163299=CARTESIAN_POINT('Ctrl Pts',(-1.49612430276273,7.98689541309926,
13.1403037168932));
#163300=CARTESIAN_POINT('Ctrl Pts',(-1.59029561554957,7.96867906091219,
13.1440884340889));
#163301=CARTESIAN_POINT('Ctrl Pts',(-2.07638046892051,7.86569167020248,
13.1637430540058));
#163302=CARTESIAN_POINT('Ctrl Pts',(-2.46194117266534,7.7536634151502,13.1796706999063));
#163303=CARTESIAN_POINT('Ctrl Pts',(-3.37548708643007,7.41317937668523,
13.219369094247));
#163304=CARTESIAN_POINT('Ctrl Pts',(-3.89055131671592,7.15630364767962,
13.2436235605803));
#163305=CARTESIAN_POINT('Ctrl Pts',(-4.6817238195332,6.65088776830117,13.2833193094023));
#163306=CARTESIAN_POINT('Ctrl Pts',(-4.97567075385715,6.43393864775923,
13.2986554155622));
#163307=CARTESIAN_POINT('Ctrl Pts',(-5.271039703248,6.18355273141817,13.31405987864));
#163308=CARTESIAN_POINT('Ctrl Pts',(-5.28797527843433,6.16907621948654,
13.3149429953921));
#163309=CARTESIAN_POINT('Ctrl Pts',(-5.31157585719797,6.14873387727936,
13.3161732273468));
#163310=CARTESIAN_POINT('Ctrl Pts',(-5.31829103236338,6.14292657258945,
13.3165232208836));
#163311=CARTESIAN_POINT('Ctrl Pts',(-5.33054637658521,6.13229295416775,
13.3171618545407));
#163312=CARTESIAN_POINT('Ctrl Pts',(-5.3360895382101,6.12747011329402,13.3174506699977));
#163313=CARTESIAN_POINT('Ctrl Pts',(-5.34726691166493,6.11771854323587,
13.3180329461882));
#163314=CARTESIAN_POINT('Ctrl Pts',(-5.35290087026406,6.11278953281106,
13.3183263918714));
#163315=CARTESIAN_POINT('Ctrl Pts',(-5.36667910793966,6.1007016394232,13.3190438917053));
#163316=CARTESIAN_POINT('Ctrl Pts',(-5.37481589761371,6.09353421333666,
13.3194674920889));
#163317=CARTESIAN_POINT('Ctrl Pts',(-5.40403519183322,6.06769185358593,
13.3209881278449));
#163318=CARTESIAN_POINT('Ctrl Pts',(-5.42503507162761,6.04892348136956,
13.3220800358314));
#163319=CARTESIAN_POINT('Ctrl Pts',(-5.47489135842505,6.00389659496003,
13.3246691023441));
#163320=CARTESIAN_POINT('Ctrl Pts',(-5.50365661898026,5.97753909517631,
13.3261600399065));
#163321=CARTESIAN_POINT('Ctrl Pts',(-5.61319005240674,5.87571301501655,
13.3318254670337));
#163322=CARTESIAN_POINT('Ctrl Pts',(-5.69260618936603,5.7988052445606,13.3359105932849));
#163323=CARTESIAN_POINT('Ctrl Pts',(-5.84121769827905,5.64889132300337,
13.3435581474931));
#163324=CARTESIAN_POINT('Ctrl Pts',(-5.91067464328007,5.57617462807115,
13.3471337754295));
#163325=CARTESIAN_POINT('Ctrl Pts',(-6.34754353353314,5.10146574407053,
13.3697503737428));
#163326=CARTESIAN_POINT('Ctrl Pts',(-6.6751135739383,4.66467236324227,13.3873648446608));
#163327=CARTESIAN_POINT('Ctrl Pts',(-7.23816479058777,3.73172183817601,
13.4241844453894));
#163328=CARTESIAN_POINT('Ctrl Pts',(-7.47210109343363,3.23796257742278,
13.4433330854693));
#163329=CARTESIAN_POINT('Ctrl Pts',(-7.66589678109804,2.69347372518248,
13.4655461536033));
#163330=CARTESIAN_POINT('Ctrl Pts',(-7.67676087554533,2.66235170405505,
13.466819014893));
#163331=CARTESIAN_POINT('Ctrl Pts',(-7.69155799754245,2.61911916946679,
13.4685917905977));
#163332=CARTESIAN_POINT('Ctrl Pts',(-7.6956524539559,2.60706404976685,13.469086612322));
#163333=CARTESIAN_POINT('Ctrl Pts',(-7.70264339496538,2.58632097044656,
13.4699389058854));
#163334=CARTESIAN_POINT('Ctrl Pts',(-7.70555356083715,2.57763763018865,
13.4702959465569));
#163335=CARTESIAN_POINT('Ctrl Pts',(-7.71151842262826,2.55973932786888,
13.4710324245912));
#163336=CARTESIAN_POINT('Ctrl Pts',(-7.7145712958446,2.55052377556824,13.4714119185104));
#163337=CARTESIAN_POINT('Ctrl Pts',(-7.72162018532796,2.52911721060339,
13.4722941208803));
#163338=CARTESIAN_POINT('Ctrl Pts',(-7.72560385391594,2.51692217638347,
13.4727972154702));
#163339=CARTESIAN_POINT('Ctrl Pts',(-7.73813365574603,2.47825521040637,
13.4743940346073));
#163340=CARTESIAN_POINT('Ctrl Pts',(-7.74657269533374,2.45174893072979,
13.4754911045726));
#163341=CARTESIAN_POINT('Ctrl Pts',(-7.89106858409783,1.9897055463641,13.4946580149614));
#163342=CARTESIAN_POINT('Ctrl Pts',(-7.99032050392628,1.54356395549976,
13.5138974622575));
#163343=CARTESIAN_POINT('Ctrl Pts',(-8.13590801593221,0.469610143936951,
13.561464420844));
#163344=CARTESIAN_POINT('Ctrl Pts',(-8.14787814512287,-0.159913341030507,
13.5903960898329));
#163345=CARTESIAN_POINT('Ctrl Pts',(-8.06448285092655,-1.01960194796715,
13.6277739166654));
#163346=CARTESIAN_POINT('Ctrl Pts',(-8.03143646325101,-1.25360759790878,
13.6376928214678));
#163347=CARTESIAN_POINT('Ctrl Pts',(-7.9843266000613,-1.50687505773135,
13.6479782746439));
#163348=CARTESIAN_POINT('Ctrl Pts',(-7.98033816120067,-1.52785684564516,
13.6488274191142));
#163349=CARTESIAN_POINT('Ctrl Pts',(-7.97439042339924,-1.55848704097327,
13.6500630086645));
#163350=CARTESIAN_POINT('Ctrl Pts',(-7.97249626333242,-1.568147892881,13.6504521304163));
#163351=CARTESIAN_POINT('Ctrl Pts',(-7.96911149429858,-1.58524669946106,
13.6511398331978));
#163352=CARTESIAN_POINT('Ctrl Pts',(-7.96762802074529,-1.59268604258533,
13.6514387010863));
#163353=CARTESIAN_POINT('Ctrl Pts',(-7.96452861838806,-1.60811626267442,
13.652057911054));
#163354=CARTESIAN_POINT('Ctrl Pts',(-7.96291107627683,-1.61610680937648,
13.6523781888274));
#163355=CARTESIAN_POINT('Ctrl Pts',(-7.95897655298582,-1.63539376545993,
13.6531503567509));
#163356=CARTESIAN_POINT('Ctrl Pts',(-7.95664754097391,-1.64668772068941,
13.6536017782278));
#163357=CARTESIAN_POINT('Ctrl Pts',(-7.94724951612034,-1.69177560196719,
13.6554011076346));
#163358=CARTESIAN_POINT('Ctrl Pts',(-7.93998913030676,-1.72552954523484,
13.6567417524963));
#163359=CARTESIAN_POINT('Ctrl Pts',(-7.85045011729405,-2.12926688375388,
13.6727103171344));
#163360=CARTESIAN_POINT('Ctrl Pts',(-7.74259037580817,-2.49312490423682,
13.686446536905));
#163361=CARTESIAN_POINT('Ctrl Pts',(-7.51812037466152,-3.09286863595076,
13.7094869402501));
#163362=CARTESIAN_POINT('Ctrl Pts',(-7.41477146620844,-3.33303679540352,
13.7188240421466));
#163363=CARTESIAN_POINT('Ctrl Pts',(-7.22080962029552,-3.72989888120363,
13.734797834149));
#163364=CARTESIAN_POINT('Ctrl Pts',(-7.1362134658379,-3.88930494587637,
13.7413695874925));
#163365=CARTESIAN_POINT('Ctrl Pts',(-6.89634112509056,-4.30708354358129,
13.7591388010169));
#163366=CARTESIAN_POINT('Ctrl Pts',(-6.73188462752959,-4.55984736301125,
13.77047879151));
#163367=CARTESIAN_POINT('Ctrl Pts',(-6.52640603715794,-4.84023301346545,
13.7838664348178));
#163368=CARTESIAN_POINT('Ctrl Pts',(-6.49871836672879,-4.87734466039689,
13.7856553234286));
#163369=CARTESIAN_POINT('Ctrl Pts',(-6.45364850054224,-4.93668966660062,
13.788543322045));
#163370=CARTESIAN_POINT('Ctrl Pts',(-6.43646496279797,-4.95907275675567,
13.7896389474758));
#163371=CARTESIAN_POINT('Ctrl Pts',(-6.40562921220849,-4.99880880204938,
13.7915953392448));
#163372=CARTESIAN_POINT('Ctrl Pts',(-6.39202218135125,-5.01619651448734,
13.7924553334493));
#163373=CARTESIAN_POINT('Ctrl Pts',(-6.3640932228792,-5.05158729831142,
13.7942137650788));
#163374=CARTESIAN_POINT('Ctrl Pts',(-6.34976535078684,-5.06958546305727,
13.795112306174));
#163375=CARTESIAN_POINT('Ctrl Pts',(-6.31488382093588,-5.11302253745017,
13.7972914658354));
#163376=CARTESIAN_POINT('Ctrl Pts',(-6.2942526715158,-5.13839862539558,
13.7985734205575));
#163377=CARTESIAN_POINT('Ctrl Pts',(-6.24979673645968,-5.19240944362112,
13.8013215170356));
#163378=CARTESIAN_POINT('Ctrl Pts',(-6.22592713022495,-5.22100626552055,
13.802788463463));
#163379=CARTESIAN_POINT('Ctrl Pts',(-6.15891938904798,-5.30017145713959,
13.8068836613977));
#163380=CARTESIAN_POINT('Ctrl Pts',(-6.11535637965859,-5.35037584988356,
13.8095201028655));
#163381=CARTESIAN_POINT('Ctrl Pts',(-5.60167378669033,-5.92790138346935,
13.8403273616097));
#163382=CARTESIAN_POINT('Ctrl Pts',(-5.06535293188475,-6.39224516803299,
13.870189554341));
#163383=CARTESIAN_POINT('Ctrl Pts',(-4.1731431339223,-6.98112513724939,
13.9154807261136));
#163384=CARTESIAN_POINT('Ctrl Pts',(-3.85739039063744,-7.16043244712547,
13.9307341555609));
#163385=CARTESIAN_POINT('Ctrl Pts',(-3.50968662207309,-7.32818749529782,
13.9461324872889));
#163386=CARTESIAN_POINT('Ctrl Pts',(-3.48862483465983,-7.33823745373713,
13.9470598791207));
#163387=CARTESIAN_POINT('Ctrl Pts',(-3.4591168882185,-7.35216187597435,
13.9483514514342));
#163388=CARTESIAN_POINT('Ctrl Pts',(-3.4507070411492,-7.35611275157657,
13.9487186795228));
#163389=CARTESIAN_POINT('Ctrl Pts',(-3.43532726855884,-7.36330586161073,
13.9493886424841));
#163390=CARTESIAN_POINT('Ctrl Pts',(-3.42835948964244,-7.36655264448757,
13.9496915628579));
#163391=CARTESIAN_POINT('Ctrl Pts',(-3.41428626500377,-7.37308606704384,
13.9503021541476));
#163392=CARTESIAN_POINT('Ctrl Pts',(-3.40718065477388,-7.37637233589074,
13.9506098094754));
#163393=CARTESIAN_POINT('Ctrl Pts',(-3.39077061745227,-7.38393303225723,
13.9513188446949));
#163394=CARTESIAN_POINT('Ctrl Pts',(-3.38146282629712,-7.38820015704858,
13.9517199149312));
#163395=CARTESIAN_POINT('Ctrl Pts',(-3.34941098096333,-7.40282095767582,
13.9530971989544));
#163396=CARTESIAN_POINT('Ctrl Pts',(-3.32662710202135,-7.41308735905932,
13.9540696240554));
#163397=CARTESIAN_POINT('Ctrl Pts',(-3.04938497800849,-7.53647692759427,
13.9658194137989));
#163398=CARTESIAN_POINT('Ctrl Pts',(-2.78932587080811,-7.63654979001016,
13.9759205824542));
#163399=CARTESIAN_POINT('Ctrl Pts',(-2.24623522085326,-7.81408395708418,
13.9959170691738));
#163400=CARTESIAN_POINT('Ctrl Pts',(-1.96310325567743,-7.88997562693376,
14.0057762624287));
#163401=CARTESIAN_POINT('Ctrl Pts',(-1.05389143425787,-8.0816990929973,
14.0370185658688));
#163402=CARTESIAN_POINT('Ctrl Pts',(-0.418044759607934,-8.1393936853567,
14.0584267287375));
#163403=CARTESIAN_POINT('Ctrl Pts',(0.332034642464033,-8.11926481577325,
14.0864905474198));
#163404=CARTESIAN_POINT('Ctrl Pts',(0.446021357419688,-8.11380132263703,
14.0908253368615));
#163405=CARTESIAN_POINT('Ctrl Pts',(0.580351035453153,-8.10452357779809,
14.0960250643709));
#163406=CARTESIAN_POINT('Ctrl Pts',(0.600843807705472,-8.10303007885709,
14.0968208180633));
#163407=CARTESIAN_POINT('Ctrl Pts',(0.633771616807793,-8.10050472435891,
14.0981035155635));
#163408=CARTESIAN_POINT('Ctrl Pts',(0.64621037939032,-8.09952192388845,
14.098589001801));
#163409=CARTESIAN_POINT('Ctrl Pts',(0.668302200619706,-8.09772520987412,
14.0994529232982));
#163410=CARTESIAN_POINT('Ctrl Pts',(0.677956173038525,-8.09692267671162,
14.0998310195746));
#163411=CARTESIAN_POINT('Ctrl Pts',(0.698054440783082,-8.09521571432498,
14.1006193552372));
#163412=CARTESIAN_POINT('Ctrl Pts',(0.708498463867401,-8.09430833298691,
14.1010296817812));
#163413=CARTESIAN_POINT('Ctrl Pts',(0.735531870432197,-8.09190693655351,
14.1020935176946));
#163414=CARTESIAN_POINT('Ctrl Pts',(0.752118431179804,-8.09038212099813,
14.1027479425286));
#163415=CARTESIAN_POINT('Ctrl Pts',(0.822228055981327,-8.08371942252818,
14.1055213714936));
#163416=CARTESIAN_POINT('Ctrl Pts',(0.87570352049668,-8.07810137887934,
14.1076546511089));
#163417=CARTESIAN_POINT('Ctrl Pts',(1.24022518812339,-8.03614326948219,
14.1223208471738));
#163418=CARTESIAN_POINT('Ctrl Pts',(1.54897642954337,-7.98238078572129,
14.135376048327));
#163419=CARTESIAN_POINT('Ctrl Pts',(2.18728447981832,-7.83280074373423,
14.1636382699979));
#163420=CARTESIAN_POINT('Ctrl Pts',(2.51544151354283,-7.73366100248514,
14.1789059796341));
#163421=CARTESIAN_POINT('Ctrl Pts',(3.05109891142204,-7.53412241829739,
14.2046454737515));
#163422=CARTESIAN_POINT('Ctrl Pts',(3.26236994671229,-7.44507543081946,
14.2150168142248));
#163423=CARTESIAN_POINT('Ctrl Pts',(3.85611953556844,-7.16468759245913,
14.2444354636741));
#163424=CARTESIAN_POINT('Ctrl Pts',(4.22770209726597,-6.95191043031932,
14.2631858947543));
#163425=CARTESIAN_POINT('Ctrl Pts',(4.60406820829356,-6.69500059460983,
14.2814260489235));
#163426=CARTESIAN_POINT('Ctrl Pts',(4.62719245635694,-6.67903937922231,
14.2825440338913));
#163427=CARTESIAN_POINT('Ctrl Pts',(4.65847882429817,-6.65720389526688,
14.2840536065798));
#163428=CARTESIAN_POINT('Ctrl Pts',(4.6667133330728,-6.6514340805399,14.2844506366657));
#163429=CARTESIAN_POINT('Ctrl Pts',(4.68065410986139,-6.64162732497241,
14.2851223480283));
#163430=CARTESIAN_POINT('Ctrl Pts',(4.68636590397448,-6.63759828812231,
14.2853974325158));
#163431=CARTESIAN_POINT('Ctrl Pts',(4.6973584469272,-6.62982300698355,14.2859266092858));
#163432=CARTESIAN_POINT('Ctrl Pts',(4.70263992857332,-6.62607781310718,
14.2861807540156));
#163433=CARTESIAN_POINT('Ctrl Pts',(4.71509489543437,-6.61722337936885,
14.2867798553238));
#163434=CARTESIAN_POINT('Ctrl Pts',(4.72226456996205,-6.61210877538087,
14.287124545213));
#163435=CARTESIAN_POINT('Ctrl Pts',(4.74315948847447,-6.59715172512569,
14.2881286037214));
#163436=CARTESIAN_POINT('Ctrl Pts',(4.75686242450724,-6.58727809471519,
14.2887864526372));
#163437=CARTESIAN_POINT('Ctrl Pts',(4.85526228792436,-6.51590906199142,
14.2935067227391));
#163438=CARTESIAN_POINT('Ctrl Pts',(4.93879690337251,-6.45282333609843,
14.2974942624056));
#163439=CARTESIAN_POINT('Ctrl Pts',(5.31333347994523,-6.15843681109112,
14.3153886311979));
#163440=CARTESIAN_POINT('Ctrl Pts',(5.58948205134802,-5.90893994422799,
14.3286539555681));
#163441=CARTESIAN_POINT('Ctrl Pts',(6.06029308553835,-5.42092168292343,
14.3529351721314));
#163442=CARTESIAN_POINT('Ctrl Pts',(6.26035707750009,-5.18859035543701,
14.3639118186475));
#163443=CARTESIAN_POINT('Ctrl Pts',(6.72256391815325,-4.58607210050807,
14.391673525633));
#163444=CARTESIAN_POINT('Ctrl Pts',(6.96774721820448,-4.20421096007589,
14.4087209982007));
#163445=CARTESIAN_POINT('Ctrl Pts',(7.26203408503647,-3.64875137428103,
14.432884768104));
#163446=CARTESIAN_POINT('Ctrl Pts',(7.33919405593078,-3.49095336930485,
14.4396670969788));
#163447=CARTESIAN_POINT('Ctrl Pts',(7.4358103804484,-3.2759764516292,14.4488321095968));
#163448=CARTESIAN_POINT('Ctrl Pts',(7.45983210649493,-3.22090090167561,
14.451173687549));
#163449=CARTESIAN_POINT('Ctrl Pts',(7.49716967973637,-3.13263668391524,
14.4549174866989));
#163450=CARTESIAN_POINT('Ctrl Pts',(7.51088117621391,-3.09961767738581,
14.4563160642541));
#163451=CARTESIAN_POINT('Ctrl Pts',(7.53874294288063,-3.03125253053726,
14.4592081124436));
#163452=CARTESIAN_POINT('Ctrl Pts',(7.55286360259231,-2.99589526682532,
14.4607018158985));
#163453=CARTESIAN_POINT('Ctrl Pts',(7.58029613157925,-2.92577911101131,
14.4636603307241));
#163454=CARTESIAN_POINT('Ctrl Pts',(7.59361870678652,-2.89102538417816,
14.4651250048073));
#163455=CARTESIAN_POINT('Ctrl Pts',(7.62404083724737,-2.8100038923447,14.4685359180104));
#163456=CARTESIAN_POINT('Ctrl Pts',(7.64095877724817,-2.76366957094366,
14.4704837649845));
#163457=CARTESIAN_POINT('Ctrl Pts',(7.68407490465732,-2.64216152334515,
14.4755854009179));
#163458=CARTESIAN_POINT('Ctrl Pts',(7.70959198382766,-2.56675202821044,
14.478745170077));
#163459=CARTESIAN_POINT('Ctrl Pts',(7.78346298305599,-2.33739730368214,
14.4883392099087));
#163460=CARTESIAN_POINT('Ctrl Pts',(7.82834298630422,-2.18237652997822,
14.494802270924));
#163461=CARTESIAN_POINT('Ctrl Pts',(7.94553954914191,-1.72723645234392,
14.5137247948711));
#163462=CARTESIAN_POINT('Ctrl Pts',(8.00540878376709,-1.42420903210038,
14.5262623520816));
#163463=CARTESIAN_POINT('Ctrl Pts',(8.08845226859735,-0.826698105907153,
14.5507795449631));
#163464=CARTESIAN_POINT('Ctrl Pts',(8.11310822517487,-0.532887231041014,
14.5627392502568));
#163465=CARTESIAN_POINT('Ctrl Pts',(8.12405742833518,-0.159848937730708,
14.5776698109421));
#163466=CARTESIAN_POINT('Ctrl Pts',(8.12522331385657,-0.0812833074808247,
14.5807997949565));
#163467=CARTESIAN_POINT('Ctrl Pts',(8.12524954711001,-0.00271287458686051,
14.5839128245719));
#163468=CARTESIAN_POINT('',(8.1269655491554,-0.00168838483458986,16.5832974432124));
#163469=CARTESIAN_POINT('Ctrl Pts',(8.12631724021387,-0.0026888491199863,
14.5832974432124));
#163470=CARTESIAN_POINT('Ctrl Pts',(8.12636183407428,0.0449434531170251,
14.5851677846816));
#163471=CARTESIAN_POINT('Ctrl Pts',(8.11510270816418,1.43976685797085,14.6399272812462));
#163472=CARTESIAN_POINT('Ctrl Pts',(7.36660492052285,4.18569279410474,14.7475759329063));
#163473=CARTESIAN_POINT('Ctrl Pts',(4.46947152341234,7.18896984766691,14.9062433981928));
#163474=CARTESIAN_POINT('Ctrl Pts',(0.494311211965678,8.45828284271795,
15.0649108634792));
#163475=CARTESIAN_POINT('Ctrl Pts',(-3.62342745787823,7.65690432669853,
15.2235783287656));
#163476=CARTESIAN_POINT('Ctrl Pts',(-6.81611969460216,5.00581298154595,
15.382245794052));
#163477=CARTESIAN_POINT('Ctrl Pts',(-8.96101480030011,-0.17955105281227,
15.593802414434));
#163478=CARTESIAN_POINT('Ctrl Pts',(-6.78077229295221,-5.84776877811949,
15.8053590348158));
#163479=CARTESIAN_POINT('Ctrl Pts',(-1.74999298391495,-8.26945455504393,
16.0169156551978));
#163480=CARTESIAN_POINT('Ctrl Pts',(3.83053466397949,-8.09334768555441,
16.2284722755797));
#163481=CARTESIAN_POINT('Ctrl Pts',(7.65853128092144,-4.25683691476263,
16.4172662049179));
#163482=CARTESIAN_POINT('Ctrl Pts',(8.13065759321727,-0.773914348631322,
16.5531709791606));
#163483=CARTESIAN_POINT('Ctrl Pts',(8.1269655491554,-0.00168838483458986,
16.5832974432124));
#163484=CARTESIAN_POINT('',(8.12524999728007,-0.000210238467608934,18.5832974432342));
#163485=CARTESIAN_POINT('Ctrl Pts',(8.12524982465525,-0.00168802839118938,
16.5832974432124));
#163486=CARTESIAN_POINT('Ctrl Pts',(8.12528831832782,0.183599557962629,
16.5905275087158));
#163487=CARTESIAN_POINT('Ctrl Pts',(8.11898455471787,0.368960515185087,
16.5977575742192));
#163488=CARTESIAN_POINT('Ctrl Pts',(8.10634970717896,0.553879036811779,
16.6049876397226));
#163489=CARTESIAN_POINT('Ctrl Pts',(8.093715609276,0.738786587069809,16.6122172762602));
#163490=CARTESIAN_POINT('Ctrl Pts',(8.07475120840512,0.923251363949085,
16.6194469127978));
#163491=CARTESIAN_POINT('Ctrl Pts',(8.04951964886878,1.10676148513372,16.6266765493355));
#163492=CARTESIAN_POINT('Ctrl Pts',(8.02427989708313,1.29033118886856,16.6339085332105));
#163493=CARTESIAN_POINT('Ctrl Pts',(7.99276898989149,1.47294523245479,16.6411405170856));
#163494=CARTESIAN_POINT('Ctrl Pts',(7.95510137049552,1.65410088798726,16.6483725009607));
#163495=CARTESIAN_POINT('Ctrl Pts',(7.9495230652595,1.68092874591926,16.6494435060883));
#163496=CARTESIAN_POINT('Ctrl Pts',(7.94380982437166,1.70772464251782,16.6505145112159));
#163497=CARTESIAN_POINT('Ctrl Pts',(7.93796211318075,1.73448697089573,16.6515855163435));
#163498=CARTESIAN_POINT('Ctrl Pts',(7.88715201736832,1.96702179087069,16.6608913577867));
#163499=CARTESIAN_POINT('Ctrl Pts',(7.82618932688376,2.1970058040725,16.67019719923));
#163500=CARTESIAN_POINT('Ctrl Pts',(7.75535875541403,2.42365388150265,16.6795030406732));
#163501=CARTESIAN_POINT('Ctrl Pts',(7.68414790889602,2.65151878673472,16.6888588433017));
#163502=CARTESIAN_POINT('Ctrl Pts',(7.60296300456688,2.87601181259765,16.6982146459302));
#163503=CARTESIAN_POINT('Ctrl Pts',(7.51213915957558,3.09636122079952,16.7075704485587));
#163504=CARTESIAN_POINT('Ctrl Pts',(7.42087441429973,3.31778030532687,16.7169716685117));
#163505=CARTESIAN_POINT('Ctrl Pts',(7.31987695578548,3.53501541466431,16.7263728884648));
#163506=CARTESIAN_POINT('Ctrl Pts',(7.20953213564697,3.74731022836029,16.7357741084178));
#163507=CARTESIAN_POINT('Ctrl Pts',(7.0990678896688,3.9598348080421,16.7451855032805));
#163508=CARTESIAN_POINT('Ctrl Pts',(6.97923607346948,4.16740836932671,16.7545968981433));
#163509=CARTESIAN_POINT('Ctrl Pts',(6.85046801357916,4.36929920667248,16.7640082930061));
#163510=CARTESIAN_POINT('Ctrl Pts',(6.72185100078244,4.57095322268047,16.7734086481448));
#163511=CARTESIAN_POINT('Ctrl Pts',(6.58431871991006,4.76693781038664,16.7828090032836));
#163512=CARTESIAN_POINT('Ctrl Pts',(6.43834511216219,4.9565511980809,16.7922093584224));
#163513=CARTESIAN_POINT('Ctrl Pts',(6.34494818769979,5.07786975367987,16.7982238994916));
#163514=CARTESIAN_POINT('Ctrl Pts',(6.24809651951929,5.19658067909184,16.8042384405607));
#163515=CARTESIAN_POINT('Ctrl Pts',(6.14792370588667,5.31250615708789,16.8102529816299));
#163516=CARTESIAN_POINT('Ctrl Pts',(6.01897491033632,5.46173278075059,16.8179952801492));
#163517=CARTESIAN_POINT('Ctrl Pts',(5.88445987714346,5.60641184966154,16.8257375786684));
#163518=CARTESIAN_POINT('Ctrl Pts',(5.7447395344376,5.74609913280041,16.8334798771877));
#163519=CARTESIAN_POINT('Ctrl Pts',(5.60510622485313,5.88569940341101,16.8412173529561));
#163520=CARTESIAN_POINT('Ctrl Pts',(5.4602743105939,6.02031383074355,16.8489548287245));
#163521=CARTESIAN_POINT('Ctrl Pts',(5.31064408635514,6.14953225461589,16.8566923044929));
#163522=CARTESIAN_POINT('Ctrl Pts',(5.16108047460359,6.27869315294048,16.8644263356864));
#163523=CARTESIAN_POINT('Ctrl Pts',(5.00672307400017,6.40246260164256,16.8721603668799));
#163524=CARTESIAN_POINT('Ctrl Pts',(4.84800812455714,6.52046814168492,16.8798943980735));
#163525=CARTESIAN_POINT('Ctrl Pts',(4.68931348562947,6.63845858073431,16.8876274395546));
#163526=CARTESIAN_POINT('Ctrl Pts',(4.52626268731236,6.75068636347696,16.8953604810357));
#163527=CARTESIAN_POINT('Ctrl Pts',(4.35932435057244,6.85681987287155,16.9030935225168));
#163528=CARTESIAN_POINT('Ctrl Pts',(4.19240269084774,6.96294277960777,16.9108257914728));
#163529=CARTESIAN_POINT('Ctrl Pts',(4.02159456643663,7.06297243912803,16.9185580604289));
#163530=CARTESIAN_POINT('Ctrl Pts',(3.84739671419705,7.15662113612882,16.9262903293849));
#163531=CARTESIAN_POINT('Ctrl Pts',(3.67313185596631,7.25030585552416,16.9340255725931));
#163532=CARTESIAN_POINT('Ctrl Pts',(3.49547497637499,7.33760454106587,16.9417608158013));
#163533=CARTESIAN_POINT('Ctrl Pts',(3.31494707532762,7.41827563860206,16.9494960590096));
#163534=CARTESIAN_POINT('Ctrl Pts',(3.163835947401,7.48580149177516,16.9559708549785));
#163535=CARTESIAN_POINT('Ctrl Pts',(3.01071373698051,7.5486844727472,16.9624456509475));
#163536=CARTESIAN_POINT('Ctrl Pts',(2.85589627835534,7.6068090556932,16.9689204469164));
#163537=CARTESIAN_POINT('Ctrl Pts',(2.65470914632731,7.68234264374637,16.9773345214208));
#163538=CARTESIAN_POINT('Ctrl Pts',(2.4505619950606,7.74987627656709,16.9857485959252));
#163539=CARTESIAN_POINT('Ctrl Pts',(2.24409501977395,7.80920771299661,16.9941626704297));
#163540=CARTESIAN_POINT('Ctrl Pts',(2.03757038394225,7.86855571906376,17.0025790947536));
#163541=CARTESIAN_POINT('Ctrl Pts',(1.8287248845117,7.91969688292368,17.0109955190775));
#163542=CARTESIAN_POINT('Ctrl Pts',(1.61821235668358,7.96247928293547,17.0194119434014));
#163543=CARTESIAN_POINT('Ctrl Pts',(1.40764762321557,8.00527229268432,17.0278304549399));
#163544=CARTESIAN_POINT('Ctrl Pts',(1.195415294672,8.03970234764673,17.0362489664784));
#163545=CARTESIAN_POINT('Ctrl Pts',(0.982178923991239,8.06566873382284,
17.0446674780168));
#163546=CARTESIAN_POINT('Ctrl Pts',(0.768860650111411,8.0916450935794,17.0530892230704));
#163547=CARTESIAN_POINT('Ctrl Pts',(0.554537825397038,8.10915125503629,
17.061510968124));
#163548=CARTESIAN_POINT('Ctrl Pts',(0.339880079721553,8.11813827757993,
17.0699327131776));
#163549=CARTESIAN_POINT('Ctrl Pts',(0.125199065731904,8.12712627429231,
17.0783553711254));
#163550=CARTESIAN_POINT('Ctrl Pts',(-0.0898166778647321,8.12759328030146,
17.0867780290732));
#163551=CARTESIAN_POINT('Ctrl Pts',(-0.304495944304193,8.11954246139536,
17.095200687021));
#163552=CARTESIAN_POINT('Ctrl Pts',(-0.519216036560872,8.11149011145525,
17.1036249467159));
#163553=CARTESIAN_POINT('Ctrl Pts',(-0.733599260085607,8.09491671049226,
17.1120492064108));
#163554=CARTESIAN_POINT('Ctrl Pts',(-0.946976624282326,8.06987749817572,
17.1204734661057));
#163555=CARTESIAN_POINT('Ctrl Pts',(-1.00704369291895,8.06282880259132,
17.1228449481381));
#163556=CARTESIAN_POINT('Ctrl Pts',(-1.06703108059628,8.05510954281571,
17.1252164301704));
#163557=CARTESIAN_POINT('Ctrl Pts',(-1.12692394473314,8.04672169180015,
17.1275879122028));
#163558=CARTESIAN_POINT('Ctrl Pts',(-1.33968413391722,8.01692514099837,
17.1360122374229));
#163559=CARTESIAN_POINT('Ctrl Pts',(-1.55127286867005,7.97868449960255,
17.144436562643));
#163560=CARTESIAN_POINT('Ctrl Pts',(-1.76102908195827,7.93211599354152,
17.1528608878631));
#163561=CARTESIAN_POINT('Ctrl Pts',(-1.97074904680779,7.88555553508782,
17.1612837572568));
#163562=CARTESIAN_POINT('Ctrl Pts',(-2.17863686517976,7.83067014357823,
17.1697066266505));
#163563=CARTESIAN_POINT('Ctrl Pts',(-2.38404252274152,7.76762697432493,
17.1781294960442));
#163564=CARTESIAN_POINT('Ctrl Pts',(-2.58940620531185,7.70459668804924,
17.1865506442104));
#163565=CARTESIAN_POINT('Ctrl Pts',(-2.79228848781976,7.6334120304237,17.1949717923765));
#163566=CARTESIAN_POINT('Ctrl Pts',(-2.99205430072729,7.55429008074216,
17.2033929405427));
#163567=CARTESIAN_POINT('Ctrl Pts',(-3.19176406608829,7.47519033000993,
17.2118117260189));
#163568=CARTESIAN_POINT('Ctrl Pts',(-3.38835886300686,7.38815783212735,
17.220230511495));
#163569=CARTESIAN_POINT('Ctrl Pts',(-3.58122245304708,7.29345825409945,
17.2286492969712));
#163570=CARTESIAN_POINT('Ctrl Pts',(-3.77403216793572,7.19878512976414,
17.237065730716));
#163571=CARTESIAN_POINT('Ctrl Pts',(-3.96311252025934,7.09644931774732,
17.2454821644608));
#163572=CARTESIAN_POINT('Ctrl Pts',(-4.14786973175427,6.9867635032894,17.2538985982057));
#163573=CARTESIAN_POINT('Ctrl Pts',(-4.33255988712078,6.87711749840644,
17.2623119772743));
#163574=CARTESIAN_POINT('Ctrl Pts',(-4.51292980825997,6.76012695288952,
17.2707253563429));
#163575=CARTESIAN_POINT('Ctrl Pts',(-4.6884118251844,6.63614964568846,17.2791387354115));
#163576=CARTESIAN_POINT('Ctrl Pts',(-4.73789026879763,6.60119333329145,
17.2815109494374));
#163577=CARTESIAN_POINT('Ctrl Pts',(-4.78698029127896,6.56568184425487,
17.2838831634633));
#163578=CARTESIAN_POINT('Ctrl Pts',(-4.83566957250315,6.52962382898641,
17.2862553774892));
#163579=CARTESIAN_POINT('Ctrl Pts',(-4.99443290048469,6.41204783771085,
17.2939905623999));
#163580=CARTESIAN_POINT('Ctrl Pts',(-5.14900346709389,6.28860545606571,
17.3017257473106));
#163581=CARTESIAN_POINT('Ctrl Pts',(-5.29892005504036,6.15963747413686,
17.3094609322213));
#163582=CARTESIAN_POINT('Ctrl Pts',(-5.44879028507363,6.03070937229461,
17.3171937252217));
#163583=CARTESIAN_POINT('Ctrl Pts',(-5.59400913483348,5.89625930293477,
17.3249265182221));
#163584=CARTESIAN_POINT('Ctrl Pts',(-5.73414793131289,5.75666874714188,
17.3326593112225));
#163585=CARTESIAN_POINT('Ctrl Pts',(-5.87426829202127,5.61709655499695,
17.3403910869457));
#163586=CARTESIAN_POINT('Ctrl Pts',(-6.00930968090495,5.47238547321573,
17.3481228626689));
#163587=CARTESIAN_POINT('Ctrl Pts',(-6.13887971955536,5.32295438185712,
17.3558546383921));
#163588=CARTESIAN_POINT('Ctrl Pts',(-6.2684961219023,5.1734698199752,17.3635891807557));
#163589=CARTESIAN_POINT('Ctrl Pts',(-6.39263702761418,5.01926213857458,
17.3713237231193));
#163590=CARTESIAN_POINT('Ctrl Pts',(-6.51094943771995,4.86078439986328,
17.3790582654829));
#163591=CARTESIAN_POINT('Ctrl Pts',(-6.62928182947274,4.70227989602876,
17.3867941141244));
#163592=CARTESIAN_POINT('Ctrl Pts',(-6.74178355890835,4.53950418568419,
17.394529962766));
#163593=CARTESIAN_POINT('Ctrl Pts',(-6.84814446647343,4.37294007834653,
17.4022658114076));
#163594=CARTESIAN_POINT('Ctrl Pts',(-6.95459240334909,4.20623968071423,
17.4100079898708));
#163595=CARTESIAN_POINT('Ctrl Pts',(-7.05488929538259,4.03574499481885,
17.417750168334));
#163596=CARTESIAN_POINT('Ctrl Pts',(-7.14877007217295,3.86196504615259,
17.4254923467972));
#163597=CARTESIAN_POINT('Ctrl Pts',(-7.22730740136443,3.71658690270414,
17.43196917879));
#163598=CARTESIAN_POINT('Ctrl Pts',(-7.30135524443815,3.56891013651415,
17.4384460107828));
#163599=CARTESIAN_POINT('Ctrl Pts',(-7.37078419891133,3.41924375492288,
17.4449228427756));
#163600=CARTESIAN_POINT('Ctrl Pts',(-7.47152716887149,3.20207447880307,
17.4543208712471));
#163601=CARTESIAN_POINT('Ctrl Pts',(-7.56260259696826,2.98059280367584,
17.4637188997187));
#163602=CARTESIAN_POINT('Ctrl Pts',(-7.64371577516674,2.75559371297133,
17.4731169281902));
#163603=CARTESIAN_POINT('Ctrl Pts',(-7.72494437062792,2.53027446739513,
17.4825283292695));
#163604=CARTESIAN_POINT('Ctrl Pts',(-7.79618234821169,2.30142782976832,
17.4919397303489));
#163605=CARTESIAN_POINT('Ctrl Pts',(-7.85718390911585,2.06986680267859,
17.5013511314282));
#163606=CARTESIAN_POINT('Ctrl Pts',(-7.91809362187505,1.83865442979492,
17.5107483620549));
#163607=CARTESIAN_POINT('Ctrl Pts',(-7.96879771652282,1.6047358719949,17.5201455926816));
#163608=CARTESIAN_POINT('Ctrl Pts',(-8.00910145045261,1.36893444651592,
17.5295428233083));
#163609=CARTESIAN_POINT('Ctrl Pts',(-8.04930352333066,1.13372780019461,
17.5389163506139));
#163610=CARTESIAN_POINT('Ctrl Pts',(-8.07915760945394,0.896647806682439,
17.5482898779194));
#163611=CARTESIAN_POINT('Ctrl Pts',(-8.09852038546559,0.658524964369773,
17.557663405225));
#163612=CARTESIAN_POINT('Ctrl Pts',(-8.11775742074714,0.42194847780847,
17.5669760613947));
#163613=CARTESIAN_POINT('Ctrl Pts',(-8.12663893851337,0.184342685548523,
17.5762887175645));
#163614=CARTESIAN_POINT('Ctrl Pts',(-8.12507409327281,-0.0534653282699481,
17.5856013737343));
#163615=CARTESIAN_POINT('Ctrl Pts',(-8.12406650754745,-0.206587153923133,
17.5915976851769));
#163616=CARTESIAN_POINT('Ctrl Pts',(-8.11872894262562,-0.359792564339886,
17.5975939966195));
#163617=CARTESIAN_POINT('Ctrl Pts',(-8.10904828820628,-0.512858091521222,
17.6035903080621));
#163618=CARTESIAN_POINT('Ctrl Pts',(-8.09683079673091,-0.706034781082006,
17.6111579662761));
#163619=CARTESIAN_POINT('Ctrl Pts',(-8.07769740879767,-0.898911817353965,
17.6187256244901));
#163620=CARTESIAN_POINT('Ctrl Pts',(-8.0516796739349,-1.09093629091876,
17.6262932827041));
#163621=CARTESIAN_POINT('Ctrl Pts',(-8.02566914291522,-1.2829075963586,
17.6338588455696));
#163622=CARTESIAN_POINT('Ctrl Pts',(-7.99277810706042,-1.47402644483414,
17.641424408435));
#163623=CARTESIAN_POINT('Ctrl Pts',(-7.95308998041258,-1.66374497022859,
17.6489899713005));
#163624=CARTESIAN_POINT('Ctrl Pts',(-7.91340533082007,-1.8534468744856,
17.6565548713511));
#163625=CARTESIAN_POINT('Ctrl Pts',(-7.86692485180811,-2.04174834014855,
17.6641197714017));
#163626=CARTESIAN_POINT('Ctrl Pts',(-7.81378307047753,-2.22811168706119,
17.6716846714523));
#163627=CARTESIAN_POINT('Ctrl Pts',(-7.76061520748913,-2.41456649995265,
17.6792532843091));
#163628=CARTESIAN_POINT('Ctrl Pts',(-7.70077960856521,-2.59908093877052,
17.6868218971659));
#163629=CARTESIAN_POINT('Ctrl Pts',(-7.63446086414704,-2.78113194154957,
17.6943905100227));
#163630=CARTESIAN_POINT('Ctrl Pts',(-7.56812737160585,-2.96322342927155,
17.701960806006));
#163631=CARTESIAN_POINT('Ctrl Pts',(-7.49530799821113,-3.14285004816545,
17.7095311019892));
#163632=CARTESIAN_POINT('Ctrl Pts',(-7.41623541380621,-3.31950897716915,
17.7171013979725));
#163633=CARTESIAN_POINT('Ctrl Pts',(-7.33708270633128,-3.49634691202988,
17.7246793648237));
#163634=CARTESIAN_POINT('Ctrl Pts',(-7.25166428915407,-3.67021081810455,
17.7322573316749));
#163635=CARTESIAN_POINT('Ctrl Pts',(-7.16025912791398,-3.8406219266708,
17.7398352985261));
#163636=CARTESIAN_POINT('Ctrl Pts',(-7.07010610196467,-4.0086986182295,
17.7473094568003));
#163637=CARTESIAN_POINT('Ctrl Pts',(-6.97412953600833,-4.17341624939413,
17.7547836150744));
#163638=CARTESIAN_POINT('Ctrl Pts',(-6.87263762475836,-4.33434419967494,
17.7622577733485));
#163639=CARTESIAN_POINT('Ctrl Pts',(-6.76298914340258,-4.50820539845095,
17.7703326050674));
#163640=CARTESIAN_POINT('Ctrl Pts',(-6.64666942776123,-4.67801477267513,
17.7784074367863));
#163641=CARTESIAN_POINT('Ctrl Pts',(-6.52400396072606,-4.84324889747891,
17.7864822685052));
#163642=CARTESIAN_POINT('Ctrl Pts',(-6.40141964896652,-5.00837370365156,
17.7945517579284));
#163643=CARTESIAN_POINT('Ctrl Pts',(-6.27249814595655,-5.16892904292965,
17.8026212473516));
#163644=CARTESIAN_POINT('Ctrl Pts',(-6.13760819416067,-5.32442045836651,
17.8106907367748));
#163645=CARTESIAN_POINT('Ctrl Pts',(-6.00278910913358,-5.47983018369938,
17.8187559867522));
#163646=CARTESIAN_POINT('Ctrl Pts',(-5.86200803576692,-5.6301810520313,
17.8268212367296));
#163647=CARTESIAN_POINT('Ctrl Pts',(-5.71567433269601,-5.77501121081683,
17.834886486707));
#163648=CARTESIAN_POINT('Ctrl Pts',(-5.56939759429301,-5.91978499023296,
17.8429485970503));
#163649=CARTESIAN_POINT('Ctrl Pts',(-5.41757276213034,-6.0590421239127,
17.8510107073936));
#163650=CARTESIAN_POINT('Ctrl Pts',(-5.26064685945091,-6.1923567551175,
17.8590728177369));
#163651=CARTESIAN_POINT('Ctrl Pts',(-5.10376070590889,-6.3256376178908,
17.8671328859576));
#163652=CARTESIAN_POINT('Ctrl Pts',(-4.94177630046075,-6.45297877583114,
17.8751929541782));
#163653=CARTESIAN_POINT('Ctrl Pts',(-4.77517509400821,-6.57399348828881,
17.8832530223989));
#163654=CARTESIAN_POINT('Ctrl Pts',(-4.6060779530136,-6.69682118162071,
17.8914338424624));
#163655=CARTESIAN_POINT('Ctrl Pts',(-4.43222482790505,-6.81313114154238,
17.8996146625258));
#163656=CARTESIAN_POINT('Ctrl Pts',(-4.25415189119161,-6.92256305490754,
17.9077954825892));
#163657=CARTESIAN_POINT('Ctrl Pts',(-4.07869034262652,-7.03039018089239,
17.9158563332909));
#163658=CARTESIAN_POINT('Ctrl Pts',(-3.89913218443488,-7.13153945333932,
17.9239171839927));
#163659=CARTESIAN_POINT('Ctrl Pts',(-3.71601769607196,-7.225711040789,17.9319780346944));
#163660=CARTESIAN_POINT('Ctrl Pts',(-3.53287283983618,-7.31989824574017,
17.9400402222149));
#163661=CARTESIAN_POINT('Ctrl Pts',(-3.34617075889484,-7.40710531267174,
17.9481024097354));
#163662=CARTESIAN_POINT('Ctrl Pts',(-3.15647496882119,-7.48707909225655,
17.9561645972559));
#163663=CARTESIAN_POINT('Ctrl Pts',(-2.9667242194974,-7.56707604209178,
17.9642291205783));
#163664=CARTESIAN_POINT('Ctrl Pts',(-2.77397832304669,-7.63983540171236,
17.9722936439006));
#163665=CARTESIAN_POINT('Ctrl Pts',(-2.57881989454899,-7.70515253022147,
17.980358167223));
#163666=CARTESIAN_POINT('Ctrl Pts',(-2.37870002529172,-7.77213019200182,
17.9886277119479));
#163667=CARTESIAN_POINT('Ctrl Pts',(-2.17604367050982,-7.83128209833625,
17.9968972566727));
#163668=CARTESIAN_POINT('Ctrl Pts',(-1.97149434979881,-7.88244236206085,
18.0051668013976));
#163669=CARTESIAN_POINT('Ctrl Pts',(-1.77174675685978,-7.932401655485,18.0132422212902));
#163670=CARTESIAN_POINT('Ctrl Pts',(-1.57019439223873,-7.97474026313108,
18.0213176411829));
#163671=CARTESIAN_POINT('Ctrl Pts',(-1.36744602125939,-8.00935571325446,
18.0293930610755));
#163672=CARTESIAN_POINT('Ctrl Pts',(-1.15738685517106,-8.04521934338656,
18.0377596682165));
#163673=CARTESIAN_POINT('Ctrl Pts',(-0.946044203840001,-8.07279244431162,
18.0461262753574));
#163674=CARTESIAN_POINT('Ctrl Pts',(-0.734100270084997,-8.09201979458535,
18.0544928824984));
#163675=CARTESIAN_POINT('Ctrl Pts',(-0.522156336329993,-8.11124714485908,
18.0628594896394));
#163676=CARTESIAN_POINT('Ctrl Pts',(-0.309611496744794,-8.12212876252602,
18.0712260967804));
#163677=CARTESIAN_POINT('Ctrl Pts',(-0.0971476232154044,-8.12466921799304,
18.0795927039214));
#163678=CARTESIAN_POINT('Ctrl Pts',(0.107985978474591,-8.12712202453951,
18.0876706525545));
#163679=CARTESIAN_POINT('Ctrl Pts',(0.313442941770192,-8.12180438688238,
18.0957486011875));
#163680=CARTESIAN_POINT('Ctrl Pts',(0.518609289507992,-8.10868250502731,
18.1038265498206));
#163681=CARTESIAN_POINT('Ctrl Pts',(0.723524555302593,-8.09557668169076,
18.1118946126851));
#163682=CARTESIAN_POINT('Ctrl Pts',(0.928149601924156,-8.07468567214938,
18.1199626755495));
#163683=CARTESIAN_POINT('Ctrl Pts',(1.13186887190644,-8.04602761735934,
18.128030738414));
#163684=CARTESIAN_POINT('Ctrl Pts',(1.33536391130014,-8.01740110603838,
18.1360899208889));
#163685=CARTESIAN_POINT('Ctrl Pts',(1.53795485079752,-7.98102463602732,
18.1441491033638));
#163686=CARTESIAN_POINT('Ctrl Pts',(1.7390290633868,-7.9369682800926,18.1522082858387));
#163687=CARTESIAN_POINT('Ctrl Pts',(1.93984500317893,-7.892968513007,18.1602571165754));
#163688=CARTESIAN_POINT('Ctrl Pts',(2.1391477956511,-7.84130860665253,18.1683059473121));
#163689=CARTESIAN_POINT('Ctrl Pts',(2.33633279343447,-7.78211003782539,
18.1763547780488));
#163690=CARTESIAN_POINT('Ctrl Pts',(2.53336864137543,-7.72295624652854,
18.1843975206863));
#163691=CARTESIAN_POINT('Ctrl Pts',(2.72828958651205,-7.65627524909058,
18.1924402633237));
#163692=CARTESIAN_POINT('Ctrl Pts',(2.92050265501969,-7.58223923419216,
18.2004830059612));
#163693=CARTESIAN_POINT('Ctrl Pts',(3.11255915874804,-7.50826352441463,
18.208519197482));
#163694=CARTESIAN_POINT('Ctrl Pts',(3.30191189189283,-7.42694486085441,
18.2165553890029));
#163695=CARTESIAN_POINT('Ctrl Pts',(3.48798422267296,-7.33850486304155,
18.2245915805238));
#163696=CARTESIAN_POINT('Ctrl Pts',(3.59347972379901,-7.28836295397996,
18.2291477767518));
#163697=CARTESIAN_POINT('Ctrl Pts',(3.69792105796595,-7.23593284044076,
18.2337039729798));
#163698=CARTESIAN_POINT('Ctrl Pts',(3.80120582549461,-7.18126185532361,
18.2382601692078));
#163699=CARTESIAN_POINT('Ctrl Pts',(3.98338619948005,-7.08482962477197,
18.2462966837165));
#163700=CARTESIAN_POINT('Ctrl Pts',(4.16182284614464,-6.98149918834426,
18.2543331982252));
#163701=CARTESIAN_POINT('Ctrl Pts',(4.33599122287397,-6.87159862605929,
18.2623697127338));
#163702=CARTESIAN_POINT('Ctrl Pts',(4.51026481463818,-6.76163167289607,
18.2704110820972));
#163703=CARTESIAN_POINT('Ctrl Pts',(4.68026472520352,-6.64508684402324,
18.2784524514605));
#163704=CARTESIAN_POINT('Ctrl Pts',(4.84549629750284,-6.52233494949365,
18.2864938208239));
#163705=CARTESIAN_POINT('Ctrl Pts',(5.01084788878781,-6.39949389187214,
18.2945410311834));
#163706=CARTESIAN_POINT('Ctrl Pts',(5.17142397839643,-6.27043696160652,
18.302588241543));
#163707=CARTESIAN_POINT('Ctrl Pts',(5.3267633583719,-6.13557492712839,18.3106354519026));
#163708=CARTESIAN_POINT('Ctrl Pts',(5.48233169749899,-6.0005141156434,18.3186945232755));
#163709=CARTESIAN_POINT('Ctrl Pts',(5.63264766150448,-5.85963130608115,
18.3267535946485));
#163710=CARTESIAN_POINT('Ctrl Pts',(5.77728601207804,-5.7133750005708,18.3348126660214));
#163711=CARTESIAN_POINT('Ctrl Pts',(5.9220414255642,-5.56700032265755,18.3428782599961));
#163712=CARTESIAN_POINT('Ctrl Pts',(6.06110984260431,-5.41524370229707,
18.3509438539708));
#163713=CARTESIAN_POINT('Ctrl Pts',(6.19410608185046,-5.25858701642211,
18.3590094479456));
#163714=CARTESIAN_POINT('Ctrl Pts',(6.32731115557887,-5.1016843437578,18.3670877067457));
#163715=CARTESIAN_POINT('Ctrl Pts',(6.45442479817904,-4.93986647417383,
18.3751659655457));
#163716=CARTESIAN_POINT('Ctrl Pts',(6.57510391216856,-4.77364599721069,
18.3832442243458));
#163717=CARTESIAN_POINT('Ctrl Pts',(6.64324160759418,-4.67979479248775,
18.3878053610619));
#163718=CARTESIAN_POINT('Ctrl Pts',(6.70932882071092,-4.5845405536798,18.3923664977781));
#163719=CARTESIAN_POINT('Ctrl Pts',(6.77331025023357,-4.4879790347751,18.3969276344942));
#163720=CARTESIAN_POINT('Ctrl Pts',(6.88817556936919,-4.31462295680121,
18.4051162046533));
#163721=CARTESIAN_POINT('Ctrl Pts',(6.99647176939325,-4.1367191744666,18.4133047748123));
#163722=CARTESIAN_POINT('Ctrl Pts',(7.0978411999887,-3.95478670249648,18.4214933449713));
#163723=CARTESIAN_POINT('Ctrl Pts',(7.1991119185707,-3.77303139360711,18.429673941225));
#163724=CARTESIAN_POINT('Ctrl Pts',(7.2934691728929,-3.58725548170466,18.4378545374786));
#163725=CARTESIAN_POINT('Ctrl Pts',(7.380598997499,-3.39800618019107,18.4460351337322));
#163726=CARTESIAN_POINT('Ctrl Pts',(7.4676520891475,-3.20892354558741,18.4542085255487));
#163727=CARTESIAN_POINT('Ctrl Pts',(7.5474903194604,-3.01637389587714,18.4623819173652));
#163728=CARTESIAN_POINT('Ctrl Pts',(7.61984564791169,-2.82092890100074,
18.4705553091817));
#163729=CARTESIAN_POINT('Ctrl Pts',(7.6921439731308,-2.62563788229526,18.4787222618076));
#163730=CARTESIAN_POINT('Ctrl Pts',(7.75697105008127,-2.42745635098308,
18.4868892144335));
#163731=CARTESIAN_POINT('Ctrl Pts',(7.81410667775081,-2.22697651339886,
18.4950561670594));
#163732=CARTESIAN_POINT('Ctrl Pts',(7.87119180948338,-2.02667385803275,
18.5032159018084));
#163733=CARTESIAN_POINT('Ctrl Pts',(7.92059897554161,-1.82407724048578,
18.5113756365574));
#163734=CARTESIAN_POINT('Ctrl Pts',(7.96215748145354,-1.61979498796403,
18.5195353713064));
#163735=CARTESIAN_POINT('Ctrl Pts',(8.00369332716982,-1.41562412240651,
18.5276906568776));
#163736=CARTESIAN_POINT('Ctrl Pts',(8.03738898762161,-1.20976975079092,
18.5358459424487));
#163737=CARTESIAN_POINT('Ctrl Pts',(8.06312434927614,-1.00285257670819,
18.5440012280198));
#163738=CARTESIAN_POINT('Ctrl Pts',(8.08884554679798,-0.796049284930593,
18.5521520251152));
#163739=CARTESIAN_POINT('Ctrl Pts',(8.10661515075115,-0.588184657728283,
18.5603028222105));
#163740=CARTESIAN_POINT('Ctrl Pts',(8.1163645301893,-0.379887319589674,
18.5684536193059));
#163741=CARTESIAN_POINT('Ctrl Pts',(8.12228289088803,-0.253440422378366,
18.5734015606081));
#163742=CARTESIAN_POINT('Ctrl Pts',(8.12524672091287,-0.12683422128016,
18.5783495019102));
#163743=CARTESIAN_POINT('Ctrl Pts',(8.12524999728006,-0.000210239024478989,
18.5832974432124));
#163744=CARTESIAN_POINT('',(8.13282513948647,0.00629553435497102,20.5832974432124));
#163745=CARTESIAN_POINT('Ctrl Pts',(8.12524999728007,-0.000210238467663868,
18.5832974432342));
#163746=CARTESIAN_POINT('Ctrl Pts',(8.12525592540781,0.22889873702772,18.5922500740262));
#163747=CARTESIAN_POINT('Ctrl Pts',(8.11556726318553,0.457755304909344,
18.6012027048182));
#163748=CARTESIAN_POINT('Ctrl Pts',(8.09627343309599,0.685597592647516,
18.6101553356103));
#163749=CARTESIAN_POINT('Ctrl Pts',(8.07688960545325,0.914502668246784,
18.6191497266367));
#163750=CARTESIAN_POINT('Ctrl Pts',(8.04781084098892,1.14238383675527,18.6281441176631));
#163751=CARTESIAN_POINT('Ctrl Pts',(8.00917884981307,1.36848153593939,18.6371385086895));
#163752=CARTESIAN_POINT('Ctrl Pts',(7.97047456489684,1.5950023416698,18.6461497313145));
#163753=CARTESIAN_POINT('Ctrl Pts',(7.9221813288671,1.81973286353389,18.6551609539395));
#163754=CARTESIAN_POINT('Ctrl Pts',(7.86449187315936,2.04192437164316,18.6641721765645));
#163755=CARTESIAN_POINT('Ctrl Pts',(7.80669877566234,2.2645150571269,18.6731995882699));
#163756=CARTESIAN_POINT('Ctrl Pts',(7.73947572271128,2.48455746566079,18.6822269999754));
#163757=CARTESIAN_POINT('Ctrl Pts',(7.66306594241722,2.70131596165003,18.6912544116808));
#163758=CARTESIAN_POINT('Ctrl Pts',(7.59815077062031,2.88546666790035,18.6989237961429));
#163759=CARTESIAN_POINT('Ctrl Pts',(7.52660580849166,3.06724741300914,18.7065931806049));
#163760=CARTESIAN_POINT('Ctrl Pts',(7.44860772744946,3.24621787393887,18.714262565067));
#163761=CARTESIAN_POINT('Ctrl Pts',(7.37153654171261,3.42306152767263,18.7218408098965));
#163762=CARTESIAN_POINT('Ctrl Pts',(7.28805534919494,3.59740693234696,18.7294190547259));
#163763=CARTESIAN_POINT('Ctrl Pts',(7.19835504487957,3.76873615557747,18.7369972995554));
#163764=CARTESIAN_POINT('Ctrl Pts',(7.10872148891895,3.93993788822854,18.7445699052136));
#163765=CARTESIAN_POINT('Ctrl Pts',(7.0128781968328,4.10812758098797,18.7521425108718));
#163766=CARTESIAN_POINT('Ctrl Pts',(6.91106436292493,4.27280668109488,18.7597151165301));
#163767=CARTESIAN_POINT('Ctrl Pts',(6.80930695719371,4.43739451127317,18.7672835252308));
#163768=CARTESIAN_POINT('Ctrl Pts',(6.70158578678349,4.59847530888974,18.7748519339316));
#163769=CARTESIAN_POINT('Ctrl Pts',(6.58818620684434,4.75557463052006,18.7824203426324));
#163770=CARTESIAN_POINT('Ctrl Pts',(6.4748140251489,4.91263599570024,18.7899869227452));
#163771=CARTESIAN_POINT('Ctrl Pts',(6.35576637298534,5.06571749724551,18.797553502858));
#163772=CARTESIAN_POINT('Ctrl Pts',(6.2313722770221,5.21437312700774,18.8051200829708));
#163773=CARTESIAN_POINT('Ctrl Pts',(6.10700024800852,5.363002385934,18.8126853208065));
#163774=CARTESIAN_POINT('Ctrl Pts',(5.97728390138052,5.50720705583517,18.8202505586423));
#163775=CARTESIAN_POINT('Ctrl Pts',(5.84259276800369,5.64657394441718,18.827815796478));
#163776=CARTESIAN_POINT('Ctrl Pts',(5.70785479605658,5.78598929755392,18.83538366511));
#163777=CARTESIAN_POINT('Ctrl Pts',(5.56813883473249,5.92056324141084,18.8429515337419));
#163778=CARTESIAN_POINT('Ctrl Pts',(5.42385185756968,6.04991889116193,18.8505194023739));
#163779=CARTESIAN_POINT('Ctrl Pts',(5.28142682683539,6.17760527529528,18.8579896117004));
#163780=CARTESIAN_POINT('Ctrl Pts',(5.13454833590424,6.30020704009739,18.865459821027));
#163781=CARTESIAN_POINT('Ctrl Pts',(4.98363930632379,6.4174003168701,18.8729300303535));
#163782=CARTESIAN_POINT('Ctrl Pts',(4.79564785384241,6.56339114580067,18.8822358717968));
#163783=CARTESIAN_POINT('Ctrl Pts',(4.60149533023253,6.70091893766865,18.8915417132401));
#163784=CARTESIAN_POINT('Ctrl Pts',(4.40190335348933,6.82956326781145,18.9008475546834));
#163785=CARTESIAN_POINT('Ctrl Pts',(4.20123980769149,6.95889826340827,18.9102033573119));
#163786=CARTESIAN_POINT('Ctrl Pts',(3.99507831279999,7.07925417467187,18.9195591599404));
#163787=CARTESIAN_POINT('Ctrl Pts',(3.78417060822886,7.19025315064197,18.9289149625689));
#163788=CARTESIAN_POINT('Ctrl Pts',(3.5722390616589,7.30179096616588,18.9383161825219));
#163789=CARTESIAN_POINT('Ctrl Pts',(3.35551516149101,7.40388078177639,18.9477174024749));
#163790=CARTESIAN_POINT('Ctrl Pts',(3.1347793400703,7.49618876840548,18.9571186224279));
#163791=CARTESIAN_POINT('Ctrl Pts',(2.91380461698811,7.58859665966822,18.9665300172908));
#163792=CARTESIAN_POINT('Ctrl Pts',(2.6888093259892,7.67120154176815,18.9759414121536));
#163793=CARTESIAN_POINT('Ctrl Pts',(2.46059342949554,7.74371794019019,18.9853528070164));
#163794=CARTESIAN_POINT('Ctrl Pts',(2.23264523407621,7.8161492756606,18.9947531621551));
#163795=CARTESIAN_POINT('Ctrl Pts',(2.00148402037825,7.87851577453662,19.0041535172939));
#163796=CARTESIAN_POINT('Ctrl Pts',(1.76792329316785,7.93058224797994,19.0135538724327));
#163797=CARTESIAN_POINT('Ctrl Pts',(1.61848632347989,7.96389545138806,19.0195684135018));
#163798=CARTESIAN_POINT('Ctrl Pts',(1.46806739129636,7.99299311936093,19.0255829545708));
#163799=CARTESIAN_POINT('Ctrl Pts',(1.31688299790545,8.01782431413457,19.0315974956399));
#163800=CARTESIAN_POINT('Ctrl Pts',(1.12226886331984,8.0497886020694,19.0393397941592));
#163801=CARTESIAN_POINT('Ctrl Pts',(0.926294388794416,8.07469507653537,
19.0470820926784));
#163802=CARTESIAN_POINT('Ctrl Pts',(0.729521306748375,8.09243388761998,
19.0548243911977));
#163803=CARTESIAN_POINT('Ctrl Pts',(0.532870796514254,8.11016164903156,
19.0625618669661));
#163804=CARTESIAN_POINT('Ctrl Pts',(0.335423019633146,8.12073060539961,
19.0702993427345));
#163805=CARTESIAN_POINT('Ctrl Pts',(0.137748106460787,8.12408228796745,
19.0780368185028));
#163806=CARTESIAN_POINT('Ctrl Pts',(-0.0598388056572187,8.12743247843093,
19.0857708496964));
#163807=CARTESIAN_POINT('Ctrl Pts',(-0.257652300201885,8.12357178815811,
19.09350488089));
#163808=CARTESIAN_POINT('Ctrl Pts',(-0.455118801602479,8.11249372504706,
19.1012389120836));
#163809=CARTESIAN_POINT('Ctrl Pts',(-0.652560033508927,8.10141707957925,
19.1089719535647));
#163810=CARTESIAN_POINT('Ctrl Pts',(-0.849654007780657,8.08312491303037,
19.1167049950458));
#163811=CARTESIAN_POINT('Ctrl Pts',(-1.04582845265743,8.05766283795197,
19.1244380365269));
#163812=CARTESIAN_POINT('Ctrl Pts',(-1.24198329985284,8.03220330651596,
19.1321703054829));
#163813=CARTESIAN_POINT('Ctrl Pts',(-1.4372184506385,7.9995753423428,19.1399025744389));
#163814=CARTESIAN_POINT('Ctrl Pts',(-1.63096817213315,7.95987627943982,
19.1476348433949));
#163815=CARTESIAN_POINT('Ctrl Pts',(-1.8247924203341,7.92016194611281,19.1553700866032));
#163816=CARTESIAN_POINT('Ctrl Pts',(-2.01712975118378,7.87337115081103,
19.1631053298114));
#163817=CARTESIAN_POINT('Ctrl Pts',(-2.20742537649299,7.8196522153939,19.1708405730196));
#163818=CARTESIAN_POINT('Ctrl Pts',(-2.36671259145059,7.77468670660105,
19.1773153689885));
#163819=CARTESIAN_POINT('Ctrl Pts',(-2.52456938131791,7.72486788974736,
19.1837901649575));
#163820=CARTESIAN_POINT('Ctrl Pts',(-2.68067922985854,7.67030940895509,
19.1902649609264));
#163821=CARTESIAN_POINT('Ctrl Pts',(-2.88354583797946,7.59941001313845,
19.1986790354308));
#163822=CARTESIAN_POINT('Ctrl Pts',(-3.08355983584028,7.52047173603659,
19.2070931099352));
#163823=CARTESIAN_POINT('Ctrl Pts',(-3.28010010219494,7.4337494497784,19.2155071844396));
#163824=CARTESIAN_POINT('Ctrl Pts',(-3.47669525683877,7.34700294437157,
19.2239236087635));
#163825=CARTESIAN_POINT('Ctrl Pts',(-3.66981450173128,7.25246819665597,
19.2323400330874));
#163826=CARTESIAN_POINT('Ctrl Pts',(-3.85885848100777,7.15044745355523,
19.2407564574114));
#163827=CARTESIAN_POINT('Ctrl Pts',(-4.04794934187362,7.0484014100212,19.2491749689499));
#163828=CARTESIAN_POINT('Ctrl Pts',(-4.23296268720622,6.9388657901859,19.2575934804884));
#163829=CARTESIAN_POINT('Ctrl Pts',(-4.41332450707338,6.82218838480479,
19.2660119920269));
#163830=CARTESIAN_POINT('Ctrl Pts',(-4.59375560316165,6.70546616412,19.2744337370805));
#163831=CARTESIAN_POINT('Ctrl Pts',(-4.76953138108732,6.58159681852937,
19.282855482134));
#163832=CARTESIAN_POINT('Ctrl Pts',(-4.94010633476706,6.45097178444413,
19.2912772271876));
#163833=CARTESIAN_POINT('Ctrl Pts',(-5.11069977830508,6.3203325909626,19.2996998851353));
#163834=CARTESIAN_POINT('Ctrl Pts',(-5.27609106428128,6.1829364097518,19.3081225430831));
#163835=CARTESIAN_POINT('Ctrl Pts',(-5.43576685901174,6.03921569551624,
19.3165452010308));
#163836=CARTESIAN_POINT('Ctrl Pts',(-5.59547301948438,5.89546764973576,
19.3249694607257));
#163837=CARTESIAN_POINT('Ctrl Pts',(-5.74946132117493,5.74539284475124,
19.3333937204206));
#163838=CARTESIAN_POINT('Ctrl Pts',(-5.8972534943276,5.58946229848103,19.3418179801156));
#163839=CARTESIAN_POINT('Ctrl Pts',(-5.93885791962491,5.54556687001903,
19.344189462148));
#163840=CARTESIAN_POINT('Ctrl Pts',(-5.97997155248067,5.50120762244448,
19.3465609441804));
#163841=CARTESIAN_POINT('Ctrl Pts',(-6.02058426057031,5.45639557985608,
19.3489324262128));
#163842=CARTESIAN_POINT('Ctrl Pts',(-6.16485466040496,5.29720769001222,
19.3573567514329));
#163843=CARTESIAN_POINT('Ctrl Pts',(-6.30281570137254,5.13228682867604,
19.365781076653));
#163844=CARTESIAN_POINT('Ctrl Pts',(-6.43403426978162,4.96214576345513,
19.3742054018731));
#163845=CARTESIAN_POINT('Ctrl Pts',(-6.56523016201678,4.79203410069175,
19.3826282712668));
#163846=CARTESIAN_POINT('Ctrl Pts',(-6.68968574781638,4.6167042447302,19.3910511406605));
#163847=CARTESIAN_POINT('Ctrl Pts',(-6.80700902898126,4.43670098630363,
19.3994740100541));
#163848=CARTESIAN_POINT('Ctrl Pts',(-6.92430833493756,4.25673451184374,
19.4078951582203));
#163849=CARTESIAN_POINT('Ctrl Pts',(-7.03447810275593,4.072096763005,19.4163163063866));
#163850=CARTESIAN_POINT('Ctrl Pts',(-7.13716979400008,3.88336128812564,
19.4247374545528));
#163851=CARTESIAN_POINT('Ctrl Pts',(-7.23983267342025,3.69467876605302,
19.4331562400289));
#163852=CARTESIAN_POINT('Ctrl Pts',(-7.33502154067406,3.50190104583061,
19.4415750255051));
#163853=CARTESIAN_POINT('Ctrl Pts',(-7.42243344493677,3.30562691754288,
19.4499938109812));
#163854=CARTESIAN_POINT('Ctrl Pts',(-7.50982093126933,3.10940761711866,
19.458410244726));
#163855=CARTESIAN_POINT('Ctrl Pts',(-7.58943568483281,2.90969409962262,
19.4668266784708));
#163856=CARTESIAN_POINT('Ctrl Pts',(-7.66102212334421,2.7071068667732,19.4752431122157));
#163857=CARTESIAN_POINT('Ctrl Pts',(-7.73258258014016,2.50459316131174,
19.4836564912843));
#163858=CARTESIAN_POINT('Ctrl Pts',(-7.79612045284465,2.29920807196793,
19.492069870353));
#163859=CARTESIAN_POINT('Ctrl Pts',(-7.85142909578997,2.09158999717502,
19.5004832494216));
#163860=CARTESIAN_POINT('Ctrl Pts',(-7.86702377391825,2.03305055600291,
19.5028554634475));
#163861=CARTESIAN_POINT('Ctrl Pts',(-7.88196453026747,1.97433369334482,
19.5052276774733));
#163862=CARTESIAN_POINT('Ctrl Pts',(-7.89624744735517,1.91545394427456,
19.5075998914992));
#163863=CARTESIAN_POINT('Ctrl Pts',(-7.94282039715334,1.72346209969962,
19.5153350764099));
#163864=CARTESIAN_POINT('Ctrl Pts',(-7.98241564907852,1.52965214723825,
19.5230702613206));
#163865=CARTESIAN_POINT('Ctrl Pts',(-8.01489740902469,1.3345812396813,19.5308054462313));
#163866=CARTESIAN_POINT('Ctrl Pts',(-8.04736912480807,1.13957065286909,
19.5385382392317));
#163867=CARTESIAN_POINT('Ctrl Pts',(-8.07273167110675,0.943300235532242,
19.5462710322321));
#163868=CARTESIAN_POINT('Ctrl Pts',(-8.09090031138873,0.746337533338505,
19.5540038252324));
#163869=CARTESIAN_POINT('Ctrl Pts',(-8.1090665615195,0.549400742309951,
19.5617356009556));
#163870=CARTESIAN_POINT('Ctrl Pts',(-8.12004075901487,0.351772199607964,
19.5694673766787));
#163871=CARTESIAN_POINT('Ctrl Pts',(-8.1237899953504,0.154024913389804,
19.5771991524018));
#163872=CARTESIAN_POINT('Ctrl Pts',(-8.12754057326508,-0.0437931322072041,
19.5849336947655));
#163873=CARTESIAN_POINT('Ctrl Pts',(-8.12406101389956,-0.241729652689559,
19.5926682371291));
#163874=CARTESIAN_POINT('Ctrl Pts',(-8.1133705443868,-0.439210623706513,
19.6004027794927));
#163875=CARTESIAN_POINT('Ctrl Pts',(-8.10267826937293,-0.636724947057523,
19.6081386281343));
#163876=CARTESIAN_POINT('Ctrl Pts',(-8.08477268431997,-0.833783215161422,
19.6158744767758));
#163877=CARTESIAN_POINT('Ctrl Pts',(-8.05972496735744,-1.02981600932158,
19.6236103254174));
#163878=CARTESIAN_POINT('Ctrl Pts',(-8.03465675521876,-1.22600920639016,
19.6313525038806));
#163879=CARTESIAN_POINT('Ctrl Pts',(-8.00243478745337,-1.42117490333365,
19.6390946823438));
#163880=CARTESIAN_POINT('Ctrl Pts',(-7.96318165813537,-1.6147524398608,
19.646836860807));
#163881=CARTESIAN_POINT('Ctrl Pts',(-7.93034388192087,-1.77669254336533,
19.6533136927999));
#163882=CARTESIAN_POINT('Ctrl Pts',(-7.89258635038262,-1.93752126949681,
19.6597905247928));
#163883=CARTESIAN_POINT('Ctrl Pts',(-7.85000767911045,-2.09691845344709,
19.6662673567857));
#163884=CARTESIAN_POINT('Ctrl Pts',(-7.7882250722227,-2.32820734200977,
19.6756653852572));
#163885=CARTESIAN_POINT('Ctrl Pts',(-7.71625675473131,-2.55661361884394,
19.6850634137287));
#163886=CARTESIAN_POINT('Ctrl Pts',(-7.63438577001621,-2.78133807313565,
19.6944614422002));
#163887=CARTESIAN_POINT('Ctrl Pts',(-7.55239828974155,-3.00638229151891,
19.7038728432797));
#163888=CARTESIAN_POINT('Ctrl Pts',(-7.46047996925675,-3.22773417284017,
19.7132842443592));
#163889=CARTESIAN_POINT('Ctrl Pts',(-7.3589629495185,-3.44461200574374,
19.7226956454386));
#163890=CARTESIAN_POINT('Ctrl Pts',(-7.25759878078772,-3.66116329246478,
19.7320928760653));
#163891=CARTESIAN_POINT('Ctrl Pts',(-7.1466648168046,-3.87325396301017,
19.741490106692));
#163892=CARTESIAN_POINT('Ctrl Pts',(-7.02653900850146,-4.08012709661198,
19.7508873373187));
#163893=CARTESIAN_POINT('Ctrl Pts',(-6.90671620229702,-4.2864784190016,
19.7602608646244));
#163894=CARTESIAN_POINT('Ctrl Pts',(-6.77774786475057,-4.48763844906163,
19.76963439193));
#163895=CARTESIAN_POINT('Ctrl Pts',(-6.64005602798172,-4.68287769515323,
19.7790079192357));
#163896=CARTESIAN_POINT('Ctrl Pts',(-6.50325835391401,-4.87684906904738,
19.7883205754055));
#163897=CARTESIAN_POINT('Ctrl Pts',(-6.35785012077209,-5.06497625902391,
19.7976332315753));
#163898=CARTESIAN_POINT('Ctrl Pts',(-6.20429146649526,-5.24656601609797,
19.8069458877452));
#163899=CARTESIAN_POINT('Ctrl Pts',(-6.10541682762634,-5.36348955738288,
19.8129421991875));
#163900=CARTESIAN_POINT('Ctrl Pts',(-6.0031640198267,-5.47770317598873,
19.8189385106297));
#163901=CARTESIAN_POINT('Ctrl Pts',(-5.89766614670997,-5.58902689065379,
19.824934822072));
#163902=CARTESIAN_POINT('Ctrl Pts',(-5.76452232092045,-5.72952323274787,
19.832502480286));
#163903=CARTESIAN_POINT('Ctrl Pts',(-5.62626035307251,-5.86535866958873,
19.8400701385));
#163904=CARTESIAN_POINT('Ctrl Pts',(-5.48325870140168,-5.9961288825377,
19.8476377967141));
#163905=CARTESIAN_POINT('Ctrl Pts',(-5.3402966443179,-6.12686288756515,
19.8552033595795));
#163906=CARTESIAN_POINT('Ctrl Pts',(-5.19259778567835,-6.25253421141723,
19.862768922445));
#163907=CARTESIAN_POINT('Ctrl Pts',(-5.04057717490936,-6.3727756359598,
19.8703344853105));
#163908=CARTESIAN_POINT('Ctrl Pts',(-4.88856988258483,-6.49300652621542,
19.877899385361));
#163909=CARTESIAN_POINT('Ctrl Pts',(-4.73224188063717,-6.60780823659695,
19.8854642854116));
#163910=CARTESIAN_POINT('Ctrl Pts',(-4.57204093794369,-6.71685411664322,
19.8930291854621));
#163911=CARTESIAN_POINT('Ctrl Pts',(-4.41176136961659,-6.82595351573418,
19.9005977983189));
#163912=CARTESIAN_POINT('Ctrl Pts',(-4.24760536564726,-6.92929123097728,
19.9081664111757));
#163913=CARTESIAN_POINT('Ctrl Pts',(-4.08004976876579,-7.02658391018667,
19.9157350240325));
#163914=CARTESIAN_POINT('Ctrl Pts',(-3.91245691046559,-7.12389822557729,
19.9233053200157));
#163915=CARTESIAN_POINT('Ctrl Pts',(-3.74146327695546,-7.21516465234817,
19.9308756159989));
#163916=CARTESIAN_POINT('Ctrl Pts',(-3.56756965920367,-7.30014618273014,
19.9384459119822));
#163917=CARTESIAN_POINT('Ctrl Pts',(-3.39349983764244,-7.38521382362943,
19.9460238788334));
#163918=CARTESIAN_POINT('Ctrl Pts',(-3.21652449632797,-7.46398369347404,
19.9536018456846));
#163919=CARTESIAN_POINT('Ctrl Pts',(-3.03716456310491,-7.53626691267764,
19.9611798125359));
#163920=CARTESIAN_POINT('Ctrl Pts',(-2.86026163448587,-7.60755994305152,
19.9686539708101));
#163921=CARTESIAN_POINT('Ctrl Pts',(-2.68103936948266,-7.67254285586047,
19.9761281290843));
#163922=CARTESIAN_POINT('Ctrl Pts',(-2.50001029116415,-7.73108246667783,
19.9836022873585));
#163923=CARTESIAN_POINT('Ctrl Pts',(-2.30443250300125,-7.79432671290568,
19.9916771190774));
#163924=CARTESIAN_POINT('Ctrl Pts',(-2.10632834216557,-7.85018583285089,
19.9997519507963));
#163925=CARTESIAN_POINT('Ctrl Pts',(-1.90628306307884,-7.89846646165689,
20.0078267825152));
#163926=CARTESIAN_POINT('Ctrl Pts',(-1.70637013362725,-7.94671514807647,
20.0158962719384));
#163927=CARTESIAN_POINT('Ctrl Pts',(-1.50451895381468,-7.98739526751259,
20.0239657613616));
#163928=CARTESIAN_POINT('Ctrl Pts',(-1.30132943440447,-8.02036341231821,
20.0320352507848));
#163929=CARTESIAN_POINT('Ctrl Pts',(-1.09824666412182,-8.05331423673887,
20.0401005007622));
#163930=CARTESIAN_POINT('Ctrl Pts',(-0.893827268475251,-8.07856111595242,
20.0481657507397));
#163931=CARTESIAN_POINT('Ctrl Pts',(-0.688681455135274,-8.09601169810498,
20.0562310007171));
#163932=CARTESIAN_POINT('Ctrl Pts',(-0.483615500793642,-8.11345548710887,
20.0642931110604));
#163933=CARTESIAN_POINT('Ctrl Pts',(-0.277824007947301,-8.12310900535834,
20.0723552214037));
#163934=CARTESIAN_POINT('Ctrl Pts',(-0.0719230421407833,-8.12493166977478,
20.0804173317471));
#163935=CARTESIAN_POINT('Ctrl Pts',(0.13392576920437,-8.12675387251257,
20.0884773999678));
#163936=CARTESIAN_POINT('Ctrl Pts',(0.33988368171443,-8.12074917529332,
20.0965374681885));
#163937=CARTESIAN_POINT('Ctrl Pts',(0.545333256425216,-8.10692908578437,
20.1045975364092));
#163938=CARTESIAN_POINT('Ctrl Pts',(0.753860772172276,-8.09290195072333,
20.1127783564726));
#163939=CARTESIAN_POINT('Ctrl Pts',(0.961864263866713,-8.07082337898981,
20.120959176536));
#163940=CARTESIAN_POINT('Ctrl Pts',(1.16870120791535,-8.0407602283066,20.1291399965995));
#163941=CARTESIAN_POINT('Ctrl Pts',(1.37250494796214,-8.01113794503893,
20.1372008473012));
#163942=CARTESIAN_POINT('Ctrl Pts',(1.57517580240228,-7.9737637259802,20.1452616980029));
#163943=CARTESIAN_POINT('Ctrl Pts',(1.7761068432484,-7.92875349874532,20.1533225487046));
#163944=CARTESIAN_POINT('Ctrl Pts',(1.97707120668057,-7.88373580697354,
20.1613847362251));
#163945=CARTESIAN_POINT('Ctrl Pts',(2.17629487176969,-7.831079650457,20.1694469237456));
#163946=CARTESIAN_POINT('Ctrl Pts',(2.37318297748875,-7.77095168675354,
20.1775091112661));
#163947=CARTESIAN_POINT('Ctrl Pts',(2.57012812623594,-7.71080630259132,
20.1855736345884));
#163948=CARTESIAN_POINT('Ctrl Pts',(2.76473606299467,-7.64318488615618,
20.1936381579107));
#163949=CARTESIAN_POINT('Ctrl Pts',(2.95642833990572,-7.5683035769915,20.201702681233));
#163950=CARTESIAN_POINT('Ctrl Pts',(3.15299393888453,-7.49151858791704,
20.2099722259579));
#163951=CARTESIAN_POINT('Ctrl Pts',(3.34649333758662,-7.40709981714679,
20.2182417706827));
#163952=CARTESIAN_POINT('Ctrl Pts',(3.53632615328153,-7.31533217975213,
20.2265113154076));
#163953=CARTESIAN_POINT('Ctrl Pts',(3.72170270630046,-7.22571875734863,
20.2345867353002));
#163954=CARTESIAN_POINT('Ctrl Pts',(3.90358262151928,-7.12909779781385,
20.2426621551928));
#163955=CARTESIAN_POINT('Ctrl Pts',(4.08143282956132,-7.02578064134364,
20.2507375750854));
#163956=CARTESIAN_POINT('Ctrl Pts',(4.26569604316778,-6.91873802676664,
20.2591041822264));
#163957=CARTESIAN_POINT('Ctrl Pts',(4.44563321745642,-6.80450753401025,
20.2674707893673));
#163958=CARTESIAN_POINT('Ctrl Pts',(4.62068516870312,-6.68348383212132,
20.2758373965083));
#163959=CARTESIAN_POINT('Ctrl Pts',(4.79573711994984,-6.56246013023236,
20.2842040036493));
#163960=CARTESIAN_POINT('Ctrl Pts',(4.96590357056133,-6.43464347433915,
20.2925706107903));
#163961=CARTESIAN_POINT('Ctrl Pts',(5.13066389792557,-6.3004742304864,20.3009372179313));
#163962=CARTESIAN_POINT('Ctrl Pts',(5.28973978601087,-6.17093399491485,
20.3090151665644));
#163963=CARTESIAN_POINT('Ctrl Pts',(5.44408564280906,-6.03522033485833,
20.3170931151974));
#163964=CARTESIAN_POINT('Ctrl Pts',(5.59320839334807,-5.893700656725,20.3251710638305));
#163965=CARTESIAN_POINT('Ctrl Pts',(5.74214864792508,-5.75235416993711,
20.3332391266949));
#163966=CARTESIAN_POINT('Ctrl Pts',(5.88587831053196,-5.60521604411245,
20.3413071895594));
#163967=CARTESIAN_POINT('Ctrl Pts',(6.02393636997626,-5.45269457910281,
20.3493752524238));
#163968=CARTESIAN_POINT('Ctrl Pts',(6.16184247109141,-5.30034099206478,
20.3574344348987));
#163969=CARTESIAN_POINT('Ctrl Pts',(6.29408920336521,-5.14261611089609,
20.3654936173736));
#163970=CARTESIAN_POINT('Ctrl Pts',(6.42025107695133,-4.97996623195432,
20.3735527998484));
#163971=CARTESIAN_POINT('Ctrl Pts',(6.54625090002091,-4.8175252710965,20.3816016305851));
#163972=CARTESIAN_POINT('Ctrl Pts',(6.66618126400666,-4.65017218087765,
20.3896504613218));
#163973=CARTESIAN_POINT('Ctrl Pts',(6.77965573911101,-4.47838761404583,
20.3976992920585));
#163974=CARTESIAN_POINT('Ctrl Pts',(6.89304438263525,-4.30673298428397,
20.405742034696));
#163975=CARTESIAN_POINT('Ctrl Pts',(6.99998669746815,-4.13065382148837,
20.4137847773335));
#163976=CARTESIAN_POINT('Ctrl Pts',(7.10013770665113,-3.95066223677636,
20.421827519971));
#163977=CARTESIAN_POINT('Ctrl Pts',(7.20020713906716,-3.7708172619855,20.4298637114919));
#163978=CARTESIAN_POINT('Ctrl Pts',(7.29349614738342,-3.58706649730646,
20.4378999030128));
#163979=CARTESIAN_POINT('Ctrl Pts',(7.37970397129483,-3.39994953764837,
20.4459360945336));
#163980=CARTESIAN_POINT('Ctrl Pts',(7.4285803278516,-3.29386177411235,20.4504922907617));
#163981=CARTESIAN_POINT('Ctrl Pts',(7.47518128976442,-3.18669247143071,
20.4550484869897));
#163982=CARTESIAN_POINT('Ctrl Pts',(7.51945855803589,-3.07854357716125,
20.4596046832177));
#163983=CARTESIAN_POINT('Ctrl Pts',(7.59483891164273,-2.89442422629621,
20.4673614328136));
#163984=CARTESIAN_POINT('Ctrl Pts',(7.66344208910574,-2.70756079826281,
20.4751181824095));
#163985=CARTESIAN_POINT('Ctrl Pts',(7.72507857473524,-2.5185012560383,20.4828749320054));
#163986=CARTESIAN_POINT('Ctrl Pts',(7.78673278871381,-2.32938733508789,
20.4906339126559));
#163987=CARTESIAN_POINT('Ctrl Pts',(7.84141621163983,-2.13807637330443,
20.4983928933064));
#163988=CARTESIAN_POINT('Ctrl Pts',(7.88898940919516,-1.94513075758588,
20.5061518739568));
#163989=CARTESIAN_POINT('Ctrl Pts',(7.936605053796,-1.75201298670952,20.513917777535));
#163990=CARTESIAN_POINT('Ctrl Pts',(7.97709772009937,-1.5572579879613,20.5216836811131));
#163991=CARTESIAN_POINT('Ctrl Pts',(8.01037906330588,-1.36143851298943,
20.5294495846912));
#163992=CARTESIAN_POINT('Ctrl Pts',(8.04367786171188,-1.16551633579244,
20.537219561284));
#163993=CARTESIAN_POINT('Ctrl Pts',(8.06975775261683,-0.968528914529841,
20.5449895378767));
#163994=CARTESIAN_POINT('Ctrl Pts',(8.08858232180068,-0.771053555827045,
20.5527595144694));
#163995=CARTESIAN_POINT('Ctrl Pts',(8.10742814851175,-0.573355199308356,
20.5605382652597));
#163996=CARTESIAN_POINT('Ctrl Pts',(8.1190022729157,-0.3751681520917,20.5683170160499));
#163997=CARTESIAN_POINT('Ctrl Pts',(8.1233203645512,-0.177070091680339,
20.5760957668402));
#163998=CARTESIAN_POINT('Ctrl Pts',(8.12465294777881,-0.115936105881015,
20.5784963256309));
#163999=CARTESIAN_POINT('Ctrl Pts',(8.12529486266356,-0.0548105630326315,
20.5808968844217));
#164000=CARTESIAN_POINT('Ctrl Pts',(8.12524756561721,0.0062896686347757,
20.5832974432124));
#164001=CARTESIAN_POINT('',(8.12952934429449,-0.00742862902943328,22.5832974432124));
#164002=CARTESIAN_POINT('Ctrl Pts',(8.13282513948647,0.00629553435497102,
20.5832974432124));
#164003=CARTESIAN_POINT('Ctrl Pts',(8.13377449793336,0.303304450376019,
20.5949556783097));
#164004=CARTESIAN_POINT('Ctrl Pts',(7.97387079026596,3.29181374846737,20.7123922235979));
#164005=CARTESIAN_POINT('Ctrl Pts',(5.18705264259532,7.30934400029911,20.8827179239816));
#164006=CARTESIAN_POINT('Ctrl Pts',(-0.307003826939621,8.45123659280713,
21.0942745443635));
#164007=CARTESIAN_POINT('Ctrl Pts',(-4.29449854831533,7.30169108010176,
21.2529420096499));
#164008=CARTESIAN_POINT('Ctrl Pts',(-7.27250765093382,4.34712832670042,
21.4116094749364));
#164009=CARTESIAN_POINT('Ctrl Pts',(-8.45799212067998,0.346168247782319,
21.5702769402227));
#164010=CARTESIAN_POINT('Ctrl Pts',(-7.60342709026192,-3.73828686763913,
21.7289444055092));
#164011=CARTESIAN_POINT('Ctrl Pts',(-4.87682214009204,-6.92632775896643,
21.8876118707956));
#164012=CARTESIAN_POINT('Ctrl Pts',(-0.996603673995455,-8.39788261494148,
22.0462793360821));
#164013=CARTESIAN_POINT('Ctrl Pts',(4.57239175033109,-7.70877801686285,
22.257835956464));
#164014=CARTESIAN_POINT('Ctrl Pts',(7.83647938259924,-3.73996568278254,
22.4368419921741));
#164015=CARTESIAN_POINT('Ctrl Pts',(8.13195251875851,-0.526615112399208,
22.5629588727887));
#164016=CARTESIAN_POINT('Ctrl Pts',(8.12952934429449,-0.00742862902943328,
22.5832974432124));
#164017=CARTESIAN_POINT('',(8.12524972840108,0.00210085977608716,24.5832973448731));
#164018=CARTESIAN_POINT('Ctrl Pts',(8.12524660770977,-0.00742471553580177,
22.5832974432124));
#164019=CARTESIAN_POINT('Ctrl Pts',(8.12542479040845,0.187569740615188,
22.590940205944));
#164020=CARTESIAN_POINT('Ctrl Pts',(8.11857947866919,0.382805355671729,
22.5985829686756));
#164021=CARTESIAN_POINT('Ctrl Pts',(8.10468543979817,0.577720939921199,
22.6062257314072));
#164022=CARTESIAN_POINT('Ctrl Pts',(8.09080312872884,0.77247199812196,22.6138620429689));
#164023=CARTESIAN_POINT('Ctrl Pts',(8.06988396792512,0.966903205231081,
22.6214983545305));
#164024=CARTESIAN_POINT('Ctrl Pts',(8.04195478485132,1.16045284303454,22.6291346660922));
#164025=CARTESIAN_POINT('Ctrl Pts',(8.01403914810007,1.35390860462911,22.6367672738599));
#164026=CARTESIAN_POINT('Ctrl Pts',(7.9791203079503,1.54648329159617,22.6443998816277));
#164027=CARTESIAN_POINT('Ctrl Pts',(7.93727699992421,1.73761946034627,22.6520324893954));
#164028=CARTESIAN_POINT('Ctrl Pts',(7.89544627498311,1.92869815078578,22.6596628018916));
#164029=CARTESIAN_POINT('Ctrl Pts',(7.84669530549005,2.11833883197029,22.6672931143878));
#164030=CARTESIAN_POINT('Ctrl Pts',(7.79115408820036,2.30599339470408,22.674923426884));
#164031=CARTESIAN_POINT('Ctrl Pts',(7.77653351531357,2.35539125355325,22.6769320169986));
#164032=CARTESIAN_POINT('Ctrl Pts',(7.76144268937172,2.40465154912763,22.6789406071132));
#164033=CARTESIAN_POINT('Ctrl Pts',(7.74588456348442,2.45376443279989,22.6809491972278));
#164034=CARTESIAN_POINT('Ctrl Pts',(7.68363537510436,2.65026863708177,22.6889857117365));
#164035=CARTESIAN_POINT('Ctrl Pts',(7.61392907563297,2.84432493762119,22.6970222262451));
#164036=CARTESIAN_POINT('Ctrl Pts',(7.53699450845214,3.03535851952652,22.7050587407538));
#164037=CARTESIAN_POINT('Ctrl Pts',(7.46001346513546,3.22650750472886,22.7131001101171));
#164038=CARTESIAN_POINT('Ctrl Pts',(7.37579556050196,3.41462983532245,22.7211414794804));
#164039=CARTESIAN_POINT('Ctrl Pts',(7.28461702904298,3.59917244692125,22.7291828488437));
#164040=CARTESIAN_POINT('Ctrl Pts',(7.19337226838382,3.78384910443377,22.7372300592033));
#164041=CARTESIAN_POINT('Ctrl Pts',(7.09515693347681,3.96494057246139,22.7452772695628));
#164042=CARTESIAN_POINT('Ctrl Pts',(6.99029256122135,4.14191953942051,22.7533244799224));
#164043=CARTESIAN_POINT('Ctrl Pts',(6.88527362637015,4.31915936073787,22.7613835512953));
#164044=CARTESIAN_POINT('Ctrl Pts',(6.77358622807121,4.49227429402328,22.7694426226682));
#164045=CARTESIAN_POINT('Ctrl Pts',(6.65559546828131,4.66076565867598,22.7775016940412));
#164046=CARTESIAN_POINT('Ctrl Pts',(6.53750921278107,4.829393391656,22.7855672880159));
#164047=CARTESIAN_POINT('Ctrl Pts',(6.41310960554954,4.99338983723397,22.7936328819907));
#164048=CARTESIAN_POINT('Ctrl Pts',(6.28280175711014,5.15228974761259,22.8016984759655));
#164049=CARTESIAN_POINT('Ctrl Pts',(6.1522892955766,5.31143916715515,22.8097767347655));
#164050=CARTESIAN_POINT('Ctrl Pts',(6.01585025820671,5.46547581907097,22.8178549935656));
#164051=CARTESIAN_POINT('Ctrl Pts',(5.87392750789945,5.6139703592415,22.8259332523657));
#164052=CARTESIAN_POINT('Ctrl Pts',(5.79379525622176,5.69781316696575,22.8304943890819));
#164053=CARTESIAN_POINT('Ctrl Pts',(5.71191545704096,5.77988988860286,22.8350555257981));
#164054=CARTESIAN_POINT('Ctrl Pts',(5.62837241333386,5.86012896951273,22.8396166625142));
#164055=CARTESIAN_POINT('Ctrl Pts',(5.48026344874251,6.00238051633197,22.8477028562464));
#164056=CARTESIAN_POINT('Ctrl Pts',(5.32663687057979,6.13913088424393,22.8557890499786));
#164057=CARTESIAN_POINT('Ctrl Pts',(5.16792796774153,6.26994482294181,22.8638752437108));
#164058=CARTESIAN_POINT('Ctrl Pts',(5.00936062571359,6.40064208181373,22.8719542249418));
#164059=CARTESIAN_POINT('Ctrl Pts',(4.8457202410562,6.52541326870424,22.8800332061729));
#164060=CARTESIAN_POINT('Ctrl Pts',(4.67747772977852,6.64386104986596,22.888112187404));
#164061=CARTESIAN_POINT('Ctrl Pts',(4.50936230842683,6.76221935590258,22.8961850657951));
#164062=CARTESIAN_POINT('Ctrl Pts',(4.33665195086314,6.87426359959673,22.9042579441861));
#164063=CARTESIAN_POINT('Ctrl Pts',(4.15984981173212,6.97963731911138,22.9123308225772));
#164064=CARTESIAN_POINT('Ctrl Pts',(3.98315712102488,7.08494580758546,22.9203987034959));
#164065=CARTESIAN_POINT('Ctrl Pts',(3.80237797166621,7.18359184517078,22.9284665844145));
#164066=CARTESIAN_POINT('Ctrl Pts',(3.61804412261134,7.2752624893771,22.9365344653332));
#164067=CARTESIAN_POINT('Ctrl Pts',(3.43379928103538,7.36688886947799,22.9445984505932));
#164068=CARTESIAN_POINT('Ctrl Pts',(3.24600344630447,7.45154643311539,22.9526624358533));
#164069=CARTESIAN_POINT('Ctrl Pts',(3.05521312959896,7.52896807638511,22.9607264211134));
#164070=CARTESIAN_POINT('Ctrl Pts',(2.86177143845073,7.60746563257234,22.9689024699456));
#164071=CARTESIAN_POINT('Ctrl Pts',(2.66525171009062,7.67852450396723,22.9770785187779));
#164072=CARTESIAN_POINT('Ctrl Pts',(2.46625633353229,7.74191625244111,22.9852545676101));
#164073=CARTESIAN_POINT('Ctrl Pts',(2.27008144123943,7.80440951054691,22.9933147322571));
#164074=CARTESIAN_POINT('Ctrl Pts',(2.07150092702902,7.85945145889397,23.001374896904));
#164075=CARTESIAN_POINT('Ctrl Pts',(1.87110888729118,7.90687290238056,23.009435061551));
#164076=CARTESIAN_POINT('Ctrl Pts',(1.67072652949127,7.95429205470093,23.0174948367712));
#164077=CARTESIAN_POINT('Ctrl Pts',(1.46853312899585,7.99409136367617,23.0255546119915));
#164078=CARTESIAN_POINT('Ctrl Pts',(1.26513496224844,8.02615232161692,23.0336143872117));
#164079=CARTESIAN_POINT('Ctrl Pts',(1.06172143868044,8.05821570020081,23.0416747709553));
#164080=CARTESIAN_POINT('Ctrl Pts',(0.857103280432245,8.0825395137122,23.0497351546988));
#164081=CARTESIAN_POINT('Ctrl Pts',(0.651894507060131,8.09905680398433,
23.0577955384424));
#164082=CARTESIAN_POINT('Ctrl Pts',(0.441527223964406,8.11598930361166,
23.0660585429961));
#164083=CARTESIAN_POINT('Ctrl Pts',(0.230539591331538,8.12471762147112,
23.0743215475498));
#164084=CARTESIAN_POINT('Ctrl Pts',(0.0195962091400046,8.12522636922119,
23.0825845521035));
#164085=CARTESIAN_POINT('Ctrl Pts',(-0.186343748433672,8.1257230498422,
23.0906515641593));
#164086=CARTESIAN_POINT('Ctrl Pts',(-0.392241209201706,8.11838569250262,
23.0987185762151));
#164087=CARTESIAN_POINT('Ctrl Pts',(-0.59747973076114,8.10325277489414,
23.1067855882709));
#164088=CARTESIAN_POINT('Ctrl Pts',(-0.81019782658627,8.08756836344206,
23.1151465890736));
#164089=CARTESIAN_POINT('Ctrl Pts',(-1.02220768026863,8.06350955838493,
23.1235075898763));
#164090=CARTESIAN_POINT('Ctrl Pts',(-1.23283064176945,8.03117775741605,
23.131868590679));
#164091=CARTESIAN_POINT('Ctrl Pts',(-1.44345360327031,7.99884595644717,
23.1402295914817));
#164092=CARTESIAN_POINT('Ctrl Pts',(-1.65268930698428,7.95824125502719,
23.1485905922844));
#164093=CARTESIAN_POINT('Ctrl Pts',(-1.85987240871919,7.90952351193073,
23.1569515930871));
#164094=CARTESIAN_POINT('Ctrl Pts',(-2.0476590513144,7.86536671857118,23.1645298379165));
#164095=CARTESIAN_POINT('Ctrl Pts',(-2.23413571045512,7.81445615747484,
23.172108082746));
#164096=CARTESIAN_POINT('Ctrl Pts',(-2.41875864124654,7.75688688830095,
23.1796863275755));
#164097=CARTESIAN_POINT('Ctrl Pts',(-2.60324418926097,7.69936045793389,
23.1872589332337));
#164098=CARTESIAN_POINT('Ctrl Pts',(-2.78587840456789,7.63518528525991,
23.1948315388919));
#164099=CARTESIAN_POINT('Ctrl Pts',(-2.96612795935251,7.56450741894324,
23.2024041445502));
#164100=CARTESIAN_POINT('Ctrl Pts',(-3.14627761461197,7.49386872434765,
23.209972553251));
#164101=CARTESIAN_POINT('Ctrl Pts',(-3.32404489826436,7.41673464122926,
23.2175409619518));
#164102=CARTESIAN_POINT('Ctrl Pts',(-3.49891193578316,7.33330095033159,
23.2251093706526));
#164103=CARTESIAN_POINT('Ctrl Pts',(-3.67373672402911,7.24988741767998,
23.2326759507654));
#164104=CARTESIAN_POINT('Ctrl Pts',(-3.84566232611258,7.16017745753476,
23.2402425308782));
#164105=CARTESIAN_POINT('Ctrl Pts',(-4.01419102258741,7.06441490830477,
23.247809110991));
#164106=CARTESIAN_POINT('Ctrl Pts',(-4.1826898228336,6.96866934691796,23.2553743488267));
#164107=CARTESIAN_POINT('Ctrl Pts',(-4.34779259874365,6.86687351797403,
23.2629395866624));
#164108=CARTESIAN_POINT('Ctrl Pts',(-4.50902666291086,6.75931698588393,
23.2705048244982));
#164109=CARTESIAN_POINT('Ctrl Pts',(-4.67031679589973,6.65172305122602,
23.2780726931301));
#164110=CARTESIAN_POINT('Ctrl Pts',(-4.82773522134604,6.53836461288113,
23.2856405617621));
#164111=CARTESIAN_POINT('Ctrl Pts',(-4.98083826730238,6.41957457449293,
23.293208430394));
#164112=CARTESIAN_POINT('Ctrl Pts',(-5.13196560016682,6.30231745814797,
23.3006786397205));
#164113=CARTESIAN_POINT('Ctrl Pts',(-5.2788880160263,6.1797683351468,23.308148849047));
#164114=CARTESIAN_POINT('Ctrl Pts',(-5.42121114614919,6.05228529328945,
23.3156190583735));
#164115=CARTESIAN_POINT('Ctrl Pts',(-5.59850691186894,5.89347622618373,
23.3249248998167));
#164116=CARTESIAN_POINT('Ctrl Pts',(-5.76857974752031,5.72709014944377,
23.33423074126));
#164117=CARTESIAN_POINT('Ctrl Pts',(-5.93088679969662,5.55376172802582,
23.3435365827032));
#164118=CARTESIAN_POINT('Ctrl Pts',(-6.09406524569156,5.37950274128128,
23.3528923853317));
#164119=CARTESIAN_POINT('Ctrl Pts',(-6.2493943065823,5.19822673571199,23.3622481879602));
#164120=CARTESIAN_POINT('Ctrl Pts',(-6.39636762042764,5.01060563473567,
23.3716039905888));
#164121=CARTESIAN_POINT('Ctrl Pts',(-6.54405440963679,4.822073735535,23.3810052105418));
#164122=CARTESIAN_POINT('Ctrl Pts',(-6.68330412251971,4.62713503538254,
23.3904064304948));
#164123=CARTESIAN_POINT('Ctrl Pts',(-6.81364856918951,4.4264975700978,23.3998076504478));
#164124=CARTESIAN_POINT('Ctrl Pts',(-6.94413408722986,4.22564295553717,
23.4092190453106));
#164125=CARTESIAN_POINT('Ctrl Pts',(-7.06569504966478,4.01907727607903,
23.4186304401733));
#164126=CARTESIAN_POINT('Ctrl Pts',(-7.17790734213764,3.80753644108451,
23.4280418350361));
#164127=CARTESIAN_POINT('Ctrl Pts',(-7.28998800770875,3.59624374703865,
23.4374421901748));
#164128=CARTESIAN_POINT('Ctrl Pts',(-7.39274190945744,3.379987596664,23.4468425453135));
#164129=CARTESIAN_POINT('Ctrl Pts',(-7.48579198072721,3.1595262277405,23.4562429004522));
#164130=CARTESIAN_POINT('Ctrl Pts',(-7.5453273351781,3.01847049761071,23.4622574415214));
#164131=CARTESIAN_POINT('Ctrl Pts',(-7.60089114414173,2.87569377480425,
23.4682719825907));
#164132=CARTESIAN_POINT('Ctrl Pts',(-7.65239452295604,2.73139993913971,
23.4742865236599));
#164133=CARTESIAN_POINT('Ctrl Pts',(-7.71869293690673,2.54565576724932,
23.4820288221792));
#164134=CARTESIAN_POINT('Ctrl Pts',(-7.77829123086381,2.35730935636452,
23.4897711206984));
#164135=CARTESIAN_POINT('Ctrl Pts',(-7.83098073752968,2.16689368704123,
23.4975134192177));
#164136=CARTESIAN_POINT('Ctrl Pts',(-7.88363742340425,1.97659662943663,
23.5052508949861));
#164137=CARTESIAN_POINT('Ctrl Pts',(-7.92939379701267,1.78423321891253,
23.5129883707545));
#164138=CARTESIAN_POINT('Ctrl Pts',(-7.968090237771,1.59035389936909,23.5207258465229));
#164139=CARTESIAN_POINT('Ctrl Pts',(-8.00676945162113,1.39656089115494,
23.5284598777165));
#164140=CARTESIAN_POINT('Ctrl Pts',(-8.03839492315798,1.20125366368059,
23.5361939089101));
#164141=CARTESIAN_POINT('Ctrl Pts',(-8.06285755130023,1.00499535816884,
23.5439279401037));
#164142=CARTESIAN_POINT('Ctrl Pts',(-8.08731704899631,0.808762167540782,
23.5516609815848));
#164143=CARTESIAN_POINT('Ctrl Pts',(-8.10461547775754,0.611578490696759,
23.5593940230659));
#164144=CARTESIAN_POINT('Ctrl Pts',(-8.11469523237386,0.414015516845526,
23.5671270645471));
#164145=CARTESIAN_POINT('Ctrl Pts',(-8.1247739800302,0.216472279388297,
23.5748593335031));
#164146=CARTESIAN_POINT('Ctrl Pts',(-8.12763547556959,0.0185501735186514,
23.5825916024591));
#164147=CARTESIAN_POINT('Ctrl Pts',(-8.12327417012775,-0.179176782634739,
23.5903238714152));
#164148=CARTESIAN_POINT('Ctrl Pts',(-8.11891118709006,-0.37697979535549,
23.5980591146234));
#164149=CARTESIAN_POINT('Ctrl Pts',(-8.10731986004562,-0.574587154785271,
23.6057943578316));
#164150=CARTESIAN_POINT('Ctrl Pts',(-8.0885467637086,-0.771426479840539,
23.6135296010399));
#164151=CARTESIAN_POINT('Ctrl Pts',(-8.07283271759351,-0.936191107670352,
23.6200043970087));
#164152=CARTESIAN_POINT('Ctrl Pts',(-8.05208766086729,-1.10041754659114,
23.6264791929775));
#164153=CARTESIAN_POINT('Ctrl Pts',(-8.02636671998218,-1.26377404580982,
23.6329539889464));
#164154=CARTESIAN_POINT('Ctrl Pts',(-7.9929420508541,-1.47605776282834,
23.6413680634508));
#164155=CARTESIAN_POINT('Ctrl Pts',(-7.95109761222765,-1.68697455658355,
23.6497821379552));
#164156=CARTESIAN_POINT('Ctrl Pts',(-7.90097292802332,-1.89586770454655,
23.6581962124596));
#164157=CARTESIAN_POINT('Ctrl Pts',(-7.85083424537385,-2.10481919061817,
23.6666126367834));
#164158=CARTESIAN_POINT('Ctrl Pts',(-7.79241076234982,-2.3117456459217,
23.6750290611073));
#164159=CARTESIAN_POINT('Ctrl Pts',(-7.72589250952882,-2.51600327776148,
23.6834454854312));
#164160=CARTESIAN_POINT('Ctrl Pts',(-7.65935776064481,-2.7203115640701,
23.6918639969697));
#164161=CARTESIAN_POINT('Ctrl Pts',(-7.58472431602536,-2.92194945462536,
23.7002825085081));
#164162=CARTESIAN_POINT('Ctrl Pts',(-7.50223155273221,-3.12028993711951,
23.7087010200466));
#164163=CARTESIAN_POINT('Ctrl Pts',(-7.41970710431301,-3.31870660136509,
23.7171227651002));
#164164=CARTESIAN_POINT('Ctrl Pts',(-7.32931740498692,-3.51382308231481,
23.7255445101538));
#164165=CARTESIAN_POINT('Ctrl Pts',(-7.23134987631622,-3.70503259483656,
23.7339662552074));
#164166=CARTESIAN_POINT('Ctrl Pts',(-7.13337172823285,-3.8962628339475,
23.7423889131551));
#164167=CARTESIAN_POINT('Ctrl Pts',(-7.02781423380644,-4.08358502552981,
23.7508115711029));
#164168=CARTESIAN_POINT('Ctrl Pts',(-6.91501093115956,-4.26641669137506,
23.7592342290507));
#164169=CARTESIAN_POINT('Ctrl Pts',(-6.80218617657099,-4.44928312654128,
23.7676584887456));
#164170=CARTESIAN_POINT('Ctrl Pts',(-6.68211299959844,-4.62765710536148,
23.7760827484405));
#164171=CARTESIAN_POINT('Ctrl Pts',(-6.55516915733622,-4.80098374098559,
23.7845070081354));
#164172=CARTESIAN_POINT('Ctrl Pts',(-6.51943366817024,-4.84977627789909,
23.7868784901679));
#164173=CARTESIAN_POINT('Ctrl Pts',(-6.48315396805183,-4.89816901507628,
23.7892499722003));
#164174=CARTESIAN_POINT('Ctrl Pts',(-6.44633908841521,-4.9461500098228,
23.7916214542328));
#164175=CARTESIAN_POINT('Ctrl Pts',(-6.31555989011196,-5.11659511486402,
23.8000457794529));
#164176=CARTESIAN_POINT('Ctrl Pts',(-6.17801053486217,-5.2818594915429,
23.808470104673));
#164177=CARTESIAN_POINT('Ctrl Pts',(-6.03411794096312,-5.44142520274303,
23.8168944298932));
#164178=CARTESIAN_POINT('Ctrl Pts',(-5.89025021346363,-5.60096333903729,
23.8253172992869));
#164179=CARTESIAN_POINT('Ctrl Pts',(-5.74004161340068,-5.75480458089382,
23.8337401686806));
#164180=CARTESIAN_POINT('Ctrl Pts',(-5.5839579273677,-5.90246570747238,
23.8421630380743));
#164181=CARTESIAN_POINT('Ctrl Pts',(-5.42790613729704,-6.05009665925273,
23.8505841862406));
#164182=CARTESIAN_POINT('Ctrl Pts',(-5.26598185035697,-6.1915498364416,
23.8590053344068));
#164183=CARTESIAN_POINT('Ctrl Pts',(-5.09868692850712,-6.32637962562876,
23.8674264825731));
#164184=CARTESIAN_POINT('Ctrl Pts',(-4.93143894396884,-6.46117158612539,
23.8758452680492));
#164185=CARTESIAN_POINT('Ctrl Pts',(-4.75882353938873,-6.58934370464174,
23.8842640535254));
#164186=CARTESIAN_POINT('Ctrl Pts',(-4.58137557411481,-6.71049069825778,
23.8926828390016));
#164187=CARTESIAN_POINT('Ctrl Pts',(-4.40397717774242,-6.83160385027193,
23.9010992727464));
#164188=CARTESIAN_POINT('Ctrl Pts',(-4.22174913378615,-6.94569564687138,
23.9095157064911));
#164189=CARTESIAN_POINT('Ctrl Pts',(-4.03525614485675,-7.05240351992821,
23.9179321402359));
#164190=CARTESIAN_POINT('Ctrl Pts',(-3.84883084204029,-7.15907266423074,
23.9263455193046));
#164191=CARTESIAN_POINT('Ctrl Pts',(-3.65814391431436,-7.25836310579939,
23.9347588983732));
#164192=CARTESIAN_POINT('Ctrl Pts',(-3.46378643510607,-7.34995721718672,
23.9431722774418));
#164193=CARTESIAN_POINT('Ctrl Pts',(-3.40898591626193,-7.37578284966323,
23.9455444914676));
#164194=CARTESIAN_POINT('Ctrl Pts',(-3.35389374188062,-7.40099690293442,
23.9479167054934));
#164195=CARTESIAN_POINT('Ctrl Pts',(-3.2985235105494,-7.42559291995278,
23.9502889195192));
#164196=CARTESIAN_POINT('Ctrl Pts',(-3.11797530822053,-7.5057942582956,
23.9580241044299));
#164197=CARTESIAN_POINT('Ctrl Pts',(-2.93438884552525,-7.57945627267954,
23.9657592893406));
#164198=CARTESIAN_POINT('Ctrl Pts',(-2.74828795142395,-7.64634559110154,
23.9734944742513));
#164199=CARTESIAN_POINT('Ctrl Pts',(-2.56224460431735,-7.71321422569356,
23.9812272672516));
#164200=CARTESIAN_POINT('Ctrl Pts',(-2.37368870625444,-7.77331421556117,
23.988960060252));
#164201=CARTESIAN_POINT('Ctrl Pts',(-2.18316345428642,-7.82646055981682,
23.9966928532524));
#164202=CARTESIAN_POINT('Ctrl Pts',(-1.99266326661282,-7.87959991247631,
24.0044246289756));
#164203=CARTESIAN_POINT('Ctrl Pts',(-1.80019458149582,-7.9257873474648,
24.0121564046987));
#164204=CARTESIAN_POINT('Ctrl Pts',(-1.60631525135556,-7.96488787590651,
24.0198881804219));
#164205=CARTESIAN_POINT('Ctrl Pts',(-1.41236654589798,-8.00400239558476,
24.0276227227855));
#164206=CARTESIAN_POINT('Ctrl Pts',(-1.21700653278392,-8.0360248681617,
24.0353572651491));
#164207=CARTESIAN_POINT('Ctrl Pts',(-1.02080340047309,-8.06087141567725,
24.0430918075127));
#164208=CARTESIAN_POINT('Ctrl Pts',(-0.824567131640385,-8.0857221594977,
24.0508276561542));
#164209=CARTESIAN_POINT('Ctrl Pts',(-0.627487811452396,-8.10339452658514,
24.0585635047958));
#164210=CARTESIAN_POINT('Ctrl Pts',(-0.43013840036865,-8.11385657496041,
24.0662993534374));
#164211=CARTESIAN_POINT('Ctrl Pts',(-0.232627509060942,-8.12432718385738,
24.0740415319006));
#164212=CARTESIAN_POINT('Ctrl Pts',(-0.0348464387509563,-8.12757567537919,
24.0817837103638));
#164213=CARTESIAN_POINT('Ctrl Pts',(0.162631259539863,-8.12362226078493,
24.089525888827));
#164214=CARTESIAN_POINT('Ctrl Pts',(0.327834100089828,-8.12031497430906,
24.0960027208199));
#164215=CARTESIAN_POINT('Ctrl Pts',(0.492824541233774,-8.11196843802761,
24.1024795528128));
#164216=CARTESIAN_POINT('Ctrl Pts',(0.657269933842987,-8.09862233942082,
24.1089563848056));
#164217=CARTESIAN_POINT('Ctrl Pts',(0.89588388638438,-8.07925685104171,
24.1183544132772));
#164218=CARTESIAN_POINT('Ctrl Pts',(1.13348584590962,-8.04935409446737,
24.1277524417488));
#164219=CARTESIAN_POINT('Ctrl Pts',(1.36923883430365,-8.00904941782324,
24.1371504702204));
#164220=CARTESIAN_POINT('Ctrl Pts',(1.60532727946876,-7.96868739099755,
24.1465618713));
#164221=CARTESIAN_POINT('Ctrl Pts',(1.83956145406953,-7.91789384362429,
24.1559732723795));
#164222=CARTESIAN_POINT('Ctrl Pts',(2.07111280434926,-7.85685556149281,
24.165384673459));
#164223=CARTESIAN_POINT('Ctrl Pts',(2.30231551498804,-7.79590918279761,
24.1747819040857));
#164224=CARTESIAN_POINT('Ctrl Pts',(2.53084344038941,-7.72474891151579,
24.1841791347124));
#164225=CARTESIAN_POINT('Ctrl Pts',(2.75588421315682,-7.64361104231325,
24.1935763653391));
#164226=CARTESIAN_POINT('Ctrl Pts',(2.98035734914987,-7.56267783308314,
24.2029498926447));
#164227=CARTESIAN_POINT('Ctrl Pts',(3.20136085931515,-7.4718172900622,24.2123234199504));
#164228=CARTESIAN_POINT('Ctrl Pts',(3.41810146809121,-7.37131398845095,
24.2216969472561));
#164229=CARTESIAN_POINT('Ctrl Pts',(3.63343457608372,-7.27146334937751,
24.2310096034259));
#164230=CARTESIAN_POINT('Ctrl Pts',(3.84455991957934,-7.16209478347236,
24.2403222595958));
#164231=CARTESIAN_POINT('Ctrl Pts',(4.05071305595546,-7.04353684598952,
24.2496349157657));
#164232=CARTESIAN_POINT('Ctrl Pts',(4.18345267265937,-6.96719876326461,
24.2556312272078));
#164233=CARTESIAN_POINT('Ctrl Pts',(4.31413112295855,-6.8870518356622,24.2616275386499));
#164234=CARTESIAN_POINT('Ctrl Pts',(4.44254749922859,-6.80319478477559,
24.2676238500921));
#164235=CARTESIAN_POINT('Ctrl Pts',(4.60461567298398,-6.69736280688885,
24.2751915083061));
#164236=CARTESIAN_POINT('Ctrl Pts',(4.76301482345829,-6.58566076221604,
24.2827591665201));
#164237=CARTESIAN_POINT('Ctrl Pts',(4.91727939477646,-6.4683885872918,24.2903268247341));
#164238=CARTESIAN_POINT('Ctrl Pts',(5.0715012530076,-6.35114888292493,24.2978923875996));
#164239=CARTESIAN_POINT('Ctrl Pts',(5.22159051755009,-6.22834233932318,
24.3054579504651));
#164240=CARTESIAN_POINT('Ctrl Pts',(5.36711158068566,-6.10031153655039,
24.3130235133306));
#164241=CARTESIAN_POINT('Ctrl Pts',(5.51261989480059,-5.97229195048613,
24.3205884133812));
#164242=CARTESIAN_POINT('Ctrl Pts',(5.65356052862592,-5.83904925973904,
24.3281533134319));
#164243=CARTESIAN_POINT('Ctrl Pts',(5.78953192706015,-5.70096549963698,
24.3357182134826));
#164244=CARTESIAN_POINT('Ctrl Pts',(5.92557005941518,-5.56281396888009,
24.3432868263393));
#164245=CARTESIAN_POINT('Ctrl Pts',(6.05663382334175,-5.41981688213972,
24.3508554391961));
#164246=CARTESIAN_POINT('Ctrl Pts',(6.18235905565871,-5.27239263232688,
24.3584240520529));
#164247=CARTESIAN_POINT('Ctrl Pts',(6.30811224705745,-5.12493559795217,
24.3659943480362));
#164248=CARTESIAN_POINT('Ctrl Pts',(6.42852431209391,-4.97304972648763,
24.3735646440194));
#164249=CARTESIAN_POINT('Ctrl Pts',(6.54327239428554,-4.81718527115999,
24.3811349400027));
#164250=CARTESIAN_POINT('Ctrl Pts',(6.65813674899674,-4.66116288070536,
24.3887129068539));
#164251=CARTESIAN_POINT('Ctrl Pts',(6.76732544559469,-4.50115415480637,
24.3962908737051));
#164252=CARTESIAN_POINT('Ctrl Pts',(6.87055937175272,-4.33763777668455,
24.4038688405563));
#164253=CARTESIAN_POINT('Ctrl Pts',(6.97237912347573,-4.17636136647107,
24.4113429988304));
#164254=CARTESIAN_POINT('Ctrl Pts',(7.06840609847094,-4.01167311764415,
24.4188171571044));
#164255=CARTESIAN_POINT('Ctrl Pts',(7.15841748436539,-3.84405341820739,
24.4262913153785));
#164256=CARTESIAN_POINT('Ctrl Pts',(7.26188771774732,-3.65137057872229,
24.4348830384507));
#164257=CARTESIAN_POINT('Ctrl Pts',(7.3575986811752,-3.45446294962123,24.4434747615229));
#164258=CARTESIAN_POINT('Ctrl Pts',(7.44523300044756,-3.25395038861175,
24.4520664845951));
#164259=CARTESIAN_POINT('Ctrl Pts',(7.5328002175112,-3.053591361467,24.460651628925));
#164260=CARTESIAN_POINT('Ctrl Pts',(7.61230304488907,-2.84963312958498,
24.469236773255));
#164261=CARTESIAN_POINT('Ctrl Pts',(7.68347137690855,-2.64271738230312,
24.477821917585));
#164262=CARTESIAN_POINT('Ctrl Pts',(7.75633467562903,-2.43087366647677,
24.4866115283307));
#164263=CARTESIAN_POINT('Ctrl Pts',(7.82046144178498,-2.21593003026772,
24.4954011390765));
#164264=CARTESIAN_POINT('Ctrl Pts',(7.87561412889134,-1.99859692166958,
24.5041907498222));
#164265=CARTESIAN_POINT('Ctrl Pts',(7.92934991502028,-1.78684721272346,
24.5127545509346));
#164266=CARTESIAN_POINT('Ctrl Pts',(7.97456692045833,-1.57282952820372,
24.5213183520469));
#164267=CARTESIAN_POINT('Ctrl Pts',(8.01109526635494,-1.35721781445919,
24.5298821531592));
#164268=CARTESIAN_POINT('Ctrl Pts',(8.04906837707402,-1.13307825167902,
24.5387846687216));
#164269=CARTESIAN_POINT('Ctrl Pts',(8.07765147264861,-0.907216233308902,
24.5476871842841));
#164270=CARTESIAN_POINT('Ctrl Pts',(8.09671154652852,-0.680404067309817,
24.5565896998465));
#164271=CARTESIAN_POINT('Ctrl Pts',(8.11577162040843,-0.453591901310732,
24.5654922154089));
#164272=CARTESIAN_POINT('Ctrl Pts',(8.12530859140817,-0.225829868379238,
24.5743947309714));
#164273=CARTESIAN_POINT('Ctrl Pts',(8.12524972905207,0.00209834202667678,
24.5832972465338));
#164274=CARTESIAN_POINT('',(8.12524906564331,0.00389663476247341,26.5832974432124));
#164275=CARTESIAN_POINT('Ctrl Pts',(8.1252497277501,0.00210337752549754,
24.5832974432124));
#164276=CARTESIAN_POINT('Ctrl Pts',(8.12519425373155,0.216396935667924,
24.5916674107232));
#164277=CARTESIAN_POINT('Ctrl Pts',(8.11665690499827,0.430542956075556,
24.600037378234));
#164278=CARTESIAN_POINT('Ctrl Pts',(8.09969814556991,0.643876939446739,
24.6084073457449));
#164279=CARTESIAN_POINT('Ctrl Pts',(8.0827194136445,0.857462168339349,24.6167871706484));
#164280=CARTESIAN_POINT('Ctrl Pts',(8.05729948082891,1.0702331833302,24.6251669955519));
#164281=CARTESIAN_POINT('Ctrl Pts',(8.02355045062957,1.28153257028528,24.6335468204554));
#164282=CARTESIAN_POINT('Ctrl Pts',(7.9897621507523,1.4930778208644,24.641936395951));
#164283=CARTESIAN_POINT('Ctrl Pts',(7.94762543634056,1.70314775912192,24.6503259714466));
#164284=CARTESIAN_POINT('Ctrl Pts',(7.89730330546843,1.9110960373402,24.6587155469422));
#164285=CARTESIAN_POINT('Ctrl Pts',(7.84689148431164,2.11941494653026,24.66712007537));
#164286=CARTESIAN_POINT('Ctrl Pts',(7.78826513417819,2.32560437296713,24.6755246037978));
#164287=CARTESIAN_POINT('Ctrl Pts',(7.72163751836189,2.52903175099207,24.6839291322256));
#164288=CARTESIAN_POINT('Ctrl Pts',(7.65494828323145,2.73264726505277,24.6923414334256));
#164289=CARTESIAN_POINT('Ctrl Pts',(7.58024309317629,2.93349537735955,24.7007537346256));
#164290=CARTESIAN_POINT('Ctrl Pts',(7.49778366339738,3.13096274321355,24.7091660358256));
#164291=CARTESIAN_POINT('Ctrl Pts',(7.41520770443899,3.32870916399406,24.717590225036));
#164292=CARTESIAN_POINT('Ctrl Pts',(7.32485570562134,3.52306504198502,24.7260144142463));
#164293=CARTESIAN_POINT('Ctrl Pts',(7.22703660311154,3.71343903946006,24.7344386034567));
#164294=CARTESIAN_POINT('Ctrl Pts',(7.19147524044649,3.7826480036859,24.7375011509549));
#164295=CARTESIAN_POINT('Ctrl Pts',(7.15492743429019,3.85133096343416,24.7405636984531));
#164296=CARTESIAN_POINT('Ctrl Pts',(7.11740948051402,3.91946040280918,24.7436262459513));
#164297=CARTESIAN_POINT('Ctrl Pts',(7.01845000197587,4.09916246848877,24.7517041945844));
#164298=CARTESIAN_POINT('Ctrl Pts',(6.91256985386025,4.2753164785814,24.7597821432174));
#164299=CARTESIAN_POINT('Ctrl Pts',(6.80004220534934,4.4473715347346,24.7678600918505));
#164300=CARTESIAN_POINT('Ctrl Pts',(6.68765226782676,4.61921603044206,24.775928154715));
#164301=CARTESIAN_POINT('Ctrl Pts',(6.56863121752924,4.78697130925881,24.7839962175795));
#164302=CARTESIAN_POINT('Ctrl Pts',(6.4432981979165,4.95011069524975,24.792064280444));
#164303=CARTESIAN_POINT('Ctrl Pts',(6.31810313038334,5.11307051628942,24.8001234629189));
#164304=CARTESIAN_POINT('Ctrl Pts',(6.18661013476264,5.27142432407205,24.8081826453937));
#164305=CARTESIAN_POINT('Ctrl Pts',(6.04918209785142,5.4246735855288,24.8162418278685));
#164306=CARTESIAN_POINT('Ctrl Pts',(5.91193058244908,5.57772600366686,24.8242906586052));
#164307=CARTESIAN_POINT('Ctrl Pts',(5.76875944385984,5.72568672171993,24.832339489342));
#164308=CARTESIAN_POINT('Ctrl Pts',(5.62007236464318,5.86808948284483,24.8403883200787));
#164309=CARTESIAN_POINT('Ctrl Pts',(5.4714977516622,6.01038453116388,24.8484310627161));
#164310=CARTESIAN_POINT('Ctrl Pts',(5.31741574139684,6.14712978477373,24.8564738053536));
#164311=CARTESIAN_POINT('Ctrl Pts',(5.15826838948651,6.27789413613548,24.8645165479911));
#164312=CARTESIAN_POINT('Ctrl Pts',(4.99925066908542,6.40855197501042,24.8725527395119));
#164313=CARTESIAN_POINT('Ctrl Pts',(4.83517608049207,6.53323842964819,24.8805889310327));
#164314=CARTESIAN_POINT('Ctrl Pts',(4.66652163703117,6.65156097270557,24.8886251225535));
#164315=CARTESIAN_POINT('Ctrl Pts',(4.57090137497581,6.71864507877495,24.8931813187816));
#164316=CARTESIAN_POINT('Ctrl Pts',(4.47380958691757,6.78368424989858,24.8977375150097));
#164317=CARTESIAN_POINT('Ctrl Pts',(4.37533792323006,6.84661271141029,24.9022937112378));
#164318=CARTESIAN_POINT('Ctrl Pts',(4.2016472140727,6.95761001456172,24.9103302257465));
#164319=CARTESIAN_POINT('Ctrl Pts',(4.02379913650775,7.0619502142526,24.9183667402552));
#164320=CARTESIAN_POINT('Ctrl Pts',(3.84233766798678,7.15933857333692,24.9264032547638));
#164321=CARTESIAN_POINT('Ctrl Pts',(3.6607665786784,7.25678576468295,24.9344446241271));
#164322=CARTESIAN_POINT('Ctrl Pts',(3.47557802179457,7.34727258763503,24.9424859934904));
#164323=CARTESIAN_POINT('Ctrl Pts',(3.28733842738293,7.43055136758717,24.9505273628537));
#164324=CARTESIAN_POINT('Ctrl Pts',(3.09896210168703,7.51389063860958,24.9585745732132));
#164325=CARTESIAN_POINT('Ctrl Pts',(2.9075306054883,7.59001129326978,24.9666217835727));
#164326=CARTESIAN_POINT('Ctrl Pts',(2.71362865353334,7.65871445434695,24.9746689939322));
#164327=CARTESIAN_POINT('Ctrl Pts',(2.51944090394765,7.72751887897748,24.9827280653051));
#164328=CARTESIAN_POINT('Ctrl Pts',(2.32277571896713,7.78888385336661,24.9907871366781));
#164329=CARTESIAN_POINT('Ctrl Pts',(2.12423292010315,7.84266039451219,24.998846208051));
#164330=CARTESIAN_POINT('Ctrl Pts',(1.92552943081086,7.89648045965097,25.0069118020258));
#164331=CARTESIAN_POINT('Ctrl Pts',(1.72494560219532,7.94269976449133,25.0149773960006));
#164332=CARTESIAN_POINT('Ctrl Pts',(1.52309055541323,7.98122062860757,25.0230429899754));
#164333=CARTESIAN_POINT('Ctrl Pts',(1.32091855008999,8.01980197928131,25.0311212487755));
#164334=CARTESIAN_POINT('Ctrl Pts',(1.1174716486926,8.0506606792476,25.0391995075756));
#164335=CARTESIAN_POINT('Ctrl Pts',(0.913364956665286,8.07375080234929,
25.0472777663756));
#164336=CARTESIAN_POINT('Ctrl Pts',(0.798122483000528,8.08678791973644,
25.0518389030918));
#164337=CARTESIAN_POINT('Ctrl Pts',(0.682669701434189,8.0973494052993,25.056400039808));
#164338=CARTESIAN_POINT('Ctrl Pts',(0.567117184085187,8.10543432901749,
25.0609611765242));
#164339=CARTESIAN_POINT('Ctrl Pts',(0.362260346926869,8.11976765502001,
25.0690473702564));
#164340=CARTESIAN_POINT('Ctrl Pts',(0.156691465199783,8.12634211374536,
25.0771335639886));
#164341=CARTESIAN_POINT('Ctrl Pts',(-0.0489763871425417,8.12510239172421,
25.0852197577207));
#164342=CARTESIAN_POINT('Ctrl Pts',(-0.254460793520063,8.12386377547628,
25.0932987389518));
#164343=CARTESIAN_POINT('Ctrl Pts',(-0.460043679226377,8.11482487766477,
25.1013777201829));
#164344=CARTESIAN_POINT('Ctrl Pts',(-0.665108907424412,8.0979823230089,
25.109456701414));
#164345=CARTESIAN_POINT('Ctrl Pts',(-0.870019229918433,8.08115249117206,
25.1175295798051));
#164346=CARTESIAN_POINT('Ctrl Pts',(-1.07441236006256,8.05653078317278,
25.1256024581962));
#164347=CARTESIAN_POINT('Ctrl Pts',(-1.27767359326996,8.02416586017267,
25.1336753365873));
#164348=CARTESIAN_POINT('Ctrl Pts',(-1.48080899869202,7.99182097250601,
25.1417432175059));
#164349=CARTESIAN_POINT('Ctrl Pts',(-1.68281359250667,7.95174247887163,
25.1498110984246));
#164350=CARTESIAN_POINT('Ctrl Pts',(-1.88307858900344,7.90403078119872,
25.1578789793432));
#164351=CARTESIAN_POINT('Ctrl Pts',(-2.08324688550376,7.85634212160574,
25.1659429646033));
#164352=CARTESIAN_POINT('Ctrl Pts',(-2.2816769524035,7.8010276825022,25.1740069498633));
#164353=CARTESIAN_POINT('Ctrl Pts',(-2.47777036642716,7.73823891940249,
25.1820709351234));
#164354=CARTESIAN_POINT('Ctrl Pts',(-2.67658885096461,7.67457759356133,
25.1902469839556));
#164355=CARTESIAN_POINT('Ctrl Pts',(-2.87300493183574,7.60323272679547,
25.1984230327879));
#164356=CARTESIAN_POINT('Ctrl Pts',(-3.06640973223818,7.52441485542464,
25.2065990816201));
#164357=CARTESIAN_POINT('Ctrl Pts',(-3.25707328706062,7.44671411838073,
25.2146592462671));
#164358=CARTESIAN_POINT('Ctrl Pts',(-3.4448100598985,7.36175094502759,25.222719410914));
#164359=CARTESIAN_POINT('Ctrl Pts',(-3.62905549654197,7.26977604644864,
25.230779575561));
#164360=CARTESIAN_POINT('Ctrl Pts',(-3.81329203137077,7.17780559163513,
25.2388393507812));
#164361=CARTESIAN_POINT('Ctrl Pts',(-3.99403728309498,7.0788242288538,25.2468991260015));
#164362=CARTESIAN_POINT('Ctrl Pts',(-4.17074981954013,6.97312939112032,
25.2549589012217));
#164363=CARTESIAN_POINT('Ctrl Pts',(-4.34747569800599,6.86742657329247,
25.2630192849653));
#164364=CARTESIAN_POINT('Ctrl Pts',(-4.52016798236891,6.7550094326517,25.2710796687088));
#164365=CARTESIAN_POINT('Ctrl Pts',(-4.68831232156532,6.63621994345868,
25.2791400524523));
#164366=CARTESIAN_POINT('Ctrl Pts',(-4.86068344987307,6.51444434053824,
25.287403057006));
#164367=CARTESIAN_POINT('Ctrl Pts',(-5.02827469447822,6.38597201126693,
25.2956660615597));
#164368=CARTESIAN_POINT('Ctrl Pts',(-5.19056590735157,6.25121693144139,
25.3039290661135));
#164369=CARTESIAN_POINT('Ctrl Pts',(-5.34900768991199,6.11965814474792,
25.3119960781692));
#164370=CARTESIAN_POINT('Ctrl Pts',(-5.50239778719732,5.98211150095628,
25.320063090225));
#164371=CARTESIAN_POINT('Ctrl Pts',(-5.6502875377432,5.83900148170249,25.3281301022808));
#164372=CARTESIAN_POINT('Ctrl Pts',(-5.80356688262015,5.69067605742136,
25.3364911030835));
#164373=CARTESIAN_POINT('Ctrl Pts',(-5.95093718245841,5.53637440841922,
25.3448521038862));
#164374=CARTESIAN_POINT('Ctrl Pts',(-6.09194232304138,5.37660918193216,
25.3532131046889));
#164375=CARTESIAN_POINT('Ctrl Pts',(-6.23294746362432,5.21684395544513,
25.3615741054916));
#164376=CARTESIAN_POINT('Ctrl Pts',(-6.36758722539411,5.05161545900265,
25.3699351062943));
#164377=CARTESIAN_POINT('Ctrl Pts',(-6.4954531649779,4.88147270237974,25.378296107097));
#164378=CARTESIAN_POINT('Ctrl Pts',(-6.61134830939662,4.72725869187157,
25.3858743519265));
#164379=CARTESIAN_POINT('Ctrl Pts',(-6.72191067443861,4.56869831513259,
25.3934525967559));
#164380=CARTESIAN_POINT('Ctrl Pts',(-6.82678366733251,4.40621292290126,
25.4010308415854));
#164381=CARTESIAN_POINT('Ctrl Pts',(-6.9315786214752,4.24384844032217,25.4086034472436));
#164382=CARTESIAN_POINT('Ctrl Pts',(-7.03069242767589,4.07756505928574,
25.4161760529018));
#164383=CARTESIAN_POINT('Ctrl Pts',(-7.12380915881508,3.90781660665932,
25.4237486585601));
#164384=CARTESIAN_POINT('Ctrl Pts',(-7.21687428196408,3.73816223354332,
25.4313170672609));
#164385=CARTESIAN_POINT('Ctrl Pts',(-7.30394876770481,3.5650469313644,25.4388854759616));
#164386=CARTESIAN_POINT('Ctrl Pts',(-7.38476041616239,3.38895281147158,
25.4464538846624));
#164387=CARTESIAN_POINT('Ctrl Pts',(-7.46555253988048,3.2129012373241,25.4540204647752));
#164388=CARTESIAN_POINT('Ctrl Pts',(-7.54008467769878,3.03387260823567,
25.4615870448881));
#164389=CARTESIAN_POINT('Ctrl Pts',(-7.60813089433697,2.85237302208797,
25.4691536250009));
#164390=CARTESIAN_POINT('Ctrl Pts',(-7.67616503988421,2.67090563314568,
25.4767188628366));
#164391=CARTESIAN_POINT('Ctrl Pts',(-7.73771542824444,2.48696850503807,
25.4842841006724));
#164392=CARTESIAN_POINT('Ctrl Pts',(-7.79260463949582,2.30108680736043,
25.4918493385081));
#164393=CARTESIAN_POINT('Ctrl Pts',(-7.84751293835988,2.11514046969674,
25.4994172071401));
#164394=CARTESIAN_POINT('Ctrl Pts',(-7.89575532499491,1.9272485636824,25.506985075772));
#164395=CARTESIAN_POINT('Ctrl Pts',(-7.93720442422442,1.73795094596259,
25.514552944404));
#164396=CARTESIAN_POINT('Ctrl Pts',(-7.97811864495121,1.55109611296469,
25.5220231537305));
#164397=CARTESIAN_POINT('Ctrl Pts',(-8.01241382660653,1.36287197969354,
25.529493363057));
#164398=CARTESIAN_POINT('Ctrl Pts',(-8.04001658451674,1.17380615230786,
25.5369635723835));
#164399=CARTESIAN_POINT('Ctrl Pts',(-8.0744020852813,0.938281746620939,
25.5462694138267));
#164400=CARTESIAN_POINT('Ctrl Pts',(-8.0983873350054,0.701567142603875,
25.5555752552699));
#164401=CARTESIAN_POINT('Ctrl Pts',(-8.11196213589248,0.46449743631869,
25.5648810967131));
#164402=CARTESIAN_POINT('Ctrl Pts',(-8.12560981714687,0.226154950608267,
25.5742368993416));
#164403=CARTESIAN_POINT('Ctrl Pts',(-8.12873501736658,-0.012546411925814,
25.5835927019701));
#164404=CARTESIAN_POINT('Ctrl Pts',(-8.12137942789707,-0.250766326747155,
25.5929485045987));
#164405=CARTESIAN_POINT('Ctrl Pts',(-8.11398813104817,-0.490142669467328,
25.6023497245517));
#164406=CARTESIAN_POINT('Ctrl Pts',(-8.09601406568459,-0.729032837388664,
25.6117509445047));
#164407=CARTESIAN_POINT('Ctrl Pts',(-8.06755136842397,-0.966593234168639,
25.6211521644577));
#164408=CARTESIAN_POINT('Ctrl Pts',(-8.03905786607876,-1.20441074179269,
25.6305635593205));
#164409=CARTESIAN_POINT('Ctrl Pts',(-8.00005304104605,-1.44089556401629,
25.6399749541832));
#164410=CARTESIAN_POINT('Ctrl Pts',(-7.9506827295727,-1.67521094079952,
25.649386349046));
#164411=CARTESIAN_POINT('Ctrl Pts',(-7.90137033030281,-1.90925146171552,
25.6587867041847));
#164412=CARTESIAN_POINT('Ctrl Pts',(-7.84171675979681,-2.1411275890458,
25.6681870593234));
#164413=CARTESIAN_POINT('Ctrl Pts',(-7.77191828339444,-2.37001556086435,
25.6775874144622));
#164414=CARTESIAN_POINT('Ctrl Pts',(-7.72725977882757,-2.51646280529752,
25.6836019555314));
#164415=CARTESIAN_POINT('Ctrl Pts',(-7.67844927289484,-2.66168699044815,
25.6896164966007));
#164416=CARTESIAN_POINT('Ctrl Pts',(-7.62554913898239,-2.80547462855483,
25.6956310376699));
#164417=CARTESIAN_POINT('Ctrl Pts',(-7.55745273333087,-2.99056719086086,
25.7033733361892));
#164418=CARTESIAN_POINT('Ctrl Pts',(-7.48254469812438,-3.1733652034248,
25.7111156347085));
#164419=CARTESIAN_POINT('Ctrl Pts',(-7.40100628188632,-3.35332574886175,
25.7188579332277));
#164420=CARTESIAN_POINT('Ctrl Pts',(-7.31951865669797,-3.53317419517499,
25.7265954089961));
#164421=CARTESIAN_POINT('Ctrl Pts',(-7.23140901920778,-3.7101883731819,
25.7343328847645));
#164422=CARTESIAN_POINT('Ctrl Pts',(-7.13690746498119,-3.88384337979735,
25.7420703605329));
#164423=CARTESIAN_POINT('Ctrl Pts',(-7.0424479810221,-4.05742107855643,
25.7498043917264));
#164424=CARTESIAN_POINT('Ctrl Pts',(-6.94160241609006,-4.22764227461244,
25.75753842292));
#164425=CARTESIAN_POINT('Ctrl Pts',(-6.83464779015968,-4.39400468217382,
25.7652724541136));
#164426=CARTESIAN_POINT('Ctrl Pts',(-6.72770685105335,-4.56034580058589,
25.7730054955947));
#164427=CARTESIAN_POINT('Ctrl Pts',(-6.61465859256753,-4.72282881294278,
25.7807385370758));
#164428=CARTESIAN_POINT('Ctrl Pts',(-6.4958247300516,-4.88097824610498,
25.7884715785569));
#164429=CARTESIAN_POINT('Ctrl Pts',(-6.37700273894996,-5.03911188025669,
25.7962038475129));
#164430=CARTESIAN_POINT('Ctrl Pts',(-6.25239651026016,-5.19291251718738,
25.8039361164689));
#164431=CARTESIAN_POINT('Ctrl Pts',(-6.12236954133246,-5.34193586276217,
25.811668385425));
#164432=CARTESIAN_POINT('Ctrl Pts',(-5.99229255694347,-5.49101653084038,
25.8194036286332));
#164433=CARTESIAN_POINT('Ctrl Pts',(-5.85679089893089,-5.63531596964487,
25.8271388718414));
#164434=CARTESIAN_POINT('Ctrl Pts',(-5.71626703704535,-5.77442453614979,
25.8348741150497));
#164435=CARTESIAN_POINT('Ctrl Pts',(-5.59864134513404,-5.89086555311572,
25.8413489110186));
#164436=CARTESIAN_POINT('Ctrl Pts',(-5.47749757611778,-6.00367010908838,
25.8478237069875));
#164437=CARTESIAN_POINT('Ctrl Pts',(-5.35309060059063,-6.11261879920286,
25.8542985029564));
#164438=CARTESIAN_POINT('Ctrl Pts',(-5.19142225366823,-6.2541989200565,
25.8627125774608));
#164439=CARTESIAN_POINT('Ctrl Pts',(-5.02416484090899,-6.38933518021291,
25.8711266519651));
#164440=CARTESIAN_POINT('Ctrl Pts',(-4.85184623503741,-6.51761272814312,
25.8795407264695));
#164441=CARTESIAN_POINT('Ctrl Pts',(-4.67947950532052,-6.64592610046295,
25.8879571507934));
#164442=CARTESIAN_POINT('Ctrl Pts',(-4.50204897257131,-6.76737677901806,
25.8963735751173));
#164443=CARTESIAN_POINT('Ctrl Pts',(-4.32011300543683,-6.88159219823113,
25.9047899994412));
#164444=CARTESIAN_POINT('Ctrl Pts',(-4.1381319194507,-6.99583594207202,
25.9132085109796));
#164445=CARTESIAN_POINT('Ctrl Pts',(-3.95164339201225,-7.10284070410267,
25.9216270225181));
#164446=CARTESIAN_POINT('Ctrl Pts',(-3.76123292994817,-7.20227841791564,
25.9300455340565));
#164447=CARTESIAN_POINT('Ctrl Pts',(-3.57074933202065,-7.30175432533931,
25.9384672791101));
#164448=CARTESIAN_POINT('Ctrl Pts',(-3.37634102263371,-7.39365725306045,
25.9468890241637));
#164449=CARTESIAN_POINT('Ctrl Pts',(-3.17861743884908,-7.47770544618766,
25.9553107692173));
#164450=CARTESIAN_POINT('Ctrl Pts',(-2.98087242236817,-7.56176274990937,
25.9637334271651));
#164451=CARTESIAN_POINT('Ctrl Pts',(-2.77981165806754,-7.63796351858892,
25.9721560851128));
#164452=CARTESIAN_POINT('Ctrl Pts',(-2.57606441916061,-7.70607420615937,
25.9805787430605));
#164453=CARTESIAN_POINT('Ctrl Pts',(-2.37227843339153,-7.77419784642274,
25.9890030027555));
#164454=CARTESIAN_POINT('Ctrl Pts',(-2.1658052027137,-7.83422824840479,
25.9974272624504));
#164455=CARTESIAN_POINT('Ctrl Pts',(-1.95729027524906,-7.88598138096429,
26.0058515221453));
#164456=CARTESIAN_POINT('Ctrl Pts',(-1.89859201309983,-7.90055021293694,
26.0082230041778));
#164457=CARTESIAN_POINT('Ctrl Pts',(-1.83973203903542,-7.91446341189762,
26.0105944862103));
#164458=CARTESIAN_POINT('Ctrl Pts',(-1.78072493887738,-7.92771759427391,
26.0129659682427));
#164459=CARTESIAN_POINT('Ctrl Pts',(-1.57111129002023,-7.97480103886061,
26.0213902934629));
#164460=CARTESIAN_POINT('Ctrl Pts',(-1.3596185723426,-8.01356919200245,
26.029814618683));
#164461=CARTESIAN_POINT('Ctrl Pts',(-1.14690640793186,-8.04389788932858,
26.0382389439031));
#164462=CARTESIAN_POINT('Ctrl Pts',(-0.934231002784703,-8.07422134548488,
26.0466618132968));
#164463=CARTESIAN_POINT('Ctrl Pts',(-0.720336832960184,-8.09610822154253,
26.0550846826904));
#164464=CARTESIAN_POINT('Ctrl Pts',(-0.505891122389207,-8.10948591063501,
26.0635075520841));
#164465=CARTESIAN_POINT('Ctrl Pts',(-0.291489234159958,-8.12286086597422,
26.0719287002503));
#164466=CARTESIAN_POINT('Ctrl Pts',(-0.0765362935174903,-8.12773009032672,
26.0803498484164));
#164467=CARTESIAN_POINT('Ctrl Pts',(0.138296870498141,-8.12407296484408,
26.0887709965826));
#164468=CARTESIAN_POINT('Ctrl Pts',(0.353069759577974,-8.12041686542743,
26.0971897820588));
#164469=CARTESIAN_POINT('Ctrl Pts',(0.567722675450266,-8.10823919853883,
26.1056085675349));
#164470=CARTESIAN_POINT('Ctrl Pts',(0.781585291870921,-8.08757145217469,
26.1140273530111));
#164471=CARTESIAN_POINT('Ctrl Pts',(0.995388167201144,-8.06690947920716,
26.1224437867559));
#164472=CARTESIAN_POINT('Ctrl Pts',(1.20840092136047,-8.03776218737824,
26.1308602205007));
#164473=CARTESIAN_POINT('Ctrl Pts',(1.41995768024003,-8.00021298146664,
26.1392766542455));
#164474=CARTESIAN_POINT('Ctrl Pts',(1.63143765631525,-7.96267740373382,
26.1476900333141));
#164475=CARTESIAN_POINT('Ctrl Pts',(1.84146243275004,-7.91674604760285,
26.1561034123828));
#164476=CARTESIAN_POINT('Ctrl Pts',(2.04937467982987,-7.86255371900073,
26.1645167914514));
#164477=CARTESIAN_POINT('Ctrl Pts',(2.10799706504014,-7.84727379390072,
26.1668890054773));
#164478=CARTESIAN_POINT('Ctrl Pts',(2.16645156523244,-7.83133743396191,
26.1692612195033));
#164479=CARTESIAN_POINT('Ctrl Pts',(2.2247236023665,-7.81474839361917,26.1716334335292));
#164480=CARTESIAN_POINT('Ctrl Pts',(2.41473385330918,-7.76065576405877,
26.1793686184399));
#164481=CARTESIAN_POINT('Ctrl Pts',(2.60288735546081,-7.69959561931575,
26.1871038033505));
#164482=CARTESIAN_POINT('Ctrl Pts',(2.78863239052449,-7.63172437611695,
26.1948389882612));
#164483=CARTESIAN_POINT('Ctrl Pts',(2.97431998863419,-7.56387412038341,
26.2025717812616));
#164484=CARTESIAN_POINT('Ctrl Pts',(3.15760027133842,-7.48921708154389,
26.210304574262));
#164485=CARTESIAN_POINT('Ctrl Pts',(3.33793763931164,-7.40795922495302,
26.2180373672624));
#164486=CARTESIAN_POINT('Ctrl Pts',(3.51825128324374,-7.32671205813075,
26.2257691429855));
#164487=CARTESIAN_POINT('Ctrl Pts',(3.69562246188648,-7.23886594900611,
26.2335009187087));
#164488=CARTESIAN_POINT('Ctrl Pts',(3.86953636465702,-7.14467465215155,
26.2412326944318));
#164489=CARTESIAN_POINT('Ctrl Pts',(4.04351249857005,-7.05044965107944,
26.2489672367954));
#164490=CARTESIAN_POINT('Ctrl Pts',(4.21402857197604,-6.94987509075678,
26.256701779159));
#164491=CARTESIAN_POINT('Ctrl Pts',(4.38059458351416,-6.84325059145041,
26.2644363215226));
#164492=CARTESIAN_POINT('Ctrl Pts',(4.54718872619452,-6.7366080844549,26.2721721701642));
#164493=CARTESIAN_POINT('Ctrl Pts',(4.70983118419788,-6.62391379951222,
26.2799080188058));
#164494=CARTESIAN_POINT('Ctrl Pts',(4.86806156612962,-6.50551029135084,
26.2876438674473));
#164495=CARTESIAN_POINT('Ctrl Pts',(5.02642141932461,-6.3870099000777,26.2953860459106));
#164496=CARTESIAN_POINT('Ctrl Pts',(5.18036170501404,-6.26279116996034,
26.3031282243738));
#164497=CARTESIAN_POINT('Ctrl Pts',(5.32945499152679,-6.13323707806817,
26.310870402837));
#164498=CARTESIAN_POINT('Ctrl Pts',(5.45418114871876,-6.02485671830715,
26.3173472348298));
#164499=CARTESIAN_POINT('Ctrl Pts',(5.57551571201498,-5.91274323077475,
26.3238240668227));
#164500=CARTESIAN_POINT('Ctrl Pts',(5.69322869546535,-5.7971402073462,26.3303008988156));
#164501=CARTESIAN_POINT('Ctrl Pts',(5.86403287429022,-5.62939762783106,
26.3396989272871));
#164502=CARTESIAN_POINT('Ctrl Pts',(6.02730908883279,-5.45421274325348,
26.3490969557586));
#164503=CARTESIAN_POINT('Ctrl Pts',(6.18250140949143,-5.27222570496906,
26.3584949842301));
#164504=CARTESIAN_POINT('Ctrl Pts',(6.3379145558335,-5.08997971436063,26.3679063853096));
#164505=CARTESIAN_POINT('Ctrl Pts',(6.48522077508968,-4.90091223758863,
26.377317786389));
#164506=CARTESIAN_POINT('Ctrl Pts',(6.62390356071435,-4.7056975233068,26.3867291874685));
#164507=CARTESIAN_POINT('Ctrl Pts',(6.76237753599913,-4.51077673772461,
26.3961264180952));
#164508=CARTESIAN_POINT('Ctrl Pts',(6.89225400991554,-4.30972724525927,
26.4055236487219));
#164509=CARTESIAN_POINT('Ctrl Pts',(7.0130606230254,-4.10325093800885,26.4149208793486));
#164510=CARTESIAN_POINT('Ctrl Pts',(7.1335625167913,-3.89729544102925,26.4242944066541));
#164511=CARTESIAN_POINT('Ctrl Pts',(7.24504020994197,-3.68594049381563,
26.4336679339596));
#164512=CARTESIAN_POINT('Ctrl Pts',(7.34706693404567,-3.4699128273132,26.4430414612652));
#164513=CARTESIAN_POINT('Ctrl Pts',(7.44843110259639,-3.25528803178695,
26.452354117435));
#164514=CARTESIAN_POINT('Ctrl Pts',(7.54046661329701,-3.03605103982633,
26.4616667736048));
#164515=CARTESIAN_POINT('Ctrl Pts',(7.62279701287586,-2.8129438783934,26.4709794297747));
#164516=CARTESIAN_POINT('Ctrl Pts',(7.67580860355992,-2.66928776132039,
26.4769757412171));
#164517=CARTESIAN_POINT('Ctrl Pts',(7.72479737831623,-2.52402769341761,
26.4829720526596));
#164518=CARTESIAN_POINT('Ctrl Pts',(7.76967232571477,-2.37736819056747,
26.4889683641021));
#164519=CARTESIAN_POINT('Ctrl Pts',(7.82403259858036,-2.1997089161741,26.4962321303034));
#164520=CARTESIAN_POINT('Ctrl Pts',(7.87234909752469,-2.02000793831355,
26.5034958965047));
#164521=CARTESIAN_POINT('Ctrl Pts',(7.91445874219333,-1.83875783631765,
26.510759662706));
#164522=CARTESIAN_POINT('Ctrl Pts',(7.9565588222911,-1.65754890254958,26.5180217790523));
#164523=CARTESIAN_POINT('Ctrl Pts',(7.99245475556078,-1.47479192120609,
26.5252838953987));
#164524=CARTESIAN_POINT('Ctrl Pts',(8.02203357363806,-1.2909937668028,26.532546011745));
#164525=CARTESIAN_POINT('Ctrl Pts',(8.05160832091196,-1.10722090773581,
26.539807128638));
#164526=CARTESIAN_POINT('Ctrl Pts',(8.07486762491511,-0.922407545912508,
26.547068245531));
#164527=CARTESIAN_POINT('Ctrl Pts',(8.0917498982538,-0.73706929566335,26.554329362424));
#164528=CARTESIAN_POINT('Ctrl Pts',(8.10863655287446,-0.551682946493031,
26.5615923637197));
#164529=CARTESIAN_POINT('Ctrl Pts',(8.11914284310628,-0.365771825371201,
26.5688553650154));
#164530=CARTESIAN_POINT('Ctrl Pts',(8.12325917997313,-0.179855101351589,
26.576118366311));
#164531=CARTESIAN_POINT('Ctrl Pts',(8.12461543742631,-0.118598952795572,
26.5785113919448));
#164532=CARTESIAN_POINT('Ctrl Pts',(8.12527843401783,-0.0573421962115691,
26.5809044175786));
#164533=CARTESIAN_POINT('Ctrl Pts',(8.12524906564331,0.00389663476247341,
26.5832974432124));
#164534=CARTESIAN_POINT('',(8.12524985409108,-0.00153983533529523,30.5838443095726));
#164535=CARTESIAN_POINT('Ctrl Pts',(8.12524912703364,0.00376644912446197,
26.5863743722194));
#164536=CARTESIAN_POINT('Ctrl Pts',(8.12504495498968,0.444220751611364,
26.6050223615419));
#164537=CARTESIAN_POINT('Ctrl Pts',(8.08902685666685,0.883951628366578,
26.623712746037));
#164538=CARTESIAN_POINT('Ctrl Pts',(8.01504120179438,1.333806306405,26.641849757576));
#164539=CARTESIAN_POINT('Ctrl Pts',(8.01249876033298,1.34899531095105,26.6424608883332));
#164540=CARTESIAN_POINT('Ctrl Pts',(8.00830498727768,1.37361950306895,26.643449516136));
#164541=CARTESIAN_POINT('Ctrl Pts',(8.00668013404125,1.38305912403317,26.6438279961786));
#164542=CARTESIAN_POINT('Ctrl Pts',(8.00380323325127,1.39959755855871,26.6444901860161));
#164543=CARTESIAN_POINT('Ctrl Pts',(8.00255842566831,1.40669761025795,26.6447741721005));
#164544=CARTESIAN_POINT('Ctrl Pts',(8.00003461415254,1.42098098880658,26.6453448665394));
#164545=CARTESIAN_POINT('Ctrl Pts',(7.99875537924197,1.42816426985755,26.6456315656395));
#164546=CARTESIAN_POINT('Ctrl Pts',(7.99627076304714,1.4420080657223,26.6461834889836));
#164547=CARTESIAN_POINT('Ctrl Pts',(7.99506673173401,1.44866881412612,26.6464487666777));
#164548=CARTESIAN_POINT('Ctrl Pts',(7.99220071902629,1.46441130463962,26.6470750862407));
#164549=CARTESIAN_POINT('Ctrl Pts',(7.99053157671914,1.47349174572936,26.6474358372344));
#164550=CARTESIAN_POINT('Ctrl Pts',(7.9855296119797,1.50044490706627,26.6485050664808));
#164551=CARTESIAN_POINT('Ctrl Pts',(7.98215226176878,1.5183093822101,26.6492116902806));
#164552=CARTESIAN_POINT('Ctrl Pts',(7.93918514452742,1.74147743152986,26.658011987617));
#164553=CARTESIAN_POINT('Ctrl Pts',(7.89174631816007,1.94518467158631,26.6657214896003));
#164554=CARTESIAN_POINT('Ctrl Pts',(7.80616977090938,2.25756079995807,26.6772609747527));
#164555=CARTESIAN_POINT('Ctrl Pts',(7.77349293372523,2.36763086703,26.6812736618258));
#164556=CARTESIAN_POINT('Ctrl Pts',(7.72019045351377,2.53415703804759,26.6873037899847));
#164557=CARTESIAN_POINT('Ctrl Pts',(7.70125348714104,2.59113630800775,26.6893597126843));
#164558=CARTESIAN_POINT('Ctrl Pts',(7.65311018921146,2.73080230995007,26.6943901908952));
#164559=CARTESIAN_POINT('Ctrl Pts',(7.62319343136999,2.81323638634756,26.6973515368996));
#164560=CARTESIAN_POINT('Ctrl Pts',(7.54814595963977,3.01003187040682,26.7044297225124));
#164561=CARTESIAN_POINT('Ctrl Pts',(7.5017426782117,3.12388481781467,26.7085318363778));
#164562=CARTESIAN_POINT('Ctrl Pts',(7.35398857354184,3.46410722027513,26.7209008103668));
#164563=CARTESIAN_POINT('Ctrl Pts',(7.24484205175407,3.68692939580951,26.7291556799172));
#164564=CARTESIAN_POINT('Ctrl Pts',(6.94753257749294,4.22952929722464,26.7501718443442));
#164565=CARTESIAN_POINT('Ctrl Pts',(6.74735537569329,4.54205858420145,26.7631315789055));
#164566=CARTESIAN_POINT('Ctrl Pts',(6.43537459756574,4.96276860101953,26.7824965863518));
#164567=CARTESIAN_POINT('Ctrl Pts',(6.34074438564564,5.08311677585026,26.7882757335438));
#164568=CARTESIAN_POINT('Ctrl Pts',(6.22800172430092,5.21844945864787,26.7950763289506));
#164569=CARTESIAN_POINT('Ctrl Pts',(6.21315378715827,5.23611881425771,26.7959703171741));
#164570=CARTESIAN_POINT('Ctrl Pts',(6.19054413108309,5.26279319837987,26.79732923558));
#164571=CARTESIAN_POINT('Ctrl Pts',(6.18283754712518,5.27184490972763,26.7977920096806));
#164572=CARTESIAN_POINT('Ctrl Pts',(6.16893258434562,5.28810445288811,26.7986262500124));
#164573=CARTESIAN_POINT('Ctrl Pts',(6.16274136140793,5.29531838952981,26.7989974350539));
#164574=CARTESIAN_POINT('Ctrl Pts',(6.15033126136748,5.30972724150064,26.7997409435223));
#164575=CARTESIAN_POINT('Ctrl Pts',(6.14411238403888,5.31692213740844,26.8001132667633));
#164576=CARTESIAN_POINT('Ctrl Pts',(6.12672227105973,5.33697028082346,26.8011536942763));
#164577=CARTESIAN_POINT('Ctrl Pts',(6.11552326700168,5.34979931694466,26.8018228950645));
#164578=CARTESIAN_POINT('Ctrl Pts',(6.07030912612532,5.40126694818107,26.8045214427148));
#164579=CARTESIAN_POINT('Ctrl Pts',(6.03596783001374,5.43961669316477,26.806563732999));
#164580=CARTESIAN_POINT('Ctrl Pts',(5.40032426472651,6.13602379163725,26.8442376855673));
#164581=CARTESIAN_POINT('Ctrl Pts',(4.69519226122991,6.69095422004784,26.8848189525063));
#164582=CARTESIAN_POINT('Ctrl Pts',(3.74917403078295,7.21102661120727,26.9328587902915));
#164583=CARTESIAN_POINT('Ctrl Pts',(3.58089608289444,7.29605362875179,26.941155126988));
#164584=CARTESIAN_POINT('Ctrl Pts',(3.27939021903004,7.43545103384776,26.955429180201));
#164585=CARTESIAN_POINT('Ctrl Pts',(3.14738980245291,7.49228090305327,26.9614865221012));
#164586=CARTESIAN_POINT('Ctrl Pts',(2.96970110594588,7.56325544356129,26.9693294310407));
#164587=CARTESIAN_POINT('Ctrl Pts',(2.92530227422235,7.58053852182867,26.9712631953241));
#164588=CARTESIAN_POINT('Ctrl Pts',(2.84986377623592,7.60914287210126,26.9745059910686));
#164589=CARTESIAN_POINT('Ctrl Pts',(2.81890445132915,7.62066640986863,26.9758248792002));
#164590=CARTESIAN_POINT('Ctrl Pts',(2.77666046922116,7.63609761321342,26.9776092625627));
#164591=CARTESIAN_POINT('Ctrl Pts',(2.7654364849857,7.6401695772657,26.9780819040022));
#164592=CARTESIAN_POINT('Ctrl Pts',(2.74762675482655,7.64658640490091,26.9788296120083));
#164593=CARTESIAN_POINT('Ctrl Pts',(2.74104691425429,7.64894752535956,26.9791053662295));
#164594=CARTESIAN_POINT('Ctrl Pts',(2.72735757256258,7.65383989810297,26.9796780716101));
#164595=CARTESIAN_POINT('Ctrl Pts',(2.72024757350879,7.6563697437958,26.9799749640592));
#164596=CARTESIAN_POINT('Ctrl Pts',(2.70395242127774,7.6621422426963,26.9806541369966));
#164597=CARTESIAN_POINT('Ctrl Pts',(2.69476493125208,7.66537829530659,26.9810361475208));
#164598=CARTESIAN_POINT('Ctrl Pts',(2.66644527566709,7.67529594453423,26.982210888139));
#164599=CARTESIAN_POINT('Ctrl Pts',(2.64729383639985,7.68192251958345,26.9830014222104));
#164600=CARTESIAN_POINT('Ctrl Pts',(2.4953607260324,7.73385713237851,26.9892433610403));
#164601=CARTESIAN_POINT('Ctrl Pts',(2.36144647314292,7.77579219058717,26.994566741772));
#164602=CARTESIAN_POINT('Ctrl Pts',(1.82242295399138,7.92937606807615,27.0154901887677));
#164603=CARTESIAN_POINT('Ctrl Pts',(1.40999927824042,8.01299935331532,27.0304116026265));
#164604=CARTESIAN_POINT('Ctrl Pts',(0.660769176253835,8.10525058116122,
27.0575458576452));
#164605=CARTESIAN_POINT('Ctrl Pts',(0.326390255874048,8.12558699641569,
27.0696587962195));
#164606=CARTESIAN_POINT('Ctrl Pts',(-0.177155189189466,8.12507360333953,
27.0883697443591));
#164607=CARTESIAN_POINT('Ctrl Pts',(-0.345976441303749,8.11963689778604,
27.0947187339356));
#164608=CARTESIAN_POINT('Ctrl Pts',(-0.621380310231354,8.10216285005407,
27.1052282514291));
#164609=CARTESIAN_POINT('Ctrl Pts',(-0.728111953039665,8.09326935241919,
27.109338386292));
#164610=CARTESIAN_POINT('Ctrl Pts',(-0.870298382844737,8.07858611981485,
27.1148651873212));
#164611=CARTESIAN_POINT('Ctrl Pts',(-0.905936419142222,8.07466730935062,
27.1162547399789));
#164612=CARTESIAN_POINT('Ctrl Pts',(-0.964819738644798,8.0677976806562,
27.1185577271724));
#164613=CARTESIAN_POINT('Ctrl Pts',(-0.98808034573605,8.06498194477458,
27.119469304014));
#164614=CARTESIAN_POINT('Ctrl Pts',(-1.03308061725437,8.05933698299409,
27.1212363744053));
#164615=CARTESIAN_POINT('Ctrl Pts',(-1.05482167936488,8.05652030276375,
27.1220916838275));
#164616=CARTESIAN_POINT('Ctrl Pts',(-1.10387839432974,8.04996274411877,
27.1240253214184));
#164617=CARTESIAN_POINT('Ctrl Pts',(-1.13118691179693,8.04617075716757,
27.1251043311196));
#164618=CARTESIAN_POINT('Ctrl Pts',(-1.20115898269141,8.03609135975492,
27.1278760987031));
#164619=CARTESIAN_POINT('Ctrl Pts',(-1.24379261550845,8.02960317452887,
27.1295716503858));
#164620=CARTESIAN_POINT('Ctrl Pts',(-1.51488467816214,7.98613625647129,
27.1403989672989));
#164621=CARTESIAN_POINT('Ctrl Pts',(-1.74172001424296,7.93975148413848,
27.149670942605));
#164622=CARTESIAN_POINT('Ctrl Pts',(-2.00682782838697,7.87363179869951,
27.1608092369255));
#164623=CARTESIAN_POINT('Ctrl Pts',(-2.047316191557,7.86320113009674,27.1625186137577));
#164624=CARTESIAN_POINT('Ctrl Pts',(-2.3051200284098,7.7946591879031,27.1734561977457));
#164625=CARTESIAN_POINT('Ctrl Pts',(-2.52001834698053,7.72785824960592,
27.1828200523401));
#164626=CARTESIAN_POINT('Ctrl Pts',(-2.98688157013249,7.56118701341906,
27.2036689058034));
#164627=CARTESIAN_POINT('Ctrl Pts',(-3.2371873230016,7.45745438236957,27.2151868003348));
#164628=CARTESIAN_POINT('Ctrl Pts',(-3.79231845979541,7.19417028891366,
27.2412291812873));
#164629=CARTESIAN_POINT('Ctrl Pts',(-4.09315255536006,7.02736681955361,
27.2557088550449));
#164630=CARTESIAN_POINT('Ctrl Pts',(-4.40889166699642,6.82512578680511,
27.2708038404595));
#164631=CARTESIAN_POINT('Ctrl Pts',(-4.43515729151717,6.80808692409041,
27.2720586049615));
#164632=CARTESIAN_POINT('Ctrl Pts',(-4.47467627013302,6.78212467223915,
27.2739443986552));
#164633=CARTESIAN_POINT('Ctrl Pts',(-4.48800272424986,6.77331339475466,
27.2745799538916));
#164634=CARTESIAN_POINT('Ctrl Pts',(-4.51238662521907,6.75708751945513,
27.2757420712478));
#164635=CARTESIAN_POINT('Ctrl Pts',(-4.52345198869404,6.74968494890674,
27.2762691411422));
#164636=CARTESIAN_POINT('Ctrl Pts',(-4.54131252194983,6.73767285940162,
27.2771193444464));
#164637=CARTESIAN_POINT('Ctrl Pts',(-4.54811896228853,6.73308019318088,
27.2774432204508));
#164638=CARTESIAN_POINT('Ctrl Pts',(-4.5611486217632,6.72425961841571,27.2780629619965));
#164639=CARTESIAN_POINT('Ctrl Pts',(-4.56737295138885,6.72003336963871,
27.2783589020312));
#164640=CARTESIAN_POINT('Ctrl Pts',(-4.58148511281325,6.71042270895644,
27.2790296022601));
#164641=CARTESIAN_POINT('Ctrl Pts',(-4.58936934785459,6.70503301720098,
27.2794041181184));
#164642=CARTESIAN_POINT('Ctrl Pts',(-4.61316302846303,6.68870594140596,
27.280533737152));
#164643=CARTESIAN_POINT('Ctrl Pts',(-4.62904308012671,6.67772569580436,
27.2812868055664));
#164644=CARTESIAN_POINT('Ctrl Pts',(-4.7576487820478,6.58812221079325,27.2873777982892));
#164645=CARTESIAN_POINT('Ctrl Pts',(-4.86839034530911,6.50671594090737,
27.2925608167521));
#164646=CARTESIAN_POINT('Ctrl Pts',(-4.99147147059543,6.41133636953067,
27.2982785279222));
#164647=CARTESIAN_POINT('Ctrl Pts',(-5.0058778935764,6.40009437471773,27.2989472119939));
#164648=CARTESIAN_POINT('Ctrl Pts',(-5.61092787975708,5.92465326648763,
27.3270120174434));
#164649=CARTESIAN_POINT('Ctrl Pts',(-6.13442693929759,5.38080109036826,
27.3507781349952));
#164650=CARTESIAN_POINT('Ctrl Pts',(-6.79573746522483,4.46966211418129,
27.3898300812517));
#164651=CARTESIAN_POINT('Ctrl Pts',(-6.99447624571964,4.15177038423666,
27.4032933162527));
#164652=CARTESIAN_POINT('Ctrl Pts',(-7.19870656872638,3.76853931490387,
27.4198284025264));
#164653=CARTESIAN_POINT('Ctrl Pts',(-7.2262514353202,3.71544813539016,27.4221248696142));
#164654=CARTESIAN_POINT('Ctrl Pts',(-7.26101351622446,3.64659708039299,
27.4251116067529));
#164655=CARTESIAN_POINT('Ctrl Pts',(-7.26877023200484,3.63111096765797,
27.425783942505));
#164656=CARTESIAN_POINT('Ctrl Pts',(-7.28120825261779,3.60607916948017,
27.426871629301));
#164657=CARTESIAN_POINT('Ctrl Pts',(-7.28592045787562,3.59654885620008,
27.4272859571489));
#164658=CARTESIAN_POINT('Ctrl Pts',(-7.29487211906814,3.57835456129404,
27.4280773661577));
#164659=CARTESIAN_POINT('Ctrl Pts',(-7.29911488066169,3.56969222175066,
27.4284543372659));
#164660=CARTESIAN_POINT('Ctrl Pts',(-7.30876951807077,3.5498914135657,27.4293164532751));
#164661=CARTESIAN_POINT('Ctrl Pts',(-7.31417136874242,3.53874809832885,
27.4298019273731));
#164662=CARTESIAN_POINT('Ctrl Pts',(-7.32813960755549,3.50976482143206,
27.4310654187901));
#164663=CARTESIAN_POINT('Ctrl Pts',(-7.3366663075571,3.49190588281732,27.4318447381637));
#164664=CARTESIAN_POINT('Ctrl Pts',(-7.38873996604644,3.38180631413665,
27.4366541301956));
#164665=CARTESIAN_POINT('Ctrl Pts',(-7.43061099778543,3.28878571923863,
27.4407388400703));
#164666=CARTESIAN_POINT('Ctrl Pts',(-7.75767053821409,2.52403855201772,
27.4745072055012));
#164667=CARTESIAN_POINT('Ctrl Pts',(-7.9528870064651,1.81755562707462,27.507247877958));
#164668=CARTESIAN_POINT('Ctrl Pts',(-8.12210712489587,0.572953983549243,
27.5638672130948));
#164669=CARTESIAN_POINT('Ctrl Pts',(-8.14217491902688,0.0454953328315635,
27.5874015854159));
#164670=CARTESIAN_POINT('Ctrl Pts',(-8.10938784797166,-0.508233392943172,
27.6095964057986));
#164671=CARTESIAN_POINT('Ctrl Pts',(-8.10758724064435,-0.536191770245362,
27.6107107550455));
#164672=CARTESIAN_POINT('Ctrl Pts',(-8.10489077804785,-0.574934884158393,
27.6122469003449));
#164673=CARTESIAN_POINT('Ctrl Pts',(-8.1041179426227,-0.585727768445667,
27.6126739656274));
#164674=CARTESIAN_POINT('Ctrl Pts',(-8.10277432282676,-0.603979968090866,
27.6133947691628));
#164675=CARTESIAN_POINT('Ctrl Pts',(-8.10221479345928,-0.611440078558552,
27.613688977288));
#164676=CARTESIAN_POINT('Ctrl Pts',(-8.10108498479843,-0.626229733087682,
27.6142714660751));
#164677=CARTESIAN_POINT('Ctrl Pts',(-8.10051505942049,-0.633559296434201,
27.6145597609602));
#164678=CARTESIAN_POINT('Ctrl Pts',(-8.09923369186252,-0.64975400234305,
27.6151959309906));
#164679=CARTESIAN_POINT('Ctrl Pts',(-8.0985176399946,-0.658618777795756,
27.6155436199414));
#164680=CARTESIAN_POINT('Ctrl Pts',(-8.09594888310631,-0.689782516011133,
27.6167640511219));
#164681=CARTESIAN_POINT('Ctrl Pts',(-8.09401861259611,-0.712075100314758,
27.6176337322592));
#164682=CARTESIAN_POINT('Ctrl Pts',(-8.06056871702522,-1.08066352035856,
27.631961831488));
#164683=CARTESIAN_POINT('Ctrl Pts',(-8.00694071291827,-1.42461627342084,
27.64460283728));
#164684=CARTESIAN_POINT('Ctrl Pts',(-7.80410019677652,-2.33659714835224,
27.6782068451738));
#164685=CARTESIAN_POINT('Ctrl Pts',(-7.61515768913519,-2.89362100891587,
27.6989790456875));
#164686=CARTESIAN_POINT('Ctrl Pts',(-7.19726980372854,-3.79246742956814,
27.7359392296924));
#164687=CARTESIAN_POINT('Ctrl Pts',(-6.99945863165327,-4.14621004875965,
27.7514187267339));
#164688=CARTESIAN_POINT('Ctrl Pts',(-6.72293651233366,-4.56411039903529,
27.7708154654909));
#164689=CARTESIAN_POINT('Ctrl Pts',(-6.66831862798011,-4.64354450432267,
27.7745586408029));
#164690=CARTESIAN_POINT('Ctrl Pts',(-6.58496682574687,-4.7602638243464,
27.7801493908441));
#164691=CARTESIAN_POINT('Ctrl Pts',(-6.55730118086169,-4.79830188425201,
27.7819860466356));
#164692=CARTESIAN_POINT('Ctrl Pts',(-6.50696372714352,-4.86626343498263,
27.7852947973815));
#164693=CARTESIAN_POINT('Ctrl Pts',(-6.48441181170715,-4.89627411490688,
27.7867656005553));
#164694=CARTESIAN_POINT('Ctrl Pts',(-6.43567861521451,-4.9601979584752,
27.7899197615014));
#164695=CARTESIAN_POINT('Ctrl Pts',(-6.40943545064592,-4.99406249561231,
27.7916037449566));
#164696=CARTESIAN_POINT('Ctrl Pts',(-6.3378632442213,-5.08492679980873,
27.7961581829827));
#164697=CARTESIAN_POINT('Ctrl Pts',(-6.29203384723242,-5.14152711074746,
27.799033998337));
#164698=CARTESIAN_POINT('Ctrl Pts',(-5.99821214250416,-5.49459061357686,
27.8172264317339));
#164699=CARTESIAN_POINT('Ctrl Pts',(-5.73009656858327,-5.77365189297787,
27.832768219621));
#164700=CARTESIAN_POINT('Ctrl Pts',(-5.14353717392916,-6.30290102227069,
27.8648101494429));
#164701=CARTESIAN_POINT('Ctrl Pts',(-4.82420207667574,-6.55054297964778,
27.8812774526664));
#164702=CARTESIAN_POINT('Ctrl Pts',(-4.41674766685772,-6.82050516829263,
27.9009137496598));
#164703=CARTESIAN_POINT('Ctrl Pts',(-4.34496580950138,-6.86645636620171,
27.9043242744606));
#164704=CARTESIAN_POINT('Ctrl Pts',(-4.22265342038315,-6.94206858780283,
27.9100486955717));
#164705=CARTESIAN_POINT('Ctrl Pts',(-4.17250108294612,-6.97232765909977,
27.9123718045247));
#164706=CARTESIAN_POINT('Ctrl Pts',(-4.10114935210433,-7.01433164383792,
27.9156414667269));
#164707=CARTESIAN_POINT('Ctrl Pts',(-4.08021813137192,-7.02652790681888,
27.9165963708055));
#164708=CARTESIAN_POINT('Ctrl Pts',(-4.04323572380125,-7.04785594740855,
27.9182759147257));
#164709=CARTESIAN_POINT('Ctrl Pts',(-4.02720739490974,-7.05702693593348,
27.9190013218911));
#164710=CARTESIAN_POINT('Ctrl Pts',(-3.99220086276577,-7.07689865010142,
27.9205803813758));
#164711=CARTESIAN_POINT('Ctrl Pts',(-3.97321058477317,-7.08757785749688,
27.9214336347637));
#164712=CARTESIAN_POINT('Ctrl Pts',(-3.92014615948622,-7.11713841266393,
27.9238089858409));
#164713=CARTESIAN_POINT('Ctrl Pts',(-3.88597875257644,-7.13585133350465,
27.9253282706055));
#164714=CARTESIAN_POINT('Ctrl Pts',(-3.64082767774847,-7.26783358683459,
27.9361628959527));
#164715=CARTESIAN_POINT('Ctrl Pts',(-3.42505979414316,-7.37197390206753,
27.9453547448434));
#164716=CARTESIAN_POINT('Ctrl Pts',(-2.9794540121391,-7.56325254263238,
27.9639950109622));
#164717=CARTESIAN_POINT('Ctrl Pts',(-2.74963268203394,-7.64980090504412,
27.9734350185419));
#164718=CARTESIAN_POINT('Ctrl Pts',(-2.46205071714114,-7.74346451913729,
27.9851771251564));
#164719=CARTESIAN_POINT('Ctrl Pts',(-2.40766934727779,-7.76054539113466,
27.9873942076133));
#164720=CARTESIAN_POINT('Ctrl Pts',(-2.31751997807577,-7.78782200307736,
27.9910654727267));
#164721=CARTESIAN_POINT('Ctrl Pts',(-2.28185359621469,-7.79834691163931,
27.9925169155283));
#164722=CARTESIAN_POINT('Ctrl Pts',(-2.21181835834764,-7.8184922326294,
27.9953653380202));
#164723=CARTESIAN_POINT('Ctrl Pts',(-2.17745586629732,-7.82813178107578,
27.9967621253935));
#164724=CARTESIAN_POINT('Ctrl Pts',(-2.10163323537106,-7.84886407170304,
27.999842802647));
#164725=CARTESIAN_POINT('Ctrl Pts',(-2.06014648992588,-7.85985533543133,
28.0015274908302));
#164726=CARTESIAN_POINT('Ctrl Pts',(-1.91599931605334,-7.89682518466611,
28.0073784373591));
#164727=CARTESIAN_POINT('Ctrl Pts',(-1.81292006381937,-7.92112504377917,
28.0115581179478));
#164728=CARTESIAN_POINT('Ctrl Pts',(-1.53134671696038,-7.98171876310866,
28.0229662656647));
#164729=CARTESIAN_POINT('Ctrl Pts',(-1.35206085761498,-8.01403691720267,
28.0302214412698));
#164730=CARTESIAN_POINT('Ctrl Pts',(-0.972042837407182,-8.06942302788869,
28.0455550208727));
#164731=CARTESIAN_POINT('Ctrl Pts',(-0.771227236737414,-8.0910854753154,
28.0536323662989));
#164732=CARTESIAN_POINT('Ctrl Pts',(-0.50454617565077,-8.10983363424549,
28.0642625999318));
#164733=CARTESIAN_POINT('Ctrl Pts',(-0.439225678494732,-8.11363354456344,
28.0668584888699));
#164734=CARTESIAN_POINT('Ctrl Pts',(-0.327234461611584,-8.11879204678575,
28.0712917005822));
#164735=CARTESIAN_POINT('Ctrl Pts',(-0.280584910102654,-8.12053808789684,
28.0731331638217));
#164736=CARTESIAN_POINT('Ctrl Pts',(-0.211503752198051,-8.12252773170449,
28.0758510581416));
#164737=CARTESIAN_POINT('Ctrl Pts',(-0.189082199637715,-8.12308060513052,
28.0767317654798));
#164738=CARTESIAN_POINT('Ctrl Pts',(-0.146857455740234,-8.1239468669636,
28.0783875900045));
#164739=CARTESIAN_POINT('Ctrl Pts',(-0.127054935295905,-8.12428069776725,
28.079163028899));
#164740=CARTESIAN_POINT('Ctrl Pts',(-0.0815579675385686,-8.12488129916687,
28.0809422912167));
#164741=CARTESIAN_POINT('Ctrl Pts',(-0.0558630553067464,-8.12509859343093,
28.0819454385214));
#164742=CARTESIAN_POINT('Ctrl Pts',(0.0123321803156192,-8.12535179092587,
28.0846038109864));
#164743=CARTESIAN_POINT('Ctrl Pts',(0.0548325785432046,-8.12517613483883,
28.0862564136738));
#164744=CARTESIAN_POINT('Ctrl Pts',(0.466865940851603,-8.12024016437,28.102246367865));
#164745=CARTESIAN_POINT('Ctrl Pts',(0.835673724279217,-8.09060689178403,
28.1163289610305));
#164746=CARTESIAN_POINT('Ctrl Pts',(1.36171559170572,-8.01197630593596,
28.1367427278862));
#164747=CARTESIAN_POINT('Ctrl Pts',(1.52149108235116,-7.98317593955166,
28.1429844969318));
#164748=CARTESIAN_POINT('Ctrl Pts',(1.8294569047133,-7.91808171486078,28.1551434116098));
#164749=CARTESIAN_POINT('Ctrl Pts',(1.97770007846394,-7.88236210945986,
28.1610547662165));
#164750=CARTESIAN_POINT('Ctrl Pts',(2.19036474760366,-7.82474262670952,
28.169637768838));
#164751=CARTESIAN_POINT('Ctrl Pts',(2.25565481629169,-7.80617167365945,
28.1722869295281));
#164752=CARTESIAN_POINT('Ctrl Pts',(2.37253447944986,-7.77133789514597,
28.1770558060398));
#164753=CARTESIAN_POINT('Ctrl Pts',(2.42420899652686,-7.75537383063506,
28.1791735847055));
#164754=CARTESIAN_POINT('Ctrl Pts',(2.53919588065115,-7.71858881878494,
28.1839074247384));
#164755=CARTESIAN_POINT('Ctrl Pts',(2.60241921002566,-7.69750240586071,
28.1865247984051));
#164756=CARTESIAN_POINT('Ctrl Pts',(2.8201751190918,-7.62188639411661,28.1955902793935));
#164757=CARTESIAN_POINT('Ctrl Pts',(2.97331235408543,-7.56346172097323,
28.2020551993836));
#164758=CARTESIAN_POINT('Ctrl Pts',(3.23082771049877,-7.45618455648439,
28.2130687196345));
#164759=CARTESIAN_POINT('Ctrl Pts',(3.33612557796847,-7.40966949471904,
28.2176136158665));
#164760=CARTESIAN_POINT('Ctrl Pts',(3.47248339557143,-7.34593771105184,
28.2235467158364));
#164761=CARTESIAN_POINT('Ctrl Pts',(3.50446870106782,-7.33073263158408,
28.2249418982325));
#164762=CARTESIAN_POINT('Ctrl Pts',(3.5842138529842,-7.2921824249444,28.2284285133474));
#164763=CARTESIAN_POINT('Ctrl Pts',(3.63184600546289,-7.26857675760056,
28.2305184755822));
#164764=CARTESIAN_POINT('Ctrl Pts',(3.71493708460978,-7.22637756351334,
28.2341759286306));
#164765=CARTESIAN_POINT('Ctrl Pts',(3.75049648094866,-7.20798629212294,
28.2357447932639));
#164766=CARTESIAN_POINT('Ctrl Pts',(3.83724572913597,-7.16230394572566,
28.2395821513508));
#164767=CARTESIAN_POINT('Ctrl Pts',(3.88828200788044,-7.1347260391798,28.24184851559));
#164768=CARTESIAN_POINT('Ctrl Pts',(4.10309923676867,-7.01565804426127,
28.2514335021144));
#164769=CARTESIAN_POINT('Ctrl Pts',(4.26398113862629,-6.91905674564863,
28.258726457263));
#164770=CARTESIAN_POINT('Ctrl Pts',(4.4726074431752,-6.78374521170415,28.2684128602265));
#164771=CARTESIAN_POINT('Ctrl Pts',(4.5234634679115,-6.74994034615889,28.2707926744326));
#164772=CARTESIAN_POINT('Ctrl Pts',(4.64547231913918,-6.66684080992021,
28.2765511623152));
#164773=CARTESIAN_POINT('Ctrl Pts',(4.71622778047766,-6.61697626587097,
28.2799317551831));
#164774=CARTESIAN_POINT('Ctrl Pts',(4.83167103075533,-6.53282577637391,
28.2855223450995));
#164775=CARTESIAN_POINT('Ctrl Pts',(4.87682315933426,-6.49918867405571,
28.2877283381414));
#164776=CARTESIAN_POINT('Ctrl Pts',(4.96265729005221,-6.43384643404949,
28.2919610396371));
#164777=CARTESIAN_POINT('Ctrl Pts',(5.00339420700395,-6.40221787375495,
28.2939871429361));
#164778=CARTESIAN_POINT('Ctrl Pts',(5.11385160527922,-6.31475944197586,
28.2995299029359));
#164779=CARTESIAN_POINT('Ctrl Pts',(5.1829568059752,-6.25816456147672,28.3030518812139));
#164780=CARTESIAN_POINT('Ctrl Pts',(5.60382535447295,-5.9017336896606,28.3248545362757));
#164781=CARTESIAN_POINT('Ctrl Pts',(5.93040213901739,-5.57347630803897,
28.3433769084533));
#164782=CARTESIAN_POINT('Ctrl Pts',(6.30944676719428,-5.12122325539886,
28.3669641391104));
#164783=CARTESIAN_POINT('Ctrl Pts',(6.3892781368325,-5.02127188926251,28.3720659022832));
#164784=CARTESIAN_POINT('Ctrl Pts',(6.49914872931917,-4.87684556159425,
28.3792682256689));
#164785=CARTESIAN_POINT('Ctrl Pts',(6.5311580874893,-4.83389397054078,28.3813895356861));
#164786=CARTESIAN_POINT('Ctrl Pts',(6.58728506909712,-4.75700493840835,
28.3851489230498));
#164787=CARTESIAN_POINT('Ctrl Pts',(6.61157096589775,-4.72319277124167,
28.3867892883353));
#164788=CARTESIAN_POINT('Ctrl Pts',(6.6488853105583,-4.67038991291695,28.3893304012743));
#164789=CARTESIAN_POINT('Ctrl Pts',(6.66209462314542,-4.65152803375784,
28.3902340900905));
#164790=CARTESIAN_POINT('Ctrl Pts',(6.68642112081441,-4.61647548153039,
28.3919058846795));
#164791=CARTESIAN_POINT('Ctrl Pts',(6.69756012531071,-4.60030016929301,
28.3926743730259));
#164792=CARTESIAN_POINT('Ctrl Pts',(6.722772751041,-4.56340241229061,28.3944205045569));
#164793=CARTESIAN_POINT('Ctrl Pts',(6.73680939544143,-4.54265497380317,
28.3953974031079));
#164794=CARTESIAN_POINT('Ctrl Pts',(6.78317025027726,-4.473441924763,28.39864063697));
#164795=CARTESIAN_POINT('Ctrl Pts',(6.81506931242188,-4.42469339469146,
28.4008995542559));
#164796=CARTESIAN_POINT('Ctrl Pts',(6.98445764197613,-4.15965414156242,
28.4130601179966));
#164797=CARTESIAN_POINT('Ctrl Pts',(7.11218039061369,-3.93729142326717,
28.4228380667149));
#164798=CARTESIAN_POINT('Ctrl Pts',(7.30652765221472,-3.55851765458915,
28.4391348646639));
#164799=CARTESIAN_POINT('Ctrl Pts',(7.37913997443588,-3.405390860543,28.4456296473036));
#164800=CARTESIAN_POINT('Ctrl Pts',(7.49144533363264,-3.14806760404676,
28.4564546324736));
#164801=CARTESIAN_POINT('Ctrl Pts',(7.53387679643335,-3.04512445606553,
28.4607619721768));
#164802=CARTESIAN_POINT('Ctrl Pts',(7.59125404797554,-2.89737369857054,
28.4669215266301));
#164803=CARTESIAN_POINT('Ctrl Pts',(7.6079455888539,-2.85325713217651,28.4687578283302));
#164804=CARTESIAN_POINT('Ctrl Pts',(7.63650475067113,-2.77574114322045,
28.4719800059662));
#164805=CARTESIAN_POINT('Ctrl Pts',(7.64853974281833,-2.74240469168815,
28.4733643369791));
#164806=CARTESIAN_POINT('Ctrl Pts',(7.67162880007682,-2.67711454237781,
28.4760731019836));
#164807=CARTESIAN_POINT('Ctrl Pts',(7.68270229199834,-2.64516846389922,
28.4773973333898));
#164808=CARTESIAN_POINT('Ctrl Pts',(7.71249874957965,-2.55744256295543,
28.481030830821));
#164809=CARTESIAN_POINT('Ctrl Pts',(7.73081568842897,-2.50152716734897,
28.4833435660064));
#164810=CARTESIAN_POINT('Ctrl Pts',(7.84458081642091,-2.14105227149758,
28.4982342846135));
#164811=CARTESIAN_POINT('Ctrl Pts',(7.92262000226991,-1.83129465904164,
28.5109599042098));
#164812=CARTESIAN_POINT('Ctrl Pts',(8.00407540433138,-1.4029016608351,28.5283499277034));
#164813=CARTESIAN_POINT('Ctrl Pts',(8.02343271857365,-1.28758834492242,
28.5330085806917));
#164814=CARTESIAN_POINT('Ctrl Pts',(8.05037215295286,-1.10275899651597,
28.5404225416406));
#164815=CARTESIAN_POINT('Ctrl Pts',(8.05955711371782,-1.0334933140502,28.5431890497934));
#164816=CARTESIAN_POINT('Ctrl Pts',(8.07103589264158,-0.937437553376661,
28.5470050190817));
#164817=CARTESIAN_POINT('Ctrl Pts',(8.07409182211956,-0.910741896416319,
28.5480633507946));
#164818=CARTESIAN_POINT('Ctrl Pts',(8.07908818026832,-0.865092323177715,
28.5498690303063));
#164819=CARTESIAN_POINT('Ctrl Pts',(8.08109446338499,-0.846145867366758,
28.5506172656255));
#164820=CARTESIAN_POINT('Ctrl Pts',(8.0848174206114,-0.809766438884356,
28.5520515383226));
#164821=CARTESIAN_POINT('Ctrl Pts',(8.08654438942083,-0.792334683167217,
28.5527377083982));
#164822=CARTESIAN_POINT('Ctrl Pts',(8.09129691783765,-0.742728797868847,
28.5546872951811));
#164823=CARTESIAN_POINT('Ctrl Pts',(8.09418692505041,-0.710541987581968,
28.555948666698));
#164824=CARTESIAN_POINT('Ctrl Pts',(8.106246228188,-0.566597980644516,28.5615750224486));
#164825=CARTESIAN_POINT('Ctrl Pts',(8.11329358806528,-0.4546743959761,28.5659103248057));
#164826=CARTESIAN_POINT('Ctrl Pts',(8.12284980933912,-0.228262882292652,
28.5746280449117));
#164827=CARTESIAN_POINT('Ctrl Pts',(8.12525961307267,-0.113795904479086,
28.5790085855748));
#164828=CARTESIAN_POINT('Ctrl Pts',(8.12521102066998,0.463152093692499,
28.601021137259));
#164829=CARTESIAN_POINT('Ctrl Pts',(8.08568865389865,0.924772151804552,
28.6184464143668));
#164830=CARTESIAN_POINT('Ctrl Pts',(8.00536840890349,1.39063642197348,28.6365482129313));
#164831=CARTESIAN_POINT('Ctrl Pts',(8.00360443074266,1.40075306046991,28.6369415453282));
#164832=CARTESIAN_POINT('Ctrl Pts',(7.96184204248208,1.63761119612558,28.6461561966252));
#164833=CARTESIAN_POINT('Ctrl Pts',(7.91224357422852,1.86255160589202,28.6550310951516));
#164834=CARTESIAN_POINT('Ctrl Pts',(7.83600451298075,2.14969542757179,28.6665813468389));
#164835=CARTESIAN_POINT('Ctrl Pts',(7.81805157199845,2.21409726869623,28.6691863202413));
#164836=CARTESIAN_POINT('Ctrl Pts',(7.78776634404721,2.31777407639103,28.6734044642257));
#164837=CARTESIAN_POINT('Ctrl Pts',(7.77592678247158,2.35718984349811,28.6750138895457));
#164838=CARTESIAN_POINT('Ctrl Pts',(7.7526120905646,2.43272052754385,28.6781093266258));
#164839=CARTESIAN_POINT('Ctrl Pts',(7.74118276003807,2.46884848805137,28.6795949694409));
#164840=CARTESIAN_POINT('Ctrl Pts',(7.71405078779952,2.55257119964036,28.6830496825253));
#164841=CARTESIAN_POINT('Ctrl Pts',(7.69815968689519,2.60010320902206,28.6850200116938));
#164842=CARTESIAN_POINT('Ctrl Pts',(7.64463098638386,2.75541980784102,28.6914882772974));
#164843=CARTESIAN_POINT('Ctrl Pts',(7.60516155718549,2.86255806637339,28.6959978278142));
#164844=CARTESIAN_POINT('Ctrl Pts',(7.33791660138649,3.54339675670948,28.7249662376889));
#164845=CARTESIAN_POINT('Ctrl Pts',(7.04766185027582,4.0903663112696,28.7496957152889));
#164846=CARTESIAN_POINT('Ctrl Pts',(6.45944286310693,4.94705511114485,28.7931144107963));
#164847=CARTESIAN_POINT('Ctrl Pts',(6.19385696125358,5.275782263275,28.8111156805866));
#164848=CARTESIAN_POINT('Ctrl Pts',(5.71598457986253,5.78118122759725,28.8403510712852));
#164849=CARTESIAN_POINT('Ctrl Pts',(5.51809146173939,5.97036135413446,28.8517051509626));
#164850=CARTESIAN_POINT('Ctrl Pts',(5.29418462694404,6.16374820111944,28.8634750693944));
#164851=CARTESIAN_POINT('Ctrl Pts',(5.277283863633,6.17822448485748,28.8643571240423));
#164852=CARTESIAN_POINT('Ctrl Pts',(5.25356075648793,6.19837605194243,28.8655861292096));
#164853=CARTESIAN_POINT('Ctrl Pts',(5.24678834445119,6.20410979695755,28.8659359505329));
#164854=CARTESIAN_POINT('Ctrl Pts',(5.23439196275649,6.21457016310033,28.8665743666754));
#164855=CARTESIAN_POINT('Ctrl Pts',(5.22877095432844,6.21930026928137,28.8668631364096));
#164856=CARTESIAN_POINT('Ctrl Pts',(5.21740837017732,6.22883564699329,28.8674454176526));
#164857=CARTESIAN_POINT('Ctrl Pts',(5.21166655141813,6.23364061971493,28.8677389138479));
#164858=CARTESIAN_POINT('Ctrl Pts',(5.19758784069716,6.24538917260404,28.8684567120695));
#164859=CARTESIAN_POINT('Ctrl Pts',(5.18924365225288,6.25232401576301,28.8688805594446));
#164860=CARTESIAN_POINT('Ctrl Pts',(5.15915754422196,6.27722682018807,28.8704030486156));
#164861=CARTESIAN_POINT('Ctrl Pts',(5.13733582630375,6.29509839107362,28.8714965461627));
#164862=CARTESIAN_POINT('Ctrl Pts',(5.01894054955742,6.39103622174745,28.877369303994));
#164863=CARTESIAN_POINT('Ctrl Pts',(4.92068219428892,6.46699271945491,28.8820202432015));
#164864=CARTESIAN_POINT('Ctrl Pts',(4.71942037264646,6.61533029714115,28.8911644107891));
#164865=CARTESIAN_POINT('Ctrl Pts',(4.61639694108509,6.68763071607416,28.8956554097436));
#164866=CARTESIAN_POINT('Ctrl Pts',(4.26847342695982,6.91992602048347,28.9103214262475));
#164867=CARTESIAN_POINT('Ctrl Pts',(4.0166133158609,7.06909255233249,28.9201411925925));
#164868=CARTESIAN_POINT('Ctrl Pts',(3.51428889040444,7.33106731651561,28.9390562081445));
#164869=CARTESIAN_POINT('Ctrl Pts',(3.26507238246662,7.44540630423332,28.9481470197449));
#164870=CARTESIAN_POINT('Ctrl Pts',(2.52446722262292,7.74084220411182,28.9751721474256));
#164871=CARTESIAN_POINT('Ctrl Pts',(2.02083344357673,7.88731448636748,28.9936397925508));
#164872=CARTESIAN_POINT('Ctrl Pts',(1.47462488986316,7.99038362122887,29.0150067851694));
#164873=CARTESIAN_POINT('Ctrl Pts',(1.44257465548439,7.99623206981226,29.0162649372631));
#164874=CARTESIAN_POINT('Ctrl Pts',(1.39801453120897,8.00408666961414,29.0180204303382));
#164875=CARTESIAN_POINT('Ctrl Pts',(1.3855336388237,8.00625658957524,29.0185128085441));
#164876=CARTESIAN_POINT('Ctrl Pts',(1.36403799224707,8.00994203975643,29.019362005657));
#164877=CARTESIAN_POINT('Ctrl Pts',(1.35502564545496,8.01147156420298,29.019718400564));
#164878=CARTESIAN_POINT('Ctrl Pts',(1.33642812901512,8.0145955503846,29.0204545843139));
#164879=CARTESIAN_POINT('Ctrl Pts',(1.32684264353852,8.01618803289866,29.0208344323483));
#164880=CARTESIAN_POINT('Ctrl Pts',(1.30453879500382,8.01985237670853,29.0217192265081));
#164881=CARTESIAN_POINT('Ctrl Pts',(1.29181833020364,8.02191118199211,29.0222245658597));
#164882=CARTESIAN_POINT('Ctrl Pts',(1.25132490918671,8.02836622222461,29.0238355295637));
#164883=CARTESIAN_POINT('Ctrl Pts',(1.22353414386686,8.03264852996908,29.0249445838759));
#164884=CARTESIAN_POINT('Ctrl Pts',(0.685409459483516,8.11271130881777,
29.0464872510533));
#164885=CARTESIAN_POINT('Ctrl Pts',(0.16909180260856,8.13985034632006,29.0684338652075));
#164886=CARTESIAN_POINT('Ctrl Pts',(-1.12268337179519,8.08475129161273,
29.1256504133413));
#164887=CARTESIAN_POINT('Ctrl Pts',(-1.89037985788163,7.94041817319647,
29.1618853402616));
#164888=CARTESIAN_POINT('Ctrl Pts',(-2.66449371428447,7.67605521460815,
29.1949045500488));
#164889=CARTESIAN_POINT('Ctrl Pts',(-2.70298428075024,7.66258614799331,
29.1965367723628));
#164890=CARTESIAN_POINT('Ctrl Pts',(-2.75397260883419,7.64431171487656,
29.1986880105995));
#164891=CARTESIAN_POINT('Ctrl Pts',(-2.76656178358605,7.63976456606172,
29.1992182662749));
#164892=CARTESIAN_POINT('Ctrl Pts',(-2.78613575088601,7.6326398165577,29.2000414050681));
#164893=CARTESIAN_POINT('Ctrl Pts',(-2.79312829941951,7.63008370171299,
29.2003351989473));
#164894=CARTESIAN_POINT('Ctrl Pts',(-2.80715708602389,7.62493363208737,
29.2009241124625));
#164895=CARTESIAN_POINT('Ctrl Pts',(-2.81419326540717,7.62233954011127,
29.201219225934));
#164896=CARTESIAN_POINT('Ctrl Pts',(-2.82994463512915,7.61650755678943,
29.2018793149002));
#164897=CARTESIAN_POINT('Ctrl Pts',(-2.83865788809669,7.61326443753016,
29.2022440749804));
#164898=CARTESIAN_POINT('Ctrl Pts',(-2.86429221991598,7.60367307708203,
29.2033161105881));
#164899=CARTESIAN_POINT('Ctrl Pts',(-2.88119776670928,7.59728330520904,
29.2040217108194));
#164900=CARTESIAN_POINT('Ctrl Pts',(-3.01217327747922,7.54727857530014,
29.2094783821334));
#164901=CARTESIAN_POINT('Ctrl Pts',(-3.12527129844734,7.50115208856428,
29.2141317423543));
#164902=CARTESIAN_POINT('Ctrl Pts',(-3.53580528194383,7.32282017330772,
29.2309299066784));
#164903=CARTESIAN_POINT('Ctrl Pts',(-3.82627153629619,7.17532405638642,
29.2426446485696));
#164904=CARTESIAN_POINT('Ctrl Pts',(-4.31543381568048,6.8887596004457,29.2630060607293));
#164905=CARTESIAN_POINT('Ctrl Pts',(-4.51820929001019,6.75749670778909,
29.2716508204654));
#164906=CARTESIAN_POINT('Ctrl Pts',(-5.08240585990947,6.35551184511476,
29.296756307632));
#164907=CARTESIAN_POINT('Ctrl Pts',(-5.42749549566616,6.0634678165698,29.3134814424705));
#164908=CARTESIAN_POINT('Ctrl Pts',(-5.7848942471704,5.70592928095342,29.332935832273));
#164909=CARTESIAN_POINT('Ctrl Pts',(-5.82286047651229,5.66717974098427,
29.335031290318));
#164910=CARTESIAN_POINT('Ctrl Pts',(-5.87963071255195,5.60806546012648,
29.3382086166792));
#164911=CARTESIAN_POINT('Ctrl Pts',(-5.89872337734747,5.58797978077181,
29.3392848790092));
#164912=CARTESIAN_POINT('Ctrl Pts',(-5.9327476148363,5.55181724244866,29.3412166510521));
#164913=CARTESIAN_POINT('Ctrl Pts',(-5.94771756131865,5.53577679831917,
29.3420714440379));
#164914=CARTESIAN_POINT('Ctrl Pts',(-5.97849766343348,5.50252663583306,
29.3438390733126));
#164915=CARTESIAN_POINT('Ctrl Pts',(-5.99429893409404,5.4853089223439,29.3447520714455));
#164916=CARTESIAN_POINT('Ctrl Pts',(-6.03396036557016,5.44171616360803,
29.3470580380991));
#164917=CARTESIAN_POINT('Ctrl Pts',(-6.05772198679256,5.41525223891945,
29.3484527918219));
#164918=CARTESIAN_POINT('Ctrl Pts',(-6.15203517129034,5.3088156730309,29.354043148718));
#164919=CARTESIAN_POINT('Ctrl Pts',(-6.22118216425379,5.22761442220968,
29.3582651676087));
#164920=CARTESIAN_POINT('Ctrl Pts',(-6.80567378490065,4.51320361615728,
29.3950979085542));
#164921=CARTESIAN_POINT('Ctrl Pts',(-7.22443059655724,3.80703759476793,
29.4301046632004));
#164922=CARTESIAN_POINT('Ctrl Pts',(-7.62326116974548,2.82243334289596,
29.4747026127156));
#164923=CARTESIAN_POINT('Ctrl Pts',(-7.70524212450984,2.59026915961201,
29.4848865695197));
#164924=CARTESIAN_POINT('Ctrl Pts',(-7.78318193915348,2.3328712572935,29.4956110856699));
#164925=CARTESIAN_POINT('Ctrl Pts',(-7.78970998080644,2.31097984159077,
29.4965187558656));
#164926=CARTESIAN_POINT('Ctrl Pts',(-7.79874055977998,2.28022325313414,
29.4977875307137));
#164927=CARTESIAN_POINT('Ctrl Pts',(-7.80132044440041,2.27138101768604,
29.4981515434644));
#164928=CARTESIAN_POINT('Ctrl Pts',(-7.80601993237078,2.25517164417241,
29.4988174510952));
#164929=CARTESIAN_POINT('Ctrl Pts',(-7.80814415421196,2.24780586278804,
29.4991195235741));
#164930=CARTESIAN_POINT('Ctrl Pts',(-7.81242352858224,2.23288778356903,
29.4997302396844));
#164931=CARTESIAN_POINT('Ctrl Pts',(-7.81457816211327,2.22533534387853,
29.5000388627305));
#164932=CARTESIAN_POINT('Ctrl Pts',(-7.81984873202484,2.2067588470496,29.500796582186));
#164933=CARTESIAN_POINT('Ctrl Pts',(-7.82295231613081,2.19573128183345,
29.501245184032));
#164934=CARTESIAN_POINT('Ctrl Pts',(-7.8341537878458,2.15560531637361,29.5028730542717));
#164935=CARTESIAN_POINT('Ctrl Pts',(-7.84211279282706,2.12646815838037,
29.5040466078946));
#164936=CARTESIAN_POINT('Ctrl Pts',(-7.8858527837557,1.96275429835592,29.5105904225291));
#164937=CARTESIAN_POINT('Ctrl Pts',(-7.91833107552188,1.82732355530139,
29.51580195099));
#164938=CARTESIAN_POINT('Ctrl Pts',(-7.96649898867044,1.60096170895218,
29.5242446944981));
#164939=CARTESIAN_POINT('Ctrl Pts',(-7.98414908105906,1.51047960836138,
29.5275507328029));
#164940=CARTESIAN_POINT('Ctrl Pts',(-8.08425921209319,0.946347628245944,
29.5478272988772));
#164941=CARTESIAN_POINT('Ctrl Pts',(-8.12608706747604,0.46644102575913,
29.5636522508804));
#164942=CARTESIAN_POINT('Ctrl Pts',(-8.1242080640507,-0.596718045028775,
29.5996011020268));
#164943=CARTESIAN_POINT('Ctrl Pts',(-8.06057789846687,-1.17721256102332,
29.6199016716797));
#164944=CARTESIAN_POINT('Ctrl Pts',(-7.92771808430967,-1.78108723528828,
29.643640451902));
#164945=CARTESIAN_POINT('Ctrl Pts',(-7.91974216599924,-1.8162240359905,
29.6450307567085));
#164946=CARTESIAN_POINT('Ctrl Pts',(-7.90852037216439,-1.86418022113962,
29.6469409461985));
#164947=CARTESIAN_POINT('Ctrl Pts',(-7.90547646707857,-1.87704666972729,
29.6474546893532));
#164948=CARTESIAN_POINT('Ctrl Pts',(-7.90024023726166,-1.89894130233668,
29.6483310565548));
#164949=CARTESIAN_POINT('Ctrl Pts',(-7.89806380357127,-1.90797327816207,
29.6486931961492));
#164950=CARTESIAN_POINT('Ctrl Pts',(-7.89382236300144,-1.92544320276013,
29.6493948640573));
#164951=CARTESIAN_POINT('Ctrl Pts',(-7.89175930487326,-1.93388161454557,
29.6497343325644));
#164952=CARTESIAN_POINT('Ctrl Pts',(-7.88682861868789,-1.95391004238932,
29.6505413555836));
#164953=CARTESIAN_POINT('Ctrl Pts',(-7.88394897285358,-1.96549706341457,
29.6510092764643));
#164954=CARTESIAN_POINT('Ctrl Pts',(-7.87536771534645,-1.99970374506789,
29.6523937249784));
#164955=CARTESIAN_POINT('Ctrl Pts',(-7.86959424304695,-2.02230515966519,
29.6533124476196));
#164956=CARTESIAN_POINT('Ctrl Pts',(-7.82346080321223,-2.19971429328974,
29.6605554698521));
#164957=CARTESIAN_POINT('Ctrl Pts',(-7.77863555744,-2.35331833991026,29.6670165185949));
#164958=CARTESIAN_POINT('Ctrl Pts',(-7.6699044722138,-2.68874755660881,
29.6815573981063));
#164959=CARTESIAN_POINT('Ctrl Pts',(-7.6040063183904,-2.86982230903358,
29.6896942914052));
#164960=CARTESIAN_POINT('Ctrl Pts',(-7.29689184978755,-3.62862131807226,
29.724967207713));
#164961=CARTESIAN_POINT('Ctrl Pts',(-6.99578470658754,-4.17976217141215,
29.7537197560156));
#164962=CARTESIAN_POINT('Ctrl Pts',(-6.41412666281492,-5.00243139653624,
29.798598682341));
#164963=CARTESIAN_POINT('Ctrl Pts',(-6.17207808033691,-5.29819710814815,
29.8151578857698));
#164964=CARTESIAN_POINT('Ctrl Pts',(-5.89360885157717,-5.59335667277126,
29.8313613095273));
#164965=CARTESIAN_POINT('Ctrl Pts',(-5.87705296038322,-5.61074974338915,
29.8323153297048));
#164966=CARTESIAN_POINT('Ctrl Pts',(-5.85390392428884,-5.63485447075486,
29.8336367782613));
#164967=CARTESIAN_POINT('Ctrl Pts',(-5.84737596831092,-5.64162834185619,
29.8340080509093));
#164968=CARTESIAN_POINT('Ctrl Pts',(-5.83609920906597,-5.6532893096456,
29.8346470782887));
#164969=CARTESIAN_POINT('Ctrl Pts',(-5.83135600410458,-5.65818178838506,
29.8349151568689));
#164970=CARTESIAN_POINT('Ctrl Pts',(-5.82154113256962,-5.66828009421042,
29.8354684317371));
#164971=CARTESIAN_POINT('Ctrl Pts',(-5.81646862395893,-5.67348509573713,
29.8357535793346));
#164972=CARTESIAN_POINT('Ctrl Pts',(-5.80462609726033,-5.68560437186763,
29.8364174667649));
#164973=CARTESIAN_POINT('Ctrl Pts',(-5.79785068874845,-5.69251338113643,
29.8367959023975));
#164974=CARTESIAN_POINT('Ctrl Pts',(-5.77643563556829,-5.71427281139948,
29.837987705191));
#164975=CARTESIAN_POINT('Ctrl Pts',(-5.76175108914249,-5.72907905441195,
29.8387985913185));
#164976=CARTESIAN_POINT('Ctrl Pts',(-5.62588767952376,-5.86501770531323,
29.8462445242745));
#164977=CARTESIAN_POINT('Ctrl Pts',(-5.50095792987442,-5.98234995085719,
29.8526800935489));
#164978=CARTESIAN_POINT('Ctrl Pts',(-5.22708443820016,-6.22372874318939,
29.8661508812412));
#164979=CARTESIAN_POINT('Ctrl Pts',(-5.07722417345722,-6.34657457128917,
29.8731510625904));
#164980=CARTESIAN_POINT('Ctrl Pts',(-4.68360836149387,-6.64636278576619,
29.8909279154655));
#164981=CARTESIAN_POINT('Ctrl Pts',(-4.43415021129654,-6.81532375125243,
29.9016428294598));
#164982=CARTESIAN_POINT('Ctrl Pts',(-3.88156966596984,-7.14638533138326,
29.9249268245644));
#164983=CARTESIAN_POINT('Ctrl Pts',(-3.57638540903953,-7.30389360585907,
29.9375295617889));
#164984=CARTESIAN_POINT('Ctrl Pts',(-2.96121525483293,-7.57356376023444,
29.9628036825153));
#164985=CARTESIAN_POINT('Ctrl Pts',(-2.65254288386724,-7.68711057698692,
29.9754032641058));
#164986=CARTESIAN_POINT('Ctrl Pts',(-2.24388601139363,-7.80988417039206,
29.9919170204162));
#164987=CARTESIAN_POINT('Ctrl Pts',(-2.1494116744319,-7.83641145136924,
29.9957267675228));
#164988=CARTESIAN_POINT('Ctrl Pts',(-2.00866857717258,-7.87319377382159,
30.0013968059592));
#164989=CARTESIAN_POINT('Ctrl Pts',(-1.96275286158611,-7.88476574365364,
30.0032457109251));
#164990=CARTESIAN_POINT('Ctrl Pts',(-1.88023255502938,-7.90479755192614,
30.0065677436987));
#164991=CARTESIAN_POINT('Ctrl Pts',(-1.84366542265012,-7.91340613101175,
30.0080395364648));
#164992=CARTESIAN_POINT('Ctrl Pts',(-1.77285824905165,-7.92955801918312,
30.0108892392314));
#164993=CARTESIAN_POINT('Ctrl Pts',(-1.73862647281402,-7.93713391144263,
30.0122668310761));
#164994=CARTESIAN_POINT('Ctrl Pts',(-1.65580289318513,-7.95490221873269,
30.0155999909796));
#164995=CARTESIAN_POINT('Ctrl Pts',(-1.60716469468192,-7.96487125722936,
30.0175574637148));
#164996=CARTESIAN_POINT('Ctrl Pts',(-1.40798594837367,-8.00379682326964,
30.0255751825452));
#164997=CARTESIAN_POINT('Ctrl Pts',(-1.25673306531207,-8.02893574162506,
30.0316679447973));
#164998=CARTESIAN_POINT('Ctrl Pts',(-0.862835566601014,-8.08299958215693,
30.0475622327331));
#164999=CARTESIAN_POINT('Ctrl Pts',(-0.619437856786041,-8.10528601980463,
30.0574120715731));
#165000=CARTESIAN_POINT('Ctrl Pts',(-0.146004772702246,-8.12718335888819,
30.0766207129285));
#165001=CARTESIAN_POINT('Ctrl Pts',(0.0837464571762289,-8.12806328904075,
30.0859645841273));
#165002=CARTESIAN_POINT('Ctrl Pts',(0.507325104650065,-8.11172236668132,
30.1031780208249));
#165003=CARTESIAN_POINT('Ctrl Pts',(0.701096048755897,-8.09727633919893,
30.1110467758922));
#165004=CARTESIAN_POINT('Ctrl Pts',(1.01819889995054,-8.06216669375217,
30.1238639838073));
#165005=CARTESIAN_POINT('Ctrl Pts',(1.14190232473057,-8.0455777037495,30.1288487005528));
#165006=CARTESIAN_POINT('Ctrl Pts',(1.29804400351407,-8.0209648104311,30.135108095079));
#165007=CARTESIAN_POINT('Ctrl Pts',(1.33088020515995,-8.01558186421176,
30.1364225950309));
#165008=CARTESIAN_POINT('Ctrl Pts',(1.38110367565676,-8.00703144069184,
30.138430009667));
#165009=CARTESIAN_POINT('Ctrl Pts',(1.39851509495466,-8.00400870737513,
30.1391253485611));
#165010=CARTESIAN_POINT('Ctrl Pts',(1.43239125474688,-7.99801367653606,
30.1404770928145));
#165011=CARTESIAN_POINT('Ctrl Pts',(1.4488568926458,-7.99504729088915,30.1411336091373));
#165012=CARTESIAN_POINT('Ctrl Pts',(1.46536600291902,-7.99202039805092,
30.1417914243835));
#165013=CARTESIAN_POINT('Ctrl Pts',(1.46541872333055,-7.99201073139202,
30.141793525055));
#165014=CARTESIAN_POINT('Ctrl Pts',(1.46552404096696,-7.9919914195842,30.1417977214806));
#165015=CARTESIAN_POINT('Ctrl Pts',(1.46557663824738,-7.9919817744276,30.141799817237));
#165016=CARTESIAN_POINT('Ctrl Pts',(1.46568171045387,-7.99196250547932,
30.1418040038657));
#165017=CARTESIAN_POINT('Ctrl Pts',(1.46573418568748,-7.99195288163371,
30.1418060947503));
#165018=CARTESIAN_POINT('Ctrl Pts',(1.46583901572518,-7.9919336549618,30.1418102717121));
#165019=CARTESIAN_POINT('Ctrl Pts',(1.46589137041116,-7.99192405215961,
30.1418123577847));
#165020=CARTESIAN_POINT('Ctrl Pts',(1.46599596040802,-7.99190486738848,
30.1418165251646));
#165021=CARTESIAN_POINT('Ctrl Pts',(1.46604819577357,-7.99189528541193,
30.1418186064742));
#165022=CARTESIAN_POINT('Ctrl Pts',(1.46615254837484,-7.99187614207087,
30.1418227643776));
#165023=CARTESIAN_POINT('Ctrl Pts',(1.46620466565408,-7.99186658070077,
30.1418248409734));
#165024=CARTESIAN_POINT('Ctrl Pts',(1.4663087836147,-7.99184747829871,30.1418289895103));
#165025=CARTESIAN_POINT('Ctrl Pts',(1.46636078419824,-7.99183793728705,
30.1418310614477));
#165026=CARTESIAN_POINT('Ctrl Pts',(1.4664646697254,-7.99181887543317,30.1418352007062));
#165027=CARTESIAN_POINT('Ctrl Pts',(1.46651655480009,-7.99180935456921,
30.1418372680326));
#165028=CARTESIAN_POINT('Ctrl Pts',(1.46662021037785,-7.99179033282166,
30.1418413981118));
#165029=CARTESIAN_POINT('Ctrl Pts',(1.46667198103232,-7.99178083191257,
30.1418434608707));
#165030=CARTESIAN_POINT('Ctrl Pts',(1.4667754097956,-7.99176184970982,30.1418475818955));
#165031=CARTESIAN_POINT('Ctrl Pts',(1.46682706760386,-7.99175236847358,
30.1418496401496));
#165032=CARTESIAN_POINT('Ctrl Pts',(1.4669302710439,-7.99173342555553,30.1418537521797));
#165033=CARTESIAN_POINT('Ctrl Pts',(1.46698181693616,-7.99172396382815,
30.1418558059661));
#165034=CARTESIAN_POINT('Ctrl Pts',(1.46708479830107,-7.99170505961204,
30.1418599091309));
#165035=CARTESIAN_POINT('Ctrl Pts',(1.46713623370998,-7.9916956171372,30.1418619585068));
#165036=CARTESIAN_POINT('Ctrl Pts',(1.46723899465904,-7.99167675133167,
30.1418660528727));
#165037=CARTESIAN_POINT('Ctrl Pts',(1.46729032046092,-7.99166732795509,
30.141868097873));
#165038=CARTESIAN_POINT('Ctrl Pts',(1.46739286448532,-7.99164849993224,
30.1418721835791));
#165039=CARTESIAN_POINT('Ctrl Pts',(1.46744408230829,-7.99163909536148,
30.1418742242688));
#165040=CARTESIAN_POINT('Ctrl Pts',(1.46754641061946,-7.99162030491178,
30.1418783013634));
#165041=CARTESIAN_POINT('Ctrl Pts',(1.46759752133859,-7.99161091899257,
30.1418803377775));
#165042=CARTESIAN_POINT('Ctrl Pts',(1.46769963697649,-7.99159216557053,
30.141884406382));
#165043=CARTESIAN_POINT('Ctrl Pts',(1.46775064182439,-7.99158279808283,
30.1418864385695));
#165044=CARTESIAN_POINT('Ctrl Pts',(1.46785254719436,-7.99156408125927,
30.1418904987797));
#165045=CARTESIAN_POINT('Ctrl Pts',(1.46790344750882,-7.99155473196361,
30.1418925267941));
#165046=CARTESIAN_POINT('Ctrl Pts',(1.46800514443233,-7.99153605141637,
30.1418965786828));
#165047=CARTESIAN_POINT('Ctrl Pts',(1.46805594120636,-7.99152672013653,
30.1418986025636));
#165048=CARTESIAN_POINT('Ctrl Pts',(1.46815743237814,-7.99150807538286,
30.1419026462382));
#165049=CARTESIAN_POINT('Ctrl Pts',(1.46820812681643,-7.9914987619036,30.1419046660335));
#165050=CARTESIAN_POINT('Ctrl Pts',(1.46830941436799,-7.991480152564,30.1419087015791));
#165051=CARTESIAN_POINT('Ctrl Pts',(1.46836000756202,-7.99147085669081,
30.1419107173325));
#165052=CARTESIAN_POINT('Ctrl Pts',(1.46846109392803,-7.99145228232987,
30.1419147448461));
#165053=CARTESIAN_POINT('Ctrl Pts',(1.46851158707424,-7.99144300384882,
30.1419167566053));
#165054=CARTESIAN_POINT('Ctrl Pts',(1.46861247432569,-7.99142446409777,
30.1419207761695));
#165055=CARTESIAN_POINT('Ctrl Pts',(1.46866286849074,-7.9914152028187,30.141922783977));
#165056=CARTESIAN_POINT('Ctrl Pts',(1.46876355896914,-7.99139669725884,
30.1419267956854));
#165057=CARTESIAN_POINT('Ctrl Pts',(1.46881385525859,-7.99138745298434,
30.1419287995853));
#165058=CARTESIAN_POINT('Ctrl Pts',(1.46891435139421,-7.99136898118046,
30.1419328035347));
#165059=CARTESIAN_POINT('Ctrl Pts',(1.46896455110614,-7.99135975367763,
30.1419348035788));
#165060=CARTESIAN_POINT('Ctrl Pts',(1.4690648544144,-7.9913413153625,30.1419387998296));
#165061=CARTESIAN_POINT('Ctrl Pts',(1.4691149583401,-7.9913321044915,30.1419407960495));
#165062=CARTESIAN_POINT('Ctrl Pts',(1.46921507178171,-7.99131369913201,
30.1419447847199));
#165063=CARTESIAN_POINT('Ctrl Pts',(1.46926508117365,-7.99130450466814,
30.1419467771654));
#165064=CARTESIAN_POINT('Ctrl Pts',(1.46936500660038,-7.99128613193484,
30.1419507583292));
#165065=CARTESIAN_POINT('Ctrl Pts',(1.46941492254477,-7.99127695368385,
30.1419527470439));
#165066=CARTESIAN_POINT('Ctrl Pts',(1.46951466213173,-7.99125861318767,
30.1419567207878));
#165067=CARTESIAN_POINT('Ctrl Pts',(1.46956448573254,-7.99124945095196,
30.1419587058155));
#165068=CARTESIAN_POINT('Ctrl Pts',(1.46966404133941,-7.99123114236166,
30.1419626722138));
#165069=CARTESIAN_POINT('Ctrl Pts',(1.46971377344337,-7.99122199599084,
30.1419646535884));
#165070=CARTESIAN_POINT('Ctrl Pts',(1.46981314797316,-7.99120371878311,
30.1419686127568));
#165071=CARTESIAN_POINT('Ctrl Pts',(1.46986278998158,-7.9911945880247,30.1419705905341));
#165072=CARTESIAN_POINT('Ctrl Pts',(1.46996198475956,-7.9911763419662,30.1419745425255));
#165073=CARTESIAN_POINT('Ctrl Pts',(1.47001153762577,-7.99116722665004,
30.1419765167435));
#165074=CARTESIAN_POINT('Ctrl Pts',(1.47011055472865,-7.99114901136908,
30.1419804616408));
#165075=CARTESIAN_POINT('Ctrl Pts',(1.47016001928639,-7.9911399113469,30.1419824323328));
#165076=CARTESIAN_POINT('Ctrl Pts',(1.4702588613271,-7.99112172637295,30.1419863702401));
#165077=CARTESIAN_POINT('Ctrl Pts',(1.47030823873138,-7.99111264143732,
30.1419883374522));
#165078=CARTESIAN_POINT('Ctrl Pts',(1.47040690751414,-7.99109448644844,
30.1419922684415));
#165079=CARTESIAN_POINT('Ctrl Pts',(1.47045619877328,-7.9910854164188,30.1419942322139));
#165080=CARTESIAN_POINT('Ctrl Pts',(1.47055469649628,-7.99106729102039,
30.1419981563728));
#165081=CARTESIAN_POINT('Ctrl Pts',(1.47060390274324,-7.99105823569317,
30.1420001167507));
#165082=CARTESIAN_POINT('Ctrl Pts',(1.47070223114057,-7.99104013957588,
30.1420040341485));
#165083=CARTESIAN_POINT('Ctrl Pts',(1.47075135331427,-7.99103109878312,
30.1420059911693));
#165084=CARTESIAN_POINT('Ctrl Pts',(1.47084951467059,-7.99101303153609,
30.142009901897));
#165085=CARTESIAN_POINT('Ctrl Pts',(1.47089855389559,-7.99100400507559,
30.1420118556055));
#165086=CARTESIAN_POINT('Ctrl Pts',(1.47099654964575,-7.99098596644421,
30.1420157597204));
#165087=CARTESIAN_POINT('Ctrl Pts',(1.47104550658709,-7.99097695419828,
30.1420177101433));
#165088=CARTESIAN_POINT('Ctrl Pts',(1.47114333973886,-7.99095894363823,
30.1420216077652));
#165089=CARTESIAN_POINT('Ctrl Pts',(1.47119221574097,-7.990949945364,30.142023554956));
#165090=CARTESIAN_POINT('Ctrl Pts',(1.47128988731677,-7.99093196269629,
30.1420274461259));
#165091=CARTESIAN_POINT('Ctrl Pts',(1.47133868311205,-7.99092297826351,
30.1420293901138));
#165092=CARTESIAN_POINT('Ctrl Pts',(1.47143619576111,-7.99090502300946,
30.1420332749372));
#165093=CARTESIAN_POINT('Ctrl Pts',(1.47148491251084,-7.99089605220883,
30.1420352157686));
#165094=CARTESIAN_POINT('Ctrl Pts',(1.47158226764469,-7.9908781241175,30.1420390943018));
#165095=CARTESIAN_POINT('Ctrl Pts',(1.47163090614589,-7.99086916680671,
30.1420410320084));
#165096=CARTESIAN_POINT('Ctrl Pts',(1.47172810619937,-7.99085126543856,
30.1420449043486));
#165097=CARTESIAN_POINT('Ctrl Pts',(1.47177666756755,-7.99084232141656,
30.1420468389749));
#165098=CARTESIAN_POINT('Ctrl Pts',(1.47187371411487,-7.99082444649038,
30.1420507051848));
#165099=CARTESIAN_POINT('Ctrl Pts',(1.4719221992592,-7.99081551559405,30.142052636767));
#165100=CARTESIAN_POINT('Ctrl Pts',(1.47201909434683,-7.9907976667415,30.1420564969283));
#165101=CARTESIAN_POINT('Ctrl Pts',(1.47206750425578,-7.99078874879302,
30.1420584255059));
#165102=CARTESIAN_POINT('Ctrl Pts',(1.47216424963049,-7.99077092570082,
30.1420622796881));
#165103=CARTESIAN_POINT('Ctrl Pts',(1.47221258517073,-7.99076202054476,
30.1420642052957));
#165104=CARTESIAN_POINT('Ctrl Pts',(1.47230918291279,-7.99074422283801,
30.1420680535818));
#165105=CARTESIAN_POINT('Ctrl Pts',(1.47235744506002,-7.99073533029875,
30.1420699762582));
#165106=CARTESIAN_POINT('Ctrl Pts',(1.47245389703113,-7.99071755764268,
30.1420738187226));
#165107=CARTESIAN_POINT('Ctrl Pts',(1.47250208677945,-7.99070867754114,
30.1420757385075));
#165108=CARTESIAN_POINT('Ctrl Pts',(1.47259839466091,-7.99069092963406,
30.1420795752171));
#165109=CARTESIAN_POINT('Ctrl Pts',(1.47264651287776,-7.99068206181443,
30.1420814921451));
#165110=CARTESIAN_POINT('Ctrl Pts',(1.47274267855942,-7.99066433831609,
30.1420853231752));
#165111=CARTESIAN_POINT('Ctrl Pts',(1.47279072608794,-7.99065548262696,
30.1420872372799));
#165112=CARTESIAN_POINT('Ctrl Pts',(1.47288675182275,-7.99063778313003,
30.1420910627205));
#165113=CARTESIAN_POINT('Ctrl Pts',(1.47293472983619,-7.99062893935906,
30.1420929740487));
#165114=CARTESIAN_POINT('Ctrl Pts',(1.47303061661909,-7.99061126368791,
30.1420967939394));
#165115=CARTESIAN_POINT('Ctrl Pts',(1.47307852571092,-7.99060243172958,
30.1420987025147));
#165116=CARTESIAN_POINT('Ctrl Pts',(1.4731742761607,-7.99058477940914,30.1421025169599));
#165117=CARTESIAN_POINT('Ctrl Pts',(1.47322211740726,-7.99057595906882,
30.1421044228254));
#165118=CARTESIAN_POINT('Ctrl Pts',(1.47331773299548,-7.99055832983534,
30.1421082318838));
#165119=CARTESIAN_POINT('Ctrl Pts',(1.47336550730776,-7.99054952094884,
30.1421101350756));
#165120=CARTESIAN_POINT('Ctrl Pts',(1.47346098966733,-7.9905319145087,30.1421139388123));
#165121=CARTESIAN_POINT('Ctrl Pts',(1.4735086978039,-7.99052311693982,30.1421158393608));
#165122=CARTESIAN_POINT('Ctrl Pts',(1.47360404914403,-7.99050553289298,
30.1421196378639));
#165123=CARTESIAN_POINT('Ctrl Pts',(1.4736516921524,-7.99049674645221,30.1421215358108));
#165124=CARTESIAN_POINT('Ctrl Pts',(1.47374691378359,-7.99047918456422,
30.1421253291326));
#165125=CARTESIAN_POINT('Ctrl Pts',(1.47379449240464,-7.99047040911851,
30.1421272245075));
#165126=CARTESIAN_POINT('Ctrl Pts',(1.47388958661129,-7.99045286897516,
30.142131012739));
#165127=CARTESIAN_POINT('Ctrl Pts',(1.47393710196607,-7.99044410432126,
30.1421329055865));
#165128=CARTESIAN_POINT('Ctrl Pts',(1.47403206985605,-7.99042658572521,
30.142136688772));
#165129=CARTESIAN_POINT('Ctrl Pts',(1.47407952266179,-7.9904178317343,30.1421385791207));
#165130=CARTESIAN_POINT('Ctrl Pts',(1.47417436605759,-7.99040033435628,
30.1421423573328));
#165131=CARTESIAN_POINT('Ctrl Pts',(1.47422175695718,-7.99039159091321,
30.1421442452084));
#165132=CARTESIAN_POINT('Ctrl Pts',(1.4743164783842,-7.9903741142941,30.1421480185477));
#165133=CARTESIAN_POINT('Ctrl Pts',(1.47436380858966,-7.9903653811786,30.1421499039986));
#165134=CARTESIAN_POINT('Ctrl Pts',(1.4744584089388,-7.99034792516072,30.1421536725007));
#165135=CARTESIAN_POINT('Ctrl Pts',(1.47450567917972,-7.9903392022415,30.1421555555559));
#165136=CARTESIAN_POINT('Ctrl Pts',(1.49288206123529,-7.98694798476592,
30.1428875949228));
#165137=CARTESIAN_POINT('Ctrl Pts',(1.51119951711735,-7.98350242577363,
30.1436167655524));
#165138=CARTESIAN_POINT('Ctrl Pts',(1.55546136568063,-7.97501887059435,
30.1453776877116));
#165139=CARTESIAN_POINT('Ctrl Pts',(1.58139338011566,-7.96991725370093,
30.146408517276));
#165140=CARTESIAN_POINT('Ctrl Pts',(1.65170744605864,-7.95572764719713,
30.1492019954247));
#165141=CARTESIAN_POINT('Ctrl Pts',(1.69603922700832,-7.94639483373781,
30.1509615122151));
#165142=CARTESIAN_POINT('Ctrl Pts',(1.84292345629172,-7.91418729947237,
30.156789895026));
#165143=CARTESIAN_POINT('Ctrl Pts',(1.94511051148342,-7.88969408812483,
30.1608425384323));
#165144=CARTESIAN_POINT('Ctrl Pts',(2.36154630305787,-7.78129603544755,
30.177409404943));
#165145=CARTESIAN_POINT('Ctrl Pts',(2.67109336479942,-7.68054219511478,
30.1898607436242));
#165146=CARTESIAN_POINT('Ctrl Pts',(3.03429369939984,-7.53770385451671,
30.2049968631895));
#165147=CARTESIAN_POINT('Ctrl Pts',(3.09453211940317,-7.51317433296674,
30.2075245217721));
#165148=CARTESIAN_POINT('Ctrl Pts',(3.19023650905459,-7.47285654267423,
30.2115702360824));
#165149=CARTESIAN_POINT('Ctrl Pts',(3.22589517901687,-7.45753271343991,
30.2130843246569));
#165150=CARTESIAN_POINT('Ctrl Pts',(3.2925127203717,-7.42833751989845,30.2159259474213));
#165151=CARTESIAN_POINT('Ctrl Pts',(3.32349718996094,-7.41452660273821,
30.2172529300907));
#165152=CARTESIAN_POINT('Ctrl Pts',(3.35472447711157,-7.40037238094552,
30.2185958257017));
#165153=CARTESIAN_POINT('Ctrl Pts',(3.35505474268786,-7.40022265662057,
30.2186100290394));
#165154=CARTESIAN_POINT('Ctrl Pts',(3.35571072501243,-7.39992521721995,
30.2186382413304));
#165155=CARTESIAN_POINT('Ctrl Pts',(3.35603644202967,-7.39977750274831,
30.2186522502782));
#165156=CARTESIAN_POINT('Ctrl Pts',(3.35668341227773,-7.39948404665378,
30.2186800773963));
#165157=CARTESIAN_POINT('Ctrl Pts',(3.35700466573514,-7.3993383056309,30.2186938955598));
#165158=CARTESIAN_POINT('Ctrl Pts',(3.3576427919385,-7.39904876084293,30.2187213446339));
#165159=CARTESIAN_POINT('Ctrl Pts',(3.35795966496274,-7.39890495763199,
30.2187349755404));
#165160=CARTESIAN_POINT('Ctrl Pts',(3.35858911172659,-7.3986192535452,30.2187620535557));
#165161=CARTESIAN_POINT('Ctrl Pts',(3.35890168570724,-7.39847735321878,
30.2187755006594));
#165162=CARTESIAN_POINT('Ctrl Pts',(3.35952261400977,-7.39819542071905,
30.2188022144486));
#165163=CARTESIAN_POINT('Ctrl Pts',(3.35983096857272,-7.39805538907429,
30.2188154811296));
#165164=CARTESIAN_POINT('Ctrl Pts',(3.36044353600026,-7.39777716043799,
30.2188418373831));
#165165=CARTESIAN_POINT('Ctrl Pts',(3.36074774908447,-7.39763896396462,
30.2188549269507));
#165166=CARTESIAN_POINT('Ctrl Pts',(3.36135210975156,-7.39736437290071,
30.2188809322128));
#165167=CARTESIAN_POINT('Ctrl Pts',(3.36165225758187,-7.3972279787963,30.218893847904));
#165168=CARTESIAN_POINT('Ctrl Pts',(3.36224856240444,-7.3969569603278,30.2189195085847));
#165169=CARTESIAN_POINT('Ctrl Pts',(3.36254471960628,-7.3968223364483,30.2189322535695));
#165170=CARTESIAN_POINT('Ctrl Pts',(3.36313311611353,-7.3965548270031,30.2189575759359));
#165171=CARTESIAN_POINT('Ctrl Pts',(3.36342535565635,-7.39642194189125,
30.2189701533146));
#165172=CARTESIAN_POINT('Ctrl Pts',(3.40605668117479,-7.377033875977,30.2208049880218));
#165173=CARTESIAN_POINT('Ctrl Pts',(3.44822954070459,-7.35741557437806,
30.2226304058214));
#165174=CARTESIAN_POINT('Ctrl Pts',(3.59006003122931,-7.28995042345373,
30.22880518051));
#165175=CARTESIAN_POINT('Ctrl Pts',(3.68890840245935,-7.24043249454735,
30.2331689395441));
#165176=CARTESIAN_POINT('Ctrl Pts',(3.93610279181215,-7.11022440194357,
30.244237974039));
#165177=CARTESIAN_POINT('Ctrl Pts',(4.08300046540657,-7.02689851247347,
30.250962508483));
#165178=CARTESIAN_POINT('Ctrl Pts',(4.44541152655336,-6.80612184090205,
30.2679030383154));
#165179=CARTESIAN_POINT('Ctrl Pts',(4.6572371040205,-6.66296642533312,30.278133541243));
#165180=CARTESIAN_POINT('Ctrl Pts',(4.9096079167721,-6.4744863549968,30.2906149367545));
#165181=CARTESIAN_POINT('Ctrl Pts',(4.95685906150458,-6.43838269849963,
30.2929647836191));
#165182=CARTESIAN_POINT('Ctrl Pts',(5.02360174453563,-6.38621566313445,
30.2962999157217));
#165183=CARTESIAN_POINT('Ctrl Pts',(5.04342113744842,-6.37057518787796,
30.2972923184733));
#165184=CARTESIAN_POINT('Ctrl Pts',(5.0776894357839,-6.34327220903865,30.29901150349));
#165185=CARTESIAN_POINT('Ctrl Pts',(5.09217179928574,-6.33165212985064,
30.2997391089253));
#165186=CARTESIAN_POINT('Ctrl Pts',(5.12295458306643,-6.30677930749208,
30.301288063531));
#165187=CARTESIAN_POINT('Ctrl Pts',(5.13924370107714,-6.29351277730319,
30.3021091606912));
#165188=CARTESIAN_POINT('Ctrl Pts',(5.15558720053953,-6.28009619344603,
30.3029345695073));
#165189=CARTESIAN_POINT('Ctrl Pts',(5.15569318195253,-6.28000918748293,
30.302939922038));
#165190=CARTESIAN_POINT('Ctrl Pts',(5.15590548975005,-6.27983488335417,
30.3029506446556));
#165191=CARTESIAN_POINT('Ctrl Pts',(5.15601181693012,-6.27974758450557,
30.3029560147831));
#165192=CARTESIAN_POINT('Ctrl Pts',(5.15622482441792,-6.27957268781964,
30.3029667730077));
#165193=CARTESIAN_POINT('Ctrl Pts',(5.15633150472092,-6.27948508995576,
30.302972161105));
#165194=CARTESIAN_POINT('Ctrl Pts',(5.15654522576583,-6.27930958914404,
30.3029829556398));
#165195=CARTESIAN_POINT('Ctrl Pts',(5.15665226642527,-6.27922168623276,
30.3029883620736));
#165196=CARTESIAN_POINT('Ctrl Pts',(5.15686671522975,-6.27904556944555,
30.3029991936389));
#165197=CARTESIAN_POINT('Ctrl Pts',(5.15697412341429,-6.27895735550526,
30.3030046187728));
#165198=CARTESIAN_POINT('Ctrl Pts',(5.15718931459771,-6.27878061054486,
30.3030154881099));
#165199=CARTESIAN_POINT('Ctrl Pts',(5.15729709759758,-6.27869207949128,
30.3030209323136));
#165200=CARTESIAN_POINT('Ctrl Pts',(5.15751304573589,-6.27851469418993,
30.3030318401618));
#165201=CARTESIAN_POINT('Ctrl Pts',(5.15762121086413,-6.27842583991714,
30.3030373038062));
#165202=CARTESIAN_POINT('Ctrl Pts',(5.15783793080416,-6.27824780187878,
30.3030482509185));
#165203=CARTESIAN_POINT('Ctrl Pts',(5.15794648551746,-6.27815861815994,
30.3030537343819));
#165204=CARTESIAN_POINT('Ctrl Pts',(5.15816399201908,-6.27797991505405,
30.3030647215071));
#165205=CARTESIAN_POINT('Ctrl Pts',(5.15827294378432,-6.27789039565098,
30.3030702251683));
#165206=CARTESIAN_POINT('Ctrl Pts',(5.15849125179416,-6.27771101498763,
30.3030812530647));
#165207=CARTESIAN_POINT('Ctrl Pts',(5.15860060810347,-6.2776211536384,30.3030867773037));
#165208=CARTESIAN_POINT('Ctrl Pts',(5.15881973276674,-6.27744108275843,
30.3030978467396));
#165209=CARTESIAN_POINT('Ctrl Pts',(5.15892950116818,-6.27735087315211,
30.3031033919395));
#165210=CARTESIAN_POINT('Ctrl Pts',(5.18800642511015,-6.25345366695034,
30.3045722977923));
#165211=CARTESIAN_POINT('Ctrl Pts',(5.2168085396806,-6.22944637267108,30.3060323351036));
#165212=CARTESIAN_POINT('Ctrl Pts',(5.28210544772624,-6.17424927852298,
30.3093552393287));
#165213=CARTESIAN_POINT('Ctrl Pts',(5.31849211309834,-6.14293364675795,
30.3112162348533));
#165214=CARTESIAN_POINT('Ctrl Pts',(5.43553092929178,-6.0403865237015,30.3172365382661));
#165215=CARTESIAN_POINT('Ctrl Pts',(5.51504646368256,-5.96787471198371,
30.3213804556262));
#165216=CARTESIAN_POINT('Ctrl Pts',(5.7493593032263,-5.74551667747788,30.3337940624134));
#165217=CARTESIAN_POINT('Ctrl Pts',(5.8996610551997,-5.59107271111529,30.3420339954998));
#165218=CARTESIAN_POINT('Ctrl Pts',(6.14589558491515,-5.31705339146994,
30.3561685992208));
#165219=CARTESIAN_POINT('Ctrl Pts',(6.2449092090683,-5.20040362897507,30.3620473470211));
#165220=CARTESIAN_POINT('Ctrl Pts',(6.42515938471843,-4.97547105453828,
30.3731689837913));
#165221=CARTESIAN_POINT('Ctrl Pts',(6.50709872949034,-4.8678178953817,30.3784048732876));
#165222=CARTESIAN_POINT('Ctrl Pts',(6.63578606519205,-4.68968745430107,
30.3869457646013));
#165223=CARTESIAN_POINT('Ctrl Pts',(6.68418889519141,-4.62043762344156,
30.3902370743582));
#165224=CARTESIAN_POINT('Ctrl Pts',(6.75996815779295,-4.50833688935472,
30.3955212442209));
#165225=CARTESIAN_POINT('Ctrl Pts',(6.78803769180149,-4.46596185334051,
30.3975089066777));
#165226=CARTESIAN_POINT('Ctrl Pts',(6.84439285965936,-4.37912667004756,
30.401562557886));
#165227=CARTESIAN_POINT('Ctrl Pts',(6.87264731107048,-4.33464911213736,
30.4036286498146));
#165228=CARTESIAN_POINT('Ctrl Pts',(6.93128826621763,-4.2403229079573,30.4079891084106));
#165229=CARTESIAN_POINT('Ctrl Pts',(6.96157421715762,-4.19041522841973,
30.4102839305323));
#165230=CARTESIAN_POINT('Ctrl Pts',(7.00721703626377,-4.11334053468719,
30.4138091290514));
#165231=CARTESIAN_POINT('Ctrl Pts',(7.0229596478429,-4.08640413189459,30.4150376509937));
#165232=CARTESIAN_POINT('Ctrl Pts',(7.07691093637252,-3.9928581039347,30.4192920208487));
#165233=CARTESIAN_POINT('Ctrl Pts',(7.1143301842911,-3.92579803804068,30.4223207665638));
#165234=CARTESIAN_POINT('Ctrl Pts',(7.24808014725884,-3.67790681400281,
30.4334372111958));
#165235=CARTESIAN_POINT('Ctrl Pts',(7.33851251863353,-3.49398035093157,
30.4415338862254));
#165236=CARTESIAN_POINT('Ctrl Pts',(7.43578454744889,-3.27566180058298,
30.4509346847701));
#165237=CARTESIAN_POINT('Ctrl Pts',(7.44947627069259,-3.24440369982931,
30.4522757002718));
#165238=CARTESIAN_POINT('Ctrl Pts',(7.4773038111099,-3.17976870895714,30.4550380018823));
#165239=CARTESIAN_POINT('Ctrl Pts',(7.49141399502494,-3.14638168207501,
30.4564589521642));
#165240=CARTESIAN_POINT('Ctrl Pts',(7.52085929775964,-3.07538815393943,
30.4594683959595));
#165241=CARTESIAN_POINT('Ctrl Pts',(7.53613679786254,-3.03775888600757,
30.4610565073474));
#165242=CARTESIAN_POINT('Ctrl Pts',(7.57516587432124,-2.93952153255506,
30.4651861205042));
#165243=CARTESIAN_POINT('Ctrl Pts',(7.59847238430118,-2.87873971037574,
30.4677250730214));
#165244=CARTESIAN_POINT('Ctrl Pts',(7.68426292898823,-2.64670034033938,
30.477366695346));
#165245=CARTESIAN_POINT('Ctrl Pts',(7.74170767784476,-2.47363734453655,
30.4844539699317));
#165246=CARTESIAN_POINT('Ctrl Pts',(7.82188357613527,-2.20182751976962,
30.4955010572092));
#165247=CARTESIAN_POINT('Ctrl Pts',(7.84867225671503,-2.10434094374101,
30.4994464644676));
#165248=CARTESIAN_POINT('Ctrl Pts',(7.88659327813456,-1.95552753551339,
30.5054534458347));
#165249=CARTESIAN_POINT('Ctrl Pts',(7.89905870405772,-1.90455061542485,
30.5075083797333));
#165250=CARTESIAN_POINT('Ctrl Pts',(7.92267390389353,-1.80375487054386,
30.5115674944845));
#165251=CARTESIAN_POINT('Ctrl Pts',(7.93384974390912,-1.75394459459873,
30.5135714413131));
#165252=CARTESIAN_POINT('Ctrl Pts',(7.95575518627726,-1.6518168418978,30.5176773882836));
#165253=CARTESIAN_POINT('Ctrl Pts',(7.96643985811064,-1.59949223977298,
30.5197795461509));
#165254=CARTESIAN_POINT('Ctrl Pts',(7.9903707577024,-1.47610553600316,30.5247343769686));
#165255=CARTESIAN_POINT('Ctrl Pts',(8.00318604566494,-1.40496457375376,
30.5275894309627));
#165256=CARTESIAN_POINT('Ctrl Pts',(8.08830978631117,-0.893387501392534,
30.5481147225231));
#165257=CARTESIAN_POINT('Ctrl Pts',(8.12516527517489,-0.447837443061713,
30.5660079510785));
#165258=CARTESIAN_POINT('Ctrl Pts',(8.12524985409108,-0.00153983533529523,
30.5838443095726));
#165259=CARTESIAN_POINT('',(8.12524976787349,-0.00315471203393718,34.5839446402054));
#165260=CARTESIAN_POINT('Ctrl Pts',(8.12524985424774,-0.0015390084936643,
30.5838443426175));
#165261=CARTESIAN_POINT('Ctrl Pts',(8.12528247079636,0.170661215270594,
30.5907263532811));
#165262=CARTESIAN_POINT('Ctrl Pts',(8.11984086030867,0.342822053948763,
30.597587868216));
#165263=CARTESIAN_POINT('Ctrl Pts',(8.1069234245787,0.546339019308158,30.6056444485861));
#165264=CARTESIAN_POINT('Ctrl Pts',(8.10472878616853,0.577983606759902,
30.606895558429));
#165265=CARTESIAN_POINT('Ctrl Pts',(8.10071272379043,0.631360835254744,
30.6090028482588));
#165266=CARTESIAN_POINT('Ctrl Pts',(8.09898900937166,0.653100426989475,
30.6098602553929));
#165267=CARTESIAN_POINT('Ctrl Pts',(8.095624524121,0.69347017906358,30.6114507150424));
#165268=CARTESIAN_POINT('Ctrl Pts',(8.09400691274582,0.712102116221887,
30.6121840824149));
#165269=CARTESIAN_POINT('Ctrl Pts',(8.09054299384729,0.750462688824823,
30.6136924866601));
#165270=CARTESIAN_POINT('Ctrl Pts',(8.08868881693465,0.770190501797474,
30.6144674020753));
#165271=CARTESIAN_POINT('Ctrl Pts',(8.08444274227309,0.813659931638667,
30.6161729724052));
#165272=CARTESIAN_POINT('Ctrl Pts',(8.08201838515726,0.837398211912516,
30.6171031059458));
#165273=CARTESIAN_POINT('Ctrl Pts',(8.07217385705014,0.929764259374635,
30.6207181314146));
#165274=CARTESIAN_POINT('Ctrl Pts',(8.06398380363852,0.998307410475564,
30.6233918974572));
#165275=CARTESIAN_POINT('Ctrl Pts',(8.05031374394521,1.10152978492683,30.6274120270276));
#165276=CARTESIAN_POINT('Ctrl Pts',(8.04548081838411,1.13629118411745,30.6287647472822));
#165277=CARTESIAN_POINT('Ctrl Pts',(8.00109498567051,1.44105180738447,30.640619645082));
#165278=CARTESIAN_POINT('Ctrl Pts',(7.94818878491817,1.7089318053496,30.6510154559394));
#165279=CARTESIAN_POINT('Ctrl Pts',(7.84740436597334,2.11142273227072,30.6669273971922));
#165280=CARTESIAN_POINT('Ctrl Pts',(7.80929739861739,2.24827376586878,30.6723887332309));
#165281=CARTESIAN_POINT('Ctrl Pts',(7.74271476470716,2.46521039637097,30.6811598054927));
#165282=CARTESIAN_POINT('Ctrl Pts',(7.71653611354067,2.54597024712916,30.6844505340548));
#165283=CARTESIAN_POINT('Ctrl Pts',(7.67783370094684,2.6592802546164,30.6891077639006));
#165284=CARTESIAN_POINT('Ctrl Pts',(7.66635849801055,2.69218297705172,30.6904649335769));
#165285=CARTESIAN_POINT('Ctrl Pts',(7.64346574112435,2.75648971149616,30.6931271949241));
#165286=CARTESIAN_POINT('Ctrl Pts',(7.63206541271041,2.78789913598944,30.6944321093348));
#165287=CARTESIAN_POINT('Ctrl Pts',(7.60895125113949,2.85037731580584,30.6970371524867));
#165288=CARTESIAN_POINT('Ctrl Pts',(7.59724007399523,2.88144637880839,30.6983372346837));
#165289=CARTESIAN_POINT('Ctrl Pts',(7.56546515317382,2.96420286987429,30.7018128285314));
#165290=CARTESIAN_POINT('Ctrl Pts',(7.54506228544194,3.01575806496623,30.7039912945516));
#165291=CARTESIAN_POINT('Ctrl Pts',(7.45840977052033,3.22833184312651,30.7130296304252));
#165292=CARTESIAN_POINT('Ctrl Pts',(7.38752126880635,3.387407750811,30.7199286936997));
#165293=CARTESIAN_POINT('Ctrl Pts',(7.30899732817388,3.54940567143891,30.7270908298909));
#165294=CARTESIAN_POINT('Ctrl Pts',(7.30641098760531,3.55472657793394,30.7273262268182));
#165295=CARTESIAN_POINT('Ctrl Pts',(7.21536591222871,3.74151545316565,30.7355951172384));
#165296=CARTESIAN_POINT('Ctrl Pts',(7.12018050810158,3.91962656204717,30.7436600314797));
#165297=CARTESIAN_POINT('Ctrl Pts',(6.97729756854017,4.16457446076842,30.754952879232));
#165298=CARTESIAN_POINT('Ctrl Pts',(6.93507192500324,4.23451759860916,30.7582010978384));
#165299=CARTESIAN_POINT('Ctrl Pts',(6.87129514370992,4.33664489925658,30.7629729818043));
#165300=CARTESIAN_POINT('Ctrl Pts',(6.85055730123445,4.36933068253685,30.7645046678036));
#165301=CARTESIAN_POINT('Ctrl Pts',(6.81266698332157,4.42811828379468,30.7672666635422));
#165302=CARTESIAN_POINT('Ctrl Pts',(6.79559607843407,4.45427175982513,30.7684980110969));
#165303=CARTESIAN_POINT('Ctrl Pts',(6.7683005737375,4.49556767237572,30.7704459535256));
#165304=CARTESIAN_POINT('Ctrl Pts',(6.75817498752247,4.51077512117577,30.7711640880348));
#165305=CARTESIAN_POINT('Ctrl Pts',(6.73785024976349,4.54107844852082,30.7725965576603));
#165306=CARTESIAN_POINT('Ctrl Pts',(6.72765143860333,4.55617444668117,30.7733108909738));
#165307=CARTESIAN_POINT('Ctrl Pts',(6.70503356722658,4.58941126270888,30.7748851384559));
#165308=CARTESIAN_POINT('Ctrl Pts',(6.6925914864767,4.6075362261853,30.7757446343125));
#165309=CARTESIAN_POINT('Ctrl Pts',(6.64937187947682,4.66995182676276,30.7787082946067));
#165310=CARTESIAN_POINT('Ctrl Pts',(6.61822689426013,4.71398656045055,30.7808059613261));
#165311=CARTESIAN_POINT('Ctrl Pts',(6.37813174307391,5.04637804579907,30.7967035595993));
#165312=CARTESIAN_POINT('Ctrl Pts',(6.15086256520502,5.32103317362352,30.8102144036779));
#165313=CARTESIAN_POINT('Ctrl Pts',(5.81142103534428,5.68033132425206,30.8289850994278));
#165314=CARTESIAN_POINT('Ctrl Pts',(5.71398878704995,5.77833111347079,30.8342299777271));
#165315=CARTESIAN_POINT('Ctrl Pts',(5.35427408959011,6.12214204831554,30.8531589818201));
#165316=CARTESIAN_POINT('Ctrl Pts',(5.07825482086978,6.35296745365093,30.866898061753));
#165317=CARTESIAN_POINT('Ctrl Pts',(4.71927078629036,6.61478488161998,30.8841269456628));
#165318=CARTESIAN_POINT('Ctrl Pts',(4.64989562896481,6.66373516122892,30.8874283553265));
#165319=CARTESIAN_POINT('Ctrl Pts',(4.54874467994175,6.73275722426316,30.8922041238203));
#165320=CARTESIAN_POINT('Ctrl Pts',(4.51757660767819,6.75371006093393,30.8936706247982));
#165321=CARTESIAN_POINT('Ctrl Pts',(4.45437064610633,6.79556716008406,30.8966345757298));
#165322=CARTESIAN_POINT('Ctrl Pts',(4.42232814298473,6.8164627677941,30.8981320576086));
#165323=CARTESIAN_POINT('Ctrl Pts',(4.36029442563252,6.85629477507591,30.9010215507255));
#165324=CARTESIAN_POINT('Ctrl Pts',(4.33032440687999,6.8752626163293,30.9024132707204));
#165325=CARTESIAN_POINT('Ctrl Pts',(4.25871598755421,6.91992917558295,30.9057285954105));
#165326=CARTESIAN_POINT('Ctrl Pts',(4.21696779556318,6.94544917535118,30.9076535200677));
#165327=CARTESIAN_POINT('Ctrl Pts',(4.06075400472072,7.03901245233356,30.9148272997049));
#165328=CARTESIAN_POINT('Ctrl Pts',(3.94485213724083,7.10461544637965,30.920092790392));
#165329=CARTESIAN_POINT('Ctrl Pts',(3.46826454477096,7.35911531849033,30.9415180185751));
#165330=CARTESIAN_POINT('Ctrl Pts',(3.09524408805171,7.52362202755177,30.9577615474354));
#165331=CARTESIAN_POINT('Ctrl Pts',(2.21333738502024,7.83581909018226,30.9961228071158));
#165332=CARTESIAN_POINT('Ctrl Pts',(1.69920155889772,7.96313926510935,31.018527855726));
#165333=CARTESIAN_POINT('Ctrl Pts',(0.926181120888742,8.07625039229386,
31.0515363904339));
#165334=CARTESIAN_POINT('Ctrl Pts',(0.674393805133385,8.10116233462654,
31.0621575254606));
#165335=CARTESIAN_POINT('Ctrl Pts',(0.353219044933369,8.11785974538554,
31.0752934584494));
#165336=CARTESIAN_POINT('Ctrl Pts',(0.28454423565166,8.12055696352107,31.0780778939256));
#165337=CARTESIAN_POINT('Ctrl Pts',(0.187960759556835,8.12312355301155,
31.0819527615336));
#165338=CARTESIAN_POINT('Ctrl Pts',(0.16007515997635,8.12372091282373,31.0830666924367));
#165339=CARTESIAN_POINT('Ctrl Pts',(0.111400383025119,8.12451289055111,
31.0850020547166));
#165340=CARTESIAN_POINT('Ctrl Pts',(0.0906125788835788,8.12477132749947,
31.0858257286801));
#165341=CARTESIAN_POINT('Ctrl Pts',(0.0601811948849875,8.12503284761978,
31.08702708921));
#165342=CARTESIAN_POINT('Ctrl Pts',(0.050538324573565,8.12509854893207,
31.087407117667));
#165343=CARTESIAN_POINT('Ctrl Pts',(0.0336328899902811,8.12518363704173,
31.0880722006534));
#165344=CARTESIAN_POINT('Ctrl Pts',(0.0263703837190008,8.12521045329035,
31.0883575405795));
#165345=CARTESIAN_POINT('Ctrl Pts',(0.0122839970648353,8.12524357979321,
31.0889102432341));
#165346=CARTESIAN_POINT('Ctrl Pts',(0.00546012760196375,8.12525103088518,
31.0891776504658));
#165347=CARTESIAN_POINT('Ctrl Pts',(-0.0108075042916905,8.1252483004969,
31.0898143107965));
#165348=CARTESIAN_POINT('Ctrl Pts',(-0.0202512684566991,8.12523025113662,
31.0901832491593));
#165349=CARTESIAN_POINT('Ctrl Pts',(-0.0539249154189347,8.12510718466993,
31.091496372948));
#165350=CARTESIAN_POINT('Ctrl Pts',(-0.0781544889130888,8.12491024885604,
31.0924367883519));
#165351=CARTESIAN_POINT('Ctrl Pts',(-0.511659506401743,8.11944739357702,
31.1091785798839));
#165352=CARTESIAN_POINT('Ctrl Pts',(-0.919967366466715,8.08337124097557,
31.1234753381119));
#165353=CARTESIAN_POINT('Ctrl Pts',(-1.67958053316098,7.95793408467524,
31.1495473342186));
#165354=CARTESIAN_POINT('Ctrl Pts',(-2.03103940878968,7.87556915019174,
31.1614069321283));
#165355=CARTESIAN_POINT('Ctrl Pts',(-2.93260403420878,7.59989847859046,
31.1931467735776));
#165356=CARTESIAN_POINT('Ctrl Pts',(-3.46936823476809,7.37034701138322,
31.213491066032));
#165357=CARTESIAN_POINT('Ctrl Pts',(-4.00173808893761,7.07153350401814,
31.2370058994623));
#165358=CARTESIAN_POINT('Ctrl Pts',(-4.02642598227002,7.05750576484256,
31.2381040028691));
#165359=CARTESIAN_POINT('Ctrl Pts',(-4.06225473612356,7.03689856446319,
31.239708909996));
#165360=CARTESIAN_POINT('Ctrl Pts',(-4.07345432698614,7.03042138081406,
31.2402121938627));
#165361=CARTESIAN_POINT('Ctrl Pts',(-4.09304524164,7.01902862146628,31.2410954026919));
#165362=CARTESIAN_POINT('Ctrl Pts',(-4.10144331246228,7.0141246704718,31.2414749260792));
#165363=CARTESIAN_POINT('Ctrl Pts',(-4.11770544667906,7.00458940334058,
31.2422116242612));
#165364=CARTESIAN_POINT('Ctrl Pts',(-4.12557055360719,6.99995988999779,
31.2425687364064));
#165365=CARTESIAN_POINT('Ctrl Pts',(-4.14428612261227,6.98890114138488,
31.2434204492749));
#165366=CARTESIAN_POINT('Ctrl Pts',(-4.15512943294846,6.98245988343932,
31.2439154661339));
#165367=CARTESIAN_POINT('Ctrl Pts',(-4.19364151223203,6.9594610526682,31.2456791752966));
#165368=CARTESIAN_POINT('Ctrl Pts',(-4.22122649595426,6.94276415539712,
31.2469527029078));
#165369=CARTESIAN_POINT('Ctrl Pts',(-4.67676331132769,6.66331407014106,
31.2681551685278));
#165370=CARTESIAN_POINT('Ctrl Pts',(-5.07949684904348,6.36164092646036,
31.2895106101507));
#165371=CARTESIAN_POINT('Ctrl Pts',(-5.6418802566825,5.85274349116283,31.3230458893457));
#165372=CARTESIAN_POINT('Ctrl Pts',(-5.82373212839376,5.67182144027073,
31.3345652369883));
#165373=CARTESIAN_POINT('Ctrl Pts',(-6.36387846540575,5.0810247336261,31.3705250870506));
#165374=CARTESIAN_POINT('Ctrl Pts',(-6.68983264678388,4.64350167313261,
31.3948988468288));
#165375=CARTESIAN_POINT('Ctrl Pts',(-6.97935005797233,4.16037476210969,
31.4174732962628));
#165376=CARTESIAN_POINT('Ctrl Pts',(-6.98901697266284,4.14411476158781,
31.418228607833));
#165377=CARTESIAN_POINT('Ctrl Pts',(-7.00628258876623,4.11484130068387,
31.419580685251));
#165378=CARTESIAN_POINT('Ctrl Pts',(-7.01390201641288,4.10184021528339,
31.4201784498773));
#165379=CARTESIAN_POINT('Ctrl Pts',(-7.02600549775053,4.08105562254526,
31.4211298457988));
#165380=CARTESIAN_POINT('Ctrl Pts',(-7.03051286671243,4.07328578430004,
31.4214845609186));
#165381=CARTESIAN_POINT('Ctrl Pts',(-7.0383863138654,4.0596614716043,31.4221049250644));
#165382=CARTESIAN_POINT('Ctrl Pts',(-7.04175798972041,4.05381025478175,
31.4223708285228));
#165383=CARTESIAN_POINT('Ctrl Pts',(-7.04936917548767,4.04056363089996,
31.4229716396852));
#165384=CARTESIAN_POINT('Ctrl Pts',(-7.05360435403549,4.03316573488961,
31.4233063535936));
#165385=CARTESIAN_POINT('Ctrl Pts',(-7.06501260536965,4.01316517572387,
31.4242090781151));
#165386=CARTESIAN_POINT('Ctrl Pts',(-7.07216361362104,4.00054992059042,
31.4247761228645));
#165387=CARTESIAN_POINT('Ctrl Pts',(-7.10393441427424,3.94415092767576,
31.4273010205447));
#165388=CARTESIAN_POINT('Ctrl Pts',(-7.12818193667875,3.90015808719331,
31.429243174669));
#165389=CARTESIAN_POINT('Ctrl Pts',(-7.15513296747459,3.85016919144534,
31.4314219938937));
#165390=CARTESIAN_POINT('Ctrl Pts',(-7.15823871129711,3.84439190735535,
31.4316733820945));
#165391=CARTESIAN_POINT('Ctrl Pts',(-7.19074644531438,3.78374526672226,
31.4343079551018));
#165392=CARTESIAN_POINT('Ctrl Pts',(-7.2195243255123,3.72854279771346,31.4366686522266));
#165393=CARTESIAN_POINT('Ctrl Pts',(-7.3044836113224,3.56089943932909,31.4437389541875));
#165394=CARTESIAN_POINT('Ctrl Pts',(-7.35869388862764,3.44747894563927,
31.4483899265534));
#165395=CARTESIAN_POINT('Ctrl Pts',(-7.55990471390446,3.00010648016679,
31.466356801721));
#165396=CARTESIAN_POINT('Ctrl Pts',(-7.68697894014235,2.6576611880201,31.4793224560771));
#165397=CARTESIAN_POINT('Ctrl Pts',(-7.92752084641353,1.84565706251403,
31.5098198431401));
#165398=CARTESIAN_POINT('Ctrl Pts',(-8.02302685373317,1.37224135173242,
31.5274604729183));
#165399=CARTESIAN_POINT('Ctrl Pts',(-8.0828506232712,0.831315728240489,
31.548240037948));
#165400=CARTESIAN_POINT('Ctrl Pts',(-8.08898033149878,0.76938750580692,
31.5506267195295));
#165401=CARTESIAN_POINT('Ctrl Pts',(-8.09875036287201,0.657593557474825,
31.5549495661381));
#165402=CARTESIAN_POINT('Ctrl Pts',(-8.10264297018093,0.607752889225413,
31.556881934779));
#165403=CARTESIAN_POINT('Ctrl Pts',(-8.10786522399183,0.531872764438596,
31.5598316777369));
#165404=CARTESIAN_POINT('Ctrl Pts',(-8.10952991247481,0.505857410521775,
31.5608443827085));
#165405=CARTESIAN_POINT('Ctrl Pts',(-8.11236055637585,0.458008524910283,
31.5627095403002));
#165406=CARTESIAN_POINT('Ctrl Pts',(-8.11356363662832,0.436177389571904,
31.5635614857001));
#165407=CARTESIAN_POINT('Ctrl Pts',(-8.11573929959759,0.393568104531198,
31.5652261752182));
#165408=CARTESIAN_POINT('Ctrl Pts',(-8.11672024080398,0.37279050551324,
31.5660388173605));
#165409=CARTESIAN_POINT('Ctrl Pts',(-8.11911203612603,0.317633773093442,
31.5681985975125));
#165410=CARTESIAN_POINT('Ctrl Pts',(-8.12038431228878,0.283249136489211,
31.5695476006472));
#165411=CARTESIAN_POINT('Ctrl Pts',(-8.124187705308,0.159125845537355,31.5744276026128));
#165412=CARTESIAN_POINT('Ctrl Pts',(-8.12544991894614,0.0693556532507427,
31.577976507428));
#165413=CARTESIAN_POINT('Ctrl Pts',(-8.12364523290431,-0.648873365100727,
31.6065565417131));
#165414=CARTESIAN_POINT('Ctrl Pts',(-8.04915849450093,-1.27498306389039,
31.6328523778494));
#165415=CARTESIAN_POINT('Ctrl Pts',(-7.80688437413114,-2.29013351656759,
31.6771420373107));
#165416=CARTESIAN_POINT('Ctrl Pts',(-7.67964846878573,-2.68610772424907,
31.6947971988147));
#165417=CARTESIAN_POINT('Ctrl Pts',(-7.50307559111217,-3.11869197162453,
31.7136373202818));
#165418=CARTESIAN_POINT('Ctrl Pts',(-7.48299505776451,-3.16657039096945,
31.7157155461714));
#165419=CARTESIAN_POINT('Ctrl Pts',(-7.45690258107033,-3.22714867802599,
31.7183335330937));
#165420=CARTESIAN_POINT('Ctrl Pts',(-7.45131495196176,-3.2400293491326,
31.7188895269094));
#165421=CARTESIAN_POINT('Ctrl Pts',(-7.44232244740854,-3.2606126836703,
31.719776875421));
#165422=CARTESIAN_POINT('Ctrl Pts',(-7.43893894768588,-3.26832461933621,
31.7201090827914));
#165423=CARTESIAN_POINT('Ctrl Pts',(-7.43251301203704,-3.28290943841109,
31.7207368546782));
#165424=CARTESIAN_POINT('Ctrl Pts',(-7.42947301878973,-3.28978338473071,
31.7210325186244));
#165425=CARTESIAN_POINT('Ctrl Pts',(-7.42257632345727,-3.30531968120215,
31.7217002797579));
#165426=CARTESIAN_POINT('Ctrl Pts',(-7.41871398326682,-3.31397952738481,
31.7220721410722));
#165427=CARTESIAN_POINT('Ctrl Pts',(-7.40733106373546,-3.33938182032185,
31.7231618858423));
#165428=CARTESIAN_POINT('Ctrl Pts',(-7.39976887469859,-3.35610563567921,
31.723877985281));
#165429=CARTESIAN_POINT('Ctrl Pts',(-7.34425757278031,-3.47776936141311,
31.7290770291821));
#165430=CARTESIAN_POINT('Ctrl Pts',(-7.29413866459474,-3.58169529646949,
31.7334535791792));
#165431=CARTESIAN_POINT('Ctrl Pts',(-6.92624761706545,-4.30477253661834,
31.763512276686));
#165432=CARTESIAN_POINT('Ctrl Pts',(-6.53227769766478,-4.88195569984678,
31.7858074583021));
#165433=CARTESIAN_POINT('Ctrl Pts',(-5.72851080681119,-5.78506499444763,
31.8270755685524));
#165434=CARTESIAN_POINT('Ctrl Pts',(-5.35200188795915,-6.13504839106379,
31.8452679142687));
#165435=CARTESIAN_POINT('Ctrl Pts',(-4.92273492580914,-6.46429875253288,
31.8661105862301));
#165436=CARTESIAN_POINT('Ctrl Pts',(-4.90034498314662,-6.48128818517181,
31.8671976901516));
#165437=CARTESIAN_POINT('Ctrl Pts',(-4.86756380394301,-6.50589549292822,
31.8687894175402));
#165438=CARTESIAN_POINT('Ctrl Pts',(-4.85724178199454,-6.51360543936992,
31.8692906285841));
#165439=CARTESIAN_POINT('Ctrl Pts',(-4.83910306685712,-6.52708690622081,
31.870171435037));
#165440=CARTESIAN_POINT('Ctrl Pts',(-4.83129426504732,-6.53286902491861,
31.8705506382207));
#165441=CARTESIAN_POINT('Ctrl Pts',(-4.81611834147574,-6.54406412393385,
31.87128762502));
#165442=CARTESIAN_POINT('Ctrl Pts',(-4.80875241663528,-6.54947870689944,
31.8716453488043));
#165443=CARTESIAN_POINT('Ctrl Pts',(-4.7911554999995,-6.56236825282006,
31.872499974418));
#165444=CARTESIAN_POINT('Ctrl Pts',(-4.7809161446393,-6.56983172744738,
31.872997296715));
#165445=CARTESIAN_POINT('Ctrl Pts',(-4.74427406698634,-6.5964091433548,
31.8747771183247));
#165446=CARTESIAN_POINT('Ctrl Pts',(-4.7177740023966,-6.61538800385599,
31.8760645471377));
#165447=CARTESIAN_POINT('Ctrl Pts',(-4.26146320762387,-6.93805314176026,
31.8982386239194));
#165448=CARTESIAN_POINT('Ctrl Pts',(-3.803319967873,-7.19939473096263,31.9206954705144));
#165449=CARTESIAN_POINT('Ctrl Pts',(-3.07124336563301,-7.52750796880281,
31.9563398205341));
#165450=CARTESIAN_POINT('Ctrl Pts',(-2.81371577029783,-7.62751008427983,
31.9688146292455));
#165451=CARTESIAN_POINT('Ctrl Pts',(-2.23350151034259,-7.81942572771731,
31.9963713431774));
#165452=CARTESIAN_POINT('Ctrl Pts',(-1.90918187769633,-7.90487129567162,
32.0114163764458));
#165453=CARTESIAN_POINT('Ctrl Pts',(-1.50483039132854,-7.98505632957965,
32.0291588720601));
#165454=CARTESIAN_POINT('Ctrl Pts',(-1.42894629344759,-7.99898444079158,
32.032444915965));
#165455=CARTESIAN_POINT('Ctrl Pts',(-1.26057295362894,-8.02741588302058,
32.0396251693525));
#165456=CARTESIAN_POINT('Ctrl Pts',(-1.168006801833,-8.04140604061696,32.0434990583466));
#165457=CARTESIAN_POINT('Ctrl Pts',(-1.02180671999395,-8.06092439326722,
32.0494830105657));
#165458=CARTESIAN_POINT('Ctrl Pts',(-0.968327469031864,-8.06752334727937,
32.0516429925421));
#165459=CARTESIAN_POINT('Ctrl Pts',(-0.901075451385636,-8.07514340355942,
32.0543267051102));
#165460=CARTESIAN_POINT('Ctrl Pts',(-0.887360830051181,-8.07666197867091,
32.0548723040733));
#165461=CARTESIAN_POINT('Ctrl Pts',(-0.865554461149743,-8.079020312903,
32.0557372208834));
#165462=CARTESIAN_POINT('Ctrl Pts',(-0.85746524469735,-8.07988286402116,
32.0560575012112));
#165463=CARTESIAN_POINT('Ctrl Pts',(-0.842241128964453,-8.08148308750492,
32.0566592336269));
#165464=CARTESIAN_POINT('Ctrl Pts',(-0.83510652622942,-8.08222346283701,
32.0569407973939));
#165465=CARTESIAN_POINT('Ctrl Pts',(-0.819083944226715,-8.08386472314833,
32.0575721711827));
#165466=CARTESIAN_POINT('Ctrl Pts',(-0.810195432698298,-8.08476040037743,
32.0579217690558));
#165467=CARTESIAN_POINT('Ctrl Pts',(-0.78759852629135,-8.08699980515402,
32.0588089090743));
#165468=CARTESIAN_POINT('Ctrl Pts',(-0.773888128070361,-8.08832334018192,
32.0593456475872));
#165469=CARTESIAN_POINT('Ctrl Pts',(-0.697694270364975,-8.09548321612502,
32.0623203557184));
#165470=CARTESIAN_POINT('Ctrl Pts',(-0.635147221693498,-8.10063047244903,
32.0647318494417));
#165471=CARTESIAN_POINT('Ctrl Pts',(0.168378852009121,-8.15739204748286,
32.0953873818867));
#165472=CARTESIAN_POINT('Ctrl Pts',(0.913042336203379,-8.10789647728921,
32.1207537490992));
#165473=CARTESIAN_POINT('Ctrl Pts',(1.93143525043313,-7.89793545087173,
32.1588528104005));
#165474=CARTESIAN_POINT('Ctrl Pts',(2.21868846704255,-7.82209940438737,
32.1699286086786));
#165475=CARTESIAN_POINT('Ctrl Pts',(2.76815283081297,-7.64432964278293,
32.1918659482263));
#165476=CARTESIAN_POINT('Ctrl Pts',(3.03050839562459,-7.54416725885528,
32.2026621821433));
#165477=CARTESIAN_POINT('Ctrl Pts',(3.35722349958563,-7.39963577039196,
32.2165222905908));
#165478=CARTESIAN_POINT('Ctrl Pts',(3.42685685089504,-7.3676462444179,32.2195030852754));
#165479=CARTESIAN_POINT('Ctrl Pts',(3.53498910794463,-7.31610569219422,
32.2241769749749));
#165480=CARTESIAN_POINT('Ctrl Pts',(3.57380252766926,-7.29722453859515,
32.2258638434513));
#165481=CARTESIAN_POINT('Ctrl Pts',(3.64605904908973,-7.26135990646171,
32.2290220055994));
#165482=CARTESIAN_POINT('Ctrl Pts',(3.67953859679297,-7.2444523590404,32.2304925471651));
#165483=CARTESIAN_POINT('Ctrl Pts',(3.7543243160916,-7.20603256772677,32.2337940616937));
#165484=CARTESIAN_POINT('Ctrl Pts',(3.79556497946751,-7.1843957922038,32.2356261845027));
#165485=CARTESIAN_POINT('Ctrl Pts',(3.91606353848306,-7.11984948404659,
32.2410141334521));
#165486=CARTESIAN_POINT('Ctrl Pts',(3.99479582906798,-7.0759745911311,32.2445791751044));
#165487=CARTESIAN_POINT('Ctrl Pts',(4.61584434419199,-6.71621536902354,
32.2730727282953));
#165488=CARTESIAN_POINT('Ctrl Pts',(5.12062435961599,-6.33977408395982,
32.2986405974118));
#165489=CARTESIAN_POINT('Ctrl Pts',(5.70083760110399,-5.79216076006512,
32.330974333908));
#165490=CARTESIAN_POINT('Ctrl Pts',(5.82095447564454,-5.67143418830815,
32.3378484183871));
#165491=CARTESIAN_POINT('Ctrl Pts',(5.98111482216503,-5.50000842473647,
32.3472392679594));
#165492=CARTESIAN_POINT('Ctrl Pts',(6.02447930698563,-5.45247433443074,
32.349805954986));
#165493=CARTESIAN_POINT('Ctrl Pts',(6.09875713207264,-5.36908644935416,
32.3542421932685));
#165494=CARTESIAN_POINT('Ctrl Pts',(6.12993011458357,-5.3334683550301,32.3561165797468));
#165495=CARTESIAN_POINT('Ctrl Pts',(6.17530749837897,-5.28069698435748,
32.3588628671799));
#165496=CARTESIAN_POINT('Ctrl Pts',(6.18975533905747,-5.26375457166278,
32.3597399703606));
#165497=CARTESIAN_POINT('Ctrl Pts',(6.21609387553395,-5.2326100148138,32.3613438143193));
#165498=CARTESIAN_POINT('Ctrl Pts',(6.22800596580027,-5.21842623111169,
32.3620710485733));
#165499=CARTESIAN_POINT('Ctrl Pts',(6.25477770944952,-5.18632674838755,
32.3637099141099));
#165500=CARTESIAN_POINT('Ctrl Pts',(6.2696091020324,-5.16838766433379,32.3646209617581));
#165501=CARTESIAN_POINT('Ctrl Pts',(6.30791479292844,-5.1216480762636,32.3669826121085));
#165502=CARTESIAN_POINT('Ctrl Pts',(6.3312690393567,-5.09274978989321,32.3684309980676));
#165503=CARTESIAN_POINT('Ctrl Pts',(6.49067129282625,-4.89271599841485,
32.378381180507));
#165504=CARTESIAN_POINT('Ctrl Pts',(6.61996362776574,-4.71630864668829,
32.3867815391193));
#165505=CARTESIAN_POINT('Ctrl Pts',(6.84009164366276,-4.38904683079814,
32.4019423483583));
#165506=CARTESIAN_POINT('Ctrl Pts',(6.93343889365346,-4.24004841101013,
32.408696778887));
#165507=CARTESIAN_POINT('Ctrl Pts',(7.07767457411369,-3.99230603235469,
32.4197679513116));
#165508=CARTESIAN_POINT('Ctrl Pts',(7.1315012617118,-3.89534007995964,32.4240626430327));
#165509=CARTESIAN_POINT('Ctrl Pts',(7.20524250773771,-3.75584439742551,
32.4301982667575));
#165510=CARTESIAN_POINT('Ctrl Pts',(7.22679945378193,-3.7141965975612,32.43202476766));
#165511=CARTESIAN_POINT('Ctrl Pts',(7.26399454421795,-3.64078618164708,
32.4352356884437));
#165512=CARTESIAN_POINT('Ctrl Pts',(7.27978791650323,-3.60910357839188,
32.436618695001));
#165513=CARTESIAN_POINT('Ctrl Pts',(7.31241338036254,-3.54256912571246,
32.4395176036191));
#165514=CARTESIAN_POINT('Ctrl Pts',(7.32920451766121,-3.50769818836835,
32.441033831366));
#165515=CARTESIAN_POINT('Ctrl Pts',(7.37324690373862,-3.41453627857709,
32.4450768217813));
#165516=CARTESIAN_POINT('Ctrl Pts',(7.40005587643885,-3.35603946132916,
32.4476073888213));
#165517=CARTESIAN_POINT('Ctrl Pts',(7.5653304115969,-2.98380091827299,32.4636627246735));
#165518=CARTESIAN_POINT('Ctrl Pts',(7.68450946151777,-2.66187903421615,
32.4773568973211));
#165519=CARTESIAN_POINT('Ctrl Pts',(7.83512182652158,-2.15951533750572,
32.4983029906778));
#165520=CARTESIAN_POINT('Ctrl Pts',(7.88141179818942,-1.98393284992453,
32.5055431625944));
#165521=CARTESIAN_POINT('Ctrl Pts',(7.93145751493271,-1.76452886687975,
32.5144374058751));
#165522=CARTESIAN_POINT('Ctrl Pts',(7.94079210973867,-1.72203401057349,
32.5161529534149));
#165523=CARTESIAN_POINT('Ctrl Pts',(7.95431498375473,-1.65802322609323,
32.5187252856981));
#165524=CARTESIAN_POINT('Ctrl Pts',(7.95875820721713,-1.63656215372334,
32.5195856981216));
#165525=CARTESIAN_POINT('Ctrl Pts',(7.96707320446151,-1.59556533455696,
32.5212254835987));
#165526=CARTESIAN_POINT('Ctrl Pts',(7.97096007348666,-1.57603289691244,
32.5220051002901));
#165527=CARTESIAN_POINT('Ctrl Pts',(7.97976232866371,-1.53093387861084,
32.5238016156476));
#165528=CARTESIAN_POINT('Ctrl Pts',(7.9846267308726,-1.50535754483411,32.5248178085377));
#165529=CARTESIAN_POINT('Ctrl Pts',(7.99750618907957,-1.43582001361855,
32.5275740537169));
#165530=CARTESIAN_POINT('Ctrl Pts',(8.00528167191042,-1.39181526713075,
32.5293111077043));
#165531=CARTESIAN_POINT('Ctrl Pts',(8.05157034809311,-1.11661778338643,
32.5401359972281));
#165532=CARTESIAN_POINT('Ctrl Pts',(8.08042845627572,-0.883910872356917,
32.5491235740261));
#165533=CARTESIAN_POINT('Ctrl Pts',(8.11659211714103,-0.433495816826945,
32.5664456895671));
#165534=CARTESIAN_POINT('Ctrl Pts',(8.12528685465813,-0.216100174705383,
32.5747735029619));
#165535=CARTESIAN_POINT('Ctrl Pts',(8.1252148313152,0.207564060050729,32.5910810763637));
#165536=CARTESIAN_POINT('Ctrl Pts',(8.11733180208154,0.413668928979134,
32.5990503936479));
#165537=CARTESIAN_POINT('Ctrl Pts',(8.09637390907078,0.687860569421236,
32.6097490170675));
#165538=CARTESIAN_POINT('Ctrl Pts',(8.09025818525974,0.756402722435157,
32.6124313259992));
#165539=CARTESIAN_POINT('Ctrl Pts',(8.07813975817032,0.875158272765247,
32.6170935771905));
#165540=CARTESIAN_POINT('Ctrl Pts',(8.07253755769331,0.925408727783274,
32.6190710091661));
#165541=CARTESIAN_POINT('Ctrl Pts',(8.05956375811885,1.03267845500922,32.6233025143087));
#165542=CARTESIAN_POINT('Ctrl Pts',(8.0520552479269,1.08967840149722,32.6255572385031));
#165543=CARTESIAN_POINT('Ctrl Pts',(8.03043517581979,1.24135428422705,32.6315738916608));
#165544=CARTESIAN_POINT('Ctrl Pts',(8.01525451054449,1.33586848182048,32.6353407045382));
#165545=CARTESIAN_POINT('Ctrl Pts',(7.973354691458,1.57021131428595,32.6447229341092));
#165546=CARTESIAN_POINT('Ctrl Pts',(7.94462414572993,1.70964782061066,32.6503437383102));
#165547=CARTESIAN_POINT('Ctrl Pts',(7.88309418467115,1.97305281031318,32.6610220856643));
#165548=CARTESIAN_POINT('Ctrl Pts',(7.85099411561768,2.09714160038705,32.6660783754364));
#165549=CARTESIAN_POINT('Ctrl Pts',(7.80352648557912,2.26422971382283,32.6729098821461));
#165550=CARTESIAN_POINT('Ctrl Pts',(7.79071236860552,2.30793470785181,32.6746989234244));
#165551=CARTESIAN_POINT('Ctrl Pts',(7.76501602029368,2.39292370613741,32.6781810876642));
#165552=CARTESIAN_POINT('Ctrl Pts',(7.75217030621685,2.43421716674739,32.67987437888));
#165553=CARTESIAN_POINT('Ctrl Pts',(7.70549457704128,2.58014201066397,32.6858662049425));
#165554=CARTESIAN_POINT('Ctrl Pts',(7.66987079878365,2.68418731722489,32.6901531768509));
#165555=CARTESIAN_POINT('Ctrl Pts',(7.54792257124269,3.0180829679344,32.7039996722679));
#165556=CARTESIAN_POINT('Ctrl Pts',(7.45329089396366,3.24475181393152,32.7135410718613));
#165557=CARTESIAN_POINT('Ctrl Pts',(7.32233868847677,3.52233096797071,32.7255396766941));
#165558=CARTESIAN_POINT('Ctrl Pts',(7.29550617516009,3.57757584597496,32.7279435012674));
#165559=CARTESIAN_POINT('Ctrl Pts',(7.24334663466436,3.68193840358759,32.7325170129718));
#165560=CARTESIAN_POINT('Ctrl Pts',(7.21813976619774,3.73111232306919,32.7346858883515));
#165561=CARTESIAN_POINT('Ctrl Pts',(7.15713918955166,3.84718101541651,32.7398401442193));
#165562=CARTESIAN_POINT('Ctrl Pts',(7.12090634880916,3.91383901596761,32.7428281175572));
#165563=CARTESIAN_POINT('Ctrl Pts',(6.97427729022818,4.1748159634934,32.7546431837811));
#165564=CARTESIAN_POINT('Ctrl Pts',(6.85681840337655,4.36505116611303,32.7635168717157));
#165565=CARTESIAN_POINT('Ctrl Pts',(6.61715442447659,4.71961543042617,32.7805929966325));
#165566=CARTESIAN_POINT('Ctrl Pts',(6.49628584743972,4.88464657636596,32.7887818613617));
#165567=CARTESIAN_POINT('Ctrl Pts',(6.22636072498286,5.2254314730179,32.8061822103099));
#165568=CARTESIAN_POINT('Ctrl Pts',(6.0757915542451,5.39976487694747,32.8153852092055));
#165569=CARTESIAN_POINT('Ctrl Pts',(5.88393646439128,5.60370000057754,32.826458874718));
#165570=CARTESIAN_POINT('Ctrl Pts',(5.84951953762156,5.63961729505303,32.8284213410047));
#165571=CARTESIAN_POINT('Ctrl Pts',(5.79732235758433,5.69309804814422,32.8313606706472));
#165572=CARTESIAN_POINT('Ctrl Pts',(5.77978746277707,5.71089912315492,32.8323419441815));
#165573=CARTESIAN_POINT('Ctrl Pts',(5.748265107292,5.74260610010903,32.8340948228185));
#165574=CARTESIAN_POINT('Ctrl Pts',(5.73430861107618,5.75654247973182,32.8348670439069));
#165575=CARTESIAN_POINT('Ctrl Pts',(5.70396513175934,5.78662237184294,32.8365375063944));
#165576=CARTESIAN_POINT('Ctrl Pts',(5.68756014066338,5.80274731035957,32.8374352974443));
#165577=CARTESIAN_POINT('Ctrl Pts',(5.63507108063098,5.853903887184,32.840291272097));
#165578=CARTESIAN_POINT('Ctrl Pts',(5.59873007104388,5.88867034602701,32.8422439569608));
#165579=CARTESIAN_POINT('Ctrl Pts',(5.50923195387236,5.97271331004832,32.8469976905782));
#165580=CARTESIAN_POINT('Ctrl Pts',(5.45573363886717,6.0216203443547,32.8497927398034));
#165581=CARTESIAN_POINT('Ctrl Pts',(5.21434179889784,6.23643765490802,32.8622222596676));
#165582=CARTESIAN_POINT('Ctrl Pts',(5.01948474468476,6.39431693517205,32.871778192934));
#165583=CARTESIAN_POINT('Ctrl Pts',(4.65316637916709,6.66404145962618,32.8892158365611));
#165584=CARTESIAN_POINT('Ctrl Pts',(4.48418521203038,6.77890017180955,32.8970725600345));
#165585=CARTESIAN_POINT('Ctrl Pts',(4.26225348471805,6.91781741855808,32.9072289483574));
#165586=CARTESIAN_POINT('Ctrl Pts',(4.21312639666072,6.94784632284871,32.9094671584578));
#165587=CARTESIAN_POINT('Ctrl Pts',(4.13484063120782,6.99456279898814,32.9130192694158));
#165588=CARTESIAN_POINT('Ctrl Pts',(4.10589040136404,7.01159609485373,32.9143297340322));
#165589=CARTESIAN_POINT('Ctrl Pts',(4.04609244235053,7.04628175971614,32.9170304132808));
#165590=CARTESIAN_POINT('Ctrl Pts',(4.01523283882967,7.06391222542537,32.9184208089124));
#165591=CARTESIAN_POINT('Ctrl Pts',(3.94252577172092,7.10482027033506,32.9216891320663));
#165592=CARTESIAN_POINT('Ctrl Pts',(3.90058628947827,7.12793147460847,32.9235685934922));
#165593=CARTESIAN_POINT('Ctrl Pts',(3.75465751071743,7.20667348580747,32.9300888076946));
#165594=CARTESIAN_POINT('Ctrl Pts',(3.64966368146107,7.26040979659319,32.9347464889797));
#165595=CARTESIAN_POINT('Ctrl Pts',(3.33667353415491,7.41209423074448,32.9485329851351));
#165596=CARTESIAN_POINT('Ctrl Pts',(3.12564873000594,7.50352249827698,32.9577063713795));
#165597=CARTESIAN_POINT('Ctrl Pts',(2.75496299822714,7.64577082206427,32.9735391667336));
#165598=CARTESIAN_POINT('Ctrl Pts',(2.5970800979167,7.70083166089534,32.9801968469499));
#165599=CARTESIAN_POINT('Ctrl Pts',(2.40494039904607,7.76125776786437,32.9881549154239));
#165600=CARTESIAN_POINT('Ctrl Pts',(2.37220556374065,7.7713255780076,32.9895057097309));
#165601=CARTESIAN_POINT('Ctrl Pts',(2.32164826973755,7.78652559171573,32.9915836394985));
#165602=CARTESIAN_POINT('Ctrl Pts',(2.30387031532559,7.79180422312438,32.9923127453324));
#165603=CARTESIAN_POINT('Ctrl Pts',(2.2700682077112,7.8017149472182,32.9936959194609));
#165604=CARTESIAN_POINT('Ctrl Pts',(2.25404755821642,7.80635865129979,32.9943501568963));
#165605=CARTESIAN_POINT('Ctrl Pts',(2.21501133281587,7.81754340275779,32.995940950572));
#165606=CARTESIAN_POINT('Ctrl Pts',(2.19198091453339,7.82403219156989,32.9968766664075));
#165607=CARTESIAN_POINT('Ctrl Pts',(2.11420729352716,7.8455744516473,33.0000275551866));
#165608=CARTESIAN_POINT('Ctrl Pts',(2.05933483172817,7.8601559194015,33.002235600231));
#165609=CARTESIAN_POINT('Ctrl Pts',(1.92509061931744,7.89432686384117,33.007605324992));
#165610=CARTESIAN_POINT('Ctrl Pts',(1.84556714299306,7.91329593870069,33.0107589549172));
#165611=CARTESIAN_POINT('Ctrl Pts',(1.37617050839793,8.01780234030301,33.0292443542907));
#165612=CARTESIAN_POINT('Ctrl Pts',(0.980704518829582,8.07571821241874,
33.0443100834936));
#165613=CARTESIAN_POINT('Ctrl Pts',(0.187528273138893,8.13273611939767,
33.0745516796444));
#165614=CARTESIAN_POINT('Ctrl Pts',(-0.209069287422505,8.13221031865402,
33.0896887638983));
#165615=CARTESIAN_POINT('Ctrl Pts',(-0.67712071932834,8.09731843804846,
33.1079189984643));
#165616=CARTESIAN_POINT('Ctrl Pts',(-0.75012628911817,8.09088183237677,
33.1107724829534));
#165617=CARTESIAN_POINT('Ctrl Pts',(-0.86575850440745,8.07910849276919,
33.1153094545543));
#165618=CARTESIAN_POINT('Ctrl Pts',(-0.908447256264389,8.07441981770192,
33.1169881647341));
#165619=CARTESIAN_POINT('Ctrl Pts',(-0.988366222594918,8.06500019117109,
33.1201382782823));
#165620=CARTESIAN_POINT('Ctrl Pts',(-1.02560476084279,8.06034929377814,
33.1216090816124));
#165621=CARTESIAN_POINT('Ctrl Pts',(-1.10929159725117,8.04930791397624,
33.1249213741454));
#165622=CARTESIAN_POINT('Ctrl Pts',(-1.15571946767966,8.04277304381749,
33.1267637856276));
#165623=CARTESIAN_POINT('Ctrl Pts',(-1.29662017735922,8.0216955794533,33.1323702017767));
#165624=CARTESIAN_POINT('Ctrl Pts',(-1.39089500128511,8.00588750870998,
33.1361419851181));
#165625=CARTESIAN_POINT('Ctrl Pts',(-1.87661071241143,7.9156038243077,33.1556837957243));
#165626=CARTESIAN_POINT('Ctrl Pts',(-2.26245830105097,7.81407215881483,
33.1715106457957));
#165627=CARTESIAN_POINT('Ctrl Pts',(-3.17441249612268,7.50086161851529,
33.2107606324346));
#165628=CARTESIAN_POINT('Ctrl Pts',(-3.68885167627541,7.26168892426218,
33.2346432486699));
#165629=CARTESIAN_POINT('Ctrl Pts',(-4.44555375225147,6.80857926200083,
33.271950159523));
#165630=CARTESIAN_POINT('Ctrl Pts',(-4.70716935697516,6.63040479873872,
33.2852665966486));
#165631=CARTESIAN_POINT('Ctrl Pts',(-5.01309809244351,6.39479612948546,
33.3009020541447));
#165632=CARTESIAN_POINT('Ctrl Pts',(-5.06790667848614,6.35144804333882,
33.3037050848216));
#165633=CARTESIAN_POINT('Ctrl Pts',(-5.13325094679323,6.29838286980679,
33.3070426977266));
#165634=CARTESIAN_POINT('Ctrl Pts',(-5.14432798413,6.2893387293319,33.3076083333918));
#165635=CARTESIAN_POINT('Ctrl Pts',(-5.16241166554682,6.27449409067359,
33.3085314295035));
#165636=CARTESIAN_POINT('Ctrl Pts',(-5.16943252351469,6.26871100658931,
33.3088897341949));
#165637=CARTESIAN_POINT('Ctrl Pts',(-5.18198469426588,6.2583363498778,33.3095301584647));
#165638=CARTESIAN_POINT('Ctrl Pts',(-5.187519646386,6.25374920816197,33.3098124988295));
#165639=CARTESIAN_POINT('Ctrl Pts',(-5.19922620390779,6.24402105709245,
33.3104095184286));
#165640=CARTESIAN_POINT('Ctrl Pts',(-5.20539629162219,6.238878226779,33.3107241041577));
#165641=CARTESIAN_POINT('Ctrl Pts',(-5.22179231492686,6.22517072094772,
33.3115598264899));
#165642=CARTESIAN_POINT('Ctrl Pts',(-5.23200483001681,6.21658997736299,
33.3120801209566));
#165643=CARTESIAN_POINT('Ctrl Pts',(-5.27941937711179,6.17655180146707,
33.314494392046));
#165644=CARTESIAN_POINT('Ctrl Pts',(-5.31635998682655,6.14478460519842,
33.3163714649488));
#165645=CARTESIAN_POINT('Ctrl Pts',(-5.63828225135742,5.86287020820128,
33.3326776606034));
#165646=CARTESIAN_POINT('Ctrl Pts',(-5.9057365426996,5.59337054007154,33.345885074585));
#165647=CARTESIAN_POINT('Ctrl Pts',(-6.47473094779781,4.93352346552174,
33.3753885300817));
#165648=CARTESIAN_POINT('Ctrl Pts',(-6.76154366202761,4.53247494956825,
33.3914161624046));
#165649=CARTESIAN_POINT('Ctrl Pts',(-7.23483215105991,3.72479549759572,
33.4235711503161));
#165650=CARTESIAN_POINT('Ctrl Pts',(-7.42754090550808,3.32392553683809,
33.4394835533475));
#165651=CARTESIAN_POINT('Ctrl Pts',(-7.59795117892184,2.87955605455806,
33.4577833649623));
#165652=CARTESIAN_POINT('Ctrl Pts',(-7.60919785367271,2.84970405217055,
33.4590155157355));
#165653=CARTESIAN_POINT('Ctrl Pts',(-7.62462518739809,2.80801280673342,
33.4607403887706));
#165654=CARTESIAN_POINT('Ctrl Pts',(-7.62895470053215,2.79622877222548,
33.4612283736669));
#165655=CARTESIAN_POINT('Ctrl Pts',(-7.63637918944062,2.77587525870261,
33.4620720121724));
#165656=CARTESIAN_POINT('Ctrl Pts',(-7.63948709919662,2.76731050612988,
33.4624272545863));
#165657=CARTESIAN_POINT('Ctrl Pts',(-7.64588545697751,2.7495850390564,33.4631629581514));
#165658=CARTESIAN_POINT('Ctrl Pts',(-7.64917386217789,2.74042360477825,
33.4635434833142));
#165659=CARTESIAN_POINT('Ctrl Pts',(-7.65681295154492,2.71902037095412,
33.4644331275457));
#165660=CARTESIAN_POINT('Ctrl Pts',(-7.66115074698399,2.70677401766435,
33.464942653103));
#165661=CARTESIAN_POINT('Ctrl Pts',(-7.67497213568423,2.66745443768777,
33.4665802010536));
#165662=CARTESIAN_POINT('Ctrl Pts',(-7.68434168568798,2.64034151158299,
33.46771181527));
#165663=CARTESIAN_POINT('Ctrl Pts',(-7.82199843728846,2.23506073598694,
33.4846641574656));
#165664=CARTESIAN_POINT('Ctrl Pts',(-7.92236684617675,1.84802748926903,
33.5013711828175));
#165665=CARTESIAN_POINT('Ctrl Pts',(-8.11431059827551,0.793631006419028,
33.5479877968932));
#165666=CARTESIAN_POINT('Ctrl Pts',(-8.15214524576274,0.119707986867872,
33.5790717026292));
#165667=CARTESIAN_POINT('Ctrl Pts',(-8.08979768496112,-0.797344986955767,
33.6189498864962));
#165668=CARTESIAN_POINT('Ctrl Pts',(-8.06184921967412,-1.04269300039899,
33.6293382421936));
#165669=CARTESIAN_POINT('Ctrl Pts',(-8.01935850934616,-1.30768503771266,
33.640054614647));
#165670=CARTESIAN_POINT('Ctrl Pts',(-8.01586544542677,-1.32892897937696,
33.6409106423736));
#165671=CARTESIAN_POINT('Ctrl Pts',(-8.01064672141316,-1.35989860736942,
33.6421543496556));
#165672=CARTESIAN_POINT('Ctrl Pts',(-8.00898771469601,-1.36963531809947,
33.6425447565389));
#165673=CARTESIAN_POINT('Ctrl Pts',(-8.00602229080303,-1.38684976259633,
33.6432339491426));
#165674=CARTESIAN_POINT('Ctrl Pts',(-8.00472314284669,-1.39432872441258,
33.6435330258265));
#165675=CARTESIAN_POINT('Ctrl Pts',(-8.00200936854663,-1.40982263719879,
33.6441519072817));
#165676=CARTESIAN_POINT('Ctrl Pts',(-8.00059317627839,-1.41783730764706,
33.6444716499121));
#165677=CARTESIAN_POINT('Ctrl Pts',(-7.99770100236625,-1.43406270198511,
33.645118184647));
#165678=CARTESIAN_POINT('Ctrl Pts',(-7.99622441285837,-1.44227330847059,
33.6454449527693));
#165679=CARTESIAN_POINT('Ctrl Pts',(-7.99036609639732,-1.47456305777359,
33.6467284970901));
#165680=CARTESIAN_POINT('Ctrl Pts',(-7.98588820377531,-1.49862476222004,
33.6476816158453));
#165681=CARTESIAN_POINT('Ctrl Pts',(-7.97484755090284,-1.55649614028407,
33.6499665775846));
#165682=CARTESIAN_POINT('Ctrl Pts',(-7.96817838746579,-1.59028516925733,
33.6512945876178));
#165683=CARTESIAN_POINT('Ctrl Pts',(-7.87812716199637,-2.03173259818602,
33.6685749822379));
#165684=CARTESIAN_POINT('Ctrl Pts',(-7.76375964116079,-2.43246798265785,
33.6835144469549));
#165685=CARTESIAN_POINT('Ctrl Pts',(-7.40130286211927,-3.41083372520171,
33.7209762249408));
#165686=CARTESIAN_POINT('Ctrl Pts',(-7.1160617334785,-3.97173797477331,
33.7435258618707));
#165687=CARTESIAN_POINT('Ctrl Pts',(-6.71934526035408,-4.56926660170042,
33.7709207418354));
#165688=CARTESIAN_POINT('Ctrl Pts',(-6.66828894152333,-4.64345994866827,
33.7743827768551));
#165689=CARTESIAN_POINT('Ctrl Pts',(-6.59601827954355,-4.74483049751722,
33.7791982912188));
#165690=CARTESIAN_POINT('Ctrl Pts',(-6.57584819510753,-4.77274492226766,
33.7805334602269));
#165691=CARTESIAN_POINT('Ctrl Pts',(-6.54320851785536,-4.81731696733,33.7826800456467));
#165692=CARTESIAN_POINT('Ctrl Pts',(-6.53085130460895,-4.83405644417927,
33.7834895701032));
#165693=CARTESIAN_POINT('Ctrl Pts',(-6.50537813431219,-4.86828726139497,
33.7851518572876));
#165694=CARTESIAN_POINT('Ctrl Pts',(-6.49225559268988,-4.88577351561603,
33.7860047104204));
#165695=CARTESIAN_POINT('Ctrl Pts',(-6.46424224172423,-4.92279016060579,
33.7878181159801));
#165696=CARTESIAN_POINT('Ctrl Pts',(-6.44933313984825,-4.94230642215768,
33.7887789728178));
#165697=CARTESIAN_POINT('Ctrl Pts',(-6.40603611082097,-4.99845341838384,
33.7915574136489));
#165698=CARTESIAN_POINT('Ctrl Pts',(-6.37742309055053,-5.03490912647706,
33.7933789086692));
#165699=CARTESIAN_POINT('Ctrl Pts',(-6.31253952978128,-5.11613643932448,
33.7974782060486));
#165700=CARTESIAN_POINT('Ctrl Pts',(-6.27610156364835,-5.16077091717461,
33.79975909037));
#165701=CARTESIAN_POINT('Ctrl Pts',(-5.97297074854373,-5.52413045624327,
33.8185697154205));
#165702=CARTESIAN_POINT('Ctrl Pts',(-5.68267465692152,-5.82233396317462,
33.8356029037756));
#165703=CARTESIAN_POINT('Ctrl Pts',(-4.95011341237386,-6.46764740613027,
33.8765686475052));
#165704=CARTESIAN_POINT('Ctrl Pts',(-4.49214409700214,-6.79372582829143,
33.900783458123));
#165705=CARTESIAN_POINT('Ctrl Pts',(-3.93214788560305,-7.11089089617738,
33.927214717837));
#165706=CARTESIAN_POINT('Ctrl Pts',(-3.85941100478618,-7.15062958733917,
33.9305880209453));
#165707=CARTESIAN_POINT('Ctrl Pts',(-3.74723530029025,-7.20970473276271,
33.9356877646213));
#165708=CARTESIAN_POINT('Ctrl Pts',(-3.70822729570702,-7.22984544342074,
33.9374424741675));
#165709=CARTESIAN_POINT('Ctrl Pts',(-3.65677885777473,-7.25588349766887,
33.9397307565242));
#165710=CARTESIAN_POINT('Ctrl Pts',(-3.64448432787603,-7.26206657453796,
33.9402756423671));
#165711=CARTESIAN_POINT('Ctrl Pts',(-3.62544209724839,-7.27158262002453,
33.9411165244803));
#165712=CARTESIAN_POINT('Ctrl Pts',(-3.618705404597,-7.27493748396271,33.9414134183786));
#165713=CARTESIAN_POINT('Ctrl Pts',(-3.60525495409538,-7.28161248460411,
33.9420050055379));
#165714=CARTESIAN_POINT('Ctrl Pts',(-3.59854124752889,-7.28493270732433,
33.9422997022343));
#165715=CARTESIAN_POINT('Ctrl Pts',(-3.58360488734655,-7.29229370728755,
33.9429540050611));
#165716=CARTESIAN_POINT('Ctrl Pts',(-3.57537996334899,-7.29632987333364,
33.9433134149623));
#165717=CARTESIAN_POINT('Ctrl Pts',(-3.55341736040113,-7.30706139126438,
33.9442707216236));
#165718=CARTESIAN_POINT('Ctrl Pts',(-3.5396675495396,-7.31373193080876,
33.9448675401887));
#165719=CARTESIAN_POINT('Ctrl Pts',(-3.45276213509059,-7.35559046718009,
33.9486235631744));
#165720=CARTESIAN_POINT('Ctrl Pts',(-3.37910137013628,-7.38971937890137,
33.9517334707855));
#165721=CARTESIAN_POINT('Ctrl Pts',(-3.15744706403265,-7.48840976585039,
33.9608647035056));
#165722=CARTESIAN_POINT('Ctrl Pts',(-3.00802815570864,-7.54967042149677,
33.9667327855221));
#165723=CARTESIAN_POINT('Ctrl Pts',(-2.54822416056238,-7.72236667659126,
33.9841656014499));
#165724=CARTESIAN_POINT('Ctrl Pts',(-2.23278909703562,-7.81940290782685,
33.9952850637137));
#165725=CARTESIAN_POINT('Ctrl Pts',(-1.66537994019427,-7.95680548702152,
34.014919921732));
#165726=CARTESIAN_POINT('Ctrl Pts',(-1.41577032388048,-8.00498822318895,
34.0234356572105));
#165727=CARTESIAN_POINT('Ctrl Pts',(-0.675254841694477,-8.11220772453912,
34.0490198485259));
#165728=CARTESIAN_POINT('Ctrl Pts',(-0.180803789254281,-8.13825099129294,
34.0665743506315));
#165729=CARTESIAN_POINT('Ctrl Pts',(0.345096415947835,-8.11798204425424,
34.0868109876204));
#165730=CARTESIAN_POINT('Ctrl Pts',(0.377258515518901,-8.11655099112909,
34.0880544864004));
#165731=CARTESIAN_POINT('Ctrl Pts',(0.421998725643097,-8.11429377648015,
34.0897926938534));
#165732=CARTESIAN_POINT('Ctrl Pts',(0.434584875729363,-8.11362942212407,
34.0902826047125));
#165733=CARTESIAN_POINT('Ctrl Pts',(0.456279798934822,-8.11243363973997,
34.091128677513));
#165734=CARTESIAN_POINT('Ctrl Pts',(0.465389332093407,-8.11191614743428,
34.0914844255091));
#165735=CARTESIAN_POINT('Ctrl Pts',(0.484207668082196,-8.11081531646407,
34.0922203388239));
#165736=CARTESIAN_POINT('Ctrl Pts',(0.493916332083764,-8.11022988698553,
34.0926005656683));
#165737=CARTESIAN_POINT('Ctrl Pts',(0.516544678422956,-8.10882462185563,
34.0934880823108));
#165738=CARTESIAN_POINT('Ctrl Pts',(0.529463482458952,-8.10799134013463,
34.0939957705801));
#165739=CARTESIAN_POINT('Ctrl Pts',(0.570754115866871,-8.10522892853629,
34.0956216247193));
#165740=CARTESIAN_POINT('Ctrl Pts',(0.599117688160791,-8.10318173439424,
34.0967432944178));
#165741=CARTESIAN_POINT('Ctrl Pts',(1.22279740266531,-8.05487401314389,
34.1215150127503));
#165742=CARTESIAN_POINT('Ctrl Pts',(1.81114176485396,-7.94328741004424,
34.1472219782726));
#165743=CARTESIAN_POINT('Ctrl Pts',(2.67870071124136,-7.67728061249906,
34.1878190799151));
#165744=CARTESIAN_POINT('Ctrl Pts',(2.97006393104812,-7.56933237039539,
34.2019094294658));
#165745=CARTESIAN_POINT('Ctrl Pts',(3.65366591513917,-7.27049966854171,
34.2353702913956));
#165746=CARTESIAN_POINT('Ctrl Pts',(4.0381867641873,-7.06417741010834,34.2545264991492));
#165747=CARTESIAN_POINT('Ctrl Pts',(4.43007032808527,-6.81139492856672,
34.2732198434407));
#165748=CARTESIAN_POINT('Ctrl Pts',(4.45569197321239,-6.79466210065862,
34.274438504391));
#165749=CARTESIAN_POINT('Ctrl Pts',(4.49088419683294,-6.7713943137474,34.2761083698036));
#165750=CARTESIAN_POINT('Ctrl Pts',(4.50053601990347,-6.76498317493022,
34.2765659288214));
#165751=CARTESIAN_POINT('Ctrl Pts',(4.51589424193868,-6.75473419527171,
34.2772933942727));
#165752=CARTESIAN_POINT('Ctrl Pts',(4.52160951732829,-6.75090973324119,
34.2775639710552));
#165753=CARTESIAN_POINT('Ctrl Pts',(4.53272636786691,-6.74345027611619,
34.2780900220962));
#165754=CARTESIAN_POINT('Ctrl Pts',(4.53812844082812,-6.73981603660379,
34.2783455332897));
#165755=CARTESIAN_POINT('Ctrl Pts',(4.55105260527848,-6.7310987339041,34.2789565668001));
#165756=CARTESIAN_POINT('Ctrl Pts',(4.5585705673934,-6.72600954240551,34.2793117900612));
#165757=CARTESIAN_POINT('Ctrl Pts',(4.57419979502485,-6.71539128867663,
34.2800498580517));
#165758=CARTESIAN_POINT('Ctrl Pts',(4.58230960524889,-6.70986010342584,
34.2804326005274));
#165759=CARTESIAN_POINT('Ctrl Pts',(4.62268420443701,-6.68221582344231,
34.282337023455));
#165760=CARTESIAN_POINT('Ctrl Pts',(4.65479935830878,-6.65988442553224,
34.2838484920453));
#165761=CARTESIAN_POINT('Ctrl Pts',(4.76582298799821,-6.5814883085693,34.2890663176853));
#165762=CARTESIAN_POINT('Ctrl Pts',(4.8438913464674,-6.52424512882819,34.2927223269575));
#165763=CARTESIAN_POINT('Ctrl Pts',(5.15829651597877,-6.2849544377533,34.3074663557614));
#165764=CARTESIAN_POINT('Ctrl Pts',(5.3855523049217,-6.09134742262948,34.3181820223332));
#165765=CARTESIAN_POINT('Ctrl Pts',(5.85317095283381,-5.6462946223562,34.3413139571226));
#165766=CARTESIAN_POINT('Ctrl Pts',(6.08908327940377,-5.39104025281047,
34.353706048313));
#165767=CARTESIAN_POINT('Ctrl Pts',(6.3156060260362,-5.11204028791617,34.3668330060366));
#165768=CARTESIAN_POINT('Ctrl Pts',(6.32324826142825,-5.10258432612098,
34.3672774078631));
#165769=CARTESIAN_POINT('Ctrl Pts',(6.37582500265867,-5.03723007467763,
34.3703454820283));
#165770=CARTESIAN_POINT('Ctrl Pts',(6.42003863745138,-4.98075647501979,
34.3729796857612));
#165771=CARTESIAN_POINT('Ctrl Pts',(6.74175157660048,-4.55843405440522,
34.3925682400157));
#165772=CARTESIAN_POINT('Ctrl Pts',(6.98852941388315,-4.17024653751808,
34.4100350729619));
#165773=CARTESIAN_POINT('Ctrl Pts',(7.25367663233563,-3.66288218579916,
34.4321517180385));
#165774=CARTESIAN_POINT('Ctrl Pts',(7.304058251123,-3.56135695340024,34.4365456890109));
#165775=CARTESIAN_POINT('Ctrl Pts',(7.37199521170549,-3.41694525725551,
34.4427610488648));
#165776=CARTESIAN_POINT('Ctrl Pts',(7.39133288143138,-3.37491133293512,
34.4445660701108));
#165777=CARTESIAN_POINT('Ctrl Pts',(7.42602012554167,-3.297784043843,34.447871342758));
#165778=CARTESIAN_POINT('Ctrl Pts',(7.44148260983002,-3.26274287353098,
34.4493705108081));
#165779=CARTESIAN_POINT('Ctrl Pts',(7.47061059140215,-3.19544861651566,
34.4522451476228));
#165780=CARTESIAN_POINT('Ctrl Pts',(7.4843164217422,-3.1632138969406,34.4536202078877));
#165781=CARTESIAN_POINT('Ctrl Pts',(7.51264123705642,-3.09538204469376,
34.4565100247779));
#165782=CARTESIAN_POINT('Ctrl Pts',(7.52721663338313,-3.05976765445253,
34.4580251494618));
#165783=CARTESIAN_POINT('Ctrl Pts',(7.5611756689012,-2.97507881858999,34.4616233450183));
#165784=CARTESIAN_POINT('Ctrl Pts',(7.5803353415005,-2.92591653101328,34.4637084196999));
#165785=CARTESIAN_POINT('Ctrl Pts',(7.72816897301282,-2.53538564026938,
34.4802453549446));
#165786=CARTESIAN_POINT('Ctrl Pts',(7.83419583355483,-2.1858960060258,34.4949002505393));
#165787=CARTESIAN_POINT('Ctrl Pts',(7.94489085578469,-1.70716576582002,
34.5148131290753));
#165788=CARTESIAN_POINT('Ctrl Pts',(7.97051813427188,-1.58320756061054,
34.5199534865266));
#165789=CARTESIAN_POINT('Ctrl Pts',(8.0247580622937,-1.28598935142951,34.5322320223368));
#165790=CARTESIAN_POINT('Ctrl Pts',(8.05067070629606,-1.11230033672865,
34.5393702383502));
#165791=CARTESIAN_POINT('Ctrl Pts',(8.0985327887415,-0.700435079277564,
34.5561678856575));
#165792=CARTESIAN_POINT('Ctrl Pts',(8.11563527375969,-0.461855511904104,
34.5657978978396));
#165793=CARTESIAN_POINT('Ctrl Pts',(8.1232414279722,-0.184654997437717,
34.5767943916186));
#165794=CARTESIAN_POINT('Ctrl Pts',(8.12402025543175,-0.146436607375029,
34.578306231622));
#165795=CARTESIAN_POINT('Ctrl Pts',(8.12479443884352,-0.0883121798156752,
34.5805985308869));
#165796=CARTESIAN_POINT('Ctrl Pts',(8.1249863921664,-0.0684094129417031,
34.5813822011467));
#165797=CARTESIAN_POINT('Ctrl Pts',(8.1251678565596,-0.0380128451970877,
34.5825771148768));
#165798=CARTESIAN_POINT('Ctrl Pts',(8.12521017267968,-0.0275195204497364,
34.5829892674196));
#165799=CARTESIAN_POINT('Ctrl Pts',(8.12524185021272,-0.0124023265984525,
34.5835825578118));
#165800=CARTESIAN_POINT('Ctrl Pts',(8.12524759234424,-0.00777851420400875,
34.5837639600232));
#165801=CARTESIAN_POINT('Ctrl Pts',(8.12524938758068,-0.00315469804944397,
34.5839452996515));
#165802=CARTESIAN_POINT('',(8.12524999535401,0.000274771867430455,38.5832974955445));
#165803=CARTESIAN_POINT('Ctrl Pts',(8.12524938756529,-0.00315473768782347,
34.5839452980969));
#165804=CARTESIAN_POINT('Ctrl Pts',(8.12525212190974,0.00388775925662743,
34.584221495017));
#165805=CARTESIAN_POINT('Ctrl Pts',(8.12524570021172,0.0109302651159309,
34.5844975467655));
#165806=CARTESIAN_POINT('Ctrl Pts',(8.1251952209293,0.0337512308952398,
34.5853916272751));
#165807=CARTESIAN_POINT('Ctrl Pts',(8.12511435888944,0.0495295917114283,
34.5860090885223));
#165808=CARTESIAN_POINT('Ctrl Pts',(8.12469453002567,0.101760909957368,
34.5880509431436));
#165809=CARTESIAN_POINT('Ctrl Pts',(8.12415620062433,0.138211921603296,
34.5894724639253));
#165810=CARTESIAN_POINT('Ctrl Pts',(8.11865004461308,0.394303865798785,
34.5994403309321));
#165811=CARTESIAN_POINT('Ctrl Pts',(8.10502098785227,0.613670069212227,
34.6078825785361));
#165812=CARTESIAN_POINT('Ctrl Pts',(8.05651078099494,1.08480344278174,34.6260885981769));
#165813=CARTESIAN_POINT('Ctrl Pts',(8.01867720209948,1.33603107781036,34.6358452139881));
#165814=CARTESIAN_POINT('Ctrl Pts',(7.96013183450352,1.63037486290319,34.6474878045885));
#165815=CARTESIAN_POINT('Ctrl Pts',(7.95073512257806,1.67559899932941,34.6492823782081));
#165816=CARTESIAN_POINT('Ctrl Pts',(7.93358549751132,1.75474188970223,34.6524338953235));
#165817=CARTESIAN_POINT('Ctrl Pts',(7.92599936934352,1.78869559559917,34.6537895123514));
#165818=CARTESIAN_POINT('Ctrl Pts',(7.91063343276423,1.85545216549814,34.6564621699032));
#165819=CARTESIAN_POINT('Ctrl Pts',(7.90286707186119,1.88825741937345,34.657779077092));
#165820=CARTESIAN_POINT('Ctrl Pts',(7.8869890112249,1.95351238051163,34.6604059132159));
#165821=CARTESIAN_POINT('Ctrl Pts',(7.87888064952394,1.98596223174793,34.6617157906311));
#165822=CARTESIAN_POINT('Ctrl Pts',(7.85646476118541,2.07337269222533,34.6652542648441));
#165823=CARTESIAN_POINT('Ctrl Pts',(7.84178102714466,2.12823474854227,34.6674859057408));
#165824=CARTESIAN_POINT('Ctrl Pts',(7.77536165569618,2.36636919079482,34.6772211395378));
#165825=CARTESIAN_POINT('Ctrl Pts',(7.71776763344515,2.547942978051,34.684771890944));
#165826=CARTESIAN_POINT('Ctrl Pts',(7.58580755604703,2.91827028414676,34.7004316959874));
#165827=CARTESIAN_POINT('Ctrl Pts',(7.51064521760747,3.10660356839709,34.7085401809579));
#165828=CARTESIAN_POINT('Ctrl Pts',(7.38332260460776,3.3939180336083,34.7210816270863));
#165829=CARTESIAN_POINT('Ctrl Pts',(7.33603007462666,3.4949671364998,34.7255259358814));
#165830=CARTESIAN_POINT('Ctrl Pts',(7.2660361428698,3.63683675352567,34.7317991828828));
#165831=CARTESIAN_POINT('Ctrl Pts',(7.24504073060462,3.67848442223049,34.7336449231816));
#165832=CARTESIAN_POINT('Ctrl Pts',(7.21161330937314,3.7433963997994,34.7365268329542));
#165833=CARTESIAN_POINT('Ctrl Pts',(7.19942466904675,3.76678477904054,34.7375662649226));
#165834=CARTESIAN_POINT('Ctrl Pts',(7.17838778414793,3.80667663643544,34.7393406626569));
#165835=CARTESIAN_POINT('Ctrl Pts',(7.16959597268729,3.82320961842986,34.7400764988261));
#165836=CARTESIAN_POINT('Ctrl Pts',(7.15175952202237,3.85647313089009,34.741557745098));
#165837=CARTESIAN_POINT('Ctrl Pts',(7.14271314518782,3.87320257649082,34.7423031317843));
#165838=CARTESIAN_POINT('Ctrl Pts',(7.1229826065227,3.90938600675234,34.7439163723241));
#165839=CARTESIAN_POINT('Ctrl Pts',(7.11227729782873,3.92882829933022,34.744783884676));
#165840=CARTESIAN_POINT('Ctrl Pts',(7.08316312212893,3.98119462059008,34.7471226379167));
#165841=CARTESIAN_POINT('Ctrl Pts',(7.06460438922882,4.01403478607073,34.7485916595854));
#165842=CARTESIAN_POINT('Ctrl Pts',(6.96495715168983,4.18753134282294,34.7563682696062));
#165843=CARTESIAN_POINT('Ctrl Pts',(6.87989440218827,4.32586417139037,34.7626242877761));
#165844=CARTESIAN_POINT('Ctrl Pts',(6.60405022690194,4.74571475518898,34.7819250060177));
#165845=CARTESIAN_POINT('Ctrl Pts',(6.39970527204536,5.01787408418438,34.7949003377759));
#165846=CARTESIAN_POINT('Ctrl Pts',(6.06993991454218,5.40404266739938,34.814472740586));
#165847=CARTESIAN_POINT('Ctrl Pts',(5.95704000488348,5.52824758463407,34.8209647054593));
#165848=CARTESIAN_POINT('Ctrl Pts',(5.8338976671695,5.65556472922741,34.8278527360451));
#165849=CARTESIAN_POINT('Ctrl Pts',(5.82740768923605,5.66225167409398,34.8282152080505));
#165850=CARTESIAN_POINT('Ctrl Pts',(5.81727192675331,5.67265916714917,34.8287804510937));
#165851=CARTESIAN_POINT('Ctrl Pts',(5.81363404175725,5.6763874008854,34.8289831557022));
#165852=CARTESIAN_POINT('Ctrl Pts',(5.80802481337773,5.68212488889154,34.8292954433741));
#165853=CARTESIAN_POINT('Ctrl Pts',(5.80605600631053,5.68413662198172,34.8294050051147));
#165854=CARTESIAN_POINT('Ctrl Pts',(5.80304106807818,5.68721409434241,34.8295727072432));
#165855=CARTESIAN_POINT('Ctrl Pts',(5.80199568765323,5.68828056912998,34.8296308413213));
#165856=CARTESIAN_POINT('Ctrl Pts',(5.796363663638,5.69402307194969,34.8299439659951));
#165857=CARTESIAN_POINT('Ctrl Pts',(5.79177166233974,5.69869383949588,34.8301990015068));
#165858=CARTESIAN_POINT('Ctrl Pts',(5.78354494819218,5.70704145113668,34.8306554299977));
#165859=CARTESIAN_POINT('Ctrl Pts',(5.77991236381637,5.71072038882402,34.8308568049596));
#165860=CARTESIAN_POINT('Ctrl Pts',(5.77344282400862,5.71725998639819,34.8312151551819));
#165861=CARTESIAN_POINT('Ctrl Pts',(5.77060724731175,5.72012200843901,34.8313721187841));
#165862=CARTESIAN_POINT('Ctrl Pts',(5.76558130167161,5.72518728674974,34.8316501536577));
#165863=CARTESIAN_POINT('Ctrl Pts',(5.76339179533751,5.72739139818271,34.8317712176427));
#165864=CARTESIAN_POINT('Ctrl Pts',(5.75952578721011,5.73127873278362,34.8319848756536));
#165865=CARTESIAN_POINT('Ctrl Pts',(5.75784981021638,5.7329624775839,34.8320774652504));
#165866=CARTESIAN_POINT('Ctrl Pts',(5.75489941426114,5.73592394919647,34.8322403995011));
#165867=CARTESIAN_POINT('Ctrl Pts',(5.75362530754072,5.73720198700158,34.8323107415223));
#165868=CARTESIAN_POINT('Ctrl Pts',(5.75138758764029,5.73944511596621,34.8324342485982));
#165869=CARTESIAN_POINT('Ctrl Pts',(5.75042415702783,5.74041038922492,34.8324874121141));
#165870=CARTESIAN_POINT('Ctrl Pts',(5.74873510732527,5.74210181746458,34.8325805964454));
#165871=CARTESIAN_POINT('Ctrl Pts',(5.74800959353507,5.74282807760712,34.8326206163738));
#165872=CARTESIAN_POINT('Ctrl Pts',(5.74510652671018,5.74573302962187,34.8327807261616));
#165873=CARTESIAN_POINT('Ctrl Pts',(5.7429278727156,5.74791062036725,34.8329008252742));
#165874=CARTESIAN_POINT('Ctrl Pts',(5.70452897669493,5.78624715090123,34.8350165605289));
#165875=CARTESIAN_POINT('Ctrl Pts',(5.66796920996702,5.82206423440826,34.8370150224519));
#165876=CARTESIAN_POINT('Ctrl Pts',(5.59210909301375,5.89499150056361,34.8411297617647));
#165877=CARTESIAN_POINT('Ctrl Pts',(5.55277190915635,5.93205976030752,34.8432462605495));
#165878=CARTESIAN_POINT('Ctrl Pts',(5.46398479265107,6.01406869368731,34.8479856115783));
#165879=CARTESIAN_POINT('Ctrl Pts',(5.414344451711,6.05879742059624,34.850609800139));
#165880=CARTESIAN_POINT('Ctrl Pts',(5.25207208880888,6.20142688986855,34.8591065291));
#165881=CARTESIAN_POINT('Ctrl Pts',(5.13729352249396,6.29683822921074,34.8649923382592));
#165882=CARTESIAN_POINT('Ctrl Pts',(4.92210510023832,6.46591476967828,34.8757956607437));
#165883=CARTESIAN_POINT('Ctrl Pts',(4.82250374100534,6.54053745106074,34.8807100605435));
#165884=CARTESIAN_POINT('Ctrl Pts',(4.65930643014928,6.65705188715999,34.8886154910679));
#165885=CARTESIAN_POINT('Ctrl Pts',(4.5967669250635,6.70038880480338,34.8916113962469));
#165886=CARTESIAN_POINT('Ctrl Pts',(4.50236519510259,6.76386090929375,34.8960807802276));
#165887=CARTESIAN_POINT('Ctrl Pts',(4.4709566407817,6.78466310754317,34.8975591725953));
#165888=CARTESIAN_POINT('Ctrl Pts',(4.40468152525041,6.82789769957922,34.9006602946229));
#165889=CARTESIAN_POINT('Ctrl Pts',(4.36978567694507,6.85028316828618,34.9022826918794));
#165890=CARTESIAN_POINT('Ctrl Pts',(4.31827577954882,6.88277268586828,34.9046633429927));
#165891=CARTESIAN_POINT('Ctrl Pts',(4.30179440232076,6.89308570052938,34.9054229561689));
#165892=CARTESIAN_POINT('Ctrl Pts',(4.19818723961457,6.95740026974355,34.9101853649551));
#165893=CARTESIAN_POINT('Ctrl Pts',(4.11008291273003,7.00980835385641,34.9141788531029));
#165894=CARTESIAN_POINT('Ctrl Pts',(3.848984644853,7.15850513001163,34.9258795982784));
#165895=CARTESIAN_POINT('Ctrl Pts',(3.67343620960111,7.25015480069218,34.9335791681863));
#165896=CARTESIAN_POINT('Ctrl Pts',(3.44347555253292,7.35971366841279,34.943527121756));
#165897=CARTESIAN_POINT('Ctrl Pts',(3.39198032275537,7.38358846561801,34.9457459744189));
#165898=CARTESIAN_POINT('Ctrl Pts',(3.29157894963733,7.42886565662324,34.9500571029993));
#165899=CARTESIAN_POINT('Ctrl Pts',(3.24270366710774,7.45032951158792,34.952148942539));
#165900=CARTESIAN_POINT('Ctrl Pts',(3.13897147623036,7.49466996164132,34.9565758312534));
#165901=CARTESIAN_POINT('Ctrl Pts',(3.08406789967719,7.51742940899239,34.9589114295993));
#165902=CARTESIAN_POINT('Ctrl Pts',(2.9353718012212,7.57716593019159,34.965219145366));
#165903=CARTESIAN_POINT('Ctrl Pts',(2.84113297527614,7.6130029810279,34.9691979268653));
#165904=CARTESIAN_POINT('Ctrl Pts',(2.29066579744459,7.81068919112221,34.9923468109638));
#165905=CARTESIAN_POINT('Ctrl Pts',(1.82137143975115,7.93325972300021,35.011781675766));
#165906=CARTESIAN_POINT('Ctrl Pts',(1.24493358579442,8.02993857246595,35.0351051038665));
#165907=CARTESIAN_POINT('Ctrl Pts',(1.14559010426156,8.04471234011166,35.0391028100846));
#165908=CARTESIAN_POINT('Ctrl Pts',(1.00046783942304,8.06355130087438,35.0449030369057));
#165909=CARTESIAN_POINT('Ctrl Pts',(0.954888367142722,8.0690757658899,35.0467190574877));
#165910=CARTESIAN_POINT('Ctrl Pts',(0.882052499240776,8.07727805808648,
35.0496110110271));
#165911=CARTESIAN_POINT('Ctrl Pts',(0.85482524299561,8.08020490151107,35.0506898347288));
#165912=CARTESIAN_POINT('Ctrl Pts',(0.807510189156024,8.08504929017713,
35.0525604766157));
#165913=CARTESIAN_POINT('Ctrl Pts',(0.787429105458315,8.08702974752103,
35.0533531125639));
#165914=CARTESIAN_POINT('Ctrl Pts',(0.748503174202609,8.09072237879436,
35.0548869848895));
#165915=CARTESIAN_POINT('Ctrl Pts',(0.729659311744389,8.09244356817922,
35.0556283444389));
#165916=CARTESIAN_POINT('Ctrl Pts',(0.692475101540281,8.09570902030665,
35.0570888304099));
#165917=CARTESIAN_POINT('Ctrl Pts',(0.674135181562731,8.09725682370546,
35.0578079980902));
#165918=CARTESIAN_POINT('Ctrl Pts',(0.621677422069094,8.10150455462117,
35.059861640936));
#165919=CARTESIAN_POINT('Ctrl Pts',(0.587547533193598,8.10405125714766,
35.0611937413131));
#165920=CARTESIAN_POINT('Ctrl Pts',(0.342648571307864,8.12076989723983,
35.0707275147846));
#165921=CARTESIAN_POINT('Ctrl Pts',(0.131411071492284,8.12693331272511,
35.0788222704203));
#165922=CARTESIAN_POINT('Ctrl Pts',(-0.259227200681319,8.12309521647083,
35.0937759633845));
#165923=CARTESIAN_POINT('Ctrl Pts',(-0.438518066267162,8.11539132358751,
35.1006326683191));
#165924=CARTESIAN_POINT('Ctrl Pts',(-0.731067458314353,8.09309717001299,
35.1118981749349));
#165925=CARTESIAN_POINT('Ctrl Pts',(-0.844533070922323,8.08204460959697,
35.1162862962646));
#165926=CARTESIAN_POINT('Ctrl Pts',(-1.04139663533081,8.05867729114972,
35.1239494405474));
#165927=CARTESIAN_POINT('Ctrl Pts',(-1.12490531834648,8.04744521742355,
35.1272157068452));
#165928=CARTESIAN_POINT('Ctrl Pts',(-1.24261299023128,8.02974531823331,
35.1318456219096));
#165929=CARTESIAN_POINT('Ctrl Pts',(-1.27696854548493,8.02435344704153,
35.1332000978312));
#165930=CARTESIAN_POINT('Ctrl Pts',(-1.34431242333893,8.0133408403655,35.1358615916867));
#165931=CARTESIAN_POINT('Ctrl Pts',(-1.3773027463569,8.00773653732853,35.137168444919));
#165932=CARTESIAN_POINT('Ctrl Pts',(-1.44303308442542,7.99615224273553,
35.1397785260649));
#165933=CARTESIAN_POINT('Ctrl Pts',(-1.47577286123667,7.99017456786248,
35.1410817102892));
#165934=CARTESIAN_POINT('Ctrl Pts',(-1.56338967279644,7.97362048088784,
35.1445778271022));
#165935=CARTESIAN_POINT('Ctrl Pts',(-1.61819572774218,7.96267878216658,
35.1467737794527));
#165936=CARTESIAN_POINT('Ctrl Pts',(-1.86061339478575,7.9116753963471,35.1565281319363));
#165937=CARTESIAN_POINT('Ctrl Pts',(-2.04688286352506,7.86554251038108,
35.1641351280624));
#165938=CARTESIAN_POINT('Ctrl Pts',(-2.44366439053522,7.75222222016196,
35.1805634253704));
#165939=CARTESIAN_POINT('Ctrl Pts',(-2.65342534770506,7.68295378145173,
35.189388727527));
#165940=CARTESIAN_POINT('Ctrl Pts',(-2.91965137689471,7.58283395539435,
35.2006991382305));
#165941=CARTESIAN_POINT('Ctrl Pts',(-2.97893399856467,7.55974121557897,
35.2032245785618));
#165942=CARTESIAN_POINT('Ctrl Pts',(-3.08066115270987,7.51873235129915,
35.2075664676156));
#165943=CARTESIAN_POINT('Ctrl Pts',(-3.12323576093065,7.50114709367621,
35.2093861572494));
#165944=CARTESIAN_POINT('Ctrl Pts',(-3.18298432258327,7.47587133799463,
35.2119422126967));
#165945=CARTESIAN_POINT('Ctrl Pts',(-3.20028449363887,7.46848181509135,
35.2126825935082));
#165946=CARTESIAN_POINT('Ctrl Pts',(-3.23406452424598,7.45391422800095,
35.21412866372));
#165947=CARTESIAN_POINT('Ctrl Pts',(-3.25054653852426,7.44674142619944,
35.2148344268593));
#165948=CARTESIAN_POINT('Ctrl Pts',(-3.28529311071579,7.43148273953059,
35.2163225694715));
#165949=CARTESIAN_POINT('Ctrl Pts',(-3.30355185747248,7.42338411092282,
35.2171047081253));
#165950=CARTESIAN_POINT('Ctrl Pts',(-3.35364376234865,7.40094453927139,
35.2192509636639));
#165951=CARTESIAN_POINT('Ctrl Pts',(-3.38541466303249,7.38646560506674,
35.2206128242698));
#165952=CARTESIAN_POINT('Ctrl Pts',(-3.56283426038929,7.30422511698172,
35.2282236052211));
#165953=CARTESIAN_POINT('Ctrl Pts',(-3.70654347269636,7.23235986783352,
35.2344100843979));
#165954=CARTESIAN_POINT('Ctrl Pts',(-4.16341040741607,6.98669632923451,
35.2542758829501));
#165955=CARTESIAN_POINT('Ctrl Pts',(-4.4672382165251,6.7964474479209,35.2678054737171));
#165956=CARTESIAN_POINT('Ctrl Pts',(-4.96904173892923,6.43400275186682,
35.2913490098663));
#165957=CARTESIAN_POINT('Ctrl Pts',(-5.17307479709484,6.27112924474943,
35.3013049557861));
#165958=CARTESIAN_POINT('Ctrl Pts',(-5.45074493110372,6.0266867036711,35.3155509933524));
#165959=CARTESIAN_POINT('Ctrl Pts',(-5.53111559373208,5.95301041182328,
35.3197633498159));
#165960=CARTESIAN_POINT('Ctrl Pts',(-5.67071636512488,5.81976916067414,
35.3272484262055));
#165961=CARTESIAN_POINT('Ctrl Pts',(-5.73055130712703,5.76086094021573,
35.3305141097278));
#165962=CARTESIAN_POINT('Ctrl Pts',(-5.81546198121001,5.67463325786226,
35.3352347097355));
#165963=CARTESIAN_POINT('Ctrl Pts',(-5.84128073350422,5.64805276606012,
35.3366819435522));
#165964=CARTESIAN_POINT('Ctrl Pts',(-5.8931978231614,5.59386718218471,35.339616446664));
#165965=CARTESIAN_POINT('Ctrl Pts',(-5.91928620629358,5.56625380592011,
35.3411037708838));
#165966=CARTESIAN_POINT('Ctrl Pts',(-5.96965688710703,5.5121841115854,35.3440005876965));
#165967=CARTESIAN_POINT('Ctrl Pts',(-5.99395934970122,5.48574774620612,
35.345409854201));
#165968=CARTESIAN_POINT('Ctrl Pts',(-6.05902495780542,5.41402040377905,
35.3492146848566));
#165969=CARTESIAN_POINT('Ctrl Pts',(-6.09945511412735,5.36843064978203,
35.3516130813039));
#165970=CARTESIAN_POINT('Ctrl Pts',(-6.25689812573659,5.18682040243138,
35.3610902014444));
#165971=CARTESIAN_POINT('Ctrl Pts',(-6.36990444139595,5.04739501328758,
35.3681977333362));
#165972=CARTESIAN_POINT('Ctrl Pts',(-6.90784827420129,4.336819335229,35.4036217736309));
#165973=CARTESIAN_POINT('Ctrl Pts',(-7.26103288330256,3.71532824108283,
35.432735717903));
#165974=CARTESIAN_POINT('Ctrl Pts',(-7.67635558963884,2.69209288273319,
35.4794316237433));
#165975=CARTESIAN_POINT('Ctrl Pts',(-7.79744362954527,2.318119578179,35.4961603448697));
#165976=CARTESIAN_POINT('Ctrl Pts',(-7.9194696069256,1.82096898233787,35.5171791218376));
#165977=CARTESIAN_POINT('Ctrl Pts',(-7.94535898206296,1.70446442989422,
35.5220164216116));
#165978=CARTESIAN_POINT('Ctrl Pts',(-7.97281025926088,1.56666285180608,
35.5276040582959));
#165979=CARTESIAN_POINT('Ctrl Pts',(-7.97686594816583,1.54588019473454,
35.5284431881772));
#165980=CARTESIAN_POINT('Ctrl Pts',(-7.98268411838763,1.51543337700562,
35.5296670655407));
#165981=CARTESIAN_POINT('Ctrl Pts',(-7.98451037152187,1.50578158515982,
35.530054239054));
#165982=CARTESIAN_POINT('Ctrl Pts',(-7.98766180079866,1.48895926415792,
35.5307276284014));
#165983=CARTESIAN_POINT('Ctrl Pts',(-7.98899483361551,1.48179022914358,
35.5310141512046));
#165984=CARTESIAN_POINT('Ctrl Pts',(-7.99154781872775,1.46795671825823,
35.531566150358));
#165985=CARTESIAN_POINT('Ctrl Pts',(-7.99276908912684,1.46129249430836,
35.531831679063));
#165986=CARTESIAN_POINT('Ctrl Pts',(-7.99563939702669,1.4455185578327,35.5324592293984));
#165987=CARTESIAN_POINT('Ctrl Pts',(-7.99728120582328,1.43640752721332,
35.5328209573329));
#165988=CARTESIAN_POINT('Ctrl Pts',(-8.00211839470062,1.40929872228121,
35.5338949797603));
#165989=CARTESIAN_POINT('Ctrl Pts',(-8.00526862993003,1.39129287406691,
35.5346053958517));
#165990=CARTESIAN_POINT('Ctrl Pts',(-8.04467637079795,1.16148386495849,
35.5436334077829));
#165991=CARTESIAN_POINT('Ctrl Pts',(-8.07257791224346,0.948339309571144,
35.5515446086187));
#165992=CARTESIAN_POINT('Ctrl Pts',(-8.10178077860499,0.62653955769214,
35.5630344761891));
#165993=CARTESIAN_POINT('Ctrl Pts',(-8.10940843079419,0.518555089387819,
35.5668155815941));
#165994=CARTESIAN_POINT('Ctrl Pts',(-8.1471196490731,-0.227023988679579,
35.5925653863522));
#165995=CARTESIAN_POINT('Ctrl Pts',(-8.10413803092976,-0.866079136845537,
35.6129862188969));
#165996=CARTESIAN_POINT('Ctrl Pts',(-7.91392581108344,-1.88326007959288,
35.6489069896832));
#165997=CARTESIAN_POINT('Ctrl Pts',(-7.81262480900694,-2.26710020180854,
35.6632585365121));
#165998=CARTESIAN_POINT('Ctrl Pts',(-7.67434427473708,-2.66926186990742,
35.6796358574786));
#165999=CARTESIAN_POINT('Ctrl Pts',(-7.66482354556395,-2.69647899535085,
35.6807508148663));
#166000=CARTESIAN_POINT('Ctrl Pts',(-7.65079400609647,-2.7359108434309,
35.6823758535913));
#166001=CARTESIAN_POINT('Ctrl Pts',(-7.64640034701529,-2.74816644295808,
35.6828822881947));
#166002=CARTESIAN_POINT('Ctrl Pts',(-7.63866887894711,-2.76957039139912,
35.6837691576179));
#166003=CARTESIAN_POINT('Ctrl Pts',(-7.6353440387107,-2.77872341279585,
35.684149180601));
#166004=CARTESIAN_POINT('Ctrl Pts',(-7.6288791277273,-2.79642158778652,
35.6848854824854));
#166005=CARTESIAN_POINT('Ctrl Pts',(-7.62574113347528,-2.8049674876381,
35.6852416950567));
#166006=CARTESIAN_POINT('Ctrl Pts',(-7.61825147280863,-2.8252590957727,
35.6860891056933));
#166007=CARTESIAN_POINT('Ctrl Pts',(-7.61388700095014,-2.83700003458964,
35.6865807102438));
#166008=CARTESIAN_POINT('Ctrl Pts',(-7.59836983315337,-2.87844930631459,
35.6883207894881));
#166009=CARTESIAN_POINT('Ctrl Pts',(-7.58707033537717,-2.90810216953385,
35.6895739317359));
#166010=CARTESIAN_POINT('Ctrl Pts',(-7.41613012697682,-3.34891626200274,
35.7083277013317));
#166011=CARTESIAN_POINT('Ctrl Pts',(-7.22346226096286,-3.74643122317459,
35.726915754654));
#166012=CARTESIAN_POINT('Ctrl Pts',(-6.73867952448173,-4.56877307563761,
35.7687588665495));
#166013=CARTESIAN_POINT('Ctrl Pts',(-6.43648092504908,-4.98549581195371,
35.7921975420767));
#166014=CARTESIAN_POINT('Ctrl Pts',(-5.98219779545448,-5.50119615750303,
35.8226319921396));
#166015=CARTESIAN_POINT('Ctrl Pts',(-5.86324575088658,-5.62780623019203,
35.8302275616457));
#166016=CARTESIAN_POINT('Ctrl Pts',(-5.63344940755418,-5.85719550351363,
35.8440914417724));
#166017=CARTESIAN_POINT('Ctrl Pts',(-5.52361418973488,-5.96088786656312,
35.850400467349));
#166018=CARTESIAN_POINT('Ctrl Pts',(-5.37596919377233,-6.09268749216142,
35.8584105855136));
#166019=CARTESIAN_POINT('Ctrl Pts',(-5.34072363013724,-6.12360652624086,
35.8602896121216));
#166020=CARTESIAN_POINT('Ctrl Pts',(-5.29495134522953,-6.1630642807339,
35.862690076382));
#166021=CARTESIAN_POINT('Ctrl Pts',(-5.2846686365472,-6.17188370610218,
35.8632267822232));
#166022=CARTESIAN_POINT('Ctrl Pts',(-5.26804176133746,-6.18607247283605,
35.8640905835701));
#166023=CARTESIAN_POINT('Ctrl Pts',(-5.26171135487337,-6.19145784585777,
35.8644185215657));
#166024=CARTESIAN_POINT('Ctrl Pts',(-5.24962331142428,-6.20170939985228,
35.8650429569472));
#166025=CARTESIAN_POINT('Ctrl Pts',(-5.24386714617091,-6.20657729717903,
35.8653395425626));
#166026=CARTESIAN_POINT('Ctrl Pts',(-5.23070627584658,-6.21767585747659,
35.866015934899));
#166027=CARTESIAN_POINT('Ctrl Pts',(-5.22329718981457,-6.22390132318167,
35.8663954794687));
#166028=CARTESIAN_POINT('Ctrl Pts',(-5.20399979876033,-6.24005717923453,
35.8673808519901));
#166029=CARTESIAN_POINT('Ctrl Pts',(-5.19209415770805,-6.24996686127758,
35.8679856620792));
#166030=CARTESIAN_POINT('Ctrl Pts',(-5.11655979007391,-6.31247324647411,
35.8718035711892));
#166031=CARTESIAN_POINT('Ctrl Pts',(-5.05215970817499,-6.36413272795087,
35.8749725129444));
#166032=CARTESIAN_POINT('Ctrl Pts',(-4.88750382144314,-6.49213915936372,
35.8828862778145));
#166033=CARTESIAN_POINT('Ctrl Pts',(-4.78623752821311,-6.56715281767075,
35.8875818171872));
#166034=CARTESIAN_POINT('Ctrl Pts',(-4.47754523141419,-6.78488405822624,
35.9014952066341));
#166035=CARTESIAN_POINT('Ctrl Pts',(-4.26518816792894,-6.92034954297207,
35.9105465344359));
#166036=CARTESIAN_POINT('Ctrl Pts',(-3.65242796048224,-7.27230239167732,
35.9359197842129));
#166037=CARTESIAN_POINT('Ctrl Pts',(-3.23965726544051,-7.46533464582141,
35.9522163590045));
#166038=CARTESIAN_POINT('Ctrl Pts',(-2.58638533019122,-7.70639983955096,
35.9781460471032));
#166039=CARTESIAN_POINT('Ctrl Pts',(-2.35625562275052,-7.77984840295317,
35.987292088998));
#166040=CARTESIAN_POINT('Ctrl Pts',(-2.07876945527919,-7.85496811652075,
35.9983777145646));
#166041=CARTESIAN_POINT('Ctrl Pts',(-2.03423507736334,-7.86661897962906,
36.0001584172041));
#166042=CARTESIAN_POINT('Ctrl Pts',(-1.96474679361952,-7.88416862499366,
36.0029392848707));
#166043=CARTESIAN_POINT('Ctrl Pts',(-1.93985977139226,-7.89032882275543,
36.0039357171235));
#166044=CARTESIAN_POINT('Ctrl Pts',(-1.89380678936169,-7.90149710292535,
36.0057804455528));
#166045=CARTESIAN_POINT('Ctrl Pts',(-1.87264902883714,-7.90653819529095,
36.006628275466));
#166046=CARTESIAN_POINT('Ctrl Pts',(-1.82752784230803,-7.91709758922762,
36.0084370928113));
#166047=CARTESIAN_POINT('Ctrl Pts',(-1.80355907149269,-7.92259218448324,
36.0093984051002));
#166048=CARTESIAN_POINT('Ctrl Pts',(-1.73937356810138,-7.93699968252074,
36.0119741616048));
#166049=CARTESIAN_POINT('Ctrl Pts',(-1.69911350196255,-7.94571567881999,
36.0135913438358));
#166050=CARTESIAN_POINT('Ctrl Pts',(-1.51783624683178,-7.98352005384629,
36.0208818460534));
#166051=CARTESIAN_POINT('Ctrl Pts',(-1.37612954105435,-8.00916259505948,
36.026605645455));
#166052=CARTESIAN_POINT('Ctrl Pts',(-1.06649678523281,-8.05673193915344,
36.0391945575339));
#166053=CARTESIAN_POINT('Ctrl Pts',(-0.898416280861058,-8.07720191991345,
36.0460807236975));
#166054=CARTESIAN_POINT('Ctrl Pts',(-0.191505968885995,-8.140955380252,
36.0752914460687));
#166055=CARTESIAN_POINT('Ctrl Pts',(0.350298812512999,-8.13566648358123,
36.0984028383942));
#166056=CARTESIAN_POINT('Ctrl Pts',(1.10364705433365,-8.05288308602651,
36.1303954368781));
#166057=CARTESIAN_POINT('Ctrl Pts',(1.31874068321201,-8.02046699754834,
36.1394950996924));
#166058=CARTESIAN_POINT('Ctrl Pts',(1.62541922591264,-7.96157615004829,
36.1522445953865));
#166059=CARTESIAN_POINT('Ctrl Pts',(1.71824071320448,-7.94206094609121,
36.1560730096295));
#166060=CARTESIAN_POINT('Ctrl Pts',(1.8272195016843,-7.91714870215879,36.1605176585653));
#166061=CARTESIAN_POINT('Ctrl Pts',(1.84372614491277,-7.91332095817349,
36.1611895076565));
#166062=CARTESIAN_POINT('Ctrl Pts',(1.86903940233612,-7.90736753572726,
36.1622175919455));
#166063=CARTESIAN_POINT('Ctrl Pts',(1.87785458652531,-7.90527872913061,
36.1625752040756));
#166064=CARTESIAN_POINT('Ctrl Pts',(1.89323778996243,-7.9016064112902,36.1631985272878));
#166065=CARTESIAN_POINT('Ctrl Pts',(1.89980735279523,-7.90002944493805,
36.1634644887706));
#166066=CARTESIAN_POINT('Ctrl Pts',(1.91355705725721,-7.89671080505675,
36.1640206276264));
#166067=CARTESIAN_POINT('Ctrl Pts',(1.92073680764272,-7.89496752787937,
36.1643107421241));
#166068=CARTESIAN_POINT('Ctrl Pts',(1.94064265913624,-7.89010553234284,
36.1651142704634));
#166069=CARTESIAN_POINT('Ctrl Pts',(1.95336364227486,-7.88696581237407,
36.1656268480819));
#166070=CARTESIAN_POINT('Ctrl Pts',(2.00360632379976,-7.87443618957103,
36.1676475340369));
#166071=CARTESIAN_POINT('Ctrl Pts',(2.04106876044858,-7.86480908787035,
36.1691458661266));
#166072=CARTESIAN_POINT('Ctrl Pts',(2.08149656914881,-7.85411162717253,
36.1707527829844));
#166073=CARTESIAN_POINT('Ctrl Pts',(2.08453123079472,-7.85330675367765,
36.1708733429704));
#166074=CARTESIAN_POINT('Ctrl Pts',(2.87584152954999,-7.64293910041931,
36.2022941622812));
#166075=CARTESIAN_POINT('Ctrl Pts',(3.62812932137937,-7.31586438032348,
36.2279383522161));
#166076=CARTESIAN_POINT('Ctrl Pts',(4.60642238122568,-6.70191151903222,
36.26757646638));
#166077=CARTESIAN_POINT('Ctrl Pts',(4.88214351938511,-6.50379882585563,
36.279539521296));
#166078=CARTESIAN_POINT('Ctrl Pts',(5.25764080508549,-6.19662851666698,
36.2975259157453));
#166079=CARTESIAN_POINT('Ctrl Pts',(5.36810105644125,-6.10118680156614,
36.3030447017041));
#166080=CARTESIAN_POINT('Ctrl Pts',(5.4927775842711,-5.98745372789434,36.3095616672778));
#166081=CARTESIAN_POINT('Ctrl Pts',(5.50956240914706,-5.97201220558443,
36.310445240007));
#166082=CARTESIAN_POINT('Ctrl Pts',(5.53495512813061,-5.94845351895876,
36.3117914821505));
#166083=CARTESIAN_POINT('Ctrl Pts',(5.54361073082386,-5.94038783256665,
36.312252071842));
#166084=CARTESIAN_POINT('Ctrl Pts',(5.55858098871185,-5.92637664832765,
36.313051639171));
#166085=CARTESIAN_POINT('Ctrl Pts',(5.56490380768753,-5.92043988201485,
36.3133902620669));
#166086=CARTESIAN_POINT('Ctrl Pts',(5.57898374680872,-5.90717713956545,
36.3141463794268));
#166087=CARTESIAN_POINT('Ctrl Pts',(5.58673596026024,-5.89984599075726,
36.3145640845531));
#166088=CARTESIAN_POINT('Ctrl Pts',(5.60715767521192,-5.88045714822414,
36.3156681539073));
#166089=CARTESIAN_POINT('Ctrl Pts',(5.61980269233511,-5.86837380893584,
36.3163555676741));
#166090=CARTESIAN_POINT('Ctrl Pts',(5.67204451425932,-5.81812880651341,
36.3192113352447));
#166091=CARTESIAN_POINT('Ctrl Pts',(5.71129195134477,-5.77960689692655,
36.3213945349094));
#166092=CARTESIAN_POINT('Ctrl Pts',(6.48430616026728,-5.0053195401276,36.3651606142523));
#166093=CARTESIAN_POINT('Ctrl Pts',(7.07052454473827,-4.13596002392158,
36.4137675947646));
#166094=CARTESIAN_POINT('Ctrl Pts',(7.57766521280065,-2.94359778476221,
36.4704911374173));
#166095=CARTESIAN_POINT('Ctrl Pts',(7.66700988559747,-2.70236214952331,
36.4814399135141));
#166096=CARTESIAN_POINT('Ctrl Pts',(7.75725705945687,-2.41792368580554,
36.4934676328857));
#166097=CARTESIAN_POINT('Ctrl Pts',(7.76944281194368,-2.37847651303313,
36.495116693381));
#166098=CARTESIAN_POINT('Ctrl Pts',(7.78494528881399,-2.32690188028682,
36.4972500385471));
#166099=CARTESIAN_POINT('Ctrl Pts',(7.7885351250395,-2.31485768867119,36.4977466286107));
#166100=CARTESIAN_POINT('Ctrl Pts',(7.79432461538074,-2.2952675509555,36.4985518002413));
#166101=CARTESIAN_POINT('Ctrl Pts',(7.79654128142491,-2.28772668560349,
36.4988611248705));
#166102=CARTESIAN_POINT('Ctrl Pts',(7.80077593196587,-2.27324321034897,
36.4994540805397));
#166103=CARTESIAN_POINT('Ctrl Pts',(7.80279559807271,-2.26630110296022,
36.4997377834086));
#166104=CARTESIAN_POINT('Ctrl Pts',(7.8073833280754,-2.25045307459042,36.5003843038641));
#166105=CARTESIAN_POINT('Ctrl Pts',(7.80994542686963,-2.24154542730656,
36.5007468704185));
#166106=CARTESIAN_POINT('Ctrl Pts',(7.81789537591416,-2.21372674655005,
36.5018766615201));
#166107=CARTESIAN_POINT('Ctrl Pts',(7.82322984629559,-2.19480044595643,
36.5026416946868));
#166108=CARTESIAN_POINT('Ctrl Pts',(7.86655399876549,-2.03892472935387,
36.5089140739986));
#166109=CARTESIAN_POINT('Ctrl Pts',(7.90101451164937,-1.90101500980129,
36.5142839923224));
#166110=CARTESIAN_POINT('Ctrl Pts',(8.06032380919927,-1.18397564052055,
36.5415801273203));
#166111=CARTESIAN_POINT('Ctrl Pts',(8.12518544520021,-0.593344303531527,
36.5621749605033));
#166112=CARTESIAN_POINT('Ctrl Pts',(8.12531225746491,0.571359736454304,
36.6045462755366));
#166113=CARTESIAN_POINT('Ctrl Pts',(8.06492182062517,1.14198041596768,36.6261305132673));
#166114=CARTESIAN_POINT('Ctrl Pts',(7.92025865124707,1.8174889000819,36.6528063994685));
#166115=CARTESIAN_POINT('Ctrl Pts',(7.89287697407166,1.93293965918776,36.6574045826282));
#166116=CARTESIAN_POINT('Ctrl Pts',(7.85110161518185,2.09334933695066,36.6638589267518));
#166117=CARTESIAN_POINT('Ctrl Pts',(7.83882943854375,2.1388457231402,36.6656969709959));
#166118=CARTESIAN_POINT('Ctrl Pts',(7.81580821771251,2.22133135432998,36.6690436398938));
#166119=CARTESIAN_POINT('Ctrl Pts',(7.80519056784129,2.25835587710605,36.6705510834822));
#166120=CARTESIAN_POINT('Ctrl Pts',(7.78322840666032,2.33293420659731,36.6735985615533));
#166121=CARTESIAN_POINT('Ctrl Pts',(7.77187437421485,2.37048415710379,36.6751386431613));
#166122=CARTESIAN_POINT('Ctrl Pts',(7.74317078963537,2.46298895615645,36.6789472006798));
#166123=CARTESIAN_POINT('Ctrl Pts',(7.72550770376431,2.51784414665875,36.6812184158831));
#166124=CARTESIAN_POINT('Ctrl Pts',(7.65531858192967,2.72813165306475,36.6899763545899));
#166125=CARTESIAN_POINT('Ctrl Pts',(7.59867342392271,2.88214608070219,36.6964994918006));
#166126=CARTESIAN_POINT('Ctrl Pts',(7.38594796939817,3.41056373907316,36.7192880564137));
#166127=CARTESIAN_POINT('Ctrl Pts',(7.20653660629888,3.77491625561562,36.7357458514446));
#166128=CARTESIAN_POINT('Ctrl Pts',(6.92217154077558,4.25759907073516,36.7585140857127));
#166129=CARTESIAN_POINT('Ctrl Pts',(6.83987535277774,4.38858908808458,36.7647962019272));
#166130=CARTESIAN_POINT('Ctrl Pts',(6.74099578967446,4.53643045926457,36.7719920884833));
#166131=CARTESIAN_POINT('Ctrl Pts',(6.72801852177775,4.55565498267227,36.7729298999151));
#166132=CARTESIAN_POINT('Ctrl Pts',(6.6069725036783,4.73332719802691,36.7816160983808));
#166133=CARTESIAN_POINT('Ctrl Pts',(6.49340597611092,4.88796000930419,36.7893171041997));
#166134=CARTESIAN_POINT('Ctrl Pts',(6.35117826922837,5.06790226201678,36.7984093801731));
#166135=CARTESIAN_POINT('Ctrl Pts',(6.32767973886511,5.09721177620872,36.7998946432409));
#166136=CARTESIAN_POINT('Ctrl Pts',(6.29108704159569,5.1422105084732,36.8021811512811));
#166137=CARTESIAN_POINT('Ctrl Pts',(6.27813561271742,5.15801495856683,36.8029853984066));
#166138=CARTESIAN_POINT('Ctrl Pts',(6.25310310061931,5.1883278239817,36.8045302105095));
#166139=CARTESIAN_POINT('Ctrl Pts',(6.24103084355399,5.20284326200802,36.8052709832846));
#166140=CARTESIAN_POINT('Ctrl Pts',(6.21227881432031,5.23717005555784,36.8070254988119));
#166141=CARTESIAN_POINT('Ctrl Pts',(6.19555467901422,5.25694402522529,36.8080383379982));
#166142=CARTESIAN_POINT('Ctrl Pts',(6.13772406271013,5.32466141307292,36.8115151893253));
#166143=CARTESIAN_POINT('Ctrl Pts',(6.09615315390873,5.37220556601296,36.8139707233928));
#166144=CARTESIAN_POINT('Ctrl Pts',(6.01819376327414,5.45929653478943,36.8185023654904));
#166145=CARTESIAN_POINT('Ctrl Pts',(5.98195914882804,5.4989762325039,36.8205803174095));
#166146=CARTESIAN_POINT('Ctrl Pts',(5.769923233633,5.72659583849324,36.8325897514008));
#166147=CARTESIAN_POINT('Ctrl Pts',(5.58566569856093,5.90645864221255,36.8424434608015));
#166148=CARTESIAN_POINT('Ctrl Pts',(5.36427886832688,6.10292497201267,36.8538484782136));
#166149=CARTESIAN_POINT('Ctrl Pts',(5.33519184989719,6.12836918832851,36.8553386316102));
#166150=CARTESIAN_POINT('Ctrl Pts',(5.21695299834538,6.23032022758931,36.8613645598991));
#166151=CARTESIAN_POINT('Ctrl Pts',(5.12632875123194,6.30509650775852,36.8659116862093));
#166152=CARTESIAN_POINT('Ctrl Pts',(4.99956641569756,6.40515109198602,36.8721891698899));
#166153=CARTESIAN_POINT('Ctrl Pts',(4.96479633468429,6.43213978337149,36.8739026862686));
#166154=CARTESIAN_POINT('Ctrl Pts',(4.90123654671812,6.48065273283447,36.8770206081783));
#166155=CARTESIAN_POINT('Ctrl Pts',(4.87251999146576,6.50227102270908,36.8784240460397));
#166156=CARTESIAN_POINT('Ctrl Pts',(4.81408304603306,6.54565879951769,36.8812697481869));
#166157=CARTESIAN_POINT('Ctrl Pts',(4.78435615145248,6.56741813031245,36.8827120756956));
#166158=CARTESIAN_POINT('Ctrl Pts',(4.70975343137167,6.62125007601148,36.8863189907494));
#166159=CARTESIAN_POINT('Ctrl Pts',(4.66469714847353,6.65306924869126,36.8884860001418));
#166160=CARTESIAN_POINT('Ctrl Pts',(4.46890306496718,6.78837413212094,36.8978555449286));
#166161=CARTESIAN_POINT('Ctrl Pts',(4.3150213719998,6.88721331881913,36.9051015130549));
#166162=CARTESIAN_POINT('Ctrl Pts',(3.93092016645313,7.11599432806845,36.9229013176412));
#166163=CARTESIAN_POINT('Ctrl Pts',(3.69744233740538,7.24005718718887,36.9334850347367));
#166164=CARTESIAN_POINT('Ctrl Pts',(3.35299403627075,7.40207204874327,36.9486439654369));
#166165=CARTESIAN_POINT('Ctrl Pts',(3.24659832048503,7.44935160758738,36.9532652616882));
#166166=CARTESIAN_POINT('Ctrl Pts',(3.1101921085545,7.50648941035271,36.959096746244));
#166167=CARTESIAN_POINT('Ctrl Pts',(3.08109088575267,7.51848104246908,36.9603355100902));
#166168=CARTESIAN_POINT('Ctrl Pts',(3.0351720827525,7.53709125463276,36.9622813049226));
#166169=CARTESIAN_POINT('Ctrl Pts',(3.01840092689088,7.54382330109867,36.9629901133941));
#166170=CARTESIAN_POINT('Ctrl Pts',(2.98243881361758,7.55811959349055,36.9645061446395));
#166171=CARTESIAN_POINT('Ctrl Pts',(2.96324120935344,7.5656668314918,36.9653131068324));
#166172=CARTESIAN_POINT('Ctrl Pts',(2.91570218016145,7.58414735609598,36.9673058684282));
#166173=CARTESIAN_POINT('Ctrl Pts',(2.88732774747386,7.59499498427004,36.9684904473159));
#166174=CARTESIAN_POINT('Ctrl Pts',(2.77830382789714,7.63597588208995,36.9730247383472));
#166175=CARTESIAN_POINT('Ctrl Pts',(2.6972376993684,7.66498589719664,36.9763602419914));
#166176=CARTESIAN_POINT('Ctrl Pts',(2.53946354156291,7.71863334916932,36.9827961774222));
#166177=CARTESIAN_POINT('Ctrl Pts',(2.46281999595053,7.74342906068706,36.9858975488375));
#166178=CARTESIAN_POINT('Ctrl Pts',(1.94896226853173,7.90127112892282,37.0065595550243));
#166179=CARTESIAN_POINT('Ctrl Pts',(1.50156382844315,7.99836511061295,37.0239653412887));
#166180=CARTESIAN_POINT('Ctrl Pts',(0.936820774476916,8.07184681462946,
37.0460353699289));
#166181=CARTESIAN_POINT('Ctrl Pts',(0.824970751193029,8.08404398672223,
37.0504084235212));
#166182=CARTESIAN_POINT('Ctrl Pts',(0.651625994246511,8.09931202436136,
37.0571951293637));
#166183=CARTESIAN_POINT('Ctrl Pts',(0.590288697053064,8.10401326008582,
37.0595983417141));
#166184=CARTESIAN_POINT('Ctrl Pts',(0.479455008772099,8.1112431892095,37.0639446893855));
#166185=CARTESIAN_POINT('Ctrl Pts',(0.429977542506816,8.11401642061859,
37.0658863299871));
#166186=CARTESIAN_POINT('Ctrl Pts',(0.307841494888655,8.11974191824522,
37.0706829402597));
#166187=CARTESIAN_POINT('Ctrl Pts',(0.235162830702437,8.12217172909592,
37.0735404148275));
#166188=CARTESIAN_POINT('Ctrl Pts',(0.074311987732583,8.12538852871123,
37.0798714590032));
#166189=CARTESIAN_POINT('Ctrl Pts',(-0.0138602377930529,8.12571651275672,
37.0833465282569));
#166190=CARTESIAN_POINT('Ctrl Pts',(-0.331099602795912,8.1217329617424,
37.0958631325346));
#166191=CARTESIAN_POINT('Ctrl Pts',(-0.559955207509258,8.10916911467058,
37.1049205555704));
#166192=CARTESIAN_POINT('Ctrl Pts',(-0.832912518291242,8.08257279461785,
37.1157060478797));
#166193=CARTESIAN_POINT('Ctrl Pts',(-0.877814268914422,8.07781953068325,
37.1174795902134));
#166194=CARTESIAN_POINT('Ctrl Pts',(-0.965958097893199,8.0677450684702,
37.1209588086008));
#166195=CARTESIAN_POINT('Ctrl Pts',(-1.00920163269568,8.06244985194533,
37.1226645815448));
#166196=CARTESIAN_POINT('Ctrl Pts',(-1.16631669276499,8.04192708463447,
37.1288610723782));
#166197=CARTESIAN_POINT('Ctrl Pts',(-1.27990480261986,8.02463268486345,
37.1333390870921));
#166198=CARTESIAN_POINT('Ctrl Pts',(-1.62786416739518,7.96407778132853,
37.1470954496238));
#166199=CARTESIAN_POINT('Ctrl Pts',(-1.86072828706355,7.91291137565185,
37.1563587235238));
#166200=CARTESIAN_POINT('Ctrl Pts',(-2.15069763973565,7.83568778525316,
37.1680892408126));
#166201=CARTESIAN_POINT('Ctrl Pts',(-2.2102062441972,7.81911067398425,37.17050694979));
#166202=CARTESIAN_POINT('Ctrl Pts',(-2.32248887998552,7.78644823374001,
37.1750906684271));
#166203=CARTESIAN_POINT('Ctrl Pts',(-2.37529945309148,7.77050083178002,
37.1772558155614));
#166204=CARTESIAN_POINT('Ctrl Pts',(-2.4996355222113,7.73156863143087,37.1823770365599));
#166205=CARTESIAN_POINT('Ctrl Pts',(-2.57101261945997,7.70812722304184,
37.1853355988369));
#166206=CARTESIAN_POINT('Ctrl Pts',(-2.84548604213709,7.61374903360236,
37.1967903236632));
#166207=CARTESIAN_POINT('Ctrl Pts',(-3.04605780890262,7.53574783376042,
37.2053292329106));
#166208=CARTESIAN_POINT('Ctrl Pts',(-3.43914479004118,7.36461792670848,
37.2224290542481));
#166209=CARTESIAN_POINT('Ctrl Pts',(-3.63155482000086,7.2716657698307,37.2309826625957));
#166210=CARTESIAN_POINT('Ctrl Pts',(-4.02498365326236,7.06208856917623,
37.2488248246091));
#166211=CARTESIAN_POINT('Ctrl Pts',(-4.22511930649394,6.94420312453342,
37.2581047900152));
#166212=CARTESIAN_POINT('Ctrl Pts',(-4.45765602806329,6.79345356826654,
37.2690639667071));
#166213=CARTESIAN_POINT('Ctrl Pts',(-4.49517561882424,6.76868560620335,
37.2708378177359));
#166214=CARTESIAN_POINT('Ctrl Pts',(-4.55415734680582,6.72904303092446,
37.2736343195132));
#166215=CARTESIAN_POINT('Ctrl Pts',(-4.57575656662218,6.71437421518159,
37.2746601115597));
#166216=CARTESIAN_POINT('Ctrl Pts',(-4.61371543992115,6.68832673317683,
37.2764656628244));
#166217=CARTESIAN_POINT('Ctrl Pts',(-4.63010462158914,6.6769915266387,37.2772461600805));
#166218=CARTESIAN_POINT('Ctrl Pts',(-4.66439429131561,6.6530888927767,37.2788809638243));
#166219=CARTESIAN_POINT('Ctrl Pts',(-4.68228600789291,6.64050929256558,
37.2797350014692));
#166220=CARTESIAN_POINT('Ctrl Pts',(-4.7353904189701,6.60285044641319,37.282273078244));
#166221=CARTESIAN_POINT('Ctrl Pts',(-4.77045403140547,6.577562223487,37.2839532452505));
#166222=CARTESIAN_POINT('Ctrl Pts',(-4.83100169349847,6.53315581991052,
37.2868641500685));
#166223=CARTESIAN_POINT('Ctrl Pts',(-4.85657814364462,6.51416541661162,
37.2880967879791));
#166224=CARTESIAN_POINT('Ctrl Pts',(-4.92771580974685,6.46069416844313,
37.2915349384889));
#166225=CARTESIAN_POINT('Ctrl Pts',(-4.97302607511141,6.42588234740215,
37.2937360834726));
#166226=CARTESIAN_POINT('Ctrl Pts',(-5.23730694547424,6.21836611197104,
37.3066559117297));
#166227=CARTESIAN_POINT('Ctrl Pts',(-5.44763640421366,6.03495815963397,
37.3172784499985));
#166228=CARTESIAN_POINT('Ctrl Pts',(-5.77344463889071,5.71991405206738,
37.3346744063742));
#166229=CARTESIAN_POINT('Ctrl Pts',(-5.89483619001525,5.59472833245317,
37.341391299524));
#166230=CARTESIAN_POINT('Ctrl Pts',(-6.04953844358453,5.42456161279612,
37.350315043653));
#166231=CARTESIAN_POINT('Ctrl Pts',(-6.08654678626711,5.38300401726181,
37.352478749762));
#166232=CARTESIAN_POINT('Ctrl Pts',(-6.14497671301229,5.31601860457312,
37.3559427166102));
#166233=CARTESIAN_POINT('Ctrl Pts',(-6.16667424127562,5.29083371509603,
37.3572398454762));
#166234=CARTESIAN_POINT('Ctrl Pts',(-6.21138111746079,5.23829265191314,
37.3599353522033));
#166235=CARTESIAN_POINT('Ctrl Pts',(-6.23436571971809,5.21091636425199,
37.3613339696851));
#166236=CARTESIAN_POINT('Ctrl Pts',(-6.28855855415036,5.14549706166993,
37.3646625506542));
#166237=CARTESIAN_POINT('Ctrl Pts',(-6.31960328727504,5.10732052683797,
37.3665942183325));
#166238=CARTESIAN_POINT('Ctrl Pts',(-6.43021904730197,4.96874053892814,
37.3735682163607));
#166239=CARTESIAN_POINT('Ctrl Pts',(-6.50775912934821,4.86674123106792,
37.3786308862793));
#166240=CARTESIAN_POINT('Ctrl Pts',(-6.65313256662602,4.66582125550979,
37.3884685363232));
#166241=CARTESIAN_POINT('Ctrl Pts',(-6.72125181436785,4.56714733262331,
37.3932398884131));
#166242=CARTESIAN_POINT('Ctrl Pts',(-6.92436992050757,4.25852975226594,
37.4079663257018));
#166243=CARTESIAN_POINT('Ctrl Pts',(-7.05189979707022,4.04384526566632,
37.4179427814488));
#166244=CARTESIAN_POINT('Ctrl Pts',(-7.18731112831798,3.78994771072142,
37.4293273762951));
#166245=CARTESIAN_POINT('Ctrl Pts',(-7.20503828235505,3.75613741401394,
37.4308350727097));
#166246=CARTESIAN_POINT('Ctrl Pts',(-7.23332315298065,3.7012537308262,37.4332682411994));
#166247=CARTESIAN_POINT('Ctrl Pts',(-7.24402857630317,3.68025719292538,
37.4341957381148));
#166248=CARTESIAN_POINT('Ctrl Pts',(-7.26299657439394,3.64265184023095,
37.4358507160412));
#166249=CARTESIAN_POINT('Ctrl Pts',(-7.27129390453646,3.6260607586376,37.4365787323128));
#166250=CARTESIAN_POINT('Ctrl Pts',(-7.2893011607907,3.58974365940494,37.4381675119752));
#166251=CARTESIAN_POINT('Ctrl Pts',(-7.29898795445569,3.57000641399389,
37.4390278538829));
#166252=CARTESIAN_POINT('Ctrl Pts',(-7.32861120175805,3.50902323739837,
37.4416768092871));
#166253=CARTESIAN_POINT('Ctrl Pts',(-7.34827908632698,3.4676477235463,37.4434610245958));
#166254=CARTESIAN_POINT('Ctrl Pts',(-7.3818123117158,3.39553695917885,37.4465497289992));
#166255=CARTESIAN_POINT('Ctrl Pts',(-7.39583816218207,3.36487773013587,
37.4478564563702));
#166256=CARTESIAN_POINT('Ctrl Pts',(-7.4538689188653,3.23591195432174,37.4533275106493));
#166257=CARTESIAN_POINT('Ctrl Pts',(-7.49610802228035,3.13682210138511,
37.4574690966713));
#166258=CARTESIAN_POINT('Ctrl Pts',(-7.69790516422688,2.63604621061694,
37.4781500982383));
#166259=CARTESIAN_POINT('Ctrl Pts',(-7.82720384377732,2.22291883598962,
37.4944365599125));
#166260=CARTESIAN_POINT('Ctrl Pts',(-7.94457133691743,1.70672625379305,
37.5146186533732));
#166261=CARTESIAN_POINT('Ctrl Pts',(-7.96441236199904,1.611602877583,37.5183299258014));
#166262=CARTESIAN_POINT('Ctrl Pts',(-8.02642445376506,1.28510802657773,
37.5310584673055));
#166263=CARTESIAN_POINT('Ctrl Pts',(-8.06025468096189,1.05227573223682,
37.5401209007361));
#166264=CARTESIAN_POINT('Ctrl Pts',(-8.09071468911015,0.751365732986816,
37.5518786850018));
#166265=CARTESIAN_POINT('Ctrl Pts',(-8.09665915119347,0.684342876344953,
37.5545002457673));
#166266=CARTESIAN_POINT('Ctrl Pts',(-8.10490386671329,0.576126850744388,
37.5587385843922));
#166267=CARTESIAN_POINT('Ctrl Pts',(-8.10772404064693,0.534976357811187,
37.5603515488994));
#166268=CARTESIAN_POINT('Ctrl Pts',(-8.11253189252067,0.456012620539981,
37.5634493811644));
#166269=CARTESIAN_POINT('Ctrl Pts',(-8.11456881803018,0.418203424295577,
37.564933867445));
#166270=CARTESIAN_POINT('Ctrl Pts',(-8.11867798966098,0.330524489802689,
37.5683793165677));
#166271=CARTESIAN_POINT('Ctrl Pts',(-8.12055514569915,0.280647181741935,
37.5703415168093));
#166272=CARTESIAN_POINT('Ctrl Pts',(-8.12517923581325,0.117891912762824,
37.5767520528683));
#166273=CARTESIAN_POINT('Ctrl Pts',(-8.1260329277843,0.00497391683127357,
37.58121172188));
#166274=CARTESIAN_POINT('Ctrl Pts',(-8.11665230415639,-0.701196864132818,
37.6091807082722));
#166275=CARTESIAN_POINT('Ctrl Pts',(-8.04381465928052,-1.29179221580849,
37.6329213363231));
#166276=CARTESIAN_POINT('Ctrl Pts',(-7.81238451289496,-2.27083316461565,
37.6748536593953));
#166277=CARTESIAN_POINT('Ctrl Pts',(-7.6869719600454,-2.66467296174595,
37.6924274748187));
#166278=CARTESIAN_POINT('Ctrl Pts',(-7.41659325181163,-3.33299204629362,
37.7228173492243));
#166279=CARTESIAN_POINT('Ctrl Pts',(-7.28482673799094,-3.61192553044677,
37.7356724099883));
#166280=CARTESIAN_POINT('Ctrl Pts',(-7.12694563527753,-3.90215629721046,
37.7488173307995));
#166281=CARTESIAN_POINT('Ctrl Pts',(-7.11628512855021,-3.92156395290631,
37.7496951091407));
#166282=CARTESIAN_POINT('Ctrl Pts',(-7.10117773045857,-3.9488027923744,
37.7509251099551));
#166283=CARTESIAN_POINT('Ctrl Pts',(-7.09679700226935,-3.95667043889293,
37.7512801503172));
#166284=CARTESIAN_POINT('Ctrl Pts',(-7.08912805737579,-3.97038990581443,
37.7518988366926));
#166285=CARTESIAN_POINT('Ctrl Pts',(-7.08584565599744,-3.97624495696774,
37.752162737189));
#166286=CARTESIAN_POINT('Ctrl Pts',(-7.07895676186823,-3.98849754432416,
37.752714693498));
#166287=CARTESIAN_POINT('Ctrl Pts',(-7.07534884220114,-3.99489427382888,
37.7530026851226));
#166288=CARTESIAN_POINT('Ctrl Pts',(-7.06674921007585,-4.01009296096322,
37.7536865373082));
#166289=CARTESIAN_POINT('Ctrl Pts',(-7.06174971083145,-4.01889051560899,
37.7540820415204));
#166290=CARTESIAN_POINT('Ctrl Pts',(-7.04496872040151,-4.04829181342596,
37.7554026316139));
#166291=CARTESIAN_POINT('Ctrl Pts',(-7.03311331796509,-4.06885339510998,
37.7563242358379));
#166292=CARTESIAN_POINT('Ctrl Pts',(-6.85147081991003,-4.38072165329726,
37.7702695720496));
#166293=CARTESIAN_POINT('Ctrl Pts',(-6.66380210607934,-4.66123576650295,
37.7822764784878));
#166294=CARTESIAN_POINT('Ctrl Pts',(-6.36942033038937,-5.04698887739755,
37.7989411004005));
#166295=CARTESIAN_POINT('Ctrl Pts',(-6.27639023583888,-5.16222228308908,
37.8039421614306));
#166296=CARTESIAN_POINT('Ctrl Pts',(-5.69224879535813,-5.84662977798414,
37.8341213880324));
#166297=CARTESIAN_POINT('Ctrl Pts',(-5.12729278828457,-6.34788275721227,
37.8586461976948));
#166298=CARTESIAN_POINT('Ctrl Pts',(-4.397775925233,-6.83335756294451,37.8912973635573));
#166299=CARTESIAN_POINT('Ctrl Pts',(-4.29248813739423,-6.89998207903976,
37.896020176308));
#166300=CARTESIAN_POINT('Ctrl Pts',(-4.16758827443107,-6.97505144784735,
37.9016452888115));
#166301=CARTESIAN_POINT('Ctrl Pts',(-4.1494214556568,-6.98587405416044,
37.9024640060834));
#166302=CARTESIAN_POINT('Ctrl Pts',(-4.12031503642813,-7.00306016864682,
37.9037766448004));
#166303=CARTESIAN_POINT('Ctrl Pts',(-4.1094024076463,-7.00946927915374,
37.9042689850591));
#166304=CARTESIAN_POINT('Ctrl Pts',(-4.09008618469824,-7.02075330351876,
37.905140836942));
#166305=CARTESIAN_POINT('Ctrl Pts',(-4.08168872559977,-7.02563869649252,
37.9055199857134));
#166306=CARTESIAN_POINT('Ctrl Pts',(-4.06446027107756,-7.03562038671822,
37.9062981155256));
#166307=CARTESIAN_POINT('Ctrl Pts',(-4.05562840624721,-7.04071514483439,
37.9066971485883));
#166308=CARTESIAN_POINT('Ctrl Pts',(-4.03312209054852,-7.05364176109653,
37.9077143674218));
#166309=CARTESIAN_POINT('Ctrl Pts',(-4.01943443013445,-7.06145047066264,
37.9083333461994));
#166310=CARTESIAN_POINT('Ctrl Pts',(-3.98974274318605,-7.07827505959329,
37.909676803749));
#166311=CARTESIAN_POINT('Ctrl Pts',(-3.97373070204795,-7.08727657695736,
37.9104017692501));
#166312=CARTESIAN_POINT('Ctrl Pts',(-3.92777101827637,-7.11290909821862,
37.9124840352482));
#166313=CARTESIAN_POINT('Ctrl Pts',(-3.89774870999761,-7.12940502217578,
37.9138459138456));
#166314=CARTESIAN_POINT('Ctrl Pts',(-3.60835263734616,-7.28604094650006,
37.9269902949133));
#166315=CARTESIAN_POINT('Ctrl Pts',(-3.34165616195927,-7.41214636706515,
37.9392431162941));
#166316=CARTESIAN_POINT('Ctrl Pts',(-2.3253892448422,-7.82666643400389,
37.9863302161116));
#166317=CARTESIAN_POINT('Ctrl Pts',(-1.5413366552053,-8.0179935602057,38.023851977727));
#166318=CARTESIAN_POINT('Ctrl Pts',(-0.550792223272148,-8.10883456324062,
38.0663988107547));
#166319=CARTESIAN_POINT('Ctrl Pts',(-0.358968438655843,-8.1195892367817,
38.0743831353632));
#166320=CARTESIAN_POINT('Ctrl Pts',(-0.146292963925848,-8.12395909474444,
38.0828725226761));
#166321=CARTESIAN_POINT('Ctrl Pts',(-0.125669405570101,-8.12430429117005,
38.0836923663129));
#166322=CARTESIAN_POINT('Ctrl Pts',(-0.095339674949844,-8.12469643191405,
38.0848933261827));
#166323=CARTESIAN_POINT('Ctrl Pts',(-0.0856344763786124,-8.12480452084219,
38.0852769085455));
#166324=CARTESIAN_POINT('Ctrl Pts',(-0.0683648892897313,-8.12496590924495,
38.0859582253492));
#166325=CARTESIAN_POINT('Ctrl Pts',(-0.0608005870605701,-8.12502603525592,
38.0862562290318));
#166326=CARTESIAN_POINT('Ctrl Pts',(-0.0450206665026735,-8.1251294266556,
38.0868770330987));
#166327=CARTESIAN_POINT('Ctrl Pts',(-0.0368050415279358,-8.12517079511895,
38.087199759495));
#166328=CARTESIAN_POINT('Ctrl Pts',(-0.0154694692249841,-8.12524586652023,
38.0880366251711));
#166329=CARTESIAN_POINT('Ctrl Pts',(-0.00234944978153691,-8.12526025296515,
38.0885500278008));
#166330=CARTESIAN_POINT('Ctrl Pts',(0.0537593022354977,-8.12518587678321,
38.0907406157975));
#166331=CARTESIAN_POINT('Ctrl Pts',(0.096747353920764,-8.12478772793749,
38.0924063553373));
#166332=CARTESIAN_POINT('Ctrl Pts',(0.428863352570705,-8.1190754538842,
38.1051898146597));
#166333=CARTESIAN_POINT('Ctrl Pts',(0.717539034679774,-8.09867045626168,
38.1158064118681));
#166334=CARTESIAN_POINT('Ctrl Pts',(1.47688289625519,-8.00406721871315,
38.1435128653537));
#166335=CARTESIAN_POINT('Ctrl Pts',(1.94315502220824,-7.90382372627553,
38.1603511095473));
#166336=CARTESIAN_POINT('Ctrl Pts',(2.72693599327359,-7.66172636292324,
38.190433974542));
#166337=CARTESIAN_POINT('Ctrl Pts',(3.04909583246139,-7.53931227673395,
38.2033358106881));
#166338=CARTESIAN_POINT('Ctrl Pts',(3.40986830431454,-7.37530961912341,
38.2185931745888));
#166339=CARTESIAN_POINT('Ctrl Pts',(3.45701835618854,-7.35332699250995,
38.2206031942479));
#166340=CARTESIAN_POINT('Ctrl Pts',(3.5281829894454,-7.31931236692451,38.2236613493931));
#166341=CARTESIAN_POINT('Ctrl Pts',(3.55235454295654,-7.30761150617925,
38.2247043762492));
#166342=CARTESIAN_POINT('Ctrl Pts',(3.59616437697616,-7.28613550037504,
38.2266026283042));
#166343=CARTESIAN_POINT('Ctrl Pts',(3.61582196510093,-7.27640022730247,
38.2274572517716));
#166344=CARTESIAN_POINT('Ctrl Pts',(3.65635295502987,-7.25612275663772,
38.2292253037126));
#166345=CARTESIAN_POINT('Ctrl Pts',(3.67722078418132,-7.2455697975122,38.2301388962755));
#166346=CARTESIAN_POINT('Ctrl Pts',(3.72977441057085,-7.21870766642493,
38.2324482368461));
#166347=CARTESIAN_POINT('Ctrl Pts',(3.76139893641345,-7.20227988555951,
38.2338457810541));
#166348=CARTESIAN_POINT('Ctrl Pts',(3.88773803660394,-7.13559228865542,
38.2394617742274));
#166349=CARTESIAN_POINT('Ctrl Pts',(3.98156055472042,-7.08366849594916,
38.2437069544241));
#166350=CARTESIAN_POINT('Ctrl Pts',(4.21363294470644,-6.94916611545733,
38.2544114808591));
#166351=CARTESIAN_POINT('Ctrl Pts',(4.35050530885193,-6.86430724083353,
38.2609113765764));
#166352=CARTESIAN_POINT('Ctrl Pts',(4.55559190907852,-6.72855738594327,
38.270956421412));
#166353=CARTESIAN_POINT('Ctrl Pts',(4.62567988378337,-6.68056790062044,
38.2744458740129));
#166354=CARTESIAN_POINT('Ctrl Pts',(5.02295929208667,-6.39929960150985,
38.2945532403175));
#166355=CARTESIAN_POINT('Ctrl Pts',(5.33323121619031,-6.14310832854294,
38.3115915519528));
#166356=CARTESIAN_POINT('Ctrl Pts',(5.92115130602959,-5.57942307948749,
38.3461481302878));
#166357=CARTESIAN_POINT('Ctrl Pts',(6.19685755177092,-5.27152512183989,
38.3636140891569));
#166358=CARTESIAN_POINT('Ctrl Pts',(6.46190407002446,-4.9258508646601,38.3809845082919));
#166359=CARTESIAN_POINT('Ctrl Pts',(6.47574789880091,-4.90763691755449,
38.3818935354847));
#166360=CARTESIAN_POINT('Ctrl Pts',(6.4950607049772,-4.88200357891946,38.3831638804721));
#166361=CARTESIAN_POINT('Ctrl Pts',(6.50059419916956,-4.87463306972731,
38.3835281158643));
#166362=CARTESIAN_POINT('Ctrl Pts',(6.51070814152812,-4.86111364271003,
38.38419430383));
#166363=CARTESIAN_POINT('Ctrl Pts',(6.5152924458337,-4.85496763091724,38.3844964345482));
#166364=CARTESIAN_POINT('Ctrl Pts',(6.52455378603278,-4.8425145440255,38.3851071395459));
#166365=CARTESIAN_POINT('Ctrl Pts',(6.52923039364126,-4.83620715884043,
38.3854156935906));
#166366=CARTESIAN_POINT('Ctrl Pts',(6.54070250292334,-4.82068764516996,
38.386173008969));
#166367=CARTESIAN_POINT('Ctrl Pts',(6.54748770574271,-4.81146789960011,
38.386621276952));
#166368=CARTESIAN_POINT('Ctrl Pts',(6.57207127214443,-4.77791540498625,
38.3882466038051));
#166369=CARTESIAN_POINT('Ctrl Pts',(6.58975379945234,-4.7534977982744,38.3894179718311));
#166370=CARTESIAN_POINT('Ctrl Pts',(6.68809068872795,-4.61610219657266,
38.395942851039));
#166371=CARTESIAN_POINT('Ctrl Pts',(6.76597309302061,-4.50117367956736,
38.4011386815693));
#166372=CARTESIAN_POINT('Ctrl Pts',(7.31415715154847,-3.64583640047183,
38.4382074511942));
#166373=CARTESIAN_POINT('Ctrl Pts',(7.66478285444663,-2.835564676331,38.4653766302818));
#166374=CARTESIAN_POINT('Ctrl Pts',(7.89231785045313,-1.93234034343207,
38.4985622363037));
#166375=CARTESIAN_POINT('Ctrl Pts',(7.90502134343568,-1.87969617621614,
38.5005040552427));
#166376=CARTESIAN_POINT('Ctrl Pts',(7.97060789577559,-1.59546970793206,
38.511036158012));
#166377=CARTESIAN_POINT('Ctrl Pts',(8.01383973962798,-1.36179164402329,
38.5198712366129));
#166378=CARTESIAN_POINT('Ctrl Pts',(8.05030829622664,-1.1013057759995,38.5300037371131));
#166379=CARTESIAN_POINT('Ctrl Pts',(8.05372561466883,-1.07603056937347,
38.5309897882464));
#166380=CARTESIAN_POINT('Ctrl Pts',(8.05865928522981,-1.03819941419508,
38.5324700867801));
#166381=CARTESIAN_POINT('Ctrl Pts',(8.0602654320464,-1.02565523559198,38.5329616528943));
#166382=CARTESIAN_POINT('Ctrl Pts',(8.06298135965207,-1.00404313387082,
38.5338098204781));
#166383=CARTESIAN_POINT('Ctrl Pts',(8.06410514757251,-0.994976979126865,
38.5341660032078));
#166384=CARTESIAN_POINT('Ctrl Pts',(8.06633167306494,-0.97676292044406,
38.5348823509958));
#166385=CARTESIAN_POINT('Ctrl Pts',(8.06743414469654,-0.967614997290918,
38.5352425234403));
#166386=CARTESIAN_POINT('Ctrl Pts',(8.06963369640123,-0.949098802267439,
38.5359723384472));
#166387=CARTESIAN_POINT('Ctrl Pts',(8.07073002877807,-0.939730457322439,
38.5363420027014));
#166388=CARTESIAN_POINT('Ctrl Pts',(8.07321103188665,-0.918205262162394,
38.5371923130173));
#166389=CARTESIAN_POINT('Ctrl Pts',(8.07458455919379,-0.906047164163022,
38.5376732908264));
#166390=CARTESIAN_POINT('Ctrl Pts',(8.07803815099798,-0.874845236316933,
38.5389094468736));
#166391=CARTESIAN_POINT('Ctrl Pts',(8.08007833162871,-0.855797116816095,
38.539665812593));
#166392=CARTESIAN_POINT('Ctrl Pts',(8.11085524541885,-0.558524386217931,
38.5514970428282));
#166393=CARTESIAN_POINT('Ctrl Pts',(8.12527172054597,-0.279029717205217,
38.5629994860888));
#166394=CARTESIAN_POINT('Ctrl Pts',(8.12524997543795,0.000631779634971061,
38.5748840163789));
#166395=CARTESIAN_POINT('',(8.13321556035817,0.00564624965145891,40.5832974432124));
#166396=CARTESIAN_POINT('Ctrl Pts',(8.12524999535401,0.000274771867430455,
38.5832974955445));
#166397=CARTESIAN_POINT('Ctrl Pts',(8.12524210757769,0.233523376081798,
38.5924146984481));
#166398=CARTESIAN_POINT('Ctrl Pts',(8.11518633213374,0.466490767603277,
38.6015319013518));
#166399=CARTESIAN_POINT('Ctrl Pts',(8.09518039536984,0.698385229597441,
38.6106491042555));
#166400=CARTESIAN_POINT('Ctrl Pts',(8.07505952886503,0.931611874670458,
38.6198186835003));
#166401=CARTESIAN_POINT('Ctrl Pts',(8.04487389372223,1.16375312819179,38.628988262745));
#166402=CARTESIAN_POINT('Ctrl Pts',(8.00477373273416,1.39401759322803,38.6381578419898));
#166403=CARTESIAN_POINT('Ctrl Pts',(7.96458288338273,1.62480281197092,38.6473481586609));
#166404=CARTESIAN_POINT('Ctrl Pts',(7.91443266829132,1.85370265519256,38.6565384753319));
#166405=CARTESIAN_POINT('Ctrl Pts',(7.85452446651707,2.07993580847695,38.665728792003));
#166406=CARTESIAN_POINT('Ctrl Pts',(7.79451478749117,2.30655217337424,38.6749346759595));
#166407=CARTESIAN_POINT('Ctrl Pts',(7.72471407706188,2.53049271850867,38.6841405599161));
#166408=CARTESIAN_POINT('Ctrl Pts',(7.64537423766149,2.7509889728245,38.6933464438726));
#166409=CARTESIAN_POINT('Ctrl Pts',(7.60797979718048,2.85491323232152,38.697685359634));
#166410=CARTESIAN_POINT('Ctrl Pts',(7.56846701995292,2.95807261897161,38.7020242753955));
#166411=CARTESIAN_POINT('Ctrl Pts',(7.52686604962479,3.06038805276484,38.706363191157));
#166412=CARTESIAN_POINT('Ctrl Pts',(7.4542068057907,3.23908970307095,38.7139414359864));
#166413=CARTESIAN_POINT('Ctrl Pts',(7.3750775372003,3.41545293191262,38.7215196808159));
#166414=CARTESIAN_POINT('Ctrl Pts',(7.28965622804766,3.58895522950425,38.7290979256453));
#166415=CARTESIAN_POINT('Ctrl Pts',(7.20429848313715,3.76232841947436,38.7366705313035));
#166416=CARTESIAN_POINT('Ctrl Pts',(7.11265817321843,3.93284458582282,38.7442431369617));
#166417=CARTESIAN_POINT('Ctrl Pts',(7.01496204782145,4.09999939391761,38.7518157426199));
#166418=CARTESIAN_POINT('Ctrl Pts',(6.91732006844743,4.26706155997525,38.7593841513207));
#166419=CARTESIAN_POINT('Ctrl Pts',(6.81362913699136,4.43076575860533,38.7669525600214));
#166420=CARTESIAN_POINT('Ctrl Pts',(6.70416274786647,4.59063061165015,38.7745209687222));
#166421=CARTESIAN_POINT('Ctrl Pts',(6.59472280669528,4.75045684006997,38.782087548835));
#166422=CARTESIAN_POINT('Ctrl Pts',(6.47951038602011,4.90644526182936,38.7896541289478));
#166423=CARTESIAN_POINT('Ctrl Pts',(6.35884334392026,5.05814184162336,38.7972207090606));
#166424=CARTESIAN_POINT('Ctrl Pts',(6.23819770760759,5.20981151113062,38.8047859468963));
#166425=CARTESIAN_POINT('Ctrl Pts',(6.11209960723124,5.35719056827615,38.812351184732));
#166426=CARTESIAN_POINT('Ctrl Pts',(5.98090820689058,5.49985677843059,38.8199164225677));
#166427=CARTESIAN_POINT('Ctrl Pts',(5.84967118500481,5.64257260047213,38.8274842911997));
#166428=CARTESIAN_POINT('Ctrl Pts',(5.71333757148827,5.78057202814926,38.8350521598316));
#166429=CARTESIAN_POINT('Ctrl Pts',(5.57230486251974,5.913468194016,38.8426200284635));
#166430=CARTESIAN_POINT('Ctrl Pts',(5.43309210538238,6.04464940579732,38.8500902377902));
#166431=CARTESIAN_POINT('Ctrl Pts',(5.28930108925228,6.17085807234827,38.8575604471169));
#166432=CARTESIAN_POINT('Ctrl Pts',(5.14134656895274,6.2917599302912,38.8650306564436));
#166433=CARTESIAN_POINT('Ctrl Pts',(4.95703562845422,6.44237063890872,38.8743364978869));
#166434=CARTESIAN_POINT('Ctrl Pts',(4.76635551154618,6.58467379760845,38.8836423393301));
#166435=CARTESIAN_POINT('Ctrl Pts',(4.57001718157966,6.71823120490555,38.8929481807734));
#166436=CARTESIAN_POINT('Ctrl Pts',(4.37262475073004,6.85250565497774,38.9023039834019));
#166437=CARTESIAN_POINT('Ctrl Pts',(4.16951325608752,6.97794021200562,38.9116597860305));
#166438=CARTESIAN_POINT('Ctrl Pts',(3.96142482957386,7.09413848766259,38.9210155886591));
#166439=CARTESIAN_POINT('Ctrl Pts',(3.75232624712042,7.21090084264062,38.9304168086122));
#166440=CARTESIAN_POINT('Ctrl Pts',(3.53820234340236,7.31833702468645,38.9398180285652));
#166441=CARTESIAN_POINT('Ctrl Pts',(3.31982502679976,7.41609394182234,38.9492192485183));
#166442=CARTESIAN_POINT('Ctrl Pts',(3.101211361138,7.51395666095154,38.9586306433812));
#166443=CARTESIAN_POINT('Ctrl Pts',(2.87833511302379,7.60211915607006,38.968042038244));
#166444=CARTESIAN_POINT('Ctrl Pts',(2.65198891477359,7.68027619024329,38.9774534331069));
#166445=CARTESIAN_POINT('Ctrl Pts',(2.42590822441072,7.75834154490441,38.9868537882457));
#166446=CARTESIAN_POINT('Ctrl Pts',(2.19636575557207,7.82642489015275,38.9962541433845));
#166447=CARTESIAN_POINT('Ctrl Pts',(1.96416892654065,7.88427092320604,39.0056544985233));
#166448=CARTESIAN_POINT('Ctrl Pts',(1.81560460703967,7.9212820080354,39.0116690395921));
#166449=CARTESIAN_POINT('Ctrl Pts',(1.66595402282328,7.95410322194627,39.017683580661));
#166450=CARTESIAN_POINT('Ctrl Pts',(1.51543234454219,7.98267827058158,39.0236981217298));
#166451=CARTESIAN_POINT('Ctrl Pts',(1.32167129884812,8.0194618845272,39.0314404202491));
#166452=CARTESIAN_POINT('Ctrl Pts',(1.12637519902295,8.04922361378799,39.0391827187683));
#166453=CARTESIAN_POINT('Ctrl Pts',(0.930102878696077,8.0718397034097,39.0469250172875));
#166454=CARTESIAN_POINT('Ctrl Pts',(0.733952818251539,8.09444170525555,
39.0546624930559));
#166455=CARTESIAN_POINT('Ctrl Pts',(0.536828097577449,8.10990688979997,
39.0623999688243));
#166456=CARTESIAN_POINT('Ctrl Pts',(0.339297220629357,8.11816265903641,
39.0701374445926));
#166457=CARTESIAN_POINT('Ctrl Pts',(0.141854280614204,8.12641475296378,
39.0778714757861));
#166458=CARTESIAN_POINT('Ctrl Pts',(-0.0559941033429836,8.12746380893499,
39.0856055069797));
#166459=CARTESIAN_POINT('Ctrl Pts',(-0.253674693380241,8.12128910410401,
39.0933395381732));
#166460=CARTESIAN_POINT('Ctrl Pts',(-0.451329986527172,8.11511518944079,
39.1010725796543));
#166461=CARTESIAN_POINT('Ctrl Pts',(-0.648817175395356,8.10171935859924,
39.1088056211354));
#166462=CARTESIAN_POINT('Ctrl Pts',(-0.845563032603451,8.08113300969576,
39.1165386626164));
#166463=CARTESIAN_POINT('Ctrl Pts',(-1.04228923504712,8.06054871735318,
39.1242709315724));
#166464=CARTESIAN_POINT('Ctrl Pts',(-1.23827390224691,8.03277537814228,
39.1320032005285));
#166465=CARTESIAN_POINT('Ctrl Pts',(-1.43294906026735,7.99789625796552,
39.1397354694845));
#166466=CARTESIAN_POINT('Ctrl Pts',(-1.62769910096705,7.96300372137758,
39.1474707126927));
#166467=CARTESIAN_POINT('Ctrl Pts',(-1.82113827796923,7.92100000530547,
39.1552059559009));
#166468=CARTESIAN_POINT('Ctrl Pts',(-2.01270829344443,7.87201961938612,
39.1629411991091));
#166469=CARTESIAN_POINT('Ctrl Pts',(-2.17306223844902,7.83102051996792,
39.1694159950782));
#166470=CARTESIAN_POINT('Ctrl Pts',(-2.33210662913009,7.7851341122364,39.1758907910473));
#166471=CARTESIAN_POINT('Ctrl Pts',(-2.48952222673874,7.73446615126563,
39.1823655870165));
#166472=CARTESIAN_POINT('Ctrl Pts',(-2.69408567132472,7.66862253231183,
39.1907796615209));
#166473=CARTESIAN_POINT('Ctrl Pts',(-2.8959968613616,7.59467172251155,39.1991937360253));
#166474=CARTESIAN_POINT('Ctrl Pts',(-3.09462854244247,7.51285310296963,
39.2076078105297));
#166475=CARTESIAN_POINT('Ctrl Pts',(-3.29331569588629,7.43101163373861,
39.2160242348536));
#166476=CARTESIAN_POINT('Ctrl Pts',(-3.48872126784141,7.34129806886591,
39.2244406591775));
#166477=CARTESIAN_POINT('Ctrl Pts',(-3.68023858701895,7.24399968975129,
39.2328570835014));
#166478=CARTESIAN_POINT('Ctrl Pts',(-3.87180340115735,7.14667718131652,
39.2412755950399));
#166479=CARTESIAN_POINT('Ctrl Pts',(-4.05947780215079,7.0417662229967,39.2496941065784));
#166480=CARTESIAN_POINT('Ctrl Pts',(-4.2426793267108,6.9296002549354,39.2581126181169));
#166481=CARTESIAN_POINT('Ctrl Pts',(-4.42595121821116,6.81739120439429,
39.2665343631705));
#166482=CARTESIAN_POINT('Ctrl Pts',(-4.60474657423996,6.69792171228346,
39.2749561082241));
#166483=CARTESIAN_POINT('Ctrl Pts',(-4.77851034355444,6.57156955825952,
39.2833778532777));
#166484=CARTESIAN_POINT('Ctrl Pts',(-4.95229294838677,6.44520370800729,
39.2918005112255));
#166485=CARTESIAN_POINT('Ctrl Pts',(-5.1210426658387,6.31195386392228,39.3002231691733));
#166486=CARTESIAN_POINT('Ctrl Pts',(-5.28423558932979,6.17223960965227,
39.3086458271211));
#166487=CARTESIAN_POINT('Ctrl Pts',(-5.44745954741912,6.03249878575132,
39.317070086816));
#166488=CARTESIAN_POINT('Ctrl Pts',(-5.60512439998086,5.88629126742338,
39.325494346511));
#166489=CARTESIAN_POINT('Ctrl Pts',(-5.75674033665574,5.73407605973454,
39.3339186062059));
#166490=CARTESIAN_POINT('Ctrl Pts',(-5.79942117540584,5.69122652242889,
39.3362900882382));
#166491=CARTESIAN_POINT('Ctrl Pts',(-5.84162288207641,5.64790113027133,
39.3386615702704));
#166492=CARTESIAN_POINT('Ctrl Pts',(-5.88333505391007,5.60411065254184,
39.3410330523027));
#166493=CARTESIAN_POINT('Ctrl Pts',(-6.03151112962291,5.44855171474736,
39.3494573775228));
#166494=CARTESIAN_POINT('Ctrl Pts',(-6.17352204756723,5.28710500987745,
39.3578817027429));
#166495=CARTESIAN_POINT('Ctrl Pts',(-6.30892210356419,5.12027240033762,
39.366306027963));
#166496=CARTESIAN_POINT('Ctrl Pts',(-6.44429876077515,4.95346862151356,
39.3747288973567));
#166497=CARTESIAN_POINT('Ctrl Pts',(-6.57306667160138,4.78128100183735,
39.3831517667504));
#166498=CARTESIAN_POINT('Ctrl Pts',(-6.69482044007219,4.6042444372222,39.391574636144));
#166499=CARTESIAN_POINT('Ctrl Pts',(-6.81654932795624,4.42724405032592,
39.3999957843102));
#166500=CARTESIAN_POINT('Ctrl Pts',(-6.93126678632341,4.2453969145697,39.4084169324764));
#166501=CARTESIAN_POINT('Ctrl Pts',(-7.03861015199073,4.05926775303046,
39.4168380806426));
#166502=CARTESIAN_POINT('Ctrl Pts',(-7.14592340073171,3.87319081305343,
39.4252568661188));
#166503=CARTESIAN_POINT('Ctrl Pts',(-7.24586655720186,3.68283447526028,
39.4336756515949));
#166504=CARTESIAN_POINT('Ctrl Pts',(-7.33812190544222,3.48878982791584,
39.4420944370711));
#166505=CARTESIAN_POINT('Ctrl Pts',(-7.43035148276851,3.2947993856449,39.4505108708158));
#166506=CARTESIAN_POINT('Ctrl Pts',(-7.51489742641705,3.09712292911058,
39.4589273045606));
#166507=CARTESIAN_POINT('Ctrl Pts',(-7.59148883563105,2.89637442693258,
39.4673437383054));
#166508=CARTESIAN_POINT('Ctrl Pts',(-7.66805244661633,2.69569878478992,
39.475757117374));
#166509=CARTESIAN_POINT('Ctrl Pts',(-7.73666719450974,2.49195356996512,
39.4841704964427));
#166510=CARTESIAN_POINT('Ctrl Pts',(-7.79711065601113,2.28577185659849,
39.4925838755113));
#166511=CARTESIAN_POINT('Ctrl Pts',(-7.8141531339479,2.2276374080786,39.4949560895373));
#166512=CARTESIAN_POINT('Ctrl Pts',(-7.83054629400759,2.16930936624431,
39.4973283035632));
#166513=CARTESIAN_POINT('Ctrl Pts',(-7.84628585923969,2.11080216448517,
39.4997005175892));
#166514=CARTESIAN_POINT('Ctrl Pts',(-7.89760856712009,1.92002510168161,
39.5074357024999));
#166515=CARTESIAN_POINT('Ctrl Pts',(-7.94200084032748,1.72725734574842,
39.5151708874106));
#166516=CARTESIAN_POINT('Ctrl Pts',(-7.97931310134191,1.53305250831581,
39.5229060723212));
#166517=CARTESIAN_POINT('Ctrl Pts',(-8.01661382448334,1.33890772381724,
39.5306388653216));
#166518=CARTESIAN_POINT('Ctrl Pts',(-8.04683882868994,1.14332708930259,
39.538371658322));
#166519=CARTESIAN_POINT('Ctrl Pts',(-8.06988932040479,0.94687587302495,
39.5461044513224));
#166520=CARTESIAN_POINT('Ctrl Pts',(-8.09293677974301,0.750450500624451,
39.5538362270456));
#166521=CARTESIAN_POINT('Ctrl Pts',(-8.10881156616961,0.553155125470171,
39.5615680027687));
#166522=CARTESIAN_POINT('Ctrl Pts',(-8.11746656262995,0.355561762686395,
39.5692997784919));
#166523=CARTESIAN_POINT('Ctrl Pts',(-8.12612465608434,0.157897695602473,
39.5770343208555));
#166524=CARTESIAN_POINT('Ctrl Pts',(-8.12755777838015,-0.0400642190034208,
39.584768863219));
#166525=CARTESIAN_POINT('Ctrl Pts',(-8.1217709068508,-0.237749656428669,
39.5925034055826));
#166526=CARTESIAN_POINT('Ctrl Pts',(-8.11598305798337,-0.435468480720032,
39.6002392542242));
#166527=CARTESIAN_POINT('Ctrl Pts',(-8.10297280358738,-0.632910381755871,
39.6079751028658));
#166528=CARTESIAN_POINT('Ctrl Pts',(-8.0827971702813,-0.829504349953945,
39.6157109515074));
#166529=CARTESIAN_POINT('Ctrl Pts',(-8.06260502835847,-1.02625918023887,
39.6234531299706));
#166530=CARTESIAN_POINT('Ctrl Pts',(-8.0352358371097,-1.22216434056028,
39.6311953084338));
#166531=CARTESIAN_POINT('Ctrl Pts',(-8.00079824059787,-1.41665630120576,
39.638937486897));
#166532=CARTESIAN_POINT('Ctrl Pts',(-7.97198896838768,-1.57936137950603,
39.6454143188899));
#166533=CARTESIAN_POINT('Ctrl Pts',(-7.93823387793344,-1.74107750178691,
39.6518911508828));
#166534=CARTESIAN_POINT('Ctrl Pts',(-7.89962360986838,-1.90148215477032,
39.6583679828757));
#166535=CARTESIAN_POINT('Ctrl Pts',(-7.84359924502978,-2.1342329034937,
39.6677660113473));
#166536=CARTESIAN_POINT('Ctrl Pts',(-7.77732077661169,-2.36435467700588,
39.6771640398188));
#166537=CARTESIAN_POINT('Ctrl Pts',(-7.70105132916896,-2.59104148712539,
39.6865620682903));
#166538=CARTESIAN_POINT('Ctrl Pts',(-7.62467335668622,-2.8180508536022,
39.6959734693698));
#166539=CARTESIAN_POINT('Ctrl Pts',(-7.53827597995956,-3.04161544449088,
39.7053848704492));
#166540=CARTESIAN_POINT('Ctrl Pts',(-7.4421718402354,-3.26094554736923,
39.7147962715287));
#166541=CARTESIAN_POINT('Ctrl Pts',(-7.34621240151355,-3.4799454117603,
39.7241935021554));
#166542=CARTESIAN_POINT('Ctrl Pts',(-7.24057542820372,-3.69472349902118,
39.7335907327821));
#166543=CARTESIAN_POINT('Ctrl Pts',(-7.12561997257765,-3.90451374295218,
39.7429879634088));
#166544=CARTESIAN_POINT('Ctrl Pts',(-7.01095447749335,-4.11377481762839,
39.7523614907143));
#166545=CARTESIAN_POINT('Ctrl Pts',(-6.88701745004613,-4.31807313629427,
39.7617350180199));
#166546=CARTESIAN_POINT('Ctrl Pts',(-6.75421269074996,-4.51666895959979,
39.7711085453255));
#166547=CARTESIAN_POINT('Ctrl Pts',(-6.62227035775963,-4.71397511329438,
39.7804212014953));
#166548=CARTESIAN_POINT('Ctrl Pts',(-6.48157509905111,-4.90565254558841,
39.7897338576651));
#166549=CARTESIAN_POINT('Ctrl Pts',(-6.33256970855235,-5.0909968030657,
39.799046513835));
#166550=CARTESIAN_POINT('Ctrl Pts',(-6.23662686349042,-5.21033782367401,
39.8050428252773));
#166551=CARTESIAN_POINT('Ctrl Pts',(-6.13723964548609,-5.32705358214587,
39.8110391367196));
#166552=CARTESIAN_POINT('Ctrl Pts',(-6.03453665110094,-5.44096084979661,
39.817035448162));
#166553=CARTESIAN_POINT('Ctrl Pts',(-5.90492010824206,-5.58471777069049,
39.824603106376));
#166554=CARTESIAN_POINT('Ctrl Pts',(-5.77007134326542,-5.72394222342455,
39.83217076459));
#166555=CARTESIAN_POINT('Ctrl Pts',(-5.63035866508292,-5.85822062276812,
39.839738422804));
#166556=CARTESIAN_POINT('Ctrl Pts',(-5.49068467082975,-5.99246184283649,
39.8473039856694));
#166557=CARTESIAN_POINT('Ctrl Pts',(-5.34614970784548,-6.12175947992718,
39.8548695485349));
#166558=CARTESIAN_POINT('Ctrl Pts',(-5.19715958558022,-6.24573612991388,
39.8624351114004));
#166559=CARTESIAN_POINT('Ctrl Pts',(-5.04818251625903,-6.3697019183733,
39.870000011451));
#166560=CARTESIAN_POINT('Ctrl Pts',(-4.89475134769421,-6.48834741307377,
39.8775649115016));
#166561=CARTESIAN_POINT('Ctrl Pts',(-4.73730560536102,-6.60133495316781,
39.8851298115521));
#166562=CARTESIAN_POINT('Ctrl Pts',(-4.57978258963036,-6.71437794684837,
39.8926984244089));
#166563=CARTESIAN_POINT('Ctrl Pts',(-4.41824136106163,-6.82175722093497,
39.9002670372657));
#166564=CARTESIAN_POINT('Ctrl Pts',(-4.25315158443686,-6.92317767808268,
39.9078356501225));
#166565=CARTESIAN_POINT('Ctrl Pts',(-4.08802509474823,-7.02462068935697,
39.9154059461058));
#166566=CARTESIAN_POINT('Ctrl Pts',(-3.91934880428558,-7.12010206132231,
39.922976242089));
#166567=CARTESIAN_POINT('Ctrl Pts',(-3.74761746868852,-7.20937243252703,
39.9305465380722));
#166568=CARTESIAN_POINT('Ctrl Pts',(-3.57571212029093,-7.29873326006718,
39.9381245049234));
#166569=CARTESIAN_POINT('Ctrl Pts',(-3.40074587347904,-7.38187035350387,
39.9457024717746));
#166570=CARTESIAN_POINT('Ctrl Pts',(-3.22323480882442,-7.45858196507101,
39.9532804386259));
#166571=CARTESIAN_POINT('Ctrl Pts',(-3.04815542160801,-7.53424272442532,
39.9607545969001));
#166572=CARTESIAN_POINT('Ctrl Pts',(-2.87060083248374,-7.60365286137363,
39.9682287551743));
#166573=CARTESIAN_POINT('Ctrl Pts',(-2.69108010185882,-7.66666651471678,
39.9757029134486));
#166574=CARTESIAN_POINT('Ctrl Pts',(-2.49713188231875,-7.73474436750891,
39.9837777451675));
#166575=CARTESIAN_POINT('Ctrl Pts',(-2.30047481299285,-7.79550205760272,
39.9918525768864));
#166576=CARTESIAN_POINT('Ctrl Pts',(-2.10168916992473,-7.84873175713893,
39.9999274086052));
#166577=CARTESIAN_POINT('Ctrl Pts',(-1.90303504311832,-7.90192623999154,
40.0079968980285));
#166578=CARTESIAN_POINT('Ctrl Pts',(-1.70225545583536,-7.94760258222244,
40.0160663874517));
#166579=CARTESIAN_POINT('Ctrl Pts',(-1.49994657558979,-7.98560253411579,
40.0241358768749));
#166580=CARTESIAN_POINT('Ctrl Pts',(-1.29774398181256,-8.02358252207735,
40.0322011268523));
#166581=CARTESIAN_POINT('Ctrl Pts',(-1.09401400802125,-8.05389410411521,
40.0402663768297));
#166582=CARTESIAN_POINT('Ctrl Pts',(-0.889364382368222,-8.07642981507762,
40.0483316268072));
#166583=CARTESIAN_POINT('Ctrl Pts',(-0.684794422560027,-8.09895675335625,
40.0563937371504));
#166584=CARTESIAN_POINT('Ctrl Pts',(-0.479305839345301,-8.11371382319431,
40.0644558474937));
#166585=CARTESIAN_POINT('Ctrl Pts',(-0.273513501540643,-8.12064516691716,
40.072517957837));
#166586=CARTESIAN_POINT('Ctrl Pts',(-0.0677732906805856,-8.12757475493921,
40.0805780260577));
#166587=CARTESIAN_POINT('Ctrl Pts',(0.138270204976888,-8.12668256027873,
40.0886380942784));
#166588=CARTESIAN_POINT('Ctrl Pts',(0.343999451035131,-8.11796476588729,
40.0966981624991));
#166589=CARTESIAN_POINT('Ctrl Pts',(0.552810828024079,-8.10911636593415,
40.1048789825625));
#166590=CARTESIAN_POINT('Ctrl Pts',(0.761298131211823,-8.09220600530942,
40.1130598026259));
#166591=CARTESIAN_POINT('Ctrl Pts',(0.968817375836679,-8.06728457752526,
40.1212406226894));
#166592=CARTESIAN_POINT('Ctrl Pts',(1.17329341071894,-8.04272861527645,
40.1293014733911));
#166593=CARTESIAN_POINT('Ctrl Pts',(1.37682926588926,-8.01039499268433,
40.1373623240928));
#166594=CARTESIAN_POINT('Ctrl Pts',(1.5788153236076,-7.97038454131555,40.1454231747945));
#166595=CARTESIAN_POINT('Ctrl Pts',(1.78083487887691,-7.93036745457723,
40.1534853623151));
#166596=CARTESIAN_POINT('Ctrl Pts',(1.98130381317512,-7.88267106129582,
40.1615475498356));
#166597=CARTESIAN_POINT('Ctrl Pts',(2.17962331319072,-7.8274472067907,40.1696097373561));
#166598=CARTESIAN_POINT('Ctrl Pts',(2.37800027094315,-7.77220735266023,
40.1776742606784));
#166599=CARTESIAN_POINT('Ctrl Pts',(2.57422624714499,-7.70943577251278,
40.1857387840007));
#166600=CARTESIAN_POINT('Ctrl Pts',(2.76771760874932,-7.63933418569439,
40.1938033073231));
#166601=CARTESIAN_POINT('Ctrl Pts',(2.96612802988728,-7.56745043208517,
40.2020728520479));
#166602=CARTESIAN_POINT('Ctrl Pts',(3.16166262005876,-7.48785916244496,
40.2103423967728));
#166603=CARTESIAN_POINT('Ctrl Pts',(3.35371411149903,-7.40083030617729,
40.2186119414977));
#166604=CARTESIAN_POINT('Ctrl Pts',(3.54125725758373,-7.31584442357785,
40.2266873613903));
#166605=CARTESIAN_POINT('Ctrl Pts',(3.72547872804214,-7.22376639577497,
40.234762781283));
#166606=CARTESIAN_POINT('Ctrl Pts',(3.90583789202167,-7.12489423947806,
40.2428382011756));
#166607=CARTESIAN_POINT('Ctrl Pts',(4.09270053066488,-7.02245690495992,
40.2512048083166));
#166608=CARTESIAN_POINT('Ctrl Pts',(4.27541682254546,-6.91272655889478,
40.2595714154575));
#166609=CARTESIAN_POINT('Ctrl Pts',(4.45341796277665,-6.79608387318155,
40.2679380225985));
#166610=CARTESIAN_POINT('Ctrl Pts',(4.63141910300777,-6.67944118746835,
40.2763046297395));
#166611=CARTESIAN_POINT('Ctrl Pts',(4.80470480775092,-6.55588641026857,
40.2846712368804));
#166612=CARTESIAN_POINT('Ctrl Pts',(4.97274368742939,-6.4258468532662,40.2930378440214));
#166613=CARTESIAN_POINT('Ctrl Pts',(5.13498501363584,-6.30029382513525,
40.3011157926545));
#166614=CARTESIAN_POINT('Ctrl Pts',(5.29265095278334,-6.16845190210063,
40.3091937412875));
#166615=CARTESIAN_POINT('Ctrl Pts',(5.44523946487812,-6.03067614224424,
40.3172716899206));
#166616=CARTESIAN_POINT('Ctrl Pts',(5.59764123962346,-5.89306899193688,
40.3253397527851));
#166617=CARTESIAN_POINT('Ctrl Pts',(5.74497774094924,-5.7495426899506,40.3334078156496));
#166618=CARTESIAN_POINT('Ctrl Pts',(5.88677796803571,-5.60049397085198,
40.3414758785141));
#166619=CARTESIAN_POINT('Ctrl Pts',(6.02842211784675,-5.45160930732971,
40.3495350609889));
#166620=CARTESIAN_POINT('Ctrl Pts',(6.16454192508588,-5.29721457162391,
40.3575942434637));
#166621=CARTESIAN_POINT('Ctrl Pts',(6.29470095649393,-5.13774536453631,
40.3656534259386));
#166622=CARTESIAN_POINT('Ctrl Pts',(6.4246928031767,-4.97848099006993,40.3737022566753));
#166623=CARTESIAN_POINT('Ctrl Pts',(6.54873894957274,-4.81415539079815,
40.381751087412));
#166624=CARTESIAN_POINT('Ctrl Pts',(6.66644115792267,-4.64523948257295,
40.3897999181487));
#166625=CARTESIAN_POINT('Ctrl Pts',(6.78405433685325,-4.47645134157862,
40.3978426607861));
#166626=CARTESIAN_POINT('Ctrl Pts',(6.89533296268568,-4.30308007029934,
40.4058854034236));
#166627=CARTESIAN_POINT('Ctrl Pts',(6.99991945712543,-4.12562906188338,
40.413928146061));
#166628=CARTESIAN_POINT('Ctrl Pts',(7.10442076192845,-3.94832259399369,
40.4219643375818));
#166629=CARTESIAN_POINT('Ctrl Pts',(7.20224064897075,-3.76694328896893,
40.4300005291027));
#166630=CARTESIAN_POINT('Ctrl Pts',(7.2930650610116,-3.58202311248154,40.4380367206235));
#166631=CARTESIAN_POINT('Ctrl Pts',(7.34455883669927,-3.47718083633352,
40.4425929168516));
#166632=CARTESIAN_POINT('Ctrl Pts',(7.39380475576001,-3.37120089226644,
40.4471491130796));
#166633=CARTESIAN_POINT('Ctrl Pts',(7.44075200433485,-3.26418399795216,
40.4517053093077));
#166634=CARTESIAN_POINT('Ctrl Pts',(7.52120398147608,-3.08079261727573,
40.4595131150027));
#166635=CARTESIAN_POINT('Ctrl Pts',(7.59485701558088,-2.89445919022869,
40.4673209206978));
#166636=CARTESIAN_POINT('Ctrl Pts',(7.66150718331788,-2.70573377154303,
40.4751287263929));
#166637=CARTESIAN_POINT('Ctrl Pts',(7.72817956003812,-2.51694546629906,
40.4829391337833));
#166638=CARTESIAN_POINT('Ctrl Pts',(7.78784430650326,-2.32576390492744,
40.4907495411736));
#166639=CARTESIAN_POINT('Ctrl Pts',(7.84034725305165,-2.13275467742199,
40.498559948564));
#166640=CARTESIAN_POINT('Ctrl Pts',(7.89290272100167,-1.93955237284525,
40.5063781691071));
#166641=CARTESIAN_POINT('Ctrl Pts',(7.93828198712675,-1.74451908146978,
40.5141963896502));
#166642=CARTESIAN_POINT('Ctrl Pts',(7.97638169558376,-1.548232091405,40.5220146101934));
#166643=CARTESIAN_POINT('Ctrl Pts',(8.01450240419812,-1.35183691002216,
40.5298371400572));
#166644=CARTESIAN_POINT('Ctrl Pts',(8.04533550241622,-1.15418699087737,
40.537659669921));
#166645=CARTESIAN_POINT('Ctrl Pts',(8.06882945521055,-0.955865463978399,
40.5454821997848));
#166646=CARTESIAN_POINT('Ctrl Pts',(8.09235375840566,-0.75728773762769,
40.5533148350965));
#166647=CARTESIAN_POINT('Ctrl Pts',(8.10851994674541,-0.5580370118204,40.5611474704083));
#166648=CARTESIAN_POINT('Ctrl Pts',(8.11732856393124,-0.358698407699219,
40.56898010572));
#166649=CARTESIAN_POINT('Ctrl Pts',(8.12269567815148,-0.237240858318737,
40.5737525515508));
#166650=CARTESIAN_POINT('Ctrl Pts',(8.12533231449817,-0.115750656374641,
40.5785249973816));
#166651=CARTESIAN_POINT('Ctrl Pts',(8.12524804204743,0.00564071843232957,
40.5832974432124));
#166652=CARTESIAN_POINT('',(8.12839272208226,-0.00745291321414085,42.5832974432124));
#166653=CARTESIAN_POINT('Ctrl Pts',(8.1335321614197,0.00564646944258829,
40.5832974432124));
#166654=CARTESIAN_POINT('Ctrl Pts',(8.13406518936364,0.235442656146337,
40.592322553673));
#166655=CARTESIAN_POINT('Ctrl Pts',(8.01157082498974,3.15609430641961,40.7071259743246));
#166656=CARTESIAN_POINT('Ctrl Pts',(5.36683002199982,7.17838145731516,40.8748185500716));
#166657=CARTESIAN_POINT('Ctrl Pts',(-0.0971997372527671,8.45625233235374,
41.0863751704535));
#166658=CARTESIAN_POINT('Ctrl Pts',(-4.11199154399871,7.40600674809268,
41.2450426357399));
#166659=CARTESIAN_POINT('Ctrl Pts',(-7.16239838942506,4.52625027289421,
41.4037101010264));
#166660=CARTESIAN_POINT('Ctrl Pts',(-8.44679792391067,0.555938847209571,
41.5623775663127));
#166661=CARTESIAN_POINT('Ctrl Pts',(-7.69384797441526,-3.5484638321857,
41.7210450315993));
#166662=CARTESIAN_POINT('Ctrl Pts',(-5.04719085354645,-6.80318123369981,
41.8797124968856));
#166663=CARTESIAN_POINT('Ctrl Pts',(-1.20468243235761,-8.37056697807599,
42.0383799621721));
#166664=CARTESIAN_POINT('Ctrl Pts',(4.37969769530886,-7.8198639968973,42.249936582554));
#166665=CARTESIAN_POINT('Ctrl Pts',(7.7907102434175,-3.87609838062196,42.4315757429007));
#166666=CARTESIAN_POINT('Ctrl Pts',(8.13117600443575,-0.594204244146628,
42.560325748152));
#166667=CARTESIAN_POINT('Ctrl Pts',(8.12839272208226,-0.00745291321414085,
42.5832974432124));
#166668=CARTESIAN_POINT('',(8.12524955251516,0.00269662821826551,44.583297171399));
#166669=CARTESIAN_POINT('Ctrl Pts',(8.12524658453976,-0.00745002852452582,
42.5832974432124));
#166670=CARTESIAN_POINT('Ctrl Pts',(8.125424793707,0.186910761202144,42.5909097800438));
#166671=CARTESIAN_POINT('Ctrl Pts',(8.1186250423802,0.38149919825017,42.5985221168752));
#166672=CARTESIAN_POINT('Ctrl Pts',(8.10482517209636,0.575757320624921,
42.6061344537066));
#166673=CARTESIAN_POINT('Ctrl Pts',(8.0910334440581,0.769900826173182,42.6137422990816));
#166674=CARTESIAN_POINT('Ctrl Pts',(8.07024984038095,0.963714043864039,
42.6213501444566));
#166675=CARTESIAN_POINT('Ctrl Pts',(8.04250426345775,1.15663854974833,42.6289579898316));
#166676=CARTESIAN_POINT('Ctrl Pts',(8.01476867647924,1.34949359212325,42.6365630959608));
#166677=CARTESIAN_POINT('Ctrl Pts',(7.98007615324187,1.54146019994278,42.6441682020901));
#166678=CARTESIAN_POINT('Ctrl Pts',(7.93850849296427,1.73198454659221,42.6517733082193));
#166679=CARTESIAN_POINT('Ctrl Pts',(7.89974440751617,1.90965877709106,42.6588654799188));
#166680=CARTESIAN_POINT('Ctrl Pts',(7.85500184496421,2.08607854171707,42.6659576516182));
#166681=CARTESIAN_POINT('Ctrl Pts',(7.80438735580326,2.26080197343293,42.6730498233177));
#166682=CARTESIAN_POINT('Ctrl Pts',(7.74703340365876,2.45879032631913,42.6810863378217));
#166683=CARTESIAN_POINT('Ctrl Pts',(7.68216389414845,2.65451657047691,42.6891228523257));
#166684=CARTESIAN_POINT('Ctrl Pts',(7.60999333669341,2.84740038947492,42.6971593668296));
#166685=CARTESIAN_POINT('Ctrl Pts',(7.53777918103935,3.04040072949511,42.7052007361881));
#166686=CARTESIAN_POINT('Ctrl Pts',(7.45825528881192,3.23055492283526,42.7132421055467));
#166687=CARTESIAN_POINT('Ctrl Pts',(7.37168408566763,3.417303220906,42.7212834749052));
#166688=CARTESIAN_POINT('Ctrl Pts',(7.28504999994233,3.60418716702778,42.7293306852598));
#166689=CARTESIAN_POINT('Ctrl Pts',(7.19135852319594,3.78765999591063,42.7373778956144));
#166690=CARTESIAN_POINT('Ctrl Pts',(7.09091800857552,3.96718657970096,42.745425105969));
#166691=CARTESIAN_POINT('Ctrl Pts',(6.99032945180891,4.14697777285597,42.7534841773371));
#166692=CARTESIAN_POINT('Ctrl Pts',(6.88297212967956,4.32281081980967,42.7615432487051));
#166693=CARTESIAN_POINT('Ctrl Pts',(6.76919865742865,4.49417813384897,42.7696023200731));
#166694=CARTESIAN_POINT('Ctrl Pts',(6.65533310272477,4.66568414386302,42.777667914043));
#166695=CARTESIAN_POINT('Ctrl Pts',(6.53504121920107,4.83271695246856,42.7857335080129));
#166696=CARTESIAN_POINT('Ctrl Pts',(6.40871644794992,4.99480140268621,42.7937991019827));
#166697=CARTESIAN_POINT('Ctrl Pts',(6.28219331794693,5.15714036252158,42.8018773607779));
#166698=CARTESIAN_POINT('Ctrl Pts',(6.14961856844111,5.31451519149669,42.809955619573));
#166699=CARTESIAN_POINT('Ctrl Pts',(6.01142427219216,5.46648568846558,42.8180338783681));
#166700=CARTESIAN_POINT('Ctrl Pts',(5.93339717518889,5.55229108731696,42.8225950151135));
#166701=CARTESIAN_POINT('Ctrl Pts',(5.85357924497781,5.63637430762845,42.8271561518589));
#166702=CARTESIAN_POINT('Ctrl Pts',(5.77205298301743,5.71866172489155,42.8317172886043));
#166703=CARTESIAN_POINT('Ctrl Pts',(5.62751946306841,5.86454465609143,42.8398034823403));
#166704=CARTESIAN_POINT('Ctrl Pts',(5.47733352188085,6.00506501671852,42.8478896760762));
#166705=CARTESIAN_POINT('Ctrl Pts',(5.32191951398793,6.13977688919837,42.8559758698122));
#166706=CARTESIAN_POINT('Ctrl Pts',(5.16664412801486,6.27436860508074,42.8640548510471));
#166707=CARTESIAN_POINT('Ctrl Pts',(5.00615021152948,6.40316195653402,42.872133832282));
#166708=CARTESIAN_POINT('Ctrl Pts',(4.84089867607219,6.52574804681444,42.8802128135169));
#166709=CARTESIAN_POINT('Ctrl Pts',(4.6757719711654,6.64824153590304,42.8882856919118));
#166710=CARTESIAN_POINT('Ctrl Pts',(4.50589506732835,6.7645369259048,42.8963585703067));
#166711=CARTESIAN_POINT('Ctrl Pts',(4.33176211900848,6.87426537942951,42.9044314487016));
#166712=CARTESIAN_POINT('Ctrl Pts',(4.15773696676393,6.98392590613879,42.9124993296241));
#166713=CARTESIAN_POINT('Ctrl Pts',(3.97946129164463,7.08702743509267,42.9205672105466));
#166714=CARTESIAN_POINT('Ctrl Pts',(3.79745892349286,7.18324392505812,42.9286350914691));
#166715=CARTESIAN_POINT('Ctrl Pts',(3.61554443704029,7.27941395591035,42.936699076733));
#166716=CARTESIAN_POINT('Ctrl Pts',(3.42990712615521,7.36870543069015,42.944763061997));
#166717=CARTESIAN_POINT('Ctrl Pts',(3.24109670272519,7.45083751843267,42.9528270472609));
#166718=CARTESIAN_POINT('Ctrl Pts',(3.04966241917648,7.5341109791226,42.9610030960907));
#166719=CARTESIAN_POINT('Ctrl Pts',(2.85496646216837,7.61002442414159,42.9691791449206));
#166720=CARTESIAN_POINT('Ctrl Pts',(2.65760536674899,7.67833453797938,42.9773551937504));
#166721=CARTESIAN_POINT('Ctrl Pts',(2.46304159177226,7.74567645047297,42.9854153584012));
#166722=CARTESIAN_POINT('Ctrl Pts',(2.26588803830114,7.80562904084697,42.9934755230519));
#166723=CARTESIAN_POINT('Ctrl Pts',(2.06673442137547,7.85800842414933,43.0015356877026));
#166724=CARTESIAN_POINT('Ctrl Pts',(1.86759042655388,7.91038527674255,43.0095954629266));
#166725=CARTESIAN_POINT('Ctrl Pts',(1.66644686737592,7.9551895715948,43.0176552381506));
#166726=CARTESIAN_POINT('Ctrl Pts',(1.46390689294527,7.99228779332222,43.0257150133746));
#166727=CARTESIAN_POINT('Ctrl Pts',(1.26135162649032,8.02938881601231,43.0337753971218));
#166728=CARTESIAN_POINT('Ctrl Pts',(1.05740004618877,8.05878254864867,43.0418357808691));
#166729=CARTESIAN_POINT('Ctrl Pts',(0.852664321026222,8.08038681735899,
43.0498961646163));
#166730=CARTESIAN_POINT('Ctrl Pts',(0.642781977833522,8.10253417115514,
43.058159169163));
#166731=CARTESIAN_POINT('Ctrl Pts',(0.432075896998746,8.11649526279491,
43.0664221737098));
#166732=CARTESIAN_POINT('Ctrl Pts',(0.221210092009776,8.12223821724609,
43.0746851782565));
#166733=CARTESIAN_POINT('Ctrl Pts',(0.0153458712982696,8.12784495297424,
43.0827521903159));
#166734=CARTESIAN_POINT('Ctrl Pts',(-0.19067026004267,8.12561900844492,
43.0908192023752));
#166735=CARTESIAN_POINT('Ctrl Pts',(-0.396221094634212,8.11558355305808,
43.0988862144346));
#166736=CARTESIAN_POINT('Ctrl Pts',(-0.609262884810202,8.10518237232296,
43.107247215225));
#166737=CARTESIAN_POINT('Ctrl Pts',(-0.821804453695356,8.0863918022516,
43.1156082160154));
#166738=CARTESIAN_POINT('Ctrl Pts',(-1.03316484413242,8.05929636924644,
43.1239692168059));
#166739=CARTESIAN_POINT('Ctrl Pts',(-1.24452523456955,8.03220093624127,
43.1323302175963));
#166740=CARTESIAN_POINT('Ctrl Pts',(-1.45470407869705,7.99680072666137,
43.1406912183867));
#166741=CARTESIAN_POINT('Ctrl Pts',(-1.6630322704497,7.95323904016112,43.1490522191772));
#166742=CARTESIAN_POINT('Ctrl Pts',(-1.85185679999638,7.91375559391954,
43.156630464001));
#166743=CARTESIAN_POINT('Ctrl Pts',(-2.03953933790646,7.86748795352796,
43.1642087088247));
#166744=CARTESIAN_POINT('Ctrl Pts',(-2.22553394789696,7.81451765685242,
43.1717869536485));
#166745=CARTESIAN_POINT('Ctrl Pts',(-2.41139015440928,7.76158677676696,
43.1793595593011));
#166746=CARTESIAN_POINT('Ctrl Pts',(-2.59556058061479,7.70196326254506,
43.1869321649537));
#166747=CARTESIAN_POINT('Ctrl Pts',(-2.77750843885825,7.63577988384757,
43.1945047706063));
#166748=CARTESIAN_POINT('Ctrl Pts',(-2.95935545632893,7.56963318589541,
43.2020731793015));
#166749=CARTESIAN_POINT('Ctrl Pts',(-3.13898201277821,7.49693398313537,
43.2096415879967));
#166750=CARTESIAN_POINT('Ctrl Pts',(-3.31586553502567,7.41786514545317,
43.2172099966919));
#166751=CARTESIAN_POINT('Ctrl Pts',(-3.49270632080368,7.33881541143265,
43.2247765767993));
#166752=CARTESIAN_POINT('Ctrl Pts',(-3.66680505310869,7.2533992480984,43.2323431569066));
#166753=CARTESIAN_POINT('Ctrl Pts',(-3.83765811512838,7.16184806833329,
43.2399097370139));
#166754=CARTESIAN_POINT('Ctrl Pts',(-4.00848086858873,7.07031312933279,
43.2474749748442));
#166755=CARTESIAN_POINT('Ctrl Pts',(-4.17605877515832,6.97264551658212,
43.2550402126745));
#166756=CARTESIAN_POINT('Ctrl Pts',(-4.33991210770841,6.86912297603311,
43.2626054505048));
#166757=CARTESIAN_POINT('Ctrl Pts',(-4.50382241992725,6.76556443572763,
43.2701733191314));
#166758=CARTESIAN_POINT('Ctrl Pts',(-4.66400525755614,6.65614709391517,
43.277741187758));
#166759=CARTESIAN_POINT('Ctrl Pts',(-4.82000882456867,6.54119274242703,
43.2853090563847));
#166760=CARTESIAN_POINT('Ctrl Pts',(-4.97399924960415,6.42772181490706,
43.2927792657442));
#166761=CARTESIAN_POINT('Ctrl Pts',(-5.12391736857331,6.30885616908336,
43.3002494751038));
#166762=CARTESIAN_POINT('Ctrl Pts',(-5.26936004855676,6.18494399660772,
43.3077196844634));
#166763=CARTESIAN_POINT('Ctrl Pts',(-5.4505419208893,6.0305832586422,43.3170255259031));
#166764=CARTESIAN_POINT('Ctrl Pts',(-5.6246911036513,5.86846861385627,43.3263313673427));
#166765=CARTESIAN_POINT('Ctrl Pts',(-5.79124916197024,5.69922106138014,
43.3356372087824));
#166766=CARTESIAN_POINT('Ctrl Pts',(-5.95870143688861,5.52906485295327,
43.3449930114066));
#166767=CARTESIAN_POINT('Ctrl Pts',(-6.11848086444778,5.35169901118755,
43.3543488140308));
#166768=CARTESIAN_POINT('Ctrl Pts',(-6.27006456547053,5.16778268770377,
43.363704616655));
#166769=CARTESIAN_POINT('Ctrl Pts',(-6.42238412276047,4.9829735506895,43.3731058366027));
#166770=CARTESIAN_POINT('Ctrl Pts',(-6.56642818044302,4.79155022730358,
43.3825070565505));
#166771=CARTESIAN_POINT('Ctrl Pts',(-6.70171112354593,4.59420891765283,
43.3919082764983));
#166772=CARTESIAN_POINT('Ctrl Pts',(-6.83714048293256,4.39665402615264,
43.4013196713554));
#166773=CARTESIAN_POINT('Ctrl Pts',(-6.96378974949471,4.19316837376188,
43.4107310662125));
#166774=CARTESIAN_POINT('Ctrl Pts',(-7.08121667856289,3.98447711923945,
43.4201424610697));
#166775=CARTESIAN_POINT('Ctrl Pts',(-7.19850586387032,3.77603066306491,
43.4295428162025));
#166776=CARTESIAN_POINT('Ctrl Pts',(-7.30659432077361,3.5623908439446,43.4389431713354));
#166777=CARTESIAN_POINT('Ctrl Pts',(-7.40508628375777,3.34430630962574,
43.4483435264682));
#166778=CARTESIAN_POINT('Ctrl Pts',(-7.46810347304673,3.20477132663045,
43.4543580675621));
#166779=CARTESIAN_POINT('Ctrl Pts',(-7.52719304454957,3.06341733066499,
43.4603726086561));
#166780=CARTESIAN_POINT('Ctrl Pts',(-7.58226108188434,2.92044593318249,
43.46638714975));
#166781=CARTESIAN_POINT('Ctrl Pts',(-7.65314815031847,2.73640408734998,
43.4741294483094));
#166782=CARTESIAN_POINT('Ctrl Pts',(-7.71740173389768,2.54959454654449,
43.4818717468688));
#166783=CARTESIAN_POINT('Ctrl Pts',(-7.77480000416057,2.36054494932947,
43.4896140454281));
#166784=CARTESIAN_POINT('Ctrl Pts',(-7.83216252049865,2.17161311289453,
43.4973515212366));
#166785=CARTESIAN_POINT('Ctrl Pts',(-7.88267812383826,1.98044433497426,
43.5050889970451));
#166786=CARTESIAN_POINT('Ctrl Pts',(-7.92617358399279,1.7875849291474,43.5128264728536));
#166787=CARTESIAN_POINT('Ctrl Pts',(-7.96964968080811,1.59481138060497,
43.5205605040872));
#166788=CARTESIAN_POINT('Ctrl Pts',(-8.00611178113934,1.40034904700722,
43.5282945353208));
#166789=CARTESIAN_POINT('Ctrl Pts',(-8.03543684367452,1.20475818894004,
43.5360285665544));
#166790=CARTESIAN_POINT('Ctrl Pts',(-8.06475815352443,1.00919236034829,
43.5437616080753));
#166791=CARTESIAN_POINT('Ctrl Pts',(-8.08694418480647,0.812498642957925,
43.5514946495963));
#166792=CARTESIAN_POINT('Ctrl Pts',(-8.10192317652025,0.615246620684689,
43.5592276911173));
#166793=CARTESIAN_POINT('Ctrl Pts',(-8.11690067184377,0.418014303743525,
43.5669599601131));
#166794=CARTESIAN_POINT('Ctrl Pts',(-8.12467253855411,0.220224145668624,
43.5746922291089));
#166795=CARTESIAN_POINT('Ctrl Pts',(-8.12521898577066,0.0224498501542118,
43.5824244981047));
#166796=CARTESIAN_POINT('Ctrl Pts',(-8.12576564318059,-0.175400520128988,
43.5901597413524));
#166797=CARTESIAN_POINT('Ctrl Pts',(-8.11908132728276,-0.373234661977047,
43.5978949846001));
#166798=CARTESIAN_POINT('Ctrl Pts',(-8.10519839534709,-0.570479214838729,
43.6056302278478));
#166799=CARTESIAN_POINT('Ctrl Pts',(-8.09357766856049,-0.735583032214666,
43.6121050235773));
#166800=CARTESIAN_POINT('Ctrl Pts',(-8.0769141260109,-0.900273666263304,
43.6185798193067));
#166801=CARTESIAN_POINT('Ctrl Pts',(-8.05525464508299,-1.06421810047043,
43.6250546150362));
#166802=CARTESIAN_POINT('Ctrl Pts',(-8.02710789116816,-1.27726584896878,
43.6334686893463));
#166803=CARTESIAN_POINT('Ctrl Pts',(-7.9905100417965,-1.48915602392358,
43.6418827636564));
#166804=CARTESIAN_POINT('Ctrl Pts',(-7.94558428195602,-1.69922864289459,
43.6502968379666));
#166805=CARTESIAN_POINT('Ctrl Pts',(-7.90064597559849,-1.909359929314,43.658713262094));
#166806=CARTESIAN_POINT('Ctrl Pts',(-7.84737517101555,-2.11767238822419,
43.6671296862214));
#166807=CARTESIAN_POINT('Ctrl Pts',(-7.78594586514241,-2.32351770976074,
43.6755461103488));
#166808=CARTESIAN_POINT('Ctrl Pts',(-7.72450132523735,-2.52941407947623,
43.6839646216896));
#166809=CARTESIAN_POINT('Ctrl Pts',(-7.65489432029978,-2.73284183743178,
43.6923831330305));
#166810=CARTESIAN_POINT('Ctrl Pts',(-7.57734859494423,-2.93316822449663,
43.7008016443713));
#166811=CARTESIAN_POINT('Ctrl Pts',(-7.49977308459219,-3.13357155610882,
43.709223389228));
#166812=CARTESIAN_POINT('Ctrl Pts',(-7.41425285454955,-3.33087088965249,
43.7176451340847));
#166813=CARTESIAN_POINT('Ctrl Pts',(-7.32106018105627,-3.52445249476458,
43.7260668789414));
#166814=CARTESIAN_POINT('Ctrl Pts',(-7.22785740571858,-3.71805508362124,
43.7344895366934));
#166815=CARTESIAN_POINT('Ctrl Pts',(-7.12698064362,-3.90793890291983,43.7429121944454));
#166816=CARTESIAN_POINT('Ctrl Pts',(-7.01874887651428,-4.09351337739717,
43.7513348521975));
#166817=CARTESIAN_POINT('Ctrl Pts',(-6.91049652679755,-4.27912314287384,
43.7597591117));
#166818=CARTESIAN_POINT('Ctrl Pts',(-6.79488651080306,-4.46042169837938,
43.7681833712025));
#166819=CARTESIAN_POINT('Ctrl Pts',(-6.67228270029433,-4.6368449542607,
43.776607630705));
#166820=CARTESIAN_POINT('Ctrl Pts',(-6.63776893946875,-4.68650923494083,
43.778979113911));
#166821=CARTESIAN_POINT('Ctrl Pts',(-6.60270121405478,-4.73578734269762,
43.7813505971169));
#166822=CARTESIAN_POINT('Ctrl Pts',(-6.56708825637221,-4.78466711438927,
43.7837220803228));
#166823=CARTESIAN_POINT('Ctrl Pts',(-6.4405787570321,-4.95830490936511,
43.7921464059783));
#166824=CARTESIAN_POINT('Ctrl Pts',(-6.30717262978249,-5.12693156576806,
43.8005707316338));
#166825=CARTESIAN_POINT('Ctrl Pts',(-6.16728380939353,-5.29001871233859,
43.8089950572893));
#166826=CARTESIAN_POINT('Ctrl Pts',(-6.02741916346917,-5.45307767549574,
43.8174179271204));
#166827=CARTESIAN_POINT('Ctrl Pts',(-5.88107423370648,-5.61059884060153,
43.8258407969515));
#166828=CARTESIAN_POINT('Ctrl Pts',(-5.72870267265477,-5.76208757750332,
43.8342636667826));
#166829=CARTESIAN_POINT('Ctrl Pts',(-5.57636224899295,-5.91354535742186,
43.8426848153857));
#166830=CARTESIAN_POINT('Ctrl Pts',(-5.41799784042819,-6.05897298485688,
43.8511059639889));
#166831=CARTESIAN_POINT('Ctrl Pts',(-5.25410009696062,-6.19791253032974,
43.8595271125921));
#166832=CARTESIAN_POINT('Ctrl Pts',(-5.09024833777183,-6.3368130939676,
43.8679458984999));
#166833=CARTESIAN_POINT('Ctrl Pts',(-4.92086654555653,-6.46922904080733,
43.8763646844076));
#166834=CARTESIAN_POINT('Ctrl Pts',(-4.7464793583057,-6.59474194064316,
43.8847834703154));
#166835=CARTESIAN_POINT('Ctrl Pts',(-4.57214088504883,-6.72021977921823,
43.8931999044868));
#166836=CARTESIAN_POINT('Ctrl Pts',(-4.39280002251156,-6.83879826683661,
43.9016163386583));
#166837=CARTESIAN_POINT('Ctrl Pts',(-4.20901230268642,-6.95010093439904,
43.9100327728297));
#166838=CARTESIAN_POINT('Ctrl Pts',(-4.02529128734135,-7.0613632054291,
43.9184461523147));
#166839=CARTESIAN_POINT('Ctrl Pts',(-3.83712686331025,-7.1653547932383,
43.9268595317996));
#166840=CARTESIAN_POINT('Ctrl Pts',(-3.64510204044308,-7.26174350120256,
43.9352729112845));
#166841=CARTESIAN_POINT('Ctrl Pts',(-3.59095929284808,-7.28892097445001,
43.9376451227261));
#166842=CARTESIAN_POINT('Ctrl Pts',(-3.53650980442697,-7.31549429527996,
43.9400173341677));
#166843=CARTESIAN_POINT('Ctrl Pts',(-3.48176700930949,-7.34145667121887,
43.9423895456093));
#166844=CARTESIAN_POINT('Ctrl Pts',(-3.3032645331394,-7.42611344445103,
43.950124730037));
#166845=CARTESIAN_POINT('Ctrl Pts',(-3.12156246520276,-7.50430829972414,
43.9578599144647));
#166846=CARTESIAN_POINT('Ctrl Pts',(-2.93717868219316,-7.57579493857708,
43.9655950988925));
#166847=CARTESIAN_POINT('Ctrl Pts',(-2.7528519152153,-7.647259471991,43.9733278914096));
#166848=CARTESIAN_POINT('Ctrl Pts',(-2.56584541356301,-7.71201979231342,
43.9810606839267));
#166849=CARTESIAN_POINT('Ctrl Pts',(-2.37669761634251,-7.76987747670269,
43.9887934764439));
#166850=CARTESIAN_POINT('Ctrl Pts',(-2.18757470220896,-7.82772754970123,
43.9965252516837));
#166851=CARTESIAN_POINT('Ctrl Pts',(-1.99631139158246,-7.87867669292311,
44.0042570269237));
#166852=CARTESIAN_POINT('Ctrl Pts',(-1.80346201542789,-7.92257611647933,
44.0119888021636));
#166853=CARTESIAN_POINT('Ctrl Pts',(-1.61054363246769,-7.96649124845551,
44.0197233440451));
#166854=CARTESIAN_POINT('Ctrl Pts',(-1.41603839399175,-8.00335153823512,
44.0274578859266));
#166855=CARTESIAN_POINT('Ctrl Pts',(-1.22051223209202,-8.0330590346277,
44.0351924278081));
#166856=CARTESIAN_POINT('Ctrl Pts',(-1.02495304799253,-8.06277154828688,
44.042928275968));
#166857=CARTESIAN_POINT('Ctrl Pts',(-0.828372947453864,-8.08532881595842,
44.0506641241278));
#166858=CARTESIAN_POINT('Ctrl Pts',(-0.631343921841026,-8.10068468802819,
44.0583999722877));
#166859=CARTESIAN_POINT('Ctrl Pts',(-0.434153678079574,-8.11605312497391,
44.0661421502718));
#166860=CARTESIAN_POINT('Ctrl Pts',(-0.23651412839142,-8.12420837346987,
44.073884328256));
#166861=CARTESIAN_POINT('Ctrl Pts',(-0.038999148654981,-8.12515640642715,
44.0816265062402));
#166862=CARTESIAN_POINT('Ctrl Pts',(0.126234964240147,-8.12594949758864,
44.0881033411253));
#166863=CARTESIAN_POINT('Ctrl Pts',(0.291381787375085,-8.12169961560909,
44.0945801760104));
#166864=CARTESIAN_POINT('Ctrl Pts',(0.456107788770162,-8.11243818143,44.1010570108955));
#166865=CARTESIAN_POINT('Ctrl Pts',(0.695128841881753,-8.09899963662188,
44.1104550408481));
#166866=CARTESIAN_POINT('Ctrl Pts',(0.933399685667861,-8.07500195327902,
44.1198530708006));
#166867=CARTESIAN_POINT('Ctrl Pts',(1.17008024090096,-8.04055966909973,
44.1292511007531));
#166868=CARTESIAN_POINT('Ctrl Pts',(1.4070975736774,-8.00606837629849,44.1386625033523));
#166869=CARTESIAN_POINT('Ctrl Pts',(1.64252005459376,-7.96110275970635,
44.1480739059515));
#166870=CARTESIAN_POINT('Ctrl Pts',(1.87551474980376,-7.90582898789042,
44.1574853085507));
#166871=CARTESIAN_POINT('Ctrl Pts',(2.10815863109604,-7.8506384403231,44.1668825406513));
#166872=CARTESIAN_POINT('Ctrl Pts',(2.33838199799642,-7.78517076979389,
44.1762797727518));
#166873=CARTESIAN_POINT('Ctrl Pts',(2.56536686952964,-7.70964204014815,
44.1856770048524));
#166874=CARTESIAN_POINT('Ctrl Pts',(2.79177919885259,-7.6343038226961,44.1950505335581));
#166875=CARTESIAN_POINT('Ctrl Pts',(3.01496930701531,-7.54895522985642,
44.2044240622637));
#166876=CARTESIAN_POINT('Ctrl Pts',(3.23413710097516,-7.45386106488416,
44.2137975909694));
#166877=CARTESIAN_POINT('Ctrl Pts',(3.45188162845257,-7.35938443743981,
44.2231102483719));
#166878=CARTESIAN_POINT('Ctrl Pts',(3.66565586421285,-7.25528839971713,
44.2324229057745));
#166879=CARTESIAN_POINT('Ctrl Pts',(3.87468744798139,-7.14188243693184,
44.241735563177));
#166880=CARTESIAN_POINT('Ctrl Pts',(4.0092802862809,-7.06886174725337,44.247731867512));
#166881=CARTESIAN_POINT('Ctrl Pts',(4.14190711030131,-6.99198224877317,
44.2537281718471));
#166882=CARTESIAN_POINT('Ctrl Pts',(4.27236462532949,-6.91133764699231,
44.2597244761822));
#166883=CARTESIAN_POINT('Ctrl Pts',(4.43700901099099,-6.80955983132367,
44.2672921340766));
#166884=CARTESIAN_POINT('Ctrl Pts',(4.59813116368294,-6.7018227134163,44.2748597919709));
#166885=CARTESIAN_POINT('Ctrl Pts',(4.75525822826502,-6.58841458508933,
44.2824274498653));
#166886=CARTESIAN_POINT('Ctrl Pts',(4.91234178719294,-6.4750378574305,44.2899930124115));
#166887=CARTESIAN_POINT('Ctrl Pts',(5.06543216120311,-6.35599345862215,
44.2975585749578));
#166888=CARTESIAN_POINT('Ctrl Pts',(5.21408537593068,-6.23161305401786,
44.305124137504));
#166889=CARTESIAN_POINT('Ctrl Pts',(5.36272556724018,-6.10724354630546,
44.3126890372359));
#166890=CARTESIAN_POINT('Ctrl Pts',(5.5069290915758,-5.9775391998602,44.3202539369678));
#166891=CARTESIAN_POINT('Ctrl Pts',(5.64628503765839,-5.84287196813476,
44.3278188366996));
#166892=CARTESIAN_POINT('Ctrl Pts',(5.78570937880555,-5.7081386425377,44.335387449239));
#166893=CARTESIAN_POINT('Ctrl Pts',(5.92028112157277,-5.56843781904027,
44.3429560617784));
#166894=CARTESIAN_POINT('Ctrl Pts',(6.04962583290827,-5.42417872532874,
44.3505246743178));
#166895=CARTESIAN_POINT('Ctrl Pts',(6.17899930824242,-5.27988755092111,
44.3580949699841));
#166896=CARTESIAN_POINT('Ctrl Pts',(6.30314319972982,-5.13103636841071,
44.3656652656504));
#166897=CARTESIAN_POINT('Ctrl Pts',(6.42172357771468,-4.97806728097595,
44.3732355613167));
#166898=CARTESIAN_POINT('Ctrl Pts',(6.54042411146642,-4.82494319219679,
44.3808135278531));
#166899=CARTESIAN_POINT('Ctrl Pts',(6.65354965238771,-4.6676931595859,44.3883914943895));
#166900=CARTESIAN_POINT('Ctrl Pts',(6.76080929604574,-4.5067887930323,44.3959694609259));
#166901=CARTESIAN_POINT('Ctrl Pts',(6.86659964940591,-4.34808856604691,
44.4034436211068));
#166902=CARTESIAN_POINT('Ctrl Pts',(6.9666836684079,-4.1858338068307,44.4109177812876));
#166903=CARTESIAN_POINT('Ctrl Pts',(7.06082668873177,-4.02049922698577,
44.4183919414685));
#166904=CARTESIAN_POINT('Ctrl Pts',(7.16778999590138,-3.8326495766466,44.4268839240765));
#166905=CARTESIAN_POINT('Ctrl Pts',(7.26728547124287,-3.64047231742024,
44.4353759066845));
#166906=CARTESIAN_POINT('Ctrl Pts',(7.35898571646831,-3.44456336671506,
44.4438678892926));
#166907=CARTESIAN_POINT('Ctrl Pts',(7.45061782538993,-3.24879998281566,
44.4523535620777));
#166908=CARTESIAN_POINT('Ctrl Pts',(7.53446616010904,-3.04931067214259,
44.4608392348629));
#166909=CARTESIAN_POINT('Ctrl Pts',(7.61024988985641,-2.84671462855703,
44.469324907648));
#166910=CARTESIAN_POINT('Ctrl Pts',(7.68597193347051,-2.6442834932781,44.4778036732996));
#166911=CARTESIAN_POINT('Ctrl Pts',(7.7536423872849,-2.43875091019721,44.4862824389512));
#166912=CARTESIAN_POINT('Ctrl Pts',(7.81302862644311,-2.23075575643781,
44.4947612046028));
#166913=CARTESIAN_POINT('Ctrl Pts',(7.87233923567211,-2.02302548994825,
44.5032291723245));
#166914=CARTESIAN_POINT('Ctrl Pts',(7.92338662845627,-1.8128391587275,44.5116971400462));
#166915=CARTESIAN_POINT('Ctrl Pts',(7.9659879565569,-1.60085084829613,44.5201651077679));
#166916=CARTESIAN_POINT('Ctrl Pts',(8.0085517595314,-1.38904926650542,44.5286256165307));
#166917=CARTESIAN_POINT('Ctrl Pts',(8.04268429491224,-1.17544912102911,
44.5370861252935));
#166918=CARTESIAN_POINT('Ctrl Pts',(8.06825326753697,-0.960716801861529,
44.5455466340563));
#166919=CARTESIAN_POINT('Ctrl Pts',(8.09378829972018,-0.746269519946942,
44.5539959122778));
#166920=CARTESIAN_POINT('Ctrl Pts',(8.11078243346433,-0.530693315926462,
44.5624451904993));
#166921=CARTESIAN_POINT('Ctrl Pts',(8.1191548345446,-0.314662255745863,
44.5708944687207));
#166922=CARTESIAN_POINT('Ctrl Pts',(8.12325136298361,-0.208960513407529,
44.5750286123423));
#166923=CARTESIAN_POINT('Ctrl Pts',(8.12528459051782,-0.103150010145808,
44.5791627559639));
#166924=CARTESIAN_POINT('Ctrl Pts',(8.12524955482466,0.00268966942621325,
44.5832968995855));
#166925=CARTESIAN_POINT('',(8.12524981409313,0.00169347021508326,46.5833637857063));
#166926=CARTESIAN_POINT('Ctrl Pts',(8.12524955020566,0.00270358701031778,
44.5832974432124));
#166927=CARTESIAN_POINT('Ctrl Pts',(8.1251775121146,0.219203912218492,44.5917540392692));
#166928=CARTESIAN_POINT('Ctrl Pts',(8.11644813158616,0.435525939744223,
44.600210635326));
#166929=CARTESIAN_POINT('Ctrl Pts',(8.0991293976781,0.65099198318127,44.6086672313829));
#166930=CARTESIAN_POINT('Ctrl Pts',(8.08178443997324,0.866784282438916,
44.6171366323051));
#166931=CARTESIAN_POINT('Ctrl Pts',(8.0558241595595,1.08171775676946,44.6256060332273));
#166932=CARTESIAN_POINT('Ctrl Pts',(8.02136810729963,1.2951220983739,44.6340754341495));
#166933=CARTESIAN_POINT('Ctrl Pts',(7.98683179491984,1.50902353285235,44.6425645632498));
#166934=CARTESIAN_POINT('Ctrl Pts',(7.94376015720404,1.72138845859037,44.6510536923501));
#166935=CARTESIAN_POINT('Ctrl Pts',(7.89232403806732,1.93155606717607,44.6595428214504));
#166936=CARTESIAN_POINT('Ctrl Pts',(7.84083155612169,2.14195397378895,44.6680412527913));
#166937=CARTESIAN_POINT('Ctrl Pts',(7.78095634937928,2.35014951053943,44.6765396841323));
#166938=CARTESIAN_POINT('Ctrl Pts',(7.7129190397752,2.55549749527821,44.6850381154733));
#166939=CARTESIAN_POINT('Ctrl Pts',(7.64475713806993,2.76122151982578,44.693552109414));
#166940=CARTESIAN_POINT('Ctrl Pts',(7.56840332027205,2.96408732389021,44.7020661033548));
#166941=CARTESIAN_POINT('Ctrl Pts',(7.48412725595363,3.16346752459892,44.7105800972955));
#166942=CARTESIAN_POINT('Ctrl Pts',(7.40115518195288,3.359762746751,44.7189623555441));
#166943=CARTESIAN_POINT('Ctrl Pts',(7.31050436684576,3.55267925432863,44.7273446137927));
#166944=CARTESIAN_POINT('Ctrl Pts',(7.21247566442981,3.74164166543347,44.7357268720413));
#166945=CARTESIAN_POINT('Ctrl Pts',(7.11800573674497,3.92374409943778,44.7438048258555));
#166946=CARTESIAN_POINT('Ctrl Pts',(7.01652922040552,4.10247129525327,44.7518827796697));
#166947=CARTESIAN_POINT('Ctrl Pts',(6.90830553088348,4.27726574513027,44.7599607334839));
#166948=CARTESIAN_POINT('Ctrl Pts',(6.80021428578587,4.45184628111825,44.7680288014778));
#166949=CARTESIAN_POINT('Ctrl Pts',(6.68539249179063,4.62250339863331,44.7760968694717));
#166950=CARTESIAN_POINT('Ctrl Pts',(6.56414612554026,4.78870266408918,44.7841649374656));
#166951=CARTESIAN_POINT('Ctrl Pts',(6.44303321409428,4.95471899548157,44.7922241250084));
#166952=CARTESIAN_POINT('Ctrl Pts',(6.31551001255445,5.11628700299728,44.8002833125511));
#166953=CARTESIAN_POINT('Ctrl Pts',(6.18192692576556,5.27289930180681,44.8083425000938));
#166954=CARTESIAN_POINT('Ctrl Pts',(6.04851542357616,5.42931043548973,44.8163913357837));
#166955=CARTESIAN_POINT('Ctrl Pts',(5.90905976844119,5.5807783203165,44.8244401714735));
#166956=CARTESIAN_POINT('Ctrl Pts',(5.76395194930333,5.72682682544376,44.8324890071633));
#166957=CARTESIAN_POINT('Ctrl Pts',(5.61895389027642,5.8727648589216,44.8405317546829));
#166958=CARTESIAN_POINT('Ctrl Pts',(5.4683124106001,6.01329146051201,44.8485745022026));
#166959=CARTESIAN_POINT('Ctrl Pts',(5.31245873268391,6.14796468565252,44.8566172497222));
#166960=CARTESIAN_POINT('Ctrl Pts',(5.15673200583406,6.28252821232606,44.8646534459985));
#166961=CARTESIAN_POINT('Ctrl Pts',(4.99580178793621,6.41124766756013,44.8726896422747));
#166962=CARTESIAN_POINT('Ctrl Pts',(4.8301352056564,6.53371880766066,44.880725838551));
#166963=CARTESIAN_POINT('Ctrl Pts',(4.73620961368876,6.60315450298674,44.8852820048099));
#166964=CARTESIAN_POINT('Ctrl Pts',(4.64076222582698,6.67058243382526,44.8898381710689));
#166965=CARTESIAN_POINT('Ctrl Pts',(4.54388303022122,6.73593457288353,44.8943943373278));
#166966=CARTESIAN_POINT('Ctrl Pts',(4.37300026917792,6.85120755685635,44.9024308436719));
#166967=CARTESIAN_POINT('Ctrl Pts',(4.19779623704759,6.9599286625938,44.910467350016));
#166968=CARTESIAN_POINT('Ctrl Pts',(4.01880742894209,7.06178974563672,44.9185038563602));
#166969=CARTESIAN_POINT('Ctrl Pts',(3.83971049624867,7.16371236150811,44.9265452174432));
#166970=CARTESIAN_POINT('Ctrl Pts',(3.65682450071894,7.25876653088662,44.9345865785263));
#166971=CARTESIAN_POINT('Ctrl Pts',(3.47070955099071,7.34669060020645,44.9426279396094));
#166972=CARTESIAN_POINT('Ctrl Pts',(3.2844594154123,7.43467853376761,44.9506751415893));
#166973=CARTESIAN_POINT('Ctrl Pts',(3.09497593164756,7.51552589990583,44.9587223435693));
#166974=CARTESIAN_POINT('Ctrl Pts',(2.90283869828506,7.58901937368977,44.9667695455493));
#166975=CARTESIAN_POINT('Ctrl Pts',(2.71041827043903,7.66262117081108,44.9748286084433));
#166976=CARTESIAN_POINT('Ctrl Pts',(2.51533657074099,7.72884729907743,44.9828876713373));
#166977=CARTESIAN_POINT('Ctrl Pts',(2.3181895379757,7.78753393755173,44.9909467342313));
#166978=CARTESIAN_POINT('Ctrl Pts',(2.12088294562527,7.8462680736503,44.999012319672));
#166979=CARTESIAN_POINT('Ctrl Pts',(1.92150798975258,7.89745046444227,45.0070779051127));
#166980=CARTESIAN_POINT('Ctrl Pts',(1.72067117894991,7.94096834500876,45.0151434905535));
#166981=CARTESIAN_POINT('Ctrl Pts',(1.51951900875534,7.98455455852824,45.0232217407946));
#166982=CARTESIAN_POINT('Ctrl Pts',(1.31690070611728,8.02045215062923,45.0312999910357));
#166983=CARTESIAN_POINT('Ctrl Pts',(1.11343004629675,8.04859994623311,45.0393782412769));
#166984=CARTESIAN_POINT('Ctrl Pts',(0.998545297293156,8.06449291299209,
45.0439394283893));
#166985=CARTESIAN_POINT('Ctrl Pts',(0.883388868159684,8.07791617415651,
45.0485006155018));
#166986=CARTESIAN_POINT('Ctrl Pts',(0.768071277691702,8.08886605618396,
45.0530618026143));
#166987=CARTESIAN_POINT('Ctrl Pts',(0.563633125916835,8.10827830400114,
45.0611479988259));
#166988=CARTESIAN_POINT('Ctrl Pts',(0.358290620238147,8.11995173760702,
45.0692341950375));
#166989=CARTESIAN_POINT('Ctrl Pts',(0.152655273641481,8.12381584785927,
45.0773203912491));
#166990=CARTESIAN_POINT('Ctrl Pts',(-0.0527966563140229,8.12767651151474,
45.0853993749704));
#166991=CARTESIAN_POINT('Ctrl Pts',(-0.25854059115977,8.12374173451219,
45.0934783586916));
#166992=CARTESIAN_POINT('Ctrl Pts',(-0.463960667191387,8.1119928539046,
45.1015573424129));
#166993=CARTESIAN_POINT('Ctrl Pts',(-0.669225569659059,8.10025284835787,
45.1096302232998));
#166994=CARTESIAN_POINT('Ctrl Pts',(-0.874166786002571,8.08071052779534,
45.1177031041867));
#166995=CARTESIAN_POINT('Ctrl Pts',(-1.07816859310736,8.05339928522961,
45.1257759850737));
#166996=CARTESIAN_POINT('Ctrl Pts',(-1.28204411402979,8.02610494953647,
45.1338438684886));
#166997=CARTESIAN_POINT('Ctrl Pts',(-1.48498107227109,7.99105132484738,
45.1419117519036));
#166998=CARTESIAN_POINT('Ctrl Pts',(-1.68636837788461,7.94832367588102,
45.1499796353186));
#166999=CARTESIAN_POINT('Ctrl Pts',(-1.88765844149699,7.90561665841414,
45.1580436230703));
#167000=CARTESIAN_POINT('Ctrl Pts',(-2.08740003554838,7.85524307286104,
45.166107610822));
#167001=CARTESIAN_POINT('Ctrl Pts',(-2.28499116249876,7.79733947893783,
45.1741715985737));
#167002=CARTESIAN_POINT('Ctrl Pts',(-2.48532807333227,7.73863123979891,
45.1823476458493));
#167003=CARTESIAN_POINT('Ctrl Pts',(-2.68345398019448,7.67218221586229,
45.1905236931249));
#167004=CARTESIAN_POINT('Ctrl Pts',(-2.87875497010913,7.59818776976273,
45.1986997404004));
#167005=CARTESIAN_POINT('Ctrl Pts',(-3.0712879338831,7.52524205649939,45.2067599075025));
#167006=CARTESIAN_POINT('Ctrl Pts',(-3.26107522538182,7.44496351391998,
45.2148200746046));
#167007=CARTESIAN_POINT('Ctrl Pts',(-3.44754624276917,7.35758876714839,
45.2228802417068));
#167008=CARTESIAN_POINT('Ctrl Pts',(-3.6340082503288,7.27021824211284,45.2309400193611));
#167009=CARTESIAN_POINT('Ctrl Pts',(-3.81715401658874,7.17575233124587,
45.2389997970155));
#167010=CARTESIAN_POINT('Ctrl Pts',(-3.99643489526495,7.07447494096973,
45.2470595746698));
#167011=CARTESIAN_POINT('Ctrl Pts',(-4.17572930930138,6.97318990444615,
45.2551199608219));
#167012=CARTESIAN_POINT('Ctrl Pts',(-4.35115797826423,6.86509251914933,
45.2631803469739));
#167013=CARTESIAN_POINT('Ctrl Pts',(-4.5221982233869,6.75051189102696,45.2712407331259));
#167014=CARTESIAN_POINT('Ctrl Pts',(-4.6975379055891,6.63305105070194,45.279503733131));
#167015=CARTESIAN_POINT('Ctrl Pts',(-4.86826535365477,6.508776945701,45.2877667331361));
#167016=CARTESIAN_POINT('Ctrl Pts',(-5.03385030828329,6.37809051647091,
45.2960297331412));
#167017=CARTESIAN_POINT('Ctrl Pts',(-5.19550784286892,6.25050376802187,
45.3040967475152));
#167018=CARTESIAN_POINT('Ctrl Pts',(-5.35226382801139,6.11680564990189,
45.3121637618892));
#167019=CARTESIAN_POINT('Ctrl Pts',(-5.50365920692788,5.97740938003229,
45.3202307762632));
#167020=CARTESIAN_POINT('Ctrl Pts',(-5.6605717420389,5.83293322595942,45.3285917690839));
#167021=CARTESIAN_POINT('Ctrl Pts',(-5.8117253570236,5.68233607149676,45.3369527619045));
#167022=CARTESIAN_POINT('Ctrl Pts',(-5.9566513585496,5.52611908622943,45.3453137547252));
#167023=CARTESIAN_POINT('Ctrl Pts',(-6.10157736007554,5.36990210096216,
45.3536747475458));
#167024=CARTESIAN_POINT('Ctrl Pts',(-6.24027552102279,5.20806558687446,
45.3620357403665));
#167025=CARTESIAN_POINT('Ctrl Pts',(-6.3723239016619,5.04114824765236,45.3703967331871));
#167026=CARTESIAN_POINT('Ctrl Pts',(-6.49201017224205,4.88985738191084,
45.3779749862805));
#167027=CARTESIAN_POINT('Ctrl Pts',(-6.60647314287351,4.73408915259941,
45.3855532393739));
#167028=CARTESIAN_POINT('Ctrl Pts',(-6.7153458748783,4.57425593329178,45.3931314924672));
#167029=CARTESIAN_POINT('Ctrl Pts',(-6.82413759189688,4.41454164997315,
45.4007041063885));
#167030=CARTESIAN_POINT('Ctrl Pts',(-6.92734714018761,4.25076869588969,
45.4082767203098));
#167031=CARTESIAN_POINT('Ctrl Pts',(-7.02464742836837,4.08338291978816,
45.4158493342311));
#167032=CARTESIAN_POINT('Ctrl Pts',(-7.12189378992831,3.91608991370249,
45.4234177511917));
#167033=CARTESIAN_POINT('Ctrl Pts',(-7.21323722427045,3.74518838659905,
45.4309861681524));
#167034=CARTESIAN_POINT('Ctrl Pts',(-7.29839365196104,3.57115354801705,
45.438554585113));
#167035=CARTESIAN_POINT('Ctrl Pts',(-7.38352950497776,3.39716075805245,
45.4461211734658));
#167036=CARTESIAN_POINT('Ctrl Pts',(-7.46248115814338,3.22003648961031,
45.4536877618186));
#167037=CARTESIAN_POINT('Ctrl Pts',(-7.53501018718415,3.04028107936274,
45.4612543501714));
#167038=CARTESIAN_POINT('Ctrl Pts',(-7.60752634987313,2.86055755698647,
45.4688195962426));
#167039=CARTESIAN_POINT('Ctrl Pts',(-7.67362202155401,2.67820416402399,
45.4763848423137));
#167040=CARTESIAN_POINT('Ctrl Pts',(-7.73310680513213,2.4937415068365,45.4839500883848));
#167041=CARTESIAN_POINT('Ctrl Pts',(-7.79261227411411,2.30921470409225,
45.4915179652156));
#167042=CARTESIAN_POINT('Ctrl Pts',(-7.84550214617388,2.1225775211719,45.4990858420464));
#167043=CARTESIAN_POINT('Ctrl Pts',(-7.89163568911035,1.9343664887657,45.5066537188772));
#167044=CARTESIAN_POINT('Ctrl Pts',(-7.93717355244986,1.74858565063447,
45.5141238787426));
#167045=CARTESIAN_POINT('Ctrl Pts',(-7.97612847971321,1.5612717107185,45.521594038608));
#167046=CARTESIAN_POINT('Ctrl Pts',(-8.00841401837734,1.37295028051175,
45.5290641984733));
#167047=CARTESIAN_POINT('Ctrl Pts',(-8.04863283525662,1.13835406718165,
45.5383699435256));
#167048=CARTESIAN_POINT('Ctrl Pts',(-8.07848435405988,0.902309964408368,
45.5476756885779));
#167049=CARTESIAN_POINT('Ctrl Pts',(-8.09793765476928,0.665652538468628,
45.5569814336302));
#167050=CARTESIAN_POINT('Ctrl Pts',(-8.11749538044108,0.427724739795072,
45.5663371317518));
#167051=CARTESIAN_POINT('Ctrl Pts',(-8.12654300334931,0.189177065574376,
45.5756928298733));
#167052=CARTESIAN_POINT('Ctrl Pts',(-8.12510134696751,-0.0491494049483041,
45.5850485279948));
#167053=CARTESIAN_POINT('Ctrl Pts',(-8.12365269291446,-0.288632690862096,
45.594449637839));
#167054=CARTESIAN_POINT('Ctrl Pts',(-8.1116127085664,-0.527892578407454,
45.6038507476832));
#167055=CARTESIAN_POINT('Ctrl Pts',(-8.08905456527946,-0.766083417410555,
45.6132518575274));
#167056=CARTESIAN_POINT('Ctrl Pts',(-8.06647200674089,-1.00453205641074,
45.6226631424317));
#167057=CARTESIAN_POINT('Ctrl Pts',(-8.03334853306665,-1.24190929656614,
45.6320744273359));
#167058=CARTESIAN_POINT('Ctrl Pts',(-7.98980916896147,-1.47737503907411,
45.6414857122402));
#167059=CARTESIAN_POINT('Ctrl Pts',(-7.94632085025944,-1.71256472234232,
45.6508859633858));
#167060=CARTESIAN_POINT('Ctrl Pts',(-7.89244106074854,-1.9458473523388,
45.6602862145315));
#167061=CARTESIAN_POINT('Ctrl Pts',(-7.82834556146667,-2.17639457193891,
45.6696864656771));
#167062=CARTESIAN_POINT('Ctrl Pts',(-7.78733190616315,-2.32391794412263,
45.6757015317048));
#167063=CARTESIAN_POINT('Ctrl Pts',(-7.74213644666728,-2.470321477707,45.6817165977324));
#167064=CARTESIAN_POINT('Ctrl Pts',(-7.69281625609412,-2.61539014536531,
45.68773166376));
#167065=CARTESIAN_POINT('Ctrl Pts',(-7.62933277835497,-2.80211820596099,
45.6954740772793));
#167066=CARTESIAN_POINT('Ctrl Pts',(-7.55898263820285,-2.98672135988384,
45.7032164907985));
#167067=CARTESIAN_POINT('Ctrl Pts',(-7.4819335647481,-3.16865234684964,
45.7109589043177));
#167068=CARTESIAN_POINT('Ctrl Pts',(-7.40493248768656,-3.3504700030407,
45.7186964948338));
#167069=CARTESIAN_POINT('Ctrl Pts',(-7.32124092339205,-3.52961848270866,
45.7264340853499));
#167070=CARTESIAN_POINT('Ctrl Pts',(-7.23107587985975,-3.7055673225851,
45.734171675866));
#167071=CARTESIAN_POINT('Ctrl Pts',(-7.14095097913265,-3.88143782744693,
45.7419058214928));
#167072=CARTESIAN_POINT('Ctrl Pts',(-7.04435849994866,-4.05411121590283,
45.7496399671197));
#167073=CARTESIAN_POINT('Ctrl Pts',(-6.94156292139606,-4.22307847083137,
45.7573741127465));
#167074=CARTESIAN_POINT('Ctrl Pts',(-6.83878050738632,-4.39202408692386,
45.7651072678979));
#167075=CARTESIAN_POINT('Ctrl Pts',(-6.72979675326218,-4.55726420926014,
45.7728404230494));
#167076=CARTESIAN_POINT('Ctrl Pts',(-6.61492148497391,-4.71831551616999,
45.7805735782008));
#167077=CARTESIAN_POINT('Ctrl Pts',(-6.50005769781426,-4.87935072691924,
45.7883059604674));
#167078=CARTESIAN_POINT('Ctrl Pts',(-6.37930377750725,-5.036197670542,45.7960383427341));
#167079=CARTESIAN_POINT('Ctrl Pts',(-6.25301209286992,-5.18840315790153,
45.8037707250007));
#167080=CARTESIAN_POINT('Ctrl Pts',(-6.12667184686641,-5.34066717093857,
45.8115060805039));
#167081=CARTESIAN_POINT('Ctrl Pts',(-5.99478980803626,-5.48828588977686,
45.819241436007));
#167082=CARTESIAN_POINT('Ctrl Pts',(-5.85775816550998,-5.63083979854702,
45.8269767915102));
#167083=CARTESIAN_POINT('Ctrl Pts',(-5.74306941318777,-5.7501504164021,
45.8334509040222));
#167084=CARTESIAN_POINT('Ctrl Pts',(-5.62477420040151,-5.86591373289273,
45.8399250165342));
#167085=CARTESIAN_POINT('Ctrl Pts',(-5.50312178915066,-5.97790415917445,
45.8463991290463));
#167086=CARTESIAN_POINT('Ctrl Pts',(-5.34502286193654,-6.12344641412314,
45.854812856586));
#167087=CARTESIAN_POINT('Ctrl Pts',(-5.18117711555769,-6.26268603461247,
45.8632265841257));
#167088=CARTESIAN_POINT('Ctrl Pts',(-5.01210191567926,-6.39519522370852,
45.8716403116655));
#167089=CARTESIAN_POINT('Ctrl Pts',(-4.84297956428164,-6.52774136683199,
45.880056385617));
#167090=CARTESIAN_POINT('Ctrl Pts',(-4.66862505583531,-6.65355316859082,
45.8884724595685));
#167091=CARTESIAN_POINT('Ctrl Pts',(-4.48958729244214,-6.77224434778029,
45.89688853352));
#167092=CARTESIAN_POINT('Ctrl Pts',(-4.31050515898738,-6.89096494162972,
45.9053066931863));
#167093=CARTESIAN_POINT('Ctrl Pts',(-4.12673767354954,-7.00256124405006,
45.9137248528526));
#167094=CARTESIAN_POINT('Ctrl Pts',(-3.93886197256506,-7.10669078570194,
45.922143012519));
#167095=CARTESIAN_POINT('Ctrl Pts',(-3.75091406528485,-7.21086034747584,
45.9305644075378));
#167096=CARTESIAN_POINT('Ctrl Pts',(-3.55885501763653,-7.30755728468961,
45.9389858025567));
#167097=CARTESIAN_POINT('Ctrl Pts',(-3.3632870383451,-7.3964848313371,45.9474071975756));
#167098=CARTESIAN_POINT('Ctrl Pts',(-3.16769780320298,-7.48542204332276,
45.9558295078972));
#167099=CARTESIAN_POINT('Ctrl Pts',(-2.96859911653299,-7.56658807220789,
45.9642518182189));
#167100=CARTESIAN_POINT('Ctrl Pts',(-2.76661421295655,-7.6397338539485,
45.9726741285405));
#167101=CARTESIAN_POINT('Ctrl Pts',(-2.56459073951853,-7.71289360318186,
45.9810980471375));
#167102=CARTESIAN_POINT('Ctrl Pts',(-2.35968019637371,-7.77802995587455,
45.9895219657345));
#167103=CARTESIAN_POINT('Ctrl Pts',(-2.15252331638041,-7.83494294394916,
45.9979458843315));
#167104=CARTESIAN_POINT('Ctrl Pts',(-2.09415364553419,-7.85097906295663,
46.000319454332));
#167105=CARTESIAN_POINT('Ctrl Pts',(-2.03560572557095,-7.86636261812646,
46.0026930243325));
#167106=CARTESIAN_POINT('Ctrl Pts',(-1.97689409283714,-7.88108985535666,
46.0050665943329));
#167107=CARTESIAN_POINT('Ctrl Pts',(-1.76850020764732,-7.93336341753856,
46.0134914575353));
#167108=CARTESIAN_POINT('Ctrl Pts',(-1.55802131713765,-7.97736981620701,
46.0219163207376));
#167109=CARTESIAN_POINT('Ctrl Pts',(-1.34611384576586,-8.01296855583107,
46.0303411839399));
#167110=CARTESIAN_POINT('Ctrl Pts',(-1.13424294864029,-8.04856115127786,
46.0387645930499));
#167111=CARTESIAN_POINT('Ctrl Pts',(-0.92094422318279,-8.07574894233483,
46.0471880021599));
#167112=CARTESIAN_POINT('Ctrl Pts',(-0.706882971391528,-8.09444278670599,
46.05561141127));
#167113=CARTESIAN_POINT('Ctrl Pts',(-0.492865491282712,-8.11313280852164,
46.0640330979441));
#167114=CARTESIAN_POINT('Ctrl Pts',(-0.278086058892827,-8.12333232910829,
46.0724547846182));
#167115=CARTESIAN_POINT('Ctrl Pts',(-0.0632148695584683,-8.12500408878461,
46.0808764712923));
#167116=CARTESIAN_POINT('Ctrl Pts',(0.151595840548115,-8.12667537791515,
46.0892957875364));
#167117=CARTESIAN_POINT('Ctrl Pts',(0.366497992376845,-8.11982369810707,
46.0977151037805));
#167118=CARTESIAN_POINT('Ctrl Pts',(0.580820601175361,-8.10446389292656,
46.1061344200247));
#167119=CARTESIAN_POINT('Ctrl Pts',(0.795083174252925,-8.08910839031115,
46.1145513778628));
#167120=CARTESIAN_POINT('Ctrl Pts',(1.00876626547239,-8.06524953964482,
46.122968335701));
#167121=CARTESIAN_POINT('Ctrl Pts',(1.22120205190785,-8.03295419574368,
46.1313852935392));
#167122=CARTESIAN_POINT('Ctrl Pts',(1.43356039372482,-8.00067062528538,
46.1397991829297));
#167123=CARTESIAN_POINT('Ctrl Pts',(1.64467207818713,-7.95995674306305,
46.1482130723202));
#167124=CARTESIAN_POINT('Ctrl Pts',(1.85387654835768,-7.91093100121278,
46.1566269617107));
#167125=CARTESIAN_POINT('Ctrl Pts',(1.91278060502567,-7.89712720880918,
46.1589959943468));
#167126=CARTESIAN_POINT('Ctrl Pts',(1.97153351604792,-7.88266478779449,
46.161365026983));
#167127=CARTESIAN_POINT('Ctrl Pts',(2.03012067429592,-7.8675471152257,46.1637340596191));
#167128=CARTESIAN_POINT('Ctrl Pts',(2.22140634855614,-7.81818827487497,
46.1714688946699));
#167129=CARTESIAN_POINT('Ctrl Pts',(2.41100894077351,-7.7618185879595,46.1792037297208));
#167130=CARTESIAN_POINT('Ctrl Pts',(2.5983730610885,-7.69858071321653,46.1869385647716));
#167131=CARTESIAN_POINT('Ctrl Pts',(2.78567924938508,-7.63536239129786,
46.1946710082514));
#167132=CARTESIAN_POINT('Ctrl Pts',(2.97074800970908,-7.56528022338878,
46.2024034517312));
#167133=CARTESIAN_POINT('Ctrl Pts',(3.15303883602665,-7.48852680178202,
46.210135895211));
#167134=CARTESIAN_POINT('Ctrl Pts',(3.33530569256797,-7.41178347263235,
46.2178673219367));
#167135=CARTESIAN_POINT('Ctrl Pts',(3.5147950174207,-7.32837077485111,46.2255987486624));
#167136=CARTESIAN_POINT('Ctrl Pts',(3.69098590082337,-7.23852959118239,
46.2333301753881));
#167137=CARTESIAN_POINT('Ctrl Pts',(3.86723987279149,-7.14865623813415,
46.2410643705012));
#167138=CARTESIAN_POINT('Ctrl Pts',(4.04019272660983,-7.05234995721369,
46.2487985656144));
#167139=CARTESIAN_POINT('Ctrl Pts',(4.20934721600092,-6.94989809836413,
46.2565327607275));
#167140=CARTESIAN_POINT('Ctrl Pts',(4.37853029070763,-6.84742892623644,
46.2642682628376));
#167141=CARTESIAN_POINT('Ctrl Pts',(4.54391342364262,-6.73881229647638,
46.2720037649477));
#167142=CARTESIAN_POINT('Ctrl Pts',(4.70502790461982,-6.62437921463203,
46.2797392670578));
#167143=CARTESIAN_POINT('Ctrl Pts',(4.86627427876861,-6.50985245441681,
46.2874811016831));
#167144=CARTESIAN_POINT('Ctrl Pts',(5.02324473536826,-6.38949993976282,
46.2952229363085));
#167145=CARTESIAN_POINT('Ctrl Pts',(5.17550251143273,-6.26369390349285,
46.3029647709338));
#167146=CARTESIAN_POINT('Ctrl Pts',(5.30292265049419,-6.15841046214334,
46.3094436889244));
#167147=CARTESIAN_POINT('Ctrl Pts',(5.42704275918094,-6.04930841442362,
46.315922606915));
#167148=CARTESIAN_POINT('Ctrl Pts',(5.54762664613986,-5.93662582259813,
46.3224015249056));
#167149=CARTESIAN_POINT('Ctrl Pts',(5.72253925643606,-5.77317441322492,
46.3317995007564));
#167150=CARTESIAN_POINT('Ctrl Pts',(5.89011105866949,-5.60209625368084,
46.3411974766071));
#167151=CARTESIAN_POINT('Ctrl Pts',(6.04977040429898,-5.42401747948586,
46.3505954524579));
#167152=CARTESIAN_POINT('Ctrl Pts',(6.2096566341494,-5.24568564610547,46.3600067833204));
#167153=CARTESIAN_POINT('Ctrl Pts',(6.36160789097475,-5.06033332628138,
46.3694181141828));
#167154=CARTESIAN_POINT('Ctrl Pts',(6.50509109190373,-4.86862171959731,
46.3788294450453));
#167155=CARTESIAN_POINT('Ctrl Pts',(6.64835793060362,-4.67719920006977,
46.3882265843055));
#167156=CARTESIAN_POINT('Ctrl Pts',(6.78318221548041,-4.47943659066402,
46.3976237235656));
#167157=CARTESIAN_POINT('Ctrl Pts',(6.90907431273789,-4.27602381934028,
46.4070208628258));
#167158=CARTESIAN_POINT('Ctrl Pts',(7.03464874314137,-4.07312432483484,
46.4163942900363));
#167159=CARTESIAN_POINT('Ctrl Pts',(7.15133596888961,-3.86460316810055,
46.4257677172467));
#167160=CARTESIAN_POINT('Ctrl Pts',(7.25869131645649,-3.65117623991217,
46.4351411444572));
#167161=CARTESIAN_POINT('Ctrl Pts',(7.36534939771774,-3.43913550634857,
46.4444536918409));
#167162=CARTESIAN_POINT('Ctrl Pts',(7.46279638797377,-3.22225254998496,
46.4537662392247));
#167163=CARTESIAN_POINT('Ctrl Pts',(7.55063753374129,-3.00125980157619,
46.4630787866084));
#167164=CARTESIAN_POINT('Ctrl Pts',(7.60720208155978,-2.85895342822822,
46.4690755211363));
#167165=CARTESIAN_POINT('Ctrl Pts',(7.65978429862617,-2.71494349904361,
46.4750722556643));
#167166=CARTESIAN_POINT('Ctrl Pts',(7.70828810210639,-2.56943225196248,
46.4810689901922));
#167167=CARTESIAN_POINT('Ctrl Pts',(7.76719546373361,-2.3927103654793,46.4883519615073));
#167168=CARTESIAN_POINT('Ctrl Pts',(7.82007886233047,-2.21378882965252,
46.4956349328224));
#167169=CARTESIAN_POINT('Ctrl Pts',(7.8667627137631,-2.03315812662141,46.5029179041375));
#167170=CARTESIAN_POINT('Ctrl Pts',(7.91343787853713,-1.85256103429721,
46.5101995202798));
#167171=CARTESIAN_POINT('Ctrl Pts',(7.95391568214445,-1.67025577966911,
46.5174811364221));
#167172=CARTESIAN_POINT('Ctrl Pts',(7.9880702730007,-1.48674842394486,46.5247627525644));
#167173=CARTESIAN_POINT('Ctrl Pts',(8.02222016869862,-1.30326629458312,
46.5320433677186));
#167174=CARTESIAN_POINT('Ctrl Pts',(8.05004851392273,-1.11858277549143,
46.5393239828727));
#167175=CARTESIAN_POINT('Ctrl Pts',(8.07148061401522,-0.933213941214172,
46.5466045980269));
#167176=CARTESIAN_POINT('Ctrl Pts',(8.09292046468911,-0.747778071217875,
46.5538878461008));
#167177=CARTESIAN_POINT('Ctrl Pts',(8.10795940919785,-0.561656777498488,
46.5611710941748));
#167178=CARTESIAN_POINT('Ctrl Pts',(8.11657465044426,-0.375371158009863,
46.5684543422488));
#167179=CARTESIAN_POINT('Ctrl Pts',(8.12238652308375,-0.249702211073741,
46.5733676475175));
#167180=CARTESIAN_POINT('Ctrl Pts',(8.12527611288442,-0.12395856849932,
46.5782809527863));
#167181=CARTESIAN_POINT('Ctrl Pts',(8.12524982216074,0.00169999318035808,
46.5831942580551));
#167182=CARTESIAN_POINT('',(8.12779981229061,-5.30458549197524E-5,48.5834001493614));
#167183=CARTESIAN_POINT('Ctrl Pts',(8.12524981409313,0.00169347021508326,
46.5833637857063));
#167184=CARTESIAN_POINT('Ctrl Pts',(8.12475676563394,2.24736674679337,46.6713392646829));
#167185=CARTESIAN_POINT('Ctrl Pts',(7.14356931219011,4.47573372637722,46.7593147436594));
#167186=CARTESIAN_POINT('Ctrl Pts',(3.83078204044914,7.50935546634369,46.9352878157772));
#167187=CARTESIAN_POINT('Ctrl Pts',(1.52412477697731,8.29110090552138,47.0232854089184));
#167188=CARTESIAN_POINT('Ctrl Pts',(-2.9510162393256,7.89663306204424,47.1992805952008));
#167189=CARTESIAN_POINT('Ctrl Pts',(-5.08535169588728,6.7234298308579,47.287278188342));
#167190=CARTESIAN_POINT('Ctrl Pts',(-7.81671694684396,3.15661951052958,
47.4632733746244));
#167191=CARTESIAN_POINT('Ctrl Pts',(-8.39290461146698,0.790229551554374,
47.5512709677656));
#167192=CARTESIAN_POINT('Ctrl Pts',(-7.60701611462498,-3.63299000730381,
47.727266154048));
#167193=CARTESIAN_POINT('Ctrl Pts',(-6.25093680401385,-5.65606750609986,
47.8152637471892));
#167194=CARTESIAN_POINT('Ctrl Pts',(-2.45807268688606,-8.06369575488301,
47.9912589334716));
#167195=CARTESIAN_POINT('Ctrl Pts',(-0.0502299510459392,-8.42987470330084,
48.0792565266128));
#167196=CARTESIAN_POINT('Ctrl Pts',(4.28689960880937,-7.25863639434595,
48.2552517128952));
#167197=CARTESIAN_POINT('Ctrl Pts',(6.1830912555711,-5.73015646266433,48.3432493060364));
#167198=CARTESIAN_POINT('Ctrl Pts',(7.81049469094434,-2.58642819611753,
48.4819294849132));
#167199=CARTESIAN_POINT('Ctrl Pts',(8.12523846244703,-1.2938062194213,48.5326120706489));
#167200=CARTESIAN_POINT('Ctrl Pts',(8.1252499996828,-7.11371931539338E-5,
48.5832946563846));
#167201=CARTESIAN_POINT('',(8.11795043021363,-0.00244482526706127,50.5832974432124));
#167202=CARTESIAN_POINT('Ctrl Pts',(8.12779981229061,-5.30458549197522E-5,
48.5834001493614));
#167203=CARTESIAN_POINT('Ctrl Pts',(8.10719593127611,2.35984343847289,48.6759604227372));
#167204=CARTESIAN_POINT('Ctrl Pts',(5.81138593698418,7.42468183755121,48.8742990063037));
#167205=CARTESIAN_POINT('Ctrl Pts',(-2.84362164243682,9.17837728242667,
49.1784159000614));
#167206=CARTESIAN_POINT('Ctrl Pts',(-8.15113057818095,3.70434890315244,
49.4428616755388));
#167207=CARTESIAN_POINT('Ctrl Pts',(-8.24488799843749,-1.87812548990129,
49.6544182959206));
#167208=CARTESIAN_POINT('Ctrl Pts',(-6.36260440029279,-5.60229600309865,
49.8130857612071));
#167209=CARTESIAN_POINT('Ctrl Pts',(-2.90807460908608,-7.94038890968604,
49.9717532264935));
#167210=CARTESIAN_POINT('Ctrl Pts',(2.64399874568358,-8.55485708321899,
50.1833098468754));
#167211=CARTESIAN_POINT('Ctrl Pts',(7.34346692161665,-5.03063998245504,
50.3871579191151));
#167212=CARTESIAN_POINT('Ctrl Pts',(8.11601312705655,-1.16362153771914,
50.5381168362592));
#167213=CARTESIAN_POINT('Ctrl Pts',(8.11226079205514,-0.00435044046600885,
50.5832974432124));
#167214=CARTESIAN_POINT('',(8.12525,1.19476911003558E-13,52.5832974432124));
#167215=CARTESIAN_POINT('Ctrl Pts',(8.12525,6.37338797166611E-14,50.5832974432124));
#167216=CARTESIAN_POINT('Ctrl Pts',(8.12524999999998,2.24624642433412,50.6712950363536));
#167217=CARTESIAN_POINT('Ctrl Pts',(7.14398562317601,4.47535249753447,50.7592926294948));
#167218=CARTESIAN_POINT('Ctrl Pts',(3.83078204044946,7.50935546634353,50.9352878157772));
#167219=CARTESIAN_POINT('Ctrl Pts',(1.52412477697767,8.29110090552131,51.0232854089184));
#167220=CARTESIAN_POINT('Ctrl Pts',(-2.95101623932526,7.89663306204436,
51.1992805952008));
#167221=CARTESIAN_POINT('Ctrl Pts',(-5.08535169588699,6.72342983085812,
51.287278188342));
#167222=CARTESIAN_POINT('Ctrl Pts',(-7.81671694684382,3.15661951052992,
51.4632733746244));
#167223=CARTESIAN_POINT('Ctrl Pts',(-8.39290461146695,0.790229551554735,
51.5512709677656));
#167224=CARTESIAN_POINT('Ctrl Pts',(-7.60701611462514,-3.63299000730349,
51.727266154048));
#167225=CARTESIAN_POINT('Ctrl Pts',(-6.25093680401409,-5.65606750609959,
51.8152637471892));
#167226=CARTESIAN_POINT('Ctrl Pts',(-2.45807268688641,-8.0636957548829,
51.9912589334716));
#167227=CARTESIAN_POINT('Ctrl Pts',(-0.0502299510463028,-8.42987470330084,
52.0792565266128));
#167228=CARTESIAN_POINT('Ctrl Pts',(4.28689960880906,-7.25863639434614,
52.2552517128952));
#167229=CARTESIAN_POINT('Ctrl Pts',(6.18309125557085,-5.7301564626646,52.3432493060364));
#167230=CARTESIAN_POINT('Ctrl Pts',(7.81050559202884,-2.5864071380034,52.4819304138558));
#167231=CARTESIAN_POINT('Ctrl Pts',(8.12525000000002,-1.29375883538179,
52.5326139285341));
#167232=CARTESIAN_POINT('Ctrl Pts',(8.12525,1.19477141073054E-13,52.5832974432124));
#167233=CARTESIAN_POINT('',(8.12525,-4.6183759941365E-13,56.5832974432124));
#167234=CARTESIAN_POINT('Ctrl Pts',(8.12524980819547,0.00176547994832403,
52.5830473882962));
#167235=CARTESIAN_POINT('Ctrl Pts',(8.12524364980434,0.0301081787410185,
52.5841494397994));
#167236=CARTESIAN_POINT('Ctrl Pts',(8.12508919290422,0.05845064286214,52.5852526953861));
#167237=CARTESIAN_POINT('Ctrl Pts',(8.12444520351248,0.118736080490925,
52.5876021191595));
#167238=CARTESIAN_POINT('Ctrl Pts',(8.12391557225265,0.150678096441481,
52.5888486012718));
#167239=CARTESIAN_POINT('Ctrl Pts',(8.12241848601408,0.217272047186492,
52.5914509636609));
#167240=CARTESIAN_POINT('Ctrl Pts',(8.12141762297129,0.251922582637177,
52.5928071001308));
#167241=CARTESIAN_POINT('Ctrl Pts',(8.11855027708299,0.333172424316436,
52.5959920901548));
#167242=CARTESIAN_POINT('Ctrl Pts',(8.11650427598706,0.379764110366802,
52.5978224004088));
#167243=CARTESIAN_POINT('Ctrl Pts',(8.1084684309325,0.532703079706359,52.6038438746892));
#167244=CARTESIAN_POINT('Ctrl Pts',(8.10078858546559,0.638949838364625,
52.6080484828693));
#167245=CARTESIAN_POINT('Ctrl Pts',(8.08063974503247,0.8577707765569,52.6167526943706));
#167246=CARTESIAN_POINT('Ctrl Pts',(8.06790134402783,0.970297412420684,
52.6212532560794));
#167247=CARTESIAN_POINT('Ctrl Pts',(8.0390913503981,1.18461350552756,52.6298659506021));
#167248=CARTESIAN_POINT('Ctrl Pts',(8.02342700255712,1.28643615053409,52.6339756641758));
#167249=CARTESIAN_POINT('Ctrl Pts',(7.97269296883845,1.57907854654426,52.6458250754722));
#167250=CARTESIAN_POINT('Ctrl Pts',(7.93271981166649,1.76897697253052,52.6535626818822));
#167251=CARTESIAN_POINT('Ctrl Pts',(7.87956828591667,1.98312920696857,52.6622845119913));
#167252=CARTESIAN_POINT('Ctrl Pts',(7.87302124809859,2.00896347833129,52.663336561779));
#167253=CARTESIAN_POINT('Ctrl Pts',(7.86153479496716,2.05336979698259,52.6651444331469));
#167254=CARTESIAN_POINT('Ctrl Pts',(7.85665638235957,2.07195737114584,52.6659010230804));
#167255=CARTESIAN_POINT('Ctrl Pts',(7.84718558242081,2.10752829488696,52.6673484896315));
#167256=CARTESIAN_POINT('Ctrl Pts',(7.84260388745124,2.12451437874236,52.6680395125751));
#167257=CARTESIAN_POINT('Ctrl Pts',(7.83345778635271,2.15798966484895,52.6694008784996));
#167258=CARTESIAN_POINT('Ctrl Pts',(7.82889640601104,2.17447955851659,52.6700712499469));
#167259=CARTESIAN_POINT('Ctrl Pts',(7.81615638224685,2.21997640851222,52.6719201965385));
#167260=CARTESIAN_POINT('Ctrl Pts',(7.80786837905136,2.24895247458976,52.6730970546445));
#167261=CARTESIAN_POINT('Ctrl Pts',(7.77781867944381,2.35184201129915,52.6772743654238));
#167262=CARTESIAN_POINT('Ctrl Pts',(7.7551669512367,2.42549169822684,52.6802617312939));
#167263=CARTESIAN_POINT('Ctrl Pts',(7.70104970078162,2.5929338795687,52.6870572082245));
#167264=CARTESIAN_POINT('Ctrl Pts',(7.66891189196776,2.68649646263372,52.6908570679943));
#167265=CARTESIAN_POINT('Ctrl Pts',(7.63057555018146,2.79180537228536,52.6951473183141));
#167266=CARTESIAN_POINT('Ctrl Pts',(7.62604754298188,2.80415037692119,52.6956504584141));
#167267=CARTESIAN_POINT('Ctrl Pts',(7.50826267281147,3.12287970464047,52.7086467029539));
#167268=CARTESIAN_POINT('Ctrl Pts',(7.37666184033898,3.42217014181975,52.7209987710771));
#167269=CARTESIAN_POINT('Ctrl Pts',(7.10194013991312,3.95695900570685,52.7438563981186));
#167270=CARTESIAN_POINT('Ctrl Pts',(6.96417927904945,4.19467312589471,52.7543267985542));
#167271=CARTESIAN_POINT('Ctrl Pts',(6.7552169514716,4.51648556842928,52.7691022334592));
#167272=CARTESIAN_POINT('Ctrl Pts',(6.6939451979396,4.6068096751942,52.773318835394));
#167273=CARTESIAN_POINT('Ctrl Pts',(6.5956544134045,4.74560258961966,52.7799151332479));
#167274=CARTESIAN_POINT('Ctrl Pts',(6.55987756512564,4.79493559538267,52.7822834641372));
#167275=CARTESIAN_POINT('Ctrl Pts',(6.49869709897378,4.87733138658489,52.786280357297));
#167276=CARTESIAN_POINT('Ctrl Pts',(6.47358776137376,4.91060962811642,52.7879062077734));
#167277=CARTESIAN_POINT('Ctrl Pts',(6.42690649413506,4.97149755920482,52.7909026886655));
#167278=CARTESIAN_POINT('Ctrl Pts',(6.40540991914324,4.99916381253992,52.7922726154028));
#167279=CARTESIAN_POINT('Ctrl Pts',(6.36053392030442,5.05615489079459,52.7951122120692));
#167280=CARTESIAN_POINT('Ctrl Pts',(6.3371290482563,5.08545862695046,52.7965820783784));
#167281=CARTESIAN_POINT('Ctrl Pts',(6.28387947523037,5.15119053401777,52.799901579663));
#167282=CARTESIAN_POINT('Ctrl Pts',(6.25391928403291,5.18752337306637,52.8017521633865));
#167283=CARTESIAN_POINT('Ctrl Pts',(6.16135495271028,5.29780904610997,52.8074183505815));
#167284=CARTESIAN_POINT('Ctrl Pts',(6.09774264110756,5.37090402746593,52.8112419931888));
#167285=CARTESIAN_POINT('Ctrl Pts',(5.81855289916133,5.68035746699471,52.8277295692925));
#167286=CARTESIAN_POINT('Ctrl Pts',(5.59043004009725,5.90500681505646,52.8404288021798));
#167287=CARTESIAN_POINT('Ctrl Pts',(5.05543404332821,6.37299682983889,52.8691317044041));
#167288=CARTESIAN_POINT('Ctrl Pts',(4.74302764078544,6.60879483677502,52.8852560908435));
#167289=CARTESIAN_POINT('Ctrl Pts',(4.22292207081797,6.94542282654672,52.9112908980809));
#167290=CARTESIAN_POINT('Ctrl Pts',(4.0258108205282,7.06150228536007,52.9209808249307));
#167291=CARTESIAN_POINT('Ctrl Pts',(3.58411376410034,7.29710746165448,52.9421679662169));
#167292=CARTESIAN_POINT('Ctrl Pts',(3.33787837770958,7.41297663020197,52.9536491842324));
#167293=CARTESIAN_POINT('Ctrl Pts',(2.96920252204968,7.56436023241498,52.9700379370817));
#167294=CARTESIAN_POINT('Ctrl Pts',(2.85100111303177,7.60969800405325,52.9751747443793));
#167295=CARTESIAN_POINT('Ctrl Pts',(2.71167995292251,7.65943438942436,52.9810572929424));
#167296=CARTESIAN_POINT('Ctrl Pts',(2.6915456165161,7.66653282374316,52.9819032603197));
#167297=CARTESIAN_POINT('Ctrl Pts',(2.66223391662965,7.67673706692509,52.983128547788));
#167298=CARTESIAN_POINT('Ctrl Pts',(2.65307869349873,7.67990591535224,52.9835103663421));
#167299=CARTESIAN_POINT('Ctrl Pts',(2.63704505729796,7.68542345979927,52.9841774691844));
#167300=CARTESIAN_POINT('Ctrl Pts',(2.63016912886034,7.68777931165431,52.9844630444677));
#167301=CARTESIAN_POINT('Ctrl Pts',(2.61684589222069,7.69232419351748,52.9850153978052));
#167302=CARTESIAN_POINT('Ctrl Pts',(2.61039897746855,7.69451435118389,52.9852822224627));
#167303=CARTESIAN_POINT('Ctrl Pts',(2.59330113024004,7.70029890147038,52.9859886585913));
#167304=CARTESIAN_POINT('Ctrl Pts',(2.58264545584154,7.70387930689289,52.986427679381));
#167305=CARTESIAN_POINT('Ctrl Pts',(2.54495994649214,7.71645501233108,52.9879758731397));
#167306=CARTESIAN_POINT('Ctrl Pts',(2.51789006627449,7.7253303313814,52.9890798327609));
#167307=CARTESIAN_POINT('Ctrl Pts',(2.0670385329708,7.87052816327125,53.007324847304));
#167308=CARTESIAN_POINT('Ctrl Pts',(1.63279095495319,7.97194318363231,53.0226952712351));
#167309=CARTESIAN_POINT('Ctrl Pts',(0.956991521298055,8.07220542378015,
53.0456933946499));
#167310=CARTESIAN_POINT('Ctrl Pts',(0.720142929848893,8.09677272844999,
53.0535848358485));
#167311=CARTESIAN_POINT('Ctrl Pts',(0.123726161042556,8.13225643387959,
53.0735568585539));
#167312=CARTESIAN_POINT('Ctrl Pts',(-0.236114537315934,8.12976861940751,
53.0857107651117));
#167313=CARTESIAN_POINT('Ctrl Pts',(-0.899715183285292,8.08107663315175,
53.109308456053));
#167314=CARTESIAN_POINT('Ctrl Pts',(-1.2033054909797,8.041475128801,53.1205665819576));
#167315=CARTESIAN_POINT('Ctrl Pts',(-1.52994162646951,7.97995407201859,
53.1333796028177));
#167316=CARTESIAN_POINT('Ctrl Pts',(-1.55593275762511,7.97492705984995,
53.134403944482));
#167317=CARTESIAN_POINT('Ctrl Pts',(-1.59422907750533,7.96732572690989,
53.1359204024423));
#167318=CARTESIAN_POINT('Ctrl Pts',(-1.60655371162721,7.96484970104272,
53.1364095281425));
#167319=CARTESIAN_POINT('Ctrl Pts',(-1.62834828306713,7.96041851496297,
53.1372764342931));
#167320=CARTESIAN_POINT('Ctrl Pts',(-1.63782058250833,7.95847502999453,
53.1376538587581));
#167321=CARTESIAN_POINT('Ctrl Pts',(-1.65633791039776,7.95464126624829,
53.1383929636836));
#167322=CARTESIAN_POINT('Ctrl Pts',(-1.66538323037867,7.95275245707023,
53.1387545989205));
#167323=CARTESIAN_POINT('Ctrl Pts',(-1.68976902745533,7.94761687980665,
53.1397311719023));
#167324=CARTESIAN_POINT('Ctrl Pts',(-1.70510332490954,7.94434113582644,
53.140346991521));
#167325=CARTESIAN_POINT('Ctrl Pts',(-1.76155669317739,7.93211047246434,
53.1426205509197));
#167326=CARTESIAN_POINT('Ctrl Pts',(-1.80261515888727,7.92288060334149,
53.1442866596397));
#167327=CARTESIAN_POINT('Ctrl Pts',(-2.50359534796896,7.75957053081513,
53.1729492991114));
#167328=CARTESIAN_POINT('Ctrl Pts',(-3.14166840407209,7.52386786522178,
53.2026434635012));
#167329=CARTESIAN_POINT('Ctrl Pts',(-4.08816258099939,7.03262804904752,
53.2505134909075));
#167330=CARTESIAN_POINT('Ctrl Pts',(-4.42004227846969,6.82892181270963,
53.2680752781826));
#167331=CARTESIAN_POINT('Ctrl Pts',(-4.86346280159948,6.5108371267576,53.2916706494515));
#167332=CARTESIAN_POINT('Ctrl Pts',(-4.9881969189763,6.41577479799822,53.2983208620974));
#167333=CARTESIAN_POINT('Ctrl Pts',(-5.17537780956116,6.2643595143959,53.3082335444692));
#167334=CARTESIAN_POINT('Ctrl Pts',(-5.23982252973921,6.21055519564037,
53.3116305437736));
#167335=CARTESIAN_POINT('Ctrl Pts',(-5.31509526012769,6.14570477041037,
53.3155848220997));
#167336=CARTESIAN_POINT('Ctrl Pts',(-5.32673453854297,6.13561927678388,
53.3161959406604));
#167337=CARTESIAN_POINT('Ctrl Pts',(-5.34527493106549,6.119461411683,53.3171689964752));
#167338=CARTESIAN_POINT('Ctrl Pts',(-5.3521945013234,6.1134103476423,53.3175320659135));
#167339=CARTESIAN_POINT('Ctrl Pts',(-5.36473441860925,6.1024067625279,53.318189897479));
#167340=CARTESIAN_POINT('Ctrl Pts',(-5.37035820733078,6.09745819198557,
53.3184848655716));
#167341=CARTESIAN_POINT('Ctrl Pts',(-5.38160424078162,6.08753478153266,
53.3190746363133));
#167342=CARTESIAN_POINT('Ctrl Pts',(-5.3872264497955,6.08255991337862,53.3193694369066));
#167343=CARTESIAN_POINT('Ctrl Pts',(-5.40306794553901,6.06850321341805,
53.3201999891223));
#167344=CARTESIAN_POINT('Ctrl Pts',(-5.41327124360715,6.05940334697036,
53.3207348229191));
#167345=CARTESIAN_POINT('Ctrl Pts',(-5.4556021226161,6.02145806877636,53.3229534411135));
#167346=CARTESIAN_POINT('Ctrl Pts',(-5.48752280765111,5.99238227337843,
53.3246257987157));
#167347=CARTESIAN_POINT('Ctrl Pts',(-5.97033212278799,5.54550946973115,
53.3499339597509));
#167348=CARTESIAN_POINT('Ctrl Pts',(-6.37264919323184,5.07809061416835,
53.3713685981259));
#167349=CARTESIAN_POINT('Ctrl Pts',(-6.96678705617603,4.20459128241462,
53.4095269562731));
#167350=CARTESIAN_POINT('Ctrl Pts',(-7.18496127042977,3.81981869399859,
53.4257761720295));
#167351=CARTESIAN_POINT('Ctrl Pts',(-7.39581230987746,3.36529113397211,
53.4449234833113));
#167352=CARTESIAN_POINT('Ctrl Pts',(-7.42024471149788,3.31107119722726,
53.4472057502132));
#167353=CARTESIAN_POINT('Ctrl Pts',(-7.45787772142508,3.22504769761268,
53.450824233195));
#167354=CARTESIAN_POINT('Ctrl Pts',(-7.47147524395176,3.19341986311009,
53.4521540938941));
#167355=CARTESIAN_POINT('Ctrl Pts',(-7.49420432098751,3.13961214663148,
53.4544156671137));
#167356=CARTESIAN_POINT('Ctrl Pts',(-7.50343943801816,3.11747645228425,
53.4553457906309));
#167357=CARTESIAN_POINT('Ctrl Pts',(-7.52147381051481,3.07370538314876,
53.4571845017296));
#167358=CARTESIAN_POINT('Ctrl Pts',(-7.53027806140087,3.05207230873849,
53.4580930060731));
#167359=CARTESIAN_POINT('Ctrl Pts',(-7.53901433962415,3.03033832337175,
53.459005490529));
#167360=CARTESIAN_POINT('Ctrl Pts',(-7.53903978272908,3.03027502408319,
53.4590081480982));
#167361=CARTESIAN_POINT('Ctrl Pts',(-7.53909088779636,3.03014787638837,
53.4590134862864));
#167362=CARTESIAN_POINT('Ctrl Pts',(-7.5391165497118,3.03008402805877,53.4590161669021));
#167363=CARTESIAN_POINT('Ctrl Pts',(-7.53916809297861,3.02995578072195,
53.4590215512489));
#167364=CARTESIAN_POINT('Ctrl Pts',(-7.53919397427158,3.02989138181951,
53.4590242549754));
#167365=CARTESIAN_POINT('Ctrl Pts',(-7.53924595678346,3.02976203199594,
53.4590296855999));
#167366=CARTESIAN_POINT('Ctrl Pts',(-7.53927205799163,3.02969708106049,
53.4590324124985));
#167367=CARTESIAN_POINT('Ctrl Pts',(-7.53932448071584,3.02956662609727,
53.4590378895119));
#167368=CARTESIAN_POINT('Ctrl Pts',(-7.53935080229867,3.0295011218618,53.4590406396355));
#167369=CARTESIAN_POINT('Ctrl Pts',(-7.53940366632769,3.02936955879153,
53.4590461631622));
#167370=CARTESIAN_POINT('Ctrl Pts',(-7.53943020877195,3.02930349991962,
53.4590489365668));
#167371=CARTESIAN_POINT('Ctrl Pts',(-7.53948351511514,3.02917082597877,
53.4590545067226));
#167372=CARTESIAN_POINT('Ctrl Pts',(-7.53951027893799,3.02910421105684,
53.4590573034675));
#167373=CARTESIAN_POINT('Ctrl Pts',(-7.53956401754028,3.02897045101929,
53.4590629192119));
#167374=CARTESIAN_POINT('Ctrl Pts',(-7.53959099232742,3.02890330584792,
53.4590657382133));
#167375=CARTESIAN_POINT('Ctrl Pts',(-7.53964520790905,3.02876834813996,
53.4590714042305));
#167376=CARTESIAN_POINT('Ctrl Pts',(-7.5396724162355,3.02870061638599,53.4590742478543));
#167377=CARTESIAN_POINT('Ctrl Pts',(-7.53972705406999,3.02856459697546,
53.4590799584355));
#167378=CARTESIAN_POINT('Ctrl Pts',(-7.53975448496652,3.0284963058182,53.4590828255399));
#167379=CARTESIAN_POINT('Ctrl Pts',(-7.53980957794039,3.02835914257522,
53.4590885841331));
#167380=CARTESIAN_POINT('Ctrl Pts',(-7.53983724119974,3.02829026749664,
53.4590914757478));
#167381=CARTESIAN_POINT('Ctrl Pts',(-7.53989761676832,3.02813994043697,
53.4590977869927));
#167382=CARTESIAN_POINT('Ctrl Pts',(-7.53993035782358,3.02805841578205,
53.4591012096733));
#167383=CARTESIAN_POINT('Ctrl Pts',(-7.53999694110362,3.02789261680388,
53.4591081704675));
#167384=CARTESIAN_POINT('Ctrl Pts',(-7.54003078327093,3.02780834236157,
53.4591117085859));
#167385=CARTESIAN_POINT('Ctrl Pts',(-7.54009959633272,3.02763697438965,
53.4591189031692));
#167386=CARTESIAN_POINT('Ctrl Pts',(-7.54013456707983,3.02754988094928,
53.4591225596302));
#167387=CARTESIAN_POINT('Ctrl Pts',(-7.54020566465514,3.02737280601586,
53.4591299937933));
#167388=CARTESIAN_POINT('Ctrl Pts',(-7.54024179141008,3.02728282441113,
53.4591337714999));
#167389=CARTESIAN_POINT('Ctrl Pts',(-7.54031522852707,3.02709990369866,
53.4591414510692));
#167390=CARTESIAN_POINT('Ctrl Pts',(-7.54035253877454,3.02700696456519,
53.4591453529327));
#167391=CARTESIAN_POINT('Ctrl Pts',(-7.54042837035463,3.02681805940569,
53.4591532837281));
#167392=CARTESIAN_POINT('Ctrl Pts',(-7.54046689155222,3.02672209338719,
53.4591573126594));
#167393=CARTESIAN_POINT('Ctrl Pts',(-7.54054517236893,3.02652706536018,
53.4591655004903));
#167394=CARTESIAN_POINT('Ctrl Pts',(-7.54058493187534,3.02642800328518,
53.4591696593923));
#167395=CARTESIAN_POINT('Ctrl Pts',(-7.54066571651116,3.02622671432042,
53.4591781100533));
#167396=CARTESIAN_POINT('Ctrl Pts',(-7.54070674153946,3.0261244873162,53.4591824018166));
#167397=CARTESIAN_POINT('Ctrl Pts',(-7.54079008433386,3.02591679981866,
53.4591911210822));
#167398=CARTESIAN_POINT('Ctrl Pts',(-7.54083240195278,3.02581133930582,
53.4591955485848));
#167399=CARTESIAN_POINT('Ctrl Pts',(-7.54091835674091,3.02559711680211,
53.4592045421822));
#167400=CARTESIAN_POINT('Ctrl Pts',(-7.5409619937665,3.02548835476233,53.4592091082786));
#167401=CARTESIAN_POINT('Ctrl Pts',(-7.54105061390349,3.02526746183582,
53.4592183818907));
#167402=CARTESIAN_POINT('Ctrl Pts',(-7.54109559686292,3.02515533089981,
53.4592230894081));
#167403=CARTESIAN_POINT('Ctrl Pts',(-7.54930805871703,3.00468245654526,
53.4600825869985));
#167404=CARTESIAN_POINT('Ctrl Pts',(-7.55739303655472,2.98428874575111,
53.4609385218818));
#167405=CARTESIAN_POINT('Ctrl Pts',(-7.57551424033519,2.93803354119027,
53.4628794789341));
#167406=CARTESIAN_POINT('Ctrl Pts',(-7.5855008042606,2.91215292092137,53.4639652041845));
#167407=CARTESIAN_POINT('Ctrl Pts',(-7.61468345057594,2.83535613696169,
53.4671865292511));
#167408=CARTESIAN_POINT('Ctrl Pts',(-7.63350072338563,2.78429795722043,
53.4693277134119));
#167409=CARTESIAN_POINT('Ctrl Pts',(-7.81365719075656,2.27990929505585,
53.4904840891173));
#167410=CARTESIAN_POINT('Ctrl Pts',(-7.93492731954391,1.81331260290932,
53.5101723806308));
#167411=CARTESIAN_POINT('Ctrl Pts',(-8.0578859729071,1.07724564580059,53.5415444711816));
#167412=CARTESIAN_POINT('Ctrl Pts',(-8.0887443694058,0.813754326795947,
53.5528169504256));
#167413=CARTESIAN_POINT('Ctrl Pts',(-8.13058321827464,0.196211154622309,
53.5790622868739));
#167414=CARTESIAN_POINT('Ctrl Pts',(-8.13141645595455,-0.158007032505852,
53.5939918025026));
#167415=CARTESIAN_POINT('Ctrl Pts',(-8.10614464323266,-0.558925034036176,
53.6101680111357));
#167416=CARTESIAN_POINT('Ctrl Pts',(-8.10271174310439,-0.606663568979511,
53.6120821385718));
#167417=CARTESIAN_POINT('Ctrl Pts',(-8.09775859865418,-0.667966561195639,
53.6145226484334));
#167418=CARTESIAN_POINT('Ctrl Pts',(-8.09662574423342,-0.6815608626115,
53.6150627385459));
#167419=CARTESIAN_POINT('Ctrl Pts',(-8.09474584089639,-0.703453446227345,
53.6159306675297));
#167420=CARTESIAN_POINT('Ctrl Pts',(-8.09402025659813,-0.711753515005144,
53.6162592954643));
#167421=CARTESIAN_POINT('Ctrl Pts',(-8.0926143483367,-0.72755571323603,
53.616884127871));
#167422=CARTESIAN_POINT('Ctrl Pts',(-8.09193635585925,-0.735058038497996,
53.617180419709));
#167423=CARTESIAN_POINT('Ctrl Pts',(-8.09036727638708,-0.752155405516818,
53.617854824384));
#167424=CARTESIAN_POINT('Ctrl Pts',(-8.08946955042374,-0.761749837316664,
53.6182326821159));
#167425=CARTESIAN_POINT('Ctrl Pts',(-8.08710127774096,-0.786584329029695,
53.6192091660627));
#167426=CARTESIAN_POINT('Ctrl Pts',(-8.08560471511598,-0.801821911727744,
53.6198067682296));
#167427=CARTESIAN_POINT('Ctrl Pts',(-8.07590900627188,-0.897752685501701,
53.6235590612171));
#167428=CARTESIAN_POINT('Ctrl Pts',(-8.0665451537695,-0.97832329952201,
53.6266642550969));
#167429=CARTESIAN_POINT('Ctrl Pts',(-7.9808792123672,-1.63015319844165,
53.6513915846882));
#167430=CARTESIAN_POINT('Ctrl Pts',(-7.84519476196112,-2.19200057581035,
53.6704387144985));
#167431=CARTESIAN_POINT('Ctrl Pts',(-7.52317004892309,-3.09293663648932,
53.7026340557152));
#167432=CARTESIAN_POINT('Ctrl Pts',(-7.37017093402944,-3.44164338884954,
53.7155355568344));
#167433=CARTESIAN_POINT('Ctrl Pts',(-7.07175799200144,-4.00977104690499,
53.7384189845445));
#167434=CARTESIAN_POINT('Ctrl Pts',(-6.93910643618912,-4.23518762216387,
53.7480331063399));
#167435=CARTESIAN_POINT('Ctrl Pts',(-6.76954146201848,-4.49391761185007,
53.7598605949337));
#167436=CARTESIAN_POINT('Ctrl Pts',(-6.74290170676816,-4.53379130408999,
53.7617063909744));
#167437=CARTESIAN_POINT('Ctrl Pts',(-6.70693207382814,-4.58661140496663,
53.764182958554));
#167438=CARTESIAN_POINT('Ctrl Pts',(-6.69791455914659,-4.59976983968183,
53.7648025440128));
#167439=CARTESIAN_POINT('Ctrl Pts',(-6.68299538066868,-4.62140313709725,
53.7658255435798));
#167440=CARTESIAN_POINT('Ctrl Pts',(-6.67711618734289,-4.62989347970297,
53.7662281485481));
#167441=CARTESIAN_POINT('Ctrl Pts',(-6.66565615059951,-4.64637607887285,
53.7670119112615));
#167442=CARTESIAN_POINT('Ctrl Pts',(-6.66007707842383,-4.65436954839298,
53.7673930047172));
#167443=CARTESIAN_POINT('Ctrl Pts',(-6.64710938159008,-4.67287808423019,
53.768277730539));
#167444=CARTESIAN_POINT('Ctrl Pts',(-6.63971017654716,-4.6833856867158,
53.7687817458024));
#167445=CARTESIAN_POINT('Ctrl Pts',(-6.61571360933007,-4.71729201711857,
53.7704137808348));
#167446=CARTESIAN_POINT('Ctrl Pts',(-6.59901733310505,-4.74062029194703,
53.7715453958729));
#167447=CARTESIAN_POINT('Ctrl Pts',(-6.43646655468301,-4.96521579061872,
53.7825255226603));
#167448=CARTESIAN_POINT('Ctrl Pts',(-6.28158171166152,-5.1597662209341,
53.7927080582552));
#167449=CARTESIAN_POINT('Ctrl Pts',(-5.74159481102126,-5.77762989287939,
53.8273480140395));
#167450=CARTESIAN_POINT('Ctrl Pts',(-5.3207525944797,-6.16736531919509,
53.8531512935697));
#167451=CARTESIAN_POINT('Ctrl Pts',(-4.44069035079091,-6.82474932264212,
53.9026677062644));
#167452=CARTESIAN_POINT('Ctrl Pts',(-3.98914149207106,-7.09815935361309,
53.9262034684646));
#167453=CARTESIAN_POINT('Ctrl Pts',(-3.48899896729561,-7.3380758693166,
53.9483984446961));
#167454=CARTESIAN_POINT('Ctrl Pts',(-3.46369560122287,-7.35005333778223,
53.9495119384426));
#167455=CARTESIAN_POINT('Ctrl Pts',(-3.42852960117716,-7.366477404413,53.9510471099722));
#167456=CARTESIAN_POINT('Ctrl Pts',(-3.4187194247629,-7.37103534601368,
53.9514740479467));
#167457=CARTESIAN_POINT('Ctrl Pts',(-3.40210986448248,-7.37871208205247,
53.9521947013737));
#167458=CARTESIAN_POINT('Ctrl Pts',(-3.3953152398686,-7.38184109435135,
53.9524888862204));
#167459=CARTESIAN_POINT('Ctrl Pts',(-3.38183377594752,-7.38802693091668,
53.9530713795946));
#167460=CARTESIAN_POINT('Ctrl Pts',(-3.37514708995806,-7.39108407080477,
53.9533597021996));
#167461=CARTESIAN_POINT('Ctrl Pts',(-3.36036066512558,-7.397820145331,53.9539959949062));
#167462=CARTESIAN_POINT('Ctrl Pts',(-3.35225900885114,-7.40149486528041,
53.9543437785741));
#167463=CARTESIAN_POINT('Ctrl Pts',(-3.32374531574716,-7.41437158261301,
53.955564870252));
#167464=CARTESIAN_POINT('Ctrl Pts',(-3.30330118722569,-7.42350255390154,
53.9564351128522));
#167465=CARTESIAN_POINT('Ctrl Pts',(-2.96812674576461,-7.57154290765394,
53.9706202156254));
#167466=CARTESIAN_POINT('Ctrl Pts',(-2.64490304387577,-7.69041967842869,
53.9831348263974));
#167467=CARTESIAN_POINT('Ctrl Pts',(-1.75029168147407,-7.95634108712757,
54.0167136835833));
#167468=CARTESIAN_POINT('Ctrl Pts',(-1.16890894714928,-8.0622912723805,
54.0375727501024));
#167469=CARTESIAN_POINT('Ctrl Pts',(-0.176676835861371,-8.13344560927159,
54.0746605155247));
#167470=CARTESIAN_POINT('Ctrl Pts',(0.229420777241419,-8.13212734769299,
54.0901700021729));
#167471=CARTESIAN_POINT('Ctrl Pts',(0.729896328458756,-8.09297531033613,
54.1096013996823));
#167472=CARTESIAN_POINT('Ctrl Pts',(0.825950943604796,-8.08373693700102,
54.1133483580759));
#167473=CARTESIAN_POINT('Ctrl Pts',(0.968565452347753,-8.06745203739496,
54.1189435908539));
#167474=CARTESIAN_POINT('Ctrl Pts',(1.01526583984839,-8.06170804860475,
54.1207809197321));
#167475=CARTESIAN_POINT('Ctrl Pts',(1.09913153172508,-8.05065256276127,
54.1240903654974));
#167476=CARTESIAN_POINT('Ctrl Pts',(1.13631496230111,-8.04548849380078,
54.1255611881129));
#167477=CARTESIAN_POINT('Ctrl Pts',(1.21584084841255,-8.03388155805482,
54.128714828822));
#167478=CARTESIAN_POINT('Ctrl Pts',(1.25817083177055,-8.02736121001849,
54.1303982707186));
#167479=CARTESIAN_POINT('Ctrl Pts',(1.37227592879423,-8.00886017768247,
54.1349498576967));
#167480=CARTESIAN_POINT('Ctrl Pts',(1.44394466066106,-7.99624951405341,
54.1378233522897));
#167481=CARTESIAN_POINT('Ctrl Pts',(1.89348683523406,-7.91090829203186,
54.1559459271916));
#167482=CARTESIAN_POINT('Ctrl Pts',(2.26595581947577,-7.81237446075199,
54.1714180780486));
#167483=CARTESIAN_POINT('Ctrl Pts',(3.0126659260573,-7.55692245166015,54.2034241673218));
#167484=CARTESIAN_POINT('Ctrl Pts',(3.38499690252614,-7.3976369110117,54.219927284617));
#167485=CARTESIAN_POINT('Ctrl Pts',(3.82004468955709,-7.17177128653606,
54.2396220297491));
#167486=CARTESIAN_POINT('Ctrl Pts',(3.89554088451969,-7.1310452423553,54.2430548394567));
#167487=CARTESIAN_POINT('Ctrl Pts',(4.02172702588589,-7.06037272412983,
54.2488126731674));
#167488=CARTESIAN_POINT('Ctrl Pts',(4.07276181134012,-7.03105700376996,
54.2511470433447));
#167489=CARTESIAN_POINT('Ctrl Pts',(4.14438712530256,-6.98887201163811,
54.2544296980245));
#167490=CARTESIAN_POINT('Ctrl Pts',(4.16524512180752,-6.97646111732856,
54.2553864212102));
#167491=CARTESIAN_POINT('Ctrl Pts',(4.20036359491391,-6.95535133882824,
54.2569984343586));
#167492=CARTESIAN_POINT('Ctrl Pts',(4.21465338516476,-6.94670162168263,
54.257654695852));
#167493=CARTESIAN_POINT('Ctrl Pts',(4.24464069325903,-6.9284234903019,54.2590327127431));
#167494=CARTESIAN_POINT('Ctrl Pts',(4.26033236761147,-6.91878564461391,
54.2597542864382));
#167495=CARTESIAN_POINT('Ctrl Pts',(4.30453835918811,-6.89142685985561,
54.261788725878));
#167496=CARTESIAN_POINT('Ctrl Pts',(4.33297586902503,-6.87358238358548,
54.263099418368));
#167497=CARTESIAN_POINT('Ctrl Pts',(4.48010073291159,-6.77998597811191,
54.2698934814721));
#167498=CARTESIAN_POINT('Ctrl Pts',(4.59691600681669,-6.701333925397,54.2753327364994));
#167499=CARTESIAN_POINT('Ctrl Pts',(4.90754315397383,-6.48024185858617,
54.2900199295934));
#167500=CARTESIAN_POINT('Ctrl Pts',(5.09716991908419,-6.33216971881919,
54.2992346229609));
#167501=CARTESIAN_POINT('Ctrl Pts',(5.34771319825525,-6.11797344881262,
54.3119481904637));
#167502=CARTESIAN_POINT('Ctrl Pts',(5.41451794881067,-6.05892984266549,
54.3153935533495));
#167503=CARTESIAN_POINT('Ctrl Pts',(5.53215109279547,-5.95146344872346,
54.3215692070606));
#167504=CARTESIAN_POINT('Ctrl Pts',(5.58334922731551,-5.9034586667603,54.3242953685686));
#167505=CARTESIAN_POINT('Ctrl Pts',(5.66263144601188,-5.82716744779668,
54.3285804460464));
#167506=CARTESIAN_POINT('Ctrl Pts',(5.69114033595974,-5.79932729032866,
54.3301345200194));
#167507=CARTESIAN_POINT('Ctrl Pts',(5.74441198773741,-5.74653410394675,
54.3330639830113));
#167508=CARTESIAN_POINT('Ctrl Pts',(5.76921986082141,-5.72162786977985,
54.3344388234295));
#167509=CARTESIAN_POINT('Ctrl Pts',(5.82522755806615,-5.6646634969339,54.3375673764925));
#167510=CARTESIAN_POINT('Ctrl Pts',(5.85632580090224,-5.63250714422822,
54.3393221752628));
#167511=CARTESIAN_POINT('Ctrl Pts',(5.95338834748967,-5.5304691677471,54.3448559742541));
#167512=CARTESIAN_POINT('Ctrl Pts',(6.0183790741575,-5.45967353919144,54.3486453556684));
#167513=CARTESIAN_POINT('Ctrl Pts',(6.20757599735532,-5.24609347828311,
54.3599339236108));
#167514=CARTESIAN_POINT('Ctrl Pts',(6.32806586628197,-5.10010567051107,
54.3674671502798));
#167515=CARTESIAN_POINT('Ctrl Pts',(6.57137996739337,-4.78338993721634,
54.3834102417702));
#167516=CARTESIAN_POINT('Ctrl Pts',(6.69289812019851,-4.61182924767036,
54.3918194686756));
#167517=CARTESIAN_POINT('Ctrl Pts',(6.86131204173906,-4.35336129611263,
54.4040880818385));
#167518=CARTESIAN_POINT('Ctrl Pts',(6.91349603492676,-4.27000355426077,
54.4079860718544));
#167519=CARTESIAN_POINT('Ctrl Pts',(6.97907978094137,-4.16088601147033,
54.4130030875769));
#167520=CARTESIAN_POINT('Ctrl Pts',(6.99387225281498,-4.13597363511027,
54.4141428264914));
#167521=CARTESIAN_POINT('Ctrl Pts',(7.0185679885778,-4.09387157548053,54.4160590542634));
#167522=CARTESIAN_POINT('Ctrl Pts',(7.02854209568946,-4.07672381928628,
54.4168367541));
#167523=CARTESIAN_POINT('Ctrl Pts',(7.0479523348723,-4.04307023457226,54.4183578259819));
#167524=CARTESIAN_POINT('Ctrl Pts',(7.05739353045289,-4.02656747060298,
54.4191012760194));
#167525=CARTESIAN_POINT('Ctrl Pts',(7.08016606869002,-3.98643600637395,
54.420903484131));
#167526=CARTESIAN_POINT('Ctrl Pts',(7.09343717530291,-3.96277335212363,
54.4219613318108));
#167527=CARTESIAN_POINT('Ctrl Pts',(7.14436662771634,-3.87088946925784,
54.4260514465524));
#167528=CARTESIAN_POINT('Ctrl Pts',(7.18116151213758,-3.80219400696609,
54.4290720116325));
#167529=CARTESIAN_POINT('Ctrl Pts',(7.41042626853166,-3.35895686149777,
54.448357485444));
#167530=CARTESIAN_POINT('Ctrl Pts',(7.57452243004856,-2.97045851589731,
54.4643694992375));
#167531=CARTESIAN_POINT('Ctrl Pts',(7.77144712261527,-2.38008380501974,
54.488336553349));
#167532=CARTESIAN_POINT('Ctrl Pts',(7.82801146504211,-2.18687552143272,
54.4961195618154));
#167533=CARTESIAN_POINT('Ctrl Pts',(7.89543080501839,-1.92023541996281,
54.5068237724786));
#167534=CARTESIAN_POINT('Ctrl Pts',(7.91254248276351,-1.84845964385544,
54.5097013779439));
#167535=CARTESIAN_POINT('Ctrl Pts',(7.94070087922207,-1.72278351086976,
54.5147347202849));
#167536=CARTESIAN_POINT('Ctrl Pts',(7.95218216816694,-1.66898538526603,
54.516887676653));
#167537=CARTESIAN_POINT('Ctrl Pts',(7.9755349218177,-1.55384478924321,54.5214923484539));
#167538=CARTESIAN_POINT('Ctrl Pts',(7.98724692976988,-1.49247357309473,
54.5239447895776));
#167539=CARTESIAN_POINT('Ctrl Pts',(8.02249802562068,-1.29544192400184,
54.5318124285837));
#167540=CARTESIAN_POINT('Ctrl Pts',(8.04329719357104,-1.15931633250214,
54.5372394604156));
#167541=CARTESIAN_POINT('Ctrl Pts',(8.07606386219592,-0.901066095978931,
54.547513096205));
#167542=CARTESIAN_POINT('Ctrl Pts',(8.08874391057554,-0.779069683750958,
54.5523569417624));
#167543=CARTESIAN_POINT('Ctrl Pts',(8.10413328956513,-0.58932085915289,
54.5598675185954));
#167544=CARTESIAN_POINT('Ctrl Pts',(8.10876440015107,-0.521742642218499,
54.5625377387602));
#167545=CARTESIAN_POINT('Ctrl Pts',(8.11550561902531,-0.401313773201119,
54.5672855645311));
#167546=CARTESIAN_POINT('Ctrl Pts',(8.11794568117978,-0.348485494709742,
54.5693646229922));
#167547=CARTESIAN_POINT('Ctrl Pts',(8.12132835570185,-0.255578071603307,
54.573013217846));
#167548=CARTESIAN_POINT('Ctrl Pts',(8.12249040205009,-0.215508905339158,
54.57458408784));
#167549=CARTESIAN_POINT('Ctrl Pts',(8.12461691524859,-0.11704134067931,
54.5784389024037));
#167550=CARTESIAN_POINT('Ctrl Pts',(8.12524832286776,-0.0586380201683644,
54.5807206687261));
#167551=CARTESIAN_POINT('Ctrl Pts',(8.12525491971375,0.171550475355112,
54.589703608444));
#167552=CARTESIAN_POINT('Ctrl Pts',(8.11981210020081,0.343291064673441,
54.5963838175675));
#167553=CARTESIAN_POINT('Ctrl Pts',(8.10033545336368,0.650121364090579,
54.6083574108132));
#167554=CARTESIAN_POINT('Ctrl Pts',(8.08835174174705,0.785275842340364,
54.6136449609056));
#167555=CARTESIAN_POINT('Ctrl Pts',(8.06595498332815,0.981792965271103,
54.6213765104582));
#167556=CARTESIAN_POINT('Ctrl Pts',(8.05821240080725,1.04343667327795,54.6238079401888));
#167557=CARTESIAN_POINT('Ctrl Pts',(8.04227267466351,1.1595567866989,54.6284021290327));
#167558=CARTESIAN_POINT('Ctrl Pts',(8.03422697667461,1.21405048364178,54.6305639763526));
#167559=CARTESIAN_POINT('Ctrl Pts',(8.01400737120932,1.34198142321735,54.635654673723));
#167560=CARTESIAN_POINT('Ctrl Pts',(8.00137718659765,1.41534142009171,54.6385859157454));
#167561=CARTESIAN_POINT('Ctrl Pts',(7.94967077612587,1.69281042539589,54.6497238707111));
#167562=CARTESIAN_POINT('Ctrl Pts',(7.90377761902846,1.89556601208526,54.6579701059781));
#167563=CARTESIAN_POINT('Ctrl Pts',(7.79371943108897,2.30770138678517,54.6749784275962));
#167564=CARTESIAN_POINT('Ctrl Pts',(7.72876273184253,2.5166990655296,54.6837380667358));
#167565=CARTESIAN_POINT('Ctrl Pts',(7.64706873457894,2.74638911102583,54.693496128925));
#167566=CARTESIAN_POINT('Ctrl Pts',(7.63857679674621,2.7699201976613,54.6944973403019));
#167567=CARTESIAN_POINT('Ctrl Pts',(7.62561224975355,2.80533180085954,54.6960062718883));
#167568=CARTESIAN_POINT('Ctrl Pts',(7.6212202501178,2.81724166443451,54.6965141458834));
#167569=CARTESIAN_POINT('Ctrl Pts',(7.54144306083189,3.03202307098823,54.705679831278));
#167570=CARTESIAN_POINT('Ctrl Pts',(7.45800909820819,3.23181519351035,54.7143166417663));
#167571=CARTESIAN_POINT('Ctrl Pts',(7.35024820374394,3.46338837896831,54.724398390452));
#167572=CARTESIAN_POINT('Ctrl Pts',(7.33354439619643,3.4986189176203,54.7259341040434));
#167573=CARTESIAN_POINT('Ctrl Pts',(7.30681650733137,3.55395904038534,54.728348817017));
#167574=CARTESIAN_POINT('Ctrl Pts',(7.29696152200569,3.57414953290101,54.7292303196149));
#167575=CARTESIAN_POINT('Ctrl Pts',(7.27917835967306,3.61020282547512,54.7308051531294));
#167576=CARTESIAN_POINT('Ctrl Pts',(7.27128176127388,3.62608102275784,54.7314989934957));
#167577=CARTESIAN_POINT('Ctrl Pts',(7.25202795780423,3.66448007626066,54.7331774993387));
#167578=CARTESIAN_POINT('Ctrl Pts',(7.24061775785639,3.68697412758726,54.7341611879483));
#167579=CARTESIAN_POINT('Ctrl Pts',(7.19927691140022,3.76754134875716,54.737686770168));
#167580=CARTESIAN_POINT('Ctrl Pts',(7.16875067865304,3.82530648033681,54.7402189113684));
#167581=CARTESIAN_POINT('Ctrl Pts',(7.11024974095552,3.93284827446323,54.7449486534155));
#167582=CARTESIAN_POINT('Ctrl Pts',(7.08244063637543,3.98271033436281,54.7471480212174));
#167583=CARTESIAN_POINT('Ctrl Pts',(6.91596063943906,4.27395233157063,54.7600467535308));
#167584=CARTESIAN_POINT('Ctrl Pts',(6.76548408037174,4.50837071384147,54.7706502379134));
#167585=CARTESIAN_POINT('Ctrl Pts',(6.50139478530221,4.87669166387859,54.7880457239908));
#167586=CARTESIAN_POINT('Ctrl Pts',(6.39495785568427,5.01545300206225,54.7947818405298));
#167587=CARTESIAN_POINT('Ctrl Pts',(6.2488257688162,5.19374291722215,54.8037267873984));
#167588=CARTESIAN_POINT('Ctrl Pts',(6.21308136641001,5.23645002586101,54.8058921952017));
#167589=CARTESIAN_POINT('Ctrl Pts',(6.1552990878859,5.30406318459684,54.8093581709499));
#167590=CARTESIAN_POINT('Ctrl Pts',(6.13354240118779,5.32920732675398,54.8106556001825));
#167591=CARTESIAN_POINT('Ctrl Pts',(6.08808076059829,5.38110003307974,54.8133511958206));
#167592=CARTESIAN_POINT('Ctrl Pts',(6.06435242413952,5.40782715870297,54.8147496004526));
#167593=CARTESIAN_POINT('Ctrl Pts',(6.00756070051975,5.47095237726221,54.8180766800091));
#167594=CARTESIAN_POINT('Ctrl Pts',(5.97434176569944,5.50720854182416,54.8200070548782));
#167595=CARTESIAN_POINT('Ctrl Pts',(5.85357816175083,5.63663504446512,54.8269693346248));
#167596=CARTESIAN_POINT('Ctrl Pts',(5.76416712152762,5.72803708736207,54.8320214866746));
#167597=CARTESIAN_POINT('Ctrl Pts',(5.58711683662652,5.90068481994672,54.8418310596393));
#167598=CARTESIAN_POINT('Ctrl Pts',(5.49976804789478,5.98218246830628,54.8465848177993));
#167599=CARTESIAN_POINT('Ctrl Pts',(5.22557466854112,6.22692564815762,54.8612341714903));
#167600=CARTESIAN_POINT('Ctrl Pts',(5.03302522813126,6.38356416823953,54.8711510601231));
#167601=CARTESIAN_POINT('Ctrl Pts',(4.80191457551451,6.55460593272378,54.8825288926992));
#167602=CARTESIAN_POINT('Ctrl Pts',(4.77004753158206,6.57783316068726,54.8840865404307));
#167603=CARTESIAN_POINT('Ctrl Pts',(4.71857719517437,6.61477808901411,54.8865835918864));
#167604=CARTESIAN_POINT('Ctrl Pts',(4.69908025486382,6.62864274774648,54.8875251893748));
#167605=CARTESIAN_POINT('Ctrl Pts',(4.66432560948276,6.65312706390264,54.8891958274031));
#167606=CARTESIAN_POINT('Ctrl Pts',(4.64909217144247,6.66378084152205,54.8899254406974));
#167607=CARTESIAN_POINT('Ctrl Pts',(4.61601560144214,6.68674490632637,54.8915037931138));
#167608=CARTESIAN_POINT('Ctrl Pts',(4.598159559891,6.69903620970059,54.892352151513));
#167609=CARTESIAN_POINT('Ctrl Pts',(4.54378563311166,6.73614497482338,54.8949245681965));
#167610=CARTESIAN_POINT('Ctrl Pts',(4.50711437256985,6.76073642943636,54.8966445897787));
#167611=CARTESIAN_POINT('Ctrl Pts',(4.42115019818308,6.81737302276155,54.9006440927892));
#167612=CARTESIAN_POINT('Ctrl Pts',(4.37170619913412,6.84918454881104,54.9029198739501));
#167613=CARTESIAN_POINT('Ctrl Pts',(3.96075286205719,7.10732262570993,54.9216494705733));
#167614=CARTESIAN_POINT('Ctrl Pts',(3.58227712442212,7.30540201743851,54.9377415406392));
#167615=CARTESIAN_POINT('Ctrl Pts',(2.81297508839463,7.63380058022156,54.9695405034757));
#167616=CARTESIAN_POINT('Ctrl Pts',(2.42431493264281,7.76597885469104,54.9851957795141));
#167617=CARTESIAN_POINT('Ctrl Pts',(1.95608643892728,7.88662342581524,55.0039757342705));
#167618=CARTESIAN_POINT('Ctrl Pts',(1.88457698294298,7.90401624055325,55.0068410308658));
#167619=CARTESIAN_POINT('Ctrl Pts',(1.77091281975116,7.93003186948286,55.0113924993629));
#167620=CARTESIAN_POINT('Ctrl Pts',(1.72890877170877,7.93929544161359,55.0130738408235));
#167621=CARTESIAN_POINT('Ctrl Pts',(1.65013063668587,7.95601434130762,55.0162262855057));
#167622=CARTESIAN_POINT('Ctrl Pts',(1.6133745850648,7.96354931893501,55.0176967803366));
#167623=CARTESIAN_POINT('Ctrl Pts',(1.53066932644215,7.97990777237776,55.0210049299776));
#167624=CARTESIAN_POINT('Ctrl Pts',(1.48469346556338,7.98858948354417,55.0228434969444));
#167625=CARTESIAN_POINT('Ctrl Pts',(1.3450865663206,8.0137048997076,55.0284254019004));
#167626=CARTESIAN_POINT('Ctrl Pts',(1.25124005771281,8.02889296626107,55.0321764205572));
#167627=CARTESIAN_POINT('Ctrl Pts',(0.766701645013365,8.09860860288,55.0515391838316));
#167628=CARTESIAN_POINT('Ctrl Pts',(0.372689014007289,8.12627747082148,
55.0672063488518));
#167629=CARTESIAN_POINT('Ctrl Pts',(-0.34289161676561,8.12436064912986,
55.096319247919));
#167630=CARTESIAN_POINT('Ctrl Pts',(-0.663673446429851,8.10446396591863,
55.1096228669449));
#167631=CARTESIAN_POINT('Ctrl Pts',(-1.5373082662281,7.9980517858644,55.1466075546246));
#167632=CARTESIAN_POINT('Ctrl Pts',(-2.08372021081485,7.8733883833925,55.1706924029175));
#167633=CARTESIAN_POINT('Ctrl Pts',(-2.68480165772514,7.66924235424176,
55.1964420545646));
#167634=CARTESIAN_POINT('Ctrl Pts',(-2.75626291818493,7.64385068982573,
55.1994877887156));
#167635=CARTESIAN_POINT('Ctrl Pts',(-2.84114273002132,7.6123460051626,55.203078528361));
#167636=CARTESIAN_POINT('Ctrl Pts',(-2.85491217903827,7.60719266011208,
55.2036601754846));
#167637=CARTESIAN_POINT('Ctrl Pts',(-2.87729287426484,7.59874715114003,
55.204604102707));
#167638=CARTESIAN_POINT('Ctrl Pts',(-2.88591260645369,7.59547766635075,
55.2049672913469));
#167639=CARTESIAN_POINT('Ctrl Pts',(-2.90125704990698,7.58962759121779,
55.2056131633811));
#167640=CARTESIAN_POINT('Ctrl Pts',(-2.90798392131558,7.58705271873085,
55.2058960819924));
#167641=CARTESIAN_POINT('Ctrl Pts',(-2.92214022231411,7.58161245976892,
55.2064909777932));
#167642=CARTESIAN_POINT('Ctrl Pts',(-2.92956888516327,7.57874508851252,
55.2068028710785));
#167643=CARTESIAN_POINT('Ctrl Pts',(-2.94914063198376,7.57115756201886,
55.2076238205742));
#167644=CARTESIAN_POINT('Ctrl Pts',(-2.96127662933375,7.56641910174797,
55.2081320878101));
#167645=CARTESIAN_POINT('Ctrl Pts',(-3.01581145079337,7.54497485695481,
55.2104123536861));
#167646=CARTESIAN_POINT('Ctrl Pts',(-3.05808125307775,7.52794151589894,
55.21216969965));
#167647=CARTESIAN_POINT('Ctrl Pts',(-3.39265507183691,7.3898361380272,55.2259858337095));
#167648=CARTESIAN_POINT('Ctrl Pts',(-3.67782491947923,7.25213198888382,
55.2371924239793));
#167649=CARTESIAN_POINT('Ctrl Pts',(-4.44722685057959,6.82351108149312,
55.2673899993585));
#167650=CARTESIAN_POINT('Ctrl Pts',(-4.91025224341217,6.49827517588439,
55.2856005167446));
#167651=CARTESIAN_POINT('Ctrl Pts',(-5.66659133634096,5.83967224588078,
55.3200851109417));
#167652=CARTESIAN_POINT('Ctrl Pts',(-5.97344608767826,5.52538865518179,
55.3358161660439));
#167653=CARTESIAN_POINT('Ctrl Pts',(-6.2737571496323,5.16339736061569,55.3539019320307));
#167654=CARTESIAN_POINT('Ctrl Pts',(-6.29393966021838,5.13877656670567,
55.3551316121641));
#167655=CARTESIAN_POINT('Ctrl Pts',(-6.32187159770565,5.1042907832107,55.3568535728849));
#167656=CARTESIAN_POINT('Ctrl Pts',(-6.32974377103172,5.09452536443244,
55.3573411372647));
#167657=CARTESIAN_POINT('Ctrl Pts',(-6.34329324678662,5.07763737480393,
55.3581842443098));
#167658=CARTESIAN_POINT('Ctrl Pts',(-6.34898125319001,5.070523402047,55.358539377));
#167659=CARTESIAN_POINT('Ctrl Pts',(-6.36072408551017,5.05578593781766,
55.3592750379849));
#167660=CARTESIAN_POINT('Ctrl Pts',(-6.36677719494577,5.04816109986301,
55.3596556307584));
#167661=CARTESIAN_POINT('Ctrl Pts',(-6.38088260977397,5.03032739921414,
55.3605457524435));
#167662=CARTESIAN_POINT('Ctrl Pts',(-6.38892413232806,5.02011006377935,
55.3610556891497));
#167663=CARTESIAN_POINT('Ctrl Pts',(-6.41466302881888,4.98724492173958,
55.3626958628609));
#167664=CARTESIAN_POINT('Ctrl Pts',(-6.43226467724993,4.96452261389915,
55.3638297078879));
#167665=CARTESIAN_POINT('Ctrl Pts',(-6.69254279793944,4.62481663760166,
55.3807798045638));
#167666=CARTESIAN_POINT('Ctrl Pts',(-6.91163133368011,4.29049605428955,
55.397481762485));
#167667=CARTESIAN_POINT('Ctrl Pts',(-7.43295379304438,3.35070995430275,
55.4442273647866));
#167668=CARTESIAN_POINT('Ctrl Pts',(-7.68568069993485,2.72144926764525,
55.47546426592));
#167669=CARTESIAN_POINT('Ctrl Pts',(-7.91968314750162,1.83241794263414,
55.5153206380395));
#167670=CARTESIAN_POINT('Ctrl Pts',(-7.97110905701792,1.59392341402694,
55.5255777670406));
#167671=CARTESIAN_POINT('Ctrl Pts',(-8.01531084491505,1.33226893738488,
55.5361733570518));
#167672=CARTESIAN_POINT('Ctrl Pts',(-8.01880301558406,1.31108606560518,
55.5370269631362));
#167673=CARTESIAN_POINT('Ctrl Pts',(-8.02377739468524,1.28014890325953,
55.5382678151921));
#167674=CARTESIAN_POINT('Ctrl Pts',(-8.0253258401415,1.27040546860291,55.5386577706184));
#167675=CARTESIAN_POINT('Ctrl Pts',(-8.02803401729628,1.25316199048123,
55.539346439498));
#167676=CARTESIAN_POINT('Ctrl Pts',(-8.02920099246855,1.24566310866684,
55.5396454424723));
#167677=CARTESIAN_POINT('Ctrl Pts',(-8.03159842356689,1.23011407745162,
55.5402644375711));
#167678=CARTESIAN_POINT('Ctrl Pts',(-8.03282728697256,1.2220636887081,55.5405843667977));
#167679=CARTESIAN_POINT('Ctrl Pts',(-8.0359559134222,1.20135917002332,55.5414057931157));
#167680=CARTESIAN_POINT('Ctrl Pts',(-8.03783789490505,1.18870234935667,
55.5419066038318));
#167681=CARTESIAN_POINT('Ctrl Pts',(-8.04550795507297,1.13626803710548,
55.543975995905));
#167682=CARTESIAN_POINT('Ctrl Pts',(-8.05103077262727,1.09645194651257,
55.5455346457859));
#167683=CARTESIAN_POINT('Ctrl Pts',(-8.08949968271721,0.803136973157356,
55.556932177959));
#167684=CARTESIAN_POINT('Ctrl Pts',(-8.11076321836762,0.548238389725825,
55.5663763775683));
#167685=CARTESIAN_POINT('Ctrl Pts',(-8.1494928135335,-0.525989991370179,
55.6054683896953));
#167686=CARTESIAN_POINT('Ctrl Pts',(-8.05501936117255,-1.34447685449076,
55.634135299819));
#167687=CARTESIAN_POINT('Ctrl Pts',(-7.81927449074317,-2.21013542941061,
55.6684858824329));
#167688=CARTESIAN_POINT('Ctrl Pts',(-7.79773282169068,-2.2849758915302,
55.6714840406774));
#167689=CARTESIAN_POINT('Ctrl Pts',(-7.76664232282143,-2.38742678497604,
55.6756278248987));
#167690=CARTESIAN_POINT('Ctrl Pts',(-7.75801536502182,-2.41531306677976,
55.6767597791747));
#167691=CARTESIAN_POINT('Ctrl Pts',(-7.74294592405669,-2.46311061742236,
55.6787069143481));
#167692=CARTESIAN_POINT('Ctrl Pts',(-7.73657642861731,-2.48304463455409,
55.6795210518575));
#167693=CARTESIAN_POINT('Ctrl Pts',(-7.72407583305769,-2.52165151156284,
55.6811018465898));
#167694=CARTESIAN_POINT('Ctrl Pts',(-7.71795384489583,-2.54032719669085,
55.6818683647127));
#167695=CARTESIAN_POINT('Ctrl Pts',(-7.70379612539194,-2.58299301474311,
55.6836237854757));
#167696=CARTESIAN_POINT('Ctrl Pts',(-7.69571598805979,-2.60696817790623,
55.6846133063275));
#167697=CARTESIAN_POINT('Ctrl Pts',(-7.67296609160513,-2.67344354111665,
55.6873658459873));
#167698=CARTESIAN_POINT('Ctrl Pts',(-7.65805540371864,-2.71586015961871,
55.6891323500269));
#167699=CARTESIAN_POINT('Ctrl Pts',(-7.6242407406841,-2.809560076873,55.693058418425));
#167700=CARTESIAN_POINT('Ctrl Pts',(-7.60516985278962,-2.86078068651013,
55.6952205065328));
#167701=CARTESIAN_POINT('Ctrl Pts',(-7.45094295529511,-3.26255936846552,
55.7123125074208));
#167702=CARTESIAN_POINT('Ctrl Pts',(-7.29214365340171,-3.6035345337436,
55.7276463139283));
#167703=CARTESIAN_POINT('Ctrl Pts',(-6.7830002427891,-4.52416421359069,
55.7715917645383));
#167704=CARTESIAN_POINT('Ctrl Pts',(-6.38306439301049,-5.07282897109627,
55.8010419421066));
#167705=CARTESIAN_POINT('Ctrl Pts',(-5.90946767918903,-5.5765676541628,
55.8289626428903));
#167706=CARTESIAN_POINT('Ctrl Pts',(-5.89910576315515,-5.58752774051972,
55.82957045944));
#167707=CARTESIAN_POINT('Ctrl Pts',(-5.85913223703797,-5.62957371053287,
55.8319033096499));
#167708=CARTESIAN_POINT('Ctrl Pts',(-5.82930465890093,-5.66045386916352,
55.8336189596199));
#167709=CARTESIAN_POINT('Ctrl Pts',(-5.78967839095846,-5.70083307875243,
55.8358639240323));
#167710=CARTESIAN_POINT('Ctrl Pts',(-5.78009881232172,-5.71054562935977,
55.8364040334341));
#167711=CARTESIAN_POINT('Ctrl Pts',(-5.76521356238555,-5.72556166829836,
55.8372391953913));
#167712=CARTESIAN_POINT('Ctrl Pts',(-5.75992495335559,-5.73088198880345,
55.8375351260863));
#167713=CARTESIAN_POINT('Ctrl Pts',(-5.74933954637718,-5.74150141332026,
55.83812584505));
#167714=CARTESIAN_POINT('Ctrl Pts',(-5.74404277199276,-5.74680053009074,
55.8384206339817));
#167715=CARTESIAN_POINT('Ctrl Pts',(-5.73222283931056,-5.75859302243623,
55.8390766761705));
#167716=CARTESIAN_POINT('Ctrl Pts',(-5.72569595602653,-5.76508266181649,
55.8394377279647));
#167717=CARTESIAN_POINT('Ctrl Pts',(-5.70720188104462,-5.78340881894663,
55.840457325942));
#167718=CARTESIAN_POINT('Ctrl Pts',(-5.69520887529767,-5.79521930130685,
55.8411144404594));
#167719=CARTESIAN_POINT('Ctrl Pts',(-5.60937887075496,-5.87921928882449,
55.8457877036063));
#167720=CARTESIAN_POINT('Ctrl Pts',(-5.53421195294095,-5.95002941592452,
55.8497204248492));
#167721=CARTESIAN_POINT('Ctrl Pts',(-5.3822153303341,-6.08784279986626,
55.8573663618184));
#167722=CARTESIAN_POINT('Ctrl Pts',(-5.30543993508116,-6.15486636356064,
55.8610852528738));
#167723=CARTESIAN_POINT('Ctrl Pts',(-4.91198153066215,-6.48551446248936,
55.8795331863471));
#167724=CARTESIAN_POINT('Ctrl Pts',(-4.57681865562434,-6.72623393890671,
55.8933181545188));
#167725=CARTESIAN_POINT('Ctrl Pts',(-3.63790663158238,-7.29776995294777,
55.9302711589322));
#167726=CARTESIAN_POINT('Ctrl Pts',(-3.00810306977071,-7.5791186369829,
55.953628626276));
#167727=CARTESIAN_POINT('Ctrl Pts',(-2.30904047697838,-7.7903715590882,
55.9815891295643));
#167728=CARTESIAN_POINT('Ctrl Pts',(-2.26755376810707,-7.80254809624716,
55.9832545725002));
#167729=CARTESIAN_POINT('Ctrl Pts',(-2.21072098795639,-7.81873722219118,
55.9855448271214));
#167730=CARTESIAN_POINT('Ctrl Pts',(-2.19545712486625,-7.82303694518714,
55.9861607917615));
#167731=CARTESIAN_POINT('Ctrl Pts',(-2.17124500805291,-7.82978088589587,
55.9871392418767));
#167732=CARTESIAN_POINT('Ctrl Pts',(-2.16230495512371,-7.83225452130359,
55.9875008220774));
#167733=CARTESIAN_POINT('Ctrl Pts',(-2.14497992602915,-7.83701628317341,
55.9882021154146));
#167734=CARTESIAN_POINT('Ctrl Pts',(-2.13659547308613,-7.8393062760449,
55.9885417706599));
#167735=CARTESIAN_POINT('Ctrl Pts',(-2.11665117056621,-7.84471916433469,
55.9893503495815));
#167736=CARTESIAN_POINT('Ctrl Pts',(-2.10508807518004,-7.84782996371639,
55.9898196437291));
#167737=CARTESIAN_POINT('Ctrl Pts',(-2.07081646886335,-7.85696880027689,
55.9912120842996));
#167738=CARTESIAN_POINT('Ctrl Pts',(-2.04808872985772,-7.86292389125557,
55.9921374641323));
#167739=CARTESIAN_POINT('Ctrl Pts',(-1.86563847357267,-7.9098845363327,
55.999582078006));
#167740=CARTESIAN_POINT('Ctrl Pts',(-1.70473351549258,-7.94611603410732,
56.0062467606417));
#167741=CARTESIAN_POINT('Ctrl Pts',(-1.24320039350266,-8.03537705489935,
56.0256574111411));
#167742=CARTESIAN_POINT('Ctrl Pts',(-0.940551602083811,-8.07639597431814,
56.0387456574778));
#167743=CARTESIAN_POINT('Ctrl Pts',(-0.218983071062598,-8.13307983714946,
56.0705906156286));
#167744=CARTESIAN_POINT('Ctrl Pts',(0.200263853118031,-8.13356089963595,
56.089613541702));
#167745=CARTESIAN_POINT('Ctrl Pts',(1.07816644292469,-8.0666315613289,56.1291822371697));
#167746=CARTESIAN_POINT('Ctrl Pts',(1.53491561674973,-7.99231828318995,
56.14959530881));
#167747=CARTESIAN_POINT('Ctrl Pts',(2.01254697376187,-7.87212009879678,
56.1693375757093));
#167748=CARTESIAN_POINT('Ctrl Pts',(2.04212029594849,-7.86450029599521,
56.170553727011));
#167749=CARTESIAN_POINT('Ctrl Pts',(2.08284474932164,-7.85376211394954,
56.1722207175643));
#167750=CARTESIAN_POINT('Ctrl Pts',(2.09403297249518,-7.85078642584977,
56.1726778826741));
#167751=CARTESIAN_POINT('Ctrl Pts',(2.11185495863049,-7.84600557355632,
56.173404878649));
#167752=CARTESIAN_POINT('Ctrl Pts',(2.1184928304322,-7.84421589162311,56.1736753782817));
#167753=CARTESIAN_POINT('Ctrl Pts',(2.13141330219778,-7.84071471854976,
56.1742013818009));
#167754=CARTESIAN_POINT('Ctrl Pts',(2.13769612968913,-7.83900409617749,
56.1744569223436));
#167755=CARTESIAN_POINT('Ctrl Pts',(2.15273871210266,-7.83488903011752,
56.1750681893285));
#167756=CARTESIAN_POINT('Ctrl Pts',(2.16149651632871,-7.83247744252098,
56.1754236160871));
#167757=CARTESIAN_POINT('Ctrl Pts',(2.18781774030315,-7.82518200568449,
56.1764905210807));
#167758=CARTESIAN_POINT('Ctrl Pts',(2.20536885342132,-7.82025371161029,
56.1772001752968));
#167759=CARTESIAN_POINT('Ctrl Pts',(2.34551024136531,-7.78039316920706,
56.1828535174552));
#167760=CARTESIAN_POINT('Ctrl Pts',(2.46728332245264,-7.74263850564397,
56.187686133726));
#167761=CARTESIAN_POINT('Ctrl Pts',(2.85035960308856,-7.61391306115816,
56.2027667160194));
#167762=CARTESIAN_POINT('Ctrl Pts',(3.10793576483658,-7.51245411920426,
56.2127314092396));
#167763=CARTESIAN_POINT('Ctrl Pts',(3.81836550529207,-7.18981095470229,
56.2407122165747));
#167764=CARTESIAN_POINT('Ctrl Pts',(4.25652565444596,-6.93940048920717,
56.2586536535914));
#167765=CARTESIAN_POINT('Ctrl Pts',(5.00822790389797,-6.41166551928036,
56.2927587094915));
#167766=CARTESIAN_POINT('Ctrl Pts',(5.32900554474826,-6.14763984322507,
56.3085862666471));
#167767=CARTESIAN_POINT('Ctrl Pts',(5.70857292842675,-5.78310468659756,
56.328926373727));
#167768=CARTESIAN_POINT('Ctrl Pts',(5.78734592750742,-5.70427309262744,
56.3332485922348));
#167769=CARTESIAN_POINT('Ctrl Pts',(5.89848256171367,-5.58838129907681,
56.3395040260937));
#167770=CARTESIAN_POINT('Ctrl Pts',(5.93217042103995,-5.55260804870382,
56.3414218643622));
#167771=CARTESIAN_POINT('Ctrl Pts',(5.99124531570703,-5.4887249457577,56.3448245520158));
#167772=CARTESIAN_POINT('Ctrl Pts',(6.01676422519282,-5.46073898006491,
56.3463078357722));
#167773=CARTESIAN_POINT('Ctrl Pts',(6.06543322164883,-5.40660953903579,
56.3491630405478));
#167774=CARTESIAN_POINT('Ctrl Pts',(6.08861228823701,-5.3804932178072,56.3505345918358));
#167775=CARTESIAN_POINT('Ctrl Pts',(6.13814215006504,-5.3239570028834,56.353491098669));
#167776=CARTESIAN_POINT('Ctrl Pts',(6.16443672784731,-5.29348911730637,
56.3550766522827));
#167777=CARTESIAN_POINT('Ctrl Pts',(6.2647213375988,-5.17552737701982,56.3611865364457));
#167778=CARTESIAN_POINT('Ctrl Pts',(6.3370833423599,-5.08666800640684,56.3657287357331));
#167779=CARTESIAN_POINT('Ctrl Pts',(6.50787466341803,-4.86763581384776,
56.3767888679848));
#167780=CARTESIAN_POINT('Ctrl Pts',(6.60430830654675,-4.73597105989008,
56.3833256951038));
#167781=CARTESIAN_POINT('Ctrl Pts',(7.01254854543007,-4.1418450403868,56.4123545398637));
#167782=CARTESIAN_POINT('Ctrl Pts',(7.28022082534449,-3.65090335351244,
56.4351960478313));
#167783=CARTESIAN_POINT('Ctrl Pts',(7.5438338686116,-3.02091686176344,56.4626326684866));
#167784=CARTESIAN_POINT('Ctrl Pts',(7.58949460401749,-2.90429690182776,
56.4676346598135));
#167785=CARTESIAN_POINT('Ctrl Pts',(7.6438482206309,-2.75542700515786,56.4739103569023));
#167786=CARTESIAN_POINT('Ctrl Pts',(7.65506235796125,-2.7241170888217,56.475224184652));
#167787=CARTESIAN_POINT('Ctrl Pts',(7.67193958023488,-2.67606854074539,
56.4772308200315));
#167788=CARTESIAN_POINT('Ctrl Pts',(7.67774077721127,-2.65937893480693,
56.4779260487926));
#167789=CARTESIAN_POINT('Ctrl Pts',(7.68931437094285,-2.62572904746364,
56.4793242356882));
#167790=CARTESIAN_POINT('Ctrl Pts',(7.6950851883416,-2.60876838234592,56.4800271776854));
#167791=CARTESIAN_POINT('Ctrl Pts',(7.70683181963275,-2.57386644163167,
56.4814702067843));
#167792=CARTESIAN_POINT('Ctrl Pts',(7.71280119168006,-2.55592310838589,
56.4822101850719));
#167793=CARTESIAN_POINT('Ctrl Pts',(7.72171698176592,-2.52880747040263,
56.483325725167));
#167794=CARTESIAN_POINT('Ctrl Pts',(7.72470980743395,-2.5196505234156,56.4837019788923));
#167795=CARTESIAN_POINT('Ctrl Pts',(7.74835873990877,-2.44685530865725,
56.4866895129049));
#167796=CARTESIAN_POINT('Ctrl Pts',(7.76824449742634,-2.3829690706462,56.4892897268689));
#167797=CARTESIAN_POINT('Ctrl Pts',(7.82714837271466,-2.18515308620252,
56.4972873416449));
#167798=CARTESIAN_POINT('Ctrl Pts',(7.86350860015525,-2.05045814927303,
56.5026581446648));
#167799=CARTESIAN_POINT('Ctrl Pts',(7.96321282977818,-1.63931106426365,
56.5189282563003));
#167800=CARTESIAN_POINT('Ctrl Pts',(8.01556938038562,-1.36042112700604,
56.5298048188836));
#167801=CARTESIAN_POINT('Ctrl Pts',(8.06217360284147,-1.01270340509562,
56.5434073140678));
#167802=CARTESIAN_POINT('Ctrl Pts',(8.07028029365234,-0.945931978640632,
56.5460207023135));
#167803=CARTESIAN_POINT('Ctrl Pts',(8.08180460768298,-0.840037644324885,
56.5501698536874));
#167804=CARTESIAN_POINT('Ctrl Pts',(8.08576925024965,-0.800977264886989,
56.5517012806729));
#167805=CARTESIAN_POINT('Ctrl Pts',(8.09265254853609,-0.72789306859219,
56.5545689145146));
#167806=CARTESIAN_POINT('Ctrl Pts',(8.095640114529,-0.693876586676744,56.5559045404415));
#167807=CARTESIAN_POINT('Ctrl Pts',(8.10118014524423,-0.625882379252799,
56.5585763387248));
#167808=CARTESIAN_POINT('Ctrl Pts',(8.10373348998193,-0.591905408462573,
56.5599124769073));
#167809=CARTESIAN_POINT('Ctrl Pts',(8.10909810953572,-0.513961422844948,
56.562980201026));
#167810=CARTESIAN_POINT('Ctrl Pts',(8.11176565111623,-0.469985633929632,
56.5647128937034));
#167811=CARTESIAN_POINT('Ctrl Pts',(8.12151373445906,-0.284308500723278,
56.5720373795651));
#167812=CARTESIAN_POINT('Ctrl Pts',(8.12523976150824,-0.142458168230421,
56.5776547667235));
#167813=CARTESIAN_POINT('Ctrl Pts',(8.12524997892878,-0.000585164859018793,
56.5832945039328));
#167814=CARTESIAN_POINT('',(8.12525,-6.37027323252548E-13,58.5832974432124));
#167815=CARTESIAN_POINT('Ctrl Pts',(8.12525,-4.61836819862331E-13,56.5832974432124));
#167816=CARTESIAN_POINT('Ctrl Pts',(8.12525000000013,2.24624642433368,56.6712950363536));
#167817=CARTESIAN_POINT('Ctrl Pts',(7.14398562317623,4.47535249753416,56.7592926294948));
#167818=CARTESIAN_POINT('Ctrl Pts',(3.83078204044967,7.50935546634344,56.9352878157772));
#167819=CARTESIAN_POINT('Ctrl Pts',(1.52412477697781,8.29110090552131,57.0232854089184));
#167820=CARTESIAN_POINT('Ctrl Pts',(-2.95101623932528,7.89663306204438,
57.1992805952008));
#167821=CARTESIAN_POINT('Ctrl Pts',(-5.08535169588709,6.72342983085807,
57.287278188342));
#167822=CARTESIAN_POINT('Ctrl Pts',(-7.81671694684393,3.1566195105297,57.4632733746244));
#167823=CARTESIAN_POINT('Ctrl Pts',(-8.392904611467,0.790229551554399,57.5512709677656));
#167824=CARTESIAN_POINT('Ctrl Pts',(-7.60701611462495,-3.63299000730394,
57.727266154048));
#167825=CARTESIAN_POINT('Ctrl Pts',(-6.25093680401372,-5.65606750610003,
57.8152637471892));
#167826=CARTESIAN_POINT('Ctrl Pts',(-2.45807268688572,-8.06369575488313,
57.9912589334716));
#167827=CARTESIAN_POINT('Ctrl Pts',(-0.0502299510454843,-8.42987470330086,
58.0792565266128));
#167828=CARTESIAN_POINT('Ctrl Pts',(4.2868996088099,-7.25863639434566,58.2552517128952));
#167829=CARTESIAN_POINT('Ctrl Pts',(6.18309125557158,-5.73015646266383,
58.3432493060364));
#167830=CARTESIAN_POINT('Ctrl Pts',(7.81050559202891,-2.5864071380029,58.4819304138558));
#167831=CARTESIAN_POINT('Ctrl Pts',(8.1252499999999,-1.29375883538193,58.5326139285341));
#167832=CARTESIAN_POINT('Ctrl Pts',(8.12525,-6.37027053055327E-13,58.5832974432124));
#167833=CARTESIAN_POINT('',(8.1189210508199,-0.00515126165391927,62.5832974432123));
#167834=CARTESIAN_POINT('Ctrl Pts',(8.12524831310126,0.00523573729693267,
58.5811705099486));
#167835=CARTESIAN_POINT('Ctrl Pts',(8.12517639820438,0.116839196648762,
58.5855840757637));
#167836=CARTESIAN_POINT('Ctrl Pts',(8.12280511641629,0.228429150564323,
58.5900170165289));
#167837=CARTESIAN_POINT('Ctrl Pts',(8.09554846868868,0.879357742915142,
58.6160064250618));
#167838=CARTESIAN_POINT('Ctrl Pts',(8.01925291345264,1.41518046884007,58.6379906428653));
#167839=CARTESIAN_POINT('Ctrl Pts',(7.8456709357679,2.12137481707722,58.6674904038425));
#167840=CARTESIAN_POINT('Ctrl Pts',(7.79467526836033,2.30169989202382,58.6750639744105));
#167841=CARTESIAN_POINT('Ctrl Pts',(7.71662152594249,2.54521411760971,58.6853079485774));
#167842=CARTESIAN_POINT('Ctrl Pts',(7.69493002073038,2.61006030061168,58.6880373903059));
#167843=CARTESIAN_POINT('Ctrl Pts',(7.66101751902347,2.7073416043261,58.6921318486831));
#167844=CARTESIAN_POINT('Ctrl Pts',(7.64940336487783,2.73998470227198,58.693505721117));
#167845=CARTESIAN_POINT('Ctrl Pts',(7.63013644960529,2.7930594821971,58.6957390767557));
#167846=CARTESIAN_POINT('Ctrl Pts',(7.62260958606683,2.81353631822115,58.6966006228165));
#167847=CARTESIAN_POINT('Ctrl Pts',(7.60904562803237,2.84998309925561,58.6981337943674));
#167848=CARTESIAN_POINT('Ctrl Pts',(7.60304050095886,2.86596479045633,58.6988059757282));
#167849=CARTESIAN_POINT('Ctrl Pts',(7.59040562475238,2.89927130679426,58.7002065697299));
#167850=CARTESIAN_POINT('Ctrl Pts',(7.58376683666184,2.91659257162282,58.7009348254452));
#167851=CARTESIAN_POINT('Ctrl Pts',(7.56855970114562,2.95586652972008,58.7025859823375));
#167852=CARTESIAN_POINT('Ctrl Pts',(7.55995504196469,2.97780500712256,58.7035082647737));
#167853=CARTESIAN_POINT('Ctrl Pts',(7.53716482510704,3.03517554669036,58.7059204603003));
#167854=CARTESIAN_POINT('Ctrl Pts',(7.52282481877938,3.07054571155132,58.7074080005668));
#167855=CARTESIAN_POINT('Ctrl Pts',(7.44326500322929,3.26287981344836,58.7155032849761));
#167856=CARTESIAN_POINT('Ctrl Pts',(7.37338074734861,3.41787009532359,58.7220513151932));
#167857=CARTESIAN_POINT('Ctrl Pts',(7.20307136067912,3.76600494777748,58.7369582573678));
#167858=CARTESIAN_POINT('Ctrl Pts',(7.0996444986761,3.95753433021788,58.745306083062));
#167859=CARTESIAN_POINT('Ctrl Pts',(6.93023548385204,4.24318749720711,58.7581288463335));
#167860=CARTESIAN_POINT('Ctrl Pts',(6.8697395515003,4.34044723752279,58.7625632697958));
#167861=CARTESIAN_POINT('Ctrl Pts',(6.7813201258849,4.4761180747232,58.7688597814188));
#167862=CARTESIAN_POINT('Ctrl Pts',(6.75508479004031,4.51561348265956,58.7707063442652));
#167863=CARTESIAN_POINT('Ctrl Pts',(6.70963848219389,4.58274717955366,58.7738692413421));
#167864=CARTESIAN_POINT('Ctrl Pts',(6.69059868554859,4.6104999179843,58.7751839201951));
#167865=CARTESIAN_POINT('Ctrl Pts',(6.65025187452325,4.66853386462594,58.7779484252841));
#167866=CARTESIAN_POINT('Ctrl Pts',(6.62890920167816,4.69878933598517,58.7793985716873));
#167867=CARTESIAN_POINT('Ctrl Pts',(6.57387285159557,4.77568780614257,58.7831075219588));
#167868=CARTESIAN_POINT('Ctrl Pts',(6.5398892255511,4.82212060867021,58.7853691163673));
#167869=CARTESIAN_POINT('Ctrl Pts',(6.36558813767213,5.05504113104128,58.7968281630274));
#167870=CARTESIAN_POINT('Ctrl Pts',(6.21777712093239,5.23578059801488,58.8060992719619));
#167871=CARTESIAN_POINT('Ctrl Pts',(5.94843837352386,5.53760430764653,58.8222394875947));
#167872=CARTESIAN_POINT('Ctrl Pts',(5.8304767478359,5.66167125450615,58.8290847258098));
#167873=CARTESIAN_POINT('Ctrl Pts',(5.63631903988984,5.85336972774976,58.8399678629975));
#167874=CARTESIAN_POINT('Ctrl Pts',(5.56261740700668,5.92345484252977,58.8440164441594));
#167875=CARTESIAN_POINT('Ctrl Pts',(5.4551653617551,6.02185976800279,58.8497915404399));
#167876=CARTESIAN_POINT('Ctrl Pts',(5.42247032911268,6.05131719103418,58.8515323651981));
#167877=CARTESIAN_POINT('Ctrl Pts',(5.37054119072963,6.09734526217226,58.8542704580458));
#167878=CARTESIAN_POINT('Ctrl Pts',(5.35146604192433,6.1140938114996,58.8552706191594));
#167879=CARTESIAN_POINT('Ctrl Pts',(5.31833511189125,6.1429099268764,58.8569978108813));
#167880=CARTESIAN_POINT('Ctrl Pts',(5.30431597924443,6.15501931180698,58.8577256047691));
#167881=CARTESIAN_POINT('Ctrl Pts',(5.27678165517953,6.17863885185846,58.8591489703175));
#167882=CARTESIAN_POINT('Ctrl Pts',(5.26326993962654,6.190152844888,58.8598446303911));
#167883=CARTESIAN_POINT('Ctrl Pts',(5.23269824573322,6.21603201615392,58.8614124453043));
#167884=CARTESIAN_POINT('Ctrl Pts',(5.21561662497796,6.23037143212756,58.8622841278934));
#167885=CARTESIAN_POINT('Ctrl Pts',(5.16910103062298,6.26909427178939,58.8646465134454));
#167886=CARTESIAN_POINT('Ctrl Pts',(5.13955363439077,6.29334067977217,58.8661349215696));
#167887=CARTESIAN_POINT('Ctrl Pts',(4.97341868307297,6.42771959657778,58.8744394122587));
#167888=CARTESIAN_POINT('Ctrl Pts',(4.83346157034619,6.53361484987605,58.8811950796788));
#167889=CARTESIAN_POINT('Ctrl Pts',(4.67850676352344,6.64315185392802,58.8884819117514));
#167890=CARTESIAN_POINT('Ctrl Pts',(4.66680683580172,6.65137625219593,58.8890309448283));
#167891=CARTESIAN_POINT('Ctrl Pts',(4.38269759554519,6.84997057429744,58.9023356537205));
#167892=CARTESIAN_POINT('Ctrl Pts',(4.09888596099478,7.02347977651387,58.9150289364623));
#167893=CARTESIAN_POINT('Ctrl Pts',(3.65446067558194,7.25904468311497,58.9344345847304));
#167894=CARTESIAN_POINT('Ctrl Pts',(3.50119302349636,7.33419792147085,58.9410450961357));
#167895=CARTESIAN_POINT('Ctrl Pts',(3.28159910007937,7.4334203897415,58.9504284333985));
#167896=CARTESIAN_POINT('Ctrl Pts',(3.21715146298764,7.4615392346003,58.9531717537745));
#167897=CARTESIAN_POINT('Ctrl Pts',(3.10374022027842,7.50927862605939,58.9579821030075));
#167898=CARTESIAN_POINT('Ctrl Pts',(3.05493529813128,7.52926551130056,58.9600466663165));
#167899=CARTESIAN_POINT('Ctrl Pts',(2.95163296167352,7.57040073213325,58.9644053616558));
#167900=CARTESIAN_POINT('Ctrl Pts',(2.89709489965346,7.59143896106725,58.9666999981994));
#167901=CARTESIAN_POINT('Ctrl Pts',(2.72414353771271,7.65602027560811,58.9739563878941));
#167902=CARTESIAN_POINT('Ctrl Pts',(2.60494088674676,7.69739483554199,58.9789279968587));
#167903=CARTESIAN_POINT('Ctrl Pts',(2.34134770668796,7.78206191617339,58.9898521127108));
#167904=CARTESIAN_POINT('Ctrl Pts',(2.19661740383074,7.82414651867458,58.9958054318505));
#167905=CARTESIAN_POINT('Ctrl Pts',(1.9922889655688,7.8774443066285,59.0041331661356));
#167906=CARTESIAN_POINT('Ctrl Pts',(1.93360857502958,7.8920530934995,59.0065159067674));
#167907=CARTESIAN_POINT('Ctrl Pts',(1.87346085416673,7.90631607020695,59.0089481548735));
#167908=CARTESIAN_POINT('Ctrl Pts',(1.87215113534358,7.9066263033319,59.0090011122884));
#167909=CARTESIAN_POINT('Ctrl Pts',(1.86953208979945,7.90724598945849,59.0091070014892));
#167910=CARTESIAN_POINT('Ctrl Pts',(1.86822276318755,7.90755544272094,59.0091599332747));
#167911=CARTESIAN_POINT('Ctrl Pts',(1.8656041969171,7.90817364202238,59.0092657835395));
#167912=CARTESIAN_POINT('Ctrl Pts',(1.86429495732805,7.90848238817119,59.0093187020179));
#167913=CARTESIAN_POINT('Ctrl Pts',(1.86167624904031,7.90909924807504,59.0094245384235));
#167914=CARTESIAN_POINT('Ctrl Pts',(1.86036678037349,7.90940736178287,59.0094774563488));
#167915=CARTESIAN_POINT('Ctrl Pts',(1.85774728717747,7.91002303348357,59.0095833048255));
#167916=CARTESIAN_POINT('Ctrl Pts',(1.85643726262336,7.91033059127112,59.0096362353749));
#167917=CARTESIAN_POINT('Ctrl Pts',(1.85470348126303,7.91073718110188,59.0097062809692));
#167918=CARTESIAN_POINT('Ctrl Pts',(1.85427979291708,7.91083650453328,59.0097233976647));
#167919=CARTESIAN_POINT('Ctrl Pts',(1.85339565177952,7.91104369499479,59.0097591152349));
#167920=CARTESIAN_POINT('Ctrl Pts',(1.85293519751876,7.91115155587025,59.0097777160754));
#167921=CARTESIAN_POINT('Ctrl Pts',(1.85197463397678,7.91137647830131,59.0098165184163));
#167922=CARTESIAN_POINT('Ctrl Pts',(1.85147452301665,7.91149353263548,59.0098367198748));
#167923=CARTESIAN_POINT('Ctrl Pts',(1.85043157463926,7.91173753741028,59.00987884718));
#167924=CARTESIAN_POINT('Ctrl Pts',(1.84988873526236,7.91186447940296,59.0099007729775));
#167925=CARTESIAN_POINT('Ctrl Pts',(1.84875707272207,7.91212899377904,59.0099464801304));
#167926=CARTESIAN_POINT('Ctrl Pts',(1.84816824723772,7.91226655630618,59.0099702614295));
#167927=CARTESIAN_POINT('Ctrl Pts',(1.84694116460128,7.91255308522884,59.0100198183735));
#167928=CARTESIAN_POINT('Ctrl Pts',(1.84630290477098,7.91270204013126,59.0100455939515));
#167929=CARTESIAN_POINT('Ctrl Pts',(1.84497331089033,7.91301216658495,59.0100992860132));
#167930=CARTESIAN_POINT('Ctrl Pts',(1.84428197373153,7.91317332476599,59.0101272024187));
#167931=CARTESIAN_POINT('Ctrl Pts',(1.84284238426513,7.91350870976285,59.0101853306024));
#167932=CARTESIAN_POINT('Ctrl Pts',(1.84209412833682,7.91368292106043,59.0102155422902));
#167933=CARTESIAN_POINT('Ctrl Pts',(1.84053665857069,7.91404530320573,59.0102784235363));
#167934=CARTESIAN_POINT('Ctrl Pts',(1.83972744055999,7.91423345607052,59.0103110929886));
#167935=CARTESIAN_POINT('Ctrl Pts',(1.8380437987702,7.91462465074278,59.0103790604062));
#167936=CARTESIAN_POINT('Ctrl Pts',(1.83716937017526,7.91482767175841,59.0104143582479));
#167937=CARTESIAN_POINT('Ctrl Pts',(1.83535085093715,7.91524957001853,59.0104877613445));
#167938=CARTESIAN_POINT('Ctrl Pts',(1.83440675472972,7.91546842327834,59.0105258664567));
#167939=CARTESIAN_POINT('Ctrl Pts',(1.83244423187037,7.91592299055131,59.0106050713787));
#167940=CARTESIAN_POINT('Ctrl Pts',(1.83142579884042,7.91615867694652,59.0106461710223));
#167941=CARTESIAN_POINT('Ctrl Pts',(1.82930971754439,7.91664795155981,59.010731560823));
#167942=CARTESIAN_POINT('Ctrl Pts',(1.82821206193691,7.91690150805397,59.0107758507886));
#167943=CARTESIAN_POINT('Ctrl Pts',(1.82593242896765,7.91742759983886,59.0108678257664));
#167944=CARTESIAN_POINT('Ctrl Pts',(1.82475044324223,7.91770009874921,59.0109155105558));
#167945=CARTESIAN_POINT('Ctrl Pts',(1.82229681518712,7.91826518768737,59.0110144886661));
#167946=CARTESIAN_POINT('Ctrl Pts',(1.82102516329836,7.91855773609168,59.0110657817302));
#167947=CARTESIAN_POINT('Ctrl Pts',(1.81838663144945,7.9191640712823,59.0111721991246));
#167948=CARTESIAN_POINT('Ctrl Pts',(1.8170197405945,7.91947781053858,59.0112273231591));
#167949=CARTESIAN_POINT('Ctrl Pts',(1.81418491251236,7.92012770942205,59.0113416348503));
#167950=CARTESIAN_POINT('Ctrl Pts',(1.81271696291293,7.92046381487289,59.011400822166));
#167951=CARTESIAN_POINT('Ctrl Pts',(1.80967394008507,7.92115966278591,59.0115235028407));
#167952=CARTESIAN_POINT('Ctrl Pts',(1.8080988528043,7.92151934361447,59.0115869958082));
#167953=CARTESIAN_POINT('Ctrl Pts',(1.80483520448675,7.92226359358714,59.0117185407826));
#167954=CARTESIAN_POINT('Ctrl Pts',(1.80314662755011,7.92264809272674,59.0117865923393));
#167955=CARTESIAN_POINT('Ctrl Pts',(1.76554242181326,7.93119815210983,59.0133018963152));
#167956=CARTESIAN_POINT('Ctrl Pts',(1.7295717167814,7.93911996776487,59.0147475443942));
#167957=CARTESIAN_POINT('Ctrl Pts',(1.64670008571176,7.9567808076879,59.0180688043332));
#167958=CARTESIAN_POINT('Ctrl Pts',(1.59976440767895,7.96635022167018,59.0199431663738));
#167959=CARTESIAN_POINT('Ctrl Pts',(1.2743947319643,8.02969627556278,59.0328983584521));
#167960=CARTESIAN_POINT('Ctrl Pts',(0.993395927647598,8.06927937728133,
59.0438996042274));
#167961=CARTESIAN_POINT('Ctrl Pts',(0.626014712685072,8.10154644718201,
59.0582869832803));
#167962=CARTESIAN_POINT('Ctrl Pts',(0.541014108906461,8.10766630546251,
59.0616154960695));
#167963=CARTESIAN_POINT('Ctrl Pts',(0.402785371362971,8.11543499276543,
59.0670337438848));
#167964=CARTESIAN_POINT('Ctrl Pts',(0.34960956935855,8.11789962395833,59.0691193917072));
#167965=CARTESIAN_POINT('Ctrl Pts',(0.269876817884071,8.12081025510544,
59.0722496580054));
#167966=CARTESIAN_POINT('Ctrl Pts',(0.24333557722588,8.12164887754905,59.0732921508082));
#167967=CARTESIAN_POINT('Ctrl Pts',(0.208106929980383,8.12258915188453,
59.0746766355035));
#167968=CARTESIAN_POINT('Ctrl Pts',(0.199422766000694,8.12280700157982,
59.0750179845692));
#167969=CARTESIAN_POINT('Ctrl Pts',(0.118948716521843,8.12469663109209,
59.0781817799492));
#167970=CARTESIAN_POINT('Ctrl Pts',(0.0471401921666107,8.12543056615178,
59.0810093219135));
#167971=CARTESIAN_POINT('Ctrl Pts',(-0.20714062953554,8.12465856179557,
59.0910420715853));
#167972=CARTESIAN_POINT('Ctrl Pts',(-0.389540940211746,8.11795792411037,
59.0982766459217));
#167973=CARTESIAN_POINT('Ctrl Pts',(-0.942294311702755,8.07897870548056,
59.1203444063101));
#167974=CARTESIAN_POINT('Ctrl Pts',(-1.31079637625268,8.02742959643593,
59.135269770985));
#167975=CARTESIAN_POINT('Ctrl Pts',(-1.76517645901725,7.93173574998711,
59.1537872496946));
#167976=CARTESIAN_POINT('Ctrl Pts',(-1.8555487450105,7.91108203533322,59.1574746838856));
#167977=CARTESIAN_POINT('Ctrl Pts',(-1.98785592553225,7.87845258841415,
59.1628733588026));
#167978=CARTESIAN_POINT('Ctrl Pts',(-2.03007914073925,7.86767850619569,
59.1645962537011));
#167979=CARTESIAN_POINT('Ctrl Pts',(-2.09781448000107,7.84981292515265,
59.1673593458153));
#167980=CARTESIAN_POINT('Ctrl Pts',(-2.12338208731236,7.84293548809502,
59.1684021243841));
#167981=CARTESIAN_POINT('Ctrl Pts',(-2.1680709757334,7.83068006799212,59.170224222229));
#167982=CARTESIAN_POINT('Ctrl Pts',(-2.18720698095181,7.82535671446688,
59.1710042780461));
#167983=CARTESIAN_POINT('Ctrl Pts',(-2.22551015953701,7.81454986113021,
59.172565199465));
#167984=CARTESIAN_POINT('Ctrl Pts',(-2.24467706129464,7.80906587859042,
59.173346052295));
#167985=CARTESIAN_POINT('Ctrl Pts',(-2.28479759050127,7.79742678469476,
59.1749799438289));
#167986=CARTESIAN_POINT('Ctrl Pts',(-2.30574690615566,7.79125764567903,
59.1758327192332));
#167987=CARTESIAN_POINT('Ctrl Pts',(-2.36789795393136,7.77268282505951,
59.17836169248));
#167988=CARTESIAN_POINT('Ctrl Pts',(-2.40902633978774,7.76003422317414,
59.1800340612331));
#167989=CARTESIAN_POINT('Ctrl Pts',(-2.62815632246915,7.69073309558562,
59.1889442195982));
#167990=CARTESIAN_POINT('Ctrl Pts',(-2.80426671610509,7.62828098713956,
59.1961062011256));
#167991=CARTESIAN_POINT('Ctrl Pts',(-3.1270413609876,7.50112901419255,59.2093880004823));
#167992=CARTESIAN_POINT('Ctrl Pts',(-3.27424594026636,7.43805334788783,
59.2155073190374));
#167993=CARTESIAN_POINT('Ctrl Pts',(-3.53748853251465,7.31592665324726,
59.2266361830694));
#167994=CARTESIAN_POINT('Ctrl Pts',(-3.65415432155833,7.25835820050681,
59.2316367364208));
#167995=CARTESIAN_POINT('Ctrl Pts',(-3.85206786767999,7.15471672900817,
59.2402649880761));
#167996=CARTESIAN_POINT('Ctrl Pts',(-3.93399596570049,7.10999816416011,
59.2438806966601));
#167997=CARTESIAN_POINT('Ctrl Pts',(-4.05361217227407,7.04200786180014,
59.2492308977332));
#167998=CARTESIAN_POINT('Ctrl Pts',(-4.09190982239516,7.0198233847916,59.2509548245374));
#167999=CARTESIAN_POINT('Ctrl Pts',(-4.15902370420061,6.98021083709141,
59.2539957817299));
#168000=CARTESIAN_POINT('Ctrl Pts',(-4.18791645523312,6.9629144226491,59.2553114960037));
#168001=CARTESIAN_POINT('Ctrl Pts',(-4.2497020330876,6.92540328801208,59.2581394609702));
#168002=CARTESIAN_POINT('Ctrl Pts',(-4.28255997790765,6.90513273539684,
59.2596522308104));
#168003=CARTESIAN_POINT('Ctrl Pts',(-4.37032702626561,6.85012051796895,
59.2637171308492));
#168004=CARTESIAN_POINT('Ctrl Pts',(-4.42496579079804,6.81495319969432,
59.2662733153385));
#168005=CARTESIAN_POINT('Ctrl Pts',(-4.65862133612102,6.66057000033471,
59.2773168565769));
#168006=CARTESIAN_POINT('Ctrl Pts',(-4.83328585317899,6.53492858624563,
59.2858633508653));
#168007=CARTESIAN_POINT('Ctrl Pts',(-5.14542407679601,6.29103163774024,
59.3016535114714));
#168008=CARTESIAN_POINT('Ctrl Pts',(-5.28432440690271,6.17481851671146,
59.3088842936542));
#168009=CARTESIAN_POINT('Ctrl Pts',(-5.46507540606076,6.01302127662469,
59.3185288515002));
#168010=CARTESIAN_POINT('Ctrl Pts',(-5.51045682054391,5.97146043681014,
59.3209710186146));
#168011=CARTESIAN_POINT('Ctrl Pts',(-5.57888727382927,5.90734657992605,
59.324682536134));
#168012=CARTESIAN_POINT('Ctrl Pts',(-5.60228133131514,5.88516530987907,
59.3259566494335));
#168013=CARTESIAN_POINT('Ctrl Pts',(-5.6435284955051,5.84558765187151,59.3282119643844));
#168014=CARTESIAN_POINT('Ctrl Pts',(-5.66143470810622,5.82824724310359,
59.3291940470956));
#168015=CARTESIAN_POINT('Ctrl Pts',(-5.69330490854421,5.79709862086708,
59.3309471322092));
#168016=CARTESIAN_POINT('Ctrl Pts',(-5.7072991557919,5.78332167107031,59.3317187046542));
#168017=CARTESIAN_POINT('Ctrl Pts',(-5.73329025026406,5.75754794224224,
59.3331549323709));
#168018=CARTESIAN_POINT('Ctrl Pts',(-5.74529972021392,5.74556407403909,
59.3338198388954));
#168019=CARTESIAN_POINT('Ctrl Pts',(-5.77398545076476,5.71675962397565,
59.3354110584742));
#168020=CARTESIAN_POINT('Ctrl Pts',(-5.79062585951541,5.69990357328113,
59.336336614615));
#168021=CARTESIAN_POINT('Ctrl Pts',(-5.85388624917053,5.63526044983365,
59.3398653112408));
#168022=CARTESIAN_POINT('Ctrl Pts',(-5.89999058582909,5.58697196639273,
59.3424581262394));
#168023=CARTESIAN_POINT('Ctrl Pts',(-5.95571411938024,5.52714950828046,
59.3456216211734));
#168024=CARTESIAN_POINT('Ctrl Pts',(-5.96590302162596,5.51615024236272,
59.3462012976702));
#168025=CARTESIAN_POINT('Ctrl Pts',(-6.26436743077006,5.19215353939417,
59.3632192968626));
#168026=CARTESIAN_POINT('Ctrl Pts',(-6.52764693208651,4.85701489405826,
59.3792790636033));
#168027=CARTESIAN_POINT('Ctrl Pts',(-6.99716044568987,4.15177805421225,
59.4114802274014));
#168028=CARTESIAN_POINT('Ctrl Pts',(-7.2031682621337,3.78310348790634,59.4275758609787));
#168029=CARTESIAN_POINT('Ctrl Pts',(-7.40190662686562,3.35176079300264,
59.4460235178255));
#168030=CARTESIAN_POINT('Ctrl Pts',(-7.42370998418252,3.30318818206961,
59.4480952492352));
#168031=CARTESIAN_POINT('Ctrl Pts',(-7.46051997127221,3.21897874192921,
59.4516779830287));
#168032=CARTESIAN_POINT('Ctrl Pts',(-7.47575253349082,3.18344254369155,
59.4531871529378));
#168033=CARTESIAN_POINT('Ctrl Pts',(-7.5055482448697,3.11253850860205,59.456193162822));
#168034=CARTESIAN_POINT('Ctrl Pts',(-7.52011645598667,3.07717384962502,
59.4576899235039));
#168035=CARTESIAN_POINT('Ctrl Pts',(-7.54849214588069,3.00688610544065,
59.4606599320223));
#168036=CARTESIAN_POINT('Ctrl Pts',(-7.56230829711621,2.97196751944103,
59.4621330770831));
#168037=CARTESIAN_POINT('Ctrl Pts',(-7.59294888873917,2.89293003211595,
59.4654624123954));
#168038=CARTESIAN_POINT('Ctrl Pts',(-7.60963180729591,2.84875775306758,
59.4673195440113));
#168039=CARTESIAN_POINT('Ctrl Pts',(-7.66709289784579,2.69250774835765,
59.4738766236124));
#168040=CARTESIAN_POINT('Ctrl Pts',(-7.70578737788031,2.57968061904721,
59.4785897004082));
#168041=CARTESIAN_POINT('Ctrl Pts',(-7.93796827582238,1.8507636398737,59.5089030704495));
#168042=CARTESIAN_POINT('Ctrl Pts',(-8.05989870723231,1.214348575592,59.5348486980382));
#168043=CARTESIAN_POINT('Ctrl Pts',(-8.14252652616689,0.039914066182005,
59.5842067721203));
#168044=CARTESIAN_POINT('Ctrl Pts',(-8.12769819033082,-0.492782213575494,
59.6070710319487));
#168045=CARTESIAN_POINT('Ctrl Pts',(-8.04442315318636,-1.15076697046135,
59.6343405564969));
#168046=CARTESIAN_POINT('Ctrl Pts',(-8.02472805810492,-1.28091764975282,
59.6396779210998));
#168047=CARTESIAN_POINT('Ctrl Pts',(-7.9987968435175,-1.42802379475317,
59.645606815264));
#168048=CARTESIAN_POINT('Ctrl Pts',(-7.99565676758626,-1.44550190702236,
59.6463095647355));
#168049=CARTESIAN_POINT('Ctrl Pts',(-7.99084120059462,-1.47181019253954,
59.6473646815934));
#168050=CARTESIAN_POINT('Ctrl Pts',(-7.98920832673511,-1.48064805029021,
59.6477186770873));
#168051=CARTESIAN_POINT('Ctrl Pts',(-7.9863696512218,-1.49587084245384,
59.6483276132234));
#168052=CARTESIAN_POINT('Ctrl Pts',(-7.98517084967779,-1.50225706356726,
59.6485828282269));
#168053=CARTESIAN_POINT('Ctrl Pts',(-7.98268105076628,-1.51543346180957,
59.6491088882593));
#168054=CARTESIAN_POINT('Ctrl Pts',(-7.98138904706195,-1.52222344457988,
59.6493796928077));
#168055=CARTESIAN_POINT('Ctrl Pts',(-7.97824966358184,-1.53860824807813,
59.6500324738051));
#168056=CARTESIAN_POINT('Ctrl Pts',(-7.9763936345962,-1.54820141537254,
59.6504140975156));
#168057=CARTESIAN_POINT('Ctrl Pts',(-7.96948600636523,-1.5835623932717,
59.6518186080484));
#168058=CARTESIAN_POINT('Ctrl Pts',(-7.96432677457999,-1.60930920234527,
59.6528369868329));
#168059=CARTESIAN_POINT('Ctrl Pts',(-7.8818453352122,-2.01081437587897,
59.6686464048692));
#168060=CARTESIAN_POINT('Ctrl Pts',(-7.77812968353715,-2.3806656808802,
59.6821215020093));
#168061=CARTESIAN_POINT('Ctrl Pts',(-7.4645410449366,-3.25546685099195,
59.7137134929888));
#168062=CARTESIAN_POINT('Ctrl Pts',(-7.22913812289554,-3.7492683997744,
59.7313928219961));
#168063=CARTESIAN_POINT('Ctrl Pts',(-6.73128452625287,-4.5695491060633,
59.7645459658327));
#168064=CARTESIAN_POINT('Ctrl Pts',(-6.48985689610431,-4.90639207327964,
59.7794574271049));
#168065=CARTESIAN_POINT('Ctrl Pts',(-6.2029620518516,-5.24823816199646,
59.7966180179185));
#168066=CARTESIAN_POINT('Ctrl Pts',(-6.18193817944885,-5.27298609311895,
59.7978724119289));
#168067=CARTESIAN_POINT('Ctrl Pts',(-6.15185584776279,-5.30796985474002,
59.7996630137157));
#168068=CARTESIAN_POINT('Ctrl Pts',(-6.14291892634242,-5.31831001472116,
59.8001944408744));
#168069=CARTESIAN_POINT('Ctrl Pts',(-6.1274948305561,-5.33606519160659,
59.8011107298327));
#168070=CARTESIAN_POINT('Ctrl Pts',(-6.12102016774566,-5.34349106229028,
59.8014950968996));
#168071=CARTESIAN_POINT('Ctrl Pts',(-6.10863493613453,-5.35764378853692,
59.8022298368414));
#168072=CARTESIAN_POINT('Ctrl Pts',(-6.10272671912686,-5.36437268828977,
59.8025801162743));
#168073=CARTESIAN_POINT('Ctrl Pts',(-6.08891647591992,-5.38004890389295,
59.8033983766707));
#168074=CARTESIAN_POINT('Ctrl Pts',(-6.08100584135918,-5.3889885892341,
59.8038666997749));
#168075=CARTESIAN_POINT('Ctrl Pts',(-6.0530310297287,-5.42046245966269,
59.8055215208989));
#168076=CARTESIAN_POINT('Ctrl Pts',(-6.03286117932124,-5.44290215699766,
59.8067122357431));
#168077=CARTESIAN_POINT('Ctrl Pts',(-5.80624333030887,-5.69221559395739,
59.8200644011216));
#168078=CARTESIAN_POINT('Ctrl Pts',(-5.58724796413447,-5.90731880299207,
59.8327403495164));
#168079=CARTESIAN_POINT('Ctrl Pts',(-4.88342893180304,-6.52440518962173,
59.8727616542604));
#168080=CARTESIAN_POINT('Ctrl Pts',(-4.36364372775441,-6.88289445994197,
59.9015269300672));
#168081=CARTESIAN_POINT('Ctrl Pts',(-3.64323174787055,-7.26507038820137,
59.9377466407012));
#168082=CARTESIAN_POINT('Ctrl Pts',(-3.4757203903129,-7.3466834564493,59.9459221489585));
#168083=CARTESIAN_POINT('Ctrl Pts',(-3.21601039246639,-7.46234356474603,
59.9580930532736));
#168084=CARTESIAN_POINT('Ctrl Pts',(-3.12575717343265,-7.50059580841624,
59.9622323647537));
#168085=CARTESIAN_POINT('Ctrl Pts',(-2.9394603794391,-7.57560760137472,
59.9705645527356));
#168086=CARTESIAN_POINT('Ctrl Pts',(-2.84337236156653,-7.6121937065427,
59.9747445293338));
#168087=CARTESIAN_POINT('Ctrl Pts',(-2.73051069950441,-7.65273097270264,
59.9795198334238));
#168088=CARTESIAN_POINT('Ctrl Pts',(-2.71439768662875,-7.6584610220005,
59.9801985636401));
#168089=CARTESIAN_POINT('Ctrl Pts',(-2.68968960568818,-7.66715984384577,
59.9812348592112));
#168090=CARTESIAN_POINT('Ctrl Pts',(-2.68110750429582,-7.6701651088701,
59.981593978953));
#168091=CARTESIAN_POINT('Ctrl Pts',(-2.66613321978502,-7.67538057435653,
59.9822191650092));
#168092=CARTESIAN_POINT('Ctrl Pts',(-2.65974329901191,-7.67759720814684,
59.982485499397));
#168093=CARTESIAN_POINT('Ctrl Pts',(-2.64537098649015,-7.68256280035275,
59.9830835475612));
#168094=CARTESIAN_POINT('Ctrl Pts',(-2.63738705574452,-7.68530730396571,
59.9834150783817));
#168095=CARTESIAN_POINT('Ctrl Pts',(-2.61602531767918,-7.69261326673342,
59.9843003074837));
#168096=CARTESIAN_POINT('Ctrl Pts',(-2.60263982886829,-7.69715228240273,
59.9848531032011));
#168097=CARTESIAN_POINT('Ctrl Pts',(-2.54465803824693,-7.7166453511911,
59.987239669946));
#168098=CARTESIAN_POINT('Ctrl Pts',(-2.49994371702045,-7.73124708715311,
59.9890597583787));
#168099=CARTESIAN_POINT('Ctrl Pts',(-2.37823574098254,-7.76982527599007,
59.9939640395288));
#168100=CARTESIAN_POINT('Ctrl Pts',(-2.30100708425179,-7.79304541804587,
59.997022238823));
#168101=CARTESIAN_POINT('Ctrl Pts',(-2.15937250927729,-7.83334126813685,
60.0025506266885));
#168102=CARTESIAN_POINT('Ctrl Pts',(-2.09507818407863,-7.8507816583953,
60.0050303494735));
#168103=CARTESIAN_POINT('Ctrl Pts',(-1.61517915015586,-7.97464313812339,
60.0233561451848));
#168104=CARTESIAN_POINT('Ctrl Pts',(-1.19193274729973,-8.04879214485667,
60.0385434078481));
#168105=CARTESIAN_POINT('Ctrl Pts',(-0.465948569070224,-8.11743133820707,
60.0648236965058));
#168106=CARTESIAN_POINT('Ctrl Pts',(-0.165766683720586,-8.12910289491409,
60.075746083675));
#168107=CARTESIAN_POINT('Ctrl Pts',(0.373160939472013,-8.120189442957,60.0958253469322));
#168108=CARTESIAN_POINT('Ctrl Pts',(0.611657436581887,-8.10571373840304,
60.1048741211254));
#168109=CARTESIAN_POINT('Ctrl Pts',(0.894816408537628,-8.07595804100068,
60.1158538008365));
#168110=CARTESIAN_POINT('Ctrl Pts',(0.9404267494293,-8.07077395143491,60.117629545636));
#168111=CARTESIAN_POINT('Ctrl Pts',(1.0114116462029,-8.06209587745681,60.1204043658754));
#168112=CARTESIAN_POINT('Ctrl Pts',(1.03681788903874,-8.05886791763399,
60.1213997357525));
#168113=CARTESIAN_POINT('Ctrl Pts',(1.08377055353067,-8.05267669541091,
60.1232433613864));
#168114=CARTESIAN_POINT('Ctrl Pts',(1.10532120207574,-8.0497469282953,60.1240911541939));
#168115=CARTESIAN_POINT('Ctrl Pts',(1.15123488338224,-8.04331720154573,
60.1259008230983));
#168116=CARTESIAN_POINT('Ctrl Pts',(1.17559431982952,-8.03979299178773,
60.1268630268368));
#168117=CARTESIAN_POINT('Ctrl Pts',(1.2407801075633,-8.03005962701958,60.1294437409101));
#168118=CARTESIAN_POINT('Ctrl Pts',(1.28157564139201,-8.02364983878517,
60.1310650082413));
#168119=CARTESIAN_POINT('Ctrl Pts',(1.46542766922892,-7.99332510095756,
60.1384013311545));
#168120=CARTESIAN_POINT('Ctrl Pts',(1.60787466974781,-7.96589367899812,
60.1441676671664));
#168121=CARTESIAN_POINT('Ctrl Pts',(1.88031086007134,-7.90582440702586,
60.155380815686));
#168122=CARTESIAN_POINT('Ctrl Pts',(2.01037739300699,-7.87375451079556,
60.1608165218205));
#168123=CARTESIAN_POINT('Ctrl Pts',(2.36061578150293,-7.77815357524732,
60.1756896800348));
#168124=CARTESIAN_POINT('Ctrl Pts',(2.57898525312594,-7.70850245319125,
60.185222346982));
#168125=CARTESIAN_POINT('Ctrl Pts',(3.04702246722017,-7.53710038884906,
60.2061817216031));
#168126=CARTESIAN_POINT('Ctrl Pts',(3.29516675451728,-7.43196483340922,
60.2176363306343));
#168127=CARTESIAN_POINT('Ctrl Pts',(3.7852460693421,-7.1949465738268,60.2407137793849));
#168128=CARTESIAN_POINT('Ctrl Pts',(4.02663034233093,-7.06269067610335,
60.2523200457162));
#168129=CARTESIAN_POINT('Ctrl Pts',(4.3560101466378,-6.85983631708373,60.2681792884972));
#168130=CARTESIAN_POINT('Ctrl Pts',(4.44995721182366,-6.79926913172143,
60.2727043118282));
#168131=CARTESIAN_POINT('Ctrl Pts',(4.55729139929475,-6.72689345013379,
60.277853420046));
#168132=CARTESIAN_POINT('Ctrl Pts',(4.57192361571225,-6.716957260947,60.2785549084256));
#168133=CARTESIAN_POINT('Ctrl Pts',(4.59413112549058,-6.70177078906364,
60.2796187437192));
#168134=CARTESIAN_POINT('Ctrl Pts',(4.6017300743744,-6.6965552958806,60.2799826188173));
#168135=CARTESIAN_POINT('Ctrl Pts',(4.61549099049545,-6.68707608955959,
60.2806412707466));
#168136=CARTESIAN_POINT('Ctrl Pts',(4.62165595963973,-6.68281676406811,
60.2809362452689));
#168137=CARTESIAN_POINT('Ctrl Pts',(4.6339700651062,-6.67428386219464,60.2815252133562));
#168138=CARTESIAN_POINT('Ctrl Pts',(4.64011920309531,-6.67001030126386,
60.2818192071481));
#168139=CARTESIAN_POINT('Ctrl Pts',(4.65741955220217,-6.65795130945561,
60.2826460139374));
#168140=CARTESIAN_POINT('Ctrl Pts',(4.66855716753571,-6.6501463518201,60.2831779053486));
#168141=CARTESIAN_POINT('Ctrl Pts',(4.71436248197956,-6.61787536747372,
60.2853636300905));
#168142=CARTESIAN_POINT('Ctrl Pts',(4.74885827629627,-6.59316563983728,
60.2870055083312));
#168143=CARTESIAN_POINT('Ctrl Pts',(5.42577472048383,-6.10021386232247,
60.319117905093));
#168144=CARTESIAN_POINT('Ctrl Pts',(5.99628601953395,-5.5404330838178,60.3442318471266));
#168145=CARTESIAN_POINT('Ctrl Pts',(6.69034809712383,-4.62432950240726,
60.383559920268));
#168146=CARTESIAN_POINT('Ctrl Pts',(6.88556738290989,-4.32829298294416,
60.3960108975434));
#168147=CARTESIAN_POINT('Ctrl Pts',(7.13490191877061,-3.890406886666,60.4146729180675));
#168148=CARTESIAN_POINT('Ctrl Pts',(7.20535389791209,-3.75831926306457,
60.4203287834228));
#168149=CARTESIAN_POINT('Ctrl Pts',(7.28235312750977,-3.60382397219841,
60.4269944232643));
#168150=CARTESIAN_POINT('Ctrl Pts',(7.29250342731437,-3.58323988155288,
60.4278835105397));
#168151=CARTESIAN_POINT('Ctrl Pts',(7.307766978784,-3.55195298847042,60.4292364571187));
#168152=CARTESIAN_POINT('Ctrl Pts',(7.31294426415695,-3.54128146811638,
60.4296982047086));
#168153=CARTESIAN_POINT('Ctrl Pts',(7.32226617083568,-3.52195935470619,
60.4305347659852));
#168154=CARTESIAN_POINT('Ctrl Pts',(7.32641888008075,-3.51331267688973,
60.4309093127197));
#168155=CARTESIAN_POINT('Ctrl Pts',(7.33467401194234,-3.49604574335888,
60.4316576345313));
#168156=CARTESIAN_POINT('Ctrl Pts',(7.33877657325894,-3.48742557027033,
60.43203140426));
#168157=CARTESIAN_POINT('Ctrl Pts',(7.35023308661733,-3.46324376560453,
60.4330804500256));
#168158=CARTESIAN_POINT('Ctrl Pts',(7.35755277856995,-3.44766600960279,
60.4337568471992));
#168159=CARTESIAN_POINT('Ctrl Pts',(7.38714915755802,-3.38415553453078,
60.4365170510512));
#168160=CARTESIAN_POINT('Ctrl Pts',(7.40900713264573,-3.33602975677801,
60.438614498745));
#168161=CARTESIAN_POINT('Ctrl Pts',(7.81088310252495,-2.42776515590612,
60.4783150648214));
#168162=CARTESIAN_POINT('Ctrl Pts',(8.03915331135233,-1.50839245211736,
60.5214962649045));
#168163=CARTESIAN_POINT('Ctrl Pts',(8.11850364623206,-0.381530010472146,
60.5718018417503));
#168164=CARTESIAN_POINT('Ctrl Pts',(8.1251981936156,-0.191901387870314,
60.5801413526158));
#168165=CARTESIAN_POINT('Ctrl Pts',(8.12530306403285,0.194326991449929,
60.5966839027687));
#168166=CARTESIAN_POINT('Ctrl Pts',(8.11822602146609,0.390818134203802,
60.6048590059351));
#168167=CARTESIAN_POINT('Ctrl Pts',(8.10272852958194,0.604814845894541,
60.6134027297524));
#168168=CARTESIAN_POINT('Ctrl Pts',(8.1013707875472,0.622737498476672,60.6141157964287));
#168169=CARTESIAN_POINT('Ctrl Pts',(8.09922980642484,0.649806406814116,
60.6151891873091));
#168170=CARTESIAN_POINT('Ctrl Pts',(8.09849052636244,0.65895600686685,60.6155513897293));
#168171=CARTESIAN_POINT('Ctrl Pts',(8.09718030352455,0.674836517362658,
60.6161790064022));
#168172=CARTESIAN_POINT('Ctrl Pts',(8.09661647011617,0.681567993079212,
60.6164447177712));
#168173=CARTESIAN_POINT('Ctrl Pts',(8.09542535404755,0.695578374583006,
60.6169970874));
#168174=CARTESIAN_POINT('Ctrl Pts',(8.0947966471583,0.702857154572223,60.6172836867319));
#168175=CARTESIAN_POINT('Ctrl Pts',(8.09329245904479,0.720001971922734,
60.6179579011816));
#168176=CARTESIAN_POINT('Ctrl Pts',(8.09240875191283,0.729867289501645,
60.6183451832726));
#168177=CARTESIAN_POINT('Ctrl Pts',(8.08945608577587,0.762164866478486,
60.6196109662545));
#168178=CARTESIAN_POINT('Ctrl Pts',(8.08731186460905,0.784590252594031,
60.6204864948873));
#168179=CARTESIAN_POINT('Ctrl Pts',(8.04959316163622,1.16247877565269,60.6351875377156));
#168180=CARTESIAN_POINT('Ctrl Pts',(7.99070464209756,1.51524848438325,60.6481515544868));
#168181=CARTESIAN_POINT('Ctrl Pts',(7.76002520682446,2.49451911717093,60.6843124984819));
#168182=CARTESIAN_POINT('Ctrl Pts',(7.53617244632897,3.10591721774189,60.7073417412755));
#168183=CARTESIAN_POINT('Ctrl Pts',(7.09240190137212,3.97823703329178,60.7441617809294));
#168184=CARTESIAN_POINT('Ctrl Pts',(6.92503953666495,4.26290403670386,60.7568113105691));
#168185=CARTESIAN_POINT('Ctrl Pts',(6.68596816716871,4.6181356778367,60.7733823145035));
#168186=CARTESIAN_POINT('Ctrl Pts',(6.62961783598603,4.69867157964452,60.7771983939031));
#168187=CARTESIAN_POINT('Ctrl Pts',(6.54395786805605,4.81648709215843,60.7828759674642));
#168188=CARTESIAN_POINT('Ctrl Pts',(6.51576044127776,4.85456469053098,60.7847260303116));
#168189=CARTESIAN_POINT('Ctrl Pts',(6.4646104734408,4.92238869114325,60.7880493238095));
#168190=CARTESIAN_POINT('Ctrl Pts',(6.44178157100305,4.95222668893286,60.7895212153291));
#168191=CARTESIAN_POINT('Ctrl Pts',(6.39261883240736,5.01556855269947,60.7926673891941));
#168192=CARTESIAN_POINT('Ctrl Pts',(6.36622671122521,5.04902573625479,60.7943422631618));
#168193=CARTESIAN_POINT('Ctrl Pts',(6.2934754699579,5.13977484044467,60.7989217096145));
#168194=CARTESIAN_POINT('Ctrl Pts',(6.24659827876539,5.19664591299531,60.8018318728236));
#168195=CARTESIAN_POINT('Ctrl Pts',(5.92853158999695,5.57199889022977,60.8213178883067));
#168196=CARTESIAN_POINT('Ctrl Pts',(5.63387517310721,5.86976098877403,60.8381604705478));
#168197=CARTESIAN_POINT('Ctrl Pts',(4.98792958335573,6.42887020666397,60.8728401923948));
#168198=CARTESIAN_POINT('Ctrl Pts',(4.63580441709636,6.68723699102904,60.8906314874597));
#168199=CARTESIAN_POINT('Ctrl Pts',(4.20270195468915,6.95429943598463,60.9109386054428));
#168200=CARTESIAN_POINT('Ctrl Pts',(4.1402424497911,6.99166482188269,60.9138308674267));
#168201=CARTESIAN_POINT('Ctrl Pts',(4.05608661621247,7.04048647163382,60.9176768333862));
#168202=CARTESIAN_POINT('Ctrl Pts',(4.0348286814298,7.05269068611266,60.9186440399612));
#168203=CARTESIAN_POINT('Ctrl Pts',(3.99862944204557,7.0732554931069,60.920283640733));
#168204=CARTESIAN_POINT('Ctrl Pts',(3.98371643483754,7.08166534469235,60.9209569680551));
#168205=CARTESIAN_POINT('Ctrl Pts',(3.95183295451385,7.0995127239852,60.9223920395896));
#168206=CARTESIAN_POINT('Ctrl Pts',(3.93485504261444,7.10893665855741,60.9231535329103));
#168207=CARTESIAN_POINT('Ctrl Pts',(3.89265361590535,7.13216391676713,60.9250399910602));
#168208=CARTESIAN_POINT('Ctrl Pts',(3.86739026549029,7.145894405407,60.9261636854468));
#168209=CARTESIAN_POINT('Ctrl Pts',(3.76718415291409,7.19966881054316,60.9306000446703));
#168210=CARTESIAN_POINT('Ctrl Pts',(3.69168765298413,7.23867045021743,60.9338968721704));
#168211=CARTESIAN_POINT('Ctrl Pts',(3.53881622261458,7.31463036213173,60.9404988412214));
#168212=CARTESIAN_POINT('Ctrl Pts',(3.46144028852124,7.35156233927766,60.9438033754844));
#168213=CARTESIAN_POINT('Ctrl Pts',(3.12042252938551,7.50775436805165,60.9582407352219));
#168214=CARTESIAN_POINT('Ctrl Pts',(2.85110361184242,7.61410665018196,60.9693253760213));
#168215=CARTESIAN_POINT('Ctrl Pts',(2.49957767473549,7.73164986578451,60.9836739687851));
#168216=CARTESIAN_POINT('Ctrl Pts',(2.42208611300805,7.75627468273187,60.9868289832247));
#168217=CARTESIAN_POINT('Ctrl Pts',(2.30355538468195,7.79199111500701,60.9916470954672));
#168218=CARTESIAN_POINT('Ctrl Pts',(2.262776973388,7.80393063131779,60.9933032783038));
#168219=CARTESIAN_POINT('Ctrl Pts',(2.18822778203746,7.82512445230124,60.9963290597273));
#168220=CARTESIAN_POINT('Ctrl Pts',(2.15448721024098,7.83448137219025,60.9976977777518));
#168221=CARTESIAN_POINT('Ctrl Pts',(2.08058319454352,7.85446287412851,61.0006944766805));
#168222=CARTESIAN_POINT('Ctrl Pts',(2.04039663839111,7.86499809357729,61.0023231565775));
#168223=CARTESIAN_POINT('Ctrl Pts',(1.9240154531896,7.89455631508567,61.0070380098315));
#168224=CARTESIAN_POINT('Ctrl Pts',(1.84762384795223,7.9127833840856,61.0101305728496));
#168225=CARTESIAN_POINT('Ctrl Pts',(1.71672453836261,7.94201705726832,61.0154271511196));
#168226=CARTESIAN_POINT('Ctrl Pts',(1.66234593583963,7.95357680749427,61.0176266898467));
#168227=CARTESIAN_POINT('Ctrl Pts',(1.43069327443569,8.00034180636538,61.0269934516233));
#168228=CARTESIAN_POINT('Ctrl Pts',(1.25239064457378,8.0301848728818,61.034196511095));
#168229=CARTESIAN_POINT('Ctrl Pts',(0.806384689260168,8.0896173607951,61.0521648470201));
#168230=CARTESIAN_POINT('Ctrl Pts',(0.537922820619334,8.11189287267858,
61.0629408866666));
#168231=CARTESIAN_POINT('Ctrl Pts',(0.229097062707495,8.12211697465617,
61.0751453871078));
#168232=CARTESIAN_POINT('Ctrl Pts',(0.189334548041407,8.12314114532041,
61.0767129549097));
#168233=CARTESIAN_POINT('Ctrl Pts',(0.12825480132642,8.12426566457234,61.0791141682226));
#168234=CARTESIAN_POINT('Ctrl Pts',(0.106942205005658,8.12457415811716,
61.0799507334359));
#168235=CARTESIAN_POINT('Ctrl Pts',(0.0655175388263775,8.125010739147,61.0815742895506));
#168236=CARTESIAN_POINT('Ctrl Pts',(0.0454057952675497,8.12514802179986,
61.0823614260348));
#168237=CARTESIAN_POINT('Ctrl Pts',(-0.00238654562119118,8.12529679894001,
61.0842295373541));
#168238=CARTESIAN_POINT('Ctrl Pts',(-0.0300671314041179,8.12524151898409,
61.0853096116265));
#168239=CARTESIAN_POINT('Ctrl Pts',(-0.12470551894208,8.12456889754107,
61.0889966447027));
#168240=CARTESIAN_POINT('Ctrl Pts',(-0.1916559813614,8.12326531097501,61.0915952690033));
#168241=CARTESIAN_POINT('Ctrl Pts',(-0.314055257674444,8.119368026531,61.0963344456969));
#168242=CARTESIAN_POINT('Ctrl Pts',(-0.369508150382494,8.11703342482815,
61.0984771469826));
#168243=CARTESIAN_POINT('Ctrl Pts',(-0.654072942869756,8.10213091073416,
61.1094594950965));
#168244=CARTESIAN_POINT('Ctrl Pts',(-0.882602861258377,8.08043005540727,
61.118237715875));
#168245=CARTESIAN_POINT('Ctrl Pts',(-1.27684366261096,8.02606722899659,
61.1334959867371));
#168246=CARTESIAN_POINT('Ctrl Pts',(-1.44302195346336,7.99786047271005,
61.1399628680115));
#168247=CARTESIAN_POINT('Ctrl Pts',(-1.790222260089,7.92775340092446,61.15361313872));
#168248=CARTESIAN_POINT('Ctrl Pts',(-1.97092745133505,7.8847709987417,61.1607986235292));
#168249=CARTESIAN_POINT('Ctrl Pts',(-2.213872798011,7.81810985601866,61.1706037138418));
#168250=CARTESIAN_POINT('Ctrl Pts',(-2.27752896207104,7.79980360418615,
61.1731863647071));
#168251=CARTESIAN_POINT('Ctrl Pts',(-2.393748786298,7.76483701738787,61.1779276210929));
#168252=CARTESIAN_POINT('Ctrl Pts',(-2.44638041629265,7.74841596651649,
61.1800846211835));
#168253=CARTESIAN_POINT('Ctrl Pts',(-2.55585042449841,7.71303479738341,
61.184592085886));
#168254=CARTESIAN_POINT('Ctrl Pts',(-2.61265445561199,7.69397906433219,
61.1869429709098));
#168255=CARTESIAN_POINT('Ctrl Pts',(-2.77921725039197,7.63604587752053,
61.1938718693162));
#168256=CARTESIAN_POINT('Ctrl Pts',(-2.88835681674073,7.59543546485952,
61.1984579551067));
#168257=CARTESIAN_POINT('Ctrl Pts',(-3.20393541744128,7.47022407232345,
61.211849373212));
#168258=CARTESIAN_POINT('Ctrl Pts',(-3.40780943167426,7.37945017508381,
61.2206686170383));
#168259=CARTESIAN_POINT('Ctrl Pts',(-3.65432236401248,7.25729455322159,
61.231497151881));
#168260=CARTESIAN_POINT('Ctrl Pts',(-3.70073221946383,7.23373881452888,
61.2335430629632));
#168261=CARTESIAN_POINT('Ctrl Pts',(-3.77898769953057,7.19306931765594,
61.2370039827339));
#168262=CARTESIAN_POINT('Ctrl Pts',(-3.81095110631346,7.17618602831645,
61.2384206652219));
#168263=CARTESIAN_POINT('Ctrl Pts',(-3.90334956624565,7.12658909806216,
61.2425258509384));
#168264=CARTESIAN_POINT('Ctrl Pts',(-3.9634836441215,7.09332132791915,61.245210127954));
#168265=CARTESIAN_POINT('Ctrl Pts',(-4.16241521353036,6.9799475050825,61.2541430255104));
#168266=CARTESIAN_POINT('Ctrl Pts',(-4.29926419472592,6.8964987592677,61.2603757542781));
#168267=CARTESIAN_POINT('Ctrl Pts',(-4.54931819830307,6.73368204634625,
61.2719959728997));
#168268=CARTESIAN_POINT('Ctrl Pts',(-4.6631390338507,6.6553665652407,61.277379406449));
#168269=CARTESIAN_POINT('Ctrl Pts',(-4.82557431433687,6.53738796790606,
61.2852265057699));
#168270=CARTESIAN_POINT('Ctrl Pts',(-4.8758138151174,6.50000373182439,61.2876771244317));
#168271=CARTESIAN_POINT('Ctrl Pts',(-4.96934372167773,6.42871165930659,
61.2922864760169));
#168272=CARTESIAN_POINT('Ctrl Pts',(-5.01273186602575,6.39493782898225,
61.2944442294149));
#168273=CARTESIAN_POINT('Ctrl Pts',(-5.11333929060061,6.31497080087364,
61.2994951898391));
#168274=CARTESIAN_POINT('Ctrl Pts',(-5.17028082684087,6.268436090637,61.3023906635151));
#168275=CARTESIAN_POINT('Ctrl Pts',(-5.37880171119411,6.09325075291125,
61.3131365448601));
#168276=CARTESIAN_POINT('Ctrl Pts',(-5.52627451862615,5.9598239295092,61.3210226859123));
#168277=CARTESIAN_POINT('Ctrl Pts',(-5.95846946899684,5.53894556536053,
61.3450649901976));
#168278=CARTESIAN_POINT('Ctrl Pts',(-6.2267599271406,5.23552628451184,61.3613267992789));
#168279=CARTESIAN_POINT('Ctrl Pts',(-6.52768190762045,4.83918772183988,
61.3811102124871));
#168280=CARTESIAN_POINT('Ctrl Pts',(-6.58274446637141,4.76401557689418,
61.3848016987598));
#168281=CARTESIAN_POINT('Ctrl Pts',(-6.65503588600647,4.66167532206538,
61.3897400641955));
#168282=CARTESIAN_POINT('Ctrl Pts',(-6.67341377276085,4.63532826048087,
61.3910037986421));
#168283=CARTESIAN_POINT('Ctrl Pts',(-6.70236428483002,4.59329493334236,
61.3930074995878));
#168284=CARTESIAN_POINT('Ctrl Pts',(-6.71303917450127,4.57767958638977,
61.393749172534));
#168285=CARTESIAN_POINT('Ctrl Pts',(-6.73482202202277,4.54557533835347,
61.3952683860332));
#168286=CARTESIAN_POINT('Ctrl Pts',(-6.74592419590036,4.52908264139374,
61.396045819375));
#168287=CARTESIAN_POINT('Ctrl Pts',(-6.77332663990799,4.48805098437757,
61.3979723519062));
#168288=CARTESIAN_POINT('Ctrl Pts',(-6.789554221519,4.46346377751756,61.3991200727112));
#168289=CARTESIAN_POINT('Ctrl Pts',(-6.86235012980001,4.35185150329611,
61.4043015663394));
#168290=CARTESIAN_POINT('Ctrl Pts',(-6.91738191672716,4.26383496120505,
61.4083097916253));
#168291=CARTESIAN_POINT('Ctrl Pts',(-7.09139901944629,3.97327569708988,
61.4213408157735));
#168292=CARTESIAN_POINT('Ctrl Pts',(-7.20329100990146,3.766624420254,61.430300693717));
#168293=CARTESIAN_POINT('Ctrl Pts',(-7.4032688075017,3.35568725227628,61.4478084145931));
#168294=CARTESIAN_POINT('Ctrl Pts',(-7.4922323670626,3.15205940236069,61.4563445519342));
#168295=CARTESIAN_POINT('Ctrl Pts',(-7.59388198332121,2.89068264474098,
61.4672220906932));
#168296=CARTESIAN_POINT('Ctrl Pts',(-7.61443729055391,2.83609492637373,
61.4694893131216));
#168297=CARTESIAN_POINT('Ctrl Pts',(-7.64594744584925,2.7496022722373,61.4730758178265));
#168298=CARTESIAN_POINT('Ctrl Pts',(-7.65729446891351,2.71784223370749,
61.4743915424886));
#168299=CARTESIAN_POINT('Ctrl Pts',(-7.68017015305105,2.6525331977834,61.4770948144507));
#168300=CARTESIAN_POINT('Ctrl Pts',(-7.69167750233672,2.61897749788778,
61.4784825210875));
#168301=CARTESIAN_POINT('Ctrl Pts',(-7.71805447015741,2.54038812243124,
61.4817299911465));
#168302=CARTESIAN_POINT('Ctrl Pts',(-7.73275027307521,2.49529753853598,
61.483591229651));
#168303=CARTESIAN_POINT('Ctrl Pts',(-7.7816063112487,2.34081685393292,61.4899616302422));
#168304=CARTESIAN_POINT('Ctrl Pts',(-7.81384649241907,2.23083459619634,
61.4944866694988));
#168305=CARTESIAN_POINT('Ctrl Pts',(-7.89616719113295,1.92628761384265,
61.5069882655948));
#168306=CARTESIAN_POINT('Ctrl Pts',(-7.9413751586908,1.73049123072408,61.5149958773726));
#168307=CARTESIAN_POINT('Ctrl Pts',(-8.01456379929508,1.34959891103702,
61.5304664603936));
#168308=CARTESIAN_POINT('Ctrl Pts',(-8.04349837003739,1.1648110698877,61.5379238851092));
#168309=CARTESIAN_POINT('Ctrl Pts',(-8.07060514929345,0.941520024572059,
61.5468227200769));
#168310=CARTESIAN_POINT('Ctrl Pts',(-8.07491412840532,0.903819267864985,
61.5483213019505));
#168311=CARTESIAN_POINT('Ctrl Pts',(-8.081464064806,0.842720893481965,61.5507427927173));
#168312=CARTESIAN_POINT('Ctrl Pts',(-8.08386786482879,0.819341372071401,
61.5516676962131));
#168313=CARTESIAN_POINT('Ctrl Pts',(-8.08798672413963,0.777497379011614,
61.5533198168065));
#168314=CARTESIAN_POINT('Ctrl Pts',(-8.08974007471084,0.759036857161392,
61.5540475622623));
#168315=CARTESIAN_POINT('Ctrl Pts',(-8.09343964543737,0.718615560348982,
61.5556384288328));
#168316=CARTESIAN_POINT('Ctrl Pts',(-8.09535970569644,0.696652607591544,
61.5565011205808));
#168317=CARTESIAN_POINT('Ctrl Pts',(-8.10102148066233,0.6287028654175,61.5591651635049));
#168318=CARTESIAN_POINT('Ctrl Pts',(-8.10446091661238,0.582691696398901,
61.5609620435754));
#168319=CARTESIAN_POINT('Ctrl Pts',(-8.11161904785845,0.474550026943905,
61.5651710623397));
#168320=CARTESIAN_POINT('Ctrl Pts',(-8.11501612977759,0.412401017819403,
61.5675789537567));
#168321=CARTESIAN_POINT('Ctrl Pts',(-8.12466965400848,0.188642614285465,
61.5762169056599));
#168322=CARTESIAN_POINT('Ctrl Pts',(-8.12681491848019,0.0268928378850284,
61.5824026345489));
#168323=CARTESIAN_POINT('Ctrl Pts',(-8.11640160148237,-0.600631030495562,
61.6063234648979));
#168324=CARTESIAN_POINT('Ctrl Pts',(-8.0686231312327,-1.06491898245423,
61.6238855130451));
#168325=CARTESIAN_POINT('Ctrl Pts',(-7.94036252037984,-1.7372724846345,
61.650129710661));
#168326=CARTESIAN_POINT('Ctrl Pts',(-7.89075246024864,-1.95025543985168,
61.6585610244123));
#168327=CARTESIAN_POINT('Ctrl Pts',(-7.81546766088394,-2.22313068525872,
61.6695676930288));
#168328=CARTESIAN_POINT('Ctrl Pts',(-7.79758040967125,-2.28507866428104,
61.6720801559474));
#168329=CARTESIAN_POINT('Ctrl Pts',(-7.76729093995983,-2.38547912761291,
61.6761756109967));
#168330=CARTESIAN_POINT('Ctrl Pts',(-7.75533587486127,-2.42406366853103,
61.6777551963373));
#168331=CARTESIAN_POINT('Ctrl Pts',(-7.73186485078844,-2.49786431916701,
61.6807876126248));
#168332=CARTESIAN_POINT('Ctrl Pts',(-7.72039474993824,-2.53309398226664,
61.6822400754721));
#168333=CARTESIAN_POINT('Ctrl Pts',(-7.69319068409944,-2.61474804579395,
61.685618131188));
#168334=CARTESIAN_POINT('Ctrl Pts',(-7.67727678440134,-2.66111093315479,
61.6875449330664));
#168335=CARTESIAN_POINT('Ctrl Pts',(-7.62510262732157,-2.8087485604071,
61.6937090947627));
#168336=CARTESIAN_POINT('Ctrl Pts',(-7.58725052254165,-2.90944803295918,
61.697956628087));
#168337=CARTESIAN_POINT('Ctrl Pts',(-7.35701012323633,-3.48688491761813,
61.7225670745153));
#168338=CARTESIAN_POINT('Ctrl Pts',(-7.1217296056915,-3.9452385944691,61.74306203922));
#168339=CARTESIAN_POINT('Ctrl Pts',(-6.42948745332216,-5.02744712178074,
61.7961337332576));
#168340=CARTESIAN_POINT('Ctrl Pts',(-5.9240538288087,-5.61417367647944,
61.8297851861502));
#168341=CARTESIAN_POINT('Ctrl Pts',(-5.30485199531406,-6.154744630721,61.8628724365981));
#168342=CARTESIAN_POINT('Ctrl Pts',(-5.26576161399473,-6.1882219515441,
61.8649287898478));
#168343=CARTESIAN_POINT('Ctrl Pts',(-5.21558854318688,-6.23037089137512,
61.8675243805212));
#168344=CARTESIAN_POINT('Ctrl Pts',(-5.20479824939517,-6.23938782910821,
61.8680800456619));
#168345=CARTESIAN_POINT('Ctrl Pts',(-5.18762092233689,-6.25366654103752,
61.8689605128334));
#168346=CARTESIAN_POINT('Ctrl Pts',(-5.18124919080095,-6.25894662573627,
61.869286217994));
#168347=CARTESIAN_POINT('Ctrl Pts',(-5.16934985855267,-6.26877666361825,
61.8698927956179));
#168348=CARTESIAN_POINT('Ctrl Pts',(-5.16382429226536,-6.27332906019362,
61.8701737910381));
#168349=CARTESIAN_POINT('Ctrl Pts',(-5.15153816340792,-6.28342410945336,
61.8707970755344));
#168350=CARTESIAN_POINT('Ctrl Pts',(-5.14477465182072,-6.28896317138708,
61.8711391806417));
#168351=CARTESIAN_POINT('Ctrl Pts',(-5.12515731084194,-6.30497621134719,
61.8721284820466));
#168352=CARTESIAN_POINT('Ctrl Pts',(-5.11228029668986,-6.31542181172606,
61.8727741942987));
#168353=CARTESIAN_POINT('Ctrl Pts',(-5.01635829319294,-6.39274637971109,
61.8775563378679));
#168354=CARTESIAN_POINT('Ctrl Pts',(-4.93204316401295,-6.45801885898859,
61.8815990186006));
#168355=CARTESIAN_POINT('Ctrl Pts',(-4.7023167011064,-6.62873715179465,
61.8922119454725));
#168356=CARTESIAN_POINT('Ctrl Pts',(-4.55465719690427,-6.73105055102272,
61.8986259138178));
#168357=CARTESIAN_POINT('Ctrl Pts',(-3.94976983885492,-7.12115074926514,
61.9237254026474));
#168358=CARTESIAN_POINT('Ctrl Pts',(-3.46774181000144,-7.367922266777,61.941195900664));
#168359=CARTESIAN_POINT('Ctrl Pts',(-2.47039456857689,-7.75878826284801,
61.9774627123021));
#168360=CARTESIAN_POINT('Ctrl Pts',(-1.95826305640002,-7.90359242045759,
61.9961720515824));
#168361=CARTESIAN_POINT('Ctrl Pts',(-1.40358744084232,-8.00316773933742,
62.0178344742494));
#168362=CARTESIAN_POINT('Ctrl Pts',(-1.37144739569775,-8.0087379517326,
62.0190941457293));
#168363=CARTESIAN_POINT('Ctrl Pts',(-1.32677351539151,-8.01620360585699,
62.0208514264824));
#168364=CARTESIAN_POINT('Ctrl Pts',(-1.31426729447796,-8.01826350830555,
62.0213440596437));
#168365=CARTESIAN_POINT('Ctrl Pts',(-1.29273146244183,-8.02175894193811,
62.0221935796831));
#168366=CARTESIAN_POINT('Ctrl Pts',(-1.28370413815077,-8.02320851290605,
62.0225500418148));
#168367=CARTESIAN_POINT('Ctrl Pts',(-1.26507876432179,-8.02616706044107,
62.0232862553839));
#168368=CARTESIAN_POINT('Ctrl Pts',(-1.25548041802125,-8.02767406421343,
62.0236660657362));
#168369=CARTESIAN_POINT('Ctrl Pts',(-1.23315170565159,-8.03113879398552,
62.0245505860221));
#168370=CARTESIAN_POINT('Ctrl Pts',(-1.22041935786317,-8.03308347065552,
62.0250556884332));
#168371=CARTESIAN_POINT('Ctrl Pts',(-1.17990761924513,-8.03917249738859,
62.0266651555246));
#168372=CARTESIAN_POINT('Ctrl Pts',(-1.15211147716946,-8.04320306579887,
62.0277729411678));
#168373=CARTESIAN_POINT('Ctrl Pts',(-0.850935757889427,-8.08528168418689,
62.0398142675268));
#168374=CARTESIAN_POINT('Ctrl Pts',(-0.575827172519357,-8.10951765209312,
62.051163082099));
#168375=CARTESIAN_POINT('Ctrl Pts',(0.108007341429484,-8.13478621513484,
62.0802124984239));
#168376=CARTESIAN_POINT('Ctrl Pts',(0.516577756190515,-8.11908359996046,
62.09832791996));
#168377=CARTESIAN_POINT('Ctrl Pts',(1.53296842456235,-8.00297389323821,
62.144229421143));
#168378=CARTESIAN_POINT('Ctrl Pts',(2.13392133622353,-7.86410624761655,
62.1721642797551));
#168379=CARTESIAN_POINT('Ctrl Pts',(2.74694008616192,-7.64691212908519,
62.1983431121043));
#168380=CARTESIAN_POINT('Ctrl Pts',(2.78028635467762,-7.63485119625819,
62.1997601833476));
#168381=CARTESIAN_POINT('Ctrl Pts',(2.82541572315839,-7.61819358190449,
62.201669690669));
#168382=CARTESIAN_POINT('Ctrl Pts',(2.83726828905259,-7.61378723884296,
62.2021704152822));
#168383=CARTESIAN_POINT('Ctrl Pts',(2.85594416800136,-7.60679457568051,
62.2029582300159));
#168384=CARTESIAN_POINT('Ctrl Pts',(2.86277433628951,-7.60422671330217,
62.2032461038299));
#168385=CARTESIAN_POINT('Ctrl Pts',(2.87594082822761,-7.59925640016529,
62.2038005753312));
#168386=CARTESIAN_POINT('Ctrl Pts',(2.88227762093635,-7.59685521772761,
62.2040672257314));
#168387=CARTESIAN_POINT('Ctrl Pts',(2.89725171383319,-7.59115969562443,
62.2046968566993));
#168388=CARTESIAN_POINT('Ctrl Pts',(2.90588642082837,-7.58785853372879,
62.2050595553486));
#168389=CARTESIAN_POINT('Ctrl Pts',(2.93114843689675,-7.57815108782815,
62.2061196296936));
#168390=CARTESIAN_POINT('Ctrl Pts',(2.94776038654476,-7.57170481322532,
62.2068153862158));
#168391=CARTESIAN_POINT('Ctrl Pts',(3.07158039100774,-7.52318715694141,
62.2119921693351));
#168392=CARTESIAN_POINT('Ctrl Pts',(3.17790714084202,-7.47889421341075,
62.2163864025545));
#168393=CARTESIAN_POINT('Ctrl Pts',(3.5344628780798,-7.32138494577898,62.2310430045235));
#168394=CARTESIAN_POINT('Ctrl Pts',(3.77988828380747,-7.19774685280098,
62.2410030044885));
#168395=CARTESIAN_POINT('Ctrl Pts',(4.33586457388257,-6.88136816541448,
62.264036540786));
#168396=CARTESIAN_POINT('Ctrl Pts',(4.64061072891498,-6.67964673342571,
62.2770423221525));
#168397=CARTESIAN_POINT('Ctrl Pts',(5.00087763164712,-6.40458375290102,
62.2935778118405));
#168398=CARTESIAN_POINT('Ctrl Pts',(5.07011877668137,-6.34991066875522,
62.2968117389642));
#168399=CARTESIAN_POINT('Ctrl Pts',(5.37332602181805,-6.10237541592036,
62.3112457567115));
#168400=CARTESIAN_POINT('Ctrl Pts',(5.5972708239307,-5.89764075144378,62.3226541829803));
#168401=CARTESIAN_POINT('Ctrl Pts',(5.84451849234334,-5.64480615125514,
62.3362735916627));
#168402=CARTESIAN_POINT('Ctrl Pts',(5.87945525899085,-5.60840785769787,
62.3382233727168));
#168403=CARTESIAN_POINT('Ctrl Pts',(5.93226733259062,-5.55235063656264,
62.3412097870372));
#168404=CARTESIAN_POINT('Ctrl Pts',(5.9503890798934,-5.5329253643324,62.3422416921391));
#168405=CARTESIAN_POINT('Ctrl Pts',(5.98295131148275,-5.49767587979276,
62.3441088538814));
#168406=CARTESIAN_POINT('Ctrl Pts',(5.99742512800038,-5.48188273354477,
62.3449434929718));
#168407=CARTESIAN_POINT('Ctrl Pts',(6.02554345695251,-5.45095668493241,
62.3465741429988));
#168408=CARTESIAN_POINT('Ctrl Pts',(6.03919386560688,-5.43582930039243,
62.3473700550967));
#168409=CARTESIAN_POINT('Ctrl Pts',(6.07494585111884,-5.39590804924719,
62.3494661271424));
#168410=CARTESIAN_POINT('Ctrl Pts',(6.09695250085984,-5.37102978557374,
62.3507679913123));
#168411=CARTESIAN_POINT('Ctrl Pts',(6.17728190776458,-5.27908843628185,
62.3555640942276));
#168412=CARTESIAN_POINT('Ctrl Pts',(6.2346552311554,-5.21120526665049,62.3590759736546));
#168413=CARTESIAN_POINT('Ctrl Pts',(6.5683907136943,-4.8029329699844,62.3800484434053));
#168414=CARTESIAN_POINT('Ctrl Pts',(6.8179305137607,-4.44158831263069,62.3980628078057));
#168415=CARTESIAN_POINT('Ctrl Pts',(7.34050314382295,-3.53625029271457,
62.4420281554622));
#168416=CARTESIAN_POINT('Ctrl Pts',(7.58405825412809,-2.9782718641043,62.4683149604618));
#168417=CARTESIAN_POINT('Ctrl Pts',(7.77870682761077,-2.3482258212521,62.494919088341));
#168418=CARTESIAN_POINT('Ctrl Pts',(7.79371892678636,-2.29790988672862,
62.4970219239637));
#168419=CARTESIAN_POINT('Ctrl Pts',(7.81227323311432,-2.23344730287871,
62.4996855633942));
#168420=CARTESIAN_POINT('Ctrl Pts',(7.81626636487498,-2.21943236890466,
62.5002628407396));
#168421=CARTESIAN_POINT('Ctrl Pts',(7.82256263188266,-2.19710623555054,
62.5011794744542));
#168422=CARTESIAN_POINT('Ctrl Pts',(7.8248902663525,-2.18880201485997,62.5015197611022));
#168423=CARTESIAN_POINT('Ctrl Pts',(7.82921502550224,-2.17327765490255,
62.5021546683733));
#168424=CARTESIAN_POINT('Ctrl Pts',(7.83121539384655,-2.16605843330477,
62.5024494147007));
#168425=CARTESIAN_POINT('Ctrl Pts',(7.83564625099783,-2.14998133955712,
62.5031046796966));
#168426=CARTESIAN_POINT('Ctrl Pts',(7.83807171155595,-2.1411220835328,62.5034649992353));
#168427=CARTESIAN_POINT('Ctrl Pts',(7.84508411590936,-2.11533692393796,
62.5045114679244));
#168428=CARTESIAN_POINT('Ctrl Pts',(7.84963131031478,-2.09840019676589,
62.5051960086753));
#168429=CARTESIAN_POINT('Ctrl Pts',(7.88364562920719,-1.97005081474732,
62.5103616014667));
#168430=CARTESIAN_POINT('Ctrl Pts',(7.91079249308458,-1.85804518721877,
62.5147368436552));
#168431=CARTESIAN_POINT('Ctrl Pts',(7.9569571824244,-1.64816556709156,62.5227047770965));
#168432=CARTESIAN_POINT('Ctrl Pts',(7.97657224980911,-1.55045587653565,
62.5263263750937));
#168433=CARTESIAN_POINT('Ctrl Pts',(8.08114970837706,-0.974837606639548,
62.5472557002737));
#168434=CARTESIAN_POINT('Ctrl Pts',(8.12494782477393,-0.490442646926205,
62.5632724758603));
#168435=CARTESIAN_POINT('Ctrl Pts',(8.12524844182851,-0.00503200391139533,
62.5796456772854));
#168436=CARTESIAN_POINT('',(8.120871211716,0.00172117854336219,64.5832974432123));
#168437=CARTESIAN_POINT('Ctrl Pts',(8.1189210508199,-0.00515126165391927,
62.5832974432123));
#168438=CARTESIAN_POINT('Ctrl Pts',(8.10078544928883,2.03703630869922,62.6634709337063));
#168439=CARTESIAN_POINT('Ctrl Pts',(6.80819671928344,5.43726497504401,62.7965335792958));
#168440=CARTESIAN_POINT('Ctrl Pts',(2.61913853473347,8.04100520042313,62.9824853799807));
#168441=CARTESIAN_POINT('Ctrl Pts',(-1.52043507705924,8.33340792156297,
63.1411528452671));
#168442=CARTESIAN_POINT('Ctrl Pts',(-5.33310408397482,6.58368385109608,
63.2998203105535));
#168443=CARTESIAN_POINT('Ctrl Pts',(-7.82264342903578,3.23476629007734,
63.45848777584));
#168444=CARTESIAN_POINT('Ctrl Pts',(-8.42537801125607,-0.894369939753464,
63.6171552411264));
#168445=CARTESIAN_POINT('Ctrl Pts',(-6.96195299981465,-4.8258285132288,
63.7758227064128));
#168446=CARTESIAN_POINT('Ctrl Pts',(-3.82482145636898,-7.54243940143088,
63.9344901716993));
#168447=CARTESIAN_POINT('Ctrl Pts',(1.64131973131632,-8.81124817329279,
64.1460467920811));
#168448=CARTESIAN_POINT('Ctrl Pts',(6.87712117603622,-5.734150059192,64.3576034124631));
#168449=CARTESIAN_POINT('Ctrl Pts',(8.08738294886851,-1.59563522457139,
64.5209833478719));
#168450=CARTESIAN_POINT('Ctrl Pts',(8.12076539718447,-0.119070448189842,
64.5785849730899));
#168451=CARTESIAN_POINT('Ctrl Pts',(8.120871211716,0.00172117854336219,
64.5832974432123));
#168452=CARTESIAN_POINT('',(8.12588319212561,0.00333877610560675,66.5832974432123));
#168453=CARTESIAN_POINT('Ctrl Pts',(8.12524981744152,0.00172240138683085,
64.5832974547079));
#168454=CARTESIAN_POINT('Ctrl Pts',(8.12520564937343,0.210080679493343,
64.5914218031291));
#168455=CARTESIAN_POINT('Ctrl Pts',(8.11714269539066,0.418310872283689,
64.5995461515503));
#168456=CARTESIAN_POINT('Ctrl Pts',(8.101116090879,0.625784023926309,64.6076704999715));
#168457=CARTESIAN_POINT('Ctrl Pts',(8.08507493566357,0.833445542379041,
64.6158022245644));
#168458=CARTESIAN_POINT('Ctrl Pts',(8.0610557220093,1.04034834560792,64.6239339491573));
#168459=CARTESIAN_POINT('Ctrl Pts',(8.02916518697421,1.24587076487951,64.6320656737502));
#168460=CARTESIAN_POINT('Ctrl Pts',(7.99721833306486,1.45175613796399,64.640211759017));
#168461=CARTESIAN_POINT('Ctrl Pts',(7.95737241127435,1.6562559525216,64.6483578442838));
#168462=CARTESIAN_POINT('Ctrl Pts',(7.90978530245305,1.85875873410125,64.6565039295506));
#168463=CARTESIAN_POINT('Ctrl Pts',(7.862154855686,2.06144593652047,64.6646574335199));
#168464=CARTESIAN_POINT('Ctrl Pts',(7.80676922922532,2.26213218325287,64.6728109374892));
#168465=CARTESIAN_POINT('Ctrl Pts',(7.74383589681935,2.46022217810345,64.6809644414584));
#168466=CARTESIAN_POINT('Ctrl Pts',(7.68078585008095,2.65867954491142,64.6891330666796));
#168467=CARTESIAN_POINT('Ctrl Pts',(7.61016020825909,2.85453074518204,64.6973016919008));
#168468=CARTESIAN_POINT('Ctrl Pts',(7.53221508499273,3.04719928391759,64.705470317122));
#168469=CARTESIAN_POINT('Ctrl Pts',(7.46110425208086,3.22297449205448,64.7129227107918));
#168470=CARTESIAN_POINT('Ctrl Pts',(7.38390187156463,3.39610080444314,64.7203751044616));
#168471=CARTESIAN_POINT('Ctrl Pts',(7.30083524784918,3.56615931307941,64.7278274981315));
#168472=CARTESIAN_POINT('Ctrl Pts',(7.21070409780524,3.75068070413351,64.7359136918636));
#168473=CARTESIAN_POINT('Ctrl Pts',(7.11349959723325,3.93193487294235,64.7439998855958));
#168474=CARTESIAN_POINT('Ctrl Pts',(7.00948073055911,4.10936338748723,64.752086079328));
#168475=CARTESIAN_POINT('Ctrl Pts',(6.90555464377817,4.28663364421642,64.7601650605591));
#168476=CARTESIAN_POINT('Ctrl Pts',(6.79482646948925,4.46008477850942,64.7682440417901));
#168477=CARTESIAN_POINT('Ctrl Pts',(6.67760168871661,4.62918170407568,64.7763230230212));
#168478=CARTESIAN_POINT('Ctrl Pts',(6.56046545921777,4.79815089429405,64.7843959014123));
#168479=CARTESIAN_POINT('Ctrl Pts',(6.43684258907658,4.96277217521777,64.7924687798034));
#168480=CARTESIAN_POINT('Ctrl Pts',(6.30708289096697,5.12253774695431,64.8005416581945));
#168481=CARTESIAN_POINT('Ctrl Pts',(6.17740351990848,5.28220441666322,64.8086095391131));
#168482=CARTESIAN_POINT('Ctrl Pts',(6.04159509627907,5.43702112650239,64.8166774200318));
#168483=CARTESIAN_POINT('Ctrl Pts',(5.90004926268348,5.58651109910363,64.8247453009504));
#168484=CARTESIAN_POINT('Ctrl Pts',(5.75857177593739,5.73592888894683,64.8328092862105));
#168485=CARTESIAN_POINT('Ctrl Pts',(5.61136262212376,5.88002484189713,64.8408732714705));
#168486=CARTESIAN_POINT('Ctrl Pts',(5.45885245468371,6.01835670598658,64.8489372567306));
#168487=CARTESIAN_POINT('Ctrl Pts',(5.30422288429272,6.15861094001294,64.8571133055628));
#168488=CARTESIAN_POINT('Ctrl Pts',(5.14414408985453,6.29293944186506,64.8652893543951));
#168489=CARTESIAN_POINT('Ctrl Pts',(4.97910310419053,6.42092048232496,64.8734654032273));
#168490=CARTESIAN_POINT('Ctrl Pts',(4.81640134625806,6.54708756852527,64.8815255678742));
#168491=CARTESIAN_POINT('Ctrl Pts',(4.64887739338601,6.66708574316072,64.8895857325212));
#168492=CARTESIAN_POINT('Ctrl Pts',(4.47703087278741,6.78055175679741,64.8976458971681));
#168493=CARTESIAN_POINT('Ctrl Pts',(4.30519265494977,6.89401228832608,64.9057056723884));
#168494=CARTESIAN_POINT('Ctrl Pts',(4.12903255032156,7.0009411138893,64.9137654476087));
#168495=CARTESIAN_POINT('Ctrl Pts',(3.94907906025992,7.10101838740871,64.9218252228289));
#168496=CARTESIAN_POINT('Ctrl Pts',(3.7691119834814,7.20110321688929,64.9298856065724));
#168497=CARTESIAN_POINT('Ctrl Pts',(3.58535122715576,7.29433530912716,64.937945990316));
#168498=CARTESIAN_POINT('Ctrl Pts',(3.39835029725013,7.38044055728924,64.9460063740595));
#168499=CARTESIAN_POINT('Ctrl Pts',(3.20664856386755,7.46871030725432,64.9542693786132));
#168500=CARTESIAN_POINT('Ctrl Pts',(3.01154193451114,7.54949005618894,64.9625323831669));
#168501=CARTESIAN_POINT('Ctrl Pts',(2.81364914934523,7.62253671863172,64.9707953877207));
#168502=CARTESIAN_POINT('Ctrl Pts',(2.6204502380647,7.69385076701802,64.9788623997765));
#168503=CARTESIAN_POINT('Ctrl Pts',(2.42459615555917,7.75779433221035,64.9869294118323));
#168504=CARTESIAN_POINT('Ctrl Pts',(2.2266789549132,7.81419147412237,64.9949964238881));
#168505=CARTESIAN_POINT('Ctrl Pts',(2.02154899328362,7.87264391543959,65.0033574246908));
#168506=CARTESIAN_POINT('Ctrl Pts',(1.8142030762292,7.9229894697624,65.0117184254935));
#168507=CARTESIAN_POINT('Ctrl Pts',(1.60531331324235,7.96508987575324,65.0200794262962));
#168508=CARTESIAN_POINT('Ctrl Pts',(1.39642355025551,8.00719028174409,65.0284404270989));
#168509=CARTESIAN_POINT('Ctrl Pts',(1.18599031746624,8.04104550326096,65.0368014279016));
#168510=CARTESIAN_POINT('Ctrl Pts',(0.974693342527283,8.06657674918754,
65.0451624287043));
#168511=CARTESIAN_POINT('Ctrl Pts',(0.783177967084079,8.0897177626856,65.0527406735337));
#168512=CARTESIAN_POINT('Ctrl Pts',(0.590569177841376,8.10606658349232,
65.0603189183632));
#168513=CARTESIAN_POINT('Ctrl Pts',(0.397410233080106,8.1155254093092,65.0678971631926));
#168514=CARTESIAN_POINT('Ctrl Pts',(0.204395022967877,8.1249771965651,65.0754697688509));
#168515=CARTESIAN_POINT('Ctrl Pts',(0.0108308363557188,8.1275491704616,
65.0830423745091));
#168516=CARTESIAN_POINT('Ctrl Pts',(-0.182731308424958,8.12319498912967,
65.0906149801674));
#168517=CARTESIAN_POINT('Ctrl Pts',(-0.376186175457095,8.11884322101118,
65.0981833888682));
#168518=CARTESIAN_POINT('Ctrl Pts',(-0.569638636746874,8.1075729443288,
65.105751797569));
#168519=CARTESIAN_POINT('Ctrl Pts',(-0.762535075129235,8.08938982999939,
65.1133202062698));
#168520=CARTESIAN_POINT('Ctrl Pts',(-0.955384908191962,8.07121110885558,
65.1208867863826));
#168521=CARTESIAN_POINT('Ctrl Pts',(-1.14767861953453,8.04612290088425,
65.1284533664954));
#168522=CARTESIAN_POINT('Ctrl Pts',(-1.33886498399562,8.01418293509266,
65.1360199466082));
#168523=CARTESIAN_POINT('Ctrl Pts',(-1.53001743286074,7.98224863530648,
65.1435851844439));
#168524=CARTESIAN_POINT('Ctrl Pts',(-1.72006256367128,7.94346506070241,
65.1511504222797));
#168525=CARTESIAN_POINT('Ctrl Pts',(-1.90845692468996,7.8979414868118,65.1587156601155));
#168526=CARTESIAN_POINT('Ctrl Pts',(-2.09691679946813,7.85240208219007,
65.1662835287474));
#168527=CARTESIAN_POINT('Ctrl Pts',(-2.28372439897868,7.80011807910052,
65.1738513973794));
#168528=CARTESIAN_POINT('Ctrl Pts',(-2.46834860628678,7.74124942889338,
65.1814192660114));
#168529=CARTESIAN_POINT('Ctrl Pts',(-2.65059033673784,7.68314044719758,
65.1888894753378));
#168530=CARTESIAN_POINT('Ctrl Pts',(-2.83070437198839,7.61861589268249,
65.1963596846642));
#168531=CARTESIAN_POINT('Ctrl Pts',(-3.00819722506586,7.54787632500732,
65.2038298939906));
#168532=CARTESIAN_POINT('Ctrl Pts',(-3.22930486420425,7.45975413568458,
65.2131357354338));
#168533=CARTESIAN_POINT('Ctrl Pts',(-3.44623709793891,7.36203258265992,
65.2224415768769));
#168534=CARTESIAN_POINT('Ctrl Pts',(-3.65826586947159,7.25512083915625,
65.2317474183201));
#168535=CARTESIAN_POINT('Ctrl Pts',(-3.87143298070287,7.14763510807062,
65.2411032209485));
#168536=CARTESIAN_POINT('Ctrl Pts',(-4.07964382046493,7.03086030960335,
65.250459023577));
#168537=CARTESIAN_POINT('Ctrl Pts',(-4.28219177836065,6.90525315508711,
65.2598148262055));
#168538=CARTESIAN_POINT('Ctrl Pts',(-4.48572299623879,6.77903624626959,
65.2692160461584));
#168539=CARTESIAN_POINT('Ctrl Pts',(-4.68353619515957,6.64390106325968,
65.2786172661114));
#168540=CARTESIAN_POINT('Ctrl Pts',(-4.87494818340455,6.50035135755142,
65.2880184860643));
#168541=CARTESIAN_POINT('Ctrl Pts',(-5.06656733622119,6.35664628846407,
65.297429880927));
#168542=CARTESIAN_POINT('Ctrl Pts',(-5.25177139773545,6.20450851170978,
65.3068412757897));
#168543=CARTESIAN_POINT('Ctrl Pts',(-5.42990897238826,6.04448311388802,
65.3162526706524));
#168544=CARTESIAN_POINT('Ctrl Pts',(-5.60783758867829,5.88464542854186,
65.3256530257911));
#168545=CARTESIAN_POINT('Ctrl Pts',(-5.77871626236403,5.71693864341223,
65.3350533809298));
#168546=CARTESIAN_POINT('Ctrl Pts',(-5.94193009243925,5.54194499603387,
65.3444537360684));
#168547=CARTESIAN_POINT('Ctrl Pts',(-6.04635766667792,5.42998045176408,
65.350468277138));
#168548=CARTESIAN_POINT('Ctrl Pts',(-6.14764816864232,5.31503366556899,
65.3564828182076));
#168549=CARTESIAN_POINT('Ctrl Pts',(-6.24564800006565,5.19726549464003,
65.3624973592772));
#168550=CARTESIAN_POINT('Ctrl Pts',(-6.37179959516469,5.0456668398382,65.3702396577965));
#168551=CARTESIAN_POINT('Ctrl Pts',(-6.49255525770672,4.88931979925239,
65.3779819563158));
#168552=CARTESIAN_POINT('Ctrl Pts',(-6.60753570050326,4.72865303538703,
65.385724254835));
#168553=CARTESIAN_POINT('Ctrl Pts',(-6.72244452089595,4.56808635236642,
65.3934617306034));
#168554=CARTESIAN_POINT('Ctrl Pts',(-6.83158507970928,4.40320558982517,
65.4011992063718));
#168555=CARTESIAN_POINT('Ctrl Pts',(-6.93461813499328,4.23447268078592,
65.4089366821402));
#168556=CARTESIAN_POINT('Ctrl Pts',(-7.03760532195016,4.06581488838033,
65.4166707133338));
#168557=CARTESIAN_POINT('Ctrl Pts',(-7.13449023674341,3.89330866577138,
65.4244047445273));
#168558=CARTESIAN_POINT('Ctrl Pts',(-7.22497670516621,3.71744524805754,
65.4321387757209));
#168559=CARTESIAN_POINT('Ctrl Pts',(-7.31545159417055,3.54160433532307,
65.439871817202));
#168560=CARTESIAN_POINT('Ctrl Pts',(-7.39952949935549,3.36240739363301,
65.4476048586831));
#168561=CARTESIAN_POINT('Ctrl Pts',(-7.4769598305001,3.18037093050289,65.4553379001642));
#168562=CARTESIAN_POINT('Ctrl Pts',(-7.5543824264124,2.99835265267963,65.4630701691203));
#168563=CARTESIAN_POINT('Ctrl Pts',(-7.62515863606883,2.81349574505808,
65.4708024380763));
#168564=CARTESIAN_POINT('Ctrl Pts',(-7.68908577496729,2.62633727988155,
65.4785347070324));
#168565=CARTESIAN_POINT('Ctrl Pts',(-7.75303750372862,2.43910682335563,
65.4862699502406));
#168566=CARTESIAN_POINT('Ctrl Pts',(-7.81013478380173,2.24957337519464,
65.4940051934488));
#168567=CARTESIAN_POINT('Ctrl Pts',(-7.86022443591833,2.05829040212803,
65.5017404366571));
#168568=CARTESIAN_POINT('Ctrl Pts',(-7.90215204813046,1.89817672637618,
65.5082152326258));
#168569=CARTESIAN_POINT('Ctrl Pts',(-7.9391705845897,1.73683761587606,65.5146900285946));
#168570=CARTESIAN_POINT('Ctrl Pts',(-7.97121767767376,1.57460353665337,
65.5211648245634));
#168571=CARTESIAN_POINT('Ctrl Pts',(-8.0128632569568,1.36377841778982,65.5295788990678));
#168572=CARTESIAN_POINT('Ctrl Pts',(-8.04613274282637,1.15134020973383,
65.5379929735722));
#168573=CARTESIAN_POINT('Ctrl Pts',(-8.07093121654614,0.937953549106291,
65.5464070480766));
#168574=CARTESIAN_POINT('Ctrl Pts',(-8.09573661579727,0.724507295455871,
65.5548234724005));
#168575=CARTESIAN_POINT('Ctrl Pts',(-8.11206624965703,0.510112322727504,
65.5632398967244));
#168576=CARTESIAN_POINT('Ctrl Pts',(-8.11987707135234,0.295438502275071,
65.5716563210483));
#168577=CARTESIAN_POINT('Ctrl Pts',(-8.127689830077,0.0807114442110189,
65.5800748325867));
#168578=CARTESIAN_POINT('Ctrl Pts',(-8.12697954942962,-0.134294335862574,
65.5884933441252));
#168579=CARTESIAN_POINT('Ctrl Pts',(-8.11775528991404,-0.348907746507043,
65.5969118556637));
#168580=CARTESIAN_POINT('Ctrl Pts',(-8.10852748739891,-0.563603589266107,
65.6053336007173));
#168581=CARTESIAN_POINT('Ctrl Pts',(-8.09077918113527,-0.777906497569484,
65.6137553457709));
#168582=CARTESIAN_POINT('Ctrl Pts',(-8.06457150215843,-0.991147844205967,
65.6221770908245));
#168583=CARTESIAN_POINT('Ctrl Pts',(-8.03836098234078,-1.20441230562191,
65.6305997487723));
#168584=CARTESIAN_POINT('Ctrl Pts',(-8.00368929417285,-1.41661471401595,
65.63902240672));
#168585=CARTESIAN_POINT('Ctrl Pts',(-7.9606692324782,-1.62709340038455,
65.6474450646678));
#168586=CARTESIAN_POINT('Ctrl Pts',(-7.91764098960571,-1.83761211374279,
65.6558693243627));
#168587=CARTESIAN_POINT('Ctrl Pts',(-7.86626125443626,-2.04640619163457,
65.6642935840577));
#168588=CARTESIAN_POINT('Ctrl Pts',(-7.80669383373301,-2.2528246600335,
65.6727178437526));
#168589=CARTESIAN_POINT('Ctrl Pts',(-7.78992523055216,-2.31093275578307,
65.675089325785));
#168590=CARTESIAN_POINT('Ctrl Pts',(-7.77250809447315,-2.36885267483412,
65.6774608078175));
#168591=CARTESIAN_POINT('Ctrl Pts',(-7.75444679713041,-2.42657009644764,
65.6798322898499));
#168592=CARTESIAN_POINT('Ctrl Pts',(-7.69028681589047,-2.63160236061273,
65.6882566150701));
#168593=CARTESIAN_POINT('Ctrl Pts',(-7.6179876353172,-2.83409919470438,
65.6966809402902));
#168594=CARTESIAN_POINT('Ctrl Pts',(-7.53777193415858,-3.03342740659986,
65.7051052655103));
#168595=CARTESIAN_POINT('Ctrl Pts',(-7.45757009525431,-3.23272117214219,
65.713528134904));
#168596=CARTESIAN_POINT('Ctrl Pts',(-7.36945456670468,-3.4288471644451,
65.7219510042977));
#168597=CARTESIAN_POINT('Ctrl Pts',(-7.27369646623844,-3.62119141713475,
65.7303738736913));
#168598=CARTESIAN_POINT('Ctrl Pts',(-7.17795793410072,-3.8134963639536,
65.7387950218575));
#168599=CARTESIAN_POINT('Ctrl Pts',(-7.07458006635887,-4.0020208782696,
65.7472161700237));
#168600=CARTESIAN_POINT('Ctrl Pts',(-6.96388079188532,-4.1861738949679,
65.7556373181899));
#168601=CARTESIAN_POINT('Ctrl Pts',(-6.8532125758928,-4.37027524454368,
65.7640561036661));
#168602=CARTESIAN_POINT('Ctrl Pts',(-6.73522719171313,-4.55000732009851,
65.7724748891422));
#168603=CARTESIAN_POINT('Ctrl Pts',(-6.61028742604854,-4.72480557351565,
65.7808936746184));
#168604=CARTESIAN_POINT('Ctrl Pts',(-6.48538256147108,-4.89955499821088,
65.7893101083632));
#168605=CARTESIAN_POINT('Ctrl Pts',(-6.35352734749046,-5.0693731380007,
65.797726542108));
#168606=CARTESIAN_POINT('Ctrl Pts',(-6.21512728728488,-5.23372528562083,
65.8061429758528));
#168607=CARTESIAN_POINT('Ctrl Pts',(-6.07677745825526,-5.39801778296601,
65.8145563549215));
#168608=CARTESIAN_POINT('Ctrl Pts',(-5.93188769648226,-5.55684804811031,
65.8229697339901));
#168609=CARTESIAN_POINT('Ctrl Pts',(-5.78090372687759,-5.70971449926113,
65.8313831130587));
#168610=CARTESIAN_POINT('Ctrl Pts',(-5.73833268764744,-5.75281631799033,
65.8337553270847));
#168611=CARTESIAN_POINT('Ctrl Pts',(-5.69527739883983,-5.7954442227784,
65.8361275411106));
#168612=CARTESIAN_POINT('Ctrl Pts',(-5.65174840765014,-5.83758747250301,
65.8384997551366));
#168613=CARTESIAN_POINT('Ctrl Pts',(-5.50981146935305,-5.97500586131276,
65.8462349400473));
#168614=CARTESIAN_POINT('Ctrl Pts',(-5.36277205502693,-6.10732929945869,
65.853970124958));
#168615=CARTESIAN_POINT('Ctrl Pts',(-5.21104173523728,-6.23415845131604,
65.8617053098687));
#168616=CARTESIAN_POINT('Ctrl Pts',(-5.05935833421132,-6.36094838446606,
65.8694381028691));
#168617=CARTESIAN_POINT('Ctrl Pts',(-4.90298718710356,-6.482247188371,65.8771708958695));
#168618=CARTESIAN_POINT('Ctrl Pts',(-4.74237469106222,-6.59769428301073,
65.8849036888699));
#168619=CARTESIAN_POINT('Ctrl Pts',(-4.58178332418309,-6.71312619016226,
65.892635464593));
#168620=CARTESIAN_POINT('Ctrl Pts',(-4.41695200700344,-6.82270771587853,
65.9003672403161));
#168621=CARTESIAN_POINT('Ctrl Pts',(-4.24835810269068,-6.9261201977588,
65.9080990160393));
#168622=CARTESIAN_POINT('Ctrl Pts',(-4.07970387087586,-7.02956968344856,
65.9158335584029));
#168623=CARTESIAN_POINT('Ctrl Pts',(-3.90728466128152,-7.12684552647708,
65.9235681007666));
#168624=CARTESIAN_POINT('Ctrl Pts',(-3.73160512545452,-7.21767349983231,
65.9313026431302));
#168625=CARTESIAN_POINT('Ctrl Pts',(-3.5558959193128,-7.30851681301947,
65.9390384917717));
#168626=CARTESIAN_POINT('Ctrl Pts',(-3.37692560721234,-7.39290993116816,
65.9467743404133));
#168627=CARTESIAN_POINT('Ctrl Pts',(-3.1952211884978,-7.47062575150667,
65.9545101890549));
#168628=CARTESIAN_POINT('Ctrl Pts',(-3.01336809100004,-7.54840516244847,
65.9622523675181));
#168629=CARTESIAN_POINT('Ctrl Pts',(-2.82877674517088,-7.61949622739521,
65.9699945459813));
#168630=CARTESIAN_POINT('Ctrl Pts',(-2.6419926466829,-7.68372061031461,
65.9777367244445));
#168631=CARTESIAN_POINT('Ctrl Pts',(-2.48573569257516,-7.73744845190108,
65.9842135564373));
#168632=CARTESIAN_POINT('Ctrl Pts',(-2.32794456532243,-7.78637155989766,
65.99069038843));
#168633=CARTESIAN_POINT('Ctrl Pts',(-2.16894526312171,-7.83041276102875,
65.9971672204228));
#168634=CARTESIAN_POINT('Ctrl Pts',(-1.93823370989737,-7.89431753154146,
66.0065652488942));
#168635=CARTESIAN_POINT('Ctrl Pts',(-1.70484733732744,-7.94798006146225,
66.0159632773656));
#168636=CARTESIAN_POINT('Ctrl Pts',(-1.46961859860419,-7.99123949942289,
66.025361305837));
#168637=CARTESIAN_POINT('Ctrl Pts',(-1.23405514907411,-8.03456049194298,
66.0347727069163));
#168638=CARTESIAN_POINT('Ctrl Pts',(-0.996644126168747,-8.06744877566463,
66.0441841079956));
#168639=CARTESIAN_POINT('Ctrl Pts',(-0.758227768568692,-8.08979469538451,
66.053595509075));
#168640=CARTESIAN_POINT('Ctrl Pts',(-0.520170387033364,-8.11210696955085,
66.0629927397016));
#168641=CARTESIAN_POINT('Ctrl Pts',(-0.281110732766663,-8.12390860495421,
66.0723899703282));
#168642=CARTESIAN_POINT('Ctrl Pts',(-0.0418928781699178,-8.12514200179041,
66.0817872009548));
#168643=CARTESIAN_POINT('Ctrl Pts',(0.196721579760263,-8.12637228753968,
66.0911607282603));
#168644=CARTESIAN_POINT('Ctrl Pts',(0.435493403104585,-8.11708756041705,
66.1005342555657));
#168645=CARTESIAN_POINT('Ctrl Pts',(0.67357983644703,-8.09728212219582,
66.1099077828712));
#168646=CARTESIAN_POINT('Ctrl Pts',(0.910120150477342,-8.07760529932695,
66.119220439041));
#168647=CARTESIAN_POINT('Ctrl Pts',(1.1459839011936,-8.04754394588073,66.1285330952107));
#168648=CARTESIAN_POINT('Ctrl Pts',(1.38034027614664,-8.00714357836472,
66.1378457513805));
#168649=CARTESIAN_POINT('Ctrl Pts',(1.5312396315234,-7.98113024966235,66.1438420628234));
#168650=CARTESIAN_POINT('Ctrl Pts',(1.68151395299948,-7.95083147595598,
66.1498383742664));
#168651=CARTESIAN_POINT('Ctrl Pts',(1.83094063365618,-7.91627083660777,
66.1558346857094));
#168652=CARTESIAN_POINT('Ctrl Pts',(2.019524908843,-7.87265350473082,66.1634023439234));
#168653=CARTESIAN_POINT('Ctrl Pts',(2.20668353749748,-7.82226218231101,
66.1709700021374));
#168654=CARTESIAN_POINT('Ctrl Pts',(2.39187619588993,-7.76521833730611,
66.1785376603514));
#168655=CARTESIAN_POINT('Ctrl Pts',(2.5770175777641,-7.70819028671654,66.1861032232169));
#168656=CARTESIAN_POINT('Ctrl Pts',(2.76019372147561,-7.64451348672376,
66.1936687860824));
#168657=CARTESIAN_POINT('Ctrl Pts',(2.9408777532014,-7.5743597487329,66.2012343489479));
#168658=CARTESIAN_POINT('Ctrl Pts',(3.12154595529721,-7.50421215687296,
66.2087992489985));
#168659=CARTESIAN_POINT('Ctrl Pts',(3.2997221375484,-7.42758889031082,66.2163641490491));
#168660=CARTESIAN_POINT('Ctrl Pts',(3.47489782680054,-7.34471052226001,
66.2239290490998));
#168661=CARTESIAN_POINT('Ctrl Pts',(3.65015949119813,-7.26179147801846,
66.2314976619566));
#168662=CARTESIAN_POINT('Ctrl Pts',(3.82241738636469,-7.1726113536418,66.2390662748134));
#168663=CARTESIAN_POINT('Ctrl Pts',(3.99118564096093,-7.07743772433833,
66.2466348876702));
#168664=CARTESIAN_POINT('Ctrl Pts',(4.15999142665,-6.98224293009288,66.2542051836535));
#168665=CARTESIAN_POINT('Ctrl Pts',(4.32530571129203,-6.88105216643253,
66.2617754796367));
#168666=CARTESIAN_POINT('Ctrl Pts',(4.48667044834525,-6.77417713456368,
66.26934577562));
#168667=CARTESIAN_POINT('Ctrl Pts',(4.64819869387933,-6.66719380781938,
66.2769237424712));
#168668=CARTESIAN_POINT('Ctrl Pts',(4.8057690958993,-6.55451491788855,66.2845017093224));
#168669=CARTESIAN_POINT('Ctrl Pts',(4.95895490144321,-6.43649390957161,
66.2920796761737));
#168670=CARTESIAN_POINT('Ctrl Pts',(5.11004225487672,-6.32008964004515,
66.2995538344476));
#168671=CARTESIAN_POINT('Ctrl Pts',(5.2568641558625,-6.19848894671413,66.3070279927216));
#168672=CARTESIAN_POINT('Ctrl Pts',(5.3990461284708,-6.07206624347466,66.3145021509956));
#168673=CARTESIAN_POINT('Ctrl Pts',(5.55066229334044,-5.93725502186904,
66.3224722416642));
#168674=CARTESIAN_POINT('Ctrl Pts',(5.69734896901088,-5.79665286581093,
66.3304423323328));
#168675=CARTESIAN_POINT('Ctrl Pts',(5.83864923950696,-5.65065152177205,
66.3384124230014));
#168676=CARTESIAN_POINT('Ctrl Pts',(5.97984530484417,-5.50475784980767,
66.3463766359419));
#168677=CARTESIAN_POINT('Ctrl Pts',(6.11566265520476,-5.35347316287123,
66.3543408488824));
#168678=CARTESIAN_POINT('Ctrl Pts',(6.24567951906185,-5.1972276174583,66.362305061823));
#168679=CARTESIAN_POINT('Ctrl Pts',(6.37562157182863,-5.04107197499536,
66.3702646921929));
#168680=CARTESIAN_POINT('Ctrl Pts',(6.49976958184366,-4.87996141738763,
66.3782243225629));
#168681=CARTESIAN_POINT('Ctrl Pts',(6.61774022143442,-4.71436124242819,
66.3861839529329));
#168682=CARTESIAN_POINT('Ctrl Pts',(6.73946700311993,-4.54348841835689,
66.3943970150279));
#168683=CARTESIAN_POINT('Ctrl Pts',(6.85461631368951,-4.36783563087224,
66.4026100771228));
#168684=CARTESIAN_POINT('Ctrl Pts',(6.96281284365788,-4.18794995990794,
66.4108231392178));
#168685=CARTESIAN_POINT('Ctrl Pts',(7.06761032618024,-4.01371548617374,
66.4187781839092));
#168686=CARTESIAN_POINT('Ctrl Pts',(7.16588506826533,-3.83551035095584,
66.4267332286006));
#168687=CARTESIAN_POINT('Ctrl Pts',(7.25734064468932,-3.65386019566163,
66.434688273292));
#168688=CARTESIAN_POINT('Ctrl Pts',(7.34879156817336,-3.47221928209216,
66.4426429132586));
#168689=CARTESIAN_POINT('Ctrl Pts',(7.43342386938551,-3.28713399200113,
66.4505975532251));
#168690=CARTESIAN_POINT('Ctrl Pts',(7.51098757048573,-3.0991536390616,66.4585521931917));
#168691=CARTESIAN_POINT('Ctrl Pts',(7.58855872367093,-2.91115522554034,
66.4665075974159));
#168692=CARTESIAN_POINT('Ctrl Pts',(7.65905979750801,-2.7202614992951,66.4744630016401));
#168693=CARTESIAN_POINT('Ctrl Pts',(7.72228919296004,-2.52704119135257,
66.4824184058643));
#168694=CARTESIAN_POINT('Ctrl Pts',(7.78553395553669,-2.33377392359758,
66.4903757435513));
#168695=CARTESIAN_POINT('Ctrl Pts',(7.84150341454393,-2.13817926000058,
66.4983330812384));
#168696=CARTESIAN_POINT('Ctrl Pts',(7.8900458824695,-1.94084093501404,66.5062904189255));
#168697=CARTESIAN_POINT('Ctrl Pts',(7.93862466296796,-1.74335498954962,
66.5142537091613));
#168698=CARTESIAN_POINT('Ctrl Pts',(7.97976527492132,-1.5441230970558,66.5222169993971));
#168699=CARTESIAN_POINT('Ctrl Pts',(8.01336696446453,-1.34374009962063,
66.5301802896329));
#168700=CARTESIAN_POINT('Ctrl Pts',(8.0469835021482,-1.14326855559952,66.5381470987409));
#168701=CARTESIAN_POINT('Ctrl Pts',(8.07305442770735,-0.941645218064171,
66.5461139078489));
#168702=CARTESIAN_POINT('Ctrl Pts',(8.09153080529629,-0.739470614318915,
66.5540807169569));
#168703=CARTESIAN_POINT('Ctrl Pts',(8.11002432341238,-0.537108453285023,
66.5620549168701));
#168704=CARTESIAN_POINT('Ctrl Pts',(8.12090920015154,-0.334194332843433,
66.5700291167833));
#168705=CARTESIAN_POINT('Ctrl Pts',(8.12418856789581,-0.131330406878931,
66.5780033166966));
#168706=CARTESIAN_POINT('Ctrl Pts',(8.12491429954366,-0.0864361520226109,
66.5797680255351));
#168707=CARTESIAN_POINT('Ctrl Pts',(8.12526775567514,-0.0415443442075146,
66.5815327343737));
#168708=CARTESIAN_POINT('Ctrl Pts',(8.12524931413266,0.00333851565678357,
66.5832974432123));
#168709=CARTESIAN_POINT('',(8.12804752138609,-0.000138485946060349,68.5832974432123));
#168710=CARTESIAN_POINT('Ctrl Pts',(8.12588319212561,0.00333877610560675,
66.5832974432123));
#168711=CARTESIAN_POINT('Ctrl Pts',(8.1295781066157,0.41488469301549,66.5994773226644));
#168712=CARTESIAN_POINT('Ctrl Pts',(8.00961219341291,2.17106617787553,66.6685463572119));
#168713=CARTESIAN_POINT('Ctrl Pts',(6.72405806064653,5.12185486701279,66.790504546855));
#168714=CARTESIAN_POINT('Ctrl Pts',(2.38173522129256,8.63148943733764,67.0020611672368));
#168715=CARTESIAN_POINT('Ctrl Pts',(-3.67416070295623,8.17511883464795,
67.2136177876189));
#168716=CARTESIAN_POINT('Ctrl Pts',(-7.44199729007036,4.01675585914095,
67.4251744080006));
#168717=CARTESIAN_POINT('Ctrl Pts',(-8.47097384492055,-0.00353968824724416,
67.5838418732871));
#168718=CARTESIAN_POINT('Ctrl Pts',(-7.43229334537619,-4.06791197667408,
67.7425093385735));
#168719=CARTESIAN_POINT('Ctrl Pts',(-4.58332861377674,-7.11692082205451,
67.9011768038601));
#168720=CARTESIAN_POINT('Ctrl Pts',(-0.628874882635375,-8.44934367887127,
68.0598442691463));
#168721=CARTESIAN_POINT('Ctrl Pts',(3.5010973142339,-7.7136066795621,68.2185117344329));
#168722=CARTESIAN_POINT('Ctrl Pts',(6.73558121933879,-5.11366765981602,
68.3771791997192));
#168723=CARTESIAN_POINT('Ctrl Pts',(8.01567158785016,-2.15330402273112,
68.4987744359791));
#168724=CARTESIAN_POINT('Ctrl Pts',(8.13188959766798,-0.403006519366052,
68.5674805171434));
#168725=CARTESIAN_POINT('Ctrl Pts',(8.12804752138609,-0.000138485946060349,
68.5832974432123));
#168726=CARTESIAN_POINT('',(8.12524925928675,-0.00225863613891466,70.5832974432123));
#168727=CARTESIAN_POINT('Ctrl Pts',(8.12524999882064,-0.000138438281777881,
68.5832974432123));
#168728=CARTESIAN_POINT('Ctrl Pts',(8.12525344319759,0.202019689155656,
68.5912370693852));
#168729=CARTESIAN_POINT('Ctrl Pts',(8.11770794645236,0.40434051216219,68.5991766955581));
#168730=CARTESIAN_POINT('Ctrl Pts',(8.10260312143478,0.606226211092314,
68.607116321731));
#168731=CARTESIAN_POINT('Ctrl Pts',(8.08750875266733,0.807972155516052,
68.6150504517318));
#168732=CARTESIAN_POINT('Ctrl Pts',(8.06486551056691,1.00928324548818,68.6229845817327));
#168733=CARTESIAN_POINT('Ctrl Pts',(8.03471506847395,1.20956245433532,68.6309187117335));
#168734=CARTESIAN_POINT('Ctrl Pts',(8.00458042802503,1.40973669819528,68.6388486835101));
#168735=CARTESIAN_POINT('Ctrl Pts',(7.96694648021616,1.60887981058078,68.6467786552868));
#168736=CARTESIAN_POINT('Ctrl Pts',(7.92190669876364,1.80640023765051,68.6547086270634));
#168737=CARTESIAN_POINT('Ctrl Pts',(7.87493732643615,2.01238281976186,68.6629783340849));
#168738=CARTESIAN_POINT('Ctrl Pts',(7.81991362556992,2.21660024398525,68.6712480411063));
#168739=CARTESIAN_POINT('Ctrl Pts',(7.75700099036818,2.4183926889418,68.6795177481278));
#168740=CARTESIAN_POINT('Ctrl Pts',(7.69669787882304,2.61181507982017,68.6874444398545));
#168741=CARTESIAN_POINT('Ctrl Pts',(7.62914716804387,2.80300925359413,68.6953711315812));
#168742=CARTESIAN_POINT('Ctrl Pts',(7.55454566102255,2.99140893527202,68.703297823308));
#168743=CARTESIAN_POINT('Ctrl Pts',(7.47994280837504,3.17981201521298,68.7112246580126));
#168744=CARTESIAN_POINT('Ctrl Pts',(7.39828902825326,3.36542019290255,68.7191514927172));
#168745=CARTESIAN_POINT('Ctrl Pts',(7.30982958087123,3.54768643782395,68.7270783274218));
#168746=CARTESIAN_POINT('Ctrl Pts',(7.22135505292155,3.72998375549695,68.7350065134932));
#168747=CARTESIAN_POINT('Ctrl Pts',(7.12607269037901,3.90893770524193,68.7429346995647));
#168748=CARTESIAN_POINT('Ctrl Pts',(7.02427426820815,4.08402480005801,68.7508628856362));
#168749=CARTESIAN_POINT('Ctrl Pts',(6.92244297212418,4.25916843600526,68.7587936319684));
#168750=CARTESIAN_POINT('Ctrl Pts',(6.81409158925194,4.43044244026811,68.7667243783005));
#168751=CARTESIAN_POINT('Ctrl Pts',(6.69955607677724,4.59735096948418,68.7746551246327));
#168752=CARTESIAN_POINT('Ctrl Pts',(6.58491859003713,4.76440810217083,68.7825929319367));
#168753=CARTESIAN_POINT('Ctrl Pts',(6.46408616331075,4.92709172093237,68.7905307392408));
#168754=CARTESIAN_POINT('Ctrl Pts',(6.3374367117051,5.08493692071322,68.7984685465448));
#168755=CARTESIAN_POINT('Ctrl Pts',(6.21072145558343,5.24286413369543,68.8064104781744));
#168756=CARTESIAN_POINT('Ctrl Pts',(6.07818336292514,5.39594766144925,68.814352409804));
#168757=CARTESIAN_POINT('Ctrl Pts',(5.94023870550447,5.54375790273408,68.8222943414336));
#168758=CARTESIAN_POINT('Ctrl Pts',(5.80214559088934,5.69172721863727,68.8302448202364));
#168759=CARTESIAN_POINT('Ctrl Pts',(5.65863452315447,5.83441167634531,68.8381952990393));
#168760=CARTESIAN_POINT('Ctrl Pts',(5.51015728330688,5.97141978726334,68.8461457778421));
#168761=CARTESIAN_POINT('Ctrl Pts',(5.46635871370853,6.01183513501455,68.8484910504209));
#168762=CARTESIAN_POINT('Ctrl Pts',(5.42212821852692,6.05175682146519,68.8508363229997));
#168763=CARTESIAN_POINT('Ctrl Pts',(5.37747790964115,6.09117549359904,68.8531815955785));
#168764=CARTESIAN_POINT('Ctrl Pts',(5.22368644638327,6.22694734867524,68.8612595442115));
#168765=CARTESIAN_POINT('Ctrl Pts',(5.06457738629581,6.3570440359296,68.8693374928446));
#168766=CARTESIAN_POINT('Ctrl Pts',(4.90059376393837,6.48103913916189,68.8774154414776));
#168767=CARTESIAN_POINT('Ctrl Pts',(4.73681082423041,6.60488249757064,68.8854835043421));
#168768=CARTESIAN_POINT('Ctrl Pts',(4.56816546328188,6.72263896752202,68.8935515672066));
#168769=CARTESIAN_POINT('Ctrl Pts',(4.39513582047105,6.83392044745271,68.9016196300711));
#168770=CARTESIAN_POINT('Ctrl Pts',(4.22229662866159,6.94507944161194,68.9096788125459));
#168771=CARTESIAN_POINT('Ctrl Pts',(4.04508303914585,7.04977748374946,68.9177379950208));
#168772=CARTESIAN_POINT('Ctrl Pts',(3.86400487316773,7.14766772469426,68.9257971774957));
#168773=CARTESIAN_POINT('Ctrl Pts',(3.68315929576284,7.24543222904707,68.9338460082324));
#168774=CARTESIAN_POINT('Ctrl Pts',(3.49845932115371,7.33640622748188,68.9418948389691));
#168775=CARTESIAN_POINT('Ctrl Pts',(3.31044228304972,7.42028701959005,68.9499436697058));
#168776=CARTESIAN_POINT('Ctrl Pts',(3.12256746018415,7.50410436464593,68.9579864123433));
#168777=CARTESIAN_POINT('Ctrl Pts',(2.93138086200307,7.58083906962743,68.9660291549808));
#168778=CARTESIAN_POINT('Ctrl Pts',(2.73744408463825,7.65023447000019,68.9740718976183));
#168779=CARTESIAN_POINT('Ctrl Pts',(2.54366527608003,7.7195733452067,68.9821080891391));
#168780=CARTESIAN_POINT('Ctrl Pts',(2.34714105325024,7.78158473475308,68.99014428066));
#168781=CARTESIAN_POINT('Ctrl Pts',(2.1484529019483,7.83606008722559,68.9981804721808));
#168782=CARTESIAN_POINT('Ctrl Pts',(2.03580473979545,7.86694541329283,69.0027366684089));
#168783=CARTESIAN_POINT('Ctrl Pts',(1.92246136079458,7.89540920653068,69.007292864637));
#168784=CARTESIAN_POINT('Ctrl Pts',(1.80853123420579,7.92142047472561,69.0118490608651));
#168785=CARTESIAN_POINT('Ctrl Pts',(1.60757388525393,7.96730083715331,69.0198855753737));
#168786=CARTESIAN_POINT('Ctrl Pts',(1.40494924650344,8.00551172220066,69.0279220898824));
#168787=CARTESIAN_POINT('Ctrl Pts',(1.20126884395045,8.03595922880734,69.035958604391));
#168788=CARTESIAN_POINT('Ctrl Pts',(0.997465398160986,8.06642512873862,
69.0439999737544));
#168789=CARTESIAN_POINT('Ctrl Pts',(0.792605228504791,8.08911824702432,
69.0520413431177));
#168790=CARTESIAN_POINT('Ctrl Pts',(0.587305116801611,8.10399656109741,
69.060082712481));
#168791=CARTESIAN_POINT('Ctrl Pts',(0.381855881596666,8.11888568230682,
69.0681299228405));
#168792=CARTESIAN_POINT('Ctrl Pts',(0.175966381454576,8.12594865147517,
69.0761771332));
#168793=CARTESIAN_POINT('Ctrl Pts',(-0.0297458548209949,8.12519555128496,
69.0842243435594));
#168794=CARTESIAN_POINT('Ctrl Pts',(-0.235761296243941,8.12444134107885,
69.0922834149323));
#168795=CARTESIAN_POINT('Ctrl Pts',(-0.441598635417027,8.11584803745462,
69.1003424863052));
#168796=CARTESIAN_POINT('Ctrl Pts',(-0.646642958207808,8.09947778854293,
69.1084015576781));
#168797=CARTESIAN_POINT('Ctrl Pts',(-0.851853233428813,8.08309429038565,
69.1164671516529));
#168798=CARTESIAN_POINT('Ctrl Pts',(-1.05626889843344,8.05892132320359,
69.1245327456277));
#168799=CARTESIAN_POINT('Ctrl Pts',(-1.25928359552268,8.02707246688028,
69.1325983396025));
#168800=CARTESIAN_POINT('Ctrl Pts',(-1.46261707206923,7.99517360057602,
69.1406765984025));
#168801=CARTESIAN_POINT('Ctrl Pts',(-1.66454487389827,7.95557481397755,
69.1487548572026));
#168802=CARTESIAN_POINT('Ctrl Pts',(-1.86447247307778,7.90844042524411,
69.1568331160026));
#168803=CARTESIAN_POINT('Ctrl Pts',(-1.97735535239345,7.88182746366776,
69.1613942527189));
#168804=CARTESIAN_POINT('Ctrl Pts',(-2.08960086992019,7.8528130957757,69.1659553894351));
#168805=CARTESIAN_POINT('Ctrl Pts',(-2.20110462444749,7.82143375569568,
69.1705165261514));
#168806=CARTESIAN_POINT('Ctrl Pts',(-2.398783627965,7.76580301299692,69.1786027198836));
#168807=CARTESIAN_POINT('Ctrl Pts',(-2.59451489447767,7.70262817661812,
69.1866889136157));
#168808=CARTESIAN_POINT('Ctrl Pts',(-2.78770264090589,7.63206404247149,
69.1947751073479));
#168809=CARTESIAN_POINT('Ctrl Pts',(-2.98071807303147,7.56156284818411,
69.202854088579));
#168810=CARTESIAN_POINT('Ctrl Pts',(-3.17119421250627,7.48368560593843,
69.2109330698101));
#168811=CARTESIAN_POINT('Ctrl Pts',(-3.35854991814908,7.39863703730632,
69.2190120510412));
#168812=CARTESIAN_POINT('Ctrl Pts',(-3.54576409581162,7.313652714127,69.2270849294323));
#168813=CARTESIAN_POINT('Ctrl Pts',(-3.72986225259659,7.22150799738674,
69.2351578078233));
#168814=CARTESIAN_POINT('Ctrl Pts',(-3.91028215388211,7.12245611004596,
69.2432306862144));
#168815=CARTESIAN_POINT('Ctrl Pts',(-4.09059036718786,7.02346554024892,
69.2512985671331));
#168816=CARTESIAN_POINT('Ctrl Pts',(-4.2672245889835,6.91757647912846,69.2593664480517));
#168817=CARTESIAN_POINT('Ctrl Pts',(-4.43964561493808,6.80508885880714,
69.2674343289704));
#168818=CARTESIAN_POINT('Ctrl Pts',(-4.61198338564122,6.6926555542809,69.2754983142305));
#168819=CARTESIAN_POINT('Ctrl Pts',(-4.78011175321662,6.57363021815613,
69.2835622994905));
#168820=CARTESIAN_POINT('Ctrl Pts',(-4.94351849471029,6.44835734547624,
69.2916262847506));
#168821=CARTESIAN_POINT('Ctrl Pts',(-5.10919606664058,6.32134358102184,
69.2998023335828));
#168822=CARTESIAN_POINT('Ctrl Pts',(-5.27001952312414,6.18790751886747,
69.307978382415));
#168823=CARTESIAN_POINT('Ctrl Pts',(-5.42548673598591,6.04845279721524,
69.3161544312473));
#168824=CARTESIAN_POINT('Ctrl Pts',(-5.57875041610606,5.91097465338595,
69.3242145958942));
#168825=CARTESIAN_POINT('Ctrl Pts',(-5.72680844615076,5.76764755740925,
69.3322747605412));
#168826=CARTESIAN_POINT('Ctrl Pts',(-5.86921397705197,5.61889801064922,
69.3403349251881));
#168827=CARTESIAN_POINT('Ctrl Pts',(-6.01161262763258,5.47015565072081,
69.3483947004084));
#168828=CARTESIAN_POINT('Ctrl Pts',(-6.14835910480783,5.31599159142366,
69.3564544756286));
#168829=CARTESIAN_POINT('Ctrl Pts',(-6.27904409057477,5.15686851404203,
69.3645142508489));
#168830=CARTESIAN_POINT('Ctrl Pts',(-6.40973894322415,4.99773342266593,
69.3725746345924));
#168831=CARTESIAN_POINT('Ctrl Pts',(-6.53437119109374,4.83363881160464,
69.3806350183359));
#168832=CARTESIAN_POINT('Ctrl Pts',(-6.65257203831887,4.66508015338193,
69.3886954020794));
#168833=CARTESIAN_POINT('Ctrl Pts',(-6.77374420207106,4.4922842909537,69.3969584066332));
#168834=CARTESIAN_POINT('Ctrl Pts',(-6.88815717651778,4.31479728879599,
69.4052214111869));
#168835=CARTESIAN_POINT('Ctrl Pts',(-6.99546100379646,4.13318435432816,
69.4134844157406));
#168836=CARTESIAN_POINT('Ctrl Pts',(-7.10021966181955,3.95587914744978,
69.4215514277964));
#168837=CARTESIAN_POINT('Ctrl Pts',(-7.19820245827846,3.77464180923979,
69.4296184398521));
#168838=CARTESIAN_POINT('Ctrl Pts',(-7.28913027432016,3.59002331559133,
69.4376854519079));
#168839=CARTESIAN_POINT('Ctrl Pts',(-7.3833718023676,3.39867671006777,69.4460464527106));
#168840=CARTESIAN_POINT('Ctrl Pts',(-7.47003431566797,3.20369821651608,
69.4544074535133));
#168841=CARTESIAN_POINT('Ctrl Pts',(-7.54886142882182,3.00572432051681,
69.462768454316));
#168842=CARTESIAN_POINT('Ctrl Pts',(-7.62768854197567,2.80775042451753,
69.4711294551187));
#168843=CARTESIAN_POINT('Ctrl Pts',(-7.69868015206915,2.60678148964838,
69.4794904559214));
#168844=CARTESIAN_POINT('Ctrl Pts',(-7.76163701836296,2.40347214622466,
69.4878514567241));
#168845=CARTESIAN_POINT('Ctrl Pts',(-7.81869986977612,2.21919660111488,
69.4954297015536));
#168846=CARTESIAN_POINT('Ctrl Pts',(-7.86927612804514,2.03262899477647,
69.503007946383));
#168847=CARTESIAN_POINT('Ctrl Pts',(-7.91317228702314,1.84428628970369,
69.5105861912125));
#168848=CARTESIAN_POINT('Ctrl Pts',(-7.95703578171511,1.65608373538968,
69.5181587968707));
#168849=CARTESIAN_POINT('Ctrl Pts',(-7.99422898302738,1.46610906559233,
69.5257314025289));
#168850=CARTESIAN_POINT('Ctrl Pts',(-8.02460762374933,1.27489609277155,
69.5333040081872));
#168851=CARTESIAN_POINT('Ctrl Pts',(-8.05496942774856,1.08378909571946,
69.540872416888));
#168852=CARTESIAN_POINT('Ctrl Pts',(-8.07852412904685,0.891445523010382,
69.5484408255888));
#168853=CARTESIAN_POINT('Ctrl Pts',(-8.09517816705029,0.698411058197308,
69.5560092342896));
#168854=CARTESIAN_POINT('Ctrl Pts',(-8.11182818130514,0.505423232052618,
69.5635758144024));
#168855=CARTESIAN_POINT('Ctrl Pts',(-8.12158081122413,0.311745211072521,
69.5711423945152));
#168856=CARTESIAN_POINT('Ctrl Pts',(-8.12439414114411,0.117929647854879,
69.578708974628));
#168857=CARTESIAN_POINT('Ctrl Pts',(-8.12720697199211,-0.0758515333592844,
69.5862742124638));
#168858=CARTESIAN_POINT('Ctrl Pts',(-8.12308295086828,-0.269769840524452,
69.5938394502995));
#168859=CARTESIAN_POINT('Ctrl Pts',(-8.11203226742937,-0.463271038037836,
69.6014046881353));
#168860=CARTESIAN_POINT('Ctrl Pts',(-8.10097774113757,-0.656839525202663,
69.6089725567673));
#168861=CARTESIAN_POINT('Ctrl Pts',(-8.08299175809912,-0.849990245181151,
69.6165404253993));
#168862=CARTESIAN_POINT('Ctrl Pts',(-8.05813657349613,-1.04217202293288,
69.6241082940312));
#168863=CARTESIAN_POINT('Ctrl Pts',(-8.03360213178454,-1.23187379741549,
69.6315785033577));
#168864=CARTESIAN_POINT('Ctrl Pts',(-8.0023748037713,-1.42063114910066,
69.6390487126842));
#168865=CARTESIAN_POINT('Ctrl Pts',(-7.96456353516324,-1.60792265263227,
69.6465189220106));
#168866=CARTESIAN_POINT('Ctrl Pts',(-7.91746101700683,-1.84123673519016,
69.6558247634538));
#168867=CARTESIAN_POINT('Ctrl Pts',(-7.86016659033934,-2.07216192790768,
69.665130604897));
#168868=CARTESIAN_POINT('Ctrl Pts',(-7.79295243627307,-2.29990866959661,
69.6744364463401));
#168869=CARTESIAN_POINT('Ctrl Pts',(-7.72537742297348,-2.52887813759577,
69.6837922489686));
#168870=CARTESIAN_POINT('Ctrl Pts',(-7.64777594680264,-2.75463490548582,
69.6931480515972));
#168871=CARTESIAN_POINT('Ctrl Pts',(-7.56047079908319,-2.97640199884195,
69.7025038542257));
#168872=CARTESIAN_POINT('Ctrl Pts',(-7.47274183243766,-3.1992456506119,
69.7119050741787));
#168873=CARTESIAN_POINT('Ctrl Pts',(-7.3752147911953,-3.41806076796294,
69.7213062941316));
#168874=CARTESIAN_POINT('Ctrl Pts',(-7.26826294017853,-3.6320849928006,
69.7307075140846));
#168875=CARTESIAN_POINT('Ctrl Pts',(-7.16119533552177,-3.84634085535968,
69.7401189089474));
#168876=CARTESIAN_POINT('Ctrl Pts',(-7.04468254438493,-4.05579542565818,
69.7495303038101));
#168877=CARTESIAN_POINT('Ctrl Pts',(-6.91914419246585,-4.25971022563344,
69.7589416986728));
#168878=CARTESIAN_POINT('Ctrl Pts',(-6.79375309913894,-4.46338583012853,
69.7683420538115));
#168879=CARTESIAN_POINT('Ctrl Pts',(-6.65935762960811,-4.66153462439478,
69.7777424089503));
#168880=CARTESIAN_POINT('Ctrl Pts',(-6.51642049528494,-4.85344738213266,
69.787142764089));
#168881=CARTESIAN_POINT('Ctrl Pts',(-6.42496636913281,-4.97623712210801,
69.7931573051584));
#168882=CARTESIAN_POINT('Ctrl Pts',(-6.33001643253913,-5.09647454965942,
69.7991718462278));
#168883=CARTESIAN_POINT('Ctrl Pts',(-6.2317014366177,-5.21397974366577,
69.8051863872972));
#168884=CARTESIAN_POINT('Ctrl Pts',(-6.1051441417948,-5.36523987790784,
69.8129286858165));
#168885=CARTESIAN_POINT('Ctrl Pts',(-5.97294893326488,-5.51204162850269,
69.8206709843357));
#168886=CARTESIAN_POINT('Ctrl Pts',(-5.83546962283214,-5.65393507598941,
69.828413282855));
#168887=CARTESIAN_POINT('Ctrl Pts',(-5.69807594956039,-5.79574013670746,
69.8361507586234));
#168888=CARTESIAN_POINT('Ctrl Pts',(-5.55540497295844,-5.93264272934101,
69.8438882343919));
#168889=CARTESIAN_POINT('Ctrl Pts',(-5.40785040869798,-6.06422637437333,
69.8516257101603));
#168890=CARTESIAN_POINT('Ctrl Pts',(-5.26036153288048,-6.19575144090756,
69.8593597413539));
#168891=CARTESIAN_POINT('Ctrl Pts',(-5.10799366244056,-6.32196204114079,
69.8670937725474));
#168892=CARTESIAN_POINT('Ctrl Pts',(-4.95117705388402,-6.44247881980161,
69.874827803741));
#168893=CARTESIAN_POINT('Ctrl Pts',(-4.79438051291575,-6.56298017610943,
69.8825608452221));
#168894=CARTESIAN_POINT('Ctrl Pts',(-4.63313664303813,-6.67778894092404,
69.8902938867033));
#168895=CARTESIAN_POINT('Ctrl Pts',(-4.4679087276712,-6.78656608040469,
69.8980269281844));
#168896=CARTESIAN_POINT('Ctrl Pts',(-4.30269731844904,-6.89533235313072,
69.9057591971405));
#168897=CARTESIAN_POINT('Ctrl Pts',(-4.13350295367036,-6.99806800943472,
69.9134914660965));
#168898=CARTESIAN_POINT('Ctrl Pts',(-3.96081772784706,-7.09447746414578,
69.9212237350526));
#168899=CARTESIAN_POINT('Ctrl Pts',(-3.7880660778721,-7.19092400318882,
69.9289589782609));
#168900=CARTESIAN_POINT('Ctrl Pts',(-3.61182119289309,-7.28103930645225,
69.9366942214691));
#168901=CARTESIAN_POINT('Ctrl Pts',(-3.4326001621191,-7.36457355788642,
69.9444294646774));
#168902=CARTESIAN_POINT('Ctrl Pts',(-3.28258295175857,-7.43449601796597,
69.9509042606461));
#168903=CARTESIAN_POINT('Ctrl Pts',(-3.13048101536807,-7.49980820338466,
69.9573790566147));
#168904=CARTESIAN_POINT('Ctrl Pts',(-2.97660830846107,-7.56038957597428,
69.9638538525834));
#168905=CARTESIAN_POINT('Ctrl Pts',(-2.7766488925416,-7.63911579144238,
69.9722679270878));
#168906=CARTESIAN_POINT('Ctrl Pts',(-2.57360250103078,-7.7098901782334,
69.9806820015921));
#168907=CARTESIAN_POINT('Ctrl Pts',(-2.36810602907813,-7.77250033113822,
69.9890960760964));
#168908=CARTESIAN_POINT('Ctrl Pts',(-2.16255216761608,-7.83512796933574,
69.9975125004202));
#168909=CARTESIAN_POINT('Ctrl Pts',(-1.95454711231985,-7.88958674496606,
70.005928924744));
#168910=CARTESIAN_POINT('Ctrl Pts',(-1.74474219750444,-7.93571434886283,
70.0143453490678));
#168911=CARTESIAN_POINT('Ctrl Pts',(-1.53488525253141,-7.98185339208409,
70.0227638606061));
#168912=CARTESIAN_POINT('Ctrl Pts',(-1.32322781472788,-8.01965708218385,
70.0311823721446));
#168913=CARTESIAN_POINT('Ctrl Pts',(-1.11043174996157,-8.04901415647763,
70.039600883683));
#168914=CARTESIAN_POINT('Ctrl Pts',(-0.897553951114326,-8.0783825067012,
70.0480226287365));
#168915=CARTESIAN_POINT('Ctrl Pts',(-0.683536912744339,-8.09929772052912,
70.0564443737901));
#168916=CARTESIAN_POINT('Ctrl Pts',(-0.469049400935833,-8.11170020538122,
70.0648661188436));
#168917=CARTESIAN_POINT('Ctrl Pts',(-0.254538639266971,-8.12410403462879,
70.0732887767913));
#168918=CARTESIAN_POINT('Ctrl Pts',(-0.0395575660154435,-8.12799328029952,
70.0817114347391));
#168919=CARTESIAN_POINT('Ctrl Pts',(0.175222646691773,-8.1233604245156,
70.0901340926868));
#168920=CARTESIAN_POINT('Ctrl Pts',(0.390043704415167,-8.11872668769582,
70.0985583523817));
#168921=CARTESIAN_POINT('Ctrl Pts',(0.60466356141743,-8.10556761748978,
70.1069826120766));
#168922=CARTESIAN_POINT('Ctrl Pts',(0.818412432624915,-8.08392779857817,
70.1154068717715));
#168923=CARTESIAN_POINT('Ctrl Pts',(0.878584082831494,-8.07783605359385,
70.1177783538043));
#168924=CARTESIAN_POINT('Ctrl Pts',(0.938686735209647,-8.07107256111987,
70.1201498358372));
#168925=CARTESIAN_POINT('Ctrl Pts',(0.998705517655859,-8.0636390576156,
70.1225213178701));
#168926=CARTESIAN_POINT('Ctrl Pts',(1.21191301222614,-8.03723267958807,
70.1309456430902));
#168927=CARTESIAN_POINT('Ctrl Pts',(1.42408360115664,-8.00236463516795,
70.1393699683103));
#168928=CARTESIAN_POINT('Ctrl Pts',(1.63455445124467,-7.95914061368539,
70.1477942935305));
#168929=CARTESIAN_POINT('Ctrl Pts',(1.84498892939666,-7.91592406184219,
70.1562171629242));
#168930=CARTESIAN_POINT('Ctrl Pts',(2.05372399698473,-7.86435447014295,
70.1646400323179));
#168931=CARTESIAN_POINT('Ctrl Pts',(2.26010706148907,-7.80458862676997,
70.1730629017116));
#168932=CARTESIAN_POINT('Ctrl Pts',(2.46644795126601,-7.74483499664792,
70.1814840498778));
#168933=CARTESIAN_POINT('Ctrl Pts',(2.67043754439279,-7.67688853292304,
70.189905198044));
#168934=CARTESIAN_POINT('Ctrl Pts',(2.87143739663591,-7.60095617930407,
70.1983263462101));
#168935=CARTESIAN_POINT('Ctrl Pts',(3.07238085510465,-7.52504512974066,
70.2067451316864));
#168936=CARTESIAN_POINT('Ctrl Pts',(3.27033600131845,-7.44115275850611,
70.2151639171626));
#168937=CARTESIAN_POINT('Ctrl Pts',(3.46468244641396,-7.34953489059076,
70.2235827026388));
#168938=CARTESIAN_POINT('Ctrl Pts',(3.65897460213065,-7.25794261551369,
70.2319991363836));
#168939=CARTESIAN_POINT('Ctrl Pts',(3.84965983089612,-7.15862926501837,
70.2404155701284));
#168940=CARTESIAN_POINT('Ctrl Pts',(4.03613945280823,-7.05189803386187,
70.2488320038733));
#168941=CARTESIAN_POINT('Ctrl Pts',(4.22255139345792,-6.94520553993782,
70.2572453829419));
#168942=CARTESIAN_POINT('Ctrl Pts',(4.4047605465545,-6.83110067273071,70.2656587620106));
#168943=CARTESIAN_POINT('Ctrl Pts',(4.58219361943055,-6.70993213054722,
70.2740721410792));
#168944=CARTESIAN_POINT('Ctrl Pts',(4.63222217759542,-6.67576777008093,
70.2764443551049));
#168945=CARTESIAN_POINT('Ctrl Pts',(4.6818712003028,-6.64104212099621,70.2788165691306));
#168946=CARTESIAN_POINT('Ctrl Pts',(4.73112823130388,-6.60576363651164,
70.2811887831563));
#168947=CARTESIAN_POINT('Ctrl Pts',(4.89174284651827,-6.49072949629494,
70.2889239680669));
#168948=CARTESIAN_POINT('Ctrl Pts',(5.0482586039032,-6.36976297473629,70.2966591529776));
#168949=CARTESIAN_POINT('Ctrl Pts',(5.20020892040662,-6.24319747778519,
70.3043943378882));
#168950=CARTESIAN_POINT('Ctrl Pts',(5.35211225011853,-6.11667111801232,
70.3121271308886));
#168951=CARTESIAN_POINT('Ctrl Pts',(5.49945267918814,-5.98454945651013,
70.319859923889));
#168952=CARTESIAN_POINT('Ctrl Pts',(5.64179551706581,-5.84720710306349,
70.3275927168894));
#168953=CARTESIAN_POINT('Ctrl Pts',(5.78411962922179,-5.70988281750649,
70.3353244926126));
#168954=CARTESIAN_POINT('Ctrl Pts',(5.92144720608923,-5.56733945381257,
70.3430562683357));
#168955=CARTESIAN_POINT('Ctrl Pts',(6.05337925185845,-5.41998959368647,
70.3507880440589));
#168956=CARTESIAN_POINT('Ctrl Pts',(6.18535850651505,-5.27258700775814,
70.3585225864225));
#168957=CARTESIAN_POINT('Ctrl Pts',(6.31193813369625,-5.12037474985404,
70.366257128786));
#168958=CARTESIAN_POINT('Ctrl Pts',(6.43275796798117,-4.96380020628095,
70.3739916711496));
#168959=CARTESIAN_POINT('Ctrl Pts',(6.55359820738985,-4.80719921901209,
70.3817275197912));
#168960=CARTESIAN_POINT('Ctrl Pts',(6.6686765057568,-4.64623476253393,70.3894633684328));
#168961=CARTESIAN_POINT('Ctrl Pts',(6.77767505817898,-4.48138464854765,
70.3971992170744));
#168962=CARTESIAN_POINT('Ctrl Pts',(6.88676279815156,-4.31639964673467,
70.4049413955375));
#168963=CARTESIAN_POINT('Ctrl Pts',(6.98976066427123,-4.14752293417595,
70.4126835740007));
#168964=CARTESIAN_POINT('Ctrl Pts',(7.08639551780897,-3.97525925288867,
70.4204257524639));
#168965=CARTESIAN_POINT('Ctrl Pts',(7.16723680996016,-3.83114956496384,
70.4269025844569));
#168966=CARTESIAN_POINT('Ctrl Pts',(7.24362577073828,-3.68467008855548,
70.4333794164498));
#168967=CARTESIAN_POINT('Ctrl Pts',(7.31542809573629,-3.53612773222521,
70.4398562484428));
#168968=CARTESIAN_POINT('Ctrl Pts',(7.420184286902,-3.31941147023267,70.4493056395373));
#168969=CARTESIAN_POINT('Ctrl Pts',(7.51523505090712,-3.09818594224481,
70.4587550306319));
#168970=CARTESIAN_POINT('Ctrl Pts',(7.60027053186312,-2.87325171277997,
70.4682044217264));
#168971=CARTESIAN_POINT('Ctrl Pts',(7.68658112354406,-2.64494458478887,
70.4777955068503));
#168972=CARTESIAN_POINT('Ctrl Pts',(7.76257371473142,-2.41281668831467,
70.4873865919741));
#168973=CARTESIAN_POINT('Ctrl Pts',(7.82797664972721,-2.17772108724364,
70.4969776770979));
#168974=CARTESIAN_POINT('Ctrl Pts',(7.89244276833816,-1.94599294072337,
70.5064313817557));
#168975=CARTESIAN_POINT('Ctrl Pts',(7.94662053333941,-1.71138155118103,
70.5158850864134));
#168976=CARTESIAN_POINT('Ctrl Pts',(7.99029987438044,-1.47471877996312,
70.5253387910712));
#168977=CARTESIAN_POINT('Ctrl Pts',(8.03493133236088,-1.23289726257288,
70.534998566428));
#168978=CARTESIAN_POINT('Ctrl Pts',(8.06860144480357,-0.988933912655596,
70.5446583417849));
#168979=CARTESIAN_POINT('Ctrl Pts',(8.09114023723057,-0.743731957070907,
70.5543181171418));
#168980=CARTESIAN_POINT('Ctrl Pts',(8.11367902965756,-0.498530001486218,
70.5639778924986));
#168981=CARTESIAN_POINT('Ctrl Pts',(8.12508640368432,-0.252089453203025,
70.5736376678555));
#168982=CARTESIAN_POINT('Ctrl Pts',(8.1252482522699,-0.00532930436001966,
70.5832974432123));
#168983=CARTESIAN_POINT('',(8.12479782686935,0.00219746833035057,72.5832974432123));
#168984=CARTESIAN_POINT('Ctrl Pts',(8.12525,-1.9191019467627E-12,70.5832974432123));
#168985=CARTESIAN_POINT('Ctrl Pts',(8.12525000000053,2.24624642433222,70.6712950363535));
#168986=CARTESIAN_POINT('Ctrl Pts',(7.14398562317703,4.47535249753288,70.7592926294947));
#168987=CARTESIAN_POINT('Ctrl Pts',(3.83078204045102,7.50935546634275,70.9352878157771));
#168988=CARTESIAN_POINT('Ctrl Pts',(1.5241247769793,8.29110090552103,71.0232854089183));
#168989=CARTESIAN_POINT('Ctrl Pts',(-2.95101623932386,7.89663306204491,
71.1992805952007));
#168990=CARTESIAN_POINT('Ctrl Pts',(-5.08535169588588,6.72342983085899,
71.2872781883419));
#168991=CARTESIAN_POINT('Ctrl Pts',(-7.81671694684337,3.1566195105311,71.4632733746243));
#168992=CARTESIAN_POINT('Ctrl Pts',(-8.39290461146686,0.790229551555905,
71.5512709677655));
#168993=CARTESIAN_POINT('Ctrl Pts',(-7.6070161146256,-3.63299000730257,
71.7272661540479));
#168994=CARTESIAN_POINT('Ctrl Pts',(-6.25093680401474,-5.65606750609891,
71.8152637471891));
#168995=CARTESIAN_POINT('Ctrl Pts',(-2.45807268688716,-8.0636957548827,
71.9912589334715));
#168996=CARTESIAN_POINT('Ctrl Pts',(-0.0502299510469964,-8.42987470330086,
72.0792565266128));
#168997=CARTESIAN_POINT('Ctrl Pts',(4.2868996088086,-7.25863639434643,72.2552517128951));
#168998=CARTESIAN_POINT('Ctrl Pts',(6.18309125557056,-5.73015646266494,
72.3432493060364));
#168999=CARTESIAN_POINT('Ctrl Pts',(7.81050559202848,-2.58640713800423,
72.4819304138558));
#169000=CARTESIAN_POINT('Ctrl Pts',(8.1252499999997,-1.29375883538323,72.5326139285341));
#169001=CARTESIAN_POINT('Ctrl Pts',(8.12525,-1.86335868540631E-12,72.5832974432123));
#169002=CARTESIAN_POINT('',(8.12465437257904,-0.000424865306044762,74.5832974342377));
#169003=CARTESIAN_POINT('Ctrl Pts',(8.12479782686935,0.00219746833035057,
72.5832974432123));
#169004=CARTESIAN_POINT('Ctrl Pts',(8.12460569558819,0.666438545426072,
72.6092652162925));
#169005=CARTESIAN_POINT('Ctrl Pts',(7.88015377287088,2.68210296929945,72.6881221444681));
#169006=CARTESIAN_POINT('Ctrl Pts',(6.23719048967404,5.71096367462421,72.8198682277392));
#169007=CARTESIAN_POINT('Ctrl Pts',(1.56871213603112,8.82446412344862,73.0314248481213));
#169008=CARTESIAN_POINT('Ctrl Pts',(-4.41553899415216,7.78962694628819,
73.2429814685029));
#169009=CARTESIAN_POINT('Ctrl Pts',(-7.77043274392739,3.32666936346098,
73.4545380888851));
#169010=CARTESIAN_POINT('Ctrl Pts',(-8.68429813962366,-2.18133867002485,
73.6660947092667));
#169011=CARTESIAN_POINT('Ctrl Pts',(-5.3027347685792,-7.22585834388306,
73.8776513296489));
#169012=CARTESIAN_POINT('Ctrl Pts',(0.172450800896261,-8.455052455108,74.0892079500306));
#169013=CARTESIAN_POINT('Ctrl Pts',(4.17773714921753,-7.36911953511191,
74.2478754153172));
#169014=CARTESIAN_POINT('Ctrl Pts',(7.20239531903236,-4.46233054468999,
74.4065428806035));
#169015=CARTESIAN_POINT('Ctrl Pts',(8.0825323422617,-1.65664906305872,74.5183502202438));
#169016=CARTESIAN_POINT('Ctrl Pts',(8.12471506055508,-0.154179418476278,
74.5772684047885));
#169017=CARTESIAN_POINT('Ctrl Pts',(8.12465437257904,-0.000424865306044762,
74.5832974342377));
#169018=CARTESIAN_POINT('',(8.12525,-2.44467206894639E-12,76.5832974432123));
#169019=CARTESIAN_POINT('Ctrl Pts',(8.12524998890234,-0.000424667563621383,
74.5832974432123));
#169020=CARTESIAN_POINT('Ctrl Pts',(8.12526121818894,0.21442753365117,74.5917216186074));
#169021=CARTESIAN_POINT('Ctrl Pts',(8.11674625019481,0.42929425617801,74.6001457940026));
#169022=CARTESIAN_POINT('Ctrl Pts',(8.09972773850733,0.643504564517582,
74.6085699693977));
#169023=CARTESIAN_POINT('Ctrl Pts',(8.08271252175064,0.857673399892047,
74.6169925137997));
#169024=CARTESIAN_POINT('Ctrl Pts',(8.05719707002555,1.07118581207959,74.6254150582018));
#169025=CARTESIAN_POINT('Ctrl Pts',(8.02325601111973,1.28337466958447,74.6338376026038));
#169026=CARTESIAN_POINT('Ctrl Pts',(7.98932386718398,1.49550779349196,74.6422579347375));
#169027=CARTESIAN_POINT('Ctrl Pts',(7.94697057779809,1.70631779677591,74.6506782668711));
#169028=CARTESIAN_POINT('Ctrl Pts',(7.89632228242461,1.91514541865222,74.6590985990048));
#169029=CARTESIAN_POINT('Ctrl Pts',(7.84568798915987,2.12391530853482,74.6675166032732));
#169030=CARTESIAN_POINT('Ctrl Pts',(7.78676333104568,2.33070365518239,74.6759346075416));
#169031=CARTESIAN_POINT('Ctrl Pts',(7.71972520522185,2.53486297822238,74.68435261181));
#169032=CARTESIAN_POINT('Ctrl Pts',(7.65271138678992,2.73894827501815,74.6927675637895));
#169033=CARTESIAN_POINT('Ctrl Pts',(7.57759005811987,2.94040620159464,74.7011825157691));
#169034=CARTESIAN_POINT('Ctrl Pts',(7.49458777931377,3.13860503737896,74.7095974677486));
#169035=CARTESIAN_POINT('Ctrl Pts',(7.44763559826222,3.25072084619541,74.7143575822245));
#169036=CARTESIAN_POINT('Ctrl Pts',(7.39816251895578,3.36179408452685,74.7191176967005));
#169037=CARTESIAN_POINT('Ctrl Pts',(7.34621646707142,3.47171300389717,74.7238778111764));
#169038=CARTESIAN_POINT('Ctrl Pts',(7.26180414490245,3.65033122217884,74.7316129960871));
#169039=CARTESIAN_POINT('Ctrl Pts',(7.17082132822503,3.8259791903351,74.7393481809978));
#169040=CARTESIAN_POINT('Ctrl Pts',(7.07351247945622,3.99813816237973,74.7470833659085));
#169041=CARTESIAN_POINT('Ctrl Pts',(6.9762337209877,4.17024389861659,74.7548161589088));
#169042=CARTESIAN_POINT('Ctrl Pts',(6.87263299960399,4.3388624800516,74.7625489519092));
#169043=CARTESIAN_POINT('Ctrl Pts',(6.76300102670223,4.50349915902341,74.7702817449096));
#169044=CARTESIAN_POINT('Ctrl Pts',(6.65338347628829,4.66811417943675,74.7780135206328));
#169045=CARTESIAN_POINT('Ctrl Pts',(6.53773645116441,4.82874804722673,74.7857452963559));
#169046=CARTESIAN_POINT('Ctrl Pts',(6.41639441292734,4.98493433259204,74.793477072079));
#169047=CARTESIAN_POINT('Ctrl Pts',(6.29500895519558,5.14117650567513,74.8012116144426));
#169048=CARTESIAN_POINT('Ctrl Pts',(6.16792462657411,5.29296763483897,74.8089461568063));
#169049=CARTESIAN_POINT('Ctrl Pts',(6.03551708426173,5.43987326029612,74.8166806991699));
#169050=CARTESIAN_POINT('Ctrl Pts',(5.90308717979186,5.58680369647536,74.8244165478114));
#169051=CARTESIAN_POINT('Ctrl Pts',(5.76533251254015,5.72884672747131,74.832152396453));
#169052=CARTESIAN_POINT('Ctrl Pts',(5.62266625905238,5.86560412078874,74.8398882450946));
#169053=CARTESIAN_POINT('Ctrl Pts',(5.47988326957604,6.00247341519781,74.8476304235578));
#169054=CARTESIAN_POINT('Ctrl Pts',(5.33218092480499,6.1340481917291,74.855372602021));
#169055=CARTESIAN_POINT('Ctrl Pts',(5.18000689493983,6.25996933945173,74.8631147804842));
#169056=CARTESIAN_POINT('Ctrl Pts',(5.05270349709213,6.3653105069307,74.8695916124771));
#169057=CARTESIAN_POINT('Ctrl Pts',(4.92227130998829,6.46669568781958,74.8760684444699));
#169058=CARTESIAN_POINT('Ctrl Pts',(4.78898823029079,6.56393778860192,74.8825452764627));
#169059=CARTESIAN_POINT('Ctrl Pts',(4.59559149263344,6.70503825759569,74.8919433049343));
#169060=CARTESIAN_POINT('Ctrl Pts',(4.39608249754805,6.83749589950495,74.9013413334058));
#169061=CARTESIAN_POINT('Ctrl Pts',(4.19118362917435,6.96086685327632,74.9107393618773));
#169062=CARTESIAN_POINT('Ctrl Pts',(3.98599320686122,7.08441335358861,74.9201507629567));
#169063=CARTESIAN_POINT('Ctrl Pts',(3.77539760211755,7.19884728328956,74.9295621640361));
#169064=CARTESIAN_POINT('Ctrl Pts',(3.56014639662484,7.30376924588251,74.9389735651155));
#169065=CARTESIAN_POINT('Ctrl Pts',(3.34521928815028,7.40853323075293,74.9483707957422));
#169066=CARTESIAN_POINT('Ctrl Pts',(3.12565062332381,7.50381386007424,74.957768026369));
#169067=CARTESIAN_POINT('Ctrl Pts',(2.90221004236492,7.58925980794545,74.9671652569957));
#169068=CARTESIAN_POINT('Ctrl Pts',(2.6793330619013,7.6744902292622,74.9765387843013));
#169069=CARTESIAN_POINT('Ctrl Pts',(2.45260370146824,7.74993548690382,74.9859123116069));
#169070=CARTESIAN_POINT('Ctrl Pts',(2.22280865699228,7.81529329180295,74.9952858389125));
#169071=CARTESIAN_POINT('Ctrl Pts',(1.99450588804002,7.88022666695531,75.0045984950823));
#169072=CARTESIAN_POINT('Ctrl Pts',(1.76317715952728,7.9352031459061,75.0139111512521));
#169073=CARTESIAN_POINT('Ctrl Pts',(1.5296160366041,7.97997257783907,75.0232238074218));
#169074=CARTESIAN_POINT('Ctrl Pts',(1.37922873481097,8.00879909651198,75.0292201188643));
#169075=CARTESIAN_POINT('Ctrl Pts',(1.22791634454046,8.03339478576714,75.0352164303068));
#169076=CARTESIAN_POINT('Ctrl Pts',(1.07589550392231,8.05370327409321,75.0412127417492));
#169077=CARTESIAN_POINT('Ctrl Pts',(0.884037263361776,8.07933364702656,
75.0487803999632));
#169078=CARTESIAN_POINT('Ctrl Pts',(0.691126325427681,8.09812214564439,
75.0563480581772));
#169079=CARTESIAN_POINT('Ctrl Pts',(0.497711160093764,8.10999205693927,
75.0639157163912));
#169080=CARTESIAN_POINT('Ctrl Pts',(0.304349547942123,8.1218586816691,75.0714812792567));
#169081=CARTESIAN_POINT('Ctrl Pts',(0.110484352777653,8.12681050822314,
75.0790468421222));
#169082=CARTESIAN_POINT('Ctrl Pts',(-0.0833308035016124,8.12482267743043,
75.0866124049877));
#169083=CARTESIAN_POINT('Ctrl Pts',(-0.277128979739505,8.1228350207905,
75.0941773050383));
#169084=CARTESIAN_POINT('Ctrl Pts',(-0.470876758184223,8.11390892154314,
75.1017422050889));
#169085=CARTESIAN_POINT('Ctrl Pts',(-0.664020555561341,8.09807163862435,
75.1093071051395));
#169086=CARTESIAN_POINT('Ctrl Pts',(-0.857259146720918,8.08222658286494,
75.1168757179963));
#169087=CARTESIAN_POINT('Ctrl Pts',(-1.04989279736519,8.0594635938141,75.1244443308531));
#169088=CARTESIAN_POINT('Ctrl Pts',(-1.24137251463595,8.02986188190098,
75.13201294371));
#169089=CARTESIAN_POINT('Ctrl Pts',(-1.43289481362932,8.00025358708758,
75.1395832396932));
#169090=CARTESIAN_POINT('Ctrl Pts',(-1.62326230649332,7.96380360742398,
75.1471535356765));
#169091=CARTESIAN_POINT('Ctrl Pts',(-1.81193649217937,7.92064225368175,
75.1547238316597));
#169092=CARTESIAN_POINT('Ctrl Pts',(-2.00080185860319,7.87743716518365,
75.1623017985109));
#169093=CARTESIAN_POINT('Ctrl Pts',(-2.18797013393669,7.82750720887086,
75.1698797653621));
#169094=CARTESIAN_POINT('Ctrl Pts',(-2.37291739471902,7.77103278852559,
75.1774577322134));
#169095=CARTESIAN_POINT('Ctrl Pts',(-2.55533111156246,7.71533199642853,
75.1849318904875));
#169096=CARTESIAN_POINT('Ctrl Pts',(-2.73558397890251,7.65326507251006,
75.1924060487616));
#169097=CARTESIAN_POINT('Ctrl Pts',(-2.91319360868311,7.58505046527891,
75.1998802070357));
#169098=CARTESIAN_POINT('Ctrl Pts',(-3.1050771385112,7.51135367509069,75.2079550387546));
#169099=CARTESIAN_POINT('Ctrl Pts',(-3.29428537116136,7.43032439323175,
75.2160298704734));
#169100=CARTESIAN_POINT('Ctrl Pts',(-3.4802415242175,7.34217995527298,75.2241047021923));
#169101=CARTESIAN_POINT('Ctrl Pts',(-3.66607464898251,7.25409383353228,
75.2321741916155));
#169102=CARTESIAN_POINT('Ctrl Pts',(-3.84865969923146,7.15890207792939,
75.2402436810388));
#169103=CARTESIAN_POINT('Ctrl Pts',(-4.0274398828275,7.05687009606315,75.248313170462));
#169104=CARTESIAN_POINT('Ctrl Pts',(-4.20612614116181,6.95489171846339,
75.2563784204394));
#169105=CARTESIAN_POINT('Ctrl Pts',(-4.38101124477215,6.8460804379753,75.2644436704168));
#169106=CARTESIAN_POINT('Ctrl Pts',(-4.55156247338365,6.73074784948788,
75.2725089203942));
#169107=CARTESIAN_POINT('Ctrl Pts',(-4.72204730994814,6.61546015757904,
75.2805710307374));
#169108=CARTESIAN_POINT('Ctrl Pts',(-4.88820137433582,6.49365639807545,
75.2886331410807));
#169109=CARTESIAN_POINT('Ctrl Pts',(-5.04951991933688,6.36569211843615,
75.296695251424));
#169110=CARTESIAN_POINT('Ctrl Pts',(-5.21079760254913,6.2377602519913,75.3047553196446));
#169111=CARTESIAN_POINT('Ctrl Pts',(-5.36724196165026,6.10367117481134,
75.3128153878652));
#169112=CARTESIAN_POINT('Ctrl Pts',(-5.51837991333216,5.9638218194906,75.3208754560859));
#169113=CARTESIAN_POINT('Ctrl Pts',(-5.67178213693864,5.82187731225466,
75.3290562761493));
#169114=CARTESIAN_POINT('Ctrl Pts',(-5.81971742717136,5.6739987614407,75.3372370962128));
#169115=CARTESIAN_POINT('Ctrl Pts',(-5.96172796739798,5.52064191967245,
75.3454179162762));
#169116=CARTESIAN_POINT('Ctrl Pts',(-6.10165596409755,5.36953401166393,
75.3534787669779));
#169117=CARTESIAN_POINT('Ctrl Pts',(-6.23583158313026,5.21310763681955,
75.3615396176796));
#169118=CARTESIAN_POINT('Ctrl Pts',(-6.36385553227013,5.05183435267773,
75.3696004683814));
#169119=CARTESIAN_POINT('Ctrl Pts',(-6.49190071301743,4.89053432282871,
75.3776626559018));
#169120=CARTESIAN_POINT('Ctrl Pts',(-6.61379199197732,4.72438602863369,
75.3857248434224));
#169121=CARTESIAN_POINT('Ctrl Pts',(-6.72917134119584,4.55389290863636,
75.3937870309428));
#169122=CARTESIAN_POINT('Ctrl Pts',(-6.84458411847528,4.38335039284647,
75.4018515542651));
#169123=CARTESIAN_POINT('Ctrl Pts',(-6.95348102549767,4.20846080295797,
75.4099160775875));
#169124=CARTESIAN_POINT('Ctrl Pts',(-7.05554789537656,4.02975575668643,
75.4179806009098));
#169125=CARTESIAN_POINT('Ctrl Pts',(-7.16020957365056,3.84650755792217,
75.4262501456347));
#169126=CARTESIAN_POINT('Ctrl Pts',(-7.25768916636869,3.65924764453877,
75.4345196903596));
#169127=CARTESIAN_POINT('Ctrl Pts',(-7.34769865973584,3.46857491892795,
75.4427892350845));
#169128=CARTESIAN_POINT('Ctrl Pts',(-7.43559520996231,3.28237817260136,
75.4508646549771));
#169129=CARTESIAN_POINT('Ctrl Pts',(-7.51636834507555,3.09292735041873,
75.4589400748697));
#169130=CARTESIAN_POINT('Ctrl Pts',(-7.5897990200549,2.90079961349862,75.4670154947624));
#169131=CARTESIAN_POINT('Ctrl Pts',(-7.66587749248386,2.70174404523337,
75.4753821019034));
#169132=CARTESIAN_POINT('Ctrl Pts',(-7.73407402572994,2.49981528299274,
75.4837487090444));
#169133=CARTESIAN_POINT('Ctrl Pts',(-7.79420162147424,2.29567172006545,
75.4921153161855));
#169134=CARTESIAN_POINT('Ctrl Pts',(-7.85432921721853,2.09152815713822,
75.5004819233265));
#169135=CARTESIAN_POINT('Ctrl Pts',(-7.9063878198325,1.88517016642369,75.5088485304675));
#169136=CARTESIAN_POINT('Ctrl Pts',(-7.95024914288406,1.67726745886612,
75.5172151376086));
#169137=CARTESIAN_POINT('Ctrl Pts',(-7.99259719492189,1.47653765716584,
75.5252930862416));
#169138=CARTESIAN_POINT('Ctrl Pts',(-8.02738648986898,1.2739776759411,75.5333710348747));
#169139=CARTESIAN_POINT('Ctrl Pts',(-8.05446432528133,1.07018315968358,
75.5414489835078));
#169140=CARTESIAN_POINT('Ctrl Pts',(-8.08150902292244,0.86663804652487,
75.5495170463723));
#169141=CARTESIAN_POINT('Ctrl Pts',(-8.10086103143785,0.661861720375482,
75.5575851092368));
#169142=CARTESIAN_POINT('Ctrl Pts',(-8.11241828749152,0.456461489364734,
75.5656531721012));
#169143=CARTESIAN_POINT('Ctrl Pts',(-8.12396282265557,0.251287339151645,
75.5737123545761));
#169144=CARTESIAN_POINT('Ctrl Pts',(-8.12772969136781,0.0454909664028391,
75.5817715370509));
#169145=CARTESIAN_POINT('Ctrl Pts',(-8.1236683387382,-0.160313083316861,
75.5898307195258));
#169146=CARTESIAN_POINT('Ctrl Pts',(-8.11961220277405,-0.365852784929534,
75.5978795502625));
#169147=CARTESIAN_POINT('Ctrl Pts',(-8.10774791116926,-0.571399829657183,
75.6059283809991));
#169148=CARTESIAN_POINT('Ctrl Pts',(-8.0880768829438,-0.776337489813555,
75.6139772117358));
#169149=CARTESIAN_POINT('Ctrl Pts',(-8.06842073379543,-0.981120136047483,
75.6220199543732));
#169150=CARTESIAN_POINT('Ctrl Pts',(-8.04096964817437,-1.18529400354725,
75.6300626970107));
#169151=CARTESIAN_POINT('Ctrl Pts',(-8.0057770593636,-1.38824394047571,
75.6381054396481));
#169152=CARTESIAN_POINT('Ctrl Pts',(-7.97061313624094,-1.59102856704221,
75.6461416311689));
#169153=CARTESIAN_POINT('Ctrl Pts',(-7.92772034221117,-1.79259094153851,
75.6541778226897));
#169154=CARTESIAN_POINT('Ctrl Pts',(-7.87720377732173,-1.99232231655631,
75.6622140142105));
#169155=CARTESIAN_POINT('Ctrl Pts',(-7.84856292402568,-2.10556194444909,
75.6667702104386));
#169156=CARTESIAN_POINT('Ctrl Pts',(-7.81747240184501,-2.21821312517741,
75.6713264066668));
#169157=CARTESIAN_POINT('Ctrl Pts',(-7.78395869918434,-2.33016620263286,
75.6758826028949));
#169158=CARTESIAN_POINT('Ctrl Pts',(-7.72484505609539,-2.5276363040543,
75.6839191174036));
#169159=CARTESIAN_POINT('Ctrl Pts',(-7.65823628448052,-2.72277750295707,
75.6919556319122));
#169160=CARTESIAN_POINT('Ctrl Pts',(-7.58435204968958,-2.91501141487807,
75.6999921464209));
#169161=CARTESIAN_POINT('Ctrl Pts',(-7.51042318146776,-3.10736145521329,
75.7080335157842));
#169162=CARTESIAN_POINT('Ctrl Pts',(-7.42921019490425,-3.2968004098709,
75.7160748851474));
#169163=CARTESIAN_POINT('Ctrl Pts',(-7.34098048664703,-3.48277088783738,
75.7241162545107));
#169164=CARTESIAN_POINT('Ctrl Pts',(-7.25268669112098,-3.66887644887565,
75.7321634648703));
#169165=CARTESIAN_POINT('Ctrl Pts',(-7.15736614066776,-3.8515082217538,
75.7402106752298));
#169166=CARTESIAN_POINT('Ctrl Pts',(-7.05533193849933,-4.03013384394256,
75.7482578855894));
#169167=CARTESIAN_POINT('Ctrl Pts',(-6.95314734520363,-4.20902274754197,
75.7563169569623));
#169168=CARTESIAN_POINT('Ctrl Pts',(-6.84422947939705,-4.38389342425324,
75.7643760283352));
#169169=CARTESIAN_POINT('Ctrl Pts',(-6.72893545953539,-4.5542414454997,
75.7724350997082));
#169170=CARTESIAN_POINT('Ctrl Pts',(-6.6135481265664,-4.72472733775812,
75.780500693683));
#169171=CARTESIAN_POINT('Ctrl Pts',(-6.49177452771158,-4.89068301576979,
75.7885662876579));
#169172=CARTESIAN_POINT('Ctrl Pts',(-6.36401231705863,-5.0516368427299,
75.7966318816327));
#169173=CARTESIAN_POINT('Ctrl Pts',(-6.23604949054567,-5.21284340397075,
75.8047101404328));
#169174=CARTESIAN_POINT('Ctrl Pts',(-6.10207946156526,-5.36903217561216,
75.8127883992329));
#169175=CARTESIAN_POINT('Ctrl Pts',(-5.96253820325935,-5.51976681909415,
75.8208666580329));
#169176=CARTESIAN_POINT('Ctrl Pts',(-5.88375058671614,-5.60487443124139,
75.8254277947491));
#169177=CARTESIAN_POINT('Ctrl Pts',(-5.80318753412615,-5.68824399586726,
75.8299889314653));
#169178=CARTESIAN_POINT('Ctrl Pts',(-5.72093219888738,-5.76980262558726,
75.8345500681814));
#169179=CARTESIAN_POINT('Ctrl Pts',(-5.5751061433143,-5.91439352945372,
75.8426362619136));
#169180=CARTESIAN_POINT('Ctrl Pts',(-5.42367561358374,-6.05357177239314,
75.8507224556458));
#169181=CARTESIAN_POINT('Ctrl Pts',(-5.26706891578806,-6.18689523095706,
75.858808649378));
#169182=CARTESIAN_POINT('Ctrl Pts',(-5.11060190373566,-6.32009977132228,
75.8668876306091));
#169183=CARTESIAN_POINT('Ctrl Pts',(-4.94896816933937,-6.44745973549497,
75.8749666118402));
#169184=CARTESIAN_POINT('Ctrl Pts',(-4.78263224479084,-6.56857034472395,
75.8830455930712));
#169185=CARTESIAN_POINT('Ctrl Pts',(-4.6164219699377,-6.68958946733511,
75.8911184714623));
#169186=CARTESIAN_POINT('Ctrl Pts',(-4.44551684314378,-6.80436846275911,
75.8991913498534));
#169187=CARTESIAN_POINT('Ctrl Pts',(-4.27041428169032,-6.91254290585131,
75.9072642282445));
#169188=CARTESIAN_POINT('Ctrl Pts',(-4.09542011654648,-7.0206503841297,
75.9153321091632));
#169189=CARTESIAN_POINT('Ctrl Pts',(-3.91623396748329,-7.12216129762214,
75.9233999900818));
#169190=CARTESIAN_POINT('Ctrl Pts',(-3.73338254514489,-7.21675427973736,
75.9314678710005));
#169191=CARTESIAN_POINT('Ctrl Pts',(-3.5506194144819,-7.31130158666577,
75.9395318562605));
#169192=CARTESIAN_POINT('Ctrl Pts',(-3.36419482129698,-7.39893747930425,
75.9475958415205));
#169193=CARTESIAN_POINT('Ctrl Pts',(-3.17466095491389,-7.47938602987205,
75.9556598267805));
#169194=CARTESIAN_POINT('Ctrl Pts',(-2.98249317472273,-7.56095255767644,
75.9638358756128));
#169195=CARTESIAN_POINT('Ctrl Pts',(-2.78712934937982,-7.63513033457791,
75.972011924445));
#169196=CARTESIAN_POINT('Ctrl Pts',(-2.58916815565461,-7.70168136345851,
75.9801879732773));
#169197=CARTESIAN_POINT('Ctrl Pts',(-2.39401278808359,-7.76728912354027,
75.9882481379242));
#169198=CARTESIAN_POINT('Ctrl Pts',(-2.19633350453126,-7.82548480685165,
75.9963083025712));
#169199=CARTESIAN_POINT('Ctrl Pts',(-1.99672163313582,-7.87608978378659,
76.0043684672182));
#169200=CARTESIAN_POINT('Ctrl Pts',(-1.79711940598434,-7.92669231574297,
76.0124282424384));
#169201=CARTESIAN_POINT('Ctrl Pts',(-1.59558508428954,-7.96970479506945,
76.0204880176586));
#169202=CARTESIAN_POINT('Ctrl Pts',(-1.39272298146644,-8.00499907928759,
76.0285477928789));
#169203=CARTESIAN_POINT('Ctrl Pts',(-1.18984556229635,-8.04029602826912,
76.0366081766224));
#169204=CARTESIAN_POINT('Ctrl Pts',(-0.985640474229856,-8.06787356616393,
76.044668560366));
#169205=CARTESIAN_POINT('Ctrl Pts',(-0.780720593302095,-8.08765497024286,
76.0527289441095));
#169206=CARTESIAN_POINT('Ctrl Pts',(-0.570649464788704,-8.10793363651782,
76.0609919486633));
#169207=CARTESIAN_POINT('Ctrl Pts',(-0.359827483434094,-8.12001903408977,
76.069254953217));
#169208=CARTESIAN_POINT('Ctrl Pts',(-0.148918920099594,-8.1238851984587,
76.0775179577707));
#169209=CARTESIAN_POINT('Ctrl Pts',(0.0569870444951847,-8.12765966020212,
76.0855849698265));
#169210=CARTESIAN_POINT('Ctrl Pts',(0.262975208159651,-8.12360039996556,
76.0936519818823));
#169211=CARTESIAN_POINT('Ctrl Pts',(0.468428594148711,-8.11173607895892,
76.1017189939381));
#169212=CARTESIAN_POINT('Ctrl Pts',(0.68136938477779,-8.09943938263888,
76.1100799947408));
#169213=CARTESIAN_POINT('Ctrl Pts',(0.89373531404555,-8.07875808080631,
76.1184409955435));
#169214=CARTESIAN_POINT('Ctrl Pts',(1.10484620398487,-8.04978275657425,
76.1268019963462));
#169215=CARTESIAN_POINT('Ctrl Pts',(1.31595709392427,-8.02080743234219,
76.1351629971489));
#169216=CARTESIAN_POINT('Ctrl Pts',(1.52581257745678,-7.98353817534003,
76.1435239979516));
#169217=CARTESIAN_POINT('Ctrl Pts',(1.73374485028036,-7.93812423413909,
76.1518849987543));
#169218=CARTESIAN_POINT('Ctrl Pts',(1.92221052664872,-7.89696194110606,
76.1594632435837));
#169219=CARTESIAN_POINT('Ctrl Pts',(2.1094738818728,-7.84902588551748,76.1670414884132));
#169220=CARTESIAN_POINT('Ctrl Pts',(2.29498972691959,-7.79440246047338,
76.1746197332426));
#169221=CARTESIAN_POINT('Ctrl Pts',(2.48036752474854,-7.73981968215601,
76.1821923389008));
#169222=CARTESIAN_POINT('Ctrl Pts',(2.66400004911832,-7.67855953702154,
76.1897649445591));
#169223=CARTESIAN_POINT('Ctrl Pts',(2.84535171518964,-7.61075956651945,
76.1973375502173));
#169224=CARTESIAN_POINT('Ctrl Pts',(3.02660287091369,-7.54299717272524,
76.2049059589181));
#169225=CARTESIAN_POINT('Ctrl Pts',(3.20557534069263,-7.46870229418943,
76.2124743676188));
#169226=CARTESIAN_POINT('Ctrl Pts',(3.38174819945708,-7.38806244410324,
76.2200427763196));
#169227=CARTESIAN_POINT('Ctrl Pts',(3.55787849345241,-7.30744207724861,
76.2276093564324));
#169228=CARTESIAN_POINT('Ctrl Pts',(3.73121018565105,-7.22047993559738,
76.2351759365452));
#169229=CARTESIAN_POINT('Ctrl Pts',(3.90124173860089,-7.12741190471677,
76.2427425166581));
#169230=CARTESIAN_POINT('Ctrl Pts',(4.07124312872238,-7.03436038368383,
76.2503077544938));
#169231=CARTESIAN_POINT('Ctrl Pts',(4.23794522380528,-6.93520530868187,
76.2578729923295));
#169232=CARTESIAN_POINT('Ctrl Pts',(4.40087078746796,-6.83022868391031,
76.2654382301652));
#169233=CARTESIAN_POINT('Ctrl Pts',(4.56385300816716,-6.72521555372897,
76.2730060987972));
#169234=CARTESIAN_POINT('Ctrl Pts',(4.72305576251727,-6.61437702603606,
76.2805739674291));
#169235=CARTESIAN_POINT('Ctrl Pts',(4.87803013611122,-6.49803890059845,
76.2881418360611));
#169236=CARTESIAN_POINT('Ctrl Pts',(5.0310046481298,-6.38320205657543,76.2956120453876));
#169237=CARTESIAN_POINT('Ctrl Pts',(5.17985900604571,-6.26300694868819,
76.3030822547141));
#169238=CARTESIAN_POINT('Ctrl Pts',(5.32419319157848,-6.13780534240451,
76.3105524640406));
#169239=CARTESIAN_POINT('Ctrl Pts',(5.50399418331556,-5.9818383211906,76.3198583054837));
#169240=CARTESIAN_POINT('Ctrl Pts',(5.67669375945295,-5.8181802863734,76.3291641469269));
#169241=CARTESIAN_POINT('Ctrl Pts',(5.84173903370327,-5.64745718218452,
76.33846998837));
#169242=CARTESIAN_POINT('Ctrl Pts',(6.00767040273525,-5.47581750009047,
76.3478257909985));
#169243=CARTESIAN_POINT('Ctrl Pts',(6.16586506739252,-5.29703675329165,
76.357181593627));
#169244=CARTESIAN_POINT('Ctrl Pts',(6.31580603520619,-5.11177872057791,
76.3665373962555));
#169245=CARTESIAN_POINT('Ctrl Pts',(6.46647488472674,-4.92562136104888,
76.3759386162085));
#169246=CARTESIAN_POINT('Ctrl Pts',(6.60880970056182,-4.73292372339899,
76.3853398361614));
#169247=CARTESIAN_POINT('Ctrl Pts',(6.74233108267822,-4.53438630181099,
76.3947410561144));
#169248=CARTESIAN_POINT('Ctrl Pts',(6.8759969745523,-4.3356340038172,76.4041524509772));
#169249=CARTESIAN_POINT('Ctrl Pts',(7.00083034152809,-4.13102931665845,
76.4135638458399));
#169250=CARTESIAN_POINT('Ctrl Pts',(7.11639540987006,-3.9213013060565,76.4229752407027));
#169251=CARTESIAN_POINT('Ctrl Pts',(7.23182491844797,-3.71181930992968,
76.4323755958414));
#169252=CARTESIAN_POINT('Ctrl Pts',(7.3380078455462,-3.49722603675443,76.44177595098));
#169253=CARTESIAN_POINT('Ctrl Pts',(7.43455510377921,-3.27827362667769,
76.4511763061187));
#169254=CARTESIAN_POINT('Ctrl Pts',(7.49632803057009,-3.13818335952877,
76.4571908471882));
#169255=CARTESIAN_POINT('Ctrl Pts',(7.55415730715697,-2.99630910459338,
76.4632053882577));
#169256=CARTESIAN_POINT('Ctrl Pts',(7.60795081508343,-2.85285330113054,
76.4692199293272));
#169257=CARTESIAN_POINT('Ctrl Pts',(7.67698634659788,-2.66875027415507,
76.4769386495883));
#169258=CARTESIAN_POINT('Ctrl Pts',(7.73940628958672,-2.48195035722015,
76.4846573698495));
#169259=CARTESIAN_POINT('Ctrl Pts',(7.79499388679409,-2.2929801279869,76.4923760901106));
#169260=CARTESIAN_POINT('Ctrl Pts',(7.85054225373071,-2.10414326219491,
76.5000893629787));
#169261=CARTESIAN_POINT('Ctrl Pts',(7.89926778015739,-1.91313947503296,
76.5078026358469));
#169262=CARTESIAN_POINT('Ctrl Pts',(7.94100250815688,-1.72051350705134,
76.5155159087151));
#169263=CARTESIAN_POINT('Ctrl Pts',(7.98271957203336,-1.5279690675463,76.5232259169591));
#169264=CARTESIAN_POINT('Ctrl Pts',(8.01745165377216,-1.33380416112158,
76.5309359252031));
#169265=CARTESIAN_POINT('Ctrl Pts',(8.04508109285943,-1.13857708207028,
76.5386459334471));
#169266=CARTESIAN_POINT('Ctrl Pts',(8.07270748774194,-0.943371513090242,
76.5463550922043));
#169267=CARTESIAN_POINT('Ctrl Pts',(8.09323274058048,-0.747104355328392,
76.5540642509615));
#169268=CARTESIAN_POINT('Ctrl Pts',(8.1065905525326,-0.550342780537027,
76.5617734097188));
#169269=CARTESIAN_POINT('Ctrl Pts',(8.11902225880618,-0.367222812049529,
76.56894808755));
#169270=CARTESIAN_POINT('Ctrl Pts',(8.12524640000166,-0.183674920503634,
76.5761227653811));
#169271=CARTESIAN_POINT('Ctrl Pts',(8.12524999843797,-0.000159322667913658,
76.5832974432123));
#169272=CARTESIAN_POINT('',(8.12525,-2.38892889845022E-12,78.5832974432123));
#169273=CARTESIAN_POINT('Ctrl Pts',(8.12525,-2.44467264634169E-12,76.5832974432123));
#169274=CARTESIAN_POINT('Ctrl Pts',(8.12525000000068,2.24624642433177,76.6712950363535));
#169275=CARTESIAN_POINT('Ctrl Pts',(7.14398562317725,4.47535249753257,76.7592926294947));
#169276=CARTESIAN_POINT('Ctrl Pts',(3.83078204045118,7.50935546634272,76.9352878157771));
#169277=CARTESIAN_POINT('Ctrl Pts',(1.52412477697928,8.29110090552108,77.0232854089183));
#169278=CARTESIAN_POINT('Ctrl Pts',(-2.9510162393241,7.89663306204484,77.1992805952007));
#169279=CARTESIAN_POINT('Ctrl Pts',(-5.08535169588616,6.7234298308588,77.2872781883419));
#169280=CARTESIAN_POINT('Ctrl Pts',(-7.81671694684357,3.15661951053066,
77.4632733746244));
#169281=CARTESIAN_POINT('Ctrl Pts',(-8.39290461146693,0.790229551555331,
77.5512709677655));
#169282=CARTESIAN_POINT('Ctrl Pts',(-7.6070161146253,-3.63299000730324,
77.727266154048));
#169283=CARTESIAN_POINT('Ctrl Pts',(-6.2509368040142,-5.65606750609953,
77.8152637471892));
#169284=CARTESIAN_POINT('Ctrl Pts',(-2.45807268688625,-8.063695754883,77.9912589334716));
#169285=CARTESIAN_POINT('Ctrl Pts',(-0.0502299510459386,-8.42987470330088,
78.0792565266128));
#169286=CARTESIAN_POINT('Ctrl Pts',(4.28689960880965,-7.25863639434584,
78.2552517128952));
#169287=CARTESIAN_POINT('Ctrl Pts',(6.18309125557145,-5.730156462664,78.3432493060364));
#169288=CARTESIAN_POINT('Ctrl Pts',(7.81050559202861,-2.58640713800351,
78.4819304138558));
#169289=CARTESIAN_POINT('Ctrl Pts',(8.12524999999962,-1.29375883538314,
78.5326139285341));
#169290=CARTESIAN_POINT('Ctrl Pts',(8.12525,-2.3889293849853E-12,78.5832974432123));
#169291=CARTESIAN_POINT('',(8.11704416097363,-0.0053549714695382,82.5832974432122));
#169292=CARTESIAN_POINT('Ctrl Pts',(8.1252484868335,0.00495880126088338,
78.5812557146917));
#169293=CARTESIAN_POINT('Ctrl Pts',(8.12477749880775,0.776696675441153,
78.6119376937694));
#169294=CARTESIAN_POINT('Ctrl Pts',(8.01436124269951,1.54444684412075,78.6436553120502));
#169295=CARTESIAN_POINT('Ctrl Pts',(7.77796842233457,2.35109110530625,78.6773309709204));
#169296=CARTESIAN_POINT('Ctrl Pts',(7.7577793397255,2.41687442786724,78.6800779117451));
#169297=CARTESIAN_POINT('Ctrl Pts',(7.72612508359144,2.51552972253561,78.6841958640216));
#169298=CARTESIAN_POINT('Ctrl Pts',(7.71528036328135,2.54859716833381,78.6855758448654));
#169299=CARTESIAN_POINT('Ctrl Pts',(7.6972722113551,2.60233870357997,78.6878177626792));
#169300=CARTESIAN_POINT('Ctrl Pts',(7.69023714527696,2.62305525640478,78.6886817836851));
#169301=CARTESIAN_POINT('Ctrl Pts',(7.67756133222762,2.65989309058917,78.6902177006716));
#169302=CARTESIAN_POINT('Ctrl Pts',(7.67195326884685,2.67602546847662,78.6908901601028));
#169303=CARTESIAN_POINT('Ctrl Pts',(7.66015077416166,2.7096349371009,78.6922907467429));
#169304=CARTESIAN_POINT('Ctrl Pts',(7.65394730689467,2.7271087256561,78.6930187182664));
#169305=CARTESIAN_POINT('Ctrl Pts',(7.63974981109642,2.7666698634588,78.6946666265749));
#169306=CARTESIAN_POINT('Ctrl Pts',(7.63171970137749,2.7887441106567,78.6955859538465));
#169307=CARTESIAN_POINT('Ctrl Pts',(7.61048348997913,2.84634238020573,78.6979848156215));
#169308=CARTESIAN_POINT('Ctrl Pts',(7.59712433962746,2.88180944636591,78.6994620189326));
#169309=CARTESIAN_POINT('Ctrl Pts',(7.51537771402441,3.09431829686392,78.7083181421541));
#169310=CARTESIAN_POINT('Ctrl Pts',(7.44105181310255,3.26901471641379,78.7156217416426));
#169311=CARTESIAN_POINT('Ctrl Pts',(7.27838352742002,3.61698513847938,78.7303906863481));
#169312=CARTESIAN_POINT('Ctrl Pts',(7.18980251307043,3.79001157867117,78.7378511297545));
#169313=CARTESIAN_POINT('Ctrl Pts',(7.03787832489437,4.06223401694974,78.7498852960312));
#169314=CARTESIAN_POINT('Ctrl Pts',(6.97843688778892,4.1635195253785,78.7544311753763));
#169315=CARTESIAN_POINT('Ctrl Pts',(6.89173159576991,4.30418511863206,78.7608555763941));
#169316=CARTESIAN_POINT('Ctrl Pts',(6.86628288265661,4.3446672226043,78.7627176708181));
#169317=CARTESIAN_POINT('Ctrl Pts',(6.82236196422982,4.4131838524819,78.765892734708));
#169318=CARTESIAN_POINT('Ctrl Pts',(6.80407060200713,4.44133287663768,78.7672039853806));
#169319=CARTESIAN_POINT('Ctrl Pts',(6.76533655143993,4.50014074379178,78.769958055071));
#169320=CARTESIAN_POINT('Ctrl Pts',(6.74485868853405,4.53077549966468,78.7714011837903));
#169321=CARTESIAN_POINT('Ctrl Pts',(6.69233422672486,4.60820647632772,78.7750706931421));
#169322=CARTESIAN_POINT('Ctrl Pts',(6.66000479870735,4.65480830647563,78.7772997474766));
#169323=CARTESIAN_POINT('Ctrl Pts',(6.5090320874639,4.86763759191837,78.7875766809654));
#169324=CARTESIAN_POINT('Ctrl Pts',(6.38463732858639,5.02969173769954,78.795679589695));
#169325=CARTESIAN_POINT('Ctrl Pts',(6.09452636068742,5.37950332377518,78.8137935221507));
#169326=CARTESIAN_POINT('Ctrl Pts',(5.9259689934141,5.564638249596,78.8238153869677));
#169327=CARTESIAN_POINT('Ctrl Pts',(5.69795651131389,5.79294613699492,78.8366557270218));
#169328=CARTESIAN_POINT('Ctrl Pts',(5.64609230262538,5.84350709378457,78.8395315702991));
#169329=CARTESIAN_POINT('Ctrl Pts',(5.56794372104095,5.91768007663899,78.8437944767271));
#169330=CARTESIAN_POINT('Ctrl Pts',(5.54217029858227,5.94182490206339,78.8451892701938));
#169331=CARTESIAN_POINT('Ctrl Pts',(5.50006927953073,5.98075334338627,78.8474490941621));
#169332=CARTESIAN_POINT('Ctrl Pts',(5.48383758780031,5.99563991154673,78.8483159263131));
#169333=CARTESIAN_POINT('Ctrl Pts',(5.45413578313851,6.02265880203591,78.849893892359));
#169334=CARTESIAN_POINT('Ctrl Pts',(5.44068526620947,6.03481234362897,78.850605416075));
#169335=CARTESIAN_POINT('Ctrl Pts',(5.41239075878761,6.06020705092514,78.8520958134319));
#169336=CARTESIAN_POINT('Ctrl Pts',(5.39753862384278,6.07343889680216,78.8528745159899));
#169337=CARTESIAN_POINT('Ctrl Pts',(5.36325199331854,6.10375993531316,78.8546640746883));
#169338=CARTESIAN_POINT('Ctrl Pts',(5.34378412456139,6.12081110052114,78.8556742421444));
#169339=CARTESIAN_POINT('Ctrl Pts',(5.29090489456037,6.16668142427111,78.8584026345208));
#169340=CARTESIAN_POINT('Ctrl Pts',(5.25733963487427,6.19532197572334,78.8601179516351));
#169341=CARTESIAN_POINT('Ctrl Pts',(5.01930906386066,6.39510109020361,78.8721734109165));
#169342=CARTESIAN_POINT('Ctrl Pts',(4.80675958453488,6.55635925223577,78.8823823729737));
#169343=CARTESIAN_POINT('Ctrl Pts',(4.37927593135916,6.84870466585796,78.9022326648068));
#169344=CARTESIAN_POINT('Ctrl Pts',(4.16542086773223,6.98083670686255,78.9118620738936));
#169345=CARTESIAN_POINT('Ctrl Pts',(3.8055670544256,7.18074349052698,78.927754498019));
#169346=CARTESIAN_POINT('Ctrl Pts',(3.6630699598506,7.25447003421125,78.9339712985295));
#169347=CARTESIAN_POINT('Ctrl Pts',(3.45631166783953,7.35379867145922,78.9429051765762));
#169348=CARTESIAN_POINT('Ctrl Pts',(3.39376055687149,7.382874404501,78.9455968238417));
#169349=CARTESIAN_POINT('Ctrl Pts',(3.28219105739829,7.43301789509689,78.9503792480907));
#169350=CARTESIAN_POINT('Ctrl Pts',(3.23332102904393,7.45440596326667,78.9524678366587));
#169351=CARTESIAN_POINT('Ctrl Pts',(3.13102052168822,7.49798271510535,78.9568273112413));
#169352=CARTESIAN_POINT('Ctrl Pts',(3.07755650463511,7.52008512164437,78.9590985679526));
#169353=CARTESIAN_POINT('Ctrl Pts',(2.89908932310429,7.59164273879105,78.966656887129));
#169354=CARTESIAN_POINT('Ctrl Pts',(2.77309561098332,7.63856654613175,78.9719554886181));
#169355=CARTESIAN_POINT('Ctrl Pts',(2.47319707476751,7.74185931113206,78.9844731127395));
#169356=CARTESIAN_POINT('Ctrl Pts',(2.29843876235628,7.79552876851279,78.9916946558399));
#169357=CARTESIAN_POINT('Ctrl Pts',(2.12076571874434,7.84359879238489,78.9989427769223));
#169358=CARTESIAN_POINT('Ctrl Pts',(2.11951179332774,7.84393772334074,78.9989939257237));
#169359=CARTESIAN_POINT('Ctrl Pts',(2.11704256139804,7.84460451139439,78.9990946386954));
#169360=CARTESIAN_POINT('Ctrl Pts',(2.11582725988835,7.84493238678788,78.9991442029502));
#169361=CARTESIAN_POINT('Ctrl Pts',(2.11343223482167,7.84557794199921,78.9992418716805));
#169362=CARTESIAN_POINT('Ctrl Pts',(2.11225251570302,7.84589563817123,78.9992899762333));
#169363=CARTESIAN_POINT('Ctrl Pts',(2.10992588347078,7.84652163313258,78.9993848393332));
#169364=CARTESIAN_POINT('Ctrl Pts',(2.10877897433242,7.84682994656895,78.9994315979499));
#169365=CARTESIAN_POINT('Ctrl Pts',(2.10651542697061,7.84743790387041,78.9995238731988));
#169366=CARTESIAN_POINT('Ctrl Pts',(2.10539879229764,7.84773756088715,78.9995693898945));
#169367=CARTESIAN_POINT('Ctrl Pts',(2.10319346793509,7.84832887111911,78.9996592767118));
#169368=CARTESIAN_POINT('Ctrl Pts',(2.10210478145191,7.84862053615817,78.9997036468904));
#169369=CARTESIAN_POINT('Ctrl Pts',(2.0999532127669,7.84919647334802,78.9997913284593));
#169370=CARTESIAN_POINT('Ctrl Pts',(2.09889033343613,7.84948075615436,78.9998346399021));
#169371=CARTESIAN_POINT('Ctrl Pts',(2.0967884027551,7.85004249117029,78.9999202850193));
#169372=CARTESIAN_POINT('Ctrl Pts',(2.09574935399928,7.85031995299039,78.9999626187411));
#169373=CARTESIAN_POINT('Ctrl Pts',(2.09369325441383,7.85086856512302,79.0000463834175));
#169374=CARTESIAN_POINT('Ctrl Pts',(2.09267620591767,7.85113972411655,79.0000878144157));
#169375=CARTESIAN_POINT('Ctrl Pts',(2.09066240711839,7.85167621122216,79.0001698432837));
#169376=CARTESIAN_POINT('Ctrl Pts',(2.08966565893997,7.85194154717527,79.0002104411923));
#169377=CARTESIAN_POINT('Ctrl Pts',(2.08769087740094,7.85246683450753,79.0002908687322));
#169378=CARTESIAN_POINT('Ctrl Pts',(2.08671284593358,7.85272679298343,79.0003306983999));
#169379=CARTESIAN_POINT('Ctrl Pts',(2.08477401840881,7.85324174101474,79.0004096500308));
#169380=CARTESIAN_POINT('Ctrl Pts',(2.08381322408138,7.85349673698234,79.0004487720264));
#169381=CARTESIAN_POINT('Ctrl Pts',(2.08190748445999,7.85400214822219,79.0005263650583));
#169382=CARTESIAN_POINT('Ctrl Pts',(2.08096254071612,7.85425256929428,79.0005648361245));
#169383=CARTESIAN_POINT('Ctrl Pts',(2.07908719917799,7.85474919440275,79.0006411806151));
#169384=CARTESIAN_POINT('Ctrl Pts',(2.07815680278088,7.85499540367861,79.0006790540668));
#169385=CARTESIAN_POINT('Ctrl Pts',(2.07630932741173,7.85548394684647,79.0007542535774));
#169386=CARTESIAN_POINT('Ctrl Pts',(2.07539224972451,7.85572628545846,79.0007915796602));
#169387=CARTESIAN_POINT('Ctrl Pts',(2.07357025005561,7.85620740920747,79.0008657319323));
#169388=CARTESIAN_POINT('Ctrl Pts',(2.07266532921069,7.8564461985996,79.0009025581441));
#169389=CARTESIAN_POINT('Ctrl Pts',(2.07086654127337,7.85692052812117,79.0009757557131));
#169390=CARTESIAN_POINT('Ctrl Pts',(2.06997267520172,7.85715607207187,79.0010121270905));
#169391=CARTESIAN_POINT('Ctrl Pts',(2.0681949482745,7.8576241990653,79.0010844578299));
#169392=CARTESIAN_POINT('Ctrl Pts',(2.067311088327,7.85785678552906,79.0011204172102));
#169393=CARTESIAN_POINT('Ctrl Pts',(2.06555237277822,7.85831927170412,79.0011919648306));
#169394=CARTESIAN_POINT('Ctrl Pts',(2.06467751798638,7.85854917446267,79.0012275530872));
#169395=CARTESIAN_POINT('Ctrl Pts',(2.06293585429693,7.85900655468996,79.0012983975867));
#169396=CARTESIAN_POINT('Ctrl Pts',(2.06206904612585,7.85923403485437,79.0013336538439));
#169397=CARTESIAN_POINT('Ctrl Pts',(2.06034255487005,7.85968682002717,79.001403871919));
#169398=CARTESIAN_POINT('Ctrl Pts',(2.05948287241317,7.85991212740665,79.0014388337498));
#169399=CARTESIAN_POINT('Ctrl Pts',(2.05776974498611,7.86036080707388,79.0015084991753));
#169400=CARTESIAN_POINT('Ctrl Pts',(2.05691630058446,7.86058418141765,79.0015432027803));
#169401=CARTESIAN_POINT('Ctrl Pts',(2.05521479084541,7.86102922614735,79.0016123867515));
#169402=CARTESIAN_POINT('Ctrl Pts',(2.05436672596706,7.86125089830442,79.0016468671278));
#169403=CARTESIAN_POINT('Ctrl Pts',(2.05267514221329,7.86169276193416,79.0017156385893));
#169404=CARTESIAN_POINT('Ctrl Pts',(2.05183162374219,7.86191295489335,79.0017499296824));
#169405=CARTESIAN_POINT('Ctrl Pts',(2.05014832159025,7.86235207651928,79.0018183556192));
#169406=CARTESIAN_POINT('Ctrl Pts',(2.04930853823697,7.86257100640595,79.0018524904696));
#169407=CARTESIAN_POINT('Ctrl Pts',(2.04763191364724,7.86300781231244,79.0019206361921));
#169408=CARTESIAN_POINT('Ctrl Pts',(2.04679507268266,7.86322568929032,79.001954647069));
#169409=CARTESIAN_POINT('Ctrl Pts',(2.04512355562556,7.86366059469195,79.0020225764719));
#169410=CARTESIAN_POINT('Ctrl Pts',(2.04428887973238,7.86387762382452,79.0020564950015));
#169411=CARTESIAN_POINT('Ctrl Pts',(2.04262092804534,7.86431103453956,79.0021242708142));
#169412=CARTESIAN_POINT('Ctrl Pts',(2.04178765237209,7.86452741658966,79.0021581281001));
#169413=CARTESIAN_POINT('Ctrl Pts',(2.04012174596573,7.864959730605,79.0022258121232));
#169414=CARTESIAN_POINT('Ctrl Pts',(2.03928911530709,7.86517566279295,79.0022596388611));
#169415=CARTESIAN_POINT('Ctrl Pts',(2.03762375069531,7.86560727172827,79.0023272921891));
#169416=CARTESIAN_POINT('Ctrl Pts',(2.03679101674031,7.86582294846434,79.0023611187791));
#169417=CARTESIAN_POINT('Ctrl Pts',(2.03512470156712,7.86625423902115,79.0024288020229));
#169418=CARTESIAN_POINT('Ctrl Pts',(2.03429112031392,7.86646985258692,79.0024626586742));
#169419=CARTESIAN_POINT('Ctrl Pts',(2.03262236831987,7.86690120786833,79.0025304321662));
#169420=CARTESIAN_POINT('Ctrl Pts',(2.03178719746098,7.86711694909821,79.0025643490037));
#169421=CARTESIAN_POINT('Ctrl Pts',(2.03011452325683,7.86754874996369,79.0026322730093));
#169422=CARTESIAN_POINT('Ctrl Pts',(2.02927701972304,7.86776480887791,79.0026662801732));
#169423=CARTESIAN_POINT('Ctrl Pts',(2.02759893389873,7.86819743519649,79.0027344150898));
#169424=CARTESIAN_POINT('Ctrl Pts',(2.02675835136632,7.86841400163635,79.0027685428364));
#169425=CARTESIAN_POINT('Ctrl Pts',(2.02507335555464,7.86884783353704,79.002836949393));
#169426=CARTESIAN_POINT('Ctrl Pts',(2.02422894198711,7.86906509778384,79.0028712281947));
#169427=CARTESIAN_POINT('Ctrl Pts',(2.02253552396981,7.86950051688035,79.00293996765));
#169428=CARTESIAN_POINT('Ctrl Pts',(2.02168651915706,7.86971867026762,79.0029744282942));
#169429=CARTESIAN_POINT('Ctrl Pts',(2.01998314790442,7.87015606088526,79.0030435626371));
#169430=CARTESIAN_POINT('Ctrl Pts',(2.01912878102475,7.87037529639753,79.0030782363251));
#169431=CARTESIAN_POINT('Ctrl Pts',(2.01741390177339,7.870815046775,79.0031478284734));
#169432=CARTESIAN_POINT('Ctrl Pts',(2.01655338891001,7.87103555965058,79.0031827469205));
#169433=CARTESIAN_POINT('Ctrl Pts',(2.01482541820033,7.87147806313634,79.0032528609208));
#169434=CARTESIAN_POINT('Ctrl Pts',(2.01395795979479,7.87170005147822,79.0032880564589));
#169435=CARTESIAN_POINT('Ctrl Pts',(2.01221528033501,7.872145707755,79.0033587576936));
#169436=CARTESIAN_POINT('Ctrl Pts',(2.01134005863004,7.87236937313598,79.003394263374));
#169437=CARTESIAN_POINT('Ctrl Pts',(2.00958101406814,7.87281858945148,79.0034656187715));
#169438=CARTESIAN_POINT('Ctrl Pts',(2.0086971904917,7.87304413752564,79.0035014684702));
#169439=CARTESIAN_POINT('Ctrl Pts',(2.00692008014992,7.87349732991471,79.0035735467168));
#169440=CARTESIAN_POINT('Ctrl Pts',(2.00602679258486,7.87372497104864,79.0036097752439));
#169441=CARTESIAN_POINT('Ctrl Pts',(2.0042298659134,7.87418256560786,79.0036826470056));
#169442=CARTESIAN_POINT('Ctrl Pts',(2.00332622591931,7.87441251551417,79.0037192902172));
#169443=CARTESIAN_POINT('Ctrl Pts',(2.00150767683684,7.87487494968464,79.0037930283672));
#169444=CARTESIAN_POINT('Ctrl Pts',(2.00059276676679,7.87510743007155,79.0038301232804));
#169445=CARTESIAN_POINT('Ctrl Pts',(1.96430039190661,7.88432265877255,79.0053014869552));
#169446=CARTESIAN_POINT('Ctrl Pts',(1.92886275333948,7.89306710411284,79.0067341908905));
#169447=CARTESIAN_POINT('Ctrl Pts',(1.84751121702681,7.91256048203342,79.0100134391076));
#169448=CARTESIAN_POINT('Ctrl Pts',(1.80156024619041,7.92314910739212,79.0118587784646));
#169449=CARTESIAN_POINT('Ctrl Pts',(1.59925465774481,7.96791607261864,79.0199575297382));
#169450=CARTESIAN_POINT('Ctrl Pts',(1.44200162774041,7.99787056927811,79.0261863174386));
#169451=CARTESIAN_POINT('Ctrl Pts',(1.16482065801442,8.04222852501486,79.0371151002937));
#169452=CARTESIAN_POINT('Ctrl Pts',(1.04526520915649,8.05863930071604,79.0418125871291));
#169453=CARTESIAN_POINT('Ctrl Pts',(0.838291908905398,8.08236597885774,
79.049938754268));
#169454=CARTESIAN_POINT('Ctrl Pts',(0.751039242055659,8.09094018783375,
79.0533625500681));
#169455=CARTESIAN_POINT('Ctrl Pts',(0.611656793337977,8.1023630236452,79.0588351771077));
#169456=CARTESIAN_POINT('Ctrl Pts',(0.559608670390351,8.10612414879205,
79.0608794696216));
#169457=CARTESIAN_POINT('Ctrl Pts',(0.451830808887094,8.11286945625869,
79.0651155516643));
#169458=CARTESIAN_POINT('Ctrl Pts',(0.396099278714087,8.11578136892283,
79.0673076140426));
#169459=CARTESIAN_POINT('Ctrl Pts',(0.255272832616235,8.12168534714179,
79.0728525112909));
#169460=CARTESIAN_POINT('Ctrl Pts',(0.170152878208164,8.12391438848635,
79.0762094355119));
#169461=CARTESIAN_POINT('Ctrl Pts',(-0.341651512919927,8.12926965683001,
79.0964376596292));
#169462=CARTESIAN_POINT('Ctrl Pts',(-0.768001583346198,8.10011820440259,
79.1135101408076));
#169463=CARTESIAN_POINT('Ctrl Pts',(-1.34351323394947,8.01490600789059,
79.1367886361178));
#169464=CARTESIAN_POINT('Ctrl Pts',(-1.49626758080993,7.98779881819189,
79.1429855493658));
#169465=CARTESIAN_POINT('Ctrl Pts',(-1.70716256719744,7.9441119764702,79.1515424516805));
#169466=CARTESIAN_POINT('Ctrl Pts',(-1.76603467166353,7.93123198026309,
79.1539312108329));
#169467=CARTESIAN_POINT('Ctrl Pts',(-1.86535327397832,7.9083424439376,79.1579590080064));
#169468=CARTESIAN_POINT('Ctrl Pts',(-1.90587587891874,7.89867458544044,
79.1596017775113));
#169469=CARTESIAN_POINT('Ctrl Pts',(-1.94636051838001,7.88868609443464,
79.1612419353231));
#169470=CARTESIAN_POINT('Ctrl Pts',(-1.94639855748499,7.88867670902132,
79.1612434764038));
#169471=CARTESIAN_POINT('Ctrl Pts',(-1.94647462843851,7.88865793940133,
79.1612465582694));
#169472=CARTESIAN_POINT('Ctrl Pts',(-1.94651266056927,7.88864855512515,
79.1612480990656));
#169473=CARTESIAN_POINT('Ctrl Pts',(-1.94658871778806,7.88862978772703,
79.1612511803709));
#169474=CARTESIAN_POINT('Ctrl Pts',(-1.94662674272849,7.88862040464162,
79.1612527208739));
#169475=CARTESIAN_POINT('Ctrl Pts',(-1.94670278552942,7.88860163963458,
79.1612558015913));
#169476=CARTESIAN_POINT('Ctrl Pts',(-1.9467408035598,7.88859225767112,79.1612573418125));
#169477=CARTESIAN_POINT('Ctrl Pts',(-1.94681683272913,7.88857349486175,
79.1612604219738));
#169478=CARTESIAN_POINT('Ctrl Pts',(-1.9468548436396,7.88856411407233,79.1612619619046));
#169479=CARTESIAN_POINT('Ctrl Pts',(-1.94693085868991,7.88854535358156,
79.1612650414901));
#169480=CARTESIAN_POINT('Ctrl Pts',(-1.94696886266647,7.8885359739206,79.1612665811381));
#169481=CARTESIAN_POINT('Ctrl Pts',(-1.94704486358882,7.88851721575127,
79.1612696601474));
#169482=CARTESIAN_POINT('Ctrl Pts',(-1.94708286077298,7.88850783718416,
79.1612711995184));
#169483=CARTESIAN_POINT('Ctrl Pts',(-1.94715884812554,7.88848908119911,
79.1612742779741));
#169484=CARTESIAN_POINT('Ctrl Pts',(-1.94719683835505,7.8884797037662,79.1612758170614));
#169485=CARTESIAN_POINT('Ctrl Pts',(-1.94727281215009,7.88846094996304,
79.1612788949641));
#169486=CARTESIAN_POINT('Ctrl Pts',(-1.94731079538129,7.88845157367541,
79.1612804337659));
#169487=CARTESIAN_POINT('Ctrl Pts',(-1.94738675498445,7.88843282221134,
79.1612835110898));
#169488=CARTESIAN_POINT('Ctrl Pts',(-1.94742473156101,7.88842344698449,
79.1612850496202));
#169489=CARTESIAN_POINT('Ctrl Pts',(-1.94750067778661,7.88840469765911,
79.1612881263983));
#169490=CARTESIAN_POINT('Ctrl Pts',(-1.9475386475168,7.88839532354065,79.1612896646494));
#169491=CARTESIAN_POINT('Ctrl Pts',(-1.94761458031149,7.88837657636773,
79.1612927408796));
#169492=CARTESIAN_POINT('Ctrl Pts',(-1.94765254317287,7.88836720336352,
79.1612942788505));
#169493=CARTESIAN_POINT('Ctrl Pts',(-1.94772846198207,7.88834845848061,
79.1612973545104));
#169494=CARTESIAN_POINT('Ctrl Pts',(-1.9477664182879,7.88833908651362,79.1612988922138));
#169495=CARTESIAN_POINT('Ctrl Pts',(-1.94784232416707,7.88832034366071,
79.1613019673459));
#169496=CARTESIAN_POINT('Ctrl Pts',(-1.9478802735894,7.88831097281219,79.1613035047686));
#169497=CARTESIAN_POINT('Ctrl Pts',(-1.94795616570425,7.8882922321959,79.1613065793393));
#169498=CARTESIAN_POINT('Ctrl Pts',(-1.94799410854456,7.88828286239173,
79.1613081164934));
#169499=CARTESIAN_POINT('Ctrl Pts',(-1.94806998759181,7.88826412384062,
79.1613111905309));
#169500=CARTESIAN_POINT('Ctrl Pts',(-1.94810792369788,7.88825475511868,
79.1613127274103));
#169501=CARTESIAN_POINT('Ctrl Pts',(-1.94818378933276,7.88823601871847,
79.1613158009006));
#169502=CARTESIAN_POINT('Ctrl Pts',(-1.94822171884716,7.88822665104386,
79.1613173375111));
#169503=CARTESIAN_POINT('Ctrl Pts',(-1.9482975714523,7.88820791670066,79.1613204104697));
#169504=CARTESIAN_POINT('Ctrl Pts',(-1.9483354943024,7.8881985500916,79.1613219468082));
#169505=CARTESIAN_POINT('Ctrl Pts',(-1.94841133337646,7.88817981792983,
79.1613250192149));
#169506=CARTESIAN_POINT('Ctrl Pts',(-1.94844924982359,7.88817045232209,
79.1613265552921));
#169507=CARTESIAN_POINT('Ctrl Pts',(-1.94852507626911,7.8881517221194,79.1613296271834));
#169508=CARTESIAN_POINT('Ctrl Pts',(-1.94856298603782,7.8881423575813,79.1613311629881));
#169509=CARTESIAN_POINT('Ctrl Pts',(-1.94863879914926,7.88812362951256,
79.1613342343354));
#169510=CARTESIAN_POINT('Ctrl Pts',(-1.94867670250201,7.88811426597956,
79.1613357698783));
#169511=CARTESIAN_POINT('Ctrl Pts',(-1.94875250263959,7.88809553995638,
79.1613388406961));
#169512=CARTESIAN_POINT('Ctrl Pts',(-1.94879039957604,7.88808617742885,
79.1613403759772));
#169513=CARTESIAN_POINT('Ctrl Pts',(-1.9488661869626,7.88806745339675,79.1613434462746));
#169514=CARTESIAN_POINT('Ctrl Pts',(-1.94890407741564,7.88805809189157,
79.1613449812912));
#169515=CARTESIAN_POINT('Ctrl Pts',(-1.94897985188041,7.88803936989332,
79.1613480510613));
#169516=CARTESIAN_POINT('Ctrl Pts',(-1.94901773595153,7.88803000938569,
79.1613495858173));
#169517=CARTESIAN_POINT('Ctrl Pts',(-1.94909349773738,7.88801128936186,
79.16135265507));
#169518=CARTESIAN_POINT('Ctrl Pts',(-1.94913137540082,7.88800192985844,
79.1613541895646));
#169519=CARTESIAN_POINT('Ctrl Pts',(-1.94920712440952,7.88798321183387,
79.1613572582959));
#169520=CARTESIAN_POINT('Ctrl Pts',(-1.94924499575073,7.88797385331382,
79.1613587925324));
#169521=CARTESIAN_POINT('Ctrl Pts',(-1.94932073227924,7.88795513721571,
79.1613618607542));
#169522=CARTESIAN_POINT('Ctrl Pts',(-1.94935859723964,7.8879457796938,79.1613633947303));
#169523=CARTESIAN_POINT('Ctrl Pts',(-1.94943432077752,7.88792706564884,
79.1613664624221));
#169524=CARTESIAN_POINT('Ctrl Pts',(-1.94947217963067,7.88791770905775,
79.1613679961489));
#169525=CARTESIAN_POINT('Ctrl Pts',(-1.94954789125288,7.88789899680085,
79.1613710633541));
#169526=CARTESIAN_POINT('Ctrl Pts',(-1.9495857436448,7.88788964122833,79.1613725968172));
#169527=CARTESIAN_POINT('Ctrl Pts',(-1.9496614421218,7.88787093106393,79.161375663486));
#169528=CARTESIAN_POINT('Ctrl Pts',(-1.94969928853972,7.88786157638986,
79.1613771967052));
#169529=CARTESIAN_POINT('Ctrl Pts',(-1.94977497504477,7.88784286802853,
79.1613802628853));
#169530=CARTESIAN_POINT('Ctrl Pts',(-1.94981281519283,7.8878335143263,79.1613817958486));
#169531=CARTESIAN_POINT('Ctrl Pts',(-1.94988848938413,7.88781480785307,
79.1613848615259));
#169532=CARTESIAN_POINT('Ctrl Pts',(-1.94992632333294,7.88780545510551,
79.1613863942362));
#169533=CARTESIAN_POINT('Ctrl Pts',(-1.95000198501738,7.88778675056867,
79.161389459403));
#169534=CARTESIAN_POINT('Ctrl Pts',(-1.95003981294821,7.88777739873124,
79.1613909918675));
#169535=CARTESIAN_POINT('Ctrl Pts',(-1.95011546267391,7.88775869599584,
79.1613940565461));
#169536=CARTESIAN_POINT('Ctrl Pts',(-1.95015328445052,7.88774934510249,
79.1613955887594));
#169537=CARTESIAN_POINT('Ctrl Pts',(-1.95022892202693,7.88773064421619,
79.161398652942));
#169538=CARTESIAN_POINT('Ctrl Pts',(-1.95026673772477,7.88772129424854,
79.1614001849072));
#169539=CARTESIAN_POINT('Ctrl Pts',(-1.95034236313225,7.88770259521673,
79.1614032485929));
#169540=CARTESIAN_POINT('Ctrl Pts',(-1.95038017284784,7.88769324615118,
79.1614047803138));
#169541=CARTESIAN_POINT('Ctrl Pts',(-1.9504557863384,7.88767454891209,79.161407843513));
#169542=CARTESIAN_POINT('Ctrl Pts',(-1.95049359004318,7.88766520075599,
79.1614093749885));
#169543=CARTESIAN_POINT('Ctrl Pts',(-1.95056919144303,7.88764650535312,
79.161412437694));
#169544=CARTESIAN_POINT('Ctrl Pts',(-1.9506069892577,7.88763715807688,79.161413968929));
#169545=CARTESIAN_POINT('Ctrl Pts',(-1.95068257902129,7.88761846439839,
79.1614170311593));
#169546=CARTESIAN_POINT('Ctrl Pts',(-1.95072037082725,7.8876091180316,79.1614185621489));
#169547=CARTESIAN_POINT('Ctrl Pts',(-1.95079594871376,7.88759042613757,
79.1614216238943));
#169548=CARTESIAN_POINT('Ctrl Pts',(-1.95083373462223,7.88758108065299,
79.161423154643));
#169549=CARTESIAN_POINT('Ctrl Pts',(-1.95090930040535,7.88756239059993,
79.1614262158943));
#169550=CARTESIAN_POINT('Ctrl Pts',(-1.95094708063404,7.88755304594398,
79.161427746411));
#169551=CARTESIAN_POINT('Ctrl Pts',(-1.95102263538902,7.88753435746646,
79.1614308072117));
#169552=CARTESIAN_POINT('Ctrl Pts',(-1.9510604095568,7.88752501373366,79.161432337481));
#169553=CARTESIAN_POINT('Ctrl Pts',(-1.95113595207191,7.88750632713192,
79.161435397782));
#169554=CARTESIAN_POINT('Ctrl Pts',(-1.95117372064528,7.88749698420716,
79.1614369278227));
#169555=CARTESIAN_POINT('Ctrl Pts',(-1.95124925209198,7.88747829919194,
79.1614399876715));
#169556=CARTESIAN_POINT('Ctrl Pts',(-1.95128701476653,7.88746895715075,
79.1614415174714));
#169557=CARTESIAN_POINT('Ctrl Pts',(-1.95136253439556,7.88745027390792,
79.1614445768376));
#169558=CARTESIAN_POINT('Ctrl Pts',(-1.95140029144312,7.88744093268333,
79.1614461064076));
#169559=CARTESIAN_POINT('Ctrl Pts',(-1.9514757999335,7.88742225104541,79.1614491653187));
#169560=CARTESIAN_POINT('Ctrl Pts',(-1.95151355120057,7.88741291067565,
79.1614506946526));
#169561=CARTESIAN_POINT('Ctrl Pts',(-1.95158904806635,7.88739423076338,
79.161453753089));
#169562=CARTESIAN_POINT('Ctrl Pts',(-1.951626793769,7.88738489119523,79.1614552821956));
#169563=CARTESIAN_POINT('Ctrl Pts',(-1.95170227959926,7.88736621286336,
79.1614583401811));
#169564=CARTESIAN_POINT('Ctrl Pts',(-1.95174001959997,7.88735687413112,
79.1614598690548));
#169565=CARTESIAN_POINT('Ctrl Pts',(-1.95181549381266,7.88733819752417,
79.1614629265658));
#169566=CARTESIAN_POINT('Ctrl Pts',(-1.95185322838488,7.88732885956042,
79.1614644552177));
#169567=CARTESIAN_POINT('Ctrl Pts',(-1.9519286921361,7.88731018439281,79.1614675123011));
#169568=CARTESIAN_POINT('Ctrl Pts',(-1.95196642088589,7.88730084729526,
79.1614690407152));
#169569=CARTESIAN_POINT('Ctrl Pts',(-1.95204187253894,7.88728217397253,
79.1614720973047));
#169570=CARTESIAN_POINT('Ctrl Pts',(-1.95207959614115,7.88727283757445,
79.1614736255083));
#169571=CARTESIAN_POINT('Ctrl Pts',(-1.95215503791157,7.88725416554876,
79.1614766816936));
#169572=CARTESIAN_POINT('Ctrl Pts',(-1.95219275564322,7.8872448300293,79.1614782096576));
#169573=CARTESIAN_POINT('Ctrl Pts',(-1.95226818567163,7.88722615976135,
79.1614812653633));
#169574=CARTESIAN_POINT('Ctrl Pts',(-1.95230589815237,7.8872168249674,79.1614827931126));
#169575=CARTESIAN_POINT('Ctrl Pts',(-1.95238131772789,7.8871981561386,79.1614858483912));
#169576=CARTESIAN_POINT('Ctrl Pts',(-1.95241902467326,7.8871888221408,79.1614873759143));
#169577=CARTESIAN_POINT('Ctrl Pts',(-1.95249443332005,7.88717015486941,
79.1614904307462));
#169578=CARTESIAN_POINT('Ctrl Pts',(-1.95253213487561,7.88716082163199,
79.1614919580491));
#169579=CARTESIAN_POINT('Ctrl Pts',(-1.95260753258819,7.88714215591984,
79.1614950124343));
#169580=CARTESIAN_POINT('Ctrl Pts',(-1.95264522888111,7.88713282341156,
79.161496539522));
#169581=CARTESIAN_POINT('Ctrl Pts',(-1.95272061609433,7.88711415915149,
79.161499593478));
#169582=CARTESIAN_POINT('Ctrl Pts',(-1.95275830702106,7.8871048273982,79.1615011203465));
#169583=CARTESIAN_POINT('Ctrl Pts',(-1.95283368340743,7.88708616467176,
79.1615041738601));
#169584=CARTESIAN_POINT('Ctrl Pts',(-1.95287136913025,7.88707683363352,
79.1615057005158));
#169585=CARTESIAN_POINT('Ctrl Pts',(-1.9529467353201,7.88705817228512,79.1615087536125));
#169586=CARTESIAN_POINT('Ctrl Pts',(-1.95298441565574,7.88704884200755,
79.1615102800481));
#169587=CARTESIAN_POINT('Ctrl Pts',(-1.95305977119553,7.88703018214994,
79.1615133327095));
#169588=CARTESIAN_POINT('Ctrl Pts',(-1.9530974463303,7.88702085258715,79.1615148589325));
#169589=CARTESIAN_POINT('Ctrl Pts',(-1.9531727913719,7.88700219418319,79.1615179111648));
#169590=CARTESIAN_POINT('Ctrl Pts',(-1.95321046137423,7.88699286531846,
79.161519437178));
#169591=CARTESIAN_POINT('Ctrl Pts',(-1.95328579625346,7.88697420828547,
79.1615224889947));
#169592=CARTESIAN_POINT('Ctrl Pts',(-1.95332346104062,7.8869648801395,79.1615240147947));
#169593=CARTESIAN_POINT('Ctrl Pts',(-1.95339878559046,7.88694622451928,
79.1615270661892));
#169594=CARTESIAN_POINT('Ctrl Pts',(-1.95343644525625,7.88693689706909,
79.1615285917798));
#169595=CARTESIAN_POINT('Ctrl Pts',(-1.95351175959471,7.88691824283288,
79.1615316427568));
#169596=CARTESIAN_POINT('Ctrl Pts',(-1.95354941417775,7.88690891606912,
79.1615331681396));
#169597=CARTESIAN_POINT('Ctrl Pts',(-1.95362471823248,7.88689026323528,
79.1615362186962));
#169598=CARTESIAN_POINT('Ctrl Pts',(-1.95366236783991,7.88688093713165,
79.1615377438755));
#169599=CARTESIAN_POINT('Ctrl Pts',(-1.97298584429292,7.88209421330181,
79.1623205341811));
#169600=CARTESIAN_POINT('Ctrl Pts',(-1.99225412139981,7.8772460827388,79.1631008368244));
#169601=CARTESIAN_POINT('Ctrl Pts',(-2.03082277879275,7.86739117920091,
79.1646621290709));
#169602=CARTESIAN_POINT('Ctrl Pts',(-2.05012290505404,7.86238393891958,
79.1654431062218));
#169603=CARTESIAN_POINT('Ctrl Pts',(-2.09051212760801,7.85174649653286,
79.1670766859053));
#169604=CARTESIAN_POINT('Ctrl Pts',(-2.11159729117103,7.84610227347256,
79.1679290270509));
#169605=CARTESIAN_POINT('Ctrl Pts',(-2.17411248571074,7.82909751786587,
79.1704548680323));
#169606=CARTESIAN_POINT('Ctrl Pts',(-2.21547549311649,7.81749329487738,
79.1721245535412));
#169607=CARTESIAN_POINT('Ctrl Pts',(-2.43424034113709,7.75424398129068,
79.1809533096732));
#169608=CARTESIAN_POINT('Ctrl Pts',(-2.60993583625333,7.69688651878376,
79.1880382373002));
#169609=CARTESIAN_POINT('Ctrl Pts',(-2.92921653656757,7.58046347814742,
79.2010498932282));
#169610=CARTESIAN_POINT('Ctrl Pts',(-3.073357727662,7.52317807079658,79.2069767897038));
#169611=CARTESIAN_POINT('Ctrl Pts',(-3.28090948526638,7.43373066420509,
79.2156417948539));
#169612=CARTESIAN_POINT('Ctrl Pts',(-3.34567739738918,7.40480663783087,
79.2183646214665));
#169613=CARTESIAN_POINT('Ctrl Pts',(-3.53871969654899,7.31554805655254,
79.2265451623967));
#169614=CARTESIAN_POINT('Ctrl Pts',(-3.66580144257269,7.25270154389465,
79.2320182092772));
#169615=CARTESIAN_POINT('Ctrl Pts',(-3.83645074542028,7.1626778382182,79.2395104028353));
#169616=CARTESIAN_POINT('Ctrl Pts',(-3.88150139102779,7.13836501280901,
79.241502105676));
#169617=CARTESIAN_POINT('Ctrl Pts',(-3.95535999665793,7.09759925304234,
79.2447911043398));
#169618=CARTESIAN_POINT('Ctrl Pts',(-3.9843023699576,7.08139269324333,79.2460860012422));
#169619=CARTESIAN_POINT('Ctrl Pts',(-4.04249282396076,7.04833870913801,
79.2487019642452));
#169620=CARTESIAN_POINT('Ctrl Pts',(-4.07173679310006,7.03148535296479,
79.2500230654698));
#169621=CARTESIAN_POINT('Ctrl Pts',(-4.14401275725236,6.9892304833494,79.2533043747269));
#169622=CARTESIAN_POINT('Ctrl Pts',(-4.1869169736638,6.96361333704036,79.2552666138396));
#169623=CARTESIAN_POINT('Ctrl Pts',(-4.34180636793745,6.8691833905108,79.2624037430102));
#169624=CARTESIAN_POINT('Ctrl Pts',(-4.45235320409623,6.79805218144114,
79.2676000198836));
#169625=CARTESIAN_POINT('Ctrl Pts',(-4.7878828626092,6.57045982335032,79.2836896437482));
#169626=CARTESIAN_POINT('Ctrl Pts',(-5.00671457330853,6.40527690979999,
79.2946457049854));
#169627=CARTESIAN_POINT('Ctrl Pts',(-5.27338084610761,6.18195700106008,
79.3084894821777));
#169628=CARTESIAN_POINT('Ctrl Pts',(-5.32933270083204,6.13378765154651,
79.3114229166483));
#169629=CARTESIAN_POINT('Ctrl Pts',(-5.41178691203125,6.06082221503731,
79.3157844830949));
#169630=CARTESIAN_POINT('Ctrl Pts',(-5.4387920973462,6.03660037102309,79.3172192988634));
#169631=CARTESIAN_POINT('Ctrl Pts',(-5.48444755217761,5.99509541740975,
79.3196551331035));
#169632=CARTESIAN_POINT('Ctrl Pts',(-5.50318053019628,5.97790415398929,
79.3206575215902));
#169633=CARTESIAN_POINT('Ctrl Pts',(-5.53492659049098,5.94849508650658,
79.3223609876884));
#169634=CARTESIAN_POINT('Ctrl Pts',(-5.54798065055964,5.93632182917712,
79.3230628403995));
#169635=CARTESIAN_POINT('Ctrl Pts',(-5.57310411556495,5.91273827755227,
79.3244161766623));
#169636=CARTESIAN_POINT('Ctrl Pts',(-5.58517885566913,5.90133379617661,
79.3250677683967));
#169637=CARTESIAN_POINT('Ctrl Pts',(-5.61384275266395,5.87409423273916,
79.3266172157638));
#169638=CARTESIAN_POINT('Ctrl Pts',(-5.63040001011275,5.85822577548536,
79.3275143464349));
#169639=CARTESIAN_POINT('Ctrl Pts',(-5.68358208450952,5.80682239566888,
79.3304031698857));
#169640=CARTESIAN_POINT('Ctrl Pts',(-5.71993954157433,5.77101233222465,
79.3323892404417));
#169641=CARTESIAN_POINT('Ctrl Pts',(-6.06434917820577,5.42533579981107,
79.3513231294378));
#169642=CARTESIAN_POINT('Ctrl Pts',(-6.34727749853782,5.09143218799429,
79.3678243463143));
#169643=CARTESIAN_POINT('Ctrl Pts',(-6.77660607443729,4.49299824290805,
79.395804094763));
#169644=CARTESIAN_POINT('Ctrl Pts',(-6.93763031206454,4.24013039441526,
79.4072052852121));
#169645=CARTESIAN_POINT('Ctrl Pts',(-7.14236390248337,3.87561264261209,
79.4232863293808));
#169646=CARTESIAN_POINT('Ctrl Pts',(-7.19813685887801,3.77101589898547,
79.4278614429181));
#169647=CARTESIAN_POINT('Ctrl Pts',(-7.28069365319139,3.60767886783991,
79.4349554897496));
#169648=CARTESIAN_POINT('Ctrl Pts',(-7.30909944012245,3.54977635981188,
79.4374607204884));
#169649=CARTESIAN_POINT('Ctrl Pts',(-7.35535626318044,3.4525764267084,79.441651560756));
#169650=CARTESIAN_POINT('Ctrl Pts',(-7.37358898553961,3.4134638120929,79.4433340174387));
#169651=CARTESIAN_POINT('Ctrl Pts',(-7.40864256056318,3.33667576854119,
79.4466298518094));
#169652=CARTESIAN_POINT('Ctrl Pts',(-7.42548974467901,3.29901376354829,
79.4482429706135));
#169653=CARTESIAN_POINT('Ctrl Pts',(-7.44209777836504,3.26111456933565,
79.4498630049378));
#169654=CARTESIAN_POINT('Ctrl Pts',(-7.44214623868653,3.26100397716454,
79.4498677322696));
#169655=CARTESIAN_POINT('Ctrl Pts',(-7.44224334356792,3.26078235893044,
79.4498772054249));
#169656=CARTESIAN_POINT('Ctrl Pts',(-7.44229198810876,3.2606713328585,79.4498819512484));
#169657=CARTESIAN_POINT('Ctrl Pts',(-7.44238946323068,3.26044884255245,
79.4498914615692));
#169658=CARTESIAN_POINT('Ctrl Pts',(-7.44243829377661,3.2603373783454,79.4498962260649));
#169659=CARTESIAN_POINT('Ctrl Pts',(-7.45706657733138,3.22694373788202,
79.4513236163018));
#169660=CARTESIAN_POINT('Ctrl Pts',(-7.4714225898597,3.19356420015875,79.4527479041842));
#169661=CARTESIAN_POINT('Ctrl Pts',(-7.5041163315556,3.11611994700133,79.4560468152676));
#169662=CARTESIAN_POINT('Ctrl Pts',(-7.52229065536023,3.07198774696187,
79.4579225653743));
#169663=CARTESIAN_POINT('Ctrl Pts',(-7.57741300256708,2.93471295172874,
79.4637446934063));
#169664=CARTESIAN_POINT('Ctrl Pts',(-7.61302753758419,2.84104548796949,
79.4676997387034));
#169665=CARTESIAN_POINT('Ctrl Pts',(-7.76073995265698,2.42981596229223,
79.4849895200201));
#169666=CARTESIAN_POINT('Ctrl Pts',(-7.854765118708,2.10612179280337,79.4983623971184));
#169667=CARTESIAN_POINT('Ctrl Pts',(-8.08129933995873,1.0956990328556,79.5402666655479));
#169668=CARTESIAN_POINT('Ctrl Pts',(-8.14556302194663,0.397010978487219,
79.5699204200111));
#169669=CARTESIAN_POINT('Ctrl Pts',(-8.108688417812,-0.597143940885287,
79.6118234874032));
#169670=CARTESIAN_POINT('Ctrl Pts',(-8.0815348683483,-0.892309858572796,
79.6241587852685));
#169671=CARTESIAN_POINT('Ctrl Pts',(-8.03488495953414,-1.20866328992491,
79.6368880368299));
#169672=CARTESIAN_POINT('Ctrl Pts',(-8.03134450689027,-1.23196943421648,
79.6378228340485));
#169673=CARTESIAN_POINT('Ctrl Pts',(-8.02614388101788,-1.26522874202748,
79.639152278399));
#169674=CARTESIAN_POINT('Ctrl Pts',(-8.02456653388719,-1.27519461761843,
79.6395500487517));
#169675=CARTESIAN_POINT('Ctrl Pts',(-8.02180986837902,-1.29240390551888,
79.6402358838933));
#169676=CARTESIAN_POINT('Ctrl Pts',(-8.0206392944218,-1.29964869432815,
79.6405242880794));
#169677=CARTESIAN_POINT('Ctrl Pts',(-8.01837909756845,-1.31351790244831,
79.6410757756098));
#169678=CARTESIAN_POINT('Ctrl Pts',(-8.01729107724848,-1.32014257387951,
79.6413389222361));
#169679=CARTESIAN_POINT('Ctrl Pts',(-8.01472287049419,-1.33565943764376,
79.6419546343519));
#169680=CARTESIAN_POINT('Ctrl Pts',(-8.01323609207674,-1.34455054114052,
79.6423069330853));
#169681=CARTESIAN_POINT('Ctrl Pts',(-8.00811313887119,-1.37487605689249,
79.6435067875559));
#169682=CARTESIAN_POINT('Ctrl Pts',(-8.00440571425925,-1.39629846046266,
79.6443513890976));
#169683=CARTESIAN_POINT('Ctrl Pts',(-7.93907008183659,-1.76501039141687,
79.6588335865131));
#169684=CARTESIAN_POINT('Ctrl Pts',(-7.8549786721865,-2.10793912567164,
79.6713548347689));
#169685=CARTESIAN_POINT('Ctrl Pts',(-7.59824952072826,-2.92181068195103,
79.7005787980686));
#169686=CARTESIAN_POINT('Ctrl Pts',(-7.40381502759464,-3.38436344734547,
79.7168387199858));
#169687=CARTESIAN_POINT('Ctrl Pts',(-6.93130672607255,-4.26959230667677,
79.7509949997151));
#169688=CARTESIAN_POINT('Ctrl Pts',(-6.65395118467857,-4.69012734905862,
79.7688454272494));
#169689=CARTESIAN_POINT('Ctrl Pts',(-6.32196444513039,-5.10423766924018,
79.7892914992691));
#169690=CARTESIAN_POINT('Ctrl Pts',(-6.30428058851691,-5.12606309676613,
79.7903779201944));
#169691=CARTESIAN_POINT('Ctrl Pts',(-6.27832336961615,-5.15776202841568,
79.7919688572227));
#169692=CARTESIAN_POINT('Ctrl Pts',(-6.27013906135957,-5.16770835328576,
79.7924699401367));
#169693=CARTESIAN_POINT('Ctrl Pts',(-6.25573982002624,-5.18512307166601,
79.7933505995412));
#169694=CARTESIAN_POINT('Ctrl Pts',(-6.24953506809218,-5.19259986866516,
79.7937297816029));
#169695=CARTESIAN_POINT('Ctrl Pts',(-6.2374655889381,-5.20709075989434,
79.7944667878446));
#169696=CARTESIAN_POINT('Ctrl Pts',(-6.23160240244877,-5.21410612206178,
79.7948245519877));
#169697=CARTESIAN_POINT('Ctrl Pts',(-6.21758312453061,-5.23082290768202,
79.7956793683499));
#169698=CARTESIAN_POINT('Ctrl Pts',(-6.20941616135637,-5.24051515934319,
79.7961768436944));
#169699=CARTESIAN_POINT('Ctrl Pts',(-6.18467455248069,-5.26973855393352,
79.7976824423594));
#169700=CARTESIAN_POINT('Ctrl Pts',(-6.16803026223607,-5.28921037740669,
79.7986932866373));
#169701=CARTESIAN_POINT('Ctrl Pts',(-5.99335275549731,-5.49161630846467,
79.8092813739953));
#169702=CARTESIAN_POINT('Ctrl Pts',(-5.8273321890406,-5.6674786537219,79.8191760323589));
#169703=CARTESIAN_POINT('Ctrl Pts',(-5.54283205088212,-5.94310870958965,
79.8358662453626));
#169704=CARTESIAN_POINT('Ctrl Pts',(-5.4289002055741,-6.04736042238196,
79.8424855703851));
#169705=CARTESIAN_POINT('Ctrl Pts',(-4.79948178503529,-6.5911717327529,
79.8786451579491));
#169706=CARTESIAN_POINT('Ctrl Pts',(-4.23356660802693,-6.96817019509298,
79.909969508988));
#169707=CARTESIAN_POINT('Ctrl Pts',(-3.54362613275228,-7.31239915819436,
79.9434093858311));
#169708=CARTESIAN_POINT('Ctrl Pts',(-3.45906120635346,-7.35277933857432,
79.9474291721293));
#169709=CARTESIAN_POINT('Ctrl Pts',(-3.24717809390565,-7.44948990554553,
79.9572770793459));
#169710=CARTESIAN_POINT('Ctrl Pts',(-3.11906883995627,-7.50403104082421,
79.9630306492516));
#169711=CARTESIAN_POINT('Ctrl Pts',(-2.96152567164898,-7.56637068065159,
79.9698290985873));
#169712=CARTESIAN_POINT('Ctrl Pts',(-2.93338255546748,-7.57732580785143,
79.9710335451564));
#169713=CARTESIAN_POINT('Ctrl Pts',(-2.89448076384879,-7.59221969472611,
79.972685399136));
#169714=CARTESIAN_POINT('Ctrl Pts',(-2.88377408540563,-7.59629289926265,
79.9731386711016));
#169715=CARTESIAN_POINT('Ctrl Pts',(-2.86571253794426,-7.60312047067602,
79.9739010789906));
#169716=CARTESIAN_POINT('Ctrl Pts',(-2.85836224385052,-7.60588683358021,
79.9742107241688));
#169717=CARTESIAN_POINT('Ctrl Pts',(-2.84382928529955,-7.61133242783804,
79.9748217410348));
#169718=CARTESIAN_POINT('Ctrl Pts',(-2.83664681789742,-7.61401215930237,
79.9751231333656));
#169719=CARTESIAN_POINT('Ctrl Pts',(-2.82082577767653,-7.61988939177973,
79.9757857536848));
#169720=CARTESIAN_POINT('Ctrl Pts',(-2.81218553165092,-7.62308237836851,
79.9761467967505));
#169721=CARTESIAN_POINT('Ctrl Pts',(-2.78209646027183,-7.6341436198291,
79.9774012715646));
#169722=CARTESIAN_POINT('Ctrl Pts',(-2.76061978548504,-7.64193613784793,
79.9782916733892));
#169723=CARTESIAN_POINT('Ctrl Pts',(-2.50724267697428,-7.73266302876462,
79.9887402592492));
#169724=CARTESIAN_POINT('Ctrl Pts',(-2.27170853626954,-7.80510695827477,
79.997903124035));
#169725=CARTESIAN_POINT('Ctrl Pts',(-1.24319359192606,-8.07093700430364,
80.036717518111));
#169726=CARTESIAN_POINT('Ctrl Pts',(-0.426899983947643,-8.15496136964204,
80.065109091841));
#169727=CARTESIAN_POINT('Ctrl Pts',(0.494831248385932,-8.11087049864078,
80.1002571489554));
#169728=CARTESIAN_POINT('Ctrl Pts',(0.601324214880989,-8.10367119843295,
80.1043537111171));
#169729=CARTESIAN_POINT('Ctrl Pts',(0.743084156623056,-8.09127796786457,
80.1098561276645));
#169730=CARTESIAN_POINT('Ctrl Pts',(0.778504157261536,-8.08794686409379,
80.1112350434894));
#169731=CARTESIAN_POINT('Ctrl Pts',(0.837154975236383,-8.0820421514253,
80.1135250930859));
#169732=CARTESIAN_POINT('Ctrl Pts',(0.860398673824311,-8.07960072696592,
80.1144344127519));
#169733=CARTESIAN_POINT('Ctrl Pts',(0.905441327269623,-8.07467305397167,
80.1161999191652));
#169734=CARTESIAN_POINT('Ctrl Pts',(0.927241410210268,-8.07219872709752,
80.1170559305187));
#169735=CARTESIAN_POINT('Ctrl Pts',(0.976548503732556,-8.06639995657468,
80.1189956446018));
#169736=CARTESIAN_POINT('Ctrl Pts',(1.00404903735945,-8.06302305353095,
80.1200800454552));
#169737=CARTESIAN_POINT('Ctrl Pts',(1.08531684146909,-8.05262163196699,
80.123292539672));
#169738=CARTESIAN_POINT('Ctrl Pts',(1.13903142057696,-8.04519950966483,
80.1254261664822));
#169739=CARTESIAN_POINT('Ctrl Pts',(1.74556550477174,-7.95519431031257,
80.1496458110455));
#169740=CARTESIAN_POINT('Ctrl Pts',(2.28848124585185,-7.81632195398078,
80.1726743097189));
#169741=CARTESIAN_POINT('Ctrl Pts',(2.9498773626595,-7.57226902120199,80.2024754480087));
#169742=CARTESIAN_POINT('Ctrl Pts',(3.08555978973163,-7.51800206380859,
80.2086771757578));
#169743=CARTESIAN_POINT('Ctrl Pts',(3.58007475896511,-7.30457454173073,
80.2315329771549));
#169744=CARTESIAN_POINT('Ctrl Pts',(3.92871379136949,-7.12312937015013,
80.248174196319));
#169745=CARTESIAN_POINT('Ctrl Pts',(4.30585141668263,-6.89070962195107,
80.2660287494273));
#169746=CARTESIAN_POINT('Ctrl Pts',(4.34857657533092,-6.86382673223187,
80.2680487075212));
#169747=CARTESIAN_POINT('Ctrl Pts',(4.40274650697278,-6.82903390234082,
80.2706038552923));
#169748=CARTESIAN_POINT('Ctrl Pts',(4.41442480561729,-6.82149063492429,
80.2711543571048));
#169749=CARTESIAN_POINT('Ctrl Pts',(4.43312023609077,-6.80934673359565,
80.2720350073022));
#169750=CARTESIAN_POINT('Ctrl Pts',(4.44014967542445,-6.80476515586194,
80.272365986127));
#169751=CARTESIAN_POINT('Ctrl Pts',(4.45346705308614,-6.79605586684041,
80.2729927409777));
#169752=CARTESIAN_POINT('Ctrl Pts',(4.45975637865332,-6.7919302986462,80.2732886123013));
#169753=CARTESIAN_POINT('Ctrl Pts',(4.47400451186946,-6.78255571923566,
80.2739585998714));
#169754=CARTESIAN_POINT('Ctrl Pts',(4.48195983645202,-6.77730141591512,
80.2743324738295));
#169755=CARTESIAN_POINT('Ctrl Pts',(4.50592873408012,-6.76140986702241,
80.2754582651974));
#169756=CARTESIAN_POINT('Ctrl Pts',(4.5219138892313,-6.75072973337289,80.2762081685908));
#169757=CARTESIAN_POINT('Ctrl Pts',(4.64961327478309,-6.66475307450011,
80.2821907617029));
#169758=CARTESIAN_POINT('Ctrl Pts',(4.75946565288033,-6.58675372179188,
80.2872750161332));
#169759=CARTESIAN_POINT('Ctrl Pts',(4.90163552238049,-6.48039282188968,
80.2938017440323));
#169760=CARTESIAN_POINT('Ctrl Pts',(4.93572683987588,-6.45446531932871,
80.2953633030543));
#169761=CARTESIAN_POINT('Ctrl Pts',(5.04254554154338,-6.37188516063423,
80.3002496549951));
#169762=CARTESIAN_POINT('Ctrl Pts',(5.11451567354246,-6.314262909118,80.303532295113));
#169763=CARTESIAN_POINT('Ctrl Pts',(5.76082675676988,-5.77849772200924,
80.3330539952394));
#169764=CARTESIAN_POINT('Ctrl Pts',(6.26762705064367,-5.22447338285556,
80.3568081953172));
#169765=CARTESIAN_POINT('Ctrl Pts',(6.86659777771854,-4.35485119343471,
80.3943050864318));
#169766=CARTESIAN_POINT('Ctrl Pts',(7.02699372817844,-4.09099407240808,
80.4056604054243));
#169767=CARTESIAN_POINT('Ctrl Pts',(7.18444551444592,-3.79527764830921,
80.418576512421));
#169768=CARTESIAN_POINT('Ctrl Pts',(7.19678498398481,-3.77182656764837,
80.4196019478341));
#169769=CARTESIAN_POINT('Ctrl Pts',(7.21481127316018,-3.73715721205776,
80.4211197223189));
#169770=CARTESIAN_POINT('Ctrl Pts',(7.2205871703039,-3.725985325965,80.4216090859016));
#169771=CARTESIAN_POINT('Ctrl Pts',(7.23075864020387,-3.70619893958151,
80.4224762887091));
#169772=CARTESIAN_POINT('Ctrl Pts',(7.23516482077516,-3.6975899053385,80.4228537736425));
#169773=CARTESIAN_POINT('Ctrl Pts',(7.24375045343898,-3.6807407268815,80.4235928986079));
#169774=CARTESIAN_POINT('Ctrl Pts',(7.24793124234487,-3.67250127784988,
80.4239544934289));
#169775=CARTESIAN_POINT('Ctrl Pts',(7.25916614117057,-3.65026576399187,
80.4249307379771));
#169776=CARTESIAN_POINT('Ctrl Pts',(7.26619380696334,-3.6362564223695,80.4255462637295));
#169777=CARTESIAN_POINT('Ctrl Pts',(7.29191839136537,-3.58460323738164,
80.4278174319999));
#169778=CARTESIAN_POINT('Ctrl Pts',(7.31036351679667,-3.54683512214842,
80.4294813843808));
#169779=CARTESIAN_POINT('Ctrl Pts',(7.62902417998136,-2.88130117491019,
80.458863744309));
#169780=CARTESIAN_POINT('Ctrl Pts',(7.84762000705927,-2.21776596444659,
80.4894339262253));
#169781=CARTESIAN_POINT('Ctrl Pts',(8.05421590018177,-1.14361082310715,
80.538737387914));
#169782=CARTESIAN_POINT('Ctrl Pts',(8.10057891496814,-0.747581756129389,
80.5567974548414));
#169783=CARTESIAN_POINT('Ctrl Pts',(8.12269738095583,-0.234200122211309,
80.5790892261596));
#169784=CARTESIAN_POINT('Ctrl Pts',(8.12520814609431,-0.11856077287903,
80.5840358250579));
#169785=CARTESIAN_POINT('Ctrl Pts',(8.12529666042017,0.129105673270558,
80.5944232779334));
#169786=CARTESIAN_POINT('Ctrl Pts',(8.1221269073351,0.261102652816135,80.5998289460686));
#169787=CARTESIAN_POINT('Ctrl Pts',(8.11485051036185,0.411373115696335,
80.6058136959489));
#169788=CARTESIAN_POINT('Ctrl Pts',(8.11389737312719,0.429762809132297,
80.6065434389428));
#169789=CARTESIAN_POINT('Ctrl Pts',(8.11237862533107,0.457256824481047,
80.6076306948971));
#169790=CARTESIAN_POINT('Ctrl Pts',(8.11186019030103,0.46636361157105,80.6079902063516));
#169791=CARTESIAN_POINT('Ctrl Pts',(8.11090559125271,0.482648702346258,
80.6086320217353));
#169792=CARTESIAN_POINT('Ctrl Pts',(8.11047523086395,0.489827326796356,
80.6089145660402));
#169793=CARTESIAN_POINT('Ctrl Pts',(8.10954493707778,0.505007676343931,
80.6095112769365));
#169794=CARTESIAN_POINT('Ctrl Pts',(8.10904268973662,0.513009255549799,
80.6098253488854));
#169795=CARTESIAN_POINT('Ctrl Pts',(8.10767755195224,0.534255021866719,
80.6106580926137));
#169796=CARTESIAN_POINT('Ctrl Pts',(8.10679405041784,0.547497891841711,
80.6111759399136));
#169797=CARTESIAN_POINT('Ctrl Pts',(8.10256105203657,0.608688916857114,
80.6135633505826));
#169798=CARTESIAN_POINT('Ctrl Pts',(8.09881854971916,0.656609482743975,
80.615417699697));
#169799=CARTESIAN_POINT('Ctrl Pts',(8.06232803287315,1.07588594626633,80.6315283753008));
#169800=CARTESIAN_POINT('Ctrl Pts',(8.00448149591947,1.44463542380424,80.6449428211977));
#169801=CARTESIAN_POINT('Ctrl Pts',(7.81282683882899,2.28428722419117,80.6758177467193));
#169802=CARTESIAN_POINT('Ctrl Pts',(7.66143275245466,2.74966762476547,80.6932327669446));
#169803=CARTESIAN_POINT('Ctrl Pts',(7.30323188719196,3.58610676120484,80.7269901137275));
#169804=CARTESIAN_POINT('Ctrl Pts',(7.10740349901889,3.96006894938149,80.7430652641163));
#169805=CARTESIAN_POINT('Ctrl Pts',(6.82408408530577,4.41180841967697,80.7636739943391));
#169806=CARTESIAN_POINT('Ctrl Pts',(6.76275853439752,4.50524958718629,80.7680086994423));
#169807=CARTESIAN_POINT('Ctrl Pts',(6.67169259382201,4.63795485454312,80.7742787784615));
#169808=CARTESIAN_POINT('Ctrl Pts',(6.64349197906995,4.67826053093083,80.776198672709));
#169809=CARTESIAN_POINT('Ctrl Pts',(6.59292970082035,4.74914734523146,80.7796037148111));
#169810=CARTESIAN_POINT('Ctrl Pts',(6.57071686423912,4.77983288656315,80.7810872898421));
#169811=CARTESIAN_POINT('Ctrl Pts',(6.52390466738483,4.84355779156074,80.7841887699726));
#169812=CARTESIAN_POINT('Ctrl Pts',(6.49926701705495,4.87656768773171,80.7858070437115));
#169813=CARTESIAN_POINT('Ctrl Pts',(6.43388540231772,4.96279133168555,80.7900655123056));
#169814=CARTESIAN_POINT('Ctrl Pts',(6.39273231220045,5.01569064848147,80.7927100227115));
#169815=CARTESIAN_POINT('Ctrl Pts',(6.18610467256461,5.2746208583289,80.8058173005992));
#169816=CARTESIAN_POINT('Ctrl Pts',(6.01130449031638,5.47300011999977,80.8163808359492));
#169817=CARTESIAN_POINT('Ctrl Pts',(5.62068189614564,5.87498069793229,80.8389777022667));
#169818=CARTESIAN_POINT('Ctrl Pts',(5.40274579160056,6.07600184752323,80.8510182949538));
#169819=CARTESIAN_POINT('Ctrl Pts',(4.91751006313996,6.4767836980718,80.8765940861616));
#169820=CARTESIAN_POINT('Ctrl Pts',(4.64789412919812,6.67290936117833,80.8901054505419));
#169821=CARTESIAN_POINT('Ctrl Pts',(4.32111236860767,6.88117987047064,80.905520331601));
#169822=CARTESIAN_POINT('Ctrl Pts',(4.27493222371801,6.90996404221723,80.9076773794519));
#169823=CARTESIAN_POINT('Ctrl Pts',(4.20859309488172,6.95039375502747,80.9107444677031));
#169824=CARTESIAN_POINT('Ctrl Pts',(4.18866802644074,6.96241979191648,80.9116616517794));
#169825=CARTESIAN_POINT('Ctrl Pts',(4.15284425202332,6.98383226018462,80.9133033574825));
#169826=CARTESIAN_POINT('Ctrl Pts',(4.13696472367219,6.99325041007904,80.9140285112471));
#169827=CARTESIAN_POINT('Ctrl Pts',(4.10198888064589,7.01383376681524,80.9156203092729));
#169828=CARTESIAN_POINT('Ctrl Pts',(4.08287877856378,7.02497528606073,80.9164865118778));
#169829=CARTESIAN_POINT('Ctrl Pts',(4.02762828412385,7.05688567436464,80.9189811771923));
#169830=CARTESIAN_POINT('Ctrl Pts',(3.99137316627603,7.07745471840137,80.9206062908325));
#169831=CARTESIAN_POINT('Ctrl Pts',(3.81747246452006,7.17435459822572,80.9283498449519));
#169832=CARTESIAN_POINT('Ctrl Pts',(3.67778542959045,7.24695488587093,80.9344178344348));
#169833=CARTESIAN_POINT('Ctrl Pts',(3.2716870945602,7.4432510076197,80.9517730955065));
#169834=CARTESIAN_POINT('Ctrl Pts',(3.00056496329956,7.55662166852448,80.963026573868));
#169835=CARTESIAN_POINT('Ctrl Pts',(2.655899843565,7.67926386047105,80.9772017949938));
#169836=CARTESIAN_POINT('Ctrl Pts',(2.58757817016605,7.70255389820744,80.9800048079079));
#169837=CARTESIAN_POINT('Ctrl Pts',(2.48030765741858,7.73753280854493,80.9843980784981));
#169838=CARTESIAN_POINT('Ctrl Pts',(2.44156585693646,7.74984491393775,80.9859831892342));
#169839=CARTESIAN_POINT('Ctrl Pts',(2.36924125897723,7.77223343902952,80.9889399345093));
#169840=CARTESIAN_POINT('Ctrl Pts',(2.3356824498974,7.78238422704716,80.9903109163695));
#169841=CARTESIAN_POINT('Ctrl Pts',(2.2602814232518,7.80465970763496,80.9933894612701));
#169842=CARTESIAN_POINT('Ctrl Pts',(2.21840531223,7.81666572880469,80.9950979692793));
#169843=CARTESIAN_POINT('Ctrl Pts',(2.09031882062074,7.85227635580488,81.0003206102493));
#169844=CARTESIAN_POINT('Ctrl Pts',(2.00381412016627,7.87479558796864,81.0038434942154));
#169845=CARTESIAN_POINT('Ctrl Pts',(1.85220985007238,7.91160194768301,81.0100115572356));
#169846=CARTESIAN_POINT('Ctrl Pts',(1.78727307790877,7.9265239288191,81.0126516041767));
#169847=CARTESIAN_POINT('Ctrl Pts',(1.48378140644731,7.99234494070813,81.0249807900875));
#169848=CARTESIAN_POINT('Ctrl Pts',(1.24319657371835,8.03328362040867,81.034732580768));
#169849=CARTESIAN_POINT('Ctrl Pts',(0.81466573281204,8.08648965914828,81.0519761769169));
#169850=CARTESIAN_POINT('Ctrl Pts',(0.627445408230941,8.10316658532627,
81.0594661245974));
#169851=CARTESIAN_POINT('Ctrl Pts',(0.405978431881623,8.11517204411552,
81.0682162877837));
#169852=CARTESIAN_POINT('Ctrl Pts',(0.372131306239305,8.11679457044921,
81.0695505095287));
#169853=CARTESIAN_POINT('Ctrl Pts',(0.319929534305792,8.11896974947659,
81.0716029425798));
#169854=CARTESIAN_POINT('Ctrl Pts',(0.301581661774526,8.1196719885897,81.0723233004479));
#169855=CARTESIAN_POINT('Ctrl Pts',(0.262936815650409,8.12101989705131,
81.0738384725647));
#169856=CARTESIAN_POINT('Ctrl Pts',(0.242639518906035,8.12165167958616,
81.0746330893633));
#169857=CARTESIAN_POINT('Ctrl Pts',(0.193602941383203,8.12299402329623,
81.0765501768139));
#169858=CARTESIAN_POINT('Ctrl Pts',(0.1648618075648,8.1236281669237,81.0776716227412));
#169859=CARTESIAN_POINT('Ctrl Pts',(0.0621024395873807,8.12534987967175,
81.0816743273612));
#169860=CARTESIAN_POINT('Ctrl Pts',(-0.0119268664681597,8.12557845625808,
81.0845452538756));
#169861=CARTESIAN_POINT('Ctrl Pts',(-0.369994541686901,8.12179058581634,
81.098391877387));
#169862=CARTESIAN_POINT('Ctrl Pts',(-0.653688961810558,8.10389236920271,
81.1092478177369));
#169863=CARTESIAN_POINT('Ctrl Pts',(-1.08978901644335,8.05332595479917,
81.1260819407022));
#169864=CARTESIAN_POINT('Ctrl Pts',(-1.24317143395505,8.03107860112409,
81.1320297526505));
#169865=CARTESIAN_POINT('Ctrl Pts',(-1.58221447599178,7.97195603875809,
81.1452899149938));
#169866=CARTESIAN_POINT('Ctrl Pts',(-1.76741206402433,7.93295274603368,
81.1526097747279));
#169867=CARTESIAN_POINT('Ctrl Pts',(-2.01583687268292,7.87150173927167,
81.1625693127194));
#169868=CARTESIAN_POINT('Ctrl Pts',(-2.08039616855866,7.85468584093349,
81.1651704116254));
#169869=CARTESIAN_POINT('Ctrl Pts',(-2.19801190844992,7.82249842111764,
81.1699338931605));
#169870=CARTESIAN_POINT('Ctrl Pts',(-2.25113280011631,7.80737721562312,
81.1720946097677));
#169871=CARTESIAN_POINT('Ctrl Pts',(-2.36132569144571,7.77479197617668,
81.1765965837412));
#169872=CARTESIAN_POINT('Ctrl Pts',(-2.41836778989625,7.75723832918322,
81.1789382242761));
#169873=CARTESIAN_POINT('Ctrl Pts',(-2.58397954931485,7.70427011446431,
81.1857696217646));
#169874=CARTESIAN_POINT('Ctrl Pts',(-2.69200208731398,7.66719328768862,
81.1902670756382));
#169875=CARTESIAN_POINT('Ctrl Pts',(-2.97427919277889,7.56360554216872,
81.2021261824926));
#169876=CARTESIAN_POINT('Ctrl Pts',(-3.14708771209144,7.49335068137522,
81.2094959931763));
#169877=CARTESIAN_POINT('Ctrl Pts',(-3.37894138490143,7.38965483751212,
81.2195083376915));
#169878=CARTESIAN_POINT('Ctrl Pts',(-3.4402116620601,7.36133053613394,81.2221662148209));
#169879=CARTESIAN_POINT('Ctrl Pts',(-3.53497466023058,7.31608153362273,
81.2262934579289));
#169880=CARTESIAN_POINT('Ctrl Pts',(-3.56871502384484,7.29968272919635,
81.2277662436392));
#169881=CARTESIAN_POINT('Ctrl Pts',(-3.64326353097164,7.26280956611457,
81.2310270058664));
#169882=CARTESIAN_POINT('Ctrl Pts',(-3.68401513931543,7.24222372074472,
81.2328140322197));
#169883=CARTESIAN_POINT('Ctrl Pts',(-3.85591077897572,7.15356359273791,
81.2403754576911));
#169884=CARTESIAN_POINT('Ctrl Pts',(-3.9853588513958,7.08226200656618,81.2461285044163));
#169885=CARTESIAN_POINT('Ctrl Pts',(-4.27382331106329,6.91295782530399,
81.259151107472));
#169886=CARTESIAN_POINT('Ctrl Pts',(-4.43154955123481,6.81292300257379,
81.2664172139082));
#169887=CARTESIAN_POINT('Ctrl Pts',(-4.63996055441071,6.67044044216308,
81.2762813878693));
#169888=CARTESIAN_POINT('Ctrl Pts',(-4.69377976955234,6.63267978098273,
81.2788532106595));
#169889=CARTESIAN_POINT('Ctrl Pts',(-4.7871010189209,6.56549895226251,81.2833586103617));
#169890=CARTESIAN_POINT('Ctrl Pts',(-4.82680489320903,6.53636498081505,
81.2852903033399));
#169891=CARTESIAN_POINT('Ctrl Pts',(-4.91932878920685,6.4671698872635,81.289828160186));
#169892=CARTESIAN_POINT('Ctrl Pts',(-4.97192817960097,6.42681975912757,
81.2924361771976));
#169893=CARTESIAN_POINT('Ctrl Pts',(-5.135339957683,6.29825616889112,81.3006313859687));
#169894=CARTESIAN_POINT('Ctrl Pts',(-5.24434262832098,6.20778681756965,
81.3062347090037));
#169895=CARTESIAN_POINT('Ctrl Pts',(-5.43445159165915,6.04141898500454,
81.3162672446698));
#169896=CARTESIAN_POINT('Ctrl Pts',(-5.5164720412083,5.96661909978844,81.3206870843479));
#169897=CARTESIAN_POINT('Ctrl Pts',(-5.74376736746391,5.75063916943936,
81.3331994109807));
#169898=CARTESIAN_POINT('Ctrl Pts',(-5.88533182185289,5.60567420615562,
81.3413110445535));
#169899=CARTESIAN_POINT('Ctrl Pts',(-6.03694456536234,5.43833877674629,
81.3503487414014));
#169900=CARTESIAN_POINT('Ctrl Pts',(-6.05248440961696,5.42103872038097,
81.3512793635894));
#169901=CARTESIAN_POINT('Ctrl Pts',(-6.11121937347249,5.35508342212963,
81.3548129633114));
#169902=CARTESIAN_POINT('Ctrl Pts',(-6.15390387138072,5.30597661662688,
81.3574144780495));
#169903=CARTESIAN_POINT('Ctrl Pts',(-6.30057988257971,5.13308068204843,
81.3664685577532));
#169904=CARTESIAN_POINT('Ctrl Pts',(-6.40146403186574,5.00670383906051,
81.3729023536171));
#169905=CARTESIAN_POINT('Ctrl Pts',(-6.52111926621317,4.84727856949658,
81.3807682647321));
#169906=CARTESIAN_POINT('Ctrl Pts',(-6.54351747562544,4.8169995931263,81.3822513989634));
#169907=CARTESIAN_POINT('Ctrl Pts',(-6.57877179243205,4.76864145295588,
81.3846024443188));
#169908=CARTESIAN_POINT('Ctrl Pts',(-6.59176573309836,4.75066354609143,
81.3854726492595));
#169909=CARTESIAN_POINT('Ctrl Pts',(-6.61617220563892,4.71660278146744,
81.3871139664015));
#169910=CARTESIAN_POINT('Ctrl Pts',(-6.62760012110755,4.70053114986841,
81.3878853525227));
#169911=CARTESIAN_POINT('Ctrl Pts',(-6.654746910764,4.66205748988672,81.389724514324));
#169912=CARTESIAN_POINT('Ctrl Pts',(-6.670411348865,4.63961732567824,81.3907912131702));
#169913=CARTESIAN_POINT('Ctrl Pts',(-6.7329011502954,4.54912662986257,81.3950698449066));
#169914=CARTESIAN_POINT('Ctrl Pts',(-6.77880122275737,4.48044251888115,
81.3982658041701));
#169915=CARTESIAN_POINT('Ctrl Pts',(-6.90670688812173,4.28258054662003,
81.4073493506183));
#169916=CARTESIAN_POINT('Ctrl Pts',(-6.98612223603341,4.15176984356778,
81.4132084872747));
#169917=CARTESIAN_POINT('Ctrl Pts',(-7.21590606495064,3.74799531883072,
81.4309890038107));
#169918=CARTESIAN_POINT('Ctrl Pts',(-7.35430936779103,3.46855886464907,
81.4428958805196));
#169919=CARTESIAN_POINT('Ctrl Pts',(-7.50284778443874,3.11954332282749,
81.457588352001));
#169920=CARTESIAN_POINT('Ctrl Pts',(-7.52859200701767,3.05689020745503,
81.4602184085665));
#169921=CARTESIAN_POINT('Ctrl Pts',(-7.56806601876324,2.95729882396646,
81.4643894495567));
#169922=CARTESIAN_POINT('Ctrl Pts',(-7.58231569140425,2.92056986559936,
81.4659256615787));
#169923=CARTESIAN_POINT('Ctrl Pts',(-7.60754859683111,2.85410175856874,
81.4687023920728));
#169924=CARTESIAN_POINT('Ctrl Pts',(-7.61862597983699,2.8243991702804,81.4699420329541));
#169925=CARTESIAN_POINT('Ctrl Pts',(-7.64453396318579,2.75366868562953,
81.4728913319673));
#169926=CARTESIAN_POINT('Ctrl Pts',(-7.65920849768165,2.71258472931922,
81.4746023374135));
#169927=CARTESIAN_POINT('Ctrl Pts',(-7.70325829742431,2.58605169799811,
81.4798660164617));
#169928=CARTESIAN_POINT('Ctrl Pts',(-7.73153954278329,2.50022957247542,
81.4834278997582));
#169929=CARTESIAN_POINT('Ctrl Pts',(-7.7962164734376,2.29235965878099,81.4920361103963));
#169930=CARTESIAN_POINT('Ctrl Pts',(-7.83118552209573,2.16989333244498,
81.4970922375113));
#169931=CARTESIAN_POINT('Ctrl Pts',(-7.92392564316205,1.81358545422193,
81.5117479636237));
#169932=CARTESIAN_POINT('Ctrl Pts',(-7.97419697936925,1.57793289309484,
81.5213774945733));
#169933=CARTESIAN_POINT('Ctrl Pts',(-8.02698230663629,1.26234132770517,
81.5340897875249));
#169934=CARTESIAN_POINT('Ctrl Pts',(-8.03889664921228,1.18409939204704,
81.5372260899323));
#169935=CARTESIAN_POINT('Ctrl Pts',(-8.05320510462085,1.07993121567006,
81.5413757022493));
#169936=CARTESIAN_POINT('Ctrl Pts',(-8.05662036561507,1.05414997904124,
81.5424006064654));
#169937=CARTESIAN_POINT('Ctrl Pts',(-8.06218889979259,1.01050552427739,
81.5441317949691));
#169938=CARTESIAN_POINT('Ctrl Pts',(-8.06440671861917,0.992650769178743,
81.5448389284957));
#169939=CARTESIAN_POINT('Ctrl Pts',(-8.06880676114472,0.956239567780087,
81.5462786516932));
#169940=CARTESIAN_POINT('Ctrl Pts',(-8.0709843207416,0.937682653378452,
81.5470111645334));
#169941=CARTESIAN_POINT('Ctrl Pts',(-8.07616680013874,0.892162220894048,
81.5488048744853));
#169942=CARTESIAN_POINT('Ctrl Pts',(-8.07910071872581,0.865190844377972,
81.5498649929472));
#169943=CARTESIAN_POINT('Ctrl Pts',(-8.08999607218282,0.760138822116573,
81.5539844571854));
#169944=CARTESIAN_POINT('Ctrl Pts',(-8.09696116041502,0.681958663565181,
81.5570294799938));
#169945=CARTESIAN_POINT('Ctrl Pts',(-8.10802951141499,0.533397899484663,
81.5627854375292));
#169946=CARTESIAN_POINT('Ctrl Pts',(-8.11235163682892,0.463040922240359,
81.5654985421627));
#169947=CARTESIAN_POINT('Ctrl Pts',(-8.13085809759842,0.0805140055900297,
81.5801976460154));
#169948=CARTESIAN_POINT('Ctrl Pts',(-8.1279402115312,-0.232222304050683,
81.5920324053402));
#169949=CARTESIAN_POINT('Ctrl Pts',(-8.09080517474827,-0.78561704156093,
81.613098804559));
#169950=CARTESIAN_POINT('Ctrl Pts',(-8.06380055018787,-1.02637316650304,
81.6223051959032));
#169951=CARTESIAN_POINT('Ctrl Pts',(-7.98942409005349,-1.49806236256277,
81.6405942038987));
#169952=CARTESIAN_POINT('Ctrl Pts',(-7.94267825250679,-1.72885739461075,
81.6496643996561));
#169953=CARTESIAN_POINT('Ctrl Pts',(-7.87009051064721,-2.0213149239379,
81.6613787439906));
#169954=CARTESIAN_POINT('Ctrl Pts',(-7.85342172396327,-2.08513928417403,
81.6639487289844));
#169955=CARTESIAN_POINT('Ctrl Pts',(-7.82520583494853,-2.18803572628742,
81.6681150423225));
#169956=CARTESIAN_POINT('Ctrl Pts',(-7.81413875724294,-2.22723644182065,
81.6697077370789));
#169957=CARTESIAN_POINT('Ctrl Pts',(-7.79246853100146,-2.3018444183806,
81.6727496501274));
#169958=CARTESIAN_POINT('Ctrl Pts',(-7.78191763001751,-2.33726582202524,
81.6741984561183));
#169959=CARTESIAN_POINT('Ctrl Pts',(-7.75701439363559,-2.41883247333226,
81.6775455221723));
#169960=CARTESIAN_POINT('Ctrl Pts',(-7.74249133222642,-2.46492409342769,
81.679444919971));
#169961=CARTESIAN_POINT('Ctrl Pts',(-7.69555339661151,-2.60938147193878,
81.6854236316002));
#169962=CARTESIAN_POINT('Ctrl Pts',(-7.66166862545484,-2.70725828762598,
81.689512287444));
#169963=CARTESIAN_POINT('Ctrl Pts',(-7.46407230654591,-3.24456461400162,
81.7121703928581));
#169964=CARTESIAN_POINT('Ctrl Pts',(-7.26443325304684,-3.66981835377763,
81.7308338806236));
#169965=CARTESIAN_POINT('Ctrl Pts',(-6.63490858955856,-4.75560213046735,
81.7823936501349));
#169966=CARTESIAN_POINT('Ctrl Pts',(-6.14400767792136,-5.37482346916863,
81.8166454670327));
#169967=CARTESIAN_POINT('Ctrl Pts',(-5.51183074622765,-5.97044549045938,
81.8519448270577));
#169968=CARTESIAN_POINT('Ctrl Pts',(-5.45090795953746,-6.02611819264225,
81.855263620101));
#169969=CARTESIAN_POINT('Ctrl Pts',(-5.37783255506363,-6.09088114479934,
81.8591371718244));
#169970=CARTESIAN_POINT('Ctrl Pts',(-5.36649053925253,-6.10087660965179,
81.8597353817757));
#169971=CARTESIAN_POINT('Ctrl Pts',(-5.34809238586035,-6.11699948713437,
81.860700812379));
#169972=CARTESIAN_POINT('Ctrl Pts',(-5.34105348542202,-6.12314645913878,
81.8610690102268));
#169973=CARTESIAN_POINT('Ctrl Pts',(-5.32855836589666,-6.13402033065851,
81.8617205337273));
#169974=CARTESIAN_POINT('Ctrl Pts',(-5.32310642958805,-6.13875212200346,
81.8620041094347));
#169975=CARTESIAN_POINT('Ctrl Pts',(-5.31167658836193,-6.14864552241621,
81.8625971400557));
#169976=CARTESIAN_POINT('Ctrl Pts',(-5.30569744643427,-6.15380569624585,
81.8629065202685));
#169977=CARTESIAN_POINT('Ctrl Pts',(-5.290055314261,-6.16726556848658,81.863713670438));
#169978=CARTESIAN_POINT('Ctrl Pts',(-5.28038029080375,-6.17555129580364,
81.8642106998065));
#169979=CARTESIAN_POINT('Ctrl Pts',(-5.23809285415745,-6.21159438856918,
81.8663733242762));
#169980=CARTESIAN_POINT('Ctrl Pts',(-5.20528035224113,-6.23911677638299,
81.8680260939126));
#169981=CARTESIAN_POINT('Ctrl Pts',(-4.95913456579828,-6.44228481318374,
81.8802269082415));
#169982=CARTESIAN_POINT('Ctrl Pts',(-4.73717089428763,-6.60721405815946,
81.8901235807326));
#169983=CARTESIAN_POINT('Ctrl Pts',(-4.02491825212102,-7.08207138350816,
81.9197726119515));
#169984=CARTESIAN_POINT('Ctrl Pts',(-3.50958010288958,-7.35109459795958,
81.938425203669));
#169985=CARTESIAN_POINT('Ctrl Pts',(-2.5360514171208,-7.73339985513728,
81.9742047373154));
#169986=CARTESIAN_POINT('Ctrl Pts',(-2.08829588195924,-7.86612937666202,
81.9908397617143));
#169987=CARTESIAN_POINT('Ctrl Pts',(-1.60017175882261,-7.96618922166575,
82.009997076446));
#169988=CARTESIAN_POINT('Ctrl Pts',(-1.56865124500534,-7.97245593382428,
82.0112383060995));
#169989=CARTESIAN_POINT('Ctrl Pts',(-1.5247278302872,-7.98091794339299,
82.0129738767691));
#169990=CARTESIAN_POINT('Ctrl Pts',(-1.51235557918698,-7.98327168371586,
82.0134634022728));
#169991=CARTESIAN_POINT('Ctrl Pts',(-1.49101300960358,-7.98728057434275,
82.0143089887137));
#169992=CARTESIAN_POINT('Ctrl Pts',(-1.48204526876412,-7.9889494045676,
82.0146646339771));
#169993=CARTESIAN_POINT('Ctrl Pts',(-1.46350828072555,-7.99236671471007,
82.0154004985665));
#169994=CARTESIAN_POINT('Ctrl Pts',(-1.45393866745994,-7.99411311782941,
82.0157807802016));
#169995=CARTESIAN_POINT('Ctrl Pts',(-1.43161806382726,-7.9981451033015,
82.0166686950485));
#169996=CARTESIAN_POINT('Ctrl Pts',(-1.41886471442816,-8.000417382513,82.0171767300198));
#169997=CARTESIAN_POINT('Ctrl Pts',(-1.37884611446021,-8.00744884459757,
82.0187731189416));
#169998=CARTESIAN_POINT('Ctrl Pts',(-1.351562080047,-8.01209919631529,82.0198647579263));
#169999=CARTESIAN_POINT('Ctrl Pts',(-1.07882516095381,-8.05715230755174,
82.0308098872083));
#170000=CARTESIAN_POINT('Ctrl Pts',(-0.831678526566427,-8.08639997640681,
82.0409992817011));
#170001=CARTESIAN_POINT('Ctrl Pts',(-0.200168510864236,-8.13187529847885,
82.0677140292404));
#170002=CARTESIAN_POINT('Ctrl Pts',(0.184704455621429,-8.13223896171834,
82.0846469081139));
#170003=CARTESIAN_POINT('Ctrl Pts',(1.22774153279123,-8.05912905421342,
82.1314375727189));
#170004=CARTESIAN_POINT('Ctrl Pts',(1.87931155853566,-7.93254612609118,
82.1617356762533));
#170005=CARTESIAN_POINT('Ctrl Pts',(2.54579791579657,-7.71622629644003,
82.189999038119));
#170006=CARTESIAN_POINT('Ctrl Pts',(2.58312918384015,-7.7038093812577,82.1915730767375));
#170007=CARTESIAN_POINT('Ctrl Pts',(2.63285733338629,-7.68686697420724,
82.1936593039519));
#170008=CARTESIAN_POINT('Ctrl Pts',(2.64533508307752,-7.68258185235168,
82.1941818907385));
#170009=CARTESIAN_POINT('Ctrl Pts',(2.66480141105156,-7.67584365772699,
82.1949958521376));
#170010=CARTESIAN_POINT('Ctrl Pts',(2.67179713225404,-7.67341139929175,
82.1952881037621));
#170011=CARTESIAN_POINT('Ctrl Pts',(2.68580781571798,-7.66851870980025,
82.195872893064));
#170012=CARTESIAN_POINT('Ctrl Pts',(2.69282274582029,-7.66605821042096,
82.196165427482));
#170013=CARTESIAN_POINT('Ctrl Pts',(2.70864268636155,-7.66048494399679,
82.1968245757013));
#170014=CARTESIAN_POINT('Ctrl Pts',(2.71744573570807,-7.65736661352736,
82.1971909616567));
#170015=CARTESIAN_POINT('Ctrl Pts',(2.7434581876743,-7.64810163886216,82.1982724751819));
#170016=CARTESIAN_POINT('Ctrl Pts',(2.76065231390488,-7.64191208495024,
82.1989858823365));
#170017=CARTESIAN_POINT('Ctrl Pts',(2.89816330922583,-7.59188611192789,
82.2046805553654));
#170018=CARTESIAN_POINT('Ctrl Pts',(3.01745291989317,-7.54526772258471,
82.2095542987271));
#170019=CARTESIAN_POINT('Ctrl Pts',(3.32049265316782,-7.41850294610265,
82.2218630097274));
#170020=CARTESIAN_POINT('Ctrl Pts',(3.50247137403872,-7.33434084950595,
82.2291859021828));
#170021=CARTESIAN_POINT('Ctrl Pts',(4.08780251824189,-7.03687625635104,
82.252945175192));
#170022=CARTESIAN_POINT('Ctrl Pts',(4.4763228269596,-6.79634426738865,82.2690974605615));
#170023=CARTESIAN_POINT('Ctrl Pts',(5.13019258780814,-6.31102835920279,
82.2989079481626));
#170024=CARTESIAN_POINT('Ctrl Pts',(5.4033380341403,-6.07880543496155,82.312310288064));
#170025=CARTESIAN_POINT('Ctrl Pts',(5.69770053235318,-5.79298013793138,
82.3281056855524));
#170026=CARTESIAN_POINT('Ctrl Pts',(5.73478446015894,-5.75627113441738,
82.3301216939825));
#170027=CARTESIAN_POINT('Ctrl Pts',(5.7906725216542,-5.69987195502733,82.3332000600365));
#170028=CARTESIAN_POINT('Ctrl Pts',(5.80973566851486,-5.68044012475289,
82.3342573153322));
#170029=CARTESIAN_POINT('Ctrl Pts',(5.84337091792872,-5.64580793616629,
82.3361356302649));
#170030=CARTESIAN_POINT('Ctrl Pts',(5.85798228876853,-5.63064600527697,
82.3369559478849));
#170031=CARTESIAN_POINT('Ctrl Pts',(5.88857494256762,-5.59865264147786,
82.3386827028612));
#170032=CARTESIAN_POINT('Ctrl Pts',(5.90454339442634,-5.58180916484072,
82.3395893739593));
#170033=CARTESIAN_POINT('Ctrl Pts',(5.94427987994433,-5.53953391110842,
82.3418592316745));
#170034=CARTESIAN_POINT('Ctrl Pts',(5.96795701514219,-5.51401743666631,
82.3432240871158));
#170035=CARTESIAN_POINT('Ctrl Pts',(6.05943343448763,-5.41415532959612,
82.3485466174853));
#170036=CARTESIAN_POINT('Ctrl Pts',(6.12601266472768,-5.33870582326983,
82.3525275336655));
#170037=CARTESIAN_POINT('Ctrl Pts',(6.65123883721597,-4.72073904252836,
82.3848541129689));
#170038=CARTESIAN_POINT('Ctrl Pts',(7.03830096881737,-4.12146893670269,
82.4148973364547));
#170039=CARTESIAN_POINT('Ctrl Pts',(7.4960163322414,-3.15562523039783,82.4601712042922));
#170040=CARTESIAN_POINT('Ctrl Pts',(7.62795014290625,-2.8218131247775,82.4752415196864));
#170041=CARTESIAN_POINT('Ctrl Pts',(7.74453635437266,-2.45812727999125,
82.4904748333208));
#170042=CARTESIAN_POINT('Ctrl Pts',(7.7515702989922,-2.43585528750969,82.491403011818));
#170043=CARTESIAN_POINT('Ctrl Pts',(7.76126912307547,-2.40467784859556,
82.4926954925195));
#170044=CARTESIAN_POINT('Ctrl Pts',(7.76401486746026,-2.39579779928162,
82.4930628479599));
#170045=CARTESIAN_POINT('Ctrl Pts',(7.76900381790987,-2.3795643181103,82.4937329718357));
#170046=CARTESIAN_POINT('Ctrl Pts',(7.77125183462766,-2.37221238299013,
82.4940359260861));
#170047=CARTESIAN_POINT('Ctrl Pts',(7.77576769238533,-2.3573683697006,82.4946465139725));
#170048=CARTESIAN_POINT('Ctrl Pts',(7.77803514828598,-2.34987618162453,
82.4949541322155));
#170049=CARTESIAN_POINT('Ctrl Pts',(7.78355807190093,-2.33153161578746,
82.4957059393094));
#170050=CARTESIAN_POINT('Ctrl Pts',(7.78680167959969,-2.32067566417503,
82.4961496512707));
#170051=CARTESIAN_POINT('Ctrl Pts',(7.79837464934966,-2.2816449294646,82.4977405804065));
#170052=CARTESIAN_POINT('Ctrl Pts',(7.80657395121732,-2.2534315897656,82.498882424986));
#170053=CARTESIAN_POINT('Ctrl Pts',(7.85102631555817,-2.09731871251159,
82.5051534347117));
#170054=CARTESIAN_POINT('Ctrl Pts',(7.88428828445487,-1.96859293647769,
82.5101386823629));
#170055=CARTESIAN_POINT('Ctrl Pts',(8.05410122680693,-1.23782263518701,
82.5375828932488));
#170056=CARTESIAN_POINT('Ctrl Pts',(8.12485328113968,-0.622553316611473,
82.5576087136251));
#170057=CARTESIAN_POINT('Ctrl Pts',(8.12524833638065,-0.0051994849222721,
82.5785614930982));
#170058=CARTESIAN_POINT('',(8.12115743020385,0.00265292485629474,84.5832974432122));
#170059=CARTESIAN_POINT('Ctrl Pts',(8.11704416097363,-0.0053549714695382,
82.5832974432122));
#170060=CARTESIAN_POINT('Ctrl Pts',(8.10035380767694,1.97061005880897,82.6608378090696));
#170061=CARTESIAN_POINT('Ctrl Pts',(6.8826360504109,5.30498188964725,82.7912673300224));
#170062=CARTESIAN_POINT('Ctrl Pts',(2.81786210763212,7.9735377618551,82.9745860060708));
#170063=CARTESIAN_POINT('Ctrl Pts',(-1.31318116064729,8.36857010785244,
83.1332534713571));
#170064=CARTESIAN_POINT('Ctrl Pts',(-5.16809395608702,6.7139926335042,83.2919209366436));
#170065=CARTESIAN_POINT('Ctrl Pts',(-7.73996699874804,3.42788185729169,
83.45058840193));
#170066=CARTESIAN_POINT('Ctrl Pts',(-8.44497665565605,-0.68502664701191,
83.6092558672165));
#170067=CARTESIAN_POINT('Ctrl Pts',(-7.07955773652491,-4.65158818748283,
83.7679233325027));
#170068=CARTESIAN_POINT('Ctrl Pts',(-4.01080233417694,-7.44520758162714,
83.9265907977894));
#170069=CARTESIAN_POINT('Ctrl Pts',(1.42217143211323,-8.84926286475008,
84.138147418171));
#170070=CARTESIAN_POINT('Ctrl Pts',(6.73271600913051,-5.90303377185105,
84.3497040385533));
#170071=CARTESIAN_POINT('Ctrl Pts',(8.06645284195508,-1.72963063830897,
84.5157170985985));
#170072=CARTESIAN_POINT('Ctrl Pts',(8.12089038625466,-0.185607932903464,
84.5759518484531));
#170073=CARTESIAN_POINT('Ctrl Pts',(8.12115743020385,0.00265292485629474,
84.5832974432122));
#170074=CARTESIAN_POINT('',(8.12771990326932,0.00255226563719405,86.5832974432122));
#170075=CARTESIAN_POINT('Ctrl Pts',(8.12115743020385,0.00265292485629474,
84.5832974432122));
#170076=CARTESIAN_POINT('Ctrl Pts',(8.12281313442001,1.16989261279775,84.6288410035486));
#170077=CARTESIAN_POINT('Ctrl Pts',(7.31450585013189,5.04406336557019,84.7801628740762));
#170078=CARTESIAN_POINT('Ctrl Pts',(2.62992883968332,8.56828449165683,84.9843738996985));
#170079=CARTESIAN_POINT('Ctrl Pts',(-2.94483553187362,7.92752136468721,
85.1959305200809));
#170080=CARTESIAN_POINT('Ctrl Pts',(-6.36979470017048,5.58418533793423,
85.354597985367));
#170081=CARTESIAN_POINT('Ctrl Pts',(-8.26960761947702,1.84403959870158,
85.5132654506537));
#170082=CARTESIAN_POINT('Ctrl Pts',(-8.139005581661,-2.3268114042503,85.6719329159399));
#170083=CARTESIAN_POINT('Ctrl Pts',(-6.04529291051799,-5.93644050317469,
85.8306003812265));
#170084=CARTESIAN_POINT('Ctrl Pts',(-2.45563682176731,-8.10723493000542,
85.9892678465127));
#170085=CARTESIAN_POINT('Ctrl Pts',(1.6903925653843,-8.28614652732205,86.1479353117993));
#170086=CARTESIAN_POINT('Ctrl Pts',(6.43672742380675,-6.03729498712186,
86.3459451773656));
#170087=CARTESIAN_POINT('Ctrl Pts',(8.10769023119457,-2.34268520044924,
86.4910658878367));
#170088=CARTESIAN_POINT('Ctrl Pts',(8.12771990326932,0.00255226563719405,
86.5832974432122));
#170089=CARTESIAN_POINT('',(8.12607929659711,-0.000602397288300138,88.5832974432122));
#170090=CARTESIAN_POINT('Ctrl Pts',(8.12771990326932,0.00255226563719405,
86.5832974432122));
#170091=CARTESIAN_POINT('Ctrl Pts',(8.13066181458726,0.347015251300818,
86.5968441980277));
#170092=CARTESIAN_POINT('Ctrl Pts',(8.03485269117909,2.03602439612352,86.6632801079386));
#170093=CARTESIAN_POINT('Ctrl Pts',(6.84908166713345,4.95342653106158,86.782605172945));
#170094=CARTESIAN_POINT('Ctrl Pts',(2.59518421047726,8.5697311209224,86.9941617933268));
#170095=CARTESIAN_POINT('Ctrl Pts',(-3.4701714152711,8.2637724545391,87.2057184137089));
#170096=CARTESIAN_POINT('Ctrl Pts',(-7.34003372474683,4.20018525983518,
87.4172750340907));
#170097=CARTESIAN_POINT('Ctrl Pts',(-8.46845332731791,0.206660721371377,
87.5759424993771));
#170098=CARTESIAN_POINT('Ctrl Pts',(-7.53094626422849,-3.88223396860557,
87.7346099646635));
#170099=CARTESIAN_POINT('Ctrl Pts',(-4.75851708790345,-7.00099837833069,
87.8932774299501));
#170100=CARTESIAN_POINT('Ctrl Pts',(-0.838343829035965,-8.43113704348407,
88.0519448952363));
#170101=CARTESIAN_POINT('Ctrl Pts',(3.30861330952905,-7.79810799993996,
88.2106123605229));
#170102=CARTESIAN_POINT('Ctrl Pts',(6.60661632725936,-5.27923024708605,
88.3692798258093));
#170103=CARTESIAN_POINT('Ctrl Pts',(7.98907354300744,-2.28814380995307,
88.4935081867057));
#170104=CARTESIAN_POINT('Ctrl Pts',(8.13073112681308,-0.470635535525396,
88.5648473925067));
#170105=CARTESIAN_POINT('Ctrl Pts',(8.12607929659711,-0.000602397288300138,
88.5832974432122));
#170106=CARTESIAN_POINT('',(8.12524838875447,-0.00511698572615098,90.5832974432122));
#170107=CARTESIAN_POINT('Ctrl Pts',(8.12524997767401,-0.000602335809762239,
88.5832974432122));
#170108=CARTESIAN_POINT('Ctrl Pts',(8.12526495996985,0.201502365521601,
88.5912314058029));
#170109=CARTESIAN_POINT('Ctrl Pts',(8.11773499501211,0.403761566827383,
88.5991653683936));
#170110=CARTESIAN_POINT('Ctrl Pts',(8.1026516106303,0.605577773081411,88.6070993309843));
#170111=CARTESIAN_POINT('Ctrl Pts',(8.08757794812149,0.80726390033737,88.6150281798037));
#170112=CARTESIAN_POINT('Ctrl Pts',(8.06496059500274,1.00850727033384,88.6229570286232));
#170113=CARTESIAN_POINT('Ctrl Pts',(8.0348431432226,1.20871139082447,88.6308858774427));
#170114=CARTESIAN_POINT('Ctrl Pts',(8.00474001668687,1.40882028503302,88.6388109549372));
#170115=CARTESIAN_POINT('Ctrl Pts',(7.96714395263145,1.60789058619621,88.6467360324317));
#170116=CARTESIAN_POINT('Ctrl Pts',(7.92215032532402,1.8053314890813,88.6546611099263));
#170117=CARTESIAN_POINT('Ctrl Pts',(7.87705752094983,2.00320760047877,88.6626036562489));
#170118=CARTESIAN_POINT('Ctrl Pts',(7.82453454514041,2.1994467879691,88.6705462025715));
#170119=CARTESIAN_POINT('Ctrl Pts',(7.76472901475924,2.39346420275216,88.6784887488941));
#170120=CARTESIAN_POINT('Ctrl Pts',(7.70507301351653,2.58699652432234,88.6864114368173));
#170121=CARTESIAN_POINT('Ctrl Pts',(7.63817094197432,2.77831785387582,88.6943341247405));
#170122=CARTESIAN_POINT('Ctrl Pts',(7.56421939868302,2.9668623916669,88.7022568126636));
#170123=CARTESIAN_POINT('Ctrl Pts',(7.49026357116724,3.1554178523825,88.7101799595708));
#170124=CARTESIAN_POINT('Ctrl Pts',(7.40925757941404,3.34119589022874,88.718103106478));
#170125=CARTESIAN_POINT('Ctrl Pts',(7.3214464610705,3.52364999399462,88.7260262533852));
#170126=CARTESIAN_POINT('Ctrl Pts',(7.23361680925743,3.7061426066377,88.7339510725567));
#170127=CARTESIAN_POINT('Ctrl Pts',(7.13897931252366,3.88530958647883,88.7418758917282));
#170128=CARTESIAN_POINT('Ctrl Pts',(7.03782549592002,4.06062801195555,88.7498007108997));
#170129=CARTESIAN_POINT('Ctrl Pts',(6.93626356518562,4.23665377531849,88.7577575034638));
#170130=CARTESIAN_POINT('Ctrl Pts',(6.82813278577759,4.40879956737382,88.7657142960279));
#170131=CARTESIAN_POINT('Ctrl Pts',(6.71377261423615,4.57656474299585,88.7736710885919));
#170132=CARTESIAN_POINT('Ctrl Pts',(6.5997274412337,4.74386781905558,88.7816059646268));
#170133=CARTESIAN_POINT('Ctrl Pts',(6.47948737991197,4.90681413481764,88.7895408406618));
#170134=CARTESIAN_POINT('Ctrl Pts',(6.35343012263957,5.0649396086465,88.7974757166967));
#170135=CARTESIAN_POINT('Ctrl Pts',(6.22685060058172,5.22372020831619,88.8054434675254));
#170136=CARTESIAN_POINT('Ctrl Pts',(6.09440579693078,5.37763967607004,88.813411218354));
#170137=CARTESIAN_POINT('Ctrl Pts',(5.95651623194406,5.52626473678984,88.8213789691827));
#170138=CARTESIAN_POINT('Ctrl Pts',(5.81862666695735,5.67488979750964,88.8293467200114));
#170139=CARTESIAN_POINT('Ctrl Pts',(5.67529260705918,5.81822024134434,88.83731447084));
#170140=CARTESIAN_POINT('Ctrl Pts',(5.52696893801207,5.95586281916816,88.8452822216686));
#170141=CARTESIAN_POINT('Ctrl Pts',(5.37659388168858,6.09540905966868,88.8533601703017));
#170142=CARTESIAN_POINT('Ctrl Pts',(5.22076204191132,6.229413831033,88.8614381189348));
#170143=CARTESIAN_POINT('Ctrl Pts',(5.0599057357018,6.35743985487177,88.8695160675679));
#170144=CARTESIAN_POINT('Ctrl Pts',(4.89924628494258,6.48530920085832,88.8775841304324));
#170145=CARTESIAN_POINT('Ctrl Pts',(4.73357486969886,6.60721418909075,88.8856521932968));
#170146=CARTESIAN_POINT('Ctrl Pts',(4.56335985174343,6.72275497292562,88.8937202561613));
#170147=CARTESIAN_POINT('Ctrl Pts',(4.39333218677518,6.83816858284098,88.9017794386362));
#170148=CARTESIAN_POINT('Ctrl Pts',(4.21877114854755,6.94723177676903,88.9098386211111));
#170149=CARTESIAN_POINT('Ctrl Pts',(4.04017779458328,7.04958516160037,88.917897803586));
#170150=CARTESIAN_POINT('Ctrl Pts',(3.86181383753915,7.15180707708683,88.9259466343227));
#170151=CARTESIAN_POINT('Ctrl Pts',(3.67942817004831,7.24733622083707,88.9339954650594));
#170152=CARTESIAN_POINT('Ctrl Pts',(3.49355044913783,7.33585665221376,88.9420442957961));
#170153=CARTESIAN_POINT('Ctrl Pts',(3.30781332529625,7.4243101271358,88.9500870384336));
#170154=CARTESIAN_POINT('Ctrl Pts',(3.11858969677777,7.50576532146182,88.958129781071));
#170155=CARTESIAN_POINT('Ctrl Pts',(2.92643461789832,7.57995171420414,88.9661725237085));
#170156=CARTESIAN_POINT('Ctrl Pts',(2.73443605656447,7.65407767933676,88.9742087152293));
#170157=CARTESIAN_POINT('Ctrl Pts',(2.5395111015908,7.72094653995816,88.9822449067502));
#170158=CARTESIAN_POINT('Ctrl Pts',(2.34223588471881,7.78033537984292,88.990281098271));
#170159=CARTESIAN_POINT('Ctrl Pts',(2.23038879936087,7.81400645494918,88.994837294499));
#170160=CARTESIAN_POINT('Ctrl Pts',(2.11778662314369,7.84527399401388,88.9993934907269));
#170161=CARTESIAN_POINT('Ctrl Pts',(2.00453702288502,7.8741043228029,89.0039496869549));
#170162=CARTESIAN_POINT('Ctrl Pts',(1.80478003041979,7.92495712720595,89.0119862014635));
#170163=CARTESIAN_POINT('Ctrl Pts',(1.60316595060972,7.96818418802857,89.0200227159722));
#170164=CARTESIAN_POINT('Ctrl Pts',(1.4003037910848,8.00367645867657,89.0280592304809));
#170165=CARTESIAN_POINT('Ctrl Pts',(1.19731908262425,8.03919017018866,89.0361005998442));
#170166=CARTESIAN_POINT('Ctrl Pts',(0.993085101348456,8.06695971503978,
89.0441419692075));
#170167=CARTESIAN_POINT('Ctrl Pts',(0.788217396409137,8.08692777873637,
89.0521833385708));
#170168=CARTESIAN_POINT('Ctrl Pts',(0.583200882053333,8.10691034660242,
89.0602305489303));
#170169=CARTESIAN_POINT('Ctrl Pts',(0.377550039657457,8.11908009699181,
89.0682777592898));
#170170=CARTESIAN_POINT('Ctrl Pts',(0.17188245807031,8.12343178608079,89.0763249696493));
#170171=CARTESIAN_POINT('Ctrl Pts',(-0.034088262845772,8.12778988924874,
89.0843840410223));
#170172=CARTESIAN_POINT('Ctrl Pts',(-0.240075456148502,8.12430689334256,
89.0924431123952));
#170173=CARTESIAN_POINT('Ctrl Pts',(-0.445462854899655,8.11302966883547,
89.1005021837682));
#170174=CARTESIAN_POINT('Ctrl Pts',(-0.651016483748779,8.10174331711734,
89.1085677777429));
#170175=CARTESIAN_POINT('Ctrl Pts',(-0.855969035467893,8.08265017736779,
89.1166333717177));
#170176=CARTESIAN_POINT('Ctrl Pts',(-1.05971152068651,8.05584874829613,
89.1246989656925));
#170177=CARTESIAN_POINT('Ctrl Pts',(-1.26377392815683,8.02900523485739,
89.1327772244926));
#170178=CARTESIAN_POINT('Ctrl Pts',(-1.46662216008448,7.99442929154823,
89.1408554832927));
#170179=CARTESIAN_POINT('Ctrl Pts',(-1.66765779420039,7.95227043327518,
89.1489337420928));
#170180=CARTESIAN_POINT('Ctrl Pts',(-1.78116629086201,7.92846674969148,
89.153494878809));
#170181=CARTESIAN_POINT('Ctrl Pts',(-1.89409721064808,7.90224658368573,
89.1580560155253));
#170182=CARTESIAN_POINT('Ctrl Pts',(-2.006345280416,7.87364376754832,89.1626171522415));
#170183=CARTESIAN_POINT('Ctrl Pts',(-2.20534384035217,7.82293537467142,
89.1707033459737));
#170184=CARTESIAN_POINT('Ctrl Pts',(-2.40258246267606,7.76463687978641,
89.1787895397059));
#170185=CARTESIAN_POINT('Ctrl Pts',(-2.59746170664314,7.69888824733951,
89.1868757334381));
#170186=CARTESIAN_POINT('Ctrl Pts',(-2.79216712757233,7.63319825955275,
89.1949547146692));
#170187=CARTESIAN_POINT('Ctrl Pts',(-2.98451706749501,7.56007148483361,
89.2030336959002));
#170188=CARTESIAN_POINT('Ctrl Pts',(-3.17392548419789,7.47969816124014,
89.2111126771313));
#170189=CARTESIAN_POINT('Ctrl Pts',(-3.36319082230855,7.39938555143222,
89.2191855555224));
#170190=CARTESIAN_POINT('Ctrl Pts',(-3.5495187775071,7.31183743171238,89.2272584339135));
#170191=CARTESIAN_POINT('Ctrl Pts',(-3.73234100480123,7.2172929957415,89.2353313123046));
#170192=CARTESIAN_POINT('Ctrl Pts',(-3.91505005696813,7.12280708700075,
89.2433991932233));
#170193=CARTESIAN_POINT('Ctrl Pts',(-4.09425742853882,7.02133364442052,
89.251467074142));
#170194=CARTESIAN_POINT('Ctrl Pts',(-4.26941663867616,6.9131591279165,89.2595349550606));
#170195=CARTESIAN_POINT('Ctrl Pts',(-4.4444912714021,6.80503684458125,89.2675989403207));
#170196=CARTESIAN_POINT('Ctrl Pts',(-4.61552137226379,6.69022010702722,
89.2756629255808));
#170197=CARTESIAN_POINT('Ctrl Pts',(-4.78198632770572,6.56904059388702,
89.2837269108408));
#170198=CARTESIAN_POINT('Ctrl Pts',(-4.95076461296472,6.44617707356212,
89.2919029596731));
#170199=CARTESIAN_POINT('Ctrl Pts',(-5.11484964076951,6.31677278271794,
89.3000790085053));
#170200=CARTESIAN_POINT('Ctrl Pts',(-5.27372942165282,6.18121877542717,
89.3082550573375));
#170201=CARTESIAN_POINT('Ctrl Pts',(-5.43035730136214,6.0475860587277,89.3163152219845));
#170202=CARTESIAN_POINT('Ctrl Pts',(-5.58192627019638,5.90797701751488,
89.3243753866314));
#170203=CARTESIAN_POINT('Ctrl Pts',(-5.72797903344587,5.76280693368297,
89.3324355512784));
#170204=CARTESIAN_POINT('Ctrl Pts',(-5.87402474015856,5.61764386374121,
89.3404953264986));
#170205=CARTESIAN_POINT('Ctrl Pts',(-6.01455454827871,5.46692051044645,
89.3485551017189));
#170206=CARTESIAN_POINT('Ctrl Pts',(-6.14914778483428,5.31108925577114,
89.3566148769391));
#170207=CARTESIAN_POINT('Ctrl Pts',(-6.28375118335059,5.15524623563768,
89.3646752606826));
#170208=CARTESIAN_POINT('Ctrl Pts',(-6.41241690972039,4.99429478505011,
89.3727356444262));
#170209=CARTESIAN_POINT('Ctrl Pts',(-6.53476398694848,4.82872107264244,
89.3807960281697));
#170210=CARTESIAN_POINT('Ctrl Pts',(-6.66018660805889,4.65898519118419,
89.3890590327234));
#170211=CARTESIAN_POINT('Ctrl Pts',(-6.77896852738852,4.48439189149325,
89.3973220372771));
#170212=CARTESIAN_POINT('Ctrl Pts',(-6.89074586973728,4.30549752307425,
89.4055850418309));
#170213=CARTESIAN_POINT('Ctrl Pts',(-6.99987193428575,4.13084639982123,
89.4136520538867));
#170214=CARTESIAN_POINT('Ctrl Pts',(-7.10232179584241,3.95209621931569,
89.4217190659425));
#170215=CARTESIAN_POINT('Ctrl Pts',(-7.19780274954632,3.76979086172209,
89.4297860779983));
#170216=CARTESIAN_POINT('Ctrl Pts',(-7.29676334673353,3.58084169062526,
89.4381470788009));
#170217=CARTESIAN_POINT('Ctrl Pts',(-7.38823738479246,3.38807368363205,
89.4465080796036));
#170218=CARTESIAN_POINT('Ctrl Pts',(-7.4719527634726,3.19211676837395,89.4548690804063));
#170219=CARTESIAN_POINT('Ctrl Pts',(-7.55566814215268,2.99615985311599,
89.4632300812089));
#170220=CARTESIAN_POINT('Ctrl Pts',(-7.63162474954995,2.7970143905052,89.4715910820116));
#170221=CARTESIAN_POINT('Ctrl Pts',(-7.69960716223356,2.59532986531225,
89.4799520828143));
#170222=CARTESIAN_POINT('Ctrl Pts',(-7.76122506893775,2.41252702312928,
89.4875303276438));
#170223=CARTESIAN_POINT('Ctrl Pts',(-7.81641525518899,2.22727186671854,
89.4951085724732));
#170224=CARTESIAN_POINT('Ctrl Pts',(-7.86497144648169,2.04007639771841,
89.5026868173026));
#170225=CARTESIAN_POINT('Ctrl Pts',(-7.913491505836,1.85302022578778,89.5102594229609));
#170226=CARTESIAN_POINT('Ctrl Pts',(-7.95538729909704,1.66402696692475,
89.5178320286192));
#170227=CARTESIAN_POINT('Ctrl Pts',(-7.99050135741784,1.47362668936324,
89.5254046342774));
#170228=CARTESIAN_POINT('Ctrl Pts',(-8.02559595451032,1.28333193715117,
89.5329730429782));
#170229=CARTESIAN_POINT('Ctrl Pts',(-8.05391622939255,1.09163207813576,
89.5405414516791));
#170230=CARTESIAN_POINT('Ctrl Pts',(-8.07535510965074,0.899070306226197,
89.5481098603799));
#170231=CARTESIAN_POINT('Ctrl Pts',(-8.09678881010417,0.706555058779329,
89.5556764404927));
#170232=CARTESIAN_POINT('Ctrl Pts',(-8.11134437658088,0.513178676856518,
89.5632430206055));
#170233=CARTESIAN_POINT('Ctrl Pts',(-8.11896619276522,0.319492602786696,
89.5708096007183));
#170234=CARTESIAN_POINT('Ctrl Pts',(-8.12658665687383,0.125840887750647,
89.5783748385541));
#170235=CARTESIAN_POINT('Ctrl Pts',(-8.12727580763376,-0.0681200425285449,
89.5859400763897));
#170236=CARTESIAN_POINT('Ctrl Pts',(-8.12103007872434,-0.261835870259456,
89.5935053142255));
#170237=CARTESIAN_POINT('Ctrl Pts',(-8.11478217787525,-0.455619062280116,
89.6010731828574));
#170238=CARTESIAN_POINT('Ctrl Pts',(-8.10159458808534,-0.64915661338977,
89.6086410514894));
#170239=CARTESIAN_POINT('Ctrl Pts',(-8.08151586847249,-0.841895973459506,
89.6162089201214));
#170240=CARTESIAN_POINT('Ctrl Pts',(-8.06169625401975,-1.03214813495714,
89.6236791294478));
#170241=CARTESIAN_POINT('Ctrl Pts',(-8.03516237914344,-1.22162224219535,
89.6311493387742));
#170242=CARTESIAN_POINT('Ctrl Pts',(-8.00201021732005,-1.40979432698729,
89.6386195481007));
#170243=CARTESIAN_POINT('Ctrl Pts',(-7.96071167427457,-1.64420537339614,
89.6479253895438));
#170244=CARTESIAN_POINT('Ctrl Pts',(-7.90916508289916,-1.8764811682522,
89.657231230987));
#170245=CARTESIAN_POINT('Ctrl Pts',(-7.8476229482722,-2.10582563956553,
89.6665370724301));
#170246=CARTESIAN_POINT('Ctrl Pts',(-7.78575040634027,-2.33640141507615,
89.6758928750586));
#170247=CARTESIAN_POINT('Ctrl Pts',(-7.71377476869098,-2.56401427705064,
89.685248677687));
#170248=CARTESIAN_POINT('Ctrl Pts',(-7.63199944735815,-2.78787948054159,
89.6946044803154));
#170249=CARTESIAN_POINT('Ctrl Pts',(-7.54982715139329,-3.01283142762868,
89.7040057002684));
#170250=CARTESIAN_POINT('Ctrl Pts',(-7.45775983349303,-3.23399921083646,
89.7134069202213));
#170251=CARTESIAN_POINT('Ctrl Pts',(-7.35615172633996,-3.45061144459437,
89.7228081401743));
#170252=CARTESIAN_POINT('Ctrl Pts',(-7.25443364906327,-3.66745811706775,
89.7322195350369));
#170253=CARTESIAN_POINT('Ctrl Pts',(-7.14315415404235,-3.87973934917524,
89.7416309298996));
#170254=CARTESIAN_POINT('Ctrl Pts',(-7.02271441312066,-4.08670647762319,
89.7510423247623));
#170255=CARTESIAN_POINT('Ctrl Pts',(-6.90241595003536,-4.29343083015775,
89.760442679901));
#170256=CARTESIAN_POINT('Ctrl Pts',(-6.77297874069724,-4.49485350946098,
89.7698430350397));
#170257=CARTESIAN_POINT('Ctrl Pts',(-6.63484775525196,-4.69025402586342,
89.7792433901783));
#170258=CARTESIAN_POINT('Ctrl Pts',(-6.54646870225914,-4.81527530576154,
89.785257931248));
#170259=CARTESIAN_POINT('Ctrl Pts',(-6.45453158198816,-4.93783180441181,
89.7912724723176));
#170260=CARTESIAN_POINT('Ctrl Pts',(-6.35916264071753,-5.05774041162676,
89.7972870133872));
#170261=CARTESIAN_POINT('Ctrl Pts',(-6.23639769419285,-5.21209437169454,
89.8050293119065));
#170262=CARTESIAN_POINT('Ctrl Pts',(-6.10788593933289,-5.36213122049771,
89.8127716104258));
#170263=CARTESIAN_POINT('Ctrl Pts',(-5.97396991466535,-5.50739239760281,
89.8205139089451));
#170264=CARTESIAN_POINT('Ctrl Pts',(-5.84013730755455,-5.65256309014855,
89.8282513847135));
#170265=CARTESIAN_POINT('Ctrl Pts',(-5.70090737190607,-5.79296377552294,
89.8359888604819));
#170266=CARTESIAN_POINT('Ctrl Pts',(-5.55666336760916,-5.92816833276269,
89.8437263362503));
#170267=CARTESIAN_POINT('Ctrl Pts',(-5.41248357795749,-6.06331269954447,
89.8514603674439));
#170268=CARTESIAN_POINT('Ctrl Pts',(-5.26329442247845,-6.19326530414008,
89.8591943986375));
#170269=CARTESIAN_POINT('Ctrl Pts',(-5.10951661184736,-6.31763623167367,
89.8669284298311));
#170270=CARTESIAN_POINT('Ctrl Pts',(-4.95575847993428,-6.4419912436444,
89.8746614713122));
#170271=CARTESIAN_POINT('Ctrl Pts',(-4.79741313216581,-6.5607657732854,
89.8823945127933));
#170272=CARTESIAN_POINT('Ctrl Pts',(-4.63493529650067,-6.67360939520379,
89.8901275542745));
#170273=CARTESIAN_POINT('Ctrl Pts',(-4.47247369224984,-6.78644174412871,
89.8978598232305));
#170274=CARTESIAN_POINT('Ctrl Pts',(-4.30588071473477,-6.89334416688666,
89.9055920921866));
#170275=CARTESIAN_POINT('Ctrl Pts',(-4.13564097227291,-6.99400895845563,
89.9133243611426));
#170276=CARTESIAN_POINT('Ctrl Pts',(-3.96533574632521,-7.09471247119134,
89.9210596043509));
#170277=CARTESIAN_POINT('Ctrl Pts',(-3.79138125728361,-7.18917337900908,
89.9287948475591));
#170278=CARTESIAN_POINT('Ctrl Pts',(-3.61428823618453,-7.27712911169495,
89.9365300907673));
#170279=CARTESIAN_POINT('Ctrl Pts',(-3.46605227924917,-7.35075257873911,
89.943004886736));
#170280=CARTESIAN_POINT('Ctrl Pts',(-3.31561783853691,-7.41981892123465,
89.9494796827047));
#170281=CARTESIAN_POINT('Ctrl Pts',(-3.16329578184691,-7.48419984761561,
89.9559544786735));
#170282=CARTESIAN_POINT('Ctrl Pts',(-2.96535145435842,-7.56786362850521,
89.9643685531779));
#170283=CARTESIAN_POINT('Ctrl Pts',(-2.76412378459261,-7.64365462963771,
89.9727826276823));
#170284=CARTESIAN_POINT('Ctrl Pts',(-2.56024420095133,-7.71134470724757,
89.9811967021867));
#170285=CARTESIAN_POINT('Ctrl Pts',(-2.35630767935196,-7.77905368883365,
89.9896131265106));
#170286=CARTESIAN_POINT('Ctrl Pts',(-2.14971801597115,-7.83865714726906,
89.9980295508345));
#170287=CARTESIAN_POINT('Ctrl Pts',(-1.94112231701676,-7.8899766611112,
90.0064459751584));
#170288=CARTESIAN_POINT('Ctrl Pts',(-1.7324748877817,-7.94130890183539,
90.0148644866969));
#170289=CARTESIAN_POINT('Ctrl Pts',(-1.5218206860995,-7.98435303358087,
90.0232829982354));
#170290=CARTESIAN_POINT('Ctrl Pts',(-1.30981861315874,-8.01898140433827,
90.0317015097739));
#170291=CARTESIAN_POINT('Ctrl Pts',(-1.0977351111085,-8.05362307570802,
90.0401232548275));
#170292=CARTESIAN_POINT('Ctrl Pts',(-0.88430296362602,-8.07984248270811,
90.0485449998811));
#170293=CARTESIAN_POINT('Ctrl Pts',(-0.670189252137193,-8.0975634563009,
90.0569667449347));
#170294=CARTESIAN_POINT('Ctrl Pts',(-0.456052331306254,-8.11528635079887,
90.0653894028824));
#170295=CARTESIAN_POINT('Ctrl Pts',(-0.241233962254784,-8.12450895384322,
90.0738120608302));
#170296=CARTESIAN_POINT('Ctrl Pts',(-0.0264049238957141,-8.12520709536034,
90.082234718778));
#170297=CARTESIAN_POINT('Ctrl Pts',(0.188464968764381,-8.12590536964389,
90.0906589784729));
#170298=CARTESIAN_POINT('Ctrl Pts',(0.403345270857372,-8.11807594302261,
90.0990832381678));
#170299=CARTESIAN_POINT('Ctrl Pts',(0.617565297220088,-8.10174676635659,
90.1075074978628));
#170300=CARTESIAN_POINT('Ctrl Pts',(0.67786958055097,-8.09715000053153,
90.1098789798952));
#170301=CARTESIAN_POINT('Ctrl Pts',(0.738121556086772,-8.09187998194235,
90.1122504619276));
#170302=CARTESIAN_POINT('Ctrl Pts',(0.798306313214766,-8.08593807747632,
90.1146219439599));
#170303=CARTESIAN_POINT('Ctrl Pts',(1.01210340735999,-8.0648303756404,90.1230462691801));
#170304=CARTESIAN_POINT('Ctrl Pts',(1.22507388350962,-8.03523788305068,
90.1314705944002));
#170305=CARTESIAN_POINT('Ctrl Pts',(1.43655248997595,-7.9972498089058,90.1398949196204));
#170306=CARTESIAN_POINT('Ctrl Pts',(1.64799455035247,-7.95926829956477,
90.1483177890141));
#170307=CARTESIAN_POINT('Ctrl Pts',(1.85794499633917,-7.91289415311656,
90.1567406584078));
#170308=CARTESIAN_POINT('Ctrl Pts',(2.06574754580753,-7.85826791599079,
90.1651635278016));
#170309=CARTESIAN_POINT('Ctrl Pts',(2.27350763047813,-7.80365284182772,
90.1735846759679));
#170310=CARTESIAN_POINT('Ctrl Pts',(2.47912044003013,-7.7407891115347,90.1820058241342));
#170311=CARTESIAN_POINT('Ctrl Pts',(2.68194259170222,-7.66986776270058,
90.1904269723005));
#170312=CARTESIAN_POINT('Ctrl Pts',(2.88470783832014,-7.59896631200462,
90.1988457577767));
#170313=CARTESIAN_POINT('Ctrl Pts',(3.0846837418909,-7.5200118450343,90.2072645432528));
#170314=CARTESIAN_POINT('Ctrl Pts',(3.28124375652037,-7.4332447136359,90.215683328729));
#170315=CARTESIAN_POINT('Ctrl Pts',(3.4777488634247,-7.34650182005521,90.2240997624738));
#170316=CARTESIAN_POINT('Ctrl Pts',(3.67083974529905,-7.25195072597193,
90.2325161962186));
#170317=CARTESIAN_POINT('Ctrl Pts',(3.85991038308934,-7.1498796771008,90.2409326299634));
#170318=CARTESIAN_POINT('Ctrl Pts',(4.04891239923137,-7.04784567408563,
90.2493460090321));
#170319=CARTESIAN_POINT('Ctrl Pts',(4.23389685306091,-6.93829729192304,
90.2577593881008));
#170320=CARTESIAN_POINT('Ctrl Pts',(4.41428197581336,-6.82156889582663,
90.2661727671695));
#170321=CARTESIAN_POINT('Ctrl Pts',(4.46514288612388,-6.78865646716311,
90.2685449811952));
#170322=CARTESIAN_POINT('Ctrl Pts',(4.51563830569596,-6.75517350489252,
90.2709171952209));
#170323=CARTESIAN_POINT('Ctrl Pts',(4.56575557235752,-6.72112815054037,
90.2732894092466));
#170324=CARTESIAN_POINT('Ctrl Pts',(4.72917519665905,-6.61011493317934,
90.2810245941572));
#170325=CARTESIAN_POINT('Ctrl Pts',(4.8886444317497,-6.49306945181757,90.2887597790678));
#170326=CARTESIAN_POINT('Ctrl Pts',(5.0436885650882,-6.37031343191986,90.2964949639785));
#170327=CARTESIAN_POINT('Ctrl Pts',(5.19868475495004,-6.24759537121639,
90.3042277569788));
#170328=CARTESIAN_POINT('Ctrl Pts',(5.34925829135822,-6.11917050754268,
90.3119605499792));
#170329=CARTESIAN_POINT('Ctrl Pts',(5.49496532201888,-5.98540254889426,
90.3196933429795));
#170330=CARTESIAN_POINT('Ctrl Pts',(5.64065318438487,-5.85165218791176,
90.3274251187026));
#170331=CARTESIAN_POINT('Ctrl Pts',(5.78147555653655,-5.7125603714665,90.3351568944257));
#170332=CARTESIAN_POINT('Ctrl Pts',(5.91702332769113,-5.56852965351348,
90.3428886701488));
#170333=CARTESIAN_POINT('Ctrl Pts',(6.05261960154003,-5.42444739743612,
90.3506232125123));
#170334=CARTESIAN_POINT('Ctrl Pts',(6.18293725807404,-5.27542296363728,
90.3583577548759));
#170335=CARTESIAN_POINT('Ctrl Pts',(6.30760514129895,-5.12189466349701,
90.3660922972394));
#170336=CARTESIAN_POINT('Ctrl Pts',(6.43229407953972,-4.96834043413813,
90.373828145881));
#170337=CARTESIAN_POINT('Ctrl Pts',(6.55133112635587,-4.81028110195774,
90.3815639945225));
#170338=CARTESIAN_POINT('Ctrl Pts',(6.66438671824976,-4.64818644549853,
90.3892998431641));
#170339=CARTESIAN_POINT('Ctrl Pts',(6.77753481734768,-4.48595915585234,
90.3970420216272));
#170340=CARTESIAN_POINT('Ctrl Pts',(6.88469148693914,-4.31969023923898,
90.4047842000904));
#170341=CARTESIAN_POINT('Ctrl Pts',(6.98557114769636,-4.14987750457434,
90.4125263785536));
#170342=CARTESIAN_POINT('Ctrl Pts',(7.06996349506373,-4.00781819168956,
90.4190032105467));
#170343=CARTESIAN_POINT('Ctrl Pts',(7.14996368609586,-3.86327933956513,
90.4254800425397));
#170344=CARTESIAN_POINT('Ctrl Pts',(7.22542984209037,-3.71656442962179,
90.4319568745328));
#170345=CARTESIAN_POINT('Ctrl Pts',(7.33517417439504,-3.50320879200267,
90.4413756079129));
#170346=CARTESIAN_POINT('Ctrl Pts',(7.43539163973831,-3.28513213101952,
90.4507943412929));
#170347=CARTESIAN_POINT('Ctrl Pts',(7.52575430349025,-3.06312091272904,
90.460213074673));
#170348=CARTESIAN_POINT('Ctrl Pts',(7.61625700988186,-2.84076562493291,
90.4696464050584));
#170349=CARTESIAN_POINT('Ctrl Pts',(7.69687434893898,-2.61446360933155,
90.4790797354438));
#170350=CARTESIAN_POINT('Ctrl Pts',(7.76732641855281,-2.38502156597202,
90.4885130658292));
#170351=CARTESIAN_POINT('Ctrl Pts',(7.83768238437844,-2.15589250489473,
90.4979335281926));
#170352=CARTESIAN_POINT('Ctrl Pts',(7.89790079023532,-1.92363200655743,
90.5073539905559));
#170353=CARTESIAN_POINT('Ctrl Pts',(7.9477522333787,-1.68905950141607,90.5167744529193));
#170354=CARTESIAN_POINT('Ctrl Pts',(7.99747776005718,-1.45507948745949,
90.5261711207595));
#170355=CARTESIAN_POINT('Ctrl Pts',(8.03688860001431,-1.21879915749754,
90.5355677885996));
#170356=CARTESIAN_POINT('Ctrl Pts',(8.06580645547962,-0.981047290013701,
90.5449644564398));
#170357=CARTESIAN_POINT('Ctrl Pts',(8.0945474977085,-0.744749115291,90.5543036699762));
#170358=CARTESIAN_POINT('Ctrl Pts',(8.1129234469417,-0.506997377249942,
90.5636428835126));
#170359=CARTESIAN_POINT('Ctrl Pts',(8.12080848834577,-0.268620658385211,
90.572982097049));
#170360=CARTESIAN_POINT('Ctrl Pts',(8.12371154976798,-0.180856723990185,
90.5764205457701));
#170361=CARTESIAN_POINT('Ctrl Pts',(8.1251930380562,-0.0930082162133875,
90.5798589944911));
#170362=CARTESIAN_POINT('Ctrl Pts',(8.12524838875447,-0.00511698572615098,
90.5832974432122));
#170363=CARTESIAN_POINT('',(8.12456002707784,-1.23182048087155E-6,94.5833205544621));
#170364=CARTESIAN_POINT('Ctrl Pts',(8.12524954479919,-0.0027197868477638,
90.5813566725845));
#170365=CARTESIAN_POINT('Ctrl Pts',(8.1253341132248,0.249924850446765,90.5913649253526));
#170366=CARTESIAN_POINT('Ctrl Pts',(8.11363502343688,0.502437433370498,
90.601402458627));
#170367=CARTESIAN_POINT('Ctrl Pts',(8.03690933001179,1.32569002632119,90.6346645596573));
#170368=CARTESIAN_POINT('Ctrl Pts',(7.923182466773,1.89009932151999,90.6585382981442));
#170369=CARTESIAN_POINT('Ctrl Pts',(7.6411133025716,2.78694483841881,90.6983243100367));
#170370=CARTESIAN_POINT('Ctrl Pts',(7.50782069243921,3.12830785446595,90.7138877135595));
#170371=CARTESIAN_POINT('Ctrl Pts',(7.29973112944332,3.57052705183164,90.7339426923139));
#170372=CARTESIAN_POINT('Ctrl Pts',(7.24498821827151,3.68033766262184,90.7389102610915));
#170373=CARTESIAN_POINT('Ctrl Pts',(7.17962776501885,3.80433150999515,90.7444728201965));
#170374=CARTESIAN_POINT('Ctrl Pts',(7.17142719911711,3.81976766514242,90.7451644655121));
#170375=CARTESIAN_POINT('Ctrl Pts',(7.15896184904297,3.84304990214713,90.7462062567885));
#170376=CARTESIAN_POINT('Ctrl Pts',(7.15473386303412,3.85091556079698,90.7465579706063));
#170377=CARTESIAN_POINT('Ctrl Pts',(7.14711772963658,3.86502861957716,90.7471885769062));
#170378=CARTESIAN_POINT('Ctrl Pts',(7.14373433955709,3.87127856885769,90.7474676774264));
#170379=CARTESIAN_POINT('Ctrl Pts',(7.13696424036494,3.88374550075098,90.7480240693077));
#170380=CARTESIAN_POINT('Ctrl Pts',(7.13357759750108,3.88996251185891,90.7483013632416));
#170381=CARTESIAN_POINT('Ctrl Pts',(7.12413718504379,3.90723890858877,90.7490714495883));
#170382=CARTESIAN_POINT('Ctrl Pts',(7.11806577763847,3.91828867079501,90.7495634354094));
#170383=CARTESIAN_POINT('Ctrl Pts',(7.09380107622702,3.96220711141761,90.7515165500079));
#170384=CARTESIAN_POINT('Ctrl Pts',(7.07540544518844,3.99496392408681,90.7529680782763));
#170385=CARTESIAN_POINT('Ctrl Pts',(6.76178965406594,4.54445315268577,90.777213370273));
#170386=CARTESIAN_POINT('Ctrl Pts',(6.41088085549522,5.02738108313936,90.7969013446664));
#170387=CARTESIAN_POINT('Ctrl Pts',(5.88196255633283,5.6087974189636,90.8231089847327));
#170388=CARTESIAN_POINT('Ctrl Pts',(5.74863875813143,5.7453671278114,90.8294731843692));
#170389=CARTESIAN_POINT('Ctrl Pts',(5.56641321698683,5.91933010160226,90.8379905597227));
#170390=CARTESIAN_POINT('Ctrl Pts',(5.52171914664393,5.96104374585259,90.8400658609274));
#170391=CARTESIAN_POINT('Ctrl Pts',(5.41051971561242,6.06250408925557,90.8452025798158));
#170392=CARTESIAN_POINT('Ctrl Pts',(5.34349136499075,6.1216647359328,90.8482760030133));
#170393=CARTESIAN_POINT('Ctrl Pts',(4.97394466046285,6.43713991054958,90.8651409216937));
#170394=CARTESIAN_POINT('Ctrl Pts',(4.65397725346166,6.67213241189768,90.8794910127026));
#170395=CARTESIAN_POINT('Ctrl Pts',(4.29349658268906,6.89829123204522,90.8958772392701));
#170396=CARTESIAN_POINT('Ctrl Pts',(4.2687568338003,6.91362783932175,90.8970026878825));
#170397=CARTESIAN_POINT('Ctrl Pts',(4.23279002248889,6.93565764787437,90.8986402446615));
#170398=CARTESIAN_POINT('Ctrl Pts',(4.22162826115478,6.94245728872055,90.8991486260085));
#170399=CARTESIAN_POINT('Ctrl Pts',(4.20211435843275,6.95428051455824,90.9000377633864));
#170400=CARTESIAN_POINT('Ctrl Pts',(4.19376948038085,6.95931606561452,90.9004181012211));
#170401=CARTESIAN_POINT('Ctrl Pts',(4.17762406492428,6.96901911092718,90.9011541834696));
#170402=CARTESIAN_POINT('Ctrl Pts',(4.16982471262103,6.97368855496806,90.9015098593127));
#170403=CARTESIAN_POINT('Ctrl Pts',(4.15130418282547,6.98473455102278,90.9023546910264));
#170404=CARTESIAN_POINT('Ctrl Pts',(4.14057613918752,6.99109951298861,90.9028442476185));
#170405=CARTESIAN_POINT('Ctrl Pts',(4.10276776302586,7.01341371716648,90.9045702439637));
#170406=CARTESIAN_POINT('Ctrl Pts',(4.07560975381132,7.0292304267962,90.9058112527841));
#170407=CARTESIAN_POINT('Ctrl Pts',(3.68832818576379,7.25178262342136,90.9235265820499));
#170408=CARTESIAN_POINT('Ctrl Pts',(3.31300405911257,7.43075094818757,90.9409603055985));
#170409=CARTESIAN_POINT('Ctrl Pts',(2.68939320859586,7.6714405464906,90.9701381901769));
#170410=CARTESIAN_POINT('Ctrl Pts',(2.4489789701589,7.75153729684824,90.9814236896893));
#170411=CARTESIAN_POINT('Ctrl Pts',(1.82282870582047,7.92810425647376,91.0106025659424));
#170412=CARTESIAN_POINT('Ctrl Pts',(1.4330313100301,8.00774480003751,91.0285780583772));
#170413=CARTESIAN_POINT('Ctrl Pts',(0.818017106523038,8.08703690328912,
91.0554835865656));
#170414=CARTESIAN_POINT('Ctrl Pts',(0.595965502406689,8.10642737210059,
91.0648991635527));
#170415=CARTESIAN_POINT('Ctrl Pts',(0.333886051134797,8.11848324648465,
91.0754779988639));
#170416=CARTESIAN_POINT('Ctrl Pts',(0.294385398168833,8.12001154150007,
91.0770590146964));
#170417=CARTESIAN_POINT('Ctrl Pts',(0.242161967235993,8.12165050444959,
91.0791331229897));
#170418=CARTESIAN_POINT('Ctrl Pts',(0.229448284910972,8.12201962702541,
91.0796367964425));
#170419=CARTESIAN_POINT('Ctrl Pts',(0.208609968997774,8.1225756682221,91.0804603351901));
#170420=CARTESIAN_POINT('Ctrl Pts',(0.200485857461575,8.12278025227411,
91.080780903893));
#170421=CARTESIAN_POINT('Ctrl Pts',(0.184767936849336,8.12315247090342,
91.0814001699404));
#170422=CARTESIAN_POINT('Ctrl Pts',(0.177174175211805,8.12332164623336,
91.0816989272464));
#170423=CARTESIAN_POINT('Ctrl Pts',(0.159674154426438,8.12368696460186,
91.0823864562268));
#170424=CARTESIAN_POINT('Ctrl Pts',(0.149767740436123,8.12387563662988,
91.0827749402045));
#170425=CARTESIAN_POINT('Ctrl Pts',(0.123248142462953,8.12433218954174,
91.0838130596602));
#170426=CARTESIAN_POINT('Ctrl Pts',(0.106634393732977,8.12456723411067,
91.0844614601777));
#170427=CARTESIAN_POINT('Ctrl Pts',(-0.0108860505627611,8.12586932771147,
91.0890348644747));
#170428=CARTESIAN_POINT('Ctrl Pts',(-0.111806535856592,8.12510744923939,
91.0928936366302));
#170429=CARTESIAN_POINT('Ctrl Pts',(-0.64119356635003,8.11124532021173,
91.1128751751197));
#170430=CARTESIAN_POINT('Ctrl Pts',(-1.06815865345377,8.06613295571054,
91.1281347079424));
#170431=CARTESIAN_POINT('Ctrl Pts',(-1.84031498679005,7.92213471002392,
91.1563404114849));
#170432=CARTESIAN_POINT('Ctrl Pts',(-2.18634734641192,7.83369991186894,
91.1692088331408));
#170433=CARTESIAN_POINT('Ctrl Pts',(-2.69013315855809,7.66895655640531,
91.1888719604313));
#170434=CARTESIAN_POINT('Ctrl Pts',(-2.85305578072236,7.60984767735848,
91.1953769434026));
#170435=CARTESIAN_POINT('Ctrl Pts',(-3.08317118977262,7.51793171080848,
91.2048037533707));
#170436=CARTESIAN_POINT('Ctrl Pts',(-3.15199680286343,7.48933627062847,
91.2076543303865));
#170437=CARTESIAN_POINT('Ctrl Pts',(-3.2575354271195,7.44377490920035,91.212074602061));
#170438=CARTESIAN_POINT('Ctrl Pts',(-3.29453182469556,7.42747480553381,
91.2136335409408));
#170439=CARTESIAN_POINT('Ctrl Pts',(-3.36353660675089,7.39645524135656,
91.2165589622938));
#170440=CARTESIAN_POINT('Ctrl Pts',(-3.39557393805853,7.38180237179491,
91.2179243841977));
#170441=CARTESIAN_POINT('Ctrl Pts',(-3.44834687085139,7.35724944072377,
91.2201854817549));
#170442=CARTESIAN_POINT('Ctrl Pts',(-3.46913763854652,7.34746891894946,
91.2210793586516));
#170443=CARTESIAN_POINT('Ctrl Pts',(-3.50843813325239,7.32877694025304,
91.2227748660566));
#170444=CARTESIAN_POINT('Ctrl Pts',(-3.5269561221458,7.31988320157539,91.2235762242921));
#170445=CARTESIAN_POINT('Ctrl Pts',(-3.56941977876788,7.29929039433775,
91.2254195735402));
#170446=CARTESIAN_POINT('Ctrl Pts',(-3.59334198911172,7.28754356143387,
91.2264622669463));
#170447=CARTESIAN_POINT('Ctrl Pts',(-3.65313981859911,7.2578142325221,91.2290796013047));
#170448=CARTESIAN_POINT('Ctrl Pts',(-3.68894072808748,7.23968329735795,
91.2306565193586));
#170449=CARTESIAN_POINT('Ctrl Pts',(-3.88681141199762,7.1376252875052,91.2394295100787));
#170450=CARTESIAN_POINT('Ctrl Pts',(-4.04614832779095,7.04852315424849,
91.2467105089181));
#170451=CARTESIAN_POINT('Ctrl Pts',(-4.32313510540156,6.88114147954904,
91.259800936259));
#170452=CARTESIAN_POINT('Ctrl Pts',(-4.44199908466109,6.80501638750348,
91.2655671268226));
#170453=CARTESIAN_POINT('Ctrl Pts',(-4.98763161991512,6.43518284315647,
91.2927535891892));
#170454=CARTESIAN_POINT('Ctrl Pts',(-5.38765580249604,6.10419280896148,
91.3148942899855));
#170455=CARTESIAN_POINT('Ctrl Pts',(-5.95303918576735,5.53723117401015,
91.3487087082865));
#170456=CARTESIAN_POINT('Ctrl Pts',(-6.14208203793715,5.32676682290274,
91.3605217508587));
#170457=CARTESIAN_POINT('Ctrl Pts',(-6.34646443358242,5.07384271983327,
91.3735915124818));
#170458=CARTESIAN_POINT('Ctrl Pts',(-6.37289479636829,5.04060539442343,
91.3752877177737));
#170459=CARTESIAN_POINT('Ctrl Pts',(-6.40711216186561,4.99687621269705,
91.3774901961565));
#170460=CARTESIAN_POINT('Ctrl Pts',(-6.41513588741348,4.98657093483233,
91.3780071383945));
#170461=CARTESIAN_POINT('Ctrl Pts',(-6.42815828890906,4.96976215281186,
91.3788468538617));
#170462=CARTESIAN_POINT('Ctrl Pts',(-6.43317200934207,4.96327036757074,
91.3791703266778));
#170463=CARTESIAN_POINT('Ctrl Pts',(-6.44279314792255,4.95077380827444,
91.3797913822087));
#170464=CARTESIAN_POINT('Ctrl Pts',(-6.4474020217203,4.94477016841105,91.3800890338399));
#170465=CARTESIAN_POINT('Ctrl Pts',(-6.4579190241183,4.93103074298908,91.3807685597568));
#170466=CARTESIAN_POINT('Ctrl Pts',(-6.46382166067951,4.92329075419443,
91.3811501691239));
#170467=CARTESIAN_POINT('Ctrl Pts',(-6.48227733611666,4.89899985810939,
91.3823440114544));
#170468=CARTESIAN_POINT('Ctrl Pts',(-6.49478088218957,4.88241132789941,
91.383153805399));
#170469=CARTESIAN_POINT('Ctrl Pts',(-6.62712103369093,4.70542686153701,
91.391733818094));
#170470=CARTESIAN_POINT('Ctrl Pts',(-6.74104921686855,4.54070806477395,
91.3991622497739));
#170471=CARTESIAN_POINT('Ctrl Pts',(-6.94599881146518,4.21964855671273,
91.4128307301745));
#170472=CARTESIAN_POINT('Ctrl Pts',(-7.03811393101973,4.0641468313091,91.4191209705052));
#170473=CARTESIAN_POINT('Ctrl Pts',(-7.31974076196958,3.55038921999287,
91.4391995539626));
#170474=CARTESIAN_POINT('Ctrl Pts',(-7.48766202856566,3.18100523807409,
91.4525869982833));
#170475=CARTESIAN_POINT('Ctrl Pts',(-7.8113688031447,2.29941257463875,91.4845536024729));
#170476=CARTESIAN_POINT('Ctrl Pts',(-7.94553825019126,1.78132736166615,
91.5034123938262));
#170477=CARTESIAN_POINT('Ctrl Pts',(-8.03227314349433,1.22599775034216,
91.5250659142335));
#170478=CARTESIAN_POINT('Ctrl Pts',(-8.03647854079838,1.19812143791007,
91.5261563057583));
#170479=CARTESIAN_POINT('Ctrl Pts',(-8.04239660847886,1.15745874951914,
91.5277519654002));
#170480=CARTESIAN_POINT('Ctrl Pts',(-8.04422405753139,1.14468916100396,
91.5282537969874));
#170481=CARTESIAN_POINT('Ctrl Pts',(-8.04737502680251,1.12229104960988,
91.5291353216633));
#170482=CARTESIAN_POINT('Ctrl Pts',(-8.04871169693577,1.1126643882335,91.5295146205276));
#170483=CARTESIAN_POINT('Ctrl Pts',(-8.05127150739504,1.09398270830026,
91.5302515182297));
#170484=CARTESIAN_POINT('Ctrl Pts',(-8.05249665243197,1.0849279763153,91.5306090565012));
#170485=CARTESIAN_POINT('Ctrl Pts',(-8.05538192712531,1.06332952168318,
91.5314628001086));
#170486=CARTESIAN_POINT('Ctrl Pts',(-8.05702803245808,1.05078396732294,
91.5319594239335));
#170487=CARTESIAN_POINT('Ctrl Pts',(-8.06279626181468,1.00601170750454,
91.5337343630535));
#170488=CARTESIAN_POINT('Ctrl Pts',(-8.06675436645838,0.973764384603706,
91.5350175726263));
#170489=CARTESIAN_POINT('Ctrl Pts',(-8.12948602377688,0.436026697749313,
91.5564970888526));
#170490=CARTESIAN_POINT('Ctrl Pts',(-8.14082950635848,-0.073797495358503,
91.5781562497802));
#170491=CARTESIAN_POINT('Ctrl Pts',(-8.06252297267184,-1.16557713196623,
91.6266813471057));
#170492=CARTESIAN_POINT('Ctrl Pts',(-7.95755304790733,-1.7436107081773,
91.6537035798851));
#170493=CARTESIAN_POINT('Ctrl Pts',(-7.72560158084465,-2.52754297635896,
91.6892723634112));
#170494=CARTESIAN_POINT('Ctrl Pts',(-7.65036684972993,-2.74687102487199,
91.6990816593317));
#170495=CARTESIAN_POINT('Ctrl Pts',(-7.5516070841766,-2.99907382888776,
91.7099854572502));
#170496=CARTESIAN_POINT('Ctrl Pts',(-7.53710173690985,-3.03534361676441,
91.7115446732268));
#170497=CARTESIAN_POINT('Ctrl Pts',(-7.51768119451012,-3.08290586865181,
91.7135793601409));
#170498=CARTESIAN_POINT('Ctrl Pts',(-7.51300125579147,-3.0942933393667,
91.7140657532789));
#170499=CARTESIAN_POINT('Ctrl Pts',(-7.50531299545572,-3.11288054495593,
91.7148584977897));
#170500=CARTESIAN_POINT('Ctrl Pts',(-7.50232016371644,-3.12008663478886,
91.7151655494323));
#170501=CARTESIAN_POINT('Ctrl Pts',(-7.49652701492568,-3.13397875252599,
91.7157569564762));
#170502=CARTESIAN_POINT('Ctrl Pts',(-7.49372812287789,-3.14066536384142,
91.7160413748296));
#170503=CARTESIAN_POINT('Ctrl Pts',(-7.48728185381759,-3.15600795831578,
91.7166934469854));
#170504=CARTESIAN_POINT('Ctrl Pts',(-7.48362840351823,-3.16466138954361,
91.7170608346469));
#170505=CARTESIAN_POINT('Ctrl Pts',(-7.47386126591454,-3.18768398514423,
91.7180372839942));
#170506=CARTESIAN_POINT('Ctrl Pts',(-7.46772113004175,-3.20204193280439,
91.7186452126462));
#170507=CARTESIAN_POINT('Ctrl Pts',(-7.42538910388895,-3.30024608741469,
91.722796758154));
#170508=CARTESIAN_POINT('Ctrl Pts',(-7.38782645017924,-3.38349651198322,
91.726283677079));
#170509=CARTESIAN_POINT('Ctrl Pts',(-7.12269210387363,-3.94563797392302,
91.7497124355835));
#170510=CARTESIAN_POINT('Ctrl Pts',(-6.85011003083093,-4.40191613374934,
91.7682702312719));
#170511=CARTESIAN_POINT('Ctrl Pts',(-6.12207756105125,-5.38727133836705,
91.8123767689571));
#170512=CARTESIAN_POINT('Ctrl Pts',(-5.63919419628615,-5.89083258509883,
91.838322286557));
#170513=CARTESIAN_POINT('Ctrl Pts',(-5.00687095493669,-6.40036604197319,
91.8696914453421));
#170514=CARTESIAN_POINT('Ctrl Pts',(-4.91396794029383,-6.47196731844397,
91.8742385876345));
#170515=CARTESIAN_POINT('Ctrl Pts',(-4.7787956998906,-6.57155700659152,
91.8807782974299));
#170516=CARTESIAN_POINT('Ctrl Pts',(-4.73776355339478,-6.60120036916218,
91.8827536675297));
#170517=CARTESIAN_POINT('Ctrl Pts',(-4.66547667998767,-6.65240229120052,
91.8862175681431));
#170518=CARTESIAN_POINT('Ctrl Pts',(-4.63434279484372,-6.67412883768865,
91.8877043135851));
#170519=CARTESIAN_POINT('Ctrl Pts',(-4.5693197890889,-6.71883028840123,
91.8907991144362));
#170520=CARTESIAN_POINT('Ctrl Pts',(-4.53540698411044,-6.74176885177694,
91.8924074966925));
#170521=CARTESIAN_POINT('Ctrl Pts',(-4.44649713665089,-6.80093284582514,
91.8966099552527));
#170522=CARTESIAN_POINT('Ctrl Pts',(-4.39123064891768,-6.8367475948886,
91.8992081380901));
#170523=CARTESIAN_POINT('Ctrl Pts',(-4.15001610900945,-6.9889320246575,
91.9104908965143));
#170524=CARTESIAN_POINT('Ctrl Pts',(-3.95983596699512,-7.09841539955821,
91.9192428340685));
#170525=CARTESIAN_POINT('Ctrl Pts',(-3.35345079974509,-7.41554022079475,
91.9467527587969));
#170526=CARTESIAN_POINT('Ctrl Pts',(-2.92370650732244,-7.59524855334279,
91.9657197079367));
#170527=CARTESIAN_POINT('Ctrl Pts',(-2.32694514049983,-7.78660232120568,
91.9911036976743));
#170528=CARTESIAN_POINT('Ctrl Pts',(-2.17148148805181,-7.83138037372527,
91.9976295449122));
#170529=CARTESIAN_POINT('Ctrl Pts',(-1.95448342815741,-7.88692312920749,
92.0065920338899));
#170530=CARTESIAN_POINT('Ctrl Pts',(-1.89400735448259,-7.90166426453254,
92.0090742476009));
#170531=CARTESIAN_POINT('Ctrl Pts',(-1.78841617188946,-7.92612037366538,
92.0133789052787));
#170532=CARTESIAN_POINT('Ctrl Pts',(-1.74337670423528,-7.93614858055619,
92.0152058198199));
#170533=CARTESIAN_POINT('Ctrl Pts',(-1.67669387153191,-7.9504007005055,
92.0178962314956));
#170534=CARTESIAN_POINT('Ctrl Pts',(-1.65511496156213,-7.95492099956906,
92.0187646362495));
#170535=CARTESIAN_POINT('Ctrl Pts',(-1.61535298273234,-7.96308144898652,
92.0203605978011));
#170536=CARTESIAN_POINT('Ctrl Pts',(-1.5971753932187,-7.96674727780008,
92.0210886161781));
#170537=CARTESIAN_POINT('Ctrl Pts',(-1.55593137413552,-7.97491802261615,
92.0227370677108));
#170538=CARTESIAN_POINT('Ctrl Pts',(-1.53285760693621,-7.97938515619657,
92.0236568898079));
#170539=CARTESIAN_POINT('Ctrl Pts',(-1.47248185710484,-7.99080249180098,
92.0260579822632));
#170540=CARTESIAN_POINT('Ctrl Pts',(-1.43514992363138,-7.99759163745963,
92.0275369144875));
#170541=CARTESIAN_POINT('Ctrl Pts',(-1.21344547183795,-8.03630822846412,
92.0362906665144));
#170542=CARTESIAN_POINT('Ctrl Pts',(-1.02806049269457,-8.06212086388244,
92.0434923785696));
#170543=CARTESIAN_POINT('Ctrl Pts',(-0.646892079442106,-8.1018317777574,
92.0582279408311));
#170544=CARTESIAN_POINT('Ctrl Pts',(-0.451164538096103,-8.11508458141697,
92.0657565407119));
#170545=CARTESIAN_POINT('Ctrl Pts',(-0.137186733452844,-8.12494901028113,
92.0778823318179));
#170546=CARTESIAN_POINT('Ctrl Pts',(-0.0191574650205549,-8.12608450102143,
92.0824510807092));
#170547=CARTESIAN_POINT('Ctrl Pts',(0.146747456388834,-8.12406590758929,
92.0889016755247));
#170548=CARTESIAN_POINT('Ctrl Pts',(0.194634710108802,-8.12305970632771,
92.0907669059179));
#170549=CARTESIAN_POINT('Ctrl Pts',(0.278036579505863,-8.12056934433482,
92.0940220596989));
#170550=CARTESIAN_POINT('Ctrl Pts',(0.313555601712088,-8.11927544120442,
92.0954104467735));
#170551=CARTESIAN_POINT('Ctrl Pts',(0.382619616057752,-8.11630567385771,
92.0981144332776));
#170552=CARTESIAN_POINT('Ctrl Pts',(0.416164978307712,-8.11465478404261,
92.0994298060961));
#170553=CARTESIAN_POINT('Ctrl Pts',(0.507168194802084,-8.10961039953391,
92.1030039504594));
#170554=CARTESIAN_POINT('Ctrl Pts',(0.564601644293109,-8.1058142928137,
92.1052658794024));
#170555=CARTESIAN_POINT('Ctrl Pts',(0.824377814177232,-8.08586984602522,
92.1155267026));
#170556=CARTESIAN_POINT('Ctrl Pts',(1.0261103598194,-8.06275299475706,92.1235797740209));
#170557=CARTESIAN_POINT('Ctrl Pts',(1.47560394559122,-7.99410074502044,
92.1417023329796));
#170558=CARTESIAN_POINT('Ctrl Pts',(1.72254346647485,-7.94455143425055,
92.1517839883327));
#170559=CARTESIAN_POINT('Ctrl Pts',(2.07071499760272,-7.85769056498425,
92.1660641957238));
#170560=CARTESIAN_POINT('Ctrl Pts',(2.17412444322425,-7.82970911697356,
92.170312999074));
#170561=CARTESIAN_POINT('Ctrl Pts',(2.30549862540778,-7.79135726742405,
92.1757072818471));
#170562=CARTESIAN_POINT('Ctrl Pts',(2.33400033231447,-7.78286672375455,
92.1768773478741));
#170563=CARTESIAN_POINT('Ctrl Pts',(2.38150300854262,-7.76843145817181,
92.1788266529969));
#170564=CARTESIAN_POINT('Ctrl Pts',(2.40052984006783,-7.76257305209962,
92.1796072076169));
#170565=CARTESIAN_POINT('Ctrl Pts',(2.43754222615371,-7.75102775573066,
92.1811253405446));
#170566=CARTESIAN_POINT('Ctrl Pts',(2.45552989513141,-7.7453480432535,92.1818630197784));
#170567=CARTESIAN_POINT('Ctrl Pts',(2.49879883054023,-7.73151974063034,
92.1836373933238));
#170568=CARTESIAN_POINT('Ctrl Pts',(2.52406026451679,-7.72330971042026,
92.1846732347543));
#170569=CARTESIAN_POINT('Ctrl Pts',(2.61917018317242,-7.69188227439443,
92.188573715468));
#170570=CARTESIAN_POINT('Ctrl Pts',(2.68874267649146,-7.6678398723011,92.1914279653892));
#170571=CARTESIAN_POINT('Ctrl Pts',(3.15870745455253,-7.4982497084062,92.2107457472262));
#170572=CARTESIAN_POINT('Ctrl Pts',(3.54744472814665,-7.32235092393076,
92.226941471631));
#170573=CARTESIAN_POINT('Ctrl Pts',(4.09745492448331,-7.01935342607266,
92.2511231719495));
#170574=CARTESIAN_POINT('Ctrl Pts',(4.27061899700236,-6.91536488510482,
92.2589318238872));
#170575=CARTESIAN_POINT('Ctrl Pts',(4.50158122225822,-6.76468094802649,
92.2696646824494));
#170576=CARTESIAN_POINT('Ctrl Pts',(4.5628811060411,-6.72348553748016,92.2725449508586));
#170577=CARTESIAN_POINT('Ctrl Pts',(4.66885159089408,-6.65015332560848,
92.2775812948471));
#170578=CARTESIAN_POINT('Ctrl Pts',(4.71377327380087,-6.61838771366723,
92.2797345793723));
#170579=CARTESIAN_POINT('Ctrl Pts',(4.80898249460813,-6.54960104504977,
92.2843381778087));
#170580=CARTESIAN_POINT('Ctrl Pts',(4.8591728964647,-6.51245155148121,92.2867892123616));
#170581=CARTESIAN_POINT('Ctrl Pts',(5.08634286412471,-6.3402185892092,92.2979946922879));
#170582=CARTESIAN_POINT('Ctrl Pts',(5.25815166319581,-6.19847527952391,
92.3067858570428));
#170583=CARTESIAN_POINT('Ctrl Pts',(5.51804839609459,-5.96546819136099,
92.3205647847534));
#170584=CARTESIAN_POINT('Ctrl Pts',(5.61019339695844,-5.87889437516912,
92.3255517792433));
#170585=CARTESIAN_POINT('Ctrl Pts',(5.73176164639371,-5.75921413886876,
92.3322597964552));
#170586=CARTESIAN_POINT('Ctrl Pts',(5.76298899024911,-5.72796621707271,
92.3339947630447));
#170587=CARTESIAN_POINT('Ctrl Pts',(5.82514426711339,-5.66474715385486,
92.337471147635));
#170588=CARTESIAN_POINT('Ctrl Pts',(5.85606761194972,-5.63277357890716,
92.3392124774255));
#170589=CARTESIAN_POINT('Ctrl Pts',(6.02422758908939,-5.45602088821721,
92.3487518638481));
#170590=CARTESIAN_POINT('Ctrl Pts',(6.15635965288398,-5.30647890731507,
92.3565082839764));
#170591=CARTESIAN_POINT('Ctrl Pts',(6.34826528728209,-5.07246059068834,
92.3682928954916));
#170592=CARTESIAN_POINT('Ctrl Pts',(6.41215114329186,-4.99145732721021,
92.3723113257211));
#170593=CARTESIAN_POINT('Ctrl Pts',(6.52285487101566,-4.8454579727847,92.3794615188229));
#170594=CARTESIAN_POINT('Ctrl Pts',(6.57028665096452,-4.78094466593479,
92.3825900264944));
#170595=CARTESIAN_POINT('Ctrl Pts',(6.64896866988736,-4.67054424316788,
92.3878968735665));
#170596=CARTESIAN_POINT('Ctrl Pts',(6.68071627945109,-4.62501868852769,
92.3900720624526));
#170597=CARTESIAN_POINT('Ctrl Pts',(6.74605808178709,-4.52924288272262,
92.3946225376633));
#170598=CARTESIAN_POINT('Ctrl Pts',(6.77956300703941,-4.4789358258076,92.3969982584681));
#170599=CARTESIAN_POINT('Ctrl Pts',(6.87051117099734,-4.33901976098782,
92.4035684828183));
#170600=CARTESIAN_POINT('Ctrl Pts',(6.92675953684029,-4.2486490032143,92.407770739258));
#170601=CARTESIAN_POINT('Ctrl Pts',(7.033015537159,-4.07021252359226,92.415994616535));
#170602=CARTESIAN_POINT('Ctrl Pts',(7.08318446648694,-3.98226508197325,
92.4200143141625));
#170603=CARTESIAN_POINT('Ctrl Pts',(7.18073410898358,-3.80357965860117,
92.4281167148098));
#170604=CARTESIAN_POINT('Ctrl Pts',(7.22807006447523,-3.71283767155708,
92.4321989093444));
#170605=CARTESIAN_POINT('Ctrl Pts',(7.3898254883973,-3.38793195625791,92.446700232125));
#170606=CARTESIAN_POINT('Ctrl Pts',(7.494680469301,-3.14918532239902,92.4571519571623));
#170607=CARTESIAN_POINT('Ctrl Pts',(7.61723394927021,-2.82916441201045,
92.470832470786));
#170608=CARTESIAN_POINT('Ctrl Pts',(7.6454242080905,-2.752074324828,92.4741031506227));
#170609=CARTESIAN_POINT('Ctrl Pts',(7.70112831188899,-2.59227799434258,
92.4808260325697));
#170610=CARTESIAN_POINT('Ctrl Pts',(7.72848926263153,-2.5095291171007,92.4842765442627));
#170611=CARTESIAN_POINT('Ctrl Pts',(7.76362438178407,-2.39723899532729,
92.4889119563045));
#170612=CARTESIAN_POINT('Ctrl Pts',(7.77257082368621,-2.36807118637777,
92.4901117791782));
#170613=CARTESIAN_POINT('Ctrl Pts',(7.7872982159503,-2.31907323497182,92.4921198897859));
#170614=CARTESIAN_POINT('Ctrl Pts',(7.79316819992216,-2.29927022872789,
92.4929294605231));
#170615=CARTESIAN_POINT('Ctrl Pts',(7.80402734338868,-2.26211642439976,
92.4944444415505));
#170616=CARTESIAN_POINT('Ctrl Pts',(7.80903430975614,-2.24477095648766,
92.4951501238388));
#170617=CARTESIAN_POINT('Ctrl Pts',(7.82256613925013,-2.19729988260506,
92.4970769830871));
#170618=CARTESIAN_POINT('Ctrl Pts',(7.83097476858211,-2.16714142680919,
92.4982962723509));
#170619=CARTESIAN_POINT('Ctrl Pts',(7.86936668682193,-2.02630314055323,
92.5039698199576));
#170620=CARTESIAN_POINT('Ctrl Pts',(7.89717939934593,-1.91504424260237,
92.5083932121764));
#170621=CARTESIAN_POINT('Ctrl Pts',(7.99293483520782,-1.49433619285397,
92.5249774384208));
#170622=CARTESIAN_POINT('Ctrl Pts',(8.04511593132074,-1.18159167699269,
92.5370319689456));
#170623=CARTESIAN_POINT('Ctrl Pts',(8.08909131823104,-0.771629623113678,
92.5528917398022));
#170624=CARTESIAN_POINT('Ctrl Pts',(8.09760301466621,-0.676487903331905,
92.5565751681093));
#170625=CARTESIAN_POINT('Ctrl Pts',(8.10977796270002,-0.506722062901886,
92.5631621022111));
#170626=CARTESIAN_POINT('Ctrl Pts',(8.11409312580478,-0.432155649202921,
92.5660601980145));
#170627=CARTESIAN_POINT('Ctrl Pts',(8.11917468930519,-0.316787010046766,
92.5705545605992));
#170628=CARTESIAN_POINT('Ctrl Pts',(8.12066279951398,-0.276020516578724,
92.5721446860148));
#170629=CARTESIAN_POINT('Ctrl Pts',(8.12285858628993,-0.200210768694241,
92.5751058398568));
#170630=CARTESIAN_POINT('Ctrl Pts',(8.12364663015118,-0.165170768644414,
92.5764761571663));
#170631=CARTESIAN_POINT('Ctrl Pts',(8.12490270687114,-0.0867501420875349,
92.5795468931977));
#170632=CARTESIAN_POINT('Ctrl Pts',(8.12525007127121,-0.0433686906354123,
92.5812482788994));
#170633=CARTESIAN_POINT('Ctrl Pts',(8.12524985383566,0.0889764527132254,
92.5864473873871));
#170634=CARTESIAN_POINT('Ctrl Pts',(8.12378862713576,0.177933077463759,
92.5899539884065));
#170635=CARTESIAN_POINT('Ctrl Pts',(8.11677939641233,0.391242446543852,
92.598391986294));
#170636=CARTESIAN_POINT('Ctrl Pts',(8.10983418366525,0.515526530941922,
92.6033326440291));
#170637=CARTESIAN_POINT('Ctrl Pts',(8.08864399641308,0.783883249664426,
92.6140460936026));
#170638=CARTESIAN_POINT('Ctrl Pts',(8.07339810971291,0.927834816599277,
92.6198216539235));
#170639=CARTESIAN_POINT('Ctrl Pts',(8.0320035369246,1.23904959113875,92.6323415848297));
#170640=CARTESIAN_POINT('Ctrl Pts',(8.00445621357875,1.4060605135341,92.6390818150515));
#170641=CARTESIAN_POINT('Ctrl Pts',(7.96508687842567,1.60569352292279,92.6471213009521));
#170642=CARTESIAN_POINT('Ctrl Pts',(7.958247561075,1.63925484318654,92.6484722158129));
#170643=CARTESIAN_POINT('Ctrl Pts',(7.94737818586265,1.69092030307857,92.650550288916));
#170644=CARTESIAN_POINT('Ctrl Pts',(7.94349801913949,1.70905550610098,92.6512794179468));
#170645=CARTESIAN_POINT('Ctrl Pts',(7.93601015429277,1.74347601450636,92.6526626117487));
#170646=CARTESIAN_POINT('Ctrl Pts',(7.93241433184351,1.75976380582013,92.6533168457235));
#170647=CARTESIAN_POINT('Ctrl Pts',(7.92353869181697,1.79938728081446,92.654907577781));
#170648=CARTESIAN_POINT('Ctrl Pts',(7.91820590241353,1.8227109699445,92.6558432356378));
#170649=CARTESIAN_POINT('Ctrl Pts',(7.89987323290624,1.90129241615368,92.658993720898));
#170650=CARTESIAN_POINT('Ctrl Pts',(7.88639726226582,1.95643764008313,92.6612014228558));
#170651=CARTESIAN_POINT('Ctrl Pts',(7.85211128844485,2.09062575625059,92.6665701503346));
#170652=CARTESIAN_POINT('Ctrl Pts',(7.83068430976363,2.16950481597874,92.6697231299059));
#170653=CARTESIAN_POINT('Ctrl Pts',(7.69764406531527,2.63158917648916,92.6882072536937));
#170654=CARTESIAN_POINT('Ctrl Pts',(7.55910628610006,3.00647705294046,92.7032723456445));
#170655=CARTESIAN_POINT('Ctrl Pts',(7.22930345213665,3.73011679811805,92.7335149763978));
#170656=CARTESIAN_POINT('Ctrl Pts',(7.03888962387209,4.07806615740555,92.7486537649256));
#170657=CARTESIAN_POINT('Ctrl Pts',(6.78408109487753,4.47228154070999,92.766885800197));
#170658=CARTESIAN_POINT('Ctrl Pts',(6.74346728117882,4.53328880927804,92.7697393178074));
#170659=CARTESIAN_POINT('Ctrl Pts',(6.67775421221683,4.62916088756795,92.7742763298372));
#170660=CARTESIAN_POINT('Ctrl Pts',(6.65319413919483,4.66439058955986,92.7759550471731));
#170661=CARTESIAN_POINT('Ctrl Pts',(6.606651131461,4.73003770581762,92.7791051666667));
#170662=CARTESIAN_POINT('Ctrl Pts',(6.58473448989053,4.76050076762459,92.7805759687621));
#170663=CARTESIAN_POINT('Ctrl Pts',(6.53496362109936,4.82867851335447,92.7838882485662));
#170664=CARTESIAN_POINT('Ctrl Pts',(6.5069924275391,4.86630611891308,92.7857306485246));
#170665=CARTESIAN_POINT('Ctrl Pts',(6.42101202943511,4.9799024164317,92.7913369923278));
#170666=CARTESIAN_POINT('Ctrl Pts',(6.36198677642911,5.05509126216758,92.7951087145605));
#170667=CARTESIAN_POINT('Ctrl Pts',(6.05012575904466,5.43823691106428,92.8146500019928));
#170668=CARTESIAN_POINT('Ctrl Pts',(5.77621832778755,5.72832731516129,92.8304763858973));
#170669=CARTESIAN_POINT('Ctrl Pts',(5.06455976488356,6.37887229406972,92.8697243155004));
#170670=CARTESIAN_POINT('Ctrl Pts',(4.60826411107181,6.71592229402071,92.8936052317998));
#170671=CARTESIAN_POINT('Ctrl Pts',(3.84854986467929,7.1629649651361,92.9308907716063));
#170672=CARTESIAN_POINT('Ctrl Pts',(3.56728098702269,7.30711440100533,92.944187588048));
#170673=CARTESIAN_POINT('Ctrl Pts',(3.21397616996505,7.46290771442859,92.959824787232));
#170674=CARTESIAN_POINT('Ctrl Pts',(3.14925469017234,7.49044922582953,92.9626464954614));
#170675=CARTESIAN_POINT('Ctrl Pts',(3.07092310402293,7.52258760444498,92.9660036512485));
#170676=CARTESIAN_POINT('Ctrl Pts',(3.0576490248136,7.52799278835976,92.9665705666569));
#170677=CARTESIAN_POINT('Ctrl Pts',(3.03591817965557,7.53677459424869,92.9674953292482));
#170678=CARTESIAN_POINT('Ctrl Pts',(3.0274699455964,7.54017216033047,92.9678540257405));
#170679=CARTESIAN_POINT('Ctrl Pts',(3.0123409579158,7.54622695182328,92.9684948845284));
#170680=CARTESIAN_POINT('Ctrl Pts',(3.00566236249887,7.54888952219057,92.9687772687676));
#170681=CARTESIAN_POINT('Ctrl Pts',(2.9915204581127,7.55450576384538,92.9693741058088));
#170682=CARTESIAN_POINT('Ctrl Pts',(2.98405628484498,7.55745724941607,92.9696884659009));
#170683=CARTESIAN_POINT('Ctrl Pts',(2.96420047090534,7.5652746387566,92.9705229502921));
#170684=CARTESIAN_POINT('Ctrl Pts',(2.95180119226931,7.57012116915082,92.9710422369641));
#170685=CARTESIAN_POINT('Ctrl Pts',(2.89422577864737,7.59246281907712,92.9734448932125));
#170686=CARTESIAN_POINT('Ctrl Pts',(2.84890464706926,7.60958455219702,92.9753115634284));
#170687=CARTESIAN_POINT('Ctrl Pts',(2.45378369314967,7.75483121988337,92.9913555770271));
#170688=CARTESIAN_POINT('Ctrl Pts',(2.09568169783588,7.85917440021571,93.0043536212772));
#170689=CARTESIAN_POINT('Ctrl Pts',(1.05516167749654,8.0861454356565,93.0404568526428));
#170690=CARTESIAN_POINT('Ctrl Pts',(0.362598493273749,8.14663450538044,
93.0627236651696));
#170691=CARTESIAN_POINT('Ctrl Pts',(-0.585419638428446,8.10818730570098,
93.0967615628309));
#170692=CARTESIAN_POINT('Ctrl Pts',(-0.840937253722497,8.08568052112567,
93.1062621856567));
#170693=CARTESIAN_POINT('Ctrl Pts',(-1.12360348951219,8.04723796083923,
93.1172475852981));
#170694=CARTESIAN_POINT('Ctrl Pts',(-1.15223287427744,8.04318860794345,
93.1183656127763));
#170695=CARTESIAN_POINT('Ctrl Pts',(-1.19244611735059,8.03728171904753,
93.1199437099653));
#170696=CARTESIAN_POINT('Ctrl Pts',(-1.20404863774974,8.03555175769981,
93.1203999324242));
#170697=CARTESIAN_POINT('Ctrl Pts',(-1.22533306186345,8.03233106957042,
93.1212385221845));
#170698=CARTESIAN_POINT('Ctrl Pts',(-1.2350161026939,8.0308479470702,93.1216206595202));
#170699=CARTESIAN_POINT('Ctrl Pts',(-1.2546405225703,8.02780580128416,93.1223964187254));
#170700=CARTESIAN_POINT('Ctrl Pts',(-1.26458173367128,8.02624581370359,
93.1227900691009));
#170701=CARTESIAN_POINT('Ctrl Pts',(-1.28906227447679,8.02235768508244,
93.1237611064198));
#170702=CARTESIAN_POINT('Ctrl Pts',(-1.3035981971649,8.02000848581037,93.1243391279877));
#170703=CARTESIAN_POINT('Ctrl Pts',(-1.35668008998067,8.01128161796277,
93.1264552402919));
#170704=CARTESIAN_POINT('Ctrl Pts',(-1.39518601763755,8.00466551163902,
93.1280005189447));
#170705=CARTESIAN_POINT('Ctrl Pts',(-1.6175676447821,7.96480244331913,93.1369848906469));
#170706=CARTESIAN_POINT('Ctrl Pts',(-1.80029237755123,7.92549965328251,
93.1446064091622));
#170707=CARTESIAN_POINT('Ctrl Pts',(-2.3770855277246,7.78045890836892,93.1694332999153));
#170708=CARTESIAN_POINT('Ctrl Pts',(-2.7645941422359,7.65134290188091,93.1873038718073));
#170709=CARTESIAN_POINT('Ctrl Pts',(-3.7721806164034,7.22904509667764,93.2361142513957));
#170710=CARTESIAN_POINT('Ctrl Pts',(-4.36770081301235,6.8856244915369,93.2675980694527));
#170711=CARTESIAN_POINT('Ctrl Pts',(-4.94405345614466,6.44806412916196,
93.2967781797405));
#170712=CARTESIAN_POINT('Ctrl Pts',(-4.97481482977613,6.42436090787477,
93.298331671286));
#170713=CARTESIAN_POINT('Ctrl Pts',(-5.01574588447303,6.39235114046577,
93.3003950086423));
#170714=CARTESIAN_POINT('Ctrl Pts',(-5.02606673857963,6.38423942397562,
93.3009149625828));
#170715=CARTESIAN_POINT('Ctrl Pts',(-5.04216959115919,6.37152007265509,
93.3017257736861));
#170716=CARTESIAN_POINT('Ctrl Pts',(-5.0479650081613,6.36692951893811,93.3020174963962));
#170717=CARTESIAN_POINT('Ctrl Pts',(-5.05957714493085,6.35770571651672,
93.3026018527));
#170718=CARTESIAN_POINT('Ctrl Pts',(-5.06539378505848,6.35307238004323,
93.3028944813418));
#170719=CARTESIAN_POINT('Ctrl Pts',(-5.07852206594827,6.34258534933163,
93.3035547840228));
#170720=CARTESIAN_POINT('Ctrl Pts',(-5.08582997002368,6.33672697887453,
93.3039222268951));
#170721=CARTESIAN_POINT('Ctrl Pts',(-5.10746863069011,6.31931883318924,
93.3050099227394));
#170722=CARTESIAN_POINT('Ctrl Pts',(-5.12177034237241,6.30773294422095,
93.305728425548));
#170723=CARTESIAN_POINT('Ctrl Pts',(-5.23842675913126,6.21257065238713,
93.3115868846551));
#170724=CARTESIAN_POINT('Ctrl Pts',(-5.33877110104034,6.12655483502121,
93.3166122840362));
#170725=CARTESIAN_POINT('Ctrl Pts',(-5.59297117555916,5.89766276210383,
93.3294163189935));
#170726=CARTESIAN_POINT('Ctrl Pts',(-5.74346918672227,5.75120150716792,
93.3370713668058));
#170727=CARTESIAN_POINT('Ctrl Pts',(-6.41263853746888,5.04748584097122,
93.3721640961438));
#170728=CARTESIAN_POINT('Ctrl Pts',(-6.85702792995148,4.42495441150281,
93.3990550745752));
#170729=CARTESIAN_POINT('Ctrl Pts',(-7.2447176474381,3.67967164622257,93.4312128251604));
#170730=CARTESIAN_POINT('Ctrl Pts',(-7.2801193993134,3.60912434589969,93.4342511024308));
#170731=CARTESIAN_POINT('Ctrl Pts',(-7.32726894840244,3.51164903081612,
93.4384416871382));
#170732=CARTESIAN_POINT('Ctrl Pts',(-7.33990712666235,3.48515602518261,
93.439579905517));
#170733=CARTESIAN_POINT('Ctrl Pts',(-7.3613273987315,3.43962006905566,93.441534966081));
#170734=CARTESIAN_POINT('Ctrl Pts',(-7.37017985566783,3.42061049848573,
93.4423507450559));
#170735=CARTESIAN_POINT('Ctrl Pts',(-7.38718248430694,3.38372699853912,
93.4439328049726));
#170736=CARTESIAN_POINT('Ctrl Pts',(-7.39534163096749,3.36585733743203,
93.4446989415956));
#170737=CARTESIAN_POINT('Ctrl Pts',(-7.41403289695554,3.32452480680324,
93.4464702787413));
#170738=CARTESIAN_POINT('Ctrl Pts',(-7.42451857386444,3.3010411884574,93.4474761502845));
#170739=CARTESIAN_POINT('Ctrl Pts',(-7.45361242283203,3.23504298948758,
93.4503018601173));
#170740=CARTESIAN_POINT('Ctrl Pts',(-7.47196803726678,3.19241834703397,
93.4521254645569));
#170741=CARTESIAN_POINT('Ctrl Pts',(-7.5866068548216,2.91980302174023,93.4637838740343));
#170742=CARTESIAN_POINT('Ctrl Pts',(-7.67262277575293,2.68564813872753,
93.4737814233935));
#170743=CARTESIAN_POINT('Ctrl Pts',(-7.84472732977312,2.14093144407124,
93.4971185373445));
#170744=CARTESIAN_POINT('Ctrl Pts',(-7.9233853814544,1.82846522772179,93.5105695114073));
#170745=CARTESIAN_POINT('Ctrl Pts',(-8.0821245570991,0.990422030426204,
93.546621976284));
#170746=CARTESIAN_POINT('Ctrl Pts',(-8.12956703598508,0.460243031389453,
93.5694736406476));
#170747=CARTESIAN_POINT('Ctrl Pts',(-8.12444251434636,-0.128091216856152,
93.5932478105546));
#170748=CARTESIAN_POINT('Ctrl Pts',(-8.12333664255147,-0.18540631272118,
93.5955459935552));
#170749=CARTESIAN_POINT('Ctrl Pts',(-8.12117453609173,-0.25775656968365,
93.5984210476238));
#170750=CARTESIAN_POINT('Ctrl Pts',(-8.12068291706426,-0.272806266345323,
93.5990176705914));
#170751=CARTESIAN_POINT('Ctrl Pts',(-8.11983993258543,-0.296586191083534,
93.5999580635789));
#170752=CARTESIAN_POINT('Ctrl Pts',(-8.11951631739125,-0.305317329815395,
93.6003028464561));
#170753=CARTESIAN_POINT('Ctrl Pts',(-8.11888934052497,-0.321526756330951,
93.6009419993758));
#170754=CARTESIAN_POINT('Ctrl Pts',(-8.11858972815591,-0.32900517483413,
93.6012365092375));
#170755=CARTESIAN_POINT('Ctrl Pts',(-8.1179051404897,-0.345522119738005,
93.6018861341483));
#170756=CARTESIAN_POINT('Ctrl Pts',(-8.11751540163881,-0.354560446468816,
93.6022410672732));
#170757=CARTESIAN_POINT('Ctrl Pts',(-8.11668392317779,-0.373122705508367,
93.6029688470262));
#170758=CARTESIAN_POINT('Ctrl Pts',(-8.11624051386584,-0.382646552588263,
93.6033416280234));
#170759=CARTESIAN_POINT('Ctrl Pts',(-8.11506270384081,-0.407020820485135,
93.6042940477138));
#170760=CARTESIAN_POINT('Ctrl Pts',(-8.11430429985016,-0.421870085268918,
93.6048727268254));
#170761=CARTESIAN_POINT('Ctrl Pts',(-8.11200793428495,-0.464532869672184,
93.6065306964587));
#170762=CARTESIAN_POINT('Ctrl Pts',(-8.11036768771832,-0.492340846580435,
93.6076057460644));
#170763=CARTESIAN_POINT('Ctrl Pts',(-8.09235482994553,-0.773147473826267,
93.6184013685156));
#170764=CARTESIAN_POINT('Ctrl Pts',(-8.06429209754929,-1.02526214079034,
93.6275711182436));
#170765=CARTESIAN_POINT('Ctrl Pts',(-7.95450336871915,-1.71588537881363,
93.6520617954594));
#170766=CARTESIAN_POINT('Ctrl Pts',(-7.84841013923517,-2.14962086652652,
93.6667677898156));
#170767=CARTESIAN_POINT('Ctrl Pts',(-7.52295331662879,-3.12470753135144,
93.7015353456496));
#170768=CARTESIAN_POINT('Ctrl Pts',(-7.27983978476436,-3.65547154298248,
93.721845101291));
#170769=CARTESIAN_POINT('Ctrl Pts',(-6.96462931177202,-4.18506813867342,
93.7455237581159));
#170770=CARTESIAN_POINT('Ctrl Pts',(-6.946955626451,-4.21434031211697,93.7468438069342));
#170771=CARTESIAN_POINT('Ctrl Pts',(-6.92234382236947,-4.25452827115195,
93.7486719161675));
#170772=CARTESIAN_POINT('Ctrl Pts',(-6.9155635229353,-4.26554052419386,
93.7491744988491));
#170773=CARTESIAN_POINT('Ctrl Pts',(-6.90390855260079,-4.28436916213679,
93.750036646164));
#170774=CARTESIAN_POINT('Ctrl Pts',(-6.89904681773824,-4.29219354481024,
93.7503957597633));
#170775=CARTESIAN_POINT('Ctrl Pts',(-6.889047551509,-4.30822529013419,93.7511332982291));
#170776=CARTESIAN_POINT('Ctrl Pts',(-6.8839086348603,-4.31643176983551,
93.7515117712047));
#170777=CARTESIAN_POINT('Ctrl Pts',(-6.8720174405855,-4.33534590383467,
93.7523862345009));
#170778=CARTESIAN_POINT('Ctrl Pts',(-6.86525479241219,-4.34604699044165,
93.7528825877653));
#170779=CARTESIAN_POINT('Ctrl Pts',(-6.84403052917533,-4.37945870963368,
93.7544373878876));
#170780=CARTESIAN_POINT('Ctrl Pts',(-6.82948108948303,-4.40211318632358,
93.7554989209249));
#170781=CARTESIAN_POINT('Ctrl Pts',(-6.62764356749219,-4.71297898010225,
93.7701670742825));
#170782=CARTESIAN_POINT('Ctrl Pts',(-6.4223808418545,-4.98907000899445,
93.784423026309));
#170783=CARTESIAN_POINT('Ctrl Pts',(-5.84025454190004,-5.67639072802745,
93.8232087044756));
#170784=CARTESIAN_POINT('Ctrl Pts',(-5.43749754265107,-6.06329314558541,
93.848590321199));
#170785=CARTESIAN_POINT('Ctrl Pts',(-4.64553360621117,-6.68124313302881,
93.8936770602743));
#170786=CARTESIAN_POINT('Ctrl Pts',(-4.27047986554562,-6.9269850970865,
93.9133892191095));
#170787=CARTESIAN_POINT('Ctrl Pts',(-3.85204446889236,-7.15417707643722,
93.9324514619052));
#170788=CARTESIAN_POINT('Ctrl Pts',(-3.82698216091663,-7.16761493115945,
93.9335830978271));
#170789=CARTESIAN_POINT('Ctrl Pts',(-3.79192100721013,-7.18617762415684,
93.9351528610127));
#170790=CARTESIAN_POINT('Ctrl Pts',(-3.78198149380261,-7.19141361299281,
93.9355963850568));
#170791=CARTESIAN_POINT('Ctrl Pts',(-3.76600065592939,-7.19978978715145,
93.936307147053));
#170792=CARTESIAN_POINT('Ctrl Pts',(-3.75996621001173,-7.20294301099246,
93.9365749998592));
#170793=CARTESIAN_POINT('Ctrl Pts',(-3.74747918444401,-7.20944798124879,
93.9371281747099));
#170794=CARTESIAN_POINT('Ctrl Pts',(-3.74102605388138,-7.21279865910471,
93.9374134471239));
#170795=CARTESIAN_POINT('Ctrl Pts',(-3.72595631212753,-7.22059770075181,
93.938078250145));
#170796=CARTESIAN_POINT('Ctrl Pts',(-3.71733620686508,-7.22503931630575,
93.938457474001));
#170797=CARTESIAN_POINT('Ctrl Pts',(-3.68967661157573,-7.23922865940013,
93.9396709915774));
#170798=CARTESIAN_POINT('Ctrl Pts',(-3.67060648474689,-7.248916686373,93.9405026426717));
#170799=CARTESIAN_POINT('Ctrl Pts',(-3.6258330165306,-7.27144056570283,
93.9424439714764));
#170800=CARTESIAN_POINT('Ctrl Pts',(-3.60009932956053,-7.28421566167321,
93.9435511130068));
#170801=CARTESIAN_POINT('Ctrl Pts',(-3.30147378708005,-7.43049469349547,
93.9563048419942));
#170802=CARTESIAN_POINT('Ctrl Pts',(-3.02135377311215,-7.54873634024201,
93.9673738301179));
#170803=CARTESIAN_POINT('Ctrl Pts',(-2.43944920029246,-7.75676879931419,
93.9896318832181));
#170804=CARTESIAN_POINT('Ctrl Pts',(-2.13775555837363,-7.84527740623423,
94.0007965906625));
#170805=CARTESIAN_POINT('Ctrl Pts',(-1.19164602508899,-8.06419634275773,
94.0358420535354));
#170806=CARTESIAN_POINT('Ctrl Pts',(-0.53603397468793,-8.13411680021638,
94.0604396781689));
#170807=CARTESIAN_POINT('Ctrl Pts',(0.239665104336485,-8.12258485979519,
94.0903955235954));
#170808=CARTESIAN_POINT('Ctrl Pts',(0.358495527963639,-8.11820822413523,
94.0950035982537));
#170809=CARTESIAN_POINT('Ctrl Pts',(0.524270408883189,-8.10845562908657,
94.1014696155473));
#170810=CARTESIAN_POINT('Ctrl Pts',(0.571329394682538,-8.10527574168545,
94.10330935506));
#170811=CARTESIAN_POINT('Ctrl Pts',(0.65677390625967,-8.0987542243183,94.1066581567038));
#170812=CARTESIAN_POINT('Ctrl Pts',(0.695168489963827,-8.09554894411697,
94.1081660327224));
#170813=CARTESIAN_POINT('Ctrl Pts',(0.768494165665619,-8.08890203938111,
94.1110520554409));
#170814=CARTESIAN_POINT('Ctrl Pts',(0.803428624046099,-8.08550690561616,
94.1124297740295));
#170815=CARTESIAN_POINT('Ctrl Pts',(0.888948745042009,-8.07663584078636,
94.1158094948154));
#170816=CARTESIAN_POINT('Ctrl Pts',(0.93950698948236,-8.07091091264257,
94.1178135852694));
#170817=CARTESIAN_POINT('Ctrl Pts',(1.10705787579913,-8.05034269877351,
94.1244764990593));
#170818=CARTESIAN_POINT('Ctrl Pts',(1.22378020424593,-8.03342743255707,
94.1291528301537));
#170819=CARTESIAN_POINT('Ctrl Pts',(1.50875887478279,-7.9857734874066,94.1406635343539));
#170820=CARTESIAN_POINT('Ctrl Pts',(1.6764915489995,-7.95225166395241,94.1475193163545));
#170821=CARTESIAN_POINT('Ctrl Pts',(2.13492130724615,-7.8454837057301,94.1664892240613));
#170822=CARTESIAN_POINT('Ctrl Pts',(2.42281623106958,-7.76140852331199,
94.1786677504523));
#170823=CARTESIAN_POINT('Ctrl Pts',(3.01965507519996,-7.5506580854287,94.204390600435));
#170824=CARTESIAN_POINT('Ctrl Pts',(3.32678602397583,-7.42046197025177,
94.2179111263362));
#170825=CARTESIAN_POINT('Ctrl Pts',(3.67356996937964,-7.24758648178896,
94.2333292001477));
#170826=CARTESIAN_POINT('Ctrl Pts',(3.72184149484221,-7.22291645301249,
94.2354787341847));
#170827=CARTESIAN_POINT('Ctrl Pts',(3.78938011786363,-7.18754278636198,
94.2384897562336));
#170828=CARTESIAN_POINT('Ctrl Pts',(3.8088558314234,-7.1772411304074,94.2393584422881));
#170829=CARTESIAN_POINT('Ctrl Pts',(3.84469072501032,-7.15809936702538,
94.2409574602725));
#170830=CARTESIAN_POINT('Ctrl Pts',(3.86106187810866,-7.14928209640021,
94.241688207567));
#170831=CARTESIAN_POINT('Ctrl Pts',(3.89293042845703,-7.13197675622056,
94.2431113334868));
#170832=CARTESIAN_POINT('Ctrl Pts',(3.90843069664883,-7.12349417519611,
94.2438038121072));
#170833=CARTESIAN_POINT('Ctrl Pts',(3.94636018847926,-7.10257604891583,
94.2454992554872));
#170834=CARTESIAN_POINT('Ctrl Pts',(3.96875847269916,-7.09008472869666,
94.2465012595828));
#170835=CARTESIAN_POINT('Ctrl Pts',(4.02096185201129,-7.06064649021562,
94.248839082556));
#170836=CARTESIAN_POINT('Ctrl Pts',(4.05071960355491,-7.04361652722853,
94.2501736149221));
#170837=CARTESIAN_POINT('Ctrl Pts',(4.1388733525322,-6.9924239007025,94.2541343625399));
#170838=CARTESIAN_POINT('Ctrl Pts',(4.1969516055638,-6.95771959319506,94.2567535095189));
#170839=CARTESIAN_POINT('Ctrl Pts',(4.44296767693062,-6.80651285286694,
94.2679074882593));
#170840=CARTESIAN_POINT('Ctrl Pts',(4.6265414970018,-6.68309012542854,94.2763835876451));
#170841=CARTESIAN_POINT('Ctrl Pts',(4.95433929213461,-6.44271465951965,
94.2920236600736));
#170842=CARTESIAN_POINT('Ctrl Pts',(5.10002929741213,-6.32801313970813,
94.2991729073603));
#170843=CARTESIAN_POINT('Ctrl Pts',(5.2831451783569,-6.17341163803696,94.3084791637397));
#170844=CARTESIAN_POINT('Ctrl Pts',(5.32427038573578,-6.13797841750926,
94.3105909299399));
#170845=CARTESIAN_POINT('Ctrl Pts',(5.3923105628403,-6.07815705369578,94.3141225691202));
#170846=CARTESIAN_POINT('Ctrl Pts',(5.41942268146581,-6.05399571889103,
94.3155400507038));
#170847=CARTESIAN_POINT('Ctrl Pts',(5.47079098675269,-6.00759655303768,
94.3182456428773));
#170848=CARTESIAN_POINT('Ctrl Pts',(5.49507585450967,-5.9853915251884,94.319533380041));
#170849=CARTESIAN_POINT('Ctrl Pts',(5.54504001266233,-5.93914607760545,
94.322201001542));
#170850=CARTESIAN_POINT('Ctrl Pts',(5.57069942198457,-5.9150851906819,94.3235810875003));
#170851=CARTESIAN_POINT('Ctrl Pts',(5.66201168794523,-5.82834030258141,
94.3285290988506));
#170852=CARTESIAN_POINT('Ctrl Pts',(5.72676903133103,-5.76472404650015,
94.3321071172336));
#170853=CARTESIAN_POINT('Ctrl Pts',(5.83822238763341,-5.65150289343008,
94.3383893736165));
#170854=CARTESIAN_POINT('Ctrl Pts',(5.88538596003253,-5.60237071619785,
94.3410884079341));
#170855=CARTESIAN_POINT('Ctrl Pts',(6.14872933151441,-5.3210396443987,94.3563905975068));
#170856=CARTESIAN_POINT('Ctrl Pts',(6.35178106232219,-5.07692920692795,
94.3691058784524));
#170857=CARTESIAN_POINT('Ctrl Pts',(6.60864429844011,-4.7285172201209,94.3863432994216));
#170858=CARTESIAN_POINT('Ctrl Pts',(6.67525793159644,-4.63400329198903,
94.390932686035));
#170859=CARTESIAN_POINT('Ctrl Pts',(6.75737771400264,-4.51204175914137,
94.396730248853));
#170860=CARTESIAN_POINT('Ctrl Pts',(6.7747718294589,-4.48588241899203,94.3979666117227));
#170861=CARTESIAN_POINT('Ctrl Pts',(6.80192898415205,-4.44452202153799,
94.3999097410327));
#170862=CARTESIAN_POINT('Ctrl Pts',(6.81179373083975,-4.42938822806896,
94.400618275963));
#170863=CARTESIAN_POINT('Ctrl Pts',(6.83180714023567,-4.39846009544633,
94.402061396736));
#170864=CARTESIAN_POINT('Ctrl Pts',(6.84195170517382,-4.38266321764517,
94.402795913185));
#170865=CARTESIAN_POINT('Ctrl Pts',(6.86312160854572,-4.34944529700583,
94.4043352422872));
#170866=CARTESIAN_POINT('Ctrl Pts',(6.87413557813542,-4.33201715854962,
94.4051398721691));
#170867=CARTESIAN_POINT('Ctrl Pts',(6.9002655692591,-4.29031935110828,94.4070581040988));
#170868=CARTESIAN_POINT('Ctrl Pts',(6.91532006909514,-4.26601141706768,
94.4081708075468));
#170869=CARTESIAN_POINT('Ctrl Pts',(6.95585551646879,-4.19978192803541,
94.4111882119207));
#170870=CARTESIAN_POINT('Ctrl Pts',(6.9810856659204,-4.15770816283401,94.413089668434));
#170871=CARTESIAN_POINT('Ctrl Pts',(7.06230665883452,-4.01944026532467,
94.4192925918609));
#170872=CARTESIAN_POINT('Ctrl Pts',(7.11670247667,-3.92232348269673,94.4235776706964));
#170873=CARTESIAN_POINT('Ctrl Pts',(7.29151932019704,-3.59459391538582,
94.4378483277363));
#170874=CARTESIAN_POINT('Ctrl Pts',(7.40285907135733,-3.35932095362181,
94.4477898999218));
#170875=CARTESIAN_POINT('Ctrl Pts',(7.59795942680543,-2.89002618666521,
94.4673169633243));
#170876=CARTESIAN_POINT('Ctrl Pts',(7.68265470320967,-2.65669971974528,
94.4768872953532));
#170877=CARTESIAN_POINT('Ctrl Pts',(7.78026772401202,-2.34381494818529,
94.489633532609));
#170878=CARTESIAN_POINT('Ctrl Pts',(7.80287426860133,-2.2674186712139,94.4927386174087));
#170879=CARTESIAN_POINT('Ctrl Pts',(7.83924191289082,-2.13752732468404,
94.4980078398094));
#170880=CARTESIAN_POINT('Ctrl Pts',(7.85358769691227,-2.08420178779168,
94.5001681864227));
#170881=CARTESIAN_POINT('Ctrl Pts',(7.87962818824257,-1.98331676804297,
94.504250251202));
#170882=CARTESIAN_POINT('Ctrl Pts',(7.89143866391432,-1.93578965378824,
94.5061712255615));
#170883=CARTESIAN_POINT('Ctrl Pts',(7.92462565439062,-1.79688673159534,
94.5117795309055));
#170884=CARTESIAN_POINT('Ctrl Pts',(7.94484967763263,-1.70524402686819,
94.515472274636));
#170885=CARTESIAN_POINT('Ctrl Pts',(7.99102255032171,-1.47732408836588,
94.5246368111807));
#170886=CARTESIAN_POINT('Ctrl Pts',(8.01507757729343,-1.3406935418348,94.5301137549015));
#170887=CARTESIAN_POINT('Ctrl Pts',(8.05471752283239,-1.07602565819084,
94.5406789793507));
#170888=CARTESIAN_POINT('Ctrl Pts',(8.07077518748635,-0.948100011774246,
94.5457658455318));
#170889=CARTESIAN_POINT('Ctrl Pts',(8.08857779114679,-0.772564218716246,
94.5527067790584));
#170890=CARTESIAN_POINT('Ctrl Pts',(8.09295816759113,-0.725240837896785,
94.5545741018293));
#170891=CARTESIAN_POINT('Ctrl Pts',(8.09998200874483,-0.641344923005015,
94.5578766013952));
#170892=CARTESIAN_POINT('Ctrl Pts',(8.1027935563917,-0.604787930219098,
94.5593128928134));
#170893=CARTESIAN_POINT('Ctrl Pts',(8.10893563513252,-0.517173357069507,
94.5627497507151));
#170894=CARTESIAN_POINT('Ctrl Pts',(8.11203152063572,-0.466100895576881,
94.5647487800398));
#170895=CARTESIAN_POINT('Ctrl Pts',(8.12171406204287,-0.276775813883193,
94.5721478635364));
#170896=CARTESIAN_POINT('Ctrl Pts',(8.12525024283596,-0.138391731887678,
94.5775341323858));
#170897=CARTESIAN_POINT('Ctrl Pts',(8.12524999998749,1.42566410947162E-5,
94.5829227676044));
#170898=CARTESIAN_POINT('',(8.12571484367965,-5.65716636902258E-7,96.5832950704718));
#170899=CARTESIAN_POINT('Ctrl Pts',(8.12456002707784,-1.23182048087137E-6,
94.5833205544621));
#170900=CARTESIAN_POINT('Ctrl Pts',(8.12402776914182,1.12776970425289,94.6275398487303));
#170901=CARTESIAN_POINT('Ctrl Pts',(7.60758318760407,3.60567669421567,94.724648298094));
#170902=CARTESIAN_POINT('Ctrl Pts',(5.15483525499198,6.72198816743881,94.8746459025528));
#170903=CARTESIAN_POINT('Ctrl Pts',(1.33775837807665,8.3503280792661,95.0333133678393));
#170904=CARTESIAN_POINT('Ctrl Pts',(-4.25467436631755,7.88859242601584,
95.2448699882213));
#170905=CARTESIAN_POINT('Ctrl Pts',(-8.30012585283032,3.35904394789376,
95.456426608603));
#170906=CARTESIAN_POINT('Ctrl Pts',(-8.15520229705827,-2.22234120788674,
95.6679832289851));
#170907=CARTESIAN_POINT('Ctrl Pts',(-5.44841867805453,-7.10570068667848,
95.8795398493668));
#170908=CARTESIAN_POINT('Ctrl Pts',(0.335793904015422,-8.95641601104346,
96.0910964697489));
#170909=CARTESIAN_POINT('Ctrl Pts',(5.38922504977475,-6.51729066085791,
96.3026530901306));
#170910=CARTESIAN_POINT('Ctrl Pts',(7.66270883609975,-3.43458399987812,
96.4490895720065));
#170911=CARTESIAN_POINT('Ctrl Pts',(8.12424186435146,-1.03981093457564,
96.542636898787));
#170912=CARTESIAN_POINT('Ctrl Pts',(8.12571484367965,-5.65716636902251E-7,
96.5832950704718));
#170913=CARTESIAN_POINT('',(8.12525,-4.14083264205223E-12,98.5832974432122));
#170914=CARTESIAN_POINT('Ctrl Pts',(8.12525,-4.42750847282105E-12,96.5832974432122));
#170915=CARTESIAN_POINT('Ctrl Pts',(8.12525000000122,2.24624642432963,96.6712950363534));
#170916=CARTESIAN_POINT('Ctrl Pts',(7.14398562317848,4.47535249753052,96.7592926294946));
#170917=CARTESIAN_POINT('Ctrl Pts',(3.83078204045361,7.50935546634141,96.935287815777));
#170918=CARTESIAN_POINT('Ctrl Pts',(1.52412477698225,8.29110090552047,97.0232854089182));
#170919=CARTESIAN_POINT('Ctrl Pts',(-2.9510162393209,7.89663306204599,97.1992805952006));
#170920=CARTESIAN_POINT('Ctrl Pts',(-5.08535169588328,6.72342983086093,
97.2872781883418));
#170921=CARTESIAN_POINT('Ctrl Pts',(-7.81671694684208,3.15661951053424,
97.4632733746242));
#170922=CARTESIAN_POINT('Ctrl Pts',(-8.39290461146651,0.790229551559375,
97.5512709677654));
#170923=CARTESIAN_POINT('Ctrl Pts',(-7.60701611462715,-3.63299000729928,
97.7272661540478));
#170924=CARTESIAN_POINT('Ctrl Pts',(-6.25093680401722,-5.65606750609613,
97.815263747189));
#170925=CARTESIAN_POINT('Ctrl Pts',(-2.45807268689086,-8.06369575488155,
97.9912589334714));
#170926=CARTESIAN_POINT('Ctrl Pts',(-0.0502299510509621,-8.42987470330081,
98.0792565266126));
#170927=CARTESIAN_POINT('Ctrl Pts',(4.28689960880504,-7.25863639434851,
98.255251712895));
#170928=CARTESIAN_POINT('Ctrl Pts',(6.18309125556768,-5.73015646266801,
98.3432493060362));
#170929=CARTESIAN_POINT('Ctrl Pts',(7.81050559202745,-2.58640713800765,
98.4819304138557));
#170930=CARTESIAN_POINT('Ctrl Pts',(8.12524999999934,-1.29375883538613,
98.5326139285339));
#170931=CARTESIAN_POINT('Ctrl Pts',(8.12525,-4.14083171691527E-12,98.5832974432122));
#170932=CARTESIAN_POINT('',(2.10208451021631,7.8486258844723,99.));
#170933=CARTESIAN_POINT('Ctrl Pts',(8.12524988254124,0.00138158011351417,
98.5832974432122));
#170934=CARTESIAN_POINT('Ctrl Pts',(8.12521252668128,0.22107618469403,98.5919091350809));
#170935=CARTESIAN_POINT('Ctrl Pts',(8.11626051648965,0.440727213117883,
98.6005208269495));
#170936=CARTESIAN_POINT('Ctrl Pts',(8.0984302060208,0.659633050043605,98.6091325188182));
#170937=CARTESIAN_POINT('Ctrl Pts',(8.08059799267019,0.878562248981262,
98.6177451297416));
#170938=CARTESIAN_POINT('Ctrl Pts',(8.05388560924342,1.09674586882328,98.6263577406649));
#170939=CARTESIAN_POINT('Ctrl Pts',(8.01838132186286,1.31348716769554,98.6349703515883));
#170940=CARTESIAN_POINT('Ctrl Pts',(7.98287816255186,1.53022158009628,98.6435826888652));
#170941=CARTESIAN_POINT('Ctrl Pts',(7.93858369612052,1.74551353666527,98.652195026142));
#170942=CARTESIAN_POINT('Ctrl Pts',(7.88563759671646,1.95867487239507,98.6608073634189));
#170943=CARTESIAN_POINT('Ctrl Pts',(7.84084602861086,2.13900601282445,98.6680932654216));
#170944=CARTESIAN_POINT('Ctrl Pts',(7.78986346722536,2.31781236312912,98.6753791674244));
#170945=CARTESIAN_POINT('Ctrl Pts',(7.73280286670696,2.49468382508658,98.6826650694271));
#170946=CARTESIAN_POINT('Ctrl Pts',(7.66976526129178,2.69008228438749,98.6907141577887));
#170947=CARTESIAN_POINT('Ctrl Pts',(7.59929130474582,2.88317067675791,98.6987632461504));
#170948=CARTESIAN_POINT('Ctrl Pts',(7.52157620346321,3.07336606638323,98.7068123345121));
#170949=CARTESIAN_POINT('Ctrl Pts',(7.44388876653266,3.26349375189272,98.7148585576286));
#170950=CARTESIAN_POINT('Ctrl Pts',(7.35896544557454,3.45073019344213,98.7229047807452));
#170951=CARTESIAN_POINT('Ctrl Pts',(7.26705019905045,3.63451082911867,98.7309510038617));
#170952=CARTESIAN_POINT('Ctrl Pts',(7.17515588441129,3.81824961237937,98.7389953946096));
#170953=CARTESIAN_POINT('Ctrl Pts',(7.07627296281827,3.99853387452038,98.7470397853575));
#170954=CARTESIAN_POINT('Ctrl Pts',(6.97069236811693,4.17482160955128,98.7550841761054));
#170955=CARTESIAN_POINT('Ctrl Pts',(6.86510685785221,4.3511175520898,98.7631289413796));
#170956=CARTESIAN_POINT('Ctrl Pts',(6.75282321108776,4.52341631961701,98.7711737066538));
#170957=CARTESIAN_POINT('Ctrl Pts',(6.63417734572678,4.69120224547456,98.779218471928));
#170958=CARTESIAN_POINT('Ctrl Pts',(6.51553126712269,4.85898847289503,98.7872632516612));
#170959=CARTESIAN_POINT('Ctrl Pts',(6.39052313404091,5.02226158400115,98.7953080313943));
#170960=CARTESIAN_POINT('Ctrl Pts',(6.25953120194918,5.18053633269033,98.8033528111274));
#170961=CARTESIAN_POINT('Ctrl Pts',(6.12849303100207,5.3388669507991,98.8114004305882));
#170962=CARTESIAN_POINT('Ctrl Pts',(5.99146704521336,5.49219543623203,98.8194480500489));
#170963=CARTESIAN_POINT('Ctrl Pts',(5.84887129471538,5.64007022477154,98.8274956695097));
#170964=CARTESIAN_POINT('Ctrl Pts',(5.76714616726557,5.72482089860158,98.832107957911));
#170965=CARTESIAN_POINT('Ctrl Pts',(5.68359223740185,5.80778083579945,98.8367202463123));
#170966=CARTESIAN_POINT('Ctrl Pts',(5.59829361147862,5.88887053705358,98.8413325347136));
#170967=CARTESIAN_POINT('Ctrl Pts',(5.44430442793545,6.03526136990382,98.8496590759386));
#170968=CARTESIAN_POINT('Ctrl Pts',(5.28455978604005,6.17561896389448,98.8579856171636));
#170969=CARTESIAN_POINT('Ctrl Pts',(5.11955079439096,6.30950768492684,98.8663121583885));
#170970=CARTESIAN_POINT('Ctrl Pts',(4.95456136904949,6.44338052980679,98.8746377122754));
#170971=CARTESIAN_POINT('Ctrl Pts',(4.78430905737275,6.57078585768088,98.8829632661622));
#170972=CARTESIAN_POINT('Ctrl Pts',(4.60931796522703,6.69132837767923,98.8912888200491));
#170973=CARTESIAN_POINT('Ctrl Pts',(4.43434348814969,6.81185945239664,98.8996135834406));
#170974=CARTESIAN_POINT('Ctrl Pts',(4.25463135912899,6.92552886226729,98.9079383468321));
#170975=CARTESIAN_POINT('Ctrl Pts',(4.07073537364008,7.03198414960496,98.9162631102236));
#170976=CARTESIAN_POINT('Ctrl Pts',(3.88683996800717,7.1384391012706,98.9245878473657));
#170977=CARTESIAN_POINT('Ctrl Pts',(3.69876097291084,7.23767983421501,98.9329125845077));
#170978=CARTESIAN_POINT('Ctrl Pts',(3.50707849817467,7.32939888190982,98.9412373216498));
#170979=CARTESIAN_POINT('Ctrl Pts',(3.31541142408727,7.42111056047585,98.9495613899443));
#170980=CARTESIAN_POINT('Ctrl Pts',(3.12014170101451,7.50530164139812,98.9578854582389));
#170981=CARTESIAN_POINT('Ctrl Pts',(2.92187192055566,7.58171168288325,98.9662095265334));
#170982=CARTESIAN_POINT('Ctrl Pts',(2.72360002813004,7.65812253828702,98.9745336834958));
#170983=CARTESIAN_POINT('Ctrl Pts',(2.52232827478524,7.7267520876479,98.9828578404582));
#170984=CARTESIAN_POINT('Ctrl Pts',(2.31867805317345,7.78738849989082,98.9911819974205));
#170985=CARTESIAN_POINT('Ctrl Pts',(2.24676734046914,7.80879975879204,98.9941213316137));
#170986=CARTESIAN_POINT('Ctrl Pts',(2.17456021842664,7.82921483522134,98.9970606658068));
#170987=CARTESIAN_POINT('Ctrl Pts',(2.10208451021631,7.8486258844723,99.));
#170988=CARTESIAN_POINT('',(-2.10208451021626,7.84862588447232,99.));
#170989=CARTESIAN_POINT('Origin',(0.,0.,99.));
#170990=CARTESIAN_POINT('',(8.13159794993647,-0.00671758913982503,98.4167025567874));
#170991=CARTESIAN_POINT('Ctrl Pts',(8.12525,-4.14083309504467E-12,98.4167025567874));
#170992=CARTESIAN_POINT('Ctrl Pts',(8.12525000000114,2.24624642432976,98.5047001499286));
#170993=CARTESIAN_POINT('Ctrl Pts',(7.14398562317847,4.47535249753047,98.5926977430698));
#170994=CARTESIAN_POINT('Ctrl Pts',(3.83078204045389,7.50935546634122,98.7686929293522));
#170995=CARTESIAN_POINT('Ctrl Pts',(1.52412477698275,8.29110090552034,98.8566905224934));
#170996=CARTESIAN_POINT('Ctrl Pts',(-1.1822624975838,8.05254244492327,98.9631254104231));
#170997=CARTESIAN_POINT('Ctrl Pts',(-1.6474727139843,7.97038381115747,98.9815627052115));
#170998=CARTESIAN_POINT('Ctrl Pts',(-2.10208451021626,7.84862588447232,
99.));
#170999=CARTESIAN_POINT('',(8.13064101234909,0.00726150239357421,96.4167025567874));
#171000=CARTESIAN_POINT('Ctrl Pts',(8.13064101234909,0.00726150239357421,
96.4167025567874));
#171001=CARTESIAN_POINT('Ctrl Pts',(8.13264513995559,0.458958580512804,
96.4344080025745));
#171002=CARTESIAN_POINT('Ctrl Pts',(7.88034319623196,3.60392890591984,96.5578917585526));
#171003=CARTESIAN_POINT('Ctrl Pts',(4.76217654495404,7.59287955017989,96.734264669626));
#171004=CARTESIAN_POINT('Ctrl Pts',(-0.787795848183394,8.42010700031842,
96.945821290008));
#171005=CARTESIAN_POINT('Ctrl Pts',(-4.70369331914029,7.04503919375108,
97.1044887552944));
#171006=CARTESIAN_POINT('Ctrl Pts',(-7.50785040472023,3.92613790885546,
97.2631562205808));
#171007=CARTESIAN_POINT('Ctrl Pts',(-8.46487839372023,-0.13681273072905,
97.4218236858673));
#171008=CARTESIAN_POINT('Ctrl Pts',(-7.37643864316404,-4.16414405786197,
97.5804911511536));
#171009=CARTESIAN_POINT('Ctrl Pts',(-4.4775289435207,-7.19508636046639,
97.7391586164401));
#171010=CARTESIAN_POINT('Ctrl Pts',(-0.510988490918713,-8.43710679026292,
97.8978260817266));
#171011=CARTESIAN_POINT('Ctrl Pts',(4.99171475646089,-7.44423893657541,
98.1093827021084));
#171012=CARTESIAN_POINT('Ctrl Pts',(7.94889191739487,-3.41866176302103,
98.2823415271287));
#171013=CARTESIAN_POINT('Ctrl Pts',(8.13566645843371,-0.371006238498034,
98.4024111970536));
#171014=CARTESIAN_POINT('Ctrl Pts',(8.13267765453462,-0.00786016460921045,
98.4167025567874));
#171015=CARTESIAN_POINT('',(8.12524935171145,-0.00324576840847315,92.4142818892175));
#171016=CARTESIAN_POINT('Ctrl Pts',(8.1252466584585,0.00736896933301007,
96.4135943073787));
#171017=CARTESIAN_POINT('Ctrl Pts',(8.12590323294949,-0.716589761930001,
96.3874241345655));
#171018=CARTESIAN_POINT('Ctrl Pts',(8.02980597704607,-1.43739644121946,
96.3618774763689));
#171019=CARTESIAN_POINT('Ctrl Pts',(7.8200332504233,-2.20731470784607,96.3315156398167));
#171020=CARTESIAN_POINT('Ctrl Pts',(7.79961632700026,-2.27840804917313,
96.3286862987029));
#171021=CARTESIAN_POINT('Ctrl Pts',(7.76661022777492,-2.38769110653584,
96.3242963068922));
#171022=CARTESIAN_POINT('Ctrl Pts',(7.75470334917227,-2.42608309630499,
96.3227462405774));
#171023=CARTESIAN_POINT('Ctrl Pts',(7.73176683133274,-2.49814418573916,
96.3198219929881));
#171024=CARTESIAN_POINT('Ctrl Pts',(7.72080088515683,-2.53183261314967,
96.3184487876053));
#171025=CARTESIAN_POINT('Ctrl Pts',(7.70225148961179,-2.58757675261307,
96.3161663991105));
#171026=CARTESIAN_POINT('Ctrl Pts',(7.69479275609644,-2.60967352283208,
96.3152590113286));
#171027=CARTESIAN_POINT('Ctrl Pts',(7.68014130838278,-2.65247002760309,
96.3134964652409));
#171028=CARTESIAN_POINT('Ctrl Pts',(7.67295977493772,-2.67317340499203,
96.3126414793574));
#171029=CARTESIAN_POINT('Ctrl Pts',(7.65650346900041,-2.7200019720856,96.3107021738355));
#171030=CARTESIAN_POINT('Ctrl Pts',(7.64717857877076,-2.74610922487601,
96.3096171501307));
#171031=CARTESIAN_POINT('Ctrl Pts',(7.61915204229363,-2.82332634622982,
96.3063961535349));
#171032=CARTESIAN_POINT('Ctrl Pts',(7.60007038372069,-2.87429636535933,
96.3042545846267));
#171033=CARTESIAN_POINT('Ctrl Pts',(7.41331266597301,-3.35828907136431,
96.2837624747453));
#171034=CARTESIAN_POINT('Ctrl Pts',(7.20932935675875,-3.77635202364663,
96.2647893508854));
#171035=CARTESIAN_POINT('Ctrl Pts',(6.8412628694122,-4.3909394887513,96.234717312196));
#171036=CARTESIAN_POINT('Ctrl Pts',(6.70175925037647,-4.60104848629454,
96.224014954117));
#171037=CARTESIAN_POINT('Ctrl Pts',(6.44179153901747,-4.95562344431865,
96.205359532329));
#171038=CARTESIAN_POINT('Ctrl Pts',(6.32565802367751,-5.10303183711418,
96.197410431286));
#171039=CARTESIAN_POINT('Ctrl Pts',(6.05620881317575,-5.42169601839635,
96.179927731469));
#171040=CARTESIAN_POINT('Ctrl Pts',(5.90051415337845,-5.59074179858677,
96.1704456528119));
#171041=CARTESIAN_POINT('Ctrl Pts',(5.7225002426769,-5.76828823659543,96.1604235084261));
#171042=CARTESIAN_POINT('Ctrl Pts',(5.70707847459305,-5.78354679268849,
96.1595616849925));
#171043=CARTESIAN_POINT('Ctrl Pts',(5.68587522695687,-5.80435825180994,
96.1583857334037));
#171044=CARTESIAN_POINT('Ctrl Pts',(5.68014644055117,-5.8099645632584,96.1580688994498));
#171045=CARTESIAN_POINT('Ctrl Pts',(5.66936982645228,-5.82047961161557,
96.1574745757998));
#171046=CARTESIAN_POINT('Ctrl Pts',(5.66432389844026,-5.82539027982304,
96.1571969864832));
#171047=CARTESIAN_POINT('Ctrl Pts',(5.65382391381546,-5.83558226338742,
96.1566207997966));
#171048=CARTESIAN_POINT('Ctrl Pts',(5.64836882349238,-5.84086250783859,
96.1563222585658));
#171049=CARTESIAN_POINT('Ctrl Pts',(5.63578987717447,-5.85300417313695,
96.1556357201409));
#171050=CARTESIAN_POINT('Ctrl Pts',(5.62866086873989,-5.8598602556906,96.1552480073913));
#171051=CARTESIAN_POINT('Ctrl Pts',(5.60649334221101,-5.88110134668094,
96.1540467335736));
#171052=CARTESIAN_POINT('Ctrl Pts',(5.59141199376807,-5.89544167748034,
96.1532356037871));
#171053=CARTESIAN_POINT('Ctrl Pts',(5.41788291487671,-6.05917960744128,
96.1439742893054));
#171054=CARTESIAN_POINT('Ctrl Pts',(5.25355147410591,-6.20220189559256,
96.1359314263433));
#171055=CARTESIAN_POINT('Ctrl Pts',(4.84747804800057,-6.52788759979342,
96.1173597964537));
#171056=CARTESIAN_POINT('Ctrl Pts',(4.60087263335696,-6.70397974772862,
96.1070744403398));
#171057=CARTESIAN_POINT('Ctrl Pts',(4.13040137264405,-7.00171208689419,
96.0883128421078));
#171058=CARTESIAN_POINT('Ctrl Pts',(3.90954649251,-7.12738614042152,96.0798226996423));
#171059=CARTESIAN_POINT('Ctrl Pts',(3.19746122590257,-7.48951635998182,
96.052668199623));
#171060=CARTESIAN_POINT('Ctrl Pts',(2.68819152705082,-7.6870125316506,96.0334640924608));
#171061=CARTESIAN_POINT('Ctrl Pts',(2.13580299627479,-7.83956823180263,
96.0113870163092));
#171062=CARTESIAN_POINT('Ctrl Pts',(2.10855277275215,-7.84694142233613,
96.010295155754));
#171063=CARTESIAN_POINT('Ctrl Pts',(2.06878924091098,-7.85747829832295,
96.0086977673924));
#171064=CARTESIAN_POINT('Ctrl Pts',(2.05630581943573,-7.86075444897327,
96.008195687338));
#171065=CARTESIAN_POINT('Ctrl Pts',(2.03440785833882,-7.86644562008079,
96.0073139038205));
#171066=CARTESIAN_POINT('Ctrl Pts',(2.02499667797925,-7.86887352046825,
96.0069345954987));
#171067=CARTESIAN_POINT('Ctrl Pts',(2.00673251509985,-7.87355038139605,
96.0061978105488));
#171068=CARTESIAN_POINT('Ctrl Pts',(1.99788004914798,-7.87580131187464,
96.0058403948314));
#171069=CARTESIAN_POINT('Ctrl Pts',(1.97676499633044,-7.88113237866811,
96.0049871528677));
#171070=CARTESIAN_POINT('Ctrl Pts',(1.96449899570235,-7.88419882517905,
96.0044909091146));
#171071=CARTESIAN_POINT('Ctrl Pts',(1.92747884955554,-7.8933619443263,96.0029914101063));
#171072=CARTESIAN_POINT('Ctrl Pts',(1.90270322619867,-7.8993707292612,96.0019854758301));
#171073=CARTESIAN_POINT('Ctrl Pts',(1.64789176958249,-7.95990134213067,
95.9916146223507));
#171074=CARTESIAN_POINT('Ctrl Pts',(1.41562248159417,-8.00447238686052,
95.981947227185));
#171075=CARTESIAN_POINT('Ctrl Pts',(0.539940577329719,-8.13320200119173,
95.9446926258298));
#171076=CARTESIAN_POINT('Ctrl Pts',(-0.110812074463072,-8.15034131647273,
95.9151948725943));
#171077=CARTESIAN_POINT('Ctrl Pts',(-1.06398572468673,-8.06120031822383,
95.8721806059189));
#171078=CARTESIAN_POINT('Ctrl Pts',(-1.36952570606803,-8.01495071254373,
95.8584649652962));
#171079=CARTESIAN_POINT('Ctrl Pts',(-1.78268547537017,-7.92808812187126,
95.8405488891613));
#171080=CARTESIAN_POINT('Ctrl Pts',(-1.89316991355354,-7.90243369382721,
95.8358215702062));
#171081=CARTESIAN_POINT('Ctrl Pts',(-2.04153632824587,-7.86469269397984,
95.829588414464));
#171082=CARTESIAN_POINT('Ctrl Pts',(-2.0799146307956,-7.85463028701927,
95.8279868684712));
#171083=CARTESIAN_POINT('Ctrl Pts',(-2.14535436763218,-7.83695937141752,
95.8252738552663));
#171084=CARTESIAN_POINT('Ctrl Pts',(-2.17245126433044,-7.82949124049688,
95.8241555805646));
#171085=CARTESIAN_POINT('Ctrl Pts',(-2.2100709004257,-7.81891261939912,
95.8226094801085));
#171086=CARTESIAN_POINT('Ctrl Pts',(-2.22062670359331,-7.81592124957927,
95.8221763623739));
#171087=CARTESIAN_POINT('Ctrl Pts',(-2.23759642112233,-7.81107511140476,
95.8214811656711));
#171088=CARTESIAN_POINT('Ctrl Pts',(-2.24401414208078,-7.80923380814827,
95.8212185030776));
#171089=CARTESIAN_POINT('Ctrl Pts',(-2.25740695536677,-7.80537341379034,
95.8206708778199));
#171090=CARTESIAN_POINT('Ctrl Pts',(-2.26438162754039,-7.80335287784375,
95.8203859771821));
#171091=CARTESIAN_POINT('Ctrl Pts',(-2.28045233928751,-7.79867389339832,
95.8197301725536));
#171092=CARTESIAN_POINT('Ctrl Pts',(-2.28954646550092,-7.79600887317518,
95.819359545004));
#171093=CARTESIAN_POINT('Ctrl Pts',(-2.31855225387609,-7.78745363875872,
95.8181789013846));
#171094=CARTESIAN_POINT('Ctrl Pts',(-2.33844609857104,-7.7815029771781,
95.8173713693193));
#171095=CARTESIAN_POINT('Ctrl Pts',(-2.52903151197649,-7.72369805045132,
95.8096546258882));
#171096=CARTESIAN_POINT('Ctrl Pts',(-2.69800142772722,-7.66630973680929,
95.802962131267));
#171097=CARTESIAN_POINT('Ctrl Pts',(-3.47677344769397,-7.37286968249113,
95.7722967750393));
#171098=CARTESIAN_POINT('Ctrl Pts',(-4.05855087043088,-7.06932897060372,
95.7496177583046));
#171099=CARTESIAN_POINT('Ctrl Pts',(-4.82773779382544,-6.54144401680282,
95.7152881181103));
#171100=CARTESIAN_POINT('Ctrl Pts',(-5.04950289487799,-6.37181725099528,
95.7048394886654));
#171101=CARTESIAN_POINT('Ctrl Pts',(-5.46136646771455,-6.02175694730635,
95.6842685184291));
#171102=CARTESIAN_POINT('Ctrl Pts',(-5.65234061166466,-5.8428693511192,
95.674204185728));
#171103=CARTESIAN_POINT('Ctrl Pts',(-5.88810219951548,-5.59963431937994,
95.6610633949834));
#171104=CARTESIAN_POINT('Ctrl Pts',(-5.94105980101686,-5.54341594685729,
95.6580593110513));
#171105=CARTESIAN_POINT('Ctrl Pts',(-6.02242793716618,-5.45453224050368,
95.6533576607653));
#171106=CARTESIAN_POINT('Ctrl Pts',(-6.05139265876349,-5.42238020533149,
95.6516664509385));
#171107=CARTESIAN_POINT('Ctrl Pts',(-6.10496004389695,-5.36195439734099,
95.6485051141478));
#171108=CARTESIAN_POINT('Ctrl Pts',(-6.12962663208127,-5.33373878579804,
95.6470357581051));
#171109=CARTESIAN_POINT('Ctrl Pts',(-6.1843747156451,-5.27023217599949,
95.6437433563248));
#171110=CARTESIAN_POINT('Ctrl Pts',(-6.21435105878343,-5.23485230983879,
95.6419191858602));
#171111=CARTESIAN_POINT('Ctrl Pts',(-6.30111174685808,-5.13065669283656,
95.6365751930641));
#171112=CARTESIAN_POINT('Ctrl Pts',(-6.35706724401277,-5.06116026460026,
95.6330463751458));
#171113=CARTESIAN_POINT('Ctrl Pts',(-6.74188379643628,-4.56676783870095,
95.6081770383364));
#171114=CARTESIAN_POINT('Ctrl Pts',(-7.02902650934413,-4.11109780259688,
95.5863854270459));
#171115=CARTESIAN_POINT('Ctrl Pts',(-7.41043995555299,-3.34741080956153,
95.5517012850208));
#171116=CARTESIAN_POINT('Ctrl Pts',(-7.53514955309206,-3.05635517404504,
95.5388792982535));
#171117=CARTESIAN_POINT('Ctrl Pts',(-7.66091133206201,-2.7079591785244,
95.524146037038));
#171118=CARTESIAN_POINT('Ctrl Pts',(-7.67874457654431,-2.65696954202366,
95.5220048793949));
#171119=CARTESIAN_POINT('Ctrl Pts',(-7.70358968506312,-2.58359121735076,
95.5189464652119));
#171120=CARTESIAN_POINT('Ctrl Pts',(-7.71101503735957,-2.5613443179146,
95.5180222118676));
#171121=CARTESIAN_POINT('Ctrl Pts',(-7.72400475790899,-2.52185769139282,
95.5163871683278));
#171122=CARTESIAN_POINT('Ctrl Pts',(-7.72960797905781,-2.50463095261046,
95.5156756759298));
#171123=CARTESIAN_POINT('Ctrl Pts',(-7.74173907873626,-2.46690623495975,
95.5141213702457));
#171124=CARTESIAN_POINT('Ctrl Pts',(-7.74824326129995,-2.44640076508538,
95.513278957571));
#171125=CARTESIAN_POINT('Ctrl Pts',(-7.76628925959023,-2.38871395249166,
95.51091547035));
#171126=CARTESIAN_POINT('Ctrl Pts',(-7.77764542408482,-2.35147504561999,
95.5093972287453));
#171127=CARTESIAN_POINT('Ctrl Pts',(-7.85579281893262,-2.08845505861087,
95.4987203323771));
#171128=CARTESIAN_POINT('Ctrl Pts',(-7.91301066549013,-1.8599435527455,
95.4896807333021));
#171129=CARTESIAN_POINT('Ctrl Pts',(-7.99359042092224,-1.4662496660108,
95.4742337862524));
#171130=CARTESIAN_POINT('Ctrl Pts',(-8.02194070821344,-1.30224529989528,
95.4678368104537));
#171131=CARTESIAN_POINT('Ctrl Pts',(-8.06021267316544,-1.03155473030517,
95.4572760987396));
#171132=CARTESIAN_POINT('Ctrl Pts',(-8.07309627064354,-0.925337709988211,
95.4531318298419));
#171133=CARTESIAN_POINT('Ctrl Pts',(-8.08845378160931,-0.773733624426063,
95.4472060347446));
#171134=CARTESIAN_POINT('Ctrl Pts',(-8.09265033258577,-0.728531998548076,
95.4454379120988));
#171135=CARTESIAN_POINT('Ctrl Pts',(-8.09647177983796,-0.683251259024802,
95.4436649748077));
#171136=CARTESIAN_POINT('Ctrl Pts',(-8.09647569822461,-0.683204824873072,
95.4436631567075));
#171137=CARTESIAN_POINT('Ctrl Pts',(-8.09648353815878,-0.683111909572502,
95.4436595186634));
#171138=CARTESIAN_POINT('Ctrl Pts',(-8.09648745969328,-0.683065428568405,
95.4436576987251));
#171139=CARTESIAN_POINT('Ctrl Pts',(-8.0964953058797,-0.682972420049493,
95.4436540570239));
#171140=CARTESIAN_POINT('Ctrl Pts',(-8.09649923055314,-0.682925892269909,
95.4436522352505));
#171141=CARTESIAN_POINT('Ctrl Pts',(-8.09650708306364,-0.682832789623486,
95.4436485898565));
#171142=CARTESIAN_POINT('Ctrl Pts',(-8.0965110108964,-0.68278621479787,
95.4436467662375));
#171143=CARTESIAN_POINT('Ctrl Pts',(-8.0965188697338,-0.682693017932335,
95.4436431171471));
#171144=CARTESIAN_POINT('Ctrl Pts',(-8.09652280073543,-0.682646395918386,
95.4436412916768));
#171145=CARTESIAN_POINT('Ctrl Pts',(-8.09653066593017,-0.682553104414559,
95.4436376388736));
#171146=CARTESIAN_POINT('Ctrl Pts',(-8.09653460011634,-0.682506434997056,
95.4436358115436));
#171147=CARTESIAN_POINT('Ctrl Pts',(-8.09654247168501,-0.682413048599427,
95.4436321550175));
#171148=CARTESIAN_POINT('Ctrl Pts',(-8.09654640906959,-0.682366331584664,
95.4436303258202));
#171149=CARTESIAN_POINT('Ctrl Pts',(-8.09655428701372,-0.682272850216289,
95.4436266655683));
#171150=CARTESIAN_POINT('Ctrl Pts',(-8.09655822759182,-0.682226085632625,
95.4436248345047));
#171151=CARTESIAN_POINT('Ctrl Pts',(-8.09656611197868,-0.682132508436122,
95.4436211704934));
#171152=CARTESIAN_POINT('Ctrl Pts',(-8.096570055774,-0.682085695972843,
95.4436193375514));
#171153=CARTESIAN_POINT('Ctrl Pts',(-8.09657794661128,-0.681992022797499,
95.4436156697747));
#171154=CARTESIAN_POINT('Ctrl Pts',(-8.09658189364436,-0.681945162180716,
95.4436138349436));
#171155=CARTESIAN_POINT('Ctrl Pts',(-8.09658979091413,-0.6818513931797,
95.4436101634075));
#171156=CARTESIAN_POINT('Ctrl Pts',(-8.09659374117379,-0.681804484512607,
95.4436083266913));
#171157=CARTESIAN_POINT('Ctrl Pts',(-8.09660164495274,-0.681710618715257,
95.4436046513577));
#171158=CARTESIAN_POINT('Ctrl Pts',(-8.09660559845918,-0.681663661727685,
95.4436028127458));
#171159=CARTESIAN_POINT('Ctrl Pts',(-8.09661350875774,-0.681569698950048,
95.4435991336075));
#171160=CARTESIAN_POINT('Ctrl Pts',(-8.0966174655273,-0.68152269341782,
95.4435972930912));
#171161=CARTESIAN_POINT('Ctrl Pts',(-8.0966253823785,-0.681428633206755,
95.4435936101305));
#171162=CARTESIAN_POINT('Ctrl Pts',(-8.09662934244232,-0.681381578729407,
95.443591767694));
#171163=CARTESIAN_POINT('Ctrl Pts',(-8.09663726578714,-0.681287421725458,
95.4435880809358));
#171164=CARTESIAN_POINT('Ctrl Pts',(-8.09664122911381,-0.681240318645962,
95.4435862365926));
#171165=CARTESIAN_POINT('Ctrl Pts',(-8.09664915908324,-0.681146063231411,
95.4435825459737));
#171166=CARTESIAN_POINT('Ctrl Pts',(-8.09665312570642,-0.68109891111903,
95.4435806997068));
#171167=CARTESIAN_POINT('Ctrl Pts',(-8.09666106229329,-0.681004557317679,
95.4435770052281));
#171168=CARTESIAN_POINT('Ctrl Pts',(-8.09666503223838,-0.680957355839471,
95.4435751570246));
#171169=CARTESIAN_POINT('Ctrl Pts',(-8.09667297541666,-0.680862903899152,
95.4435714586957));
#171170=CARTESIAN_POINT('Ctrl Pts',(-8.09667694867352,-0.680815653145048,
95.4435696085589));
#171171=CARTESIAN_POINT('Ctrl Pts',(-8.0966848985099,-0.68072110221058,
95.4435659063464));
#171172=CARTESIAN_POINT('Ctrl Pts',(-8.09668887509022,-0.680673802010453,
95.4435640542698));
#171173=CARTESIAN_POINT('Ctrl Pts',(-8.09669683162049,-0.680579151594057,
95.4435603481544));
#171174=CARTESIAN_POINT('Ctrl Pts',(-8.09670081154848,-0.680531801628782,
95.4435584941255));
#171175=CARTESIAN_POINT('Ctrl Pts',(-8.0967087747729,-0.680437051664694,
95.4435547841047));
#171176=CARTESIAN_POINT('Ctrl Pts',(-8.09671275806207,-0.680389651741915,
95.4435529281159));
#171177=CARTESIAN_POINT('Ctrl Pts',(-8.09672072799703,-0.680294801972369,
95.4435492141796));
#171178=CARTESIAN_POINT('Ctrl Pts',(-8.09672471465569,-0.680247351961756,
95.4435473562257));
#171179=CARTESIAN_POINT('Ctrl Pts',(-8.09673269131513,-0.680152402157842,
95.443543638365));
#171180=CARTESIAN_POINT('Ctrl Pts',(-8.0967366813387,-0.680104902082411,
95.443541778447));
#171181=CARTESIAN_POINT('Ctrl Pts',(-8.09969937347417,-0.644831188649415,
95.4421605957805));
#171182=CARTESIAN_POINT('Ctrl Pts',(-8.10242815214566,-0.609586115160366,
95.4407794897809));
#171183=CARTESIAN_POINT('Ctrl Pts',(-8.10767547243135,-0.535535378499249,
95.4378752338732));
#171184=CARTESIAN_POINT('Ctrl Pts',(-8.11014560882525,-0.496727186674533,
95.4363517322204));
#171185=CARTESIAN_POINT('Ctrl Pts',(-8.11601353655642,-0.392769310157494,
95.4322663123271));
#171186=CARTESIAN_POINT('Ctrl Pts',(-8.11890543664851,-0.327594114750407,
95.4297004439459));
#171187=CARTESIAN_POINT('Ctrl Pts',(-8.13336579607254,0.119953897322484,
95.412046417264));
#171188=CARTESIAN_POINT('Ctrl Pts',(-8.11870198341614,0.50269035343553,
95.3967416973508));
#171189=CARTESIAN_POINT('Ctrl Pts',(-8.06543350083459,0.989980035517573,
95.3771830144089));
#171190=CARTESIAN_POINT('Ctrl Pts',(-8.05160841328838,1.0967589566312,95.3728951412479));
#171191=CARTESIAN_POINT('Ctrl Pts',(-8.02586100660651,1.26871045561272,
95.3660016895167));
#171192=CARTESIAN_POINT('Ctrl Pts',(-8.01525648259005,1.33406698911411,
95.3633843337835));
#171193=CARTESIAN_POINT('Ctrl Pts',(-7.9994898779356,1.42425121339564,95.3597800762875));
#171194=CARTESIAN_POINT('Ctrl Pts',(-7.99500866816353,1.44919502921509,
95.3587839786189));
#171195=CARTESIAN_POINT('Ctrl Pts',(-7.98719229398234,1.49156345442184,
95.3570936327472));
#171196=CARTESIAN_POINT('Ctrl Pts',(-7.98391664570556,1.50899876618673,
95.3563984641469));
#171197=CARTESIAN_POINT('Ctrl Pts',(-7.9769079915668,1.54564204504393,95.3549382289603));
#171198=CARTESIAN_POINT('Ctrl Pts',(-7.97316264757994,1.56484754383909,
95.3541733410966));
#171199=CARTESIAN_POINT('Ctrl Pts',(-7.96242996028624,1.61884400481386,
95.3520238756442));
#171200=CARTESIAN_POINT('Ctrl Pts',(-7.955284011717,1.65360306387427,95.3506414014832));
#171201=CARTESIAN_POINT('Ctrl Pts',(-7.92152226232347,1.81253991893322,
95.3443231450896));
#171202=CARTESIAN_POINT('Ctrl Pts',(-7.89222490437997,1.9361307983205,95.3394186260104));
#171203=CARTESIAN_POINT('Ctrl Pts',(-7.76599481349782,2.41800604682047,
95.3202443616812));
#171204=CARTESIAN_POINT('Ctrl Pts',(-7.6474592633979,2.77016187275368,95.3061005780106));
#171205=CARTESIAN_POINT('Ctrl Pts',(-7.43132567193435,3.29125120820879,
95.2843655672264));
#171206=CARTESIAN_POINT('Ctrl Pts',(-7.3510559341734,3.46683014989748,95.2768985738719));
#171207=CARTESIAN_POINT('Ctrl Pts',(-7.23194987155557,3.70457905097755,
95.2665478925648));
#171208=CARTESIAN_POINT('Ctrl Pts',(-7.19841218491012,3.76933241301281,
95.2637037068278));
#171209=CARTESIAN_POINT('Ctrl Pts',(-7.13809656030164,3.88204598050795,
95.258707328456));
#171210=CARTESIAN_POINT('Ctrl Pts',(-7.11169539030135,3.93020255814595,
95.2565577823005));
#171211=CARTESIAN_POINT('Ctrl Pts',(-7.05397386699905,4.03300218201322,
95.2519367070545));
#171212=CARTESIAN_POINT('Ctrl Pts',(-7.02250226796445,4.08755621092475,
95.2494643844854));
#171213=CARTESIAN_POINT('Ctrl Pts',(-6.91427230551962,4.27022603855155,
95.2411179796271));
#171214=CARTESIAN_POINT('Ctrl Pts',(-6.83461714547703,4.39658959981555,
95.2352295324915));
#171215=CARTESIAN_POINT('Ctrl Pts',(-6.65960295658383,4.65796869777095,
95.2228131515243));
#171216=CARTESIAN_POINT('Ctrl Pts',(-6.56351490662453,4.79241652527088,
95.2162864868903));
#171217=CARTESIAN_POINT('Ctrl Pts',(-6.42775307631851,4.97062744775441,
95.2074634203575));
#171218=CARTESIAN_POINT('Ctrl Pts',(-6.39160423582731,5.01702523015997,
95.2051499608261));
#171219=CARTESIAN_POINT('Ctrl Pts',(-6.33036988774553,5.0938846952232,95.2012918220174));
#171220=CARTESIAN_POINT('Ctrl Pts',(-6.30556060766926,5.12456336074595,
95.199744962259));
#171221=CARTESIAN_POINT('Ctrl Pts',(-6.24762565895189,5.19514684473642,
95.1961695235155));
#171222=CARTESIAN_POINT('Ctrl Pts',(-6.21433944867187,5.23491760704113,
95.1941423124497));
#171223=CARTESIAN_POINT('Ctrl Pts',(-6.10786546506377,5.35968728106748,
95.1877378617262));
#171224=CARTESIAN_POINT('Ctrl Pts',(-6.03329717802386,5.44349093541879,
95.1833695156871));
#171225=CARTESIAN_POINT('Ctrl Pts',(-5.88609241158617,5.60218532463918,
95.1749415368995));
#171226=CARTESIAN_POINT('Ctrl Pts',(-5.81370153745601,5.67727387934029,
95.1708825601207));
#171227=CARTESIAN_POINT('Ctrl Pts',(-5.65943182347899,5.83124683678178,
95.162389623468));
#171228=CARTESIAN_POINT('Ctrl Pts',(-5.57730232749082,5.9098482930487,95.1579556725355));
#171229=CARTESIAN_POINT('Ctrl Pts',(-5.44962052375443,6.02701241512375,
95.1511790849693));
#171230=CARTESIAN_POINT('Ctrl Pts',(-5.40524763783641,6.0668394118841,95.1488447130368));
#171231=CARTESIAN_POINT('Ctrl Pts',(-5.31891794921337,6.14262584314597,
95.1443404496858));
#171232=CARTESIAN_POINT('Ctrl Pts',(-5.27702473755612,6.1786527894317,95.1421711646499));
#171233=CARTESIAN_POINT('Ctrl Pts',(-5.18365868673933,6.25730260170525,
95.1373711044285));
#171234=CARTESIAN_POINT('Ctrl Pts',(-5.13202091270545,6.29972336946721,
95.1347390177204));
#171235=CARTESIAN_POINT('Ctrl Pts',(-4.93175045715165,6.46015019304431,
95.1246131489552));
#171236=CARTESIAN_POINT('Ctrl Pts',(-4.77952493669337,6.57357158384015,
95.1170863150176));
#171237=CARTESIAN_POINT('Ctrl Pts',(-4.32507020188464,6.88804277716103,
95.0950678291337));
#171238=CARTESIAN_POINT('Ctrl Pts',(-4.01317549494579,7.07430462955483,
95.080495768673));
#171239=CARTESIAN_POINT('Ctrl Pts',(-3.60800429955195,7.28082671597766,
95.0623615316293));
#171240=CARTESIAN_POINT('Ctrl Pts',(-3.52542687275876,7.32116781878217,
95.0587060951519));
#171241=CARTESIAN_POINT('Ctrl Pts',(-3.38597464468263,7.38638704813591,
95.0526073617842));
#171242=CARTESIAN_POINT('Ctrl Pts',(-3.32946715488126,7.41202984761432,
95.050156187515));
#171243=CARTESIAN_POINT('Ctrl Pts',(-3.24806490347128,7.44785100967987,
95.0466559682243));
#171244=CARTESIAN_POINT('Ctrl Pts',(-3.22340493779451,7.45855689085699,
95.0455996331649));
#171245=CARTESIAN_POINT('Ctrl Pts',(-3.18032740412013,7.47700503459374,
95.043761587596));
#171246=CARTESIAN_POINT('Ctrl Pts',(-3.16193359357418,7.48480211080803,
95.0429790389893));
#171247=CARTESIAN_POINT('Ctrl Pts',(-3.1235081682538,7.50092359890265,95.0413491381858));
#171248=CARTESIAN_POINT('Ctrl Pts',(-3.10347165885324,7.5092357654427,95.040502024169));
#171249=CARTESIAN_POINT('Ctrl Pts',(-3.0444300571406,7.53345256294429,95.0380138856426));
#171250=CARTESIAN_POINT('Ctrl Pts',(-3.00533425258843,7.54913425173881,
95.0363764995468));
#171251=CARTESIAN_POINT('Ctrl Pts',(-2.74863991589329,7.64978658672482,
95.0256852153991));
#171252=CARTESIAN_POINT('Ctrl Pts',(-2.52758281196608,7.72564456057991,
95.0167526446114));
#171253=CARTESIAN_POINT('Ctrl Pts',(-2.04671251289425,7.86780741645244,
94.9975645396818));
#171254=CARTESIAN_POINT('Ctrl Pts',(-1.78626711341502,7.93099449377891,
94.9873164200191));
#171255=CARTESIAN_POINT('Ctrl Pts',(-1.44585530767933,7.99596065016857,
94.9739108887133));
#171256=CARTESIAN_POINT('Ctrl Pts',(-1.3683215638532,8.00959301578285,94.9708575019063));
#171257=CARTESIAN_POINT('Ctrl Pts',(-1.24954969227803,8.02870114455305,
94.9661765923732));
#171258=CARTESIAN_POINT('Ctrl Pts',(-1.20844706839709,8.0349904895875,94.9645560735697));
#171259=CARTESIAN_POINT('Ctrl Pts',(-1.13264788598394,8.04599417519215,
94.9615660063421));
#171260=CARTESIAN_POINT('Ctrl Pts',(-1.09796561301865,8.05080027097469,
94.9601972742627));
#171261=CARTESIAN_POINT('Ctrl Pts',(-1.0211671471473,8.06093712508518,94.9571648308177));
#171262=CARTESIAN_POINT('Ctrl Pts',(-0.979038083830723,8.06616229003021,
94.9555002698122));
#171263=CARTESIAN_POINT('Ctrl Pts',(-0.856303813839657,8.08040900753404,
94.9506474181269));
#171264=CARTESIAN_POINT('Ctrl Pts',(-0.775602394193254,8.08855405842972,
94.9474520872307));
#171265=CARTESIAN_POINT('Ctrl Pts',(-0.406408244422184,8.12024003497157,
94.9328123847811));
#171266=CARTESIAN_POINT('Ctrl Pts',(-0.116909428030769,8.12956301390118,
94.9212618277416));
#171267=CARTESIAN_POINT('Ctrl Pts',(0.281740298828503,8.12109946594301,
94.9053632595044));
#171268=CARTESIAN_POINT('Ctrl Pts',(0.390958505417069,8.11657475468431,
94.9010096705924));
#171269=CARTESIAN_POINT('Ctrl Pts',(0.566854802641656,8.10572900577889,
94.894016491461));
#171270=CARTESIAN_POINT('Ctrl Pts',(0.633604033701103,8.10078472093421,
94.8913670282648));
#171271=CARTESIAN_POINT('Ctrl Pts',(0.726642104956197,8.09273617007723,
94.8876837515468));
#171272=CARTESIAN_POINT('Ctrl Pts',(0.752988148194098,8.0903273309966,94.88664182752));
#171273=CARTESIAN_POINT('Ctrl Pts',(0.798211765801853,8.08596968056625,
94.8848555120846));
#171274=CARTESIAN_POINT('Ctrl Pts',(0.817095116096069,8.08408332912075,
94.8841102783764));
#171275=CARTESIAN_POINT('Ctrl Pts',(0.853511011673782,8.08031666665382,
94.8826745090915));
#171276=CARTESIAN_POINT('Ctrl Pts',(0.871044324734877,8.07844541150655,
94.8819838605976));
#171277=CARTESIAN_POINT('Ctrl Pts',(0.921407366838671,8.07290451278525,
94.8800018239735));
#171278=CARTESIAN_POINT('Ctrl Pts',(0.954221023103633,8.0690917123435,94.8787125978143));
#171279=CARTESIAN_POINT('Ctrl Pts',(1.10800008849012,8.05027211079362,94.8726791656735));
#171280=CARTESIAN_POINT('Ctrl Pts',(1.22864227339502,8.03274448791166,94.8679702986353));
#171281=CARTESIAN_POINT('Ctrl Pts',(1.58501303494683,7.97275215785025,94.8540817451467));
#171282=CARTESIAN_POINT('Ctrl Pts',(1.81930956446794,7.92257269153464,94.8449770189337));
#171283=CARTESIAN_POINT('Ctrl Pts',(2.32696808158619,7.79013607267649,94.8250480010857));
#171284=CARTESIAN_POINT('Ctrl Pts',(2.5989059435904,7.70368010921243,94.8142386929617));
#171285=CARTESIAN_POINT('Ctrl Pts',(3.12709995054024,7.50459529657127,94.7926694079061));
#171286=CARTESIAN_POINT('Ctrl Pts',(3.38320886979333,7.39267194894809,94.7819271511611));
#171287=CARTESIAN_POINT('Ctrl Pts',(3.69387781346811,7.23737384150959,94.7684261477287));
#171288=CARTESIAN_POINT('Ctrl Pts',(3.75432948736774,7.20620034820655,94.765776331066));
#171289=CARTESIAN_POINT('Ctrl Pts',(3.850939100764,7.1548354113467,94.761503587549));
#171290=CARTESIAN_POINT('Ctrl Pts',(3.88734660059467,7.13512004901262,94.7598845911873));
#171291=CARTESIAN_POINT('Ctrl Pts',(3.95671804393681,7.0968655099599,94.7567825561497));
#171292=CARTESIAN_POINT('Ctrl Pts',(3.98970638033427,7.07837274617624,94.7552999200764));
#171293=CARTESIAN_POINT('Ctrl Pts',(4.06491559190419,7.03551879784878,94.7519022339171));
#171294=CARTESIAN_POINT('Ctrl Pts',(4.10704873066683,7.01100664858279,94.7499860799305));
#171295=CARTESIAN_POINT('Ctrl Pts',(4.24271967082099,6.93043354519203,94.7437741323328));
#171296=CARTESIAN_POINT('Ctrl Pts',(4.33534975960675,6.8728685116897,94.739467788866));
#171297=CARTESIAN_POINT('Ctrl Pts',(4.76649515019372,6.59274767078643,94.7191108638013));
#171298=CARTESIAN_POINT('Ctrl Pts',(5.08920770188082,6.34694821485646,94.7029974764005));
#171299=CARTESIAN_POINT('Ctrl Pts',(5.84015940178961,5.6807365926197,94.662012329591));
#171300=CARTESIAN_POINT('Ctrl Pts',(6.24276819395873,5.23507364640062,94.6365790495493));
#171301=CARTESIAN_POINT('Ctrl Pts',(6.72648419142853,4.56360235496574,94.6016761490449));
#171302=CARTESIAN_POINT('Ctrl Pts',(6.85234395463876,4.37234990882098,94.5920973275313));
#171303=CARTESIAN_POINT('Ctrl Pts',(7.01952575433701,4.09331704746116,94.5788339501143));
#171304=CARTESIAN_POINT('Ctrl Pts',(7.06761128704567,4.009720411998,94.5749476346757));
#171305=CARTESIAN_POINT('Ctrl Pts',(7.12215451680144,3.91086612333966,94.5704695204145));
#171306=CARTESIAN_POINT('Ctrl Pts',(7.13006690067068,3.89642205011866,94.5698181037515));
#171307=CARTESIAN_POINT('Ctrl Pts',(7.14210059287212,3.8742951218012,94.5688247402399));
#171308=CARTESIAN_POINT('Ctrl Pts',(7.14625351839712,3.86662956863853,94.5684814351066));
#171309=CARTESIAN_POINT('Ctrl Pts',(7.15346440586678,3.85326826844846,94.5678845091736));
#171310=CARTESIAN_POINT('Ctrl Pts',(7.15652791804543,3.84757553703061,94.5676306445625));
#171311=CARTESIAN_POINT('Ctrl Pts',(7.16339195976932,3.83478396139085,94.5670612582654));
#171312=CARTESIAN_POINT('Ctrl Pts',(7.16718874073074,3.82768310537471,94.5667459041681));
#171313=CARTESIAN_POINT('Ctrl Pts',(7.17728865322545,3.80872622340325,94.5659059675328));
#171314=CARTESIAN_POINT('Ctrl Pts',(7.18357297842651,3.79686016637839,94.5653822425539));
#171315=CARTESIAN_POINT('Ctrl Pts',(7.21032472243658,3.74604338286372,94.5631482354486));
#171316=CARTESIAN_POINT('Ctrl Pts',(7.23050524338887,3.7069418205877,94.5614514707266));
#171317=CARTESIAN_POINT('Ctrl Pts',(7.63411789193703,2.90906910721405,94.5273088781268));
#171318=CARTESIAN_POINT('Ctrl Pts',(7.89648214933574,2.09484259389513,94.5009850141658));
#171319=CARTESIAN_POINT('Ctrl Pts',(8.07363102489509,0.96139863034817,94.4617702264432));
#171320=CARTESIAN_POINT('Ctrl Pts',(8.10336069915064,0.665835163129001,
94.4513593883833));
#171321=CARTESIAN_POINT('Ctrl Pts',(8.12247881749743,0.245659908234986,
94.4359580657802));
#171322=CARTESIAN_POINT('Ctrl Pts',(8.12527858156364,0.121891094380435,
94.4313492978148));
#171323=CARTESIAN_POINT('Ctrl Pts',(8.1252332658565,-0.072864439355185,
94.4239667210359));
#171324=CARTESIAN_POINT('Ctrl Pts',(8.12428682139369,-0.143833922092723,
94.4212492996346));
#171325=CARTESIAN_POINT('Ctrl Pts',(8.12190662599008,-0.233846238165964,
94.4177663800555));
#171326=CARTESIAN_POINT('Ctrl Pts',(8.12133535770459,-0.25290967991097,
94.4170266757545));
#171327=CARTESIAN_POINT('Ctrl Pts',(8.12032423101039,-0.283100611339073,
94.4158518892959));
#171328=CARTESIAN_POINT('Ctrl Pts',(8.11992860419081,-0.294229560947777,
94.415418128088));
#171329=CARTESIAN_POINT('Ctrl Pts',(8.11915015033784,-0.314928777814457,
94.4146100232922));
#171330=CARTESIAN_POINT('Ctrl Pts',(8.11877327746063,-0.324499256181384,
94.4142358580493));
#171331=CARTESIAN_POINT('Ctrl Pts',(8.11790158491443,-0.345682695317728,
94.4134064955145));
#171332=CARTESIAN_POINT('Ctrl Pts',(8.1173987667325,-0.357295296209357,
94.4129510603431));
#171333=CARTESIAN_POINT('Ctrl Pts',(8.11588010550233,-0.390709641093286,
94.4116383104904));
#171334=CARTESIAN_POINT('Ctrl Pts',(8.11480133861701,-0.412508346953228,
94.4107791214638));
#171335=CARTESIAN_POINT('Ctrl Pts',(8.10703866270235,-0.557530630675659,
94.405044428367));
#171336=CARTESIAN_POINT('Ctrl Pts',(8.09763627391413,-0.680589024523087,
94.4000881387693));
#171337=CARTESIAN_POINT('Ctrl Pts',(8.06176860241798,-1.04156995842637,
94.3852779332295));
#171338=CARTESIAN_POINT('Ctrl Pts',(8.02758980488776,-1.27858188876243,
94.3752023186942));
#171339=CARTESIAN_POINT('Ctrl Pts',(7.81307519824032,-2.40987468887371,
94.3255475141545));
#171340=CARTESIAN_POINT('Ctrl Pts',(7.49350086006586,-3.27091119580164,
94.2822853649384));
#171341=CARTESIAN_POINT('Ctrl Pts',(7.00532913730159,-4.11694644894432,
94.2423841397797));
#171342=CARTESIAN_POINT('Ctrl Pts',(6.97228242873576,-4.17266846676819,
94.2397740537291));
#171343=CARTESIAN_POINT('Ctrl Pts',(6.93112003065592,-4.24022025374476,
94.2366265371217));
#171344=CARTESIAN_POINT('Ctrl Pts',(6.92363524047266,-4.2524308036738,94.2360582552634));
#171345=CARTESIAN_POINT('Ctrl Pts',(6.91122116218759,-4.27256324248015,
94.2351222806942));
#171346=CARTESIAN_POINT('Ctrl Pts',(6.90631046280093,-4.28049651395868,
94.2347537118338));
#171347=CARTESIAN_POINT('Ctrl Pts',(6.89742671745897,-4.2947931867569,94.2340899416659));
#171348=CARTESIAN_POINT('Ctrl Pts',(6.89345850748529,-4.30115956990539,
94.2337945168686));
#171349=CARTESIAN_POINT('Ctrl Pts',(6.88496503773944,-4.31474409098104,
94.2331644575491));
#171350=CARTESIAN_POINT('Ctrl Pts',(6.88043722869696,-4.32196062964471,
94.2328299399603));
#171351=CARTESIAN_POINT('Ctrl Pts',(6.86818393447519,-4.34142218949823,
94.2319282952375));
#171352=CARTESIAN_POINT('Ctrl Pts',(6.8604370369424,-4.35365373573406,94.2313621300092));
#171353=CARTESIAN_POINT('Ctrl Pts',(6.82215501104413,-4.41374117244007,
94.2285831039246));
#171354=CARTESIAN_POINT('Ctrl Pts',(6.79115122845628,-4.46129749096856,
94.22639069999));
#171355=CARTESIAN_POINT('Ctrl Pts',(6.70285863101587,-4.59367494919469,
94.2202981938675));
#171356=CARTESIAN_POINT('Ctrl Pts',(6.64446106022355,-4.67774533402821,
94.2164408622603));
#171357=CARTESIAN_POINT('Ctrl Pts',(6.43096925963876,-4.97302482563275,
94.2028668817703));
#171358=CARTESIAN_POINT('Ctrl Pts',(6.26726346875171,-5.17781396450533,
94.1933996026619));
#171359=CARTESIAN_POINT('Ctrl Pts',(5.92489875760565,-5.56602018377624,
94.1747875683099));
#171360=CARTESIAN_POINT('Ctrl Pts',(5.74690339065847,-5.7496179843282,94.165650643581));
#171361=CARTESIAN_POINT('Ctrl Pts',(5.3910381932999,-6.08362082766119,94.1479920296429));
#171362=CARTESIAN_POINT('Ctrl Pts',(5.21477807264227,-6.23536856154968,
94.1394982494472));
#171363=CARTESIAN_POINT('Ctrl Pts',(4.8381545563583,-6.53246263267437,94.1216622920368));
#171364=CARTESIAN_POINT('Ctrl Pts',(4.63717106284379,-6.67663432112402,
94.1123091392343));
#171365=CARTESIAN_POINT('Ctrl Pts',(4.39311393318093,-6.83536147940509,
94.1010899685688));
#171366=CARTESIAN_POINT('Ctrl Pts',(4.35610178846738,-6.85900821973032,
94.0993923208304));
#171367=CARTESIAN_POINT('Ctrl Pts',(4.29534189896328,-6.89713701925577,
94.0966115677212));
#171368=CARTESIAN_POINT('Ctrl Pts',(4.27170820958984,-6.91179933556675,
94.0955314432904));
#171369=CARTESIAN_POINT('Ctrl Pts',(4.22928543454946,-6.9378176856726,94.0935953092474));
#171370=CARTESIAN_POINT('Ctrl Pts',(4.21052468321154,-6.94921948233819,
94.092740028724));
#171371=CARTESIAN_POINT('Ctrl Pts',(4.17173426726248,-6.9725795043319,94.0909735593724));
#171372=CARTESIAN_POINT('Ctrl Pts',(4.15169882130206,-6.9845278031663,94.0900622149974));
#171373=CARTESIAN_POINT('Ctrl Pts',(4.10115709014258,-7.01437445927886,
94.0877656505479));
#171374=CARTESIAN_POINT('Ctrl Pts',(4.07058494189238,-7.03216017636156,
94.0863786758069));
#171375=CARTESIAN_POINT('Ctrl Pts',(3.94875606315176,-7.10197492393839,
94.0808591977956));
#171376=CARTESIAN_POINT('Ctrl Pts',(3.85661123412561,-7.15243116349059,
94.0767011405074));
#171377=CARTESIAN_POINT('Ctrl Pts',(3.03413836426582,-7.58228146716365,
94.0396804542716));
#171378=CARTESIAN_POINT('Ctrl Pts',(2.25109561383592,-7.85043173666986,
94.0043734641504));
#171379=CARTESIAN_POINT('Ctrl Pts',(1.2238566220196,-8.03558922964224,93.9605762016838));
#171380=CARTESIAN_POINT('Ctrl Pts',(1.00486508784383,-8.06590183130673,
93.9514256666622));
#171381=CARTESIAN_POINT('Ctrl Pts',(0.747756819237211,-8.09085534487136,
93.9410599513374));
#171382=CARTESIAN_POINT('Ctrl Pts',(0.710584905970697,-8.09420469320021,
93.9395705587599));
#171383=CARTESIAN_POINT('Ctrl Pts',(0.660535048642772,-8.09836696056611,
93.9375786350616));
#171384=CARTESIAN_POINT('Ctrl Pts',(0.647676623964324,-8.09940547024974,
93.937068079694));
#171385=CARTESIAN_POINT('Ctrl Pts',(0.627485652389728,-8.10098780264962,
93.936268303769));
#171386=CARTESIAN_POINT('Ctrl Pts',(0.620154775668397,-8.10155230047332,
93.9359783217586));
#171387=CARTESIAN_POINT('Ctrl Pts',(0.606073814318241,-8.10261734922504,
93.9354221078431));
#171388=CARTESIAN_POINT('Ctrl Pts',(0.599323852732836,-8.10311941762201,
93.9351558191581));
#171389=CARTESIAN_POINT('Ctrl Pts',(0.583455715296596,-8.10427976842575,
93.9345306306485));
#171390=CARTESIAN_POINT('Ctrl Pts',(0.574337029812911,-8.10493109863662,
93.9341719967785));
#171391=CARTESIAN_POINT('Ctrl Pts',(0.547927951585274,-8.10677265596026,
93.9331352060121));
#171392=CARTESIAN_POINT('Ctrl Pts',(0.530634761879627,-8.10792295788589,
93.932458611154));
#171393=CARTESIAN_POINT('Ctrl Pts',(0.404434256397985,-8.11591202734003,
93.927538503479));
#171394=CARTESIAN_POINT('Ctrl Pts',(0.295409099186309,-8.12061141652878,
93.9233889791688));
#171395=CARTESIAN_POINT('Ctrl Pts',(0.0266944833661381,-8.12677461621692,
93.9133972613159));
#171396=CARTESIAN_POINT('Ctrl Pts',(-0.133000664167659,-8.12573028806315,
93.9076530519118));
#171397=CARTESIAN_POINT('Ctrl Pts',(-0.925489891047017,-8.09717654579639,
93.8797352788387));
#171398=CARTESIAN_POINT('Ctrl Pts',(-1.55359212828043,-8.00045124508917,
93.8593338913361));
#171399=CARTESIAN_POINT('Ctrl Pts',(-2.5669517980104,-7.72043559500461,
93.8229183591905));
#171400=CARTESIAN_POINT('Ctrl Pts',(-2.96057603497608,-7.57821302013632,
93.8078575081775));
#171401=CARTESIAN_POINT('Ctrl Pts',(-3.37018115486437,-7.39341307223594,
93.7905737100953));
#171402=CARTESIAN_POINT('Ctrl Pts',(-3.39879044657238,-7.38030496303748,
93.7893579635739));
#171403=CARTESIAN_POINT('Ctrl Pts',(-3.43863913486979,-7.36176638054491,
93.7876524704381));
#171404=CARTESIAN_POINT('Ctrl Pts',(-3.44994341229048,-7.35647563660229,
93.7871672862622));
#171405=CARTESIAN_POINT('Ctrl Pts',(-3.46946135796356,-7.34728576517244,
93.7863271860817));
#171406=CARTESIAN_POINT('Ctrl Pts',(-3.47768076844247,-7.34339885214269,
93.7859726704121));
#171407=CARTESIAN_POINT('Ctrl Pts',(-3.49469654455405,-7.33531721166527,
93.785237230924));
#171408=CARTESIAN_POINT('Ctrl Pts',(-3.50349192052005,-7.33112043935655,
93.7848562403534));
#171409=CARTESIAN_POINT('Ctrl Pts',(-3.52405914931612,-7.32126118335225,
93.7839633398338));
#171410=CARTESIAN_POINT('Ctrl Pts',(-3.53582492371385,-7.31558612208675,
93.7834510167629));
#171411=CARTESIAN_POINT('Ctrl Pts',(-3.57373005254434,-7.2971902920139,
93.7817955433889));
#171412=CARTESIAN_POINT('Ctrl Pts',(-3.59981470389926,-7.28435767399418,
93.7806487070129));
#171413=CARTESIAN_POINT('Ctrl Pts',(-3.9806586433076,-7.09445228318185,
93.7637918859624));
#171414=CARTESIAN_POINT('Ctrl Pts',(-4.32202417190279,-6.89180312107808,
93.7472113603622));
#171415=CARTESIAN_POINT('Ctrl Pts',(-5.35582661542184,-6.17098547215181,
93.6923617589405));
#171416=CARTESIAN_POINT('Ctrl Pts',(-5.9810578857684,-5.56711215960124,
93.65147926183));
#171417=CARTESIAN_POINT('Ctrl Pts',(-6.56121040277545,-4.79382970037055,
93.6113784162077));
#171418=CARTESIAN_POINT('Ctrl Pts',(-6.62141984317476,-4.71031706230643,
93.6071941109172));
#171419=CARTESIAN_POINT('Ctrl Pts',(-6.68893916914521,-4.61281097844696,
93.602479341619));
#171420=CARTESIAN_POINT('Ctrl Pts',(-6.6978087358599,-4.59992287697257,
93.6018593950244));
#171421=CARTESIAN_POINT('Ctrl Pts',(-6.71195693504179,-4.57923687220886,
93.6008693966906));
#171422=CARTESIAN_POINT('Ctrl Pts',(-6.71725930432266,-4.57145531195093,
93.6004981225444));
#171423=CARTESIAN_POINT('Ctrl Pts',(-6.72662176390864,-4.55766385445949,
93.599842085078));
#171424=CARTESIAN_POINT('Ctrl Pts',(-6.73068735077529,-4.55165771466889,
93.5995570458177));
#171425=CARTESIAN_POINT('Ctrl Pts',(-6.73910400100001,-4.53918776197313,
93.5989666043461));
#171426=CARTESIAN_POINT('Ctrl Pts',(-6.7434538206387,-4.53272311576684,
93.5986612634594));
#171427=CARTESIAN_POINT('Ctrl Pts',(-6.75462518272094,-4.51606870712732,
93.5978765493515));
#171428=CARTESIAN_POINT('Ctrl Pts',(-6.76143298355118,-4.5058697204403,
93.5973978385143));
#171429=CARTESIAN_POINT('Ctrl Pts',(-6.78961615049801,-4.46343990869116,
93.5954137742493));
#171430=CARTESIAN_POINT('Ctrl Pts',(-6.81078454885842,-4.43107178677248,
93.5939180595367));
#171431=CARTESIAN_POINT('Ctrl Pts',(-6.86515137274642,-4.34663061976467,
93.5900590667336));
#171432=CARTESIAN_POINT('Ctrl Pts',(-6.89798895671689,-4.2943276168054,
93.5877108036029));
#171433=CARTESIAN_POINT('Ctrl Pts',(-7.04314236925637,-4.05716871209813,
93.577229270678));
#171434=CARTESIAN_POINT('Ctrl Pts',(-7.14864941012239,-3.86824118229549,
93.5693262882223));
#171435=CARTESIAN_POINT('Ctrl Pts',(-7.56785470962135,-3.04171028794821,
93.5358419613534));
#171436=CARTESIAN_POINT('Ctrl Pts',(-7.80472498575103,-2.36869735521673,
93.5108373021046));
#171437=CARTESIAN_POINT('Ctrl Pts',(-8.0183415847571,-1.35374603969443,
93.4717992870617));
#171438=CARTESIAN_POINT('Ctrl Pts',(-8.06628519510275,-1.0302730025906,
93.4592708228089));
#171439=CARTESIAN_POINT('Ctrl Pts',(-8.10311417159392,-0.607296120265727,
93.4428388472676));
#171440=CARTESIAN_POINT('Ctrl Pts',(-8.10984176995107,-0.50964116556756,
93.4390384032802));
#171441=CARTESIAN_POINT('Ctrl Pts',(-8.11720153840767,-0.36464320963158,
93.4333794374685));
#171442=CARTESIAN_POINT('Ctrl Pts',(-8.11918696823725,-0.317377433393139,
93.4315322361271));
#171443=CARTESIAN_POINT('Ctrl Pts',(-8.12200815554881,-0.232555421971376,
93.4282120569847));
#171444=CARTESIAN_POINT('Ctrl Pts',(-8.12299644940413,-0.195005572077664,
93.4267404082097));
#171445=CARTESIAN_POINT('Ctrl Pts',(-8.12455100979448,-0.114797281414313,
93.4235925806025));
#171446=CARTESIAN_POINT('Ctrl Pts',(-8.12504175627157,-0.0721385205948915,
93.4219158029972));
#171447=CARTESIAN_POINT('Ctrl Pts',(-8.12546471906561,0.0444452697352801,
93.4173254997582));
#171448=CARTESIAN_POINT('Ctrl Pts',(-8.12472406330371,0.118368394972371,
93.4144063378893));
#171449=CARTESIAN_POINT('Ctrl Pts',(-8.1138633632295,0.577206721251773,
93.3962277407092));
#171450=CARTESIAN_POINT('Ctrl Pts',(-8.0774013825832,0.961000135856553,
93.3807452545336));
#171451=CARTESIAN_POINT('Ctrl Pts',(-7.9563401258764,1.68460155556326,93.3509908422658));
#171452=CARTESIAN_POINT('Ctrl Pts',(-7.8767416614841,2.02439433972723,93.3367772490979));
#171453=CARTESIAN_POINT('Ctrl Pts',(-7.76034705011079,2.40820496382675,
93.320592431989));
#171454=CARTESIAN_POINT('Ctrl Pts',(-7.74464305493016,2.45823950714455,
93.3184801617431));
#171455=CARTESIAN_POINT('Ctrl Pts',(-7.72520492050419,2.51813570075325,
93.3159495198298));
#171456=CARTESIAN_POINT('Ctrl Pts',(-7.72193461703842,2.52814640432777,
93.3155264940729));
#171457=CARTESIAN_POINT('Ctrl Pts',(-7.69125067105442,2.621457837397,93.3115828109803));
#171458=CARTESIAN_POINT('Ctrl Pts',(-7.66250936697679,2.70431664497324,
93.3080764784248));
#171459=CARTESIAN_POINT('Ctrl Pts',(-7.61515553168986,2.83401329190045,
93.3025866425489));
#171460=CARTESIAN_POINT('Ctrl Pts',(-7.59743910679157,2.88117062755141,
93.3005902508787));
#171461=CARTESIAN_POINT('Ctrl Pts',(-7.57095594309598,2.94971996315994,
93.2976888327562));
#171462=CARTESIAN_POINT('Ctrl Pts',(-7.56253470836174,2.9712439388512,93.2967778962677));
#171463=CARTESIAN_POINT('Ctrl Pts',(-7.5473820500382,3.00949110558663,93.2951594834198));
#171464=CARTESIAN_POINT('Ctrl Pts',(-7.54068660591185,3.02622835188119,
93.29445135279));
#171465=CARTESIAN_POINT('Ctrl Pts',(-7.5339286368954,3.04296021285256,93.2937434592611));
#171466=CARTESIAN_POINT('Ctrl Pts',(-7.53392176892502,3.0429772168973,93.2937427398521));
#171467=CARTESIAN_POINT('Ctrl Pts',(-7.53390802701265,3.04301123943888,
93.2937413004224));
#171468=CARTESIAN_POINT('Ctrl Pts',(-7.53390116345209,3.04302823223383,
93.2937405814893));
#171469=CARTESIAN_POINT('Ctrl Pts',(-7.53388744434638,3.04306219764829,
93.2937391444767));
#171470=CARTESIAN_POINT('Ctrl Pts',(-7.53388058877827,3.04307917032505,
93.2937384263947));
#171471=CARTESIAN_POINT('Ctrl Pts',(-7.53386688496685,3.04311309721399,
93.2937369910121));
#171472=CARTESIAN_POINT('Ctrl Pts',(-7.53386003709493,3.04313005050709,
93.2937362737502));
#171473=CARTESIAN_POINT('Ctrl Pts',(-7.53384634929344,3.04316393710107,
93.2937348400724));
#171474=CARTESIAN_POINT('Ctrl Pts',(-7.53383950929199,3.04318087058025,
93.2937341236489));
#171475=CARTESIAN_POINT('Ctrl Pts',(-7.53382583714785,3.04321471775445,
93.2937326916389));
#171476=CARTESIAN_POINT('Ctrl Pts',(-7.53381900506374,3.04323163130483,
93.2937319760585));
#171477=CARTESIAN_POINT('Ctrl Pts',(-7.53380534828561,3.04326543978276,
93.2937305456857));
#171478=CARTESIAN_POINT('Ctrl Pts',(-7.5337985239722,3.0432823337685,93.2937298309331));
#171479=CARTESIAN_POINT('Ctrl Pts',(-7.53378488270275,3.04331610319926,
93.2937284022123));
#171480=CARTESIAN_POINT('Ctrl Pts',(-7.53377806606017,3.04333297786868,
93.293727688277));
#171481=CARTESIAN_POINT('Ctrl Pts',(-7.53376444057693,3.04336670756748,
93.2937262612372));
#171482=CARTESIAN_POINT('Ctrl Pts',(-7.53375763173327,3.04338356260467,
93.2937255481325));
#171483=CARTESIAN_POINT('Ctrl Pts',(-7.5337440216806,3.04341725345418,93.2937241227364));
#171484=CARTESIAN_POINT('Ctrl Pts',(-7.53373722058697,3.04343408898129,
93.2937234104571));
#171485=CARTESIAN_POINT('Ctrl Pts',(-7.53372362601295,3.04346774086474,
93.2937219867097));
#171486=CARTESIAN_POINT('Ctrl Pts',(-7.5337168326701,3.04348455688104,93.2937212752559));
#171487=CARTESIAN_POINT('Ctrl Pts',(-7.53370325345981,3.04351817008514,
93.2937198531449));
#171488=CARTESIAN_POINT('Ctrl Pts',(-7.53369646780441,3.04353496674849,
93.2937191425099));
#171489=CARTESIAN_POINT('Ctrl Pts',(-7.53368290404449,3.04356854106103,
93.2937177220444));
#171490=CARTESIAN_POINT('Ctrl Pts',(-7.53367612608663,3.04358531834758,
93.2937170122293));
#171491=CARTESIAN_POINT('Ctrl Pts',(-7.53366257774988,3.04361885383813,
93.2937155934063));
#171492=CARTESIAN_POINT('Ctrl Pts',(-7.5336558075323,3.04363561164321,93.2937148844153));
#171493=CARTESIAN_POINT('Ctrl Pts',(-7.53364227424431,3.04366910924071,
93.2937134671956));
#171494=CARTESIAN_POINT('Ctrl Pts',(-7.53363551152804,3.04368584815693,
93.2937127590038));
#171495=CARTESIAN_POINT('Ctrl Pts',(-7.53362199400518,3.04371930609046,
93.2937113434621));
#171496=CARTESIAN_POINT('Ctrl Pts',(-7.53361523907891,3.04373602540438,
93.2937106360997));
#171497=CARTESIAN_POINT('Ctrl Pts',(-7.53360173638902,3.04376944598339,
93.2937092221385));
#171498=CARTESIAN_POINT('Ctrl Pts',(-7.53359498894672,3.04378614645354,
93.2937085155734));
#171499=CARTESIAN_POINT('Ctrl Pts',(-7.53358150188086,3.04381952772228,
93.2937071032754));
#171500=CARTESIAN_POINT('Ctrl Pts',(-7.53357476215167,3.04383620878266,
93.2937063975314));
#171501=CARTESIAN_POINT('Ctrl Pts',(-7.53356129005246,3.04386955237036,
93.2937049868276));
#171502=CARTESIAN_POINT('Ctrl Pts',(-7.53355455788635,3.04388621439336,
93.2937042818891));
#171503=CARTESIAN_POINT('Ctrl Pts',(-7.53354110106289,3.0439195195372,93.2937028728118));
#171504=CARTESIAN_POINT('Ctrl Pts',(-7.53353437651803,3.04393616237999,
93.2937021686848));
#171505=CARTESIAN_POINT('Ctrl Pts',(-7.5335209347308,3.04396942967493,93.2937007612089));
#171506=CARTESIAN_POINT('Ctrl Pts',(-7.53351421773309,3.04398605352197,
93.2937000578856));
#171507=CARTESIAN_POINT('Ctrl Pts',(-7.53350079106562,3.04401928276345,
93.2936986520197));
#171508=CARTESIAN_POINT('Ctrl Pts',(-7.5334940815995,3.04403588765431,93.2936979494984));
#171509=CARTESIAN_POINT('Ctrl Pts',(-7.5334806699575,3.04406907907789,93.2936965452325));
#171510=CARTESIAN_POINT('Ctrl Pts',(-7.53347396794667,3.04408566520247,
93.2936958435052));
#171511=CARTESIAN_POINT('Ctrl Pts',(-7.53346057167164,3.04411881796512,
93.293694440875));
#171512=CARTESIAN_POINT('Ctrl Pts',(-7.53345387735365,3.04413538473669,
93.2936937399664));
#171513=CARTESIAN_POINT('Ctrl Pts',(-7.5334404955451,3.04416850106907,93.2936923388775));
#171514=CARTESIAN_POINT('Ctrl Pts',(-7.53343380854309,3.04418504942125,
93.2936916387484));
#171515=CARTESIAN_POINT('Ctrl Pts',(-7.53342044229823,3.04421812661023,
93.2936902393156));
#171516=CARTESIAN_POINT('Ctrl Pts',(-7.53341376300435,3.04423465557371,
93.2936895400067));
#171517=CARTESIAN_POINT('Ctrl Pts',(-7.53340041099827,3.04426769690014,
93.2936881420912));
#171518=CARTESIAN_POINT('Ctrl Pts',(-7.53339373891981,3.0442842076952,93.293687443551));
#171519=CARTESIAN_POINT('Ctrl Pts',(-7.53338040236975,3.04431721014898,
93.2936860472802));
#171520=CARTESIAN_POINT('Ctrl Pts',(-7.5333737377875,3.04433370208186,93.293685349538));
#171521=CARTESIAN_POINT('Ctrl Pts',(-7.53336041606794,3.04436666721303,
93.2936839548463));
#171522=CARTESIAN_POINT('Ctrl Pts',(-7.53335375896608,3.04438314032396,
93.2936832579005));
#171523=CARTESIAN_POINT('Ctrl Pts',(-7.53334045205952,3.04441606817795,
93.2936818647859));
#171524=CARTESIAN_POINT('Ctrl Pts',(-7.53333380243665,3.04443252247144,
93.2936811686362));
#171525=CARTESIAN_POINT('Ctrl Pts',(-7.53332051012661,3.04446541358601,
93.293679777076));
#171526=CARTESIAN_POINT('Ctrl Pts',(-7.53331386781142,3.04448184948703,
93.2936790817045));
#171527=CARTESIAN_POINT('Ctrl Pts',(-7.53330059049022,3.04451470289351,
93.2936776917397));
#171528=CARTESIAN_POINT('Ctrl Pts',(-7.53329395558048,3.04453112016114,
93.2936769971565));
#171529=CARTESIAN_POINT('Ctrl Pts',(-7.53328069287546,3.04456393678375,
93.293675608748));
#171530=CARTESIAN_POINT('Ctrl Pts',(-7.53327406524153,3.04458033573985,
93.2936749149395));
#171531=CARTESIAN_POINT('Ctrl Pts',(-7.52657141531173,3.06116475031661,
93.2929732601048));
#171532=CARTESIAN_POINT('Ctrl Pts',(-7.51982074033722,3.07771066445389,
93.2922732403024));
#171533=CARTESIAN_POINT('Ctrl Pts',(-7.49951067364812,3.127024916758,93.2901866287043));
#171534=CARTESIAN_POINT('Ctrl Pts',(-7.48579124759548,3.15972698015247,
93.2888026046292));
#171535=CARTESIAN_POINT('Ctrl Pts',(-7.39070595606194,3.3822797751389,93.2793770520012));
#171536=CARTESIAN_POINT('Ctrl Pts',(-7.30233962994029,3.56905993468778,
93.2714309709452));
#171537=CARTESIAN_POINT('Ctrl Pts',(-7.08218215340431,3.99191428040401,
93.2531022773816));
#171538=CARTESIAN_POINT('Ctrl Pts',(-6.94553881460965,4.22518318161648,
93.2427307725261));
#171539=CARTESIAN_POINT('Ctrl Pts',(-6.76205928680134,4.50537835645699,
93.2297410019823));
#171540=CARTESIAN_POINT('Ctrl Pts',(-6.72594237976424,4.55912041745257,
93.2272245664502));
#171541=CARTESIAN_POINT('Ctrl Pts',(-6.66718866589827,4.6443282195857,93.2231923978165));
#171542=CARTESIAN_POINT('Ctrl Pts',(-6.64496230267298,4.67607370568202,
93.2216805845555));
#171543=CARTESIAN_POINT('Ctrl Pts',(-6.60200696473175,4.73650122382074,
93.2187840203165));
#171544=CARTESIAN_POINT('Ctrl Pts',(-6.58131603353919,4.76520923592443,
93.2173996678754));
#171545=CARTESIAN_POINT('Ctrl Pts',(-6.56040309806832,4.79382923735388,
93.216011118566));
#171546=CARTESIAN_POINT('Ctrl Pts',(-6.56036792838607,4.79387736704315,
93.2160087834459));
#171547=CARTESIAN_POINT('Ctrl Pts',(-6.56029763279905,4.79397356429252,
93.2160041161725));
#171548=CARTESIAN_POINT('Ctrl Pts',(-6.56026248621184,4.7940216601561,93.2160017826458));
#171549=CARTESIAN_POINT('Ctrl Pts',(-6.56019220978094,4.79411782675084,
93.2159971167638));
#171550=CARTESIAN_POINT('Ctrl Pts',(-6.56015707951682,4.79416589805838,
93.2159947843805));
#171551=CARTESIAN_POINT('Ctrl Pts',(-6.56008683542515,4.79426201596438,
93.215990120765));
#171552=CARTESIAN_POINT('Ctrl Pts',(-6.56005172133166,4.79431006292779,
93.215987789515));
#171553=CARTESIAN_POINT('Ctrl Pts',(-6.5599815094794,4.79440613228813,93.2159831281591));
#171554=CARTESIAN_POINT('Ctrl Pts',(-6.5599464114472,4.79445415506026,93.215980798035));
#171555=CARTESIAN_POINT('Ctrl Pts',(-6.55987623167614,4.79455017609793,
93.2159761389281));
#171556=CARTESIAN_POINT('Ctrl Pts',(-6.55984114962487,4.79459817479195,
93.2159738099246));
#171557=CARTESIAN_POINT('Ctrl Pts',(-6.55977100166118,4.79469414788804,
93.2159691530484));
#171558=CARTESIAN_POINT('Ctrl Pts',(-6.55973593545178,4.79474212269744,
93.215966825156));
#171559=CARTESIAN_POINT('Ctrl Pts',(-6.55966581925036,4.79483804792005,
93.2159621705072));
#171560=CARTESIAN_POINT('Ctrl Pts',(-6.55963076885347,4.79488599888819,
93.215959843724));
#171561=CARTESIAN_POINT('Ctrl Pts',(-6.55956068405944,4.79498187672919,
93.215955191279));
#171562=CARTESIAN_POINT('Ctrl Pts',(-6.55952564935839,4.79502980401886,
93.215952865597));
#171563=CARTESIAN_POINT('Ctrl Pts',(-6.55945559577165,4.79512563475832,
93.2159482153423));
#171564=CARTESIAN_POINT('Ctrl Pts',(-6.55942057662666,4.79517353856386,
93.2159458907522));
#171565=CARTESIAN_POINT('Ctrl Pts',(-6.55935055413489,4.79526932236171,
93.2159412426802));
#171566=CARTESIAN_POINT('Ctrl Pts',(-6.55931555044835,4.79531720281978,
93.2159389191756));
#171567=CARTESIAN_POINT('Ctrl Pts',(-6.55924555892839,4.79541293985073,
93.2159342732778));
#171568=CARTESIAN_POINT('Ctrl Pts',(-6.5592105706757,4.79546079699811,93.2159319508569));
#171569=CARTESIAN_POINT('Ctrl Pts',(-6.55914060973929,4.79555648779942,
93.2159273071075));
#171570=CARTESIAN_POINT('Ctrl Pts',(-6.55910563677732,4.79560432183497,
93.2159249857606));
#171571=CARTESIAN_POINT('Ctrl Pts',(-6.55903570622705,4.79569996668282,
93.2159203441463));
#171572=CARTESIAN_POINT('Ctrl Pts',(-6.5590007483651,4.7957477778704,93.2159180238608));
#171573=CARTESIAN_POINT('Ctrl Pts',(-6.55893084837131,4.79584337653794,
93.2159133843927));
#171574=CARTESIAN_POINT('Ctrl Pts',(-6.55889590569035,4.7958911647699,93.2159110651738));
#171575=CARTESIAN_POINT('Ctrl Pts',(-6.55882603562209,4.79598671812613,
93.21590642781));
#171576=CARTESIAN_POINT('Ctrl Pts',(-6.55879110794696,4.79603448364502,
93.2159041096459));
#171577=CARTESIAN_POINT('Ctrl Pts',(-6.55872126770312,4.79612999183424,
93.2158994743794));
#171578=CARTESIAN_POINT('Ctrl Pts',(-6.55868635487444,4.79617773486104,
93.2158971572597));
#171579=CARTESIAN_POINT('Ctrl Pts',(-6.55861654444349,4.79627319790501,
93.2158925240896));
#171580=CARTESIAN_POINT('Ctrl Pts',(-6.5585816464217,4.79632091849682,93.2158902080113));
#171581=CARTESIAN_POINT('Ctrl Pts',(-6.55851186551032,4.79641633680261,
93.215885576918));
#171582=CARTESIAN_POINT('Ctrl Pts',(-6.55847698221643,4.7964640350704,93.215883261876));
#171583=CARTESIAN_POINT('Ctrl Pts',(-6.55840723056912,4.7965594089933,93.2158786328423));
#171584=CARTESIAN_POINT('Ctrl Pts',(-6.55837236188042,4.7966070851078,93.2158763188283));
#171585=CARTESIAN_POINT('Ctrl Pts',(-6.55830263938441,4.79670241480788,
93.2158716918466));
#171586=CARTESIAN_POINT('Ctrl Pts',(-6.55826778523327,4.7967500688645,93.2158693788561));
#171587=CARTESIAN_POINT('Ctrl Pts',(-6.55819809156584,4.79684535478884,
93.2158647539048));
#171588=CARTESIAN_POINT('Ctrl Pts',(-6.55816325178624,4.79689298701748,
93.2158624419266));
#171589=CARTESIAN_POINT('Ctrl Pts',(-6.55809358692053,4.7969882292086,93.2158578190038));
#171590=CARTESIAN_POINT('Ctrl Pts',(-6.55805876144252,4.79703583970777,
93.2158555080332));
#171591=CARTESIAN_POINT('Ctrl Pts',(-6.55798912515072,4.79713103848287,
93.2158508871237));
#171592=CARTESIAN_POINT('Ctrl Pts',(-6.55795431389782,4.79717862736001,
93.2158485771555));
#171593=CARTESIAN_POINT('Ctrl Pts',(-6.55788470595877,4.79727378302717,
93.2158439582443));
#171594=CARTESIAN_POINT('Ctrl Pts',(-6.55784990884646,4.79732135040067,
93.2158416492729));
#171595=CARTESIAN_POINT('Ctrl Pts',(-6.55778032902798,4.79741646328296,
93.2158370323446));
#171596=CARTESIAN_POINT('Ctrl Pts',(-6.55774554594491,4.79746400930785,
93.2158347243625));
#171597=CARTESIAN_POINT('Ctrl Pts',(-6.55767599410069,4.79755907961091,
93.2158301094071));
#171598=CARTESIAN_POINT('Ctrl Pts',(-6.55764122496623,4.79760660440025,
93.2158278024089));
#171599=CARTESIAN_POINT('Ctrl Pts',(-6.55757170083455,4.79770163248742,
93.2158231894089));
#171600=CARTESIAN_POINT('Ctrl Pts',(-6.55753694551589,4.79774913622549,
93.2158208833857));
#171601=CARTESIAN_POINT('Ctrl Pts',(-6.55746744895978,4.79784412228955,
93.2158162723319));
#171602=CARTESIAN_POINT('Ctrl Pts',(-6.55743270734223,4.79789160513591,
93.2158139672761));
#171603=CARTESIAN_POINT('Ctrl Pts',(-6.55736323827116,4.79798654930612,
93.2158093581623));
#171604=CARTESIAN_POINT('Ctrl Pts',(-6.55732851032321,4.79803401130659,
93.2158070540716));
#171605=CARTESIAN_POINT('Ctrl Pts',(-6.55725906838534,4.79812891406929,
93.2158024468744));
#171606=CARTESIAN_POINT('Ctrl Pts',(-6.55722435398003,4.79817635540009,
93.2158001437403));
#171607=CARTESIAN_POINT('Ctrl Pts',(-6.55715493908768,4.79827121688058,
93.2157955384537));
#171608=CARTESIAN_POINT('Ctrl Pts',(-6.55712023817218,4.79831863761665,
93.2157932362726));
#171609=CARTESIAN_POINT('Ctrl Pts',(-6.5298517047507,4.83558176093202,93.2139841684961));
#171610=CARTESIAN_POINT('Ctrl Pts',(-6.50230160666431,4.87256483241269,
93.21217429565));
#171611=CARTESIAN_POINT('Ctrl Pts',(-6.40778004575286,4.99722060901601,
93.2060239744839));
#171612=CARTESIAN_POINT('Ctrl Pts',(-6.33933876926566,5.08376264253064,
93.2016691383768));
#171613=CARTESIAN_POINT('Ctrl Pts',(-6.16227216960738,5.2985204853865,93.1906420440488));
#171614=CARTESIAN_POINT('Ctrl Pts',(-6.05139276956349,5.42480990028568,
93.1839507857722));
#171615=CARTESIAN_POINT('Ctrl Pts',(-5.764170871239,5.73217765710635,93.1671577996232));
#171616=CARTESIAN_POINT('Ctrl Pts',(-5.58314559313247,5.90863881191473,
93.1570418423535));
#171617=CARTESIAN_POINT('Ctrl Pts',(-5.34745425810077,6.11786944201301,
93.1445487303525));
#171618=CARTESIAN_POINT('Ctrl Pts',(-5.30023847401889,6.15882015901992,
93.1420782065938));
#171619=CARTESIAN_POINT('Ctrl Pts',(-5.23328565854219,6.21554877951916,
93.1386227725085));
#171620=CARTESIAN_POINT('Ctrl Pts',(-5.21394051745968,6.23178543472024,
93.1376298815866));
#171621=CARTESIAN_POINT('Ctrl Pts',(-5.18051694166885,6.25957373948575,
93.1359241157322));
#171622=CARTESIAN_POINT('Ctrl Pts',(-5.16647484431986,6.27116870036991,
93.1352103859523));
#171623=CARTESIAN_POINT('Ctrl Pts',(-5.15229381191995,6.28279842545444,
93.1344924407725));
#171624=CARTESIAN_POINT('Ctrl Pts',(-5.15219376259511,6.28288047092655,
93.1344873757037));
#171625=CARTESIAN_POINT('Ctrl Pts',(-5.15199897010158,6.28304020276687,
93.13447751447));
#171626=CARTESIAN_POINT('Ctrl Pts',(-5.15190427601749,6.28311784930319,
93.1344727207752));
#171627=CARTESIAN_POINT('Ctrl Pts',(-5.15175004632635,6.28324430757024,
93.1344649134199));
#171628=CARTESIAN_POINT('Ctrl Pts',(-5.15169046009297,6.28329316297049,
93.1344618971195));
#171629=CARTESIAN_POINT('Ctrl Pts',(-5.15157204477313,6.28339025015948,
93.1344559029459));
#171630=CARTESIAN_POINT('Ctrl Pts',(-5.15151323383699,6.28343846710465,
93.1344529259903));
#171631=CARTESIAN_POINT('Ctrl Pts',(-5.15139637841243,6.28353426986887,
93.1344470109737));
#171632=CARTESIAN_POINT('Ctrl Pts',(-5.15133833607977,6.28358185395662,
93.1344440730205));
#171633=CARTESIAN_POINT('Ctrl Pts',(-5.15122300631927,6.28367640057621,
93.1344382354205));
#171634=CARTESIAN_POINT('Ctrl Pts',(-5.15116572090976,6.28372336148851,
93.1344353358746));
#171635=CARTESIAN_POINT('Ctrl Pts',(-5.15105189338562,6.2838166713788,93.1344295744978));
#171636=CARTESIAN_POINT('Ctrl Pts',(-5.15099535340933,6.28386301863799,
93.134426712774));
#171637=CARTESIAN_POINT('Ctrl Pts',(-5.15088300493899,6.28395511100634,
93.1344210264398));
#171638=CARTESIAN_POINT('Ctrl Pts',(-5.15082719889353,6.28400085414154,
93.1344182019523));
#171639=CARTESIAN_POINT('Ctrl Pts',(-5.15071630749497,6.2840917472045,93.1344125895411));
#171640=CARTESIAN_POINT('Ctrl Pts',(-5.15066122442699,6.28413689529147,
93.134409801732));
#171641=CARTESIAN_POINT('Ctrl Pts',(-5.15055176750221,6.28422660776392,
93.1344042620932));
#171642=CARTESIAN_POINT('Ctrl Pts',(-5.15049739632682,6.28427116998303,
93.1344015103982));
#171643=CARTESIAN_POINT('Ctrl Pts',(-5.15038935253042,6.28435971954687,
93.1343960424449));
#171644=CARTESIAN_POINT('Ctrl Pts',(-5.1503356825521,6.2844037047562,93.1343933263193));
#171645=CARTESIAN_POINT('Ctrl Pts',(-5.15022903060004,6.28449110903689,
93.1343879289678));
#171646=CARTESIAN_POINT('Ctrl Pts',(-5.15017605137443,6.2845345258857,93.1343852478799));
#171647=CARTESIAN_POINT('Ctrl Pts',(-5.15007076995498,6.2846208025254,93.1343799200454));
#171648=CARTESIAN_POINT('Ctrl Pts',(-5.15001847093487,6.28466365974429,
93.1343772734584));
#171649=CARTESIAN_POINT('Ctrl Pts',(-5.14991453997051,6.28474882536796,
93.1343720141187));
#171650=CARTESIAN_POINT('Ctrl Pts',(-5.1498629110753,6.28479113130228,93.1343694015193));
#171651=CARTESIAN_POINT('Ctrl Pts',(-5.14976031017698,6.28487520278459,
93.1343642096368));
#171652=CARTESIAN_POINT('Ctrl Pts',(-5.14970934139229,6.2849169657227,93.1343616305155));
#171653=CARTESIAN_POINT('Ctrl Pts',(-5.14960805090765,6.28499995932921,
93.1343565050898));
#171654=CARTESIAN_POINT('Ctrl Pts',(-5.14955773254745,6.28504118728773,
93.1343539589535));
#171655=CARTESIAN_POINT('Ctrl Pts',(-5.14945773247267,6.28512311956672,
93.1343488989668));
#171656=CARTESIAN_POINT('Ctrl Pts',(-5.14940805462437,6.28516382074528,
93.1343463853111));
#171657=CARTESIAN_POINT('Ctrl Pts',(-5.14930932652529,6.28524470695378,
93.1343413898253));
#171658=CARTESIAN_POINT('Ctrl Pts',(-5.14926027987475,6.28528488905923,
93.1343389081763));
#171659=CARTESIAN_POINT('Ctrl Pts',(-5.14916280459681,6.28536474503961,
93.1343339762167));
#171660=CARTESIAN_POINT('Ctrl Pts',(-5.14911437979497,6.28540441580493,
93.1343315260988));
#171661=CARTESIAN_POINT('Ctrl Pts',(-5.14901813901997,6.28548325670949,
93.1343266567334));
#171662=CARTESIAN_POINT('Ctrl Pts',(-5.14897032698599,6.28552242364556,
93.1343242376845));
#171663=CARTESIAN_POINT('Ctrl Pts',(-5.14887530233082,6.28560026467516,
93.1343194299783));
#171664=CARTESIAN_POINT('Ctrl Pts',(-5.14882809396667,6.28563893530464,
93.1343170415356));
#171665=CARTESIAN_POINT('Ctrl Pts',(-5.14873426787018,6.28571579098223,
93.1343122945951));
#171666=CARTESIAN_POINT('Ctrl Pts',(-5.1486876543865,6.28575397257269,93.1343099363115));
#171667=CARTESIAN_POINT('Ctrl Pts',(-5.14859500924652,6.28582985745046,
93.1343052492415));
#171668=CARTESIAN_POINT('Ctrl Pts',(-5.14854898195993,6.28586755718052,
93.1343029206754));
#171669=CARTESIAN_POINT('Ctrl Pts',(-5.1484575006427,6.28594248542269,93.1342982926043));
#171670=CARTESIAN_POINT('Ctrl Pts',(-5.14841205109036,6.28597971028821,
93.1342959933252));
#171671=CARTESIAN_POINT('Ctrl Pts',(-5.14832171650406,6.28605369602054,
93.1342914233839));
#171672=CARTESIAN_POINT('Ctrl Pts',(-5.1482768362567,6.28609045298784,93.1342891529631));
#171673=CARTESIAN_POINT('Ctrl Pts',(-5.14820204483236,6.28615170590039,
93.1342853694308));
#171674=CARTESIAN_POINT('Ctrl Pts',(-5.14817213864121,6.28617619820678,
93.1342838565551));
#171675=CARTESIAN_POINT('Ctrl Pts',(-5.14811259760543,6.28622495989124,
93.1342808445564));
#171676=CARTESIAN_POINT('Ctrl Pts',(-5.1480828255236,6.28624934166092,93.1342793384905));
#171677=CARTESIAN_POINT('Ctrl Pts',(-5.14802336814565,6.28629803342165,
93.1342763307739));
#171678=CARTESIAN_POINT('Ctrl Pts',(-5.14799368370544,6.28632234271388,
93.1342748291664));
#171679=CARTESIAN_POINT('Ctrl Pts',(-5.14793440076921,6.28637089021504,
93.134271830324));
#171680=CARTESIAN_POINT('Ctrl Pts',(-5.14790480332331,6.28639512756612,
93.134270333142));
#171681=CARTESIAN_POINT('Ctrl Pts',(-5.1478456949008,6.28644353076116,93.1342673431769));
#171682=CARTESIAN_POINT('Ctrl Pts',(-5.14781618444235,6.2864676961829,93.1342658504199));
#171683=CARTESIAN_POINT('Ctrl Pts',(-5.14775724851596,6.28651595673633,
93.1342628692297));
#171684=CARTESIAN_POINT('Ctrl Pts',(-5.14772782422087,6.28654005090968,
93.1342613808557));
#171685=CARTESIAN_POINT('Ctrl Pts',(-5.1331299317171,6.29849340828202,93.1335229793208));
#171686=CARTESIAN_POINT('Ctrl Pts',(-5.11852001434468,6.3103720156092,93.1327869725556));
#171687=CARTESIAN_POINT('Ctrl Pts',(-5.07617719364443,6.34455508712244,
93.1306622885587));
#171688=CARTESIAN_POINT('Ctrl Pts',(-5.04833881046515,6.36672831407095,
93.1292757989198));
#171689=CARTESIAN_POINT('Ctrl Pts',(-4.90865164174788,6.47649669886406,
93.1223676933497));
#171690=CARTESIAN_POINT('Ctrl Pts',(-4.79466379321652,6.56133143621268,
93.1168858369982));
#171691=CARTESIAN_POINT('Ctrl Pts',(-4.33877319253352,6.88239802625623,
93.0954395140046));
#171692=CARTESIAN_POINT('Ctrl Pts',(-3.98118386244098,7.09524706129059,
93.079611751811));
#171693=CARTESIAN_POINT('Ctrl Pts',(-3.47932482357219,7.34403826428309,
93.0579685553326));
#171694=CARTESIAN_POINT('Ctrl Pts',(-3.3480720322742,7.40479658204466,93.052360809731));
#171695=CARTESIAN_POINT('Ctrl Pts',(-3.15285400606348,7.48891300733574,
93.044081327935));
#171696=CARTESIAN_POINT('Ctrl Pts',(-3.09010455951135,7.51502230023901,
93.0414292061999));
#171697=CARTESIAN_POINT('Ctrl Pts',(-2.97633795826776,7.56069337661883,
93.036636225409));
#171698=CARTESIAN_POINT('Ctrl Pts',(-2.92543692094486,7.58053367335228,
93.0344972597739));
#171699=CARTESIAN_POINT('Ctrl Pts',(-2.81284893249944,7.62311553322266,
93.0297777834811));
#171700=CARTESIAN_POINT('Ctrl Pts',(-2.75107823072608,7.64562476707396,
93.0271961261199));
#171701=CARTESIAN_POINT('Ctrl Pts',(-2.68822626829924,7.6676676922617,93.0245769702192));
#171702=CARTESIAN_POINT('Ctrl Pts',(-2.68741116588213,7.66795341235325,
93.0245430047238));
#171703=CARTESIAN_POINT('Ctrl Pts',(-2.68577273413758,7.66852744300086,
93.0244747335468));
#171704=CARTESIAN_POINT('Ctrl Pts',(-2.68494940390215,7.66881575094744,
93.0244404278537));
#171705=CARTESIAN_POINT('Ctrl Pts',(-2.68329413473645,7.66939508213039,
93.0243714604537));
#171706=CARTESIAN_POINT('Ctrl Pts',(-2.6824621948553,7.66968610260478,93.024336798735));
#171707=CARTESIAN_POINT('Ctrl Pts',(-2.68078931157348,7.67027098758548,
93.0242671029184));
#171708=CARTESIAN_POINT('Ctrl Pts',(-2.67994836716445,7.67056484917341,
93.0242320688079));
#171709=CARTESIAN_POINT('Ctrl Pts',(-2.67825706611632,7.67115554929748,
93.0241616112703));
#171710=CARTESIAN_POINT('Ctrl Pts',(-2.6774067084173,7.67145238474707,93.0241261878301));
#171711=CARTESIAN_POINT('Ctrl Pts',(-2.67569615737389,7.67204916992957,
93.0240549340894));
#171712=CARTESIAN_POINT('Ctrl Pts',(-2.6748359629,7.67234911640361,93.0240191037747));
#171713=CARTESIAN_POINT('Ctrl Pts',(-2.492096908845,7.73603504788378,93.0164076486909));
#171714=CARTESIAN_POINT('Ctrl Pts',(-2.30802234411292,7.7929338269881,93.0088040390402));
#171715=CARTESIAN_POINT('Ctrl Pts',(-1.98937177659332,7.87914933227079,
92.9957716765212));
#171716=CARTESIAN_POINT('Ctrl Pts',(-1.85575197798406,7.91168623429992,
92.9903455786219));
#171717=CARTESIAN_POINT('Ctrl Pts',(-1.68232333873733,7.94928123111285,
92.9833665574352));
#171718=CARTESIAN_POINT('Ctrl Pts',(-1.64321399007387,7.95745761548076,
92.9817969119496));
#171719=CARTESIAN_POINT('Ctrl Pts',(-1.56750947413697,7.97270284489567,
92.97876723469));
#171720=CARTESIAN_POINT('Ctrl Pts',(-1.53092294302146,7.97980899224618,
92.9773070694807));
#171721=CARTESIAN_POINT('Ctrl Pts',(-1.41799428261572,8.00093771863274,
92.9728110332754));
#171722=CARTESIAN_POINT('Ctrl Pts',(-1.34149902368857,8.01411832947137,
92.9697807580378));
#171723=CARTESIAN_POINT('Ctrl Pts',(-1.13707977988039,8.046332184652,92.9617111423394));
#171724=CARTESIAN_POINT('Ctrl Pts',(-1.00887049827884,8.06341072092439,
92.9566791044633));
#171725=CARTESIAN_POINT('Ctrl Pts',(-0.727628800987101,8.09406151263356,
92.9456636036322));
#171726=CARTESIAN_POINT('Ctrl Pts',(-0.574508770834238,8.10636878388756,
92.9396807715246));
#171727=CARTESIAN_POINT('Ctrl Pts',(-0.358147343803119,8.11759791234234,
92.9312129433623));
#171728=CARTESIAN_POINT('Ctrl Pts',(-0.295126334846212,8.12013336094641,
92.9287448844243));
#171729=CARTESIAN_POINT('Ctrl Pts',(-0.177200895026892,8.12350305210914,
92.9241212338898));
#171730=CARTESIAN_POINT('Ctrl Pts',(-0.122305084141662,8.12451496619417,
92.9219666822249));
#171731=CARTESIAN_POINT('Ctrl Pts',(-0.0011607983394269,8.12551995835907,
92.9172055995514));
#171732=CARTESIAN_POINT('Ctrl Pts',(0.0650858149596844,8.12525936384979,
92.9145978103414));
#171733=CARTESIAN_POINT('Ctrl Pts',(0.299956336470427,8.12146285162752,
92.9053335486736));
#171734=CARTESIAN_POINT('Ctrl Pts',(0.468464002800469,8.1134871260525,92.8986520410267));
#171735=CARTESIAN_POINT('Ctrl Pts',(0.912682296226523,8.0785760390206,92.8809237290591));
#171736=CARTESIAN_POINT('Ctrl Pts',(1.18747343697251,8.0427784271147,92.8698355522543));
#171737=CARTESIAN_POINT('Ctrl Pts',(1.52827811647357,7.980531656138,92.8559696532123));
#171738=CARTESIAN_POINT('Ctrl Pts',(1.5964961399566,7.96716509276762,92.8531887688841));
#171739=CARTESIAN_POINT('Ctrl Pts',(1.83833220565102,7.91654919514451,92.8433158307784));
#171740=CARTESIAN_POINT('Ctrl Pts',(2.01089271660614,7.8744858948896,92.8362433860448));
#171741=CARTESIAN_POINT('Ctrl Pts',(2.21809746407732,7.81672184208803,92.8277539945724));
#171742=CARTESIAN_POINT('Ctrl Pts',(2.25418717044016,7.80639077529286,92.8262755148005));
#171743=CARTESIAN_POINT('Ctrl Pts',(2.31011222975119,7.78996146246456,92.8239852292487));
#171744=CARTESIAN_POINT('Ctrl Pts',(2.32999792172498,7.78403672840212,92.82317101046));
#171745=CARTESIAN_POINT('Ctrl Pts',(2.36857504070049,7.77238200491378,92.8215918948963));
#171746=CARTESIAN_POINT('Ctrl Pts',(2.38726891412584,7.76666060083999,92.8208268735176));
#171747=CARTESIAN_POINT('Ctrl Pts',(2.42997436181131,7.75342151726488,92.8190797770516));
#171748=CARTESIAN_POINT('Ctrl Pts',(2.45397200170698,7.74585967088433,92.8180984754768));
#171749=CARTESIAN_POINT('Ctrl Pts',(2.53972591951875,7.71839941720727,92.8145927272703));
#171750=CARTESIAN_POINT('Ctrl Pts',(2.60127881422242,7.69787281904638,92.8120778901396));
#171751=CARTESIAN_POINT('Ctrl Pts',(2.71597094843826,7.65809264378464,92.8073876156239));
#171752=CARTESIAN_POINT('Ctrl Pts',(2.7691678703961,7.63901763870767,92.8052103868164));
#171753=CARTESIAN_POINT('Ctrl Pts',(3.07741597590783,7.52484497215556,92.7925702843117));
#171754=CARTESIAN_POINT('Ctrl Pts',(3.32775878974398,7.41753352558002,92.7822000633599));
#171755=CARTESIAN_POINT('Ctrl Pts',(3.73504505369,7.21817018164117,92.7648005642661));
#171756=CARTESIAN_POINT('Ctrl Pts',(3.89513266216882,7.13305564489591,92.7578195040342));
#171757=CARTESIAN_POINT('Ctrl Pts',(4.10088933551553,7.01466640202612,92.7486090125817));
#171758=CARTESIAN_POINT('Ctrl Pts',(4.14924865296453,6.98617017031193,92.746426655974));
#171759=CARTESIAN_POINT('Ctrl Pts',(4.22584581398583,6.93995860942192,92.7429406525475));
#171760=CARTESIAN_POINT('Ctrl Pts',(4.25427670188204,6.92256658176761,92.741640212816));
#171761=CARTESIAN_POINT('Ctrl Pts',(4.31292910439184,6.88618935412041,92.7389436317364));
#171762=CARTESIAN_POINT('Ctrl Pts',(4.34313415428197,6.86717896863493,92.737547265882));
#171763=CARTESIAN_POINT('Ctrl Pts',(4.4029592112796,6.82897382134527,92.7347660487752));
#171764=CARTESIAN_POINT('Ctrl Pts',(4.43258135641589,6.80978382748622,92.7333812705683));
#171765=CARTESIAN_POINT('Ctrl Pts',(4.53115601596589,6.74500889947469,92.7287471131814));
#171766=CARTESIAN_POINT('Ctrl Pts',(4.59953753612754,6.69856508679117,92.7254894978782));
#171767=CARTESIAN_POINT('Ctrl Pts',(4.89761768860853,6.48939637365424,92.711097253402));
#171768=CARTESIAN_POINT('Ctrl Pts',(5.11947728618505,6.31584306981161,92.6998646672219));
#171769=CARTESIAN_POINT('Ctrl Pts',(5.45433753896578,6.02463497878707,92.6821698788836));
#171770=CARTESIAN_POINT('Ctrl Pts',(5.57357839181492,5.91449483959559,92.6757080672187));
#171771=CARTESIAN_POINT('Ctrl Pts',(5.70571001556667,5.78490104061786,92.6683958583227));
#171772=CARTESIAN_POINT('Ctrl Pts',(5.7219115053002,5.76887645568493,92.6674965821061));
#171773=CARTESIAN_POINT('Ctrl Pts',(5.75441706255619,5.73645417691248,92.6656871336822));
#171774=CARTESIAN_POINT('Ctrl Pts',(5.77071898020844,5.72005460723826,92.6647770041508));
#171775=CARTESIAN_POINT('Ctrl Pts',(5.79942210864063,5.69093194653879,92.6631699893924));
#171776=CARTESIAN_POINT('Ctrl Pts',(5.81185200099476,5.67823736164646,92.6624725525816));
#171777=CARTESIAN_POINT('Ctrl Pts',(5.83885967648232,5.65047297531502,92.6609539615564));
#171778=CARTESIAN_POINT('Ctrl Pts',(5.85342090955712,5.6353873712343,92.6601331860287));
#171779=CARTESIAN_POINT('Ctrl Pts',(5.89585593269314,5.59108228243704,92.6577351148585));
#171780=CARTESIAN_POINT('Ctrl Pts',(5.92357052592392,5.5617111143031,92.6561610838476));
#171781=CARTESIAN_POINT('Ctrl Pts',(5.98674842794419,5.49374895380421,92.6525533033023));
#171782=CARTESIAN_POINT('Ctrl Pts',(6.02205967590957,5.45501893827718,92.650522341185));
#171783=CARTESIAN_POINT('Ctrl Pts',(6.37322186484456,5.06229239902528,92.6301634768993));
#171784=CARTESIAN_POINT('Ctrl Pts',(6.65787326611589,4.68161277993397,92.6123034654986));
#171785=CARTESIAN_POINT('Ctrl Pts',(7.10513223955482,3.95947034164228,92.5799817441187));
#171786=CARTESIAN_POINT('Ctrl Pts',(7.28027274382671,3.62738615802649,92.5656351645238));
#171787=CARTESIAN_POINT('Ctrl Pts',(7.46148979324959,3.21733341453781,92.5482222035637));
#171788=CARTESIAN_POINT('Ctrl Pts',(7.49022031307785,3.14986726956872,92.5453671681984));
#171789=CARTESIAN_POINT('Ctrl Pts',(7.53432659891189,3.0422779777039,92.5408282929988));
#171790=CARTESIAN_POINT('Ctrl Pts',(7.55030413776109,3.00240570276799,92.5391492371062));
#171791=CARTESIAN_POINT('Ctrl Pts',(7.57964661642587,2.92746528063591,92.5359988179278));
#171792=CARTESIAN_POINT('Ctrl Pts',(7.59308623667504,2.89242756024388,92.5345280557786));
#171793=CARTESIAN_POINT('Ctrl Pts',(7.62276544197277,2.81341990380907,92.5312163110182));
#171794=CARTESIAN_POINT('Ctrl Pts',(7.63886823647951,2.7694000405867,92.5293744074653));
#171795=CARTESIAN_POINT('Ctrl Pts',(7.67168473108728,2.67722596756345,92.5255241554226));
#171796=CARTESIAN_POINT('Ctrl Pts',(7.68832801744688,2.62904883323022,92.5235154192683));
#171797=CARTESIAN_POINT('Ctrl Pts',(7.73145188360616,2.50030617258792,92.5181570808077));
#171798=CARTESIAN_POINT('Ctrl Pts',(7.75712626932035,2.41947745070647,92.5148028274475));
#171799=CARTESIAN_POINT('Ctrl Pts',(8.00978404278669,1.57865454717926,92.480011156819));
#171800=CARTESIAN_POINT('Ctrl Pts',(8.12556467337259,0.789785411816207,
92.4478184145232));
#171801=CARTESIAN_POINT('Ctrl Pts',(8.1252493577062,-0.0032307267043824,
92.4142825253168));
#171802=CARTESIAN_POINT('',(8.1252500832311,0.00151305119344404,88.4163212481402));
#171803=CARTESIAN_POINT('Ctrl Pts',(8.12524935171145,-0.00324576840847315,
92.4142818892175));
#171804=CARTESIAN_POINT('Ctrl Pts',(8.12505842335934,-0.481203611965918,
92.3940695088115));
#171805=CARTESIAN_POINT('Ctrl Pts',(8.08269529486795,-0.958231732574647,
92.3736492650366));
#171806=CARTESIAN_POINT('Ctrl Pts',(7.99334777073901,-1.45841875622197,
92.3532464736714));
#171807=CARTESIAN_POINT('Ctrl Pts',(7.98788932123645,-1.48802488929236,
92.3520429987674));
#171808=CARTESIAN_POINT('Ctrl Pts',(7.97940221984289,-1.53266530495396,
92.3502353455617));
#171809=CARTESIAN_POINT('Ctrl Pts',(7.97649536800879,-1.5477223171385,92.349626829814));
#171810=CARTESIAN_POINT('Ctrl Pts',(7.97170884541368,-1.57214403720874,
92.3486418882419));
#171811=CARTESIAN_POINT('Ctrl Pts',(7.96985526499509,-1.5815137829795,92.3482644892345));
#171812=CARTESIAN_POINT('Ctrl Pts',(7.96657571697868,-1.59793952572654,
92.3476037670509));
#171813=CARTESIAN_POINT('Ctrl Pts',(7.96515688782877,-1.6049969267631,92.3473201701683));
#171814=CARTESIAN_POINT('Ctrl Pts',(7.96228214280116,-1.61919850529424,
92.3467500770431));
#171815=CARTESIAN_POINT('Ctrl Pts',(7.96082598570614,-1.62634262899425,
92.3464635905037));
#171816=CARTESIAN_POINT('Ctrl Pts',(7.95799786724277,-1.6401229920588,92.3459115749195));
#171817=CARTESIAN_POINT('Ctrl Pts',(7.95662721641338,-1.6467594916934,92.3456459937473));
#171818=CARTESIAN_POINT('Ctrl Pts',(7.95336334885058,-1.66246347533802,
92.3450181865911));
#171819=CARTESIAN_POINT('Ctrl Pts',(7.95146292315046,-1.67152946380344,
92.3446562548924));
#171820=CARTESIAN_POINT('Ctrl Pts',(7.94475632826809,-1.70325303776969,
92.3433916030867));
#171821=CARTESIAN_POINT('Ctrl Pts',(7.93986875634451,-1.72589344203662,
92.3424922907919));
#171822=CARTESIAN_POINT('Ctrl Pts',(7.85233235732887,-2.12314029701398,
92.3267737934708));
#171823=CARTESIAN_POINT('Ctrl Pts',(7.743352541108,-2.49145438816358,92.313276116538));
#171824=CARTESIAN_POINT('Ctrl Pts',(7.56081438047686,-2.97866578084,92.2955747243282));
#171825=CARTESIAN_POINT('Ctrl Pts',(7.50964603274314,-3.10541158989064,
92.2909837202256));
#171826=CARTESIAN_POINT('Ctrl Pts',(7.40089438557037,-3.35636329896071,
92.2818371013519));
#171827=CARTESIAN_POINT('Ctrl Pts',(7.34332080885891,-3.48052466028751,
92.2772829763544));
#171828=CARTESIAN_POINT('Ctrl Pts',(7.15027688353463,-3.8707000123997,92.2627550196844));
#171829=CARTESIAN_POINT('Ctrl Pts',(7.00327648035908,-4.13072509715393,
92.2527375791108));
#171830=CARTESIAN_POINT('Ctrl Pts',(6.62847214826358,-4.71595725761751,
92.2286158630955));
#171831=CARTESIAN_POINT('Ctrl Pts',(6.39050381607807,-5.03371794372861,
92.2142657717043));
#171832=CARTESIAN_POINT('Ctrl Pts',(6.11120177711919,-5.35478736540524,
92.1978795037557));
#171833=CARTESIAN_POINT('Ctrl Pts',(6.09197905753035,-5.37664635540263,
92.1967540145036));
#171834=CARTESIAN_POINT('Ctrl Pts',(6.06395570710275,-5.40816970613807,
92.1951164092528));
#171835=CARTESIAN_POINT('Ctrl Pts',(6.05524847283763,-5.41791697226722,
92.1946080203855));
#171836=CARTESIAN_POINT('Ctrl Pts',(6.04000713593716,-5.43489616781846,
92.1937188742371));
#171837=CARTESIAN_POINT('Ctrl Pts',(6.03348345825478,-5.44213743994845,
92.1933385351767));
#171838=CARTESIAN_POINT('Ctrl Pts',(6.02085020848902,-5.45610969119068,
92.1926024537384));
#171839=CARTESIAN_POINT('Ctrl Pts',(6.01474233671666,-5.46284219227043,
92.1922467799399));
#171840=CARTESIAN_POINT('Ctrl Pts',(6.00022627861805,-5.47878889601,92.1914019580711));
#171841=CARTESIAN_POINT('Ctrl Pts',(5.99180815773963,-5.48799400152999,
92.1909124093009));
#171842=CARTESIAN_POINT('Ctrl Pts',(5.96657690882266,-5.51545678777282,
92.1894462209484));
#171843=CARTESIAN_POINT('Ctrl Pts',(5.94970135709016,-5.53365677783305,
92.1884670531249));
#171844=CARTESIAN_POINT('Ctrl Pts',(5.78631150996949,-5.70825845471638,
92.1790004757031));
#171845=CARTESIAN_POINT('Ctrl Pts',(5.63375465646632,-5.85887492806857,
92.1702645257141));
#171846=CARTESIAN_POINT('Ctrl Pts',(4.99377777470236,-6.44258064973689,
92.134010909694));
#171847=CARTESIAN_POINT('Ctrl Pts',(4.46104316142138,-6.82228572231415,
92.1044865273501));
#171848=CARTESIAN_POINT('Ctrl Pts',(3.74593597174448,-7.21208117126267,
92.0680491058429));
#171849=CARTESIAN_POINT('Ctrl Pts',(3.60079213519847,-7.28563307253746,
92.0608154351659));
#171850=CARTESIAN_POINT('Ctrl Pts',(3.28357387176181,-7.43458717456244,
92.0454683720216));
#171851=CARTESIAN_POINT('Ctrl Pts',(3.11088863640055,-7.50848334935149,
92.0373957570775));
#171852=CARTESIAN_POINT('Ctrl Pts',(2.86919988791821,-7.60213652636437,
92.0266121992681));
#171853=CARTESIAN_POINT('Ctrl Pts',(2.80226905825337,-7.62706213412633,
92.0236794422539));
#171854=CARTESIAN_POINT('Ctrl Pts',(2.69222961912174,-7.66639757178168,
92.0189526964495));
#171855=CARTESIAN_POINT('Ctrl Pts',(2.64931625455858,-7.68133292821855,
92.0171321637149));
#171856=CARTESIAN_POINT('Ctrl Pts',(2.5935717493254,-7.70021124024953,92.0147943568442));
#171857=CARTESIAN_POINT('Ctrl Pts',(2.58085355038893,-7.7044832738915,92.0142627992657));
#171858=CARTESIAN_POINT('Ctrl Pts',(2.56142101905766,-7.71095712955034,
92.0134533155079));
#171859=CARTESIAN_POINT('Ctrl Pts',(2.55471433552318,-7.71318171411346,
92.0131744312009));
#171860=CARTESIAN_POINT('Ctrl Pts',(2.54160451803625,-7.71751122233762,
92.0126302288682));
#171861=CARTESIAN_POINT('Ctrl Pts',(2.53520165189848,-7.71961693204703,
92.0123648784637));
#171862=CARTESIAN_POINT('Ctrl Pts',(2.52054008381536,-7.72441847142617,
92.0117582588712));
#171863=CARTESIAN_POINT('Ctrl Pts',(2.5122796550617,-7.72710903063499,92.011417204592));
#171864=CARTESIAN_POINT('Ctrl Pts',(2.48989312902347,-7.73436100273797,
92.0104948292934));
#171865=CARTESIAN_POINT('Ctrl Pts',(2.47575878426278,-7.73889697310255,
92.0099145236709));
#171866=CARTESIAN_POINT('Ctrl Pts',(2.40907902657994,-7.76009435626059,
92.0071863026476));
#171867=CARTESIAN_POINT('Ctrl Pts',(2.35637671070558,-7.7762597137135,92.005057475186));
#171868=CARTESIAN_POINT('Ctrl Pts',(1.91880342659443,-7.90561936485096,
91.9875831727675));
#171869=CARTESIAN_POINT('Ctrl Pts',(1.52617644287239,-7.99070989218256,
91.9731565700769));
#171870=CARTESIAN_POINT('Ctrl Pts',(0.65733121480216,-8.11260215404912,
91.9416483270983));
#171871=CARTESIAN_POINT('Ctrl Pts',(0.180920321578308,-8.13717724189745,
91.9246033048994));
#171872=CARTESIAN_POINT('Ctrl Pts',(-0.467285113362848,-8.11363605367949,
91.9004039650091));
#171873=CARTESIAN_POINT('Ctrl Pts',(-0.639429355346308,-8.1018870244104,
91.8938888762583));
#171874=CARTESIAN_POINT('Ctrl Pts',(-0.892866035785481,-8.07646187149219,
91.8841435108361));
#171875=CARTESIAN_POINT('Ctrl Pts',(-0.974535876972609,-8.06701467177951,
91.8809796155121));
#171876=CARTESIAN_POINT('Ctrl Pts',(-1.08841842534227,-8.05208660961738,
91.876534505384));
#171877=CARTESIAN_POINT('Ctrl Pts',(-1.12076326449219,-8.04764829802405,
91.8752682525196));
#171878=CARTESIAN_POINT('Ctrl Pts',(-1.17561965942971,-8.03978385529092,
91.8731143530182));
#171879=CARTESIAN_POINT('Ctrl Pts',(-1.19814521431303,-8.03645780579778,
91.8722280807683));
#171880=CARTESIAN_POINT('Ctrl Pts',(-1.2426108016991,-8.02970105802412,
91.8704749969147));
#171881=CARTESIAN_POINT('Ctrl Pts',(-1.2645513546987,-8.02627501108478,
91.8696082602749));
#171882=CARTESIAN_POINT('Ctrl Pts',(-1.31511424041881,-8.01816707507372,
91.867606699519));
#171883=CARTESIAN_POINT('Ctrl Pts',(-1.34372605850098,-8.01342180215072,
91.8664710247729));
#171884=CARTESIAN_POINT('Ctrl Pts',(-1.42060290601495,-8.00024846206587,
91.863410928862));
#171885=CARTESIAN_POINT('Ctrl Pts',(-1.46881794381011,-7.99153689036157,
91.8614825158935));
#171886=CARTESIAN_POINT('Ctrl Pts',(-1.92590640797534,-7.90467307934542,
91.8431067513998));
#171887=CARTESIAN_POINT('Ctrl Pts',(-2.32826042277422,-7.79564894024238,
91.8261689391368));
#171888=CARTESIAN_POINT('Ctrl Pts',(-3.22416733751635,-7.4773106381599,
91.7864489684192));
#171889=CARTESIAN_POINT('Ctrl Pts',(-3.7089531284197,-7.2490737686522,91.7634258258299));
#171890=CARTESIAN_POINT('Ctrl Pts',(-4.3139440213017,-6.88756549782854,
91.7340924264256));
#171891=CARTESIAN_POINT('Ctrl Pts',(-4.45731175435859,-6.79566384252212,
91.7271033758118));
#171892=CARTESIAN_POINT('Ctrl Pts',(-4.62400444865303,-6.68126402747384,
91.7190092461655));
#171893=CARTESIAN_POINT('Ctrl Pts',(-4.65021237455194,-6.66304968090878,
91.717737662791));
#171894=CARTESIAN_POINT('Ctrl Pts',(-4.68586895780281,-6.63795572681863,
91.7160096606297));
#171895=CARTESIAN_POINT('Ctrl Pts',(-4.69541091837173,-6.63120957520054,
91.7155474339711));
#171896=CARTESIAN_POINT('Ctrl Pts',(-4.71068028661942,-6.62036467283925,
91.7148081211404));
#171897=CARTESIAN_POINT('Ctrl Pts',(-4.71641695818835,-6.61627903288656,
91.7145304440098));
#171898=CARTESIAN_POINT('Ctrl Pts',(-4.72831401106654,-6.60778265228595,
91.7139547602278));
#171899=CARTESIAN_POINT('Ctrl Pts',(-4.73447355181724,-6.60337074188031,
91.713656807878));
#171900=CARTESIAN_POINT('Ctrl Pts',(-4.74857450558232,-6.59324074257283,
91.7129749545951));
#171901=CARTESIAN_POINT('Ctrl Pts',(-4.756511786827,-6.58751690300791,91.7125913249666));
#171902=CARTESIAN_POINT('Ctrl Pts',(-4.78148642007465,-6.56943818676379,
91.711384843472));
#171903=CARTESIAN_POINT('Ctrl Pts',(-4.79848620548932,-6.55703138787556,
91.7105645067883));
#171904=CARTESIAN_POINT('Ctrl Pts',(-4.98886920006526,-6.4169489920769,
91.7013891124866));
#171905=CARTESIAN_POINT('Ctrl Pts',(-5.15715367014994,-6.28250069654908,
91.6934317473731));
#171906=CARTESIAN_POINT('Ctrl Pts',(-5.87158677079353,-5.66364550463093,
91.6596826944939));
#171907=CARTESIAN_POINT('Ctrl Pts',(-6.35638927209257,-5.11359565535511,
91.6365014014358));
#171908=CARTESIAN_POINT('Ctrl Pts',(-6.96999327429432,-4.19292145669815,
91.5978076469144));
#171909=CARTESIAN_POINT('Ctrl Pts',(-7.1567255416074,-3.86557129821749,
91.5841156359475));
#171910=CARTESIAN_POINT('Ctrl Pts',(-7.33190603639712,-3.501939893346,91.5685594299608));
#171911=CARTESIAN_POINT('Ctrl Pts',(-7.34360161942063,-3.47734731964003,
91.5675058694669));
#171912=CARTESIAN_POINT('Ctrl Pts',(-7.36057756978936,-3.44118397465222,
91.5659543218603));
#171913=CARTESIAN_POINT('Ctrl Pts',(-7.36595480182881,-3.42965875328092,
91.5654595059189));
#171914=CARTESIAN_POINT('Ctrl Pts',(-7.37538187151951,-3.40932892714083,
91.5645860693891));
#171915=CARTESIAN_POINT('Ctrl Pts',(-7.3794430632071,-3.40052959996873,
91.5642078204962));
#171916=CARTESIAN_POINT('Ctrl Pts',(-7.38732572975457,-3.38336971487406,
91.5634697871345));
#171917=CARTESIAN_POINT('Ctrl Pts',(-7.39114877953382,-3.37500989378892,
91.5631100547497));
#171918=CARTESIAN_POINT('Ctrl Pts',(-7.40135239532739,-3.35259727309577,
91.5621451185898));
#171919=CARTESIAN_POINT('Ctrl Pts',(-7.40770710860408,-3.33853278332889,
91.5615390748387));
#171920=CARTESIAN_POINT('Ctrl Pts',(-7.43059390892505,-3.28749179378601,
91.5593377737918));
#171921=CARTESIAN_POINT('Ctrl Pts',(-7.44688939061198,-3.25041020180114,
91.557734854294));
#171922=CARTESIAN_POINT('Ctrl Pts',(-7.73127792216534,-2.58989750478238,
91.5291153816929));
#171923=CARTESIAN_POINT('Ctrl Pts',(-7.92046442442058,-1.93551286273028,
91.4993975382645));
#171924=CARTESIAN_POINT('Ctrl Pts',(-8.09555644438102,-0.824904926288004,
91.4487556891042));
#171925=CARTESIAN_POINT('Ctrl Pts',(-8.12862370169037,-0.379477489358884,
91.4284797730138));
#171926=CARTESIAN_POINT('Ctrl Pts',(-8.1233811112236,0.261823261431164,
91.4008583400842));
#171927=CARTESIAN_POINT('Ctrl Pts',(-8.1147350968487,0.457122673885287,
91.3926631373492));
#171928=CARTESIAN_POINT('Ctrl Pts',(-8.09620188454295,0.687361246080819,
91.3833820392998));
#171929=CARTESIAN_POINT('Ctrl Pts',(-8.09311814455134,0.722764965676807,
91.3819650505185));
#171930=CARTESIAN_POINT('Ctrl Pts',(-8.0886938707795,0.769974102839919,
91.3800878142285));
#171931=CARTESIAN_POINT('Ctrl Pts',(-8.08755960782569,0.781798085295039,
91.379618668753));
#171932=CARTESIAN_POINT('Ctrl Pts',(-8.08564664531005,0.801289765365157,
91.3788469212852));
#171933=CARTESIAN_POINT('Ctrl Pts',(-8.08488295965956,0.808958892682614,
91.3785436892213));
#171934=CARTESIAN_POINT('Ctrl Pts',(-8.08337588205804,0.823878041257104,
91.37795458838));
#171935=CARTESIAN_POINT('Ctrl Pts',(-8.08263364524238,0.831128169872339,
91.3776686722867));
#171936=CARTESIAN_POINT('Ctrl Pts',(-8.08088798104674,0.847956215363072,
91.3770058674632));
#171937=CARTESIAN_POINT('Ctrl Pts',(-8.07987727707015,0.857533377723981,
91.3766292739572));
#171938=CARTESIAN_POINT('Ctrl Pts',(-8.07709648076216,0.883442048431894,
91.3756121222586));
#171939=CARTESIAN_POINT('Ctrl Pts',(-8.07529387926842,0.89977007109312,
91.3749728514205));
#171940=CARTESIAN_POINT('Ctrl Pts',(-8.06127609237742,1.02330756896937,
91.3701487009231));
#171941=CARTESIAN_POINT('Ctrl Pts',(-8.04697558324632,1.13027241887401,
91.3660431779149));
#171942=CARTESIAN_POINT('Ctrl Pts',(-8.0123703159676,1.35494222932192,91.3575169787508));
#171943=CARTESIAN_POINT('Ctrl Pts',(-7.99159233698791,1.4725486385397,91.3531103430874));
#171944=CARTESIAN_POINT('Ctrl Pts',(-7.96757220555676,1.59295072033581,
91.3486248255663));
#171945=CARTESIAN_POINT('Ctrl Pts',(-7.96691291260701,1.59624480936779,
91.3485021262096));
#171946=CARTESIAN_POINT('Ctrl Pts',(-7.88108809444698,2.02368190299981,
91.3325833416261));
#171947=CARTESIAN_POINT('Ctrl Pts',(-7.76218618186128,2.44035264961898,
91.3173310721145));
#171948=CARTESIAN_POINT('Ctrl Pts',(-7.38182896381088,3.45763961478734,
91.2780985721355));
#171949=CARTESIAN_POINT('Ctrl Pts',(-7.08000058664505,4.03982268048939,
91.253592491344));
#171950=CARTESIAN_POINT('Ctrl Pts',(-6.64649038920768,4.67517493009015,
91.2238768842545));
#171951=CARTESIAN_POINT('Ctrl Pts',(-6.57919193085595,4.76941593158421,
91.2193870090111));
#171952=CARTESIAN_POINT('Ctrl Pts',(-6.47975507934423,4.9025503421081,91.2129142882603));
#171953=CARTESIAN_POINT('Ctrl Pts',(-6.44923256007434,4.94263341764401,
91.2109481468675));
#171954=CARTESIAN_POINT('Ctrl Pts',(-6.39508052940576,5.01239177137345,
91.2074948308176));
#171955=CARTESIAN_POINT('Ctrl Pts',(-6.37161226910041,5.04219033023428,
91.2060094080097));
#171956=CARTESIAN_POINT('Ctrl Pts',(-6.32231805489744,5.10388737797582,
91.2029119772274));
#171957=CARTESIAN_POINT('Ctrl Pts',(-6.29645733162535,5.13575671233051,
91.2012996255017));
#171958=CARTESIAN_POINT('Ctrl Pts',(-6.22817733832225,5.21861027764631,
91.197074682014));
#171959=CARTESIAN_POINT('Ctrl Pts',(-6.18537345127561,5.26927332587732,
91.1944579002746));
#171960=CARTESIAN_POINT('Ctrl Pts',(-5.99508172952204,5.48899014416312,
91.182958465877));
#171961=CARTESIAN_POINT('Ctrl Pts',(-5.84125077012173,5.65241581467839,
91.1740051426395));
#171962=CARTESIAN_POINT('Ctrl Pts',(-5.23401259267453,6.24623169309774,
91.1398484516222));
#171963=CARTESIAN_POINT('Ctrl Pts',(-4.73824640114135,6.63018173264989,
91.1141958390362));
#171964=CARTESIAN_POINT('Ctrl Pts',(-4.15184689095235,6.98466055711986,
91.0867900268546));
#171965=CARTESIAN_POINT('Ctrl Pts',(-4.09995403835374,7.01524715679656,
91.0843888084354));
#171966=CARTESIAN_POINT('Ctrl Pts',(-4.00871769502457,7.06766537741545,
91.0802108059653));
#171967=CARTESIAN_POINT('Ctrl Pts',(-3.96952413483381,7.08975243779715,
91.0784298880653));
#171968=CARTESIAN_POINT('Ctrl Pts',(-3.91103976647934,7.12207358822692,
91.0757936932892));
#171969=CARTESIAN_POINT('Ctrl Pts',(-3.89188800456705,7.13255718651336,
91.0749337872623));
#171970=CARTESIAN_POINT('Ctrl Pts',(-3.85637062794597,7.15181361078047,
91.0733453668089));
#171971=CARTESIAN_POINT('Ctrl Pts',(-3.84001680119728,7.16060774745978,
91.0726164223651));
#171972=CARTESIAN_POINT('Ctrl Pts',(-3.80268631437019,7.18051724599185,
91.0709577978678));
#171973=CARTESIAN_POINT('Ctrl Pts',(-3.78169077768482,7.19159690146912,
91.0700287576463));
#171974=CARTESIAN_POINT('Ctrl Pts',(-3.72627143019361,7.22053270941013,
91.0675859641771));
#171975=CARTESIAN_POINT('Ctrl Pts',(-3.69176774845453,7.23823474973324,
91.0660746805367));
#171976=CARTESIAN_POINT('Ctrl Pts',(-3.39512288244355,7.38775485034545,
91.0531559956734));
#171977=CARTESIAN_POINT('Ctrl Pts',(-3.12614304794733,7.50553227877203,
91.0419277360358));
#171978=CARTESIAN_POINT('Ctrl Pts',(-2.76144160049649,7.64220863852683,
91.0269438001028));
#171979=CARTESIAN_POINT('Ctrl Pts',(-2.67091266854636,7.67431677780503,
91.0232444129725));
#171980=CARTESIAN_POINT('Ctrl Pts',(-2.47330789031504,7.74048165132348,
91.0151973467297));
#171981=CARTESIAN_POINT('Ctrl Pts',(-2.36605201849586,7.77393759320926,
91.0108469649942));
#171982=CARTESIAN_POINT('Ctrl Pts',(-2.21288901281733,7.81824971347053,
91.0046471449027));
#171983=CARTESIAN_POINT('Ctrl Pts',(-2.16752763443435,7.83094696038992,
91.0028125688925));
#171984=CARTESIAN_POINT('Ctrl Pts',(-2.08785921645127,7.85250193660636,
90.9995924705763));
#171985=CARTESIAN_POINT('Ctrl Pts',(-2.05359981972962,7.86153105587192,
90.9982083871306));
#171986=CARTESIAN_POINT('Ctrl Pts',(-1.98651750758213,7.87874228354845,
90.9954991929199));
#171987=CARTESIAN_POINT('Ctrl Pts',(-1.95370036962425,7.88694406188557,
90.9941742733046));
#171988=CARTESIAN_POINT('Ctrl Pts',(-1.86362464715478,7.90885941642402,
90.9905385586053));
#171989=CARTESIAN_POINT('Ctrl Pts',(-1.80626686255547,7.92215589777895,
90.9882244072334));
#171990=CARTESIAN_POINT('Ctrl Pts',(-1.52288304145017,7.98461132735043,
90.9767938824655));
#171991=CARTESIAN_POINT('Ctrl Pts',(-1.29497611251476,8.02472587421883,
90.9676055432242));
#171992=CARTESIAN_POINT('Ctrl Pts',(-0.899631288846099,8.07702934212261,
90.9516949504627));
#171993=CARTESIAN_POINT('Ctrl Pts',(-0.73295176805845,8.09385699717708,
90.944996700409));
#171994=CARTESIAN_POINT('Ctrl Pts',(-0.483764740867235,8.11125351844492,
90.9350312174432));
#171995=CARTESIAN_POINT('Ctrl Pts',(-0.401575173985077,8.11573776301831,
90.9317523502175));
#171996=CARTESIAN_POINT('Ctrl Pts',(-0.236519235434454,8.12222966207281,
90.9251918044932));
#171997=CARTESIAN_POINT('Ctrl Pts',(-0.1536614963144,8.12421961484203,90.9219106377518));
#171998=CARTESIAN_POINT('Ctrl Pts',(-0.0433915389004529,8.12518032569453,
90.9175667432298));
#171999=CARTESIAN_POINT('Ctrl Pts',(-0.0159945855926529,8.12528044651396,
90.9164893669666));
#172000=CARTESIAN_POINT('Ctrl Pts',(0.0311246126927512,8.1252143224437,
90.9146399868386));
#172001=CARTESIAN_POINT('Ctrl Pts',(0.0508466549068599,8.12511483906767,
90.9138669823192));
#172002=CARTESIAN_POINT('Ctrl Pts',(0.0927379508235669,8.12475099746668,
90.9122271246504));
#172003=CARTESIAN_POINT('Ctrl Pts',(0.114906889447252,8.12446770621411,
90.9113605407372));
#172004=CARTESIAN_POINT('Ctrl Pts',(0.174678528441149,8.12345920433265,
90.9090270437801));
#172005=CARTESIAN_POINT('Ctrl Pts',(0.212277884514604,8.12256364399469,
90.9075623332755));
#172006=CARTESIAN_POINT('Ctrl Pts',(0.410289533637737,8.11647145733545,
90.8998621735274));
#172007=CARTESIAN_POINT('Ctrl Pts',(0.570529328250431,8.10678380248141,
90.8936771121736));
#172008=CARTESIAN_POINT('Ctrl Pts',(0.738146505853616,8.09165546339017,
90.8872105155033));
#172009=CARTESIAN_POINT('Ctrl Pts',(0.745913905541872,8.09094313710647,
90.8869108613));
#172010=CARTESIAN_POINT('Ctrl Pts',(0.758089991739835,8.08980881982631,
90.8864411332733));
#172011=CARTESIAN_POINT('Ctrl Pts',(0.762499378216574,8.08939440719417,
90.8862710296603));
#172012=CARTESIAN_POINT('Ctrl Pts',(0.781046822311683,8.08763594104981,
90.8855555156225));
#172013=CARTESIAN_POINT('Ctrl Pts',(0.795181686806233,8.08625842642055,
90.8850102330142));
#172014=CARTESIAN_POINT('Ctrl Pts',(1.12919074835057,8.05282329303902,90.872124606117));
#172015=CARTESIAN_POINT('Ctrl Pts',(1.44688541287374,8.00184708589281,90.8598458307875));
#172016=CARTESIAN_POINT('Ctrl Pts',(1.93827518125358,7.89277233559349,90.8404401137499));
#172017=CARTESIAN_POINT('Ctrl Pts',(2.11445313590129,7.84741057932555,90.8333994335378));
#172018=CARTESIAN_POINT('Ctrl Pts',(2.35772816594149,7.77598497455932,90.8235285081678));
#172019=CARTESIAN_POINT('Ctrl Pts',(2.42622699535237,7.75488535914606,90.8207325924299));
#172020=CARTESIAN_POINT('Ctrl Pts',(2.54659262998274,7.71605836839085,90.8157890045708));
#172021=CARTESIAN_POINT('Ctrl Pts',(2.59857611638289,7.69870722320487,90.8136437870903));
#172022=CARTESIAN_POINT('Ctrl Pts',(2.71067162346707,7.66002707710682,90.808995434294));
#172023=CARTESIAN_POINT('Ctrl Pts',(2.77071608130908,7.63851345698321,90.8064914001613));
#172024=CARTESIAN_POINT('Ctrl Pts',(3.03093284557207,7.54180715014992,90.7955776631422));
#172025=CARTESIAN_POINT('Ctrl Pts',(3.22834564226186,7.4594364886134,90.7871351198037));
#172026=CARTESIAN_POINT('Ctrl Pts',(3.54045019912149,7.31449767165344,90.773550565359));
#172027=CARTESIAN_POINT('Ctrl Pts',(3.65728548036502,7.25678488788619,90.7684101444369));
#172028=CARTESIAN_POINT('Ctrl Pts',(3.81195001304269,7.17570138576113,90.7615432441467));
#172029=CARTESIAN_POINT('Ctrl Pts',(3.85104835727102,7.15479418616419,90.7598019306484));
#172030=CARTESIAN_POINT('Ctrl Pts',(3.92888211788227,7.11235101013043,90.7563255647697));
#172031=CARTESIAN_POINT('Ctrl Pts',(3.96761638651186,7.09081601890673,90.7545905690342));
#172032=CARTESIAN_POINT('Ctrl Pts',(4.10405017880955,7.01349532079928,90.7484585266022));
#172033=CARTESIAN_POINT('Ctrl Pts',(4.20076544139305,6.95599844363115,90.7440733338596));
#172034=CARTESIAN_POINT('Ctrl Pts',(4.42753385257603,6.8147306344274,90.7336672442611));
#172035=CARTESIAN_POINT('Ctrl Pts',(4.55644995166325,6.7292178913974,90.7276510921494));
#172036=CARTESIAN_POINT('Ctrl Pts',(4.74299420821402,6.59765947673265,90.7187522013933));
#172037=CARTESIAN_POINT('Ctrl Pts',(4.80256259945274,6.55442576203791,90.7158804005881));
#172038=CARTESIAN_POINT('Ctrl Pts',(4.91349660793744,6.47158745378478,90.7104702896059));
#172039=CARTESIAN_POINT('Ctrl Pts',(4.96499144285993,6.43216550043001,90.7079331248165));
#172040=CARTESIAN_POINT('Ctrl Pts',(5.05903336332086,6.3583692872391,90.7032489603322));
#172041=CARTESIAN_POINT('Ctrl Pts',(5.10171594507861,6.3241736974093,90.7011032320043));
#172042=CARTESIAN_POINT('Ctrl Pts',(5.19745837952696,6.24586859217749,90.6962434586398));
#172043=CARTESIAN_POINT('Ctrl Pts',(5.2503080970434,6.20150892200208,90.6935277699459));
#172044=CARTESIAN_POINT('Ctrl Pts',(5.42107198749079,6.05442974433913,90.6846400050332));
#172045=CARTESIAN_POINT('Ctrl Pts',(5.53658609489731,5.94897930780426,90.6784475269729));
#172046=CARTESIAN_POINT('Ctrl Pts',(5.708784618676,5.78242055209065,90.6689219859997));
#172047=CARTESIAN_POINT('Ctrl Pts',(5.76769264749142,5.72366409826613,90.6656076192812));
#172048=CARTESIAN_POINT('Ctrl Pts',(6.05595737740519,5.42717110802156,90.649107262818));
#172049=CARTESIAN_POINT('Ctrl Pts',(6.2715688290078,5.17650747689679,90.6358455569801));
#172050=CARTESIAN_POINT('Ctrl Pts',(6.52492714692229,4.84281646419253,90.6191435876034));
#172051=CARTESIAN_POINT('Ctrl Pts',(6.57737322787202,4.77134228053209,90.6156185724485));
#172052=CARTESIAN_POINT('Ctrl Pts',(6.6636150196082,4.64968600562255,90.609712239386));
#172053=CARTESIAN_POINT('Ctrl Pts',(6.69803878232654,4.59995887194802,90.6073236300737));
#172054=CARTESIAN_POINT('Ctrl Pts',(6.7468094438123,4.52779840622776,90.6038960850108));
#172055=CARTESIAN_POINT('Ctrl Pts',(6.76160614039066,4.50567181318994,90.602850254712));
#172056=CARTESIAN_POINT('Ctrl Pts',(6.78729471093643,4.46684626232615,90.6010243560557));
#172057=CARTESIAN_POINT('Ctrl Pts',(6.79823433602036,4.45017920316605,90.6002434809412));
#172058=CARTESIAN_POINT('Ctrl Pts',(6.82102753581601,4.41517244958797,90.5986096455649));
#172059=CARTESIAN_POINT('Ctrl Pts',(6.83286870397685,4.39682495473045,90.5977569482588));
#172060=CARTESIAN_POINT('Ctrl Pts',(6.8678157767539,4.34219350105677,90.5952285383212));
#172061=CARTESIAN_POINT('Ctrl Pts',(6.89070769285334,4.30577350392393,90.5935566521223));
#172062=CARTESIAN_POINT('Ctrl Pts',(7.01128707904653,4.11051260733063,90.5846595043369));
#172063=CARTESIAN_POINT('Ctrl Pts',(7.10377486359895,3.94852434612612,90.5775097858551));
#172064=CARTESIAN_POINT('Ctrl Pts',(7.29946042047614,3.57662015134091,90.5614204825523));
#172065=CARTESIAN_POINT('Ctrl Pts',(7.39933384346655,3.36514372325678,90.5524925014136));
#172066=CARTESIAN_POINT('Ctrl Pts',(7.5151754928027,3.08966982036721,90.5409917619867));
#172067=CARTESIAN_POINT('Ctrl Pts',(7.53967931108845,3.02938246532366,90.5384828334626));
#172068=CARTESIAN_POINT('Ctrl Pts',(7.59557543996705,2.88697918405588,90.5325712458664));
#172069=CARTESIAN_POINT('Ctrl Pts',(7.62636444839535,2.80463548864361,90.5291642165655));
#172070=CARTESIAN_POINT('Ctrl Pts',(7.67031490120036,2.68101315291072,90.5240612195728));
#172071=CARTESIAN_POINT('Ctrl Pts',(7.68449230917389,2.64010229737503,90.52237441491));
#172072=CARTESIAN_POINT('Ctrl Pts',(7.70955205335733,2.56587662228152,90.5193170146055));
#172073=CARTESIAN_POINT('Ctrl Pts',(7.72054713774887,2.53260095309486,90.5179474597811));
#172074=CARTESIAN_POINT('Ctrl Pts',(7.74389349593736,2.46038011108299,90.5149771127785));
#172075=CARTESIAN_POINT('Ctrl Pts',(7.75616698953386,2.42141082461412,90.5133756762879));
#172076=CARTESIAN_POINT('Ctrl Pts',(7.7896006515906,2.31239347205932,90.5088989331611));
#172077=CARTESIAN_POINT('Ctrl Pts',(7.81010919269671,2.24214990342071,90.5060181752852));
#172078=CARTESIAN_POINT('Ctrl Pts',(7.90802502920438,1.88912243097763,90.4915574114181));
#172079=CARTESIAN_POINT('Ctrl Pts',(7.9710347882669,1.60257423619999,90.4798633240962));
#172080=CARTESIAN_POINT('Ctrl Pts',(8.03709931818856,1.19919940771406,90.4635632038446));
#172081=CARTESIAN_POINT('Ctrl Pts',(8.05334343845133,1.0847600271667,90.4589582474047));
#172082=CARTESIAN_POINT('Ctrl Pts',(8.07542142679531,0.901147770464904,
90.4516179620861));
#172083=CARTESIAN_POINT('Ctrl Pts',(8.08281983295966,0.832179166244986,
90.448871669956));
#172084=CARTESIAN_POINT('Ctrl Pts',(8.09185129570428,0.736443058619626,
90.445078571604));
#172085=CARTESIAN_POINT('Ctrl Pts',(8.0942362859731,0.709749761734331,90.4440230282214));
#172086=CARTESIAN_POINT('Ctrl Pts',(8.09808970661824,0.664073160073507,
90.4422206475326));
#172087=CARTESIAN_POINT('Ctrl Pts',(8.09962355277197,0.645095624372311,
90.4414729304123));
#172088=CARTESIAN_POINT('Ctrl Pts',(8.10263537568211,0.606126529522303,
90.4399400016355));
#172089=CARTESIAN_POINT('Ctrl Pts',(8.1041060961854,0.586134613656314,90.4391549295779));
#172090=CARTESIAN_POINT('Ctrl Pts',(8.10797637599821,0.530723036462772,
90.4369826175858));
#172091=CARTESIAN_POINT('Ctrl Pts',(8.1102178121944,0.495292754092089,90.4355977436771));
#172092=CARTESIAN_POINT('Ctrl Pts',(8.1209324651078,0.30627476080668,90.4282290802179));
#172093=CARTESIAN_POINT('Ctrl Pts',(8.12527528680073,0.152482634071241,
90.4223022292362));
#172094=CARTESIAN_POINT('Ctrl Pts',(8.12518271962617,-0.408164824613424,
90.4008194375387));
#172095=CARTESIAN_POINT('Ctrl Pts',(8.09456184015827,-0.814411358661026,
90.3854750239771));
#172096=CARTESIAN_POINT('Ctrl Pts',(8.01329831773149,-1.35099982575277,
90.3648074063706));
#172097=CARTESIAN_POINT('Ctrl Pts',(7.98958556584053,-1.48481400039786,
90.3596212478413));
#172098=CARTESIAN_POINT('Ctrl Pts',(7.91719876860025,-1.84105174690529,
90.3456915675978));
#172099=CARTESIAN_POINT('Ctrl Pts',(7.8625146010107,-2.06212749824494,90.3369157345911));
#172100=CARTESIAN_POINT('Ctrl Pts',(7.77992147002927,-2.34455711449415,
90.3254753073271));
#172101=CARTESIAN_POINT('Ctrl Pts',(7.76043598262427,-2.40826897211862,
90.3228793279538));
#172102=CARTESIAN_POINT('Ctrl Pts',(7.72766479458903,-2.51089108532431,
90.3186721328723));
#172103=CARTESIAN_POINT('Ctrl Pts',(7.71486341593251,-2.5499528778852,90.3170646257152));
#172104=CARTESIAN_POINT('Ctrl Pts',(7.68968758102669,-2.62484847594072,
90.3139704637209));
#172105=CARTESIAN_POINT('Ctrl Pts',(7.67735765767219,-2.66069614969036,
90.3124841709913));
#172106=CARTESIAN_POINT('Ctrl Pts',(7.64810768966756,-2.74384027633678,
90.3090243208187));
#172107=CARTESIAN_POINT('Ctrl Pts',(7.63099903444572,-2.79106868554986,
90.3070494925645));
#172108=CARTESIAN_POINT('Ctrl Pts',(7.57333148197439,-2.94576505771821,
90.3005490832461));
#172109=CARTESIAN_POINT('Ctrl Pts',(7.53093176954014,-3.05253140006581,
90.2960117301884));
#172110=CARTESIAN_POINT('Ctrl Pts',(7.24063132542835,-3.74063207893818,
90.2664312475233));
#172111=CARTESIAN_POINT('Ctrl Pts',(6.92790189115822,-4.29222494661871,
90.24109092315));
#172112=CARTESIAN_POINT('Ctrl Pts',(6.30402987340626,-5.14377472163197,
90.196923818038));
#172113=CARTESIAN_POINT('Ctrl Pts',(6.02728066116209,-5.46544475642925,
90.1788354203407));
#172114=CARTESIAN_POINT('Ctrl Pts',(5.54484102054954,-5.94475867008302,
90.150300386213));
#172115=CARTESIAN_POINT('Ctrl Pts',(5.35450697115553,-6.11675429334298,
90.1396870958048));
#172116=CARTESIAN_POINT('Ctrl Pts',(5.14095158550991,-6.29211423239948,
90.1286948831446));
#172117=CARTESIAN_POINT('Ctrl Pts',(5.12550340574968,-6.30470455803753,
90.1279047007098));
#172118=CARTESIAN_POINT('Ctrl Pts',(5.10250147082359,-6.32331080563039,
90.1267356930883));
#172119=CARTESIAN_POINT('Ctrl Pts',(5.0949831203597,-6.32937025371377,90.1263547853934));
#172120=CARTESIAN_POINT('Ctrl Pts',(5.08208854918351,-6.33972482777154,
90.1257035608141));
#172121=CARTESIAN_POINT('Ctrl Pts',(5.07671764991323,-6.34402654605534,
90.1254329208068));
#172122=CARTESIAN_POINT('Ctrl Pts',(5.06568701152103,-6.35283834494368,
90.124878349087));
#172123=CARTESIAN_POINT('Ctrl Pts',(5.06002669775017,-6.35734769806882,
90.1245944536989));
#172124=CARTESIAN_POINT('Ctrl Pts',(5.04694262298147,-6.36774273002923,
90.1239398002049));
#172125=CARTESIAN_POINT('Ctrl Pts',(5.03951456869824,-6.37362300645182,
90.1235693162647));
#172126=CARTESIAN_POINT('Ctrl Pts',(5.01621366711223,-6.39200251759296,
90.1224108716322));
#172127=CARTESIAN_POINT('Ctrl Pts',(5.00030439782131,-6.40445561137356,
90.121625305358));
#172128=CARTESIAN_POINT('Ctrl Pts',(4.71661439354119,-6.62481452121287,
90.1077153933778));
#172129=CARTESIAN_POINT('Ctrl Pts',(4.43612901854739,-6.81581818552268,
90.09562272667));
#172130=CARTESIAN_POINT('Ctrl Pts',(3.95773085766111,-7.09952262916357,
90.0765072060474));
#172131=CARTESIAN_POINT('Ctrl Pts',(3.76655789871067,-7.20277030281036,
90.0692263203532));
#172132=CARTESIAN_POINT('Ctrl Pts',(3.32598231851155,-7.41837101108613,
90.0528514664966));
#172133=CARTESIAN_POINT('Ctrl Pts',(3.0745850425301,-7.52604224681035,90.0437827234198));
#172134=CARTESIAN_POINT('Ctrl Pts',(2.32875672566864,-7.80185513884065,
90.0168251869194));
#172135=CARTESIAN_POINT('Ctrl Pts',(1.823023844337,-7.9352732018687,89.9984035940042));
#172136=CARTESIAN_POINT('Ctrl Pts',(1.27586993066572,-8.02451894913138,
89.9770927868911));
#172137=CARTESIAN_POINT('Ctrl Pts',(1.24369254336064,-8.0295689344628,89.9758349492949));
#172138=CARTESIAN_POINT('Ctrl Pts',(1.19896070361978,-8.03631390879297,
89.9740798262728));
#172139=CARTESIAN_POINT('Ctrl Pts',(1.18643116187188,-8.03817324433148,
89.9735875008642));
#172140=CARTESIAN_POINT('Ctrl Pts',(1.16485239359985,-8.04132389716096,
89.9727383706191));
#172141=CARTESIAN_POINT('Ctrl Pts',(1.15580522572121,-8.04262925898276,
89.9723819896282));
#172142=CARTESIAN_POINT('Ctrl Pts',(1.13713608098323,-8.04529076649055,
89.9716458120258));
#172143=CARTESIAN_POINT('Ctrl Pts',(1.12751383723432,-8.04664492382568,
89.9712659561655));
#172144=CARTESIAN_POINT('Ctrl Pts',(1.10512450221637,-8.04975487070984,
89.9703811051861));
#172145=CARTESIAN_POINT('Ctrl Pts',(1.09235563313169,-8.05149755094252,
89.9698757166854));
#172146=CARTESIAN_POINT('Ctrl Pts',(1.05170670172599,-8.05694679221253,
89.9682644424323));
#172147=CARTESIAN_POINT('Ctrl Pts',(1.02381165478707,-8.06053895687019,
89.9671551248516));
#172148=CARTESIAN_POINT('Ctrl Pts',(0.482310945039678,-8.12741405226549,
89.9455503650096));
#172149=CARTESIAN_POINT('Ctrl Pts',(-0.0360949542220756,-8.14162538655109,
89.9235322627249));
#172150=CARTESIAN_POINT('Ctrl Pts',(-1.32616396610698,-8.05373574904508,
89.8662998001465));
#172151=CARTESIAN_POINT('Ctrl Pts',(-2.08855333395648,-7.89046719698669,
89.8301401358532));
#172152=CARTESIAN_POINT('Ctrl Pts',(-2.85440477185994,-7.60747762182899,
89.7971850584204));
#172153=CARTESIAN_POINT('Ctrl Pts',(-2.89245649945786,-7.5930914555651,
89.795556835486));
#172154=CARTESIAN_POINT('Ctrl Pts',(-2.9428712085305,-7.57359725792394,
89.7934100585827));
#172155=CARTESIAN_POINT('Ctrl Pts',(-2.95533147886672,-7.56874376816158,
89.7928803237333));
#172156=CARTESIAN_POINT('Ctrl Pts',(-2.97470799792059,-7.5611411360792,
89.7920578082562));
#172157=CARTESIAN_POINT('Ctrl Pts',(-2.98163251272359,-7.55841322713757,
89.7917641191758));
#172158=CARTESIAN_POINT('Ctrl Pts',(-2.9955271003613,-7.55291739637152,
89.7911752953547));
#172159=CARTESIAN_POINT('Ctrl Pts',(-3.00249710806778,-7.55014933110006,
89.7908801671053));
#172160=CARTESIAN_POINT('Ctrl Pts',(-3.01810397394759,-7.54392619908828,
89.7902198655022));
#172161=CARTESIAN_POINT('Ctrl Pts',(-3.0267387595794,-7.54046593898535,
89.7898549081862));
#172162=CARTESIAN_POINT('Ctrl Pts',(-3.05215445995236,-7.53023028988641,
89.7887817248986));
#172163=CARTESIAN_POINT('Ctrl Pts',(-3.06891876230982,-7.52341363363619,
89.7880751796552));
#172164=CARTESIAN_POINT('Ctrl Pts',(-3.19928011008044,-7.46989821653667,
89.7825904880507));
#172165=CARTESIAN_POINT('Ctrl Pts',(-3.31183102438735,-7.42068389556017,
89.7779111824683));
#172166=CARTESIAN_POINT('Ctrl Pts',(-3.72771337855501,-7.22748650304879,
89.7607044202216));
#172167=CARTESIAN_POINT('Ctrl Pts',(-4.02315272642039,-7.06729555358356,
89.7486366167324));
#172168=CARTESIAN_POINT('Ctrl Pts',(-4.84462124104432,-6.55363441005245,
89.7138484427421));
#172169=CARTESIAN_POINT('Ctrl Pts',(-5.34030911041913,-6.15642295476436,
89.6910921975045));
#172170=CARTESIAN_POINT('Ctrl Pts',(-5.84624133465654,-5.64347342438746,
89.6635593193846));
#172171=CARTESIAN_POINT('Ctrl Pts',(-5.90662120225961,-5.5802469238601,
89.6601975851622));
#172172=CARTESIAN_POINT('Ctrl Pts',(-5.98906348670876,-5.49108035128396,
89.6554997013062));
#172173=CARTESIAN_POINT('Ctrl Pts',(-6.01200125196499,-5.46595698875673,
89.6541806740617));
#172174=CARTESIAN_POINT('Ctrl Pts',(-6.04866033216221,-5.42529496140551,
89.6520532826715));
#172175=CARTESIAN_POINT('Ctrl Pts',(-6.06248118476256,-5.40984649626293,
89.6512467452121));
#172176=CARTESIAN_POINT('Ctrl Pts',(-6.09077363225227,-5.37797760990128,
89.6495864444536));
#172177=CARTESIAN_POINT('Ctrl Pts',(-6.10523830978567,-5.36155124843075,
89.6487325802365));
#172178=CARTESIAN_POINT('Ctrl Pts',(-6.1375795416018,-5.32452335118314,
89.6468119736052));
#172179=CARTESIAN_POINT('Ctrl Pts',(-6.15541906715872,-5.30388985994851,
89.6457445852264));
#172180=CARTESIAN_POINT('Ctrl Pts',(-6.20822378785311,-5.24218980580471,
89.6425608500608));
#172181=CARTESIAN_POINT('Ctrl Pts',(-6.24288418163928,-5.2008646963119,
89.6404389984451));
#172182=CARTESIAN_POINT('Ctrl Pts',(-6.65728776487264,-4.69666512462372,
89.6146659730834));
#172183=CARTESIAN_POINT('Ctrl Pts',(-6.98513006277759,-4.19356681760353,
89.5899124066949));
#172184=CARTESIAN_POINT('Ctrl Pts',(-7.30206009909252,-3.5652012278945,
89.5601061331467));
#172185=CARTESIAN_POINT('Ctrl Pts',(-7.34758055389546,-3.4704180445728,
89.5556436407094));
#172186=CARTESIAN_POINT('Ctrl Pts',(-7.53587425402126,-3.05802784377165,
89.5364055710946));
#172187=CARTESIAN_POINT('Ctrl Pts',(-7.65999263378856,-2.73229944403452,
89.5216399975741));
#172188=CARTESIAN_POINT('Ctrl Pts',(-7.78960354694572,-2.31300265156048,
89.5037336892653));
#172189=CARTESIAN_POINT('Ctrl Pts',(-7.81492387124996,-2.22595378264975,
89.5000754152648));
#172190=CARTESIAN_POINT('Ctrl Pts',(-7.84301194590939,-2.12299538157213,
89.4958302426727));
#172191=CARTESIAN_POINT('Ctrl Pts',(-7.84719518148492,-2.10748038231436,
89.4951927023057));
#172192=CARTESIAN_POINT('Ctrl Pts',(-7.85384187502791,-2.08253460200741,
89.4941712200543));
#172193=CARTESIAN_POINT('Ctrl Pts',(-7.85633442603922,-2.0731116597331,
89.493786189224));
#172194=CARTESIAN_POINT('Ctrl Pts',(-7.86073277071643,-2.05636212280665,
89.4931032684786));
#172195=CARTESIAN_POINT('Ctrl Pts',(-7.86264528963465,-2.04903731605556,
89.4928051206491));
#172196=CARTESIAN_POINT('Ctrl Pts',(-7.86660738779841,-2.03377554427642,
89.4921849685775));
#172197=CARTESIAN_POINT('Ctrl Pts',(-7.86865519940246,-2.02583812576148,
89.4918630337216));
#172198=CARTESIAN_POINT('Ctrl Pts',(-7.8739286966889,-2.00526915955052,
89.4910303414374));
#172199=CARTESIAN_POINT('Ctrl Pts',(-7.87713600710106,-1.99263289417064,
89.4905203179258));
#172200=CARTESIAN_POINT('Ctrl Pts',(-7.89060168345194,-1.93903979467075,
89.4883638223817));
#172201=CARTESIAN_POINT('Ctrl Pts',(-7.90057125945608,-1.89801056811157,
89.4867292523952));
#172202=CARTESIAN_POINT('Ctrl Pts',(-7.96767364179614,-1.61216145065336,
89.4754630653817));
#172203=CARTESIAN_POINT('Ctrl Pts',(-8.01373824124433,-1.36487827364246,
89.466364858333));
#172204=CARTESIAN_POINT('Ctrl Pts',(-8.11173717626938,-0.658045495434903,
89.4413578800126));
#172205=CARTESIAN_POINT('Ctrl Pts',(-8.13603435273741,-0.195644302811646,
89.4261405526653));
#172206=CARTESIAN_POINT('Ctrl Pts',(-8.10888515299584,0.632203037266909,
89.3980883161775));
#172207=CARTESIAN_POINT('Ctrl Pts',(-8.07217407440557,0.996837365785144,
89.3854525729938));
#172208=CARTESIAN_POINT('Ctrl Pts',(-7.97552435984112,1.56709534165181,
89.3644266744));
#172209=CARTESIAN_POINT('Ctrl Pts',(-7.93185036206105,1.77497019717706,
89.3564950543029));
#172210=CARTESIAN_POINT('Ctrl Pts',(-7.87405094778067,2.00489954792567,
89.3473587460818));
#172211=CARTESIAN_POINT('Ctrl Pts',(-7.86790538911031,2.02888277156754,
89.3464013404125));
#172212=CARTESIAN_POINT('Ctrl Pts',(-7.85850276855301,2.06489152452899,
89.3449571304162));
#172213=CARTESIAN_POINT('Ctrl Pts',(-7.85532748201763,2.07693835249014,
89.3444728280881));
#172214=CARTESIAN_POINT('Ctrl Pts',(-7.84978847673069,2.09775856379603,
89.3436338406103));
#172215=CARTESIAN_POINT('Ctrl Pts',(-7.84743772080945,2.10653538749041,
89.3432795532693));
#172216=CARTESIAN_POINT('Ctrl Pts',(-7.84253419964623,2.12472114275437,
89.3425441933551));
#172217=CARTESIAN_POINT('Ctrl Pts',(-7.83997921313987,2.13412945808166,
89.3421630530401));
#172218=CARTESIAN_POINT('Ctrl Pts',(-7.83395520332092,2.15615506516431,
89.3412691138995));
#172219=CARTESIAN_POINT('Ctrl Pts',(-7.8304726252741,2.1687686035123,89.3407558991244));
#172220=CARTESIAN_POINT('Ctrl Pts',(-7.8191221785521,2.20949500011694,89.3390946884782));
#172221=CARTESIAN_POINT('Ctrl Pts',(-7.81113330752014,2.23757373717886,
89.337942970676));
#172222=CARTESIAN_POINT('Ctrl Pts',(-7.69242828774203,2.64640625297348,
89.3210793096807));
#172223=CARTESIAN_POINT('Ctrl Pts',(-7.55414855445613,3.01856015283658,
89.3044967474096));
#172224=CARTESIAN_POINT('Ctrl Pts',(-7.15226094770793,3.89738907133433,
89.2624376826757));
#172225=CARTESIAN_POINT('Ctrl Pts',(-6.86138408668688,4.38928467715351,
89.2363024335274));
#172226=CARTESIAN_POINT('Ctrl Pts',(-6.29179464735972,5.15570291752874,
89.1937509860266));
#172227=CARTESIAN_POINT('Ctrl Pts',(-6.04039578984724,5.448088970018,89.1770341733334));
#172228=CARTESIAN_POINT('Ctrl Pts',(-5.75242219518411,5.73845723051182,
89.1607068087172));
#172229=CARTESIAN_POINT('Ctrl Pts',(-5.73561105045182,5.75526006304766,
89.1597625772463));
#172230=CARTESIAN_POINT('Ctrl Pts',(-5.71207265279435,5.77858125323408,
89.1584524631018));
#172231=CARTESIAN_POINT('Ctrl Pts',(-5.70540760142429,5.7851620023687,89.1580828229311));
#172232=CARTESIAN_POINT('Ctrl Pts',(-5.69388160661996,5.7965029198255,89.1574458540481));
#172233=CARTESIAN_POINT('Ctrl Pts',(-5.68902604513137,5.80126852575976,
89.157178206343));
#172234=CARTESIAN_POINT('Ctrl Pts',(-5.67896664127495,5.81111679136435,
89.1566251218141));
#172235=CARTESIAN_POINT('Ctrl Pts',(-5.6737619468636,5.81619857349645,89.1563397354763));
#172236=CARTESIAN_POINT('Ctrl Pts',(-5.66158972521399,5.82805145306758,
89.1556740961599));
#172237=CARTESIAN_POINT('Ctrl Pts',(-5.65461685455987,5.83481706529293,
89.1552941522696));
#172238=CARTESIAN_POINT('Ctrl Pts',(-5.63249210562934,5.85620727938735,
89.1540928640061));
#172239=CARTESIAN_POINT('Ctrl Pts',(-5.61729543024625,5.87078555891169,
89.1532740570907));
#172240=CARTESIAN_POINT('Ctrl Pts',(-5.47611900656491,6.0051670942049,89.1457237655605));
#172241=CARTESIAN_POINT('Ctrl Pts',(-5.34637635352792,6.12096197293031,
89.1391974955641));
#172242=CARTESIAN_POINT('Ctrl Pts',(-5.0626159403596,6.35830575418146,89.1255550559194));
#172243=CARTESIAN_POINT('Ctrl Pts',(-4.90770986836957,6.47862014829483,
89.1184738842969));
#172244=CARTESIAN_POINT('Ctrl Pts',(-4.50287078323803,6.77019554513883,
89.1005546120604));
#172245=CARTESIAN_POINT('Ctrl Pts',(-4.24744016081709,6.93329973721904,
89.0897750202761));
#172246=CARTESIAN_POINT('Ctrl Pts',(-3.4331266125429,7.39135209565812,89.0559827931577));
#172247=CARTESIAN_POINT('Ctrl Pts',(-2.84856797903184,7.63570676960402,
89.0322819002105));
#172248=CARTESIAN_POINT('Ctrl Pts',(-2.1276827222347,7.8426218416518,89.003321133802));
#172249=CARTESIAN_POINT('Ctrl Pts',(-2.01299352668427,7.87283988335273,
88.99872487553));
#172250=CARTESIAN_POINT('Ctrl Pts',(-1.85187465694265,7.91154014506264,
88.9922728041213));
#172251=CARTESIAN_POINT('Ctrl Pts',(-1.80596976234776,7.92214493713761,
88.9904350909155));
#172252=CARTESIAN_POINT('Ctrl Pts',(-1.72237544491579,7.94069227076996,
88.9870888384705));
#172253=CARTESIAN_POINT('Ctrl Pts',(-1.68471677375682,7.94876721830031,
88.9855814793114));
#172254=CARTESIAN_POINT('Ctrl Pts',(-1.61263649592199,7.96368775760905,
88.9826961432325));
#172255=CARTESIAN_POINT('Ctrl Pts',(-1.57822513552084,7.97057868536676,
88.9813185932865));
#172256=CARTESIAN_POINT('Ctrl Pts',(-1.49382681276644,7.98691159221029,
88.9779394344096));
#172257=CARTESIAN_POINT('Ctrl Pts',(-1.44379383382703,7.99610746931643,
88.9759357383075));
#172258=CARTESIAN_POINT('Ctrl Pts',(-1.26794906118604,8.02672284740343,
88.9688906615199));
#172259=CARTESIAN_POINT('Ctrl Pts',(-1.14172292393769,8.04564744087221,
88.9638280864338));
#172260=CARTESIAN_POINT('Ctrl Pts',(-0.831910395821181,8.08465861124717,
88.9513790554654));
#172261=CARTESIAN_POINT('Ctrl Pts',(-0.647985112404765,8.10147478662085,
88.943968090165));
#172262=CARTESIAN_POINT('Ctrl Pts',(-0.179362750217856,8.12825929532021,
88.9250265478514));
#172263=CARTESIAN_POINT('Ctrl Pts',(0.105579271624881,8.1295523276579,88.9134511427758));
#172264=CARTESIAN_POINT('Ctrl Pts',(0.495012894545222,8.11083864444987,
88.8976078253616));
#172265=CARTESIAN_POINT('Ctrl Pts',(0.599920788761437,8.1037544649407,88.8933381627985));
#172266=CARTESIAN_POINT('Ctrl Pts',(0.864935160890542,8.08068418790813,
88.8825583506172));
#172267=CARTESIAN_POINT('Ctrl Pts',(1.02476030812926,8.06197476037542,88.8760626490737));
#172268=CARTESIAN_POINT('Ctrl Pts',(1.28179714072594,8.02411803545976,88.865655261502));
#172269=CARTESIAN_POINT('Ctrl Pts',(1.37939809289287,8.00791704707015,88.8617127388967));
#172270=CARTESIAN_POINT('Ctrl Pts',(1.5071516391476,7.98430596572611,88.8565713278));
#172271=CARTESIAN_POINT('Ctrl Pts',(1.53759121642721,7.97849992685588,88.8553477302));
#172272=CARTESIAN_POINT('Ctrl Pts',(1.58498171275378,7.96917939150578,88.8534452514913));
#172273=CARTESIAN_POINT('Ctrl Pts',(1.60195574489754,7.96578464418748,88.8527643498375));
#172274=CARTESIAN_POINT('Ctrl Pts',(1.63419410754808,7.95922987226993,88.8514720600122));
#172275=CARTESIAN_POINT('Ctrl Pts',(1.64946038657398,7.95608012627226,88.8508604902488));
#172276=CARTESIAN_POINT('Ctrl Pts',(1.66476845224285,7.95287580474031,88.8502475762809));
#172277=CARTESIAN_POINT('Ctrl Pts',(1.66481937012427,7.95286514597504,88.8502455376023));
#172278=CARTESIAN_POINT('Ctrl Pts',(1.66492108428459,7.95284385288047,88.8502414651214));
#172279=CARTESIAN_POINT('Ctrl Pts',(1.66497188694735,7.95283321721693,88.8502394310633));
#172280=CARTESIAN_POINT('Ctrl Pts',(1.66507338034592,7.95281196830691,88.8502353674359));
#172281=CARTESIAN_POINT('Ctrl Pts',(1.66512407112647,7.95280135505329,88.8502333378648));
#172282=CARTESIAN_POINT('Ctrl Pts',(1.66522534182941,7.952780150746,88.8502292831682));
#172283=CARTESIAN_POINT('Ctrl Pts',(1.66527592187131,7.95276955966952,88.850227258038));
#172284=CARTESIAN_POINT('Ctrl Pts',(1.66537697233916,7.95274839946301,88.8502232121737));
#172285=CARTESIAN_POINT('Ctrl Pts',(1.66542744284085,7.95273783031929,88.8502211914365));
#172286=CARTESIAN_POINT('Ctrl Pts',(1.66552827521413,7.95271671377837,88.8502171543186));
#172287=CARTESIAN_POINT('Ctrl Pts',(1.66557863719679,7.95270616636006,88.8502151379335));
#172288=CARTESIAN_POINT('Ctrl Pts',(1.66567925431037,7.95268509290393,88.8502111094484));
#172289=CARTESIAN_POINT('Ctrl Pts',(1.6657295091604,7.95267456692707,88.8502090973597));
#172290=CARTESIAN_POINT('Ctrl Pts',(1.66582991270533,7.95265353621427,88.8502050774397));
#172291=CARTESIAN_POINT('Ctrl Pts',(1.66588006142232,7.95264303147582,88.8502030696074));
#172292=CARTESIAN_POINT('Ctrl Pts',(1.66598025409047,7.95262204295508,88.8501990581445));
#172293=CARTESIAN_POINT('Ctrl Pts',(1.66603029793201,7.95261155919782,88.8501970545182));
#172294=CARTESIAN_POINT('Ctrl Pts',(1.66613028170609,7.9525906124662,88.850193051433));
#172295=CARTESIAN_POINT('Ctrl Pts',(1.66618022176059,7.9525801494683,88.8501910519692));
#172296=CARTESIAN_POINT('Ctrl Pts',(1.66627999872396,7.95255924410156,88.8501870571781));
#172297=CARTESIAN_POINT('Ctrl Pts',(1.66632983587104,7.95254880168483,88.8501850618413));
#172298=CARTESIAN_POINT('Ctrl Pts',(1.66642940900573,7.95252793707027,88.8501810752249));
#172299=CARTESIAN_POINT('Ctrl Pts',(1.66647914463274,7.95251751494999,88.8501790839597));
#172300=CARTESIAN_POINT('Ctrl Pts',(1.66657851568945,7.95249669073268,88.8501751054478));
#172301=CARTESIAN_POINT('Ctrl Pts',(1.66662815099231,7.95248628866418,88.8501731182062));
#172302=CARTESIAN_POINT('Ctrl Pts',(1.66672732160777,7.95246550451291,88.8501691477331));
#172303=CARTESIAN_POINT('Ctrl Pts',(1.66677685731049,7.95245512235032,88.8501671644861));
#172304=CARTESIAN_POINT('Ctrl Pts',(1.66687583076972,7.95243437758824,88.8501632019203));
#172305=CARTESIAN_POINT('Ctrl Pts',(1.66692526833097,7.95242401503159,88.8501612226094));
#172306=CARTESIAN_POINT('Ctrl Pts',(1.66702404567895,7.95240330945115,88.8501572679089));
#172307=CARTESIAN_POINT('Ctrl Pts',(1.6670733858044,7.95239296635825,88.8501552925058));
#172308=CARTESIAN_POINT('Ctrl Pts',(1.66717197016231,7.95237229931652,88.8501513455456));
#172309=CARTESIAN_POINT('Ctrl Pts',(1.66722121416035,7.9523619754187,88.8501493739979));
#172310=CARTESIAN_POINT('Ctrl Pts',(1.66731960715735,7.95234134658532,88.8501454347127));
#172311=CARTESIAN_POINT('Ctrl Pts',(1.66736875606876,7.95233104166995,88.8501434669787));
#172312=CARTESIAN_POINT('Ctrl Pts',(1.66746695988346,7.9523104505992,88.8501395352811));
#172313=CARTESIAN_POINT('Ctrl Pts',(1.66751601478815,7.95230016444533,88.8501375713175));
#172314=CARTESIAN_POINT('Ctrl Pts',(1.66761403137255,7.9522796107388,88.8501336471293));
#172315=CARTESIAN_POINT('Ctrl Pts',(1.66766299322739,7.95226934315121,88.8501316868978));
#172316=CARTESIAN_POINT('Ctrl Pts',(1.6677608247379,7.95224882636747,88.8501277701326));
#172317=CARTESIAN_POINT('Ctrl Pts',(1.66780969448112,7.95223857715474,88.8501258135955));
#172318=CARTESIAN_POINT('Ctrl Pts',(1.6679073434729,7.95221809676855,88.850121904151));
#172319=CARTESIAN_POINT('Ctrl Pts',(1.66795612242823,7.95220786565833,88.8501199512553));
#172320=CARTESIAN_POINT('Ctrl Pts',(1.66805359009366,7.95218742143006,88.8501160490836));
#172321=CARTESIAN_POINT('Ctrl Pts',(1.66810227901195,7.95217720827008,88.8501140997992));
#172322=CARTESIAN_POINT('Ctrl Pts',(1.66819956810043,7.95215679963338,88.8501102047902));
#172323=CARTESIAN_POINT('Ctrl Pts',(1.66824816817235,7.95214660417899,88.8501082590694));
#172324=CARTESIAN_POINT('Ctrl Pts',(1.66834528020997,7.95212623082394,88.8501043711618));
#172325=CARTESIAN_POINT('Ctrl Pts',(1.66839379229784,7.95211605289932,88.85010242897));
#172326=CARTESIAN_POINT('Ctrl Pts',(1.66849072973474,7.95209571432195,88.8500985480657));
#172327=CARTESIAN_POINT('Ctrl Pts',(1.66853915499677,7.9520855536891,88.8500966093566));
#172328=CARTESIAN_POINT('Ctrl Pts',(1.66863591935687,7.95206524957961,88.8500927353945));
#172329=CARTESIAN_POINT('Ctrl Pts',(1.66868425863351,7.95205510606713,88.8500908001344));
#172330=CARTESIAN_POINT('Ctrl Pts',(1.66878085223562,7.95203483594877,88.8500869330216));
#172331=CARTESIAN_POINT('Ctrl Pts',(1.66882910655204,7.9520247093464,88.8500850011693));
#172332=CARTESIAN_POINT('Ctrl Pts',(1.66892553126456,7.95200447283676,88.8500811408309));
#172333=CARTESIAN_POINT('Ctrl Pts',(1.66897370158346,7.95199436294729,88.8500792123479));
#172334=CARTESIAN_POINT('Ctrl Pts',(1.66906995950465,7.95197415961555,88.8500753586999));
#172335=CARTESIAN_POINT('Ctrl Pts',(1.6691180469154,7.95196406621506,88.8500734335425));
#172336=CARTESIAN_POINT('Ctrl Pts',(1.66921413973107,7.95194389571682,88.8500695865173));
#172337=CARTESIAN_POINT('Ctrl Pts',(1.66926214518335,7.95193381861066,88.8500676646475));
#172338=CARTESIAN_POINT('Ctrl Pts',(1.66935807458162,7.95191368060086,88.8500638241774));
#172339=CARTESIAN_POINT('Ctrl Pts',(1.66940599876927,7.95190361964801,88.8500619055674));
#172340=CARTESIAN_POINT('Ctrl Pts',(1.66950176755887,7.9518835135462,88.8500580715399));
#172341=CARTESIAN_POINT('Ctrl Pts',(1.66954961180593,7.95187346847324,88.8500561561366));
#172342=CARTESIAN_POINT('Ctrl Pts',(1.66964522089916,7.95185339409692,88.8500523285151));
#172343=CARTESIAN_POINT('Ctrl Pts',(1.6696929859104,7.95184336476038,88.8500504162903));
#172344=CARTESIAN_POINT('Ctrl Pts',(1.66978843780129,7.95182332159483,88.8500465949749));
#172345=CARTESIAN_POINT('Ctrl Pts',(1.66983612464723,7.95181330777436,88.8500446858856));
#172346=CARTESIAN_POINT('Ctrl Pts',(1.66993142072348,7.95179329553699,88.8500408708207));
#172347=CARTESIAN_POINT('Ctrl Pts',(1.66997903011656,7.95178329708737,88.8500389648385));
#172348=CARTESIAN_POINT('Ctrl Pts',(1.67007417293841,7.95176331524921,88.8500351559215));
#172349=CARTESIAN_POINT('Ctrl Pts',(1.67012170606736,7.95175333192509,88.8500332529987));
#172350=CARTESIAN_POINT('Ctrl Pts',(1.6702166970154,7.95173338020476,88.8500294501743));
#172351=CARTESIAN_POINT('Ctrl Pts',(1.67026415486125,7.95172341180433,88.8500275502716));
#172352=CARTESIAN_POINT('Ctrl Pts',(1.67035899524484,7.95170348993528,88.8500237534872));
#172353=CARTESIAN_POINT('Ctrl Pts',(1.67040637831794,7.95169353635557,88.8500218565841));
#172354=CARTESIAN_POINT('Ctrl Pts',(1.67050107108084,7.95167364372776,88.8500180657219));
#172355=CARTESIAN_POINT('Ctrl Pts',(1.67054838060708,7.95166370471538,88.8500161717694));
#172356=CARTESIAN_POINT('Ctrl Pts',(1.67064292675272,7.95164384112624,88.8500123867892));
#172357=CARTESIAN_POINT('Ctrl Pts',(1.67069016346372,7.95163391653158,88.8500104957578));
#172358=CARTESIAN_POINT('Ctrl Pts',(1.67078456523525,7.95161408151794,88.8500067165697));
#172359=CARTESIAN_POINT('Ctrl Pts',(1.67083173013139,7.95160417113483,88.8500048284194));
#172360=CARTESIAN_POINT('Ctrl Pts',(1.67092598909531,7.95158436437554,88.8500010549605));
#172361=CARTESIAN_POINT('Ctrl Pts',(1.67097308305781,7.9515744680228,88.8499991696561));
#172362=CARTESIAN_POINT('Ctrl Pts',(1.67106720112198,7.95155468912484,88.8499954018501));
#172363=CARTESIAN_POINT('Ctrl Pts',(1.67111422514948,7.95154480659651,88.8499935193515));
#172364=CARTESIAN_POINT('Ctrl Pts',(1.67120820354349,7.95152505530927,88.8499897571491));
#172365=CARTESIAN_POINT('Ctrl Pts',(1.67125515820758,7.95151518648909,88.8499878774334));
#172366=CARTESIAN_POINT('Ctrl Pts',(1.67134899953809,7.9514954622724,88.8499841207301));
#172367=CARTESIAN_POINT('Ctrl Pts',(1.67139588595541,7.95148560692949,88.8499822437525));
#172368=CARTESIAN_POINT('Ctrl Pts',(1.67148959142806,7.95146590953747,88.8499784925001));
#172369=CARTESIAN_POINT('Ctrl Pts',(1.67153641041523,7.95145606750393,88.849976618228));
#172370=CARTESIAN_POINT('Ctrl Pts',(1.67162998189814,7.95143639655136,88.8499728723515));
#172371=CARTESIAN_POINT('Ctrl Pts',(1.67167673435268,7.95142656764221,88.8499710007489));
#172372=CARTESIAN_POINT('Ctrl Pts',(1.67177017332727,7.951406922825,88.8499672601891));
#172373=CARTESIAN_POINT('Ctrl Pts',(1.6718168599382,7.95139710689904,88.8499653912284));
#172374=CARTESIAN_POINT('Ctrl Pts',(1.67191016873911,7.95137748773359,88.8499616558917));
#172375=CARTESIAN_POINT('Ctrl Pts',(1.6719567906492,7.95136768455413,88.849959789527));
#172376=CARTESIAN_POINT('Ctrl Pts',(1.67204997017649,7.95134809085832,88.8499560593773));
#172377=CARTESIAN_POINT('Ctrl Pts',(1.67209652801234,7.95133830029716,88.8499541955836));
#172378=CARTESIAN_POINT('Ctrl Pts',(1.67218958040073,7.95131873162915,88.8499504705355));
#172379=CARTESIAN_POINT('Ctrl Pts',(1.67223607501202,7.9513089535111,88.8499486092787));
#172380=CARTESIAN_POINT('Ctrl Pts',(1.69051708949392,7.94746417026244,88.8492167909699));
#172381=CARTESIAN_POINT('Ctrl Pts',(1.70873839997131,7.94356644402831,88.8484878191919));
#172382=CARTESIAN_POINT('Ctrl Pts',(1.75275318835579,7.93399277376195,88.8467278101983));
#172383=CARTESIAN_POINT('Ctrl Pts',(1.77853274489257,7.92825367630113,88.845697693053));
#172384=CARTESIAN_POINT('Ctrl Pts',(1.84840750267653,7.91234005446961,88.8429068281838));
#172385=CARTESIAN_POINT('Ctrl Pts',(1.89244652377259,7.90192265322539,88.8411492050519));
#172386=CARTESIAN_POINT('Ctrl Pts',(2.03825877972754,7.86614196765674,88.8353299027209));
#172387=CARTESIAN_POINT('Ctrl Pts',(2.13962821389219,7.83917595433868,88.8312843935935));
#172388=CARTESIAN_POINT('Ctrl Pts',(2.51601643308847,7.73120533239011,88.8162090013297));
#172389=CARTESIAN_POINT('Ctrl Pts',(2.78720745961225,7.63762717267808,88.8052285836044));
#172390=CARTESIAN_POINT('Ctrl Pts',(3.13462478321105,7.49677229173001,88.7907242815448));
#172391=CARTESIAN_POINT('Ctrl Pts',(3.21581968476767,7.46230332718995,88.7873030667635));
#172392=CARTESIAN_POINT('Ctrl Pts',(3.33596618740773,7.4089734499219,88.7821878542553));
#172393=CARTESIAN_POINT('Ctrl Pts',(3.37535461144747,7.39111217709105,88.7805023492889));
#172394=CARTESIAN_POINT('Ctrl Pts',(3.44423749853242,7.35921072591055,88.7775390640543));
#172395=CARTESIAN_POINT('Ctrl Pts',(3.47379343707519,7.34530554866485,88.7762624865879));
#172396=CARTESIAN_POINT('Ctrl Pts',(3.50398791523402,7.33087695265173,88.7749529617756));
#172397=CARTESIAN_POINT('Ctrl Pts',(3.50471110853462,7.3305312393264,88.7749215939515));
#172398=CARTESIAN_POINT('Ctrl Pts',(3.50610889220126,7.32986279256006,88.7748609602919));
#172399=CARTESIAN_POINT('Ctrl Pts',(3.50678348920247,7.32954007299134,88.774831694579));
#172400=CARTESIAN_POINT('Ctrl Pts',(3.50808734786371,7.32891610055553,88.7747751245863));
#172401=CARTESIAN_POINT('Ctrl Pts',(3.50871661530199,7.32861485976219,88.7747478204134));
#172402=CARTESIAN_POINT('Ctrl Pts',(3.50993287252752,7.32803242463337,88.7746950418725));
#172403=CARTESIAN_POINT('Ctrl Pts',(3.51051986735411,7.32775124079955,88.7746695675972));
#172404=CARTESIAN_POINT('Ctrl Pts',(3.51165443745904,7.32720758837244,88.7746203257272));
#172405=CARTESIAN_POINT('Ctrl Pts',(3.51220201709886,7.32694512892754,88.7745965582142));
#172406=CARTESIAN_POINT('Ctrl Pts',(3.51326042580475,7.32643767897748,88.7745506148163));
#172407=CARTESIAN_POINT('Ctrl Pts',(3.51377125869094,7.32619269641907,88.7745284390013));
#172408=CARTESIAN_POINT('Ctrl Pts',(3.51475866454932,7.32571903446287,88.7744855715675));
#172409=CARTESIAN_POINT('Ctrl Pts',(3.51523524084668,7.32549036197752,88.7744648800096));
#172410=CARTESIAN_POINT('Ctrl Pts',(3.51615645644207,7.32504823052992,88.7744248808368));
#172411=CARTESIAN_POINT('Ctrl Pts',(3.51660109862707,7.32483477758398,88.7744055732752));
#172412=CARTESIAN_POINT('Ctrl Pts',(3.51746061155895,7.32442206733422,88.7743682485835));
#172413=CARTESIAN_POINT('Ctrl Pts',(3.51787548479433,7.32422281527564,88.7743502315009));
#172414=CARTESIAN_POINT('Ctrl Pts',(3.51867747786589,7.32383755648087,88.7743154005835));
#172415=CARTESIAN_POINT('Ctrl Pts',(3.51906459991257,7.32365155428646,88.7742985867879));
#172416=CARTESIAN_POINT('Ctrl Pts',(3.51981297099499,7.32329190817685,88.7742660811703));
#172417=CARTESIAN_POINT('Ctrl Pts',(3.52017422191131,7.3231182682341,88.7742503893843));
#172418=CARTESIAN_POINT('Ctrl Pts',(3.52087260222681,7.32278251905136,88.7742200520507));
#172419=CARTESIAN_POINT('Ctrl Pts',(3.52120973332843,7.32262041323657,88.7742054065316));
#172420=CARTESIAN_POINT('Ctrl Pts',(3.52186150570261,7.32230696017691,88.7741770911489));
#172421=CARTESIAN_POINT('Ctrl Pts',(3.52217614837717,7.32215561595136,88.7741634213137));
#172422=CARTESIAN_POINT('Ctrl Pts',(3.52278446350025,7.32186296596925,88.77413699154));
#172423=CARTESIAN_POINT('Ctrl Pts',(3.52307813720634,7.32172166282285,88.7741242316248));
#172424=CARTESIAN_POINT('Ctrl Pts',(3.52364592975664,7.32144842341717,88.7740995604223));
#172425=CARTESIAN_POINT('Ctrl Pts',(3.52392004971366,7.32131648942145,88.7740876491544));
#172426=CARTESIAN_POINT('Ctrl Pts',(3.52445005317281,7.32106136197773,88.7740646181565));
#172427=CARTESIAN_POINT('Ctrl Pts',(3.52470593760193,7.32093817052067,88.7740534984452));
#172428=CARTESIAN_POINT('Ctrl Pts',(3.52520069786971,7.32069994416747,88.7740319973751));
#172429=CARTESIAN_POINT('Ctrl Pts',(3.52543957456747,7.32058491098002,88.7740216160303));
#172430=CARTESIAN_POINT('Ctrl Pts',(3.52590146341588,7.32036245646727,88.7740015421248));
#172431=CARTESIAN_POINT('Ctrl Pts',(3.52612447622289,7.32025503667431,88.7739918495802));
#172432=CARTESIAN_POINT('Ctrl Pts',(3.5267231487737,7.31996663710141,88.7739658293606));
#172433=CARTESIAN_POINT('Ctrl Pts',(3.52709879953588,7.31978563857414,88.7739495015177));
#172434=CARTESIAN_POINT('Ctrl Pts',(3.5278447240471,7.31942616155599,88.7739170778351));
#172435=CARTESIAN_POINT('Ctrl Pts',(3.52821500372824,7.31924768121248,88.7739009817619));
#172436=CARTESIAN_POINT('Ctrl Pts',(3.52895030846885,7.31889318456538,88.7738690163697));
#172437=CARTESIAN_POINT('Ctrl Pts',(3.52931532831221,7.31871717174947,88.7738531473013));
#172438=CARTESIAN_POINT('Ctrl Pts',(3.53004020960219,7.31836756665899,88.7738216318054));
#172439=CARTESIAN_POINT('Ctrl Pts',(3.5304000713832,7.318193975163,88.7738059853862));
#172440=CARTESIAN_POINT('Ctrl Pts',(3.53111473785338,7.31784916664837,88.7737749108517));
#172441=CARTESIAN_POINT('Ctrl Pts',(3.53146954290853,7.31767795036179,88.7737594827425));
#172442=CARTESIAN_POINT('Ctrl Pts',(3.5668227225724,7.30061459459707,88.7722221316159));
#172443=CARTESIAN_POINT('Ctrl Pts',(3.60169938983743,7.283471650579,88.7706980015291));
#172444=CARTESIAN_POINT('Ctrl Pts',(3.71112519627361,7.22870736249288,88.7658918703864));
#172445=CARTESIAN_POINT('Ctrl Pts',(3.78521782309246,7.19018680259269,88.7626020019635));
#172446=CARTESIAN_POINT('Ctrl Pts',(3.95743783503906,7.09725022401292,88.7548691933391));
#172447=CARTESIAN_POINT('Ctrl Pts',(4.05505775975313,7.04193022237695,88.7504191709854));
#172448=CARTESIAN_POINT('Ctrl Pts',(4.30808479402424,6.89153638821055,88.7387100668404));
#172449=CARTESIAN_POINT('Ctrl Pts',(4.4614946859479,6.7932269962844,88.7314319650879));
#172450=CARTESIAN_POINT('Ctrl Pts',(4.63451451329279,6.67396030726475,88.7230376628884));
#172451=CARTESIAN_POINT('Ctrl Pts',(4.6574769082477,6.65795612834693,88.7219197597267));
#172452=CARTESIAN_POINT('Ctrl Pts',(4.83115343290541,6.53557004669835,88.7134360740931));
#172453=CARTESIAN_POINT('Ctrl Pts',(4.97828937697914,6.42420075580505,88.7060839895282));
#172454=CARTESIAN_POINT('Ctrl Pts',(5.1477992327665,6.2865727969523,88.697469812716));
#172455=CARTESIAN_POINT('Ctrl Pts',(5.17395702526198,6.26506210569217,88.6961363628367));
#172456=CARTESIAN_POINT('Ctrl Pts',(5.21408643206903,6.23163921347777,88.6940847981277));
#172457=CARTESIAN_POINT('Ctrl Pts',(5.22815331613201,6.21984224174736,88.6933645398367));
#172458=CARTESIAN_POINT('Ctrl Pts',(5.25641634197733,6.19597627373232,88.6919150691661));
#172459=CARTESIAN_POINT('Ctrl Pts',(5.27061116083888,6.18390594516789,88.691185882192));
#172460=CARTESIAN_POINT('Ctrl Pts',(5.3043333703737,6.15503036428025,88.6894505134672));
#172461=CARTESIAN_POINT('Ctrl Pts',(5.32382262114243,6.13818083752522,88.6884451195529));
#172462=CARTESIAN_POINT('Ctrl Pts',(5.38857805724869,6.08165579572339,88.6850956615029));
#172463=CARTESIAN_POINT('Ctrl Pts',(5.43348362870176,6.04156986390969,88.6827582811085));
#172464=CARTESIAN_POINT('Ctrl Pts',(5.54379938578207,5.94086927430945,88.6769734639496));
#172465=CARTESIAN_POINT('Ctrl Pts',(5.60866511508464,5.87966964567739,88.6735337463379));
#172466=CARTESIAN_POINT('Ctrl Pts',(5.91256680548846,5.58333773235736,88.6571982699304));
#172467=CARTESIAN_POINT('Ctrl Pts',(6.13790438452492,5.33462626158836,88.6444094449906));
#172468=CARTESIAN_POINT('Ctrl Pts',(6.48402356277164,4.90154409291292,88.6230786880931));
#172469=CARTESIAN_POINT('Ctrl Pts',(6.61383529685443,4.72492086223655,88.6146125841701));
#172470=CARTESIAN_POINT('Ctrl Pts',(6.77430694368877,4.48698800709822,88.6034455967781));
#172471=CARTESIAN_POINT('Ctrl Pts',(6.81155823579529,4.43023366088691,88.6007991147627));
#172472=CARTESIAN_POINT('Ctrl Pts',(6.87520499438304,4.33056362971405,88.5961799833609));
#172473=CARTESIAN_POINT('Ctrl Pts',(6.90192068751406,4.28785679194547,88.5942097192014));
#172474=CARTESIAN_POINT('Ctrl Pts',(6.9556547748926,4.2001557546557,88.5901815024958));
#172475=CARTESIAN_POINT('Ctrl Pts',(6.98263784749714,4.15514264255737,88.5881234222509));
#172476=CARTESIAN_POINT('Ctrl Pts',(7.03915699892522,4.05875201792674,88.5837360663347));
#172477=CARTESIAN_POINT('Ctrl Pts',(7.06857091480966,4.00730637640782,88.5814062291663));
#172478=CARTESIAN_POINT('Ctrl Pts',(7.11106552853481,3.93105842705016,88.5779705028089));
#172479=CARTESIAN_POINT('Ctrl Pts',(7.12458487840021,3.90650273469349,88.5768666460595));
#172480=CARTESIAN_POINT('Ctrl Pts',(7.17413269186415,3.81539446600728,88.5727807837816));
#172481=CARTESIAN_POINT('Ctrl Pts',(7.20935785455462,3.74840954342111,88.5697958734544));
#172482=CARTESIAN_POINT('Ctrl Pts',(7.33647824020812,3.49825225653681,88.5587216815198));
#172483=CARTESIAN_POINT('Ctrl Pts',(7.42236997097542,3.31211505759345,88.5506232726255));
#172484=CARTESIAN_POINT('Ctrl Pts',(7.51408843924093,3.09181155545818,88.5412369821999));
#172485=CARTESIAN_POINT('Ctrl Pts',(7.52685018019015,3.06061270648176,88.5399123114768));
#172486=CARTESIAN_POINT('Ctrl Pts',(7.5530628704052,2.9953744962503,88.5371523402626));
#172487=CARTESIAN_POINT('Ctrl Pts',(7.5664786859088,2.96132190103057,88.5357174445022));
#172488=CARTESIAN_POINT('Ctrl Pts',(7.59422610417411,2.88947249994869,88.5327014995566));
#172489=CARTESIAN_POINT('Ctrl Pts',(7.60850663693776,2.85165710006786,88.5311207752705));
#172490=CARTESIAN_POINT('Ctrl Pts',(7.64483038215455,2.75325488886063,88.5270228213042));
#172491=CARTESIAN_POINT('Ctrl Pts',(7.6664357465347,2.69250942985338,88.5245080898386));
#172492=CARTESIAN_POINT('Ctrl Pts',(7.74483358703632,2.46348949941982,88.5150736395329));
#172493=CARTESIAN_POINT('Ctrl Pts',(7.7968269997611,2.2936252049468,88.5081687161023));
#172494=CARTESIAN_POINT('Ctrl Pts',(7.87061194258034,2.02093053441564,88.4971578010027));
#172495=CARTESIAN_POINT('Ctrl Pts',(7.89604774694241,1.91914627884673,88.4930642662152));
#172496=CARTESIAN_POINT('Ctrl Pts',(7.93133437247057,1.76533876374054,88.4868922301827));
#172497=CARTESIAN_POINT('Ctrl Pts',(7.94265939674813,1.71366495137517,88.4848209888653));
#172498=CARTESIAN_POINT('Ctrl Pts',(7.96396641593782,1.6116933966234,88.4807367955979));
#172499=CARTESIAN_POINT('Ctrl Pts',(7.973978487304,1.56140441337418,88.4787240989503));
#172500=CARTESIAN_POINT('Ctrl Pts',(7.99338702442752,1.45885917842703,88.4746218237507));
#172501=CARTESIAN_POINT('Ctrl Pts',(8.00274864987357,1.40659882234479,88.4725321458228));
#172502=CARTESIAN_POINT('Ctrl Pts',(8.02348828981748,1.28390539588085,88.467627176302));
#172503=CARTESIAN_POINT('Ctrl Pts',(8.03445213608582,1.21340686246497,88.4648096100065));
#172504=CARTESIAN_POINT('Ctrl Pts',(8.09819219755517,0.764712417395979,
88.4468758723622));
#172505=CARTESIAN_POINT('Ctrl Pts',(8.12517874796852,0.383346495983037,
88.4316036140856));
#172506=CARTESIAN_POINT('Ctrl Pts',(8.12524985909245,0.00151321447761893,
88.4163208663708));
#172507=CARTESIAN_POINT('',(8.12631724021387,0.00268884911775716,84.4167025567875));
#172508=CARTESIAN_POINT('Ctrl Pts',(8.12524985911998,0.00151306666855575,
88.4163208604548));
#172509=CARTESIAN_POINT('Ctrl Pts',(8.12528447581569,-0.184380461877274,
88.4088805349657));
#172510=CARTESIAN_POINT('Ctrl Pts',(8.11893963366032,-0.370222552557259,
88.4014489082081));
#172511=CARTESIAN_POINT('Ctrl Pts',(8.10137240488833,-0.62648991633224,
88.3912508305079));
#172512=CARTESIAN_POINT('Ctrl Pts',(8.0955911985821,-0.697228592091197,
88.3884412278708));
#172513=CARTESIAN_POINT('Ctrl Pts',(8.08645389199681,-0.793481059717428,
88.3846286508366));
#172514=CARTESIAN_POINT('Ctrl Pts',(8.08390232606959,-0.819067719003989,
88.3836161632892));
#172515=CARTESIAN_POINT('Ctrl Pts',(8.07919089809966,-0.864144964454268,
88.3818343871552));
#172516=CARTESIAN_POINT('Ctrl Pts',(8.07708185707336,-0.88364063095439,
88.3810644295474));
#172517=CARTESIAN_POINT('Ctrl Pts',(8.07275417006443,-0.922334625505273,
88.3795376542191));
#172518=CARTESIAN_POINT('Ctrl Pts',(8.07053756305378,-0.94153305737122,
88.378780812204));
#172519=CARTESIAN_POINT('Ctrl Pts',(8.06563264578545,-0.982725048093576,
88.3771585169738));
#172520=CARTESIAN_POINT('Ctrl Pts',(8.0629228358995,-1.00471580217326,88.3762934389335));
#172521=CARTESIAN_POINT('Ctrl Pts',(8.0544373054714,-1.07133188350332,88.3736757208578));
#172522=CARTESIAN_POINT('Ctrl Pts',(8.04838079891667,-1.11592063498418,
88.3719273377086));
#172523=CARTESIAN_POINT('Ctrl Pts',(8.03093910895339,-1.23679135802114,
88.3671944774183));
#172524=CARTESIAN_POINT('Ctrl Pts',(8.01883767034917,-1.31296549146983,
88.3642189371654));
#172525=CARTESIAN_POINT('Ctrl Pts',(7.96641459473931,-1.61512116312082,
88.352419925684));
#172526=CARTESIAN_POINT('Ctrl Pts',(7.91760916830698,-1.83952275062591,
88.3436623035118));
#172527=CARTESIAN_POINT('Ctrl Pts',(7.81026647807734,-2.24875015665204,
88.3274570707364));
#172528=CARTESIAN_POINT('Ctrl Pts',(7.7544930375797,-2.43412744671116,88.3200254854521));
#172529=CARTESIAN_POINT('Ctrl Pts',(7.6677520194328,-2.68905289181744,88.309606750686));
#172530=CARTESIAN_POINT('Ctrl Pts',(7.64234763733064,-2.76042550688426,
88.3066678798717));
#172531=CARTESIAN_POINT('Ctrl Pts',(7.61454795398322,-2.83520073088127,
88.3035636766145));
#172532=CARTESIAN_POINT('Ctrl Pts',(7.61314407820166,-2.83896829366363,
88.3034072031183));
#172533=CARTESIAN_POINT('Ctrl Pts',(7.61041160073841,-2.84628480480384,
88.3031032036105));
#172534=CARTESIAN_POINT('Ctrl Pts',(7.60908331156872,-2.8498338688956,88.3029556803782));
#172535=CARTESIAN_POINT('Ctrl Pts',(7.60648038184221,-2.85677385983538,
88.3026670886896));
#172536=CARTESIAN_POINT('Ctrl Pts',(7.60520595540433,-2.86016486613274,
88.3025260221496));
#172537=CARTESIAN_POINT('Ctrl Pts',(7.59231493296727,-2.89439589089042,
88.3011014437266));
#172538=CARTESIAN_POINT('Ctrl Pts',(7.58051310331934,-2.92516575537113,
88.2998163062399));
#172539=CARTESIAN_POINT('Ctrl Pts',(7.55674124862312,-2.98603389052831,
88.2972647101583));
#172540=CARTESIAN_POINT('Ctrl Pts',(7.54477778803705,-3.01613408438214,
88.2959983320068));
#172541=CARTESIAN_POINT('Ctrl Pts',(7.51662627282288,-3.08574794222829,
88.2930586963622));
#172542=CARTESIAN_POINT('Ctrl Pts',(7.50030609389936,-3.12520709193206,
88.2913842812909));
#172543=CARTESIAN_POINT('Ctrl Pts',(7.4505167497896,-3.24295179237185,88.2863630038643));
#172544=CARTESIAN_POINT('Ctrl Pts',(7.41612754282025,-3.32084150422497,
88.2830081444316));
#172545=CARTESIAN_POINT('Ctrl Pts',(7.24090391329714,-3.70141085691617,
88.2664501396477));
#172546=CARTESIAN_POINT('Ctrl Pts',(7.08273252838164,-3.99575114803389,
88.2531017579556));
#172547=CARTESIAN_POINT('Ctrl Pts',(6.86541905644188,-4.34648293916053,
88.2366739868948));
#172548=CARTESIAN_POINT('Ctrl Pts',(6.822957997981,-4.41283775025868,88.2335427076409));
#172549=CARTESIAN_POINT('Ctrl Pts',(6.75869344365595,-4.51011981396591,
88.2289227110258));
#172550=CARTESIAN_POINT('Ctrl Pts',(6.7376281136403,-4.54152895175203,88.22742647844));
#172551=CARTESIAN_POINT('Ctrl Pts',(6.69920652735525,-4.59796115204567,
88.224730759666));
#172552=CARTESIAN_POINT('Ctrl Pts',(6.68192742730242,-4.6230358767899,88.22353026769));
#172553=CARTESIAN_POINT('Ctrl Pts',(6.65343084461098,-4.66389542220327,
88.2215700639692));
#172554=CARTESIAN_POINT('Ctrl Pts',(6.64229719596458,-4.67973829147026,
88.2208090256917));
#172555=CARTESIAN_POINT('Ctrl Pts',(6.62037545996508,-4.71069646425686,
88.2193200960542));
#172556=CARTESIAN_POINT('Ctrl Pts',(6.60959197668369,-4.72581488373092,
88.218592136008));
#172557=CARTESIAN_POINT('Ctrl Pts',(6.58528076709651,-4.75965315996799,
88.2169610050705));
#172558=CARTESIAN_POINT('Ctrl Pts',(6.57172487491795,-4.77835255692863,
88.2160583519331));
#172559=CARTESIAN_POINT('Ctrl Pts',(6.52111528509512,-4.84754218246362,
88.2127132548391));
#172560=CARTESIAN_POINT('Ctrl Pts',(6.48355776017713,-4.89766154760364,
88.2102798247592));
#172561=CARTESIAN_POINT('Ctrl Pts',(6.18272568158983,-5.28958723497865,
88.1911497358633));
#172562=CARTESIAN_POINT('Ctrl Pts',(5.89318036540369,-5.61037140955645,
88.1748614639105));
#172563=CARTESIAN_POINT('Ctrl Pts',(5.31313419406721,-6.15829413014251,
88.144542863829));
#172564=CARTESIAN_POINT('Ctrl Pts',(5.03001957651112,-6.39162564790143,
88.1305776398499));
#172565=CARTESIAN_POINT('Ctrl Pts',(4.63853251183464,-6.67210314853453,
88.1119587984729));
#172566=CARTESIAN_POINT('Ctrl Pts',(4.5435223395634,-6.73716177097599,88.1074908367172));
#172567=CARTESIAN_POINT('Ctrl Pts',(4.41341368549829,-6.82224987081573,
88.1014336247855));
#172568=CARTESIAN_POINT('Ctrl Pts',(4.3795012398182,-6.84406915045713,88.0998603356867));
#172569=CARTESIAN_POINT('Ctrl Pts',(4.31591904075648,-6.88431187485521,
88.0969205418535));
#172570=CARTESIAN_POINT('Ctrl Pts',(4.28629018254488,-6.90279824557435,
88.0955546011133));
#172571=CARTESIAN_POINT('Ctrl Pts',(4.22430353780119,-6.9409206673375,88.0927050125827));
#172572=CARTESIAN_POINT('Ctrl Pts',(4.19192586941449,-6.96052279534235,
88.0912211266817));
#172573=CARTESIAN_POINT('Ctrl Pts',(4.11734970791505,-7.00496370545357,
88.087813461613));
#172574=CARTESIAN_POINT('Ctrl Pts',(4.07506130856448,-7.02964867127109,
88.0858885559673));
#172575=CARTESIAN_POINT('Ctrl Pts',(3.93672385041905,-7.1087324572576,88.0796152038327));
#172576=CARTESIAN_POINT('Ctrl Pts',(3.83978928832454,-7.16155638286208,
88.0752559189152));
#172577=CARTESIAN_POINT('Ctrl Pts',(3.37623285978628,-7.40205086205548,
88.0545774866923));
#172578=CARTESIAN_POINT('Ctrl Pts',(2.99677522813437,-7.56363878466678,
88.0381917320845));
#172579=CARTESIAN_POINT('Ctrl Pts',(2.08950818220156,-7.87094868987318,
87.9990458084862));
#172580=CARTESIAN_POINT('Ctrl Pts',(1.55597895186274,-7.9935442207752,87.9759363142304));
#172581=CARTESIAN_POINT('Ctrl Pts',(0.753988148230762,-8.09444190084231,
87.9417653838544));
#172582=CARTESIAN_POINT('Ctrl Pts',(0.492301924895051,-8.11456303479836,
87.9307336702937));
#172583=CARTESIAN_POINT('Ctrl Pts',(0.159308648476984,-8.12399675391221,
87.9171170330251));
#172584=CARTESIAN_POINT('Ctrl Pts',(0.0884964804720896,-8.12507668767316,
87.9142460748373));
#172585=CARTESIAN_POINT('Ctrl Pts',(-0.0108220171985221,-8.12529277722797,
87.9102615073279));
#172586=CARTESIAN_POINT('Ctrl Pts',(-0.0393226227081642,-8.12520483348696,
87.9091229593181));
#172587=CARTESIAN_POINT('Ctrl Pts',(-0.0825631533069317,-8.1248438873621,
87.9074035307122));
#172588=CARTESIAN_POINT('Ctrl Pts',(-0.0973036308914327,-8.12468072450121,
87.9068187887383));
#172589=CARTESIAN_POINT('Ctrl Pts',(-0.124576557891025,-8.12430460702016,
87.9057395877783));
#172590=CARTESIAN_POINT('Ctrl Pts',(-0.137109103134268,-8.12410276660817,
87.9052447218524));
#172591=CARTESIAN_POINT('Ctrl Pts',(-0.157492127605489,-8.12372731267102,
87.9044416327644));
#172592=CARTESIAN_POINT('Ctrl Pts',(-0.165342885362507,-8.12357131757308,
87.9041327395081));
#172593=CARTESIAN_POINT('Ctrl Pts',(-0.180424035645863,-8.12324978290116,
87.9035401953196));
#172594=CARTESIAN_POINT('Ctrl Pts',(-0.187654455465305,-8.12308596986496,
87.9032564774846));
#172595=CARTESIAN_POINT('Ctrl Pts',(-0.204164687799632,-8.12268985688925,
87.9026094800409));
#172596=CARTESIAN_POINT('Ctrl Pts',(-0.213444350695921,-8.12245130739726,
87.902246448785));
#172597=CARTESIAN_POINT('Ctrl Pts',(-0.242455918230452,-8.12165576388315,
87.9011134543929));
#172598=CARTESIAN_POINT('Ctrl Pts',(-0.262186308296341,-8.12104276360221,
87.9003457718306));
#172599=CARTESIAN_POINT('Ctrl Pts',(-0.4663327495355,-8.11395541364044,
87.8924336080277));
#172600=CARTESIAN_POINT('Ctrl Pts',(-0.650473740009095,-8.10127285133589,
87.8855854813605));
#172601=CARTESIAN_POINT('Ctrl Pts',(-0.981905472975947,-8.06707197764009,
87.8736124146225));
#172602=CARTESIAN_POINT('Ctrl Pts',(-1.12934197330756,-8.04775606740036,
87.8684091826339));
#172603=CARTESIAN_POINT('Ctrl Pts',(-1.51538556838731,-7.9863612509755,
87.8549550712973));
#172604=CARTESIAN_POINT('Ctrl Pts',(-1.75278604354459,-7.93763850759876,
87.8468517395734));
#172605=CARTESIAN_POINT('Ctrl Pts',(-2.46971699960628,-7.7567620349263,
87.8221847020955));
#172606=CARTESIAN_POINT('Ctrl Pts',(-2.9395878944736,-7.5911567052562,87.8056869946392));
#172607=CARTESIAN_POINT('Ctrl Pts',(-3.62751949168764,-7.27518588080589,
87.7787290180603));
#172608=CARTESIAN_POINT('Ctrl Pts',(-3.85833001239837,-7.15545275119635,
87.7691745270075));
#172609=CARTESIAN_POINT('Ctrl Pts',(-4.12439682990733,-7.00080932712546,
87.7574101538642));
#172610=CARTESIAN_POINT('Ctrl Pts',(-4.1655821419195,-6.9763819972725,87.7555672160709));
#172611=CARTESIAN_POINT('Ctrl Pts',(-4.22018889365918,-6.94333835025208,
87.7530938174788));
#172612=CARTESIAN_POINT('Ctrl Pts',(-4.23380469234144,-6.93504430900724,
87.7524745953414));
#172613=CARTESIAN_POINT('Ctrl Pts',(-4.25619815055805,-6.92131284343997,
87.7514520362682));
#172614=CARTESIAN_POINT('Ctrl Pts',(-4.2649900393122,-6.91589865000957,
87.7510495126774));
#172615=CARTESIAN_POINT('Ctrl Pts',(-4.28206281600574,-6.90534000905084,
87.7502657971696));
#172616=CARTESIAN_POINT('Ctrl Pts',(-4.29034481465529,-6.90019738640717,
87.7498846696228));
#172617=CARTESIAN_POINT('Ctrl Pts',(-4.30952745063559,-6.88823823656429,
87.7489997026657));
#172618=CARTESIAN_POINT('Ctrl Pts',(-4.32042119129411,-6.88141072596528,
87.7484954776047));
#172619=CARTESIAN_POINT('Ctrl Pts',(-4.35559398299998,-6.85925019165701,
87.7468620978338));
#172620=CARTESIAN_POINT('Ctrl Pts',(-4.37980784313725,-6.84381438768918,
87.7457293228081));
#172621=CARTESIAN_POINT('Ctrl Pts',(-4.61439917920111,-6.69251267963224,
87.7346730375954));
#172622=CARTESIAN_POINT('Ctrl Pts',(-4.81845774330545,-6.54712587155294,
87.7244093458401));
#172623=CARTESIAN_POINT('Ctrl Pts',(-5.333944482254,-6.14268562565857,87.6967460085545));
#172624=CARTESIAN_POINT('Ctrl Pts',(-5.633281277977,-5.86938241784143,87.6788646403132));
#172625=CARTESIAN_POINT('Ctrl Pts',(-6.15798513720825,-5.31304978471058,
87.644595317736));
#172626=CARTESIAN_POINT('Ctrl Pts',(-6.38730718404794,-5.03503649405329,
87.6283082819637));
#172627=CARTESIAN_POINT('Ctrl Pts',(-6.68079648639094,-4.6267742818475,
87.6062415808004));
#172628=CARTESIAN_POINT('Ctrl Pts',(-6.76108564918213,-4.50863675571175,
87.6000569355226));
#172629=CARTESIAN_POINT('Ctrl Pts',(-6.91721355842457,-4.2653528070661,
87.5878031219735));
#172630=CARTESIAN_POINT('Ctrl Pts',(-6.99287346818967,-4.14014571705009,
87.5817458760562));
#172631=CARTESIAN_POINT('Ctrl Pts',(-7.07538410874687,-3.9948791197118,
87.5750390533899));
#172632=CARTESIAN_POINT('Ctrl Pts',(-7.08557891277828,-3.97676890823265,
87.574208224111));
#172633=CARTESIAN_POINT('Ctrl Pts',(-7.10390022212183,-3.94392852385006,
87.5727108834586));
#172634=CARTESIAN_POINT('Ctrl Pts',(-7.1120506536081,-3.92921188959852,
87.5720432299049));
#172635=CARTESIAN_POINT('Ctrl Pts',(-7.12454665448998,-3.90648251160985,
87.571017063655));
#172636=CARTESIAN_POINT('Ctrl Pts',(-7.12892451490402,-3.8984876435866,
87.5706570693742));
#172637=CARTESIAN_POINT('Ctrl Pts',(-7.13687395894839,-3.88391216642691,
87.5700024662749));
#172638=CARTESIAN_POINT('Ctrl Pts',(-7.14044991373662,-3.87733396193181,
87.5697076614465));
#172639=CARTESIAN_POINT('Ctrl Pts',(-7.14761522799176,-3.86410936345416,
87.5691162454736));
#172640=CARTESIAN_POINT('Ctrl Pts',(-7.1512044218469,-3.85746288868348,
87.5688196417732));
#172641=CARTESIAN_POINT('Ctrl Pts',(-7.16137190811097,-3.83857176057073,
87.5679783834972));
#172642=CARTESIAN_POINT('Ctrl Pts',(-7.1679280735745,-3.82631518595839,
87.567434685506));
#172643=CARTESIAN_POINT('Ctrl Pts',(-7.19559384162369,-3.77427413429594,
87.5651348795675));
#172644=CARTESIAN_POINT('Ctrl Pts',(-7.21640413383259,-3.7343309230171,
87.5633912604));
#172645=CARTESIAN_POINT('Ctrl Pts',(-7.27419703675982,-3.62111600748921,
87.5585048477743));
#172646=CARTESIAN_POINT('Ctrl Pts',(-7.31040353164279,-3.54745321748207,
87.5553907482796));
#172647=CARTESIAN_POINT('Ctrl Pts',(-7.54553599649802,-3.05017801127673,
87.5347344655956));
#172648=CARTESIAN_POINT('Ctrl Pts',(-7.70866698695404,-2.61059232671126,
87.5181805695881));
#172649=CARTESIAN_POINT('Ctrl Pts',(-7.96132435096491,-1.6940953109874,
87.4839734067664));
#172650=CARTESIAN_POINT('Ctrl Pts',(-8.04787676111599,-1.21831640895912,
87.4663540323539));
#172651=CARTESIAN_POINT('Ctrl Pts',(-8.09801045833638,-0.668397125700044,
87.4453162399145));
#172652=CARTESIAN_POINT('Ctrl Pts',(-8.1034367853083,-0.599032742184795,
87.4426522405842));
#172653=CARTESIAN_POINT('Ctrl Pts',(-8.11154355113557,-0.47492309711704,
87.437866387093));
#172654=CARTESIAN_POINT('Ctrl Pts',(-8.11456217066969,-0.420204047850183,
87.4357496498337));
#172655=CARTESIAN_POINT('Ctrl Pts',(-8.11825758738527,-0.338126985132404,
87.4325645542927));
#172656=CARTESIAN_POINT('Ctrl Pts',(-8.11935011378706,-0.310789052255108,
87.4315020070198));
#172657=CARTESIAN_POINT('Ctrl Pts',(-8.1210708320833,-0.261493077130119,
87.429583033099));
#172658=CARTESIAN_POINT('Ctrl Pts',(-8.12174809533972,-0.23953697012244,
87.4287272724805));
#172659=CARTESIAN_POINT('Ctrl Pts',(-8.12288609377211,-0.197054798176525,
87.427069437358));
#172660=CARTESIAN_POINT('Ctrl Pts',(-8.1233580826719,-0.176529156950955,
87.4262675032742));
#172661=CARTESIAN_POINT('Ctrl Pts',(-8.12438458729711,-0.123074265723032,
87.424176435659));
#172662=CARTESIAN_POINT('Ctrl Pts',(-8.12481669957023,-0.0901431154560538,
87.4228856609259));
#172663=CARTESIAN_POINT('Ctrl Pts',(-8.12561654486722,0.0234513854260239,
87.4184235712268));
#172664=CARTESIAN_POINT('Ctrl Pts',(-8.12498330821539,0.10411636252658,
87.4152381952756));
#172665=CARTESIAN_POINT('Ctrl Pts',(-8.10434189934501,1.01164611159506,
87.3791804058906));
#172666=CARTESIAN_POINT('Ctrl Pts',(-7.9593797367279,1.83078500486084,87.3438494336284));
#172667=CARTESIAN_POINT('Ctrl Pts',(-7.61450601515398,2.84588988547919,
87.2987379491886));
#172668=CARTESIAN_POINT('Ctrl Pts',(-7.52517321019521,3.07434026356217,
87.2885502621338));
#172669=CARTESIAN_POINT('Ctrl Pts',(-7.40969693742471,3.33430984184497,
87.2771302332658));
#172670=CARTESIAN_POINT('Ctrl Pts',(-7.39348929929894,3.37009597299934,
87.2755622267616));
#172671=CARTESIAN_POINT('Ctrl Pts',(-7.37170526013057,3.41728109022426,
87.2735012623311));
#172672=CARTESIAN_POINT('Ctrl Pts',(-7.36636092467724,3.42878626067399,
87.2729992506694));
#172673=CARTESIAN_POINT('Ctrl Pts',(-7.35755192402838,3.44763443094345,
87.2721777318965));
#172674=CARTESIAN_POINT('Ctrl Pts',(-7.35410316837012,3.45498481527026,
87.2718575806897));
#172675=CARTESIAN_POINT('Ctrl Pts',(-7.3474054863351,3.46920422004098,87.2712386931006));
#172676=CARTESIAN_POINT('Ctrl Pts',(-7.34415793103988,3.47607387513617,
87.2709399003032));
#172677=CARTESIAN_POINT('Ctrl Pts',(-7.33664673587518,3.49190502763618,
87.2702518149167));
#172678=CARTESIAN_POINT('Ctrl Pts',(-7.33237629981278,3.50086330040163,
87.2698628107042));
#172679=CARTESIAN_POINT('Ctrl Pts',(-7.32091171877041,3.5248000336117,87.2688243801532));
#172680=CARTESIAN_POINT('Ctrl Pts',(-7.3136879979854,3.5397643345841,87.2681762420602));
#172681=CARTESIAN_POINT('Ctrl Pts',(-7.25730205859535,3.65566118042444,
87.2631651686594));
#172682=CARTESIAN_POINT('Ctrl Pts',(-7.20610225584859,3.75558027113001,
87.2589029470602));
#172683=CARTESIAN_POINT('Ctrl Pts',(-6.8271664449743,4.45879117447764,87.2292679120403));
#172684=CARTESIAN_POINT('Ctrl Pts',(-6.42617874716781,5.01950327629161,
87.2072239125608));
#172685=CARTESIAN_POINT('Ctrl Pts',(-5.61181927967381,5.89819239449311,
87.1664003312898));
#172686=CARTESIAN_POINT('Ctrl Pts',(-5.2296215962283,6.23956567214487,87.148330877711));
#172687=CARTESIAN_POINT('Ctrl Pts',(-4.78720368337276,6.565350072131,87.1272479344468));
#172688=CARTESIAN_POINT('Ctrl Pts',(-4.75634986417377,6.58773683437069,
87.1257773495951));
#172689=CARTESIAN_POINT('Ctrl Pts',(-4.7134784869283,6.61838505316805,87.1237332820002));
#172690=CARTESIAN_POINT('Ctrl Pts',(-4.70159431124777,6.62683265886101,
87.1231665832133));
#172691=CARTESIAN_POINT('Ctrl Pts',(-4.68149435894232,6.64103898425186,
87.1222079735667));
#172692=CARTESIAN_POINT('Ctrl Pts',(-4.67329051888297,6.64681457153868,
87.1218166756666));
#172693=CARTESIAN_POINT('Ctrl Pts',(-4.65703565493858,6.65821319187969,
87.1210412845406));
#172694=CARTESIAN_POINT('Ctrl Pts',(-4.64898509185847,6.66383685385207,
87.120657215079));
#172695=CARTESIAN_POINT('Ctrl Pts',(-4.631218729918,6.67619955135258,87.1198095363357));
#172696=CARTESIAN_POINT('Ctrl Pts',(-4.62149838371879,6.68293199588982,
87.119345690482));
#172697=CARTESIAN_POINT('Ctrl Pts',(-4.58749232705156,6.70637538192568,
87.1177227157795));
#172698=CARTESIAN_POINT('Ctrl Pts',(-4.56313053069679,6.7229752603836,87.1165596007791));
#172699=CARTESIAN_POINT('Ctrl Pts',(-4.30887055814659,6.89420670736918,
87.104415296259));
#172700=CARTESIAN_POINT('Ctrl Pts',(-4.07131296116644,7.03710480302124,
87.0930173496083));
#172701=CARTESIAN_POINT('Ctrl Pts',(-3.70578960600831,7.23226595116053,
87.0754084330883));
#172702=CARTESIAN_POINT('Ctrl Pts',(-3.58302771708291,7.29386439805088,
87.0694846652135));
#172703=CARTESIAN_POINT('Ctrl Pts',(-2.91549520809578,7.60789303890565,
87.0372728768638));
#172704=CARTESIAN_POINT('Ctrl Pts',(-2.34561249453569,7.80244731666633,
87.0096243291723));
#172705=CARTESIAN_POINT('Ctrl Pts',(-1.4305582352837,8.00541922578056,86.9681547749409));
#172706=CARTESIAN_POINT('Ctrl Pts',(-1.09731273390021,8.05786659227831,
86.9536741406324));
#172707=CARTESIAN_POINT('Ctrl Pts',(-0.738091941583653,8.09169148187367,
86.9392734399311));
#172708=CARTESIAN_POINT('Ctrl Pts',(-0.714455023279688,8.09381274733787,
86.9383309529761));
#172709=CARTESIAN_POINT('Ctrl Pts',(-0.680727218248399,8.0966907066209,
86.9369929422362));
#172710=CARTESIAN_POINT('Ctrl Pts',(-0.670643833424958,8.09753214222121,
86.9365937966184));
#172711=CARTESIAN_POINT('Ctrl Pts',(-0.653239223852168,8.09895178480713,
86.9359063079696));
#172712=CARTESIAN_POINT('Ctrl Pts',(-0.645918753371324,8.09953890420626,
86.9356175933954));
#172713=CARTESIAN_POINT('Ctrl Pts',(-0.631905803922312,8.10064365802685,
86.9350657704985));
#172714=CARTESIAN_POINT('Ctrl Pts',(-0.625213463284364,8.10116292547065,
86.9348025955091));
#172715=CARTESIAN_POINT('Ctrl Pts',(-0.609541214801772,8.10235941976177,
86.934187129163));
#172716=CARTESIAN_POINT('Ctrl Pts',(-0.600560798205658,8.10303001278166,
86.9338351053358));
#172717=CARTESIAN_POINT('Ctrl Pts',(-0.569493241817417,8.10529798353278,
86.93261947011));
#172718=CARTESIAN_POINT('Ctrl Pts',(-0.547400586532317,8.10682000318818,
86.931758828203));
#172719=CARTESIAN_POINT('Ctrl Pts',(-0.21064655863232,8.12863697703152,
86.9186948687164));
#172720=CARTESIAN_POINT('Ctrl Pts',(0.104948463570433,8.13068996839038,
86.9071650388371));
#172721=CARTESIAN_POINT('Ctrl Pts',(0.825560737317496,8.09340203035556,
86.8811369963684));
#172722=CARTESIAN_POINT('Ctrl Pts',(1.22909681658394,8.04201669537234,86.8667543410258));
#172723=CARTESIAN_POINT('Ctrl Pts',(2.2078677524544,7.84196338932469,86.8304435540159));
#172724=CARTESIAN_POINT('Ctrl Pts',(2.77387208118999,7.66006708806928,86.808082885811));
#172725=CARTESIAN_POINT('Ctrl Pts',(3.41806625228943,7.37219453093453,86.7808157477438));
#172726=CARTESIAN_POINT('Ctrl Pts',(3.52015129714024,7.32399915659644,86.7764378925807));
#172727=CARTESIAN_POINT('Ctrl Pts',(3.66587462282651,7.25145099127642,86.7700964709371));
#172728=CARTESIAN_POINT('Ctrl Pts',(3.71034480073954,7.22879794015218,86.7681486642313));
#172729=CARTESIAN_POINT('Ctrl Pts',(3.78818141483897,7.18824058675871,86.7647162861347));
#172730=CARTESIAN_POINT('Ctrl Pts',(3.82163672230387,7.17051001773245,86.7632334008194));
#172731=CARTESIAN_POINT('Ctrl Pts',(3.89127758955365,7.13297607949051,86.7601302834941));
#172732=CARTESIAN_POINT('Ctrl Pts',(3.92743873436089,7.1131296909311,86.7585096731276));
#172733=CARTESIAN_POINT('Ctrl Pts',(4.02219242284411,7.06018301646667,86.7542379811007));
#172734=CARTESIAN_POINT('Ctrl Pts',(4.08052742920507,7.02662877457023,86.7515825339732));
#172735=CARTESIAN_POINT('Ctrl Pts',(4.34092831665612,6.87250998910077,86.7396094866133));
#172736=CARTESIAN_POINT('Ctrl Pts',(4.53811366293543,6.74392864380732,86.7302136659526));
#172737=CARTESIAN_POINT('Ctrl Pts',(5.09062973698568,6.34842374825113,86.7028658904832));
#172738=CARTESIAN_POINT('Ctrl Pts',(5.43001008585655,6.06069127787336,86.6847482294732));
#172739=CARTESIAN_POINT('Ctrl Pts',(5.85951183175969,5.63137698421874,86.6601484149518));
#172740=CARTESIAN_POINT('Ctrl Pts',(5.9713621612949,5.51263282086083,86.6535676460504));
#172741=CARTESIAN_POINT('Ctrl Pts',(6.12108105277673,5.34377866444996,86.6445374320418));
#172742=CARTESIAN_POINT('Ctrl Pts',(6.16205615783314,5.29647691107933,86.6420417377251));
#172743=CARTESIAN_POINT('Ctrl Pts',(6.23241035568607,5.21333821923431,86.6377160470463));
#172744=CARTESIAN_POINT('Ctrl Pts',(6.26203684144825,5.17771463779949,86.6358815228375));
#172745=CARTESIAN_POINT('Ctrl Pts',(6.30533134974046,5.12474114096853,86.6331821487399));
#172746=CARTESIAN_POINT('Ctrl Pts',(6.31923583232925,5.1075858970073,86.6323123444997));
#172747=CARTESIAN_POINT('Ctrl Pts',(6.34468521422652,5.07592364183414,86.6307151254777));
#172748=CARTESIAN_POINT('Ctrl Pts',(6.35625069305915,5.06143343484455,86.6299872439584));
#172749=CARTESIAN_POINT('Ctrl Pts',(6.38234124170239,5.02851453442241,86.628340388655));
#172750=CARTESIAN_POINT('Ctrl Pts',(6.39683629371163,5.010062233692,86.6274220213856));
#172751=CARTESIAN_POINT('Ctrl Pts',(6.43448038961979,4.96171134376934,86.6250274851695));
#172752=CARTESIAN_POINT('Ctrl Pts',(6.45750106243129,4.93171343370384,86.6235536339798));
#172753=CARTESIAN_POINT('Ctrl Pts',(6.6311292593958,4.70216084770847,86.6123584482157));
#172754=CARTESIAN_POINT('Ctrl Pts',(6.77266536786339,4.49590908277067,86.602769009904));
#172755=CARTESIAN_POINT('Ctrl Pts',(6.9677372186389,4.18147454545883,86.5885439436141));
#172756=CARTESIAN_POINT('Ctrl Pts',(7.02873943557042,4.07810165791997,86.5839279384938));
#172757=CARTESIAN_POINT('Ctrl Pts',(7.15011457606172,3.86160336928366,86.5743533456606));
#172758=CARTESIAN_POINT('Ctrl Pts',(7.21014471652478,3.74832387014416,86.569394124825));
#172759=CARTESIAN_POINT('Ctrl Pts',(7.28947857414439,3.58965342932181,86.5624987366147));
#172760=CARTESIAN_POINT('Ctrl Pts',(7.31108719940772,3.54543559558108,86.5605825702454));
#172761=CARTESIAN_POINT('Ctrl Pts',(7.34769540266949,3.46876601569569,86.5572685190499));
#172762=CARTESIAN_POINT('Ctrl Pts',(7.36288501256494,3.43640650730609,86.5558723345331));
#172763=CARTESIAN_POINT('Ctrl Pts',(7.39178592244317,3.37376545333945,86.5531742267215));
#172764=CARTESIAN_POINT('Ctrl Pts',(7.40552591883214,3.34349791601854,86.5518725851418));
#172765=CARTESIAN_POINT('Ctrl Pts',(7.44176488909633,3.26234853958434,86.5483879927027));
#172766=CARTESIAN_POINT('Ctrl Pts',(7.46392760625363,3.21131862439481,86.5462021663001));
#172767=CARTESIAN_POINT('Ctrl Pts',(7.55328028555494,2.99965994768545,86.5371567821627));
#172768=CARTESIAN_POINT('Ctrl Pts',(7.61582209033827,2.8371210233071,86.5302584322811));
#172769=CARTESIAN_POINT('Ctrl Pts',(7.76489655973197,2.40914096803974,86.512221021849));
#172770=CARTESIAN_POINT('Ctrl Pts',(7.84305907181991,2.14102831844453,86.5010390246955));
#172771=CARTESIAN_POINT('Ctrl Pts',(7.92042105053816,1.81380396419408,86.4876537389973));
#172772=CARTESIAN_POINT('Ctrl Pts',(7.93298418599792,1.75804333997136,86.4853822118613));
#172773=CARTESIAN_POINT('Ctrl Pts',(7.95865504425514,1.6382223291081,86.4805242616879));
#172774=CARTESIAN_POINT('Ctrl Pts',(7.97158001145936,1.57412665512835,86.4779397354864));
#172775=CARTESIAN_POINT('Ctrl Pts',(7.98841825196939,1.4850918847796,86.4743725685921));
#172776=CARTESIAN_POINT('Ctrl Pts',(7.99299102015764,1.46028032819162,86.4733809705378));
#172777=CARTESIAN_POINT('Ctrl Pts',(8.0005810696049,1.41799315562026,86.4716953879883));
#172778=CARTESIAN_POINT('Ctrl Pts',(8.00365682011451,1.40052831061949,86.4710004978576));
#172779=CARTESIAN_POINT('Ctrl Pts',(8.01049901802271,1.36091794318792,86.4694271993562));
#172780=CARTESIAN_POINT('Ctrl Pts',(8.01423085739882,1.33876657207378,86.4685492826547));
#172781=CARTESIAN_POINT('Ctrl Pts',(8.0241858073605,1.27814261279842,86.4661514864202));
#172782=CARTESIAN_POINT('Ctrl Pts',(8.0302240700379,1.2396401957144,86.4646340169552));
#172783=CARTESIAN_POINT('Ctrl Pts',(8.06845771199889,0.983836285814555,
86.4545833494757));
#172784=CARTESIAN_POINT('Ctrl Pts',(8.09210663308779,0.765346948980179,
86.4461458027439));
#172785=CARTESIAN_POINT('Ctrl Pts',(8.10736665150992,0.53883900668231,86.437438955625));
#172786=CARTESIAN_POINT('Ctrl Pts',(8.10785037040559,0.531510929589214,
86.4371573140476));
#172787=CARTESIAN_POINT('Ctrl Pts',(8.11963563174538,0.349210351525483,
86.4301519705228));
#172788=CARTESIAN_POINT('Ctrl Pts',(8.12528048587411,0.173918382661803,
86.4234391042784));
#172789=CARTESIAN_POINT('Ctrl Pts',(8.1252264122484,-0.135823388346372,
86.411545053788));
#172790=CARTESIAN_POINT('Ctrl Pts',(8.121868038732,-0.270206437285089,86.406374213703));
#172791=CARTESIAN_POINT('Ctrl Pts',(8.1074111842862,-0.560283775619173,
86.3951602356333));
#172792=CARTESIAN_POINT('Ctrl Pts',(8.09515708620389,-0.715866711354673,
86.3891127780931));
#172793=CARTESIAN_POINT('Ctrl Pts',(8.07103413395062,-0.939604707821945,
86.380349225736));
#172794=CARTESIAN_POINT('Ctrl Pts',(8.06276361074699,-1.00811303921763,
86.3776568454641));
#172795=CARTESIAN_POINT('Ctrl Pts',(8.0463755951923,-1.1307158772914,86.3728212817761));
#172796=CARTESIAN_POINT('Ctrl Pts',(8.03858258780264,-1.18484959685225,
86.3706801456555));
#172797=CARTESIAN_POINT('Ctrl Pts',(8.02035646576807,-1.30298677922978,
86.3659938864546));
#172798=CARTESIAN_POINT('Ctrl Pts',(8.00970246516257,-1.36695236431319,
86.363447728529));
#172799=CARTESIAN_POINT('Ctrl Pts',(7.98532524561101,-1.50322450949963,
86.358004556188));
#172800=CARTESIAN_POINT('Ctrl Pts',(7.97138299240466,-1.57548606780182,
86.3551067844742));
#172801=CARTESIAN_POINT('Ctrl Pts',(7.92510995785551,-1.79895122795273,
86.3461112279545));
#172802=CARTESIAN_POINT('Ctrl Pts',(7.88944369389878,-1.94942849235616,
86.3400042415));
#172803=CARTESIAN_POINT('Ctrl Pts',(7.82043293381461,-2.20752902483832,
86.3294594165057));
#172804=CARTESIAN_POINT('Ctrl Pts',(7.78910373474079,-2.31564652245985,
86.3250207581936));
#172805=CARTESIAN_POINT('Ctrl Pts',(7.74231925083149,-2.46538945194183,
86.3188517928813));
#172806=CARTESIAN_POINT('Ctrl Pts',(7.72875389218584,-2.50759163788982,
86.3171108128746));
#172807=CARTESIAN_POINT('Ctrl Pts',(7.70093454236142,-2.59176764174563,
86.3136344511152));
#172808=CARTESIAN_POINT('Ctrl Pts',(7.68668105281596,-2.6337400676293,86.3118991276364));
#172809=CARTESIAN_POINT('Ctrl Pts',(7.62927066996063,-2.79836046654507,
86.3050818851993));
#172810=CARTESIAN_POINT('Ctrl Pts',(7.58351584488334,-2.92008217537805,
86.3000165198833));
#172811=CARTESIAN_POINT('Ctrl Pts',(7.45466117076445,-3.23938913376595,
86.2866084155519));
#172812=CARTESIAN_POINT('Ctrl Pts',(7.36663157529904,-3.43487320879174,
86.2782735733245));
#172813=CARTESIAN_POINT('Ctrl Pts',(7.24253407845609,-3.68367325162197,
86.2674076722357));
#172814=CARTESIAN_POINT('Ctrl Pts',(7.21342083046097,-3.74036206681567,
86.26491416792));
#172815=CARTESIAN_POINT('Ctrl Pts',(7.1580333224249,-3.84515935821158,86.2602688940297));
#172816=CARTESIAN_POINT('Ctrl Pts',(7.13193325244573,-3.893355826603,86.2581182509079));
#172817=CARTESIAN_POINT('Ctrl Pts',(7.0705427174501,-4.00403068371667,86.2531448656639));
#172818=CARTESIAN_POINT('Ctrl Pts',(7.03490830891644,-4.06631295641659,
86.2503201022861));
#172819=CARTESIAN_POINT('Ctrl Pts',(6.90569745283106,-4.28536601765933,
86.2402877708361));
#172820=CARTESIAN_POINT('Ctrl Pts',(6.80766824340771,-4.4394449330892,86.2330508131913));
#172821=CARTESIAN_POINT('Ctrl Pts',(6.52137986126716,-4.85761322935227,
86.2128717288316));
#172822=CARTESIAN_POINT('Ctrl Pts',(6.32237913536012,-5.11393405816995,
86.1998687631205));
#172823=CARTESIAN_POINT('Ctrl Pts',(6.10601226752327,-5.36062656322044,
86.186754840284));
#172824=CARTESIAN_POINT('Ctrl Pts',(6.10342260098573,-5.36357488203833,
86.1865980212806));
#172825=CARTESIAN_POINT('Ctrl Pts',(5.98322538208023,-5.50021887370896,
86.1793258881665));
#172826=CARTESIAN_POINT('Ctrl Pts',(5.86125568289897,-5.6300156862801,86.1722334135339));
#172827=CARTESIAN_POINT('Ctrl Pts',(5.70797718567077,-5.78274607151557,
86.1636936514307));
#172828=CARTESIAN_POINT('Ctrl Pts',(5.68064412432064,-5.80959878417325,
86.1621846151848));
#172829=CARTESIAN_POINT('Ctrl Pts',(5.63708801682959,-5.85178814999802,
86.1598021970486));
#172830=CARTESIAN_POINT('Ctrl Pts',(5.62099000809967,-5.86725295136704,
86.1589264190496));
#172831=CARTESIAN_POINT('Ctrl Pts',(5.59197786275281,-5.89489492610727,
86.1573567001354));
#172832=CARTESIAN_POINT('Ctrl Pts',(5.57908717754547,-5.90709648432783,
86.1566622680273));
#172833=CARTESIAN_POINT('Ctrl Pts',(5.54756602504395,-5.93673731736012,
86.1549716484984));
#172834=CARTESIAN_POINT('Ctrl Pts',(5.52889319496654,-5.95413123967668,
86.1539764793883));
#172835=CARTESIAN_POINT('Ctrl Pts',(5.46051061801756,-6.01723120837941,
86.1503542124727));
#172836=CARTESIAN_POINT('Ctrl Pts',(5.41031326679808,-6.0624053055443,86.1477375790293));
#172837=CARTESIAN_POINT('Ctrl Pts',(5.27618995971334,-6.18011412080629,
86.140845292473));
#172838=CARTESIAN_POINT('Ctrl Pts',(5.19133158447958,-6.25156522012157,
86.1365846014484));
#172839=CARTESIAN_POINT('Ctrl Pts',(4.81391007484413,-6.55637020452042,
86.117988150356));
#172840=CARTESIAN_POINT('Ctrl Pts',(4.50689161535851,-6.77108905471312,
86.1037381318701));
#172841=CARTESIAN_POINT('Ctrl Pts',(4.12867924434931,-6.9984423170726,86.086643483592));
#172842=CARTESIAN_POINT('Ctrl Pts',(4.0707624413992,-7.03228840739781,86.0840386684656));
#172843=CARTESIAN_POINT('Ctrl Pts',(3.97829232881325,-7.08480199034862,
86.0798981397679));
#172844=CARTESIAN_POINT('Ctrl Pts',(3.94401124247149,-7.10394287707296,
86.0783670773854));
#172845=CARTESIAN_POINT('Ctrl Pts',(3.8817812003564,-7.13809980264651,86.075594501455));
#172846=CARTESIAN_POINT('Ctrl Pts',(3.85388043509571,-7.15320205672022,
86.0743538466508));
#172847=CARTESIAN_POINT('Ctrl Pts',(3.78721489124895,-7.1887838328655,86.0713950207211));
#172848=CARTESIAN_POINT('Ctrl Pts',(3.74837145365251,-7.20911374951846,
86.0696754761794));
#172849=CARTESIAN_POINT('Ctrl Pts',(3.6278625697812,-7.27094852121179,86.0643539482631));
#172850=CARTESIAN_POINT('Ctrl Pts',(3.54565869093387,-7.31138724861882,
86.0607424530594));
#172851=CARTESIAN_POINT('Ctrl Pts',(3.34521615380744,-7.40581580506629,
86.0519800442096));
#172852=CARTESIAN_POINT('Ctrl Pts',(3.2263319109118,-7.45837521763892,86.0468188269849));
#172853=CARTESIAN_POINT('Ctrl Pts',(2.97358391341527,-7.56294226236704,
86.0359291557931));
#172854=CARTESIAN_POINT('Ctrl Pts',(2.83949787963817,-7.6142989575121,86.0301996092331));
#172855=CARTESIAN_POINT('Ctrl Pts',(2.55189051967794,-7.71580217994867,
86.0180386562009));
#172856=CARTESIAN_POINT('Ctrl Pts',(2.39809053954328,-7.76497977743003,
86.0116111321779));
#172857=CARTESIAN_POINT('Ctrl Pts',(2.21029082979619,-7.81891648436137,
86.0038915756531));
#172858=CARTESIAN_POINT('Ctrl Pts',(2.17759609197165,-7.82808506695261,
86.0025523640778));
#172859=CARTESIAN_POINT('Ctrl Pts',(2.1270117690769,-7.84192899302037,86.0004882089541));
#172860=CARTESIAN_POINT('Ctrl Pts',(2.1091621474017,-7.84674865379484,85.9997613347577));
#172861=CARTESIAN_POINT('Ctrl Pts',(2.07516901781517,-7.85580292827603,
85.9983800350702));
#172862=CARTESIAN_POINT('Ctrl Pts',(2.0590286071767,-7.8600488101217,85.997725446521));
#172863=CARTESIAN_POINT('Ctrl Pts',(2.01957600475349,-7.87029731376836,
85.9961286297498));
#172864=CARTESIAN_POINT('Ctrl Pts',(1.99624997003997,-7.87624613056249,
85.9951872594372));
#172865=CARTESIAN_POINT('Ctrl Pts',(1.91697601137904,-7.89608850654348,
85.9919967987102));
#172866=CARTESIAN_POINT('Ctrl Pts',(1.86090654954597,-7.90949035137273,
85.9897550790939));
#172867=CARTESIAN_POINT('Ctrl Pts',(1.72335364169449,-7.94082490809325,
85.9842872225631));
#172868=CARTESIAN_POINT('Ctrl Pts',(1.64172725737698,-7.95810151882606,
85.9810695185201));
#172869=CARTESIAN_POINT('Ctrl Pts',(1.16626473423822,-8.05110862598338,
85.9624511085643));
#172870=CARTESIAN_POINT('Ctrl Pts',(0.767516623718932,-8.09885473613727,
85.9473155089745));
#172871=CARTESIAN_POINT('Ctrl Pts',(-0.0243255284311196,-8.13464478156951,
85.9171679726225));
#172872=CARTESIAN_POINT('Ctrl Pts',(-0.41628519775045,-8.12402211317606,
85.9021982303826));
#172873=CARTESIAN_POINT('Ctrl Pts',(-0.878679879113604,-8.07792997004699,
85.8841487268657));
#172874=CARTESIAN_POINT('Ctrl Pts',(-0.951316307344746,-8.06969814394235,
85.8813024878867));
#172875=CARTESIAN_POINT('Ctrl Pts',(-1.06639268879897,-8.05508130796135,
85.8767744100433));
#172876=CARTESIAN_POINT('Ctrl Pts',(-1.10891031930456,-8.04933824189309,
85.8750973154235));
#172877=CARTESIAN_POINT('Ctrl Pts',(-1.18853382614312,-8.03794025678495,
85.8719486266537));
#172878=CARTESIAN_POINT('Ctrl Pts',(-1.22564991218905,-8.03236444080418,
85.8704776274058));
#172879=CARTESIAN_POINT('Ctrl Pts',(-1.3091006616024,-8.0192360520904,85.8671627580057));
#172880=CARTESIAN_POINT('Ctrl Pts',(-1.35541115833492,-8.01153867704218,
85.8653179592891));
#172881=CARTESIAN_POINT('Ctrl Pts',(-1.49612429180006,-7.98689541510239,
85.8596962835458));
#172882=CARTESIAN_POINT('Ctrl Pts',(-1.59029560049313,-7.96867906386644,
85.8559115665168));
#172883=CARTESIAN_POINT('Ctrl Pts',(-2.07638041669483,-7.8656916822533,
85.836256948119));
#172884=CARTESIAN_POINT('Ctrl Pts',(-2.46194108858474,-7.75366344008687,
85.8203293035835));
#172885=CARTESIAN_POINT('Ctrl Pts',(-3.37548687124406,-7.41317946604918,
85.7806309153384));
#172886=CARTESIAN_POINT('Ctrl Pts',(-3.89055101019032,-7.15630380539908,
85.7563764540706));
#172887=CARTESIAN_POINT('Ctrl Pts',(-4.68172357633412,-6.65088794788272,
85.7166807032628));
#172888=CARTESIAN_POINT('Ctrl Pts',(-4.97567064009896,-6.43393874440525,
85.7013445903703));
#172889=CARTESIAN_POINT('Ctrl Pts',(-5.27103970536602,-6.18355272960974,
85.6859401212494));
#172890=CARTESIAN_POINT('Ctrl Pts',(-5.28797527992036,-6.16907621820978,
85.6850570045303));
#172891=CARTESIAN_POINT('Ctrl Pts',(-5.31157585796183,-6.14873387661932,
85.6838267726132));
#172892=CARTESIAN_POINT('Ctrl Pts',(-5.31829103303334,-6.14292657200925,
85.6834767790813));
#172893=CARTESIAN_POINT('Ctrl Pts',(-5.33054637714349,-6.13229295368243,
85.68283814543));
#172894=CARTESIAN_POINT('Ctrl Pts',(-5.33608953875205,-6.12747011282205,
85.682549329974));
#172895=CARTESIAN_POINT('Ctrl Pts',(-5.34726691223446,-6.11771854273814,
85.681967053782));
#172896=CARTESIAN_POINT('Ctrl Pts',(-5.35290087087729,-6.11278953227413,
85.6816736080965));
#172897=CARTESIAN_POINT('Ctrl Pts',(-5.36667910877039,-6.10070163869284,
85.6809561082513));
#172898=CARTESIAN_POINT('Ctrl Pts',(-5.374815898617,-6.09353421245212,85.6805325078588));
#172899=CARTESIAN_POINT('Ctrl Pts',(-5.40403519406533,-6.06769185160452,
85.6790118720389));
#172900=CARTESIAN_POINT('Ctrl Pts',(-5.42503507490687,-6.04892347843511,
85.677919963998));
#172901=CARTESIAN_POINT('Ctrl Pts',(-5.47489136451968,-6.00389658941814,
85.6753308973395));
#172902=CARTESIAN_POINT('Ctrl Pts',(-5.50365662682912,-5.9775390879655,
85.6738399596867));
#172903=CARTESIAN_POINT('Ctrl Pts',(-5.61319006949324,-5.87571299888941,
85.6681745320842));
#172904=CARTESIAN_POINT('Ctrl Pts',(-5.6926062136657,-5.79880522090453,
85.6640894054649));
#172905=CARTESIAN_POINT('Ctrl Pts',(-5.84121773407335,-5.64889128611627,
85.6564418506644));
#172906=CARTESIAN_POINT('Ctrl Pts',(-5.91067468346907,-5.57617458559884,
85.6528662224986));
#172907=CARTESIAN_POINT('Ctrl Pts',(-6.34754356712884,-5.10146570107805,
85.6302496244705));
#172908=CARTESIAN_POINT('Ctrl Pts',(-6.6751135981627,-4.66467232727422,
85.6126351539017));
#172909=CARTESIAN_POINT('Ctrl Pts',(-7.23816480019743,-3.73172181807925,
85.5758155538352));
#172910=CARTESIAN_POINT('Ctrl Pts',(-7.47210109769261,-3.23796256591509,
85.5566669140636));
#172911=CARTESIAN_POINT('Ctrl Pts',(-7.66589678167533,-2.69347372353281,
85.5344538463291));
#172912=CARTESIAN_POINT('Ctrl Pts',(-7.67676087593777,-2.66235170291672,
85.5331809850603));
#172913=CARTESIAN_POINT('Ctrl Pts',(-7.69155799773127,-2.61911916891191,
85.5314082093794));
#172914=CARTESIAN_POINT('Ctrl Pts',(-7.69565245412017,-2.60706404928158,
85.530913387658));
#172915=CARTESIAN_POINT('Ctrl Pts',(-7.70264339510236,-2.58632097003858,
85.5300610940978));
#172916=CARTESIAN_POINT('Ctrl Pts',(-7.70555356097127,-2.57763762978768,
85.5297040534266));
#172917=CARTESIAN_POINT('Ctrl Pts',(-7.7115184227696,-2.55973932744321,
85.5289675753912));
#172918=CARTESIAN_POINT('Ctrl Pts',(-7.71457129599614,-2.55052377511001,
85.5285880814707));
#172919=CARTESIAN_POINT('Ctrl Pts',(-7.72162018552575,-2.52911721000013,
85.5277058790947));
#172920=CARTESIAN_POINT('Ctrl Pts',(-7.72560385414903,-2.51692217566856,
85.5272027845002));
#172921=CARTESIAN_POINT('Ctrl Pts',(-7.73813365617375,-2.4782552090768,
85.5256059653377));
#172922=CARTESIAN_POINT('Ctrl Pts',(-7.74657269591682,-2.45174892889349,
85.5245088953513));
#172923=CARTESIAN_POINT('Ctrl Pts',(-7.89106860892381,-1.98970546651755,
85.5053419817239));
#172924=CARTESIAN_POINT('Ctrl Pts',(-7.99032053965758,-1.54356379451311,
85.4861025307766));
#172925=CARTESIAN_POINT('Ctrl Pts',(-8.13590802265173,-0.469609953240339,
85.4385355704836));
#172926=CARTESIAN_POINT('Ctrl Pts',(-8.14787813819847,0.159913475862779,
85.4096039041595));
#172927=CARTESIAN_POINT('Ctrl Pts',(-8.06448284348034,1.01960200084586,
85.3722260810903));
#172928=CARTESIAN_POINT('Ctrl Pts',(-8.03143645827967,1.25360762486109,
85.3623071774363));
#172929=CARTESIAN_POINT('Ctrl Pts',(-7.98432659985631,1.50687505881302,
85.3520217253124));
#172930=CARTESIAN_POINT('Ctrl Pts',(-7.98033816105292,1.52785684641247,
85.3511725808549));
#172931=CARTESIAN_POINT('Ctrl Pts',(-7.97439042331957,1.55848704138068,
85.3499369913192));
#172932=CARTESIAN_POINT('Ctrl Pts',(-7.97249626326144,1.56814789324158,
85.3495478695693));
#172933=CARTESIAN_POINT('Ctrl Pts',(-7.96911149423568,1.58524669977727,
85.3488601667896));
#172934=CARTESIAN_POINT('Ctrl Pts',(-7.96762802068115,1.59268604290622,
85.3485612989009));
#172935=CARTESIAN_POINT('Ctrl Pts',(-7.9645286183128,1.60811626304742,85.3479420889311));
#172936=CARTESIAN_POINT('Ctrl Pts',(-7.96291107619187,1.61610680979537,
85.3476218111559));
#172937=CARTESIAN_POINT('Ctrl Pts',(-7.95897655286157,1.63539376606561,
85.3468496432249));
#172938=CARTESIAN_POINT('Ctrl Pts',(-7.95664754081965,1.64668772143583,
85.3463982217424));
#172939=CARTESIAN_POINT('Ctrl Pts',(-7.94724951573237,1.69177560380963,
85.3445988922921));
#172940=CARTESIAN_POINT('Ctrl Pts',(-7.93998912970386,1.72552954802855,
85.3432582473928));
#172941=CARTESIAN_POINT('Ctrl Pts',(-7.85044985771103,2.1292680534052,85.3272896366083));
#172942=CARTESIAN_POINT('Ctrl Pts',(-7.74258969523478,2.49312719942653,
85.3135533762997));
#172943=CARTESIAN_POINT('Ctrl Pts',(-7.51811921254646,3.09287141221511,
85.2905129521433));
#172944=CARTESIAN_POINT('Ctrl Pts',(-7.41477045143502,3.333039007801,85.2811758703354));
#172945=CARTESIAN_POINT('Ctrl Pts',(-7.220812793615,3.72989229437355,85.2652024299151));
#172946=CARTESIAN_POINT('Ctrl Pts',(-7.13622117424427,3.88929037692719,
85.2586310125887));
#172947=CARTESIAN_POINT('Ctrl Pts',(-6.89635065880736,4.30706884877446,
85.2408618566845));
#172948=CARTESIAN_POINT('Ctrl Pts',(-6.73189012375179,4.5598397872675,85.2295215682954));
#172949=CARTESIAN_POINT('Ctrl Pts',(-6.52640662782762,4.84023221912691,
85.216133603404));
#172950=CARTESIAN_POINT('Ctrl Pts',(-6.49871883010637,4.87734404506329,
85.2143447063804));
#172951=CARTESIAN_POINT('Ctrl Pts',(-6.45364879607592,4.93668928062373,
85.2114566968211));
#172952=CARTESIAN_POINT('Ctrl Pts',(-6.43646522025043,4.95907242297123,
85.2103610689039));
#172953=CARTESIAN_POINT('Ctrl Pts',(-6.40562942562689,4.99880852861293,
85.2084046742599));
#172954=CARTESIAN_POINT('Ctrl Pts',(-6.39202238928627,5.01619624956497,
85.2075446796748));
#172955=CARTESIAN_POINT('Ctrl Pts',(-6.36409343928026,5.05158702558722,
85.2057862485123));
#172956=CARTESIAN_POINT('Ctrl Pts',(-6.34976558134437,5.06958517418161,
85.2048877082685));
#172957=CARTESIAN_POINT('Ctrl Pts',(-6.31488409595752,5.11302219748659,
85.2027085512907));
#172958=CARTESIAN_POINT('Ctrl Pts',(-6.29425297713415,5.13839825073588,
85.201426598406));
#172959=CARTESIAN_POINT('Ctrl Pts',(-6.24979714347838,5.1924089529434,85.1986785080433));
#172960=CARTESIAN_POINT('Ctrl Pts',(-6.22592760875505,5.22100569411556,
85.1972115659069));
#172961=CARTESIAN_POINT('Ctrl Pts',(-6.15892012011215,5.30017060423759,
85.1931163830593));
#172962=CARTESIAN_POINT('Ctrl Pts',(-6.11535729561255,5.35037479961232,
85.1904799524653));
#172963=CARTESIAN_POINT('Ctrl Pts',(-5.60168411762606,5.92788998620443,
85.1596732537404));
#172964=CARTESIAN_POINT('Ctrl Pts',(-5.06537503241138,6.39222613976513,
85.1298116893153));
#172965=CARTESIAN_POINT('Ctrl Pts',(-4.17316780741306,6.98111113265038,
85.0845204638603));
#172966=CARTESIAN_POINT('Ctrl Pts',(-3.857403025468,7.16042636672237,85.0692664032416));
#172967=CARTESIAN_POINT('Ctrl Pts',(-3.50968640450292,7.32818759927291,
85.0538675031234));
#172968=CARTESIAN_POINT('Ctrl Pts',(-3.48862468080854,7.33823752665317,
85.0529401141295));
#172969=CARTESIAN_POINT('Ctrl Pts',(-3.45911680872545,7.35216191336045,
85.0516485450925));
#172970=CARTESIAN_POINT('Ctrl Pts',(-3.45070697205153,7.35611278397529,
85.0512813174631));
#172971=CARTESIAN_POINT('Ctrl Pts',(-3.4353272125972,7.36330588771629,85.0506113550815));
#172972=CARTESIAN_POINT('Ctrl Pts',(-3.42835943640434,7.36655266926118,
85.0503084348293));
#172973=CARTESIAN_POINT('Ctrl Pts',(-3.4142862113079,7.37308609191272,85.0496978435257));
#172974=CARTESIAN_POINT('Ctrl Pts',(-3.4071805978904,7.37637236216918,85.0493901880632));
#172975=CARTESIAN_POINT('Ctrl Pts',(-3.3907705473869,7.3839330644471,85.0486811522825));
#172976=CARTESIAN_POINT('Ctrl Pts',(-3.38146274622301,7.38820019371244,
85.0482800816208));
#172977=CARTESIAN_POINT('Ctrl Pts',(-3.3494108166993,7.40282103227189,85.0469027940046));
#172978=CARTESIAN_POINT('Ctrl Pts',(-3.32662686328344,7.41308746646742,
85.0459303657641));
#172979=CARTESIAN_POINT('Ctrl Pts',(-3.04938429850158,7.53647721714288,
85.0341805580989));
#172980=CARTESIAN_POINT('Ctrl Pts',(-2.78932480999776,7.63655019190068,
85.0240793765987));
#172981=CARTESIAN_POINT('Ctrl Pts',(-2.24623406438895,7.81408427715416,
85.0040828902318));
#172982=CARTESIAN_POINT('Ctrl Pts',(-1.96310240896236,7.88997582535356,
84.9942237083096));
#172983=CARTESIAN_POINT('Ctrl Pts',(-1.05389119882884,8.08169909946907,
84.9629814264044));
#172984=CARTESIAN_POINT('Ctrl Pts',(-0.418044833291394,8.13939365751577,
84.9415732731541));
#172985=CARTESIAN_POINT('Ctrl Pts',(0.332034376420807,8.1192648282605,84.9135094626895));
#172986=CARTESIAN_POINT('Ctrl Pts',(0.446021205798871,8.1138013325801,84.9091746689908));
#172987=CARTESIAN_POINT('Ctrl Pts',(0.580351004771784,8.10452358001241,
84.90397493682));
#172988=CARTESIAN_POINT('Ctrl Pts',(0.600843783824984,8.10303008064512,
84.9031791828658));
#172989=CARTESIAN_POINT('Ctrl Pts',(0.633771601765279,8.10050472553897,
84.9018964850236));
#172990=CARTESIAN_POINT('Ctrl Pts',(0.646210366387321,8.09952192492902,
84.9014109987072));
#172991=CARTESIAN_POINT('Ctrl Pts',(0.668302189978918,8.09772521075269,
84.9005470771186));
#172992=CARTESIAN_POINT('Ctrl Pts',(0.677956162722878,8.09692267757574,
84.9001689808299));
#172993=CARTESIAN_POINT('Ctrl Pts',(0.698054429891007,8.09521571526304,
84.8993806451907));
#172994=CARTESIAN_POINT('Ctrl Pts',(0.708498452072714,8.09430833401813,
84.8989703186827));
#172995=CARTESIAN_POINT('Ctrl Pts',(0.735531853613278,8.09190693807378,
84.8979064829684));
#172996=CARTESIAN_POINT('Ctrl Pts',(0.75211841024307,8.09038212293598,84.8972520582982));
#172997=CARTESIAN_POINT('Ctrl Pts',(0.822227995032138,8.08371942848762,
84.8944786309233));
#172998=CARTESIAN_POINT('Ctrl Pts',(0.875703423722341,8.07810138913002,
84.8923453527549));
#172999=CARTESIAN_POINT('Ctrl Pts',(1.24022471970237,8.03614332857444,84.8776791718487));
#173000=CARTESIAN_POINT('Ctrl Pts',(1.54897563088413,7.98238092741736,84.8646239855646));
#173001=CARTESIAN_POINT('Ctrl Pts',(2.18728376632444,7.83280096065651,84.8363617632022));
#173002=CARTESIAN_POINT('Ctrl Pts',(2.51544119488379,7.73366112403378,84.8210940357378));
#173003=CARTESIAN_POINT('Ctrl Pts',(3.05109895483064,7.53412240022367,84.7953545241231));
#173004=CARTESIAN_POINT('Ctrl Pts',(3.26236997469419,7.44507541805762,84.784983184393));
#173005=CARTESIAN_POINT('Ctrl Pts',(3.8561195476993,7.16468758588721,84.7555645357176));
#173006=CARTESIAN_POINT('Ctrl Pts',(4.22770210842211,6.95191042349121,84.7368141046931));
#173007=CARTESIAN_POINT('Ctrl Pts',(4.60406821598988,6.69500058930455,84.7185739507044));
#173008=CARTESIAN_POINT('Ctrl Pts',(4.62719246156382,6.67903937560237,84.7174559658574));
#173009=CARTESIAN_POINT('Ctrl Pts',(4.65847882667002,6.65720389360648,84.7159463933059));
#173010=CARTESIAN_POINT('Ctrl Pts',(4.66671333508219,6.65143407912942,84.7155493632374));
#173011=CARTESIAN_POINT('Ctrl Pts',(4.68065411141514,6.64162732387729,84.7148776518969));
#173012=CARTESIAN_POINT('Ctrl Pts',(4.68636590543443,6.63759828709141,84.714602567414));
#173013=CARTESIAN_POINT('Ctrl Pts',(4.6973584483303,6.62982300598948,84.7140733906467));
#173014=CARTESIAN_POINT('Ctrl Pts',(4.70263993001324,6.62607781208529,84.7138192459152));
#173015=CARTESIAN_POINT('Ctrl Pts',(4.71509489714885,6.61722337814759,84.7132201445937));
#173016=CARTESIAN_POINT('Ctrl Pts',(4.72226457191375,6.61210877398739,84.7128754546932));
#173017=CARTESIAN_POINT('Ctrl Pts',(4.74315949175458,6.59715172277083,84.711871396121));
#173018=CARTESIAN_POINT('Ctrl Pts',(4.7568624288728,6.58727809156614,84.7112135471533));
#173019=CARTESIAN_POINT('Ctrl Pts',(4.85526232029924,6.51590903840302,84.7064932757088));
#173020=CARTESIAN_POINT('Ctrl Pts',(4.9387969619139,6.45282329183333,84.7025057347998));
#173021=CARTESIAN_POINT('Ctrl Pts',(5.31333354294604,6.15843675536292,84.684611365784));
#173022=CARTESIAN_POINT('Ctrl Pts',(5.58948209517873,5.90893990133547,84.6713460422368));
#173023=CARTESIAN_POINT('Ctrl Pts',(6.06029310433106,5.42092166135052,84.6470648268455));
#173024=CARTESIAN_POINT('Ctrl Pts',(6.26035708909408,5.18859034085921,84.6360881806754));
#173025=CARTESIAN_POINT('Ctrl Pts',(6.72256862175774,4.58606596824537,84.6083261918241));
#173026=CARTESIAN_POINT('Ctrl Pts',(6.96775557051908,4.2041979491997,84.5912784181376));
#173027=CARTESIAN_POINT('Ctrl Pts',(7.26204193379715,3.64873549229596,84.567114547839));
#173028=CARTESIAN_POINT('Ctrl Pts',(7.3391992317856,3.49094221534271,84.5603324260626));
#173029=CARTESIAN_POINT('Ctrl Pts',(7.4358127127681,3.27597113800049,84.5511676643614));
#173030=CARTESIAN_POINT('Ctrl Pts',(7.45983397313095,3.22089655835049,84.548826128002));
#173031=CARTESIAN_POINT('Ctrl Pts',(7.49717101063571,3.13263349648626,84.5450823782366));
#173032=CARTESIAN_POINT('Ctrl Pts',(7.51088241760751,3.09961466700231,84.5436838082965));
#173033=CARTESIAN_POINT('Ctrl Pts',(7.53874412654534,3.03124958817437,84.5407917631937));
#173034=CARTESIAN_POINT('Ctrl Pts',(7.55286481414032,2.99589221386206,84.5392980551749));
#173035=CARTESIAN_POINT('Ctrl Pts',(7.58029743367601,2.92577574020036,84.5363395271524));
#173036=CARTESIAN_POINT('Ctrl Pts',(7.59362007026261,2.89102180562507,84.534874844425));
#173037=CARTESIAN_POINT('Ctrl Pts',(7.62404245166368,2.80999952289691,84.5314638981928));
#173038=CARTESIAN_POINT('Ctrl Pts',(7.64096057350713,2.76366461559956,84.529516026765));
#173039=CARTESIAN_POINT('Ctrl Pts',(7.68407732277075,2.64215453634266,84.5244143060415));
#173040=CARTESIAN_POINT('Ctrl Pts',(7.70959481037355,2.5667435851059,84.5212544762741));
#173041=CARTESIAN_POINT('Ctrl Pts',(7.78346736341931,2.33738302898675,84.5116601939234));
#173042=CARTESIAN_POINT('Ctrl Pts',(7.82834829574597,2.18235781850355,84.5051969493021));
#173043=CARTESIAN_POINT('Ctrl Pts',(7.94554339837831,1.72721785349693,84.4862744354011));
#173044=CARTESIAN_POINT('Ctrl Pts',(8.00541104878279,1.42419521916794,84.47373707899));
#173045=CARTESIAN_POINT('Ctrl Pts',(8.08845278629873,0.826692009431081,
84.4492202069406));
#173046=CARTESIAN_POINT('Ctrl Pts',(8.1131083316348,0.532884010314892,84.4372606206839));
#173047=CARTESIAN_POINT('Ctrl Pts',(8.12405743158788,0.159848718546276,
84.4223301803258));
#173048=CARTESIAN_POINT('Ctrl Pts',(8.12522331389318,0.0812831978779437,
84.4192002007009));
#173049=CARTESIAN_POINT('Ctrl Pts',(8.12524954711001,0.00271287458458927,
84.4160871754279));
#173050=CARTESIAN_POINT('',(8.12696554915539,0.00168838483199298,82.4167025567875));
#173051=CARTESIAN_POINT('Ctrl Pts',(8.12696554915539,0.00168838483199298,
82.4167025567875));
#173052=CARTESIAN_POINT('Ctrl Pts',(8.1306575932175,0.773914348629653,82.4468290208393));
#173053=CARTESIAN_POINT('Ctrl Pts',(7.6585312809221,4.25683691476204,82.5827337950821));
#173054=CARTESIAN_POINT('Ctrl Pts',(3.83053466397931,8.09334768555451,82.7715277244204));
#173055=CARTESIAN_POINT('Ctrl Pts',(-1.74999298391506,8.26945455504389,
82.9830843448022));
#173056=CARTESIAN_POINT('Ctrl Pts',(-6.7807722929522,5.84776877811943,83.1946409651841));
#173057=CARTESIAN_POINT('Ctrl Pts',(-8.9610148003001,0.17955105281233,83.406197585566));
#173058=CARTESIAN_POINT('Ctrl Pts',(-6.81611969460216,-5.00581298154604,
83.617754205948));
#173059=CARTESIAN_POINT('Ctrl Pts',(-3.62342745787797,-7.65690432669867,
83.7764216712344));
#173060=CARTESIAN_POINT('Ctrl Pts',(0.494311211966013,-8.45828284271794,
83.9350891365208));
#173061=CARTESIAN_POINT('Ctrl Pts',(4.46947152341248,-7.18896984766675,
84.0937566018073));
#173062=CARTESIAN_POINT('Ctrl Pts',(7.36660492052287,-4.18569279410471,
84.2524240670937));
#173063=CARTESIAN_POINT('Ctrl Pts',(8.11510270816399,-1.4397668579716,84.3600727187538));
#173064=CARTESIAN_POINT('Ctrl Pts',(8.12636183407427,-0.0449434531184864,
84.4148322153184));
#173065=CARTESIAN_POINT('Ctrl Pts',(8.12631724021387,0.00268884911775716,
84.4167025567875));
#173066=CARTESIAN_POINT('',(8.12524999728007,0.000210238465757252,80.4167025567658));
#173067=CARTESIAN_POINT('Ctrl Pts',(8.12524999728006,0.000210239022574176,
80.4167025567875));
#173068=CARTESIAN_POINT('Ctrl Pts',(8.12524459943052,0.208824588488869,
80.4248543423937));
#173069=CARTESIAN_POINT('Ctrl Pts',(8.11720065752198,0.417390467344348,
80.4330061279999));
#173070=CARTESIAN_POINT('Ctrl Pts',(8.10115533523439,0.625275776680494,
80.4411579136061));
#173071=CARTESIAN_POINT('Ctrl Pts',(8.08510346328949,0.833245944239645,
80.4493130267492));
#173072=CARTESIAN_POINT('Ctrl Pts',(8.06104371662649,1.04053468585204,80.4574681398922));
#173073=CARTESIAN_POINT('Ctrl Pts',(8.02906513843042,1.24651536907546,80.4656232530353));
#173074=CARTESIAN_POINT('Ctrl Pts',(7.99707056053867,1.45259910967143,80.4737824463889));
#173075=CARTESIAN_POINT('Ctrl Pts',(7.95714929118456,1.65737318666362,80.4819416397424));
#173076=CARTESIAN_POINT('Ctrl Pts',(7.90944159300706,1.86022075284359,80.4901008330959));
#173077=CARTESIAN_POINT('Ctrl Pts',(7.86170562258791,2.06318852929624,80.4982648617003));
#173078=CARTESIAN_POINT('Ctrl Pts',(7.80617408419124,2.26422722204124,80.5064288903046));
#173079=CARTESIAN_POINT('Ctrl Pts',(7.74303743588964,2.46273401505552,80.514592918909));
#173080=CARTESIAN_POINT('Ctrl Pts',(7.67982447814697,2.66148073120212,80.52276681488));
#173081=CARTESIAN_POINT('Ctrl Pts',(7.60898812947687,2.85768914198913,80.530940710851));
#173082=CARTESIAN_POINT('Ctrl Pts',(7.53076805115067,3.05077369240465,80.539114606822));
#173083=CARTESIAN_POINT('Ctrl Pts',(7.4524980509439,3.24398147388913,80.5472937195644));
#173084=CARTESIAN_POINT('Ctrl Pts',(7.36683503684257,3.43406113856047,80.5554728323067));
#173085=CARTESIAN_POINT('Ctrl Pts',(7.2740657327235,3.62044959618523,80.563651945049));
#173086=CARTESIAN_POINT('Ctrl Pts',(7.18117875495046,3.80707447911331,80.5718414326248));
#173087=CARTESIAN_POINT('Ctrl Pts',(7.08116761105212,3.98999852830687,80.5800309202006));
#173088=CARTESIAN_POINT('Ctrl Pts',(6.97436452454461,4.1686840898866,80.5882204077763));
#173089=CARTESIAN_POINT('Ctrl Pts',(6.90980065891797,4.2767018538343,80.5931710603528));
#173090=CARTESIAN_POINT('Ctrl Pts',(6.84275562068071,4.38317127256495,80.5981217129293));
#173091=CARTESIAN_POINT('Ctrl Pts',(6.77331025023344,4.48797903477529,80.6030723655058));
#173092=CARTESIAN_POINT('Ctrl Pts',(6.659996676596,4.65899320036341,80.6111503141389));
#173093=CARTESIAN_POINT('Ctrl Pts',(6.54007552376464,4.82590562692456,80.6192282627719));
#173094=CARTESIAN_POINT('Ctrl Pts',(6.41386406614782,4.98818958174986,80.627306211405));
#173095=CARTESIAN_POINT('Ctrl Pts',(6.28780706572278,5.15027493397276,80.6353742742695));
#173096=CARTESIAN_POINT('Ctrl Pts',(6.15547529762081,5.30774285812216,80.643442337134));
#173097=CARTESIAN_POINT('Ctrl Pts',(6.0172298773309,5.46009451986468,80.6515103999985));
#173098=CARTESIAN_POINT('Ctrl Pts',(5.87913662159627,5.61227849053428,80.6595695824734));
#173099=CARTESIAN_POINT('Ctrl Pts',(5.73514290059066,5.75935719275781,80.6676287649483));
#173100=CARTESIAN_POINT('Ctrl Pts',(5.58565112702972,5.90086341560383,80.6756879474232));
#173101=CARTESIAN_POINT('Ctrl Pts',(5.43635137042584,6.04218787865351,80.6837367781599));
#173102=CARTESIAN_POINT('Ctrl Pts',(5.281567878021,6.17795392555325,80.6917856088966));
#173103=CARTESIAN_POINT('Ctrl Pts',(5.12174108426708,6.30772984743565,80.6998344396333));
#173104=CARTESIAN_POINT('Ctrl Pts',(4.96203518277804,6.43740760739694,80.7078771822708));
#173105=CARTESIAN_POINT('Ctrl Pts',(4.79729382770052,6.56110407541399,80.7159199249083));
#173106=CARTESIAN_POINT('Ctrl Pts',(4.62799282585794,6.67842571017358,80.7239626675458));
#173107=CARTESIAN_POINT('Ctrl Pts',(4.45882972605523,6.79565178204471,80.7319988590667));
#173108=CARTESIAN_POINT('Ctrl Pts',(4.28511464679758,6.9065131992776,80.7400350505875));
#173109=CARTESIAN_POINT('Ctrl Pts',(4.10735508293929,7.01065772842697,80.7480712421083));
#173110=CARTESIAN_POINT('Ctrl Pts',(4.00657258513179,7.06970347287438,80.7526274383362));
#173111=CARTESIAN_POINT('Ctrl Pts',(3.90449059302425,7.12659087020588,80.7571836345642));
#173112=CARTESIAN_POINT('Ctrl Pts',(3.80120582549754,7.18126185532205,80.7617398307921));
#173113=CARTESIAN_POINT('Ctrl Pts',(3.61902545151273,7.27769408587345,80.7697763453008));
#173114=CARTESIAN_POINT('Ctrl Pts',(3.43324562569166,7.3671517422415,80.7778128598094));
#173115=CARTESIAN_POINT('Ctrl Pts',(3.24443259173022,7.44938552635173,80.785849374318));
#173116=CARTESIAN_POINT('Ctrl Pts',(3.0555054959029,7.53166898785266,80.7938907436814));
#173117=CARTESIAN_POINT('Ctrl Pts',(2.86354182583267,7.60671974469297,80.8019321130447));
#173118=CARTESIAN_POINT('Ctrl Pts',(2.6691263568128,7.67433723873712,80.809973482408));
#173119=CARTESIAN_POINT('Ctrl Pts',(2.47456967054992,7.74200384798869,80.8180206927675));
#173120=CARTESIAN_POINT('Ctrl Pts',(2.27755793023016,7.80222631870286,80.826067903127));
#173121=CARTESIAN_POINT('Ctrl Pts',(2.07869014701708,7.85485422112938,80.8341151134865));
#173122=CARTESIAN_POINT('Ctrl Pts',(1.87952924689276,7.90755969332591,80.8421741848595));
#173123=CARTESIAN_POINT('Ctrl Pts',(1.67850714185685,7.95264814364333,80.8502332562324));
#173124=CARTESIAN_POINT('Ctrl Pts',(1.47623382200582,7.9900201041841,80.8582923276053));
#173125=CARTESIAN_POINT('Ctrl Pts',(1.27379679243258,8.02742231168617,80.8663579215801));
#173126=CARTESIAN_POINT('Ctrl Pts',(1.07010683907458,8.05709552086541,80.8744235155549));
#173127=CARTESIAN_POINT('Ctrl Pts',(0.865779028174559,8.07899215477235,
80.8824891095297));
#173128=CARTESIAN_POINT('Ctrl Pts',(0.6611303759287,8.10092317139723,80.8905673683298));
#173129=CARTESIAN_POINT('Ctrl Pts',(0.455842178950087,8.11505318318403,
80.8986456271299));
#173130=CARTESIAN_POINT('Ctrl Pts',(0.250531238446654,8.12138668338495,
80.9067238859299));
#173131=CARTESIAN_POINT('Ctrl Pts',(0.134608823462328,8.12496269661052,
80.9112850226462));
#173132=CARTESIAN_POINT('Ctrl Pts',(0.0186791101409345,8.12605417183529,
80.9158461593624));
#173133=CARTESIAN_POINT('Ctrl Pts',(-0.0971476232167939,8.12466921799302,
80.9204072960786));
#173134=CARTESIAN_POINT('Ctrl Pts',(-0.302490603172819,8.12221390788602,
80.9284934898108));
#173135=CARTESIAN_POINT('Ctrl Pts',(-0.507909199282271,8.11196749316603,
80.936579683543));
#173136=CARTESIAN_POINT('Ctrl Pts',(-0.712787867911589,8.09392494515844,
80.9446658772752));
#173137=CARTESIAN_POINT('Ctrl Pts',(-0.917483794490565,8.0758984902475,
80.9527448585063));
#173138=CARTESIAN_POINT('Ctrl Pts',(-1.12164043977352,8.05008979489223,
80.9608238397374));
#173139=CARTESIAN_POINT('Ctrl Pts',(-1.32464345182455,8.01654584519033,
80.9689028209685));
#173140=CARTESIAN_POINT('Ctrl Pts',(-1.52749311596407,7.98302723449487,
80.9769756993596));
#173141=CARTESIAN_POINT('Ctrl Pts',(-1.7291905731799,7.94178507272085,80.9850485777507));
#173142=CARTESIAN_POINT('Ctrl Pts',(-1.9291271513624,7.89291809132569,80.9931214561418));
#173143=CARTESIAN_POINT('Ctrl Pts',(-2.1289399598695,7.84408136077547,81.0011893370605));
#173144=CARTESIAN_POINT('Ctrl Pts',(-2.32699375628324,7.7876292988069,81.0092572179792));
#173145=CARTESIAN_POINT('Ctrl Pts',(-2.52268999577819,7.72371172090858,
81.0173250988979));
#173146=CARTESIAN_POINT('Ctrl Pts',(-2.71829174134733,7.65982500626487,
81.025389084158));
#173147=CARTESIAN_POINT('Ctrl Pts',(-2.91153789986559,7.58848006361889,
81.033453069418));
#173148=CARTESIAN_POINT('Ctrl Pts',(-3.10184442633261,7.50987674448318,
81.0415170546781));
#173149=CARTESIAN_POINT('Ctrl Pts',(-3.29479560410711,7.43018109091952,
81.0496931035103));
#173150=CARTESIAN_POINT('Ctrl Pts',(-3.48472452195033,7.34302391677189,
81.0578691523426));
#173151=CARTESIAN_POINT('Ctrl Pts',(-3.67104154432248,7.24866481100888,
81.0660452011748));
#173152=CARTESIAN_POINT('Ctrl Pts',(-3.85471778056681,7.15564311507756,
81.0741053658218));
#173153=CARTESIAN_POINT('Ctrl Pts',(-4.03488354464302,7.05562244642963,
81.0821655304687));
#173154=CARTESIAN_POINT('Ctrl Pts',(-4.21099665840461,6.94889881243101,
81.0902256951157));
#173155=CARTESIAN_POINT('Ctrl Pts',(-4.38710126326462,6.84218033478265,
81.098285470336));
#173156=CARTESIAN_POINT('Ctrl Pts',(-4.55915333750779,6.72875970196976,
81.1063452455563));
#173157=CARTESIAN_POINT('Ctrl Pts',(-4.72663756575908,6.608977597515,81.1144050207765));
#173158=CARTESIAN_POINT('Ctrl Pts',(-4.89413443928235,6.48918644935919,
81.1224654045201));
#173159=CARTESIAN_POINT('Ctrl Pts',(-5.05706252164284,6.36303305635309,
81.1305257882637));
#173160=CARTESIAN_POINT('Ctrl Pts',(-5.2149371278674,6.2309002812507,81.1385861720072));
#173161=CARTESIAN_POINT('Ctrl Pts',(-5.37678036407692,6.09544597074875,
81.1468491765609));
#173162=CARTESIAN_POINT('Ctrl Pts',(-5.53331245352298,5.95370793904956,
81.1551121811146));
#173163=CARTESIAN_POINT('Ctrl Pts',(-5.68404881754922,5.80614128334966,
81.1633751856683));
#173164=CARTESIAN_POINT('Ctrl Pts',(-5.83120982392957,5.66207480210431,
81.1714421977241));
#173165=CARTESIAN_POINT('Ctrl Pts',(-5.97284671912935,5.51245330939077,
81.1795092097799));
#173166=CARTESIAN_POINT('Ctrl Pts',(-6.10854703049046,5.35773653129623,
81.1875762218357));
#173167=CARTESIAN_POINT('Ctrl Pts',(-6.2491927124805,5.19738135928412,81.1959372226383));
#173168=CARTESIAN_POINT('Ctrl Pts',(-6.38346074163059,5.03155283186272,
81.204298223441));
#173169=CARTESIAN_POINT('Ctrl Pts',(-6.51093842226193,4.86079915487292,
81.2126592242436));
#173170=CARTESIAN_POINT('Ctrl Pts',(-6.63841610289319,4.69004547788324,
81.2210202250463));
#173171=CARTESIAN_POINT('Ctrl Pts',(-6.75910324131319,4.51436697576811,
81.2293812258489));
#173172=CARTESIAN_POINT('Ctrl Pts',(-6.87263762475796,4.33434419967556,
81.2377422266515));
#173173=CARTESIAN_POINT('Ctrl Pts',(-6.9755429317437,4.17117513603027,81.245320471481));
#173174=CARTESIAN_POINT('Ctrl Pts',(-7.07277811459327,4.00411003239889,
81.2528987163104));
#173175=CARTESIAN_POINT('Ctrl Pts',(-7.16402220555559,3.8335979706806,81.2604769611398));
#173176=CARTESIAN_POINT('Ctrl Pts',(-7.2551983993909,3.66321279147042,81.268049566798));
#173177=CARTESIAN_POINT('Ctrl Pts',(-7.34039219791648,3.48938607867542,
81.2756221724562));
#173178=CARTESIAN_POINT('Ctrl Pts',(-7.41932581694009,3.31259595854766,
81.2831947781144));
#173179=CARTESIAN_POINT('Ctrl Pts',(-7.49821568866519,3.1359038206264,81.2907631868152));
#173180=CARTESIAN_POINT('Ctrl Pts',(-7.57085213553342,2.95625187796577,
81.298331595516));
#173181=CARTESIAN_POINT('Ctrl Pts',(-7.63700326572716,2.77414287335255,
81.3059000042167));
#173182=CARTESIAN_POINT('Ctrl Pts',(-7.7031384132797,2.59207786772876,81.3134665843295));
#173183=CARTESIAN_POINT('Ctrl Pts',(-7.76279123005642,2.40755732401736,
81.3210331644424));
#173184=CARTESIAN_POINT('Ctrl Pts',(-7.8157778942537,2.22110411061598,81.3285997445552));
#173185=CARTESIAN_POINT('Ctrl Pts',(-7.86875515885646,2.03468397317115,
81.3361649823909));
#173186=CARTESIAN_POINT('Ctrl Pts',(-7.9150685271603,1.84633220301755,81.3437302202266));
#173187=CARTESIAN_POINT('Ctrl Pts',(-7.95458408897748,1.65658671185251,
81.3512954580623));
#173188=CARTESIAN_POINT('Ctrl Pts',(-7.9941133922517,1.46677523707505,81.3588633266942));
#173189=CARTESIAN_POINT('Ctrl Pts',(-8.02684008813676,1.27556943279536,
81.3664311953262));
#173190=CARTESIAN_POINT('Ctrl Pts',(-8.05268134402219,1.08351775903164,
81.3739990639581));
#173191=CARTESIAN_POINT('Ctrl Pts',(-8.07818913229328,0.893944409609616,
81.3814692732848));
#173192=CARTESIAN_POINT('Ctrl Pts',(-8.09698812161514,0.703547240953842,
81.3889394826114));
#173193=CARTESIAN_POINT('Ctrl Pts',(-8.10904828820644,0.512858091518751,
81.396409691938));
#173194=CARTESIAN_POINT('Ctrl Pts',(-8.12407196333666,0.275311469730006,
81.4057155333813));
#173195=CARTESIAN_POINT('Ctrl Pts',(-8.12863291018924,0.0374285285094461,
81.4150213748245));
#173196=CARTESIAN_POINT('Ctrl Pts',(-8.12278920829472,-0.199957595781936,
81.4243272162678));
#173197=CARTESIAN_POINT('Ctrl Pts',(-8.11691413274366,-0.438618198283218,
81.4336830188964));
#173198=CARTESIAN_POINT('Ctrl Pts',(-8.1005224424968,-0.676776590626742,
81.443038821525));
#173199=CARTESIAN_POINT('Ctrl Pts',(-8.07372435994447,-0.913598665793323,
81.4523946241535));
#173200=CARTESIAN_POINT('Ctrl Pts',(-8.04679618730156,-1.15157038310867,
81.4617958441066));
#173201=CARTESIAN_POINT('Ctrl Pts',(-8.00936037089796,-1.38819273836294,
81.4711970640597));
#173202=CARTESIAN_POINT('Ctrl Pts',(-7.96157967035697,-1.62263264944919,
81.4805982840128));
#173203=CARTESIAN_POINT('Ctrl Pts',(-7.91374725691933,-1.85732629408804,
81.4900096788756));
#173204=CARTESIAN_POINT('Ctrl Pts',(-7.8555475825956,-2.08983273577795,
81.4994210737384));
#173205=CARTESIAN_POINT('Ctrl Pts',(-7.7871943750683,-2.3193299306922,81.5088324686013));
#173206=CARTESIAN_POINT('Ctrl Pts',(-7.71892134699995,-2.54855792154732,
81.51823282374));
#173207=CARTESIAN_POINT('Ctrl Pts',(-7.64051860677562,-2.77478368759938,
81.5276331788788));
#173208=CARTESIAN_POINT('Ctrl Pts',(-7.55224908031308,-2.9972022606775,
81.5370335340176));
#173209=CARTESIAN_POINT('Ctrl Pts',(-7.4957724170166,-3.13951025037706,
81.5430480750865));
#173210=CARTESIAN_POINT('Ctrl Pts',(-7.43525758628962,-3.28025997400512,
81.5490626161554));
#173211=CARTESIAN_POINT('Ctrl Pts',(-7.37078419891237,-3.41924375492063,
81.5550771572243));
#173212=CARTESIAN_POINT('Ctrl Pts',(-7.28778996778099,-3.59815248774896,
81.5628194557436));
#173213=CARTESIAN_POINT('Ctrl Pts',(-7.19819439753301,-3.77421770557299,
81.5705617542628));
#173214=CARTESIAN_POINT('Ctrl Pts',(-7.10222249715836,-3.94691311829354,
81.578304052782));
#173215=CARTESIAN_POINT('Ctrl Pts',(-7.00631037858702,-4.1195009574102,
81.5860415285504));
#173216=CARTESIAN_POINT('Ctrl Pts',(-6.90403000922432,-4.28872286342957,
81.5937790043187));
#173217=CARTESIAN_POINT('Ctrl Pts',(-6.79565360961821,-4.45407449203344,
81.601516480087));
#173218=CARTESIAN_POINT('Ctrl Pts',(-6.68732545709304,-4.6193525092843,
81.6092505112805));
#173219=CARTESIAN_POINT('Ctrl Pts',(-6.57290687248712,-4.78076338577519,
81.6169845424741));
#173220=CARTESIAN_POINT('Ctrl Pts',(-6.45271499555188,-4.93782915345194,
81.6247185736676));
#173221=CARTESIAN_POINT('Ctrl Pts',(-6.33253849939175,-5.0948748216568,
81.6324516151486));
#173222=CARTESIAN_POINT('Ctrl Pts',(-6.20659039092785,-5.24757620352785,
81.6401846566297));
#173223=CARTESIAN_POINT('Ctrl Pts',(-6.07523016469535,-5.39548570644717,
81.6479176981108));
#173224=CARTESIAN_POINT('Ctrl Pts',(-5.94388306125145,-5.54338043331749,
81.6556499670668));
#173225=CARTESIAN_POINT('Ctrl Pts',(-5.80712515435242,-5.68648397292756,
81.6633822360228));
#173226=CARTESIAN_POINT('Ctrl Pts',(-5.66535503287332,-5.82438322176666,
81.6711145049788));
#173227=CARTESIAN_POINT('Ctrl Pts',(-5.52353037887633,-5.96233551417499,
81.678849748187));
#173228=CARTESIAN_POINT('Ctrl Pts',(-5.37668991187192,-6.0950792696329,
81.6865849913952));
#173229=CARTESIAN_POINT('Ctrl Pts',(-5.22526823113462,-6.22223910463069,
81.6943202346034));
#173230=CARTESIAN_POINT('Ctrl Pts',(-5.09852050495581,-6.32867841945512,
81.7007950305725));
#173231=CARTESIAN_POINT('Ctrl Pts',(-4.96856363617686,-6.43120594199879,
81.7072698265417));
#173232=CARTESIAN_POINT('Ctrl Pts',(-4.83566957250131,-6.52962382898778,
81.7137446225108));
#173233=CARTESIAN_POINT('Ctrl Pts',(-4.66297215341838,-6.65751904570784,
81.7221586970152));
#173234=CARTESIAN_POINT('Ctrl Pts',(-4.48523094752583,-6.77853522090792,
81.7305727715196));
#173235=CARTESIAN_POINT('Ctrl Pts',(-4.30300596328412,-6.89230202780183,
81.738986846024));
#173236=CARTESIAN_POINT('Ctrl Pts',(-4.12073008861839,-7.00610060663452,
81.747403270348));
#173237=CARTESIAN_POINT('Ctrl Pts',(-3.93396815978001,-7.11264563565909,
81.7558196946719));
#173238=CARTESIAN_POINT('Ctrl Pts',(-3.7433071235897,-7.21161142470825,
81.7642361189958));
#173239=CARTESIAN_POINT('Ctrl Pts',(-3.55259880479061,-7.31060175658367,
81.7726546305343));
#173240=CARTESIAN_POINT('Ctrl Pts',(-3.35798968248173,-7.40200897445001,
81.7810731420728));
#173241=CARTESIAN_POINT('Ctrl Pts',(-3.16009011446938,-7.4855539561834,
81.7894916536113));
#173242=CARTESIAN_POINT('Ctrl Pts',(-2.96211453405986,-7.56913102719518,
81.7979133986649));
#173243=CARTESIAN_POINT('Ctrl Pts',(-2.76084622511553,-7.64483972350749,
81.8063351437186));
#173244=CARTESIAN_POINT('Ctrl Pts',(-2.55691561110987,-7.71244903517441,
81.8147568887722));
#173245=CARTESIAN_POINT('Ctrl Pts',(-2.35296289158296,-7.78006567550594,
81.8231795467199));
#173246=CARTESIAN_POINT('Ctrl Pts',(-2.14634754228693,-7.83958109807804,
81.8316022046677));
#173247=CARTESIAN_POINT('Ctrl Pts',(-1.93771581692596,-7.89081396152101,
81.8400248626155));
#173248=CARTESIAN_POINT('Ctrl Pts',(-1.7290444158138,-7.94205656798049,
81.8484491223104));
#173249=CARTESIAN_POINT('Ctrl Pts',(-1.51835612891157,-7.98501340574969,
81.8568733820054));
#173250=CARTESIAN_POINT('Ctrl Pts',(-1.30630938408856,-8.01955381274683,
81.8652976417003));
#173251=CARTESIAN_POINT('Ctrl Pts',(-1.2466168931683,-8.02927715432785,
81.8676691237326));
#173252=CARTESIAN_POINT('Ctrl Pts',(-1.18681680887079,-8.03833384078446,
81.8700406057649));
#173253=CARTESIAN_POINT('Ctrl Pts',(-1.12692394473616,-8.04672169179973,
81.8724120877972));
#173254=CARTESIAN_POINT('Ctrl Pts',(-0.914163755552061,-8.07651824260159,
81.8808364130173));
#173255=CARTESIAN_POINT('Ctrl Pts',(-0.700210299611324,-8.09787375757291,
81.8892607382374));
#173256=CARTESIAN_POINT('Ctrl Pts',(-0.485731139424045,-8.11071839128285,
81.8976850634575));
#173257=CARTESIAN_POINT('Ctrl Pts',(-0.271289043858642,-8.12356080528299,
81.9061079328512));
#173258=CARTESIAN_POINT('Ctrl Pts',(-0.0563216888205175,-8.12789525985763,
81.9145308022449));
#173259=CARTESIAN_POINT('Ctrl Pts',(0.158499999989702,-8.12370391585656,
81.9229536716386));
#173260=CARTESIAN_POINT('Ctrl Pts',(0.373277789627329,-8.11951342836367,
81.9313748198047));
#173261=CARTESIAN_POINT('Ctrl Pts',(0.587909708756205,-8.10680062662074,
81.9397959679709));
#173262=CARTESIAN_POINT('Ctrl Pts',(0.801725487033302,-8.08559978022294,
81.9482171161371));
#173263=CARTESIAN_POINT('Ctrl Pts',(1.01548127581744,-8.06440488206729,
81.9566359016133));
#173264=CARTESIAN_POINT('Ctrl Pts',(1.22842111863655,-8.0347267216894,81.9650546870894));
#173265=CARTESIAN_POINT('Ctrl Pts',(1.43987950438145,-7.9966514601652,81.9734734725656));
#173266=CARTESIAN_POINT('Ctrl Pts',(1.65127882064198,-7.9585868347104,81.9818899063104));
#173267=CARTESIAN_POINT('Ctrl Pts',(1.8611972465454,-7.91212983823219,81.9903063400551));
#173268=CARTESIAN_POINT('Ctrl Pts',(2.06897795081504,-7.85741801112434,
81.9987227737999));
#173269=CARTESIAN_POINT('Ctrl Pts',(2.27668324276792,-7.80272604122918,
82.0071361528685));
#173270=CARTESIAN_POINT('Ctrl Pts',(2.48225210746732,-7.73978529084876,
82.0155495319372));
#173271=CARTESIAN_POINT('Ctrl Pts',(2.68504042990407,-7.66878383136991,
82.0239629110058));
#173272=CARTESIAN_POINT('Ctrl Pts',(2.74221808692595,-7.64876444835341,
82.0263351250317));
#173273=CARTESIAN_POINT('Ctrl Pts',(2.79917477723441,-7.62810454540091,
82.0287073390576));
#173274=CARTESIAN_POINT('Ctrl Pts',(2.85589627835543,-7.60680905569317,
82.0310795530836));
#173275=CARTESIAN_POINT('Ctrl Pts',(3.04085062681898,-7.53736989512329,
82.0388147379943));
#173276=CARTESIAN_POINT('Ctrl Pts',(3.22338505814561,-7.46113825452443,
82.046549922905));
#173277=CARTESIAN_POINT('Ctrl Pts',(3.40296248152987,-7.37831511334397,
82.0542851078156));
#173278=CARTESIAN_POINT('Ctrl Pts',(3.58248437513806,-7.29551758312505,
82.062017900816));
#173279=CARTESIAN_POINT('Ctrl Pts',(3.75905076128054,-7.20613275912688,
82.0697506938165));
#173280=CARTESIAN_POINT('Ctrl Pts',(3.93214466327643,-7.11040968647846,
82.0774834868169));
#173281=CARTESIAN_POINT('Ctrl Pts',(4.10521579413556,-7.01469920655082,
82.08521526254));
#173282=CARTESIAN_POINT('Ctrl Pts',(4.27481504204639,-6.91265231042138,
82.0929470382632));
#173283=CARTESIAN_POINT('Ctrl Pts',(4.44045005482825,-6.80456397376612,
82.1006788139864));
#173284=CARTESIAN_POINT('Ctrl Pts',(4.60614433633973,-6.69643696015305,
82.10841335635));
#173285=CARTESIAN_POINT('Ctrl Pts',(4.76787125016454,-6.5822643766721,82.1161478987136));
#173286=CARTESIAN_POINT('Ctrl Pts',(4.92516691846625,-6.46238488390668,
82.1238824410772));
#173287=CARTESIAN_POINT('Ctrl Pts',(5.08248915225231,-6.34248514483173,
82.1316182897188));
#173288=CARTESIAN_POINT('Ctrl Pts',(5.23537837285552,-6.21687679627382,
82.1393541383604));
#173289=CARTESIAN_POINT('Ctrl Pts',(5.38340372193394,-6.08593886998282,
82.1470899870019));
#173290=CARTESIAN_POINT('Ctrl Pts',(5.53155019205584,-5.95489380435142,
82.1548321654652));
#173291=CARTESIAN_POINT('Ctrl Pts',(5.67482457935493,-5.81851068804195,
82.1625743439284));
#173292=CARTESIAN_POINT('Ctrl Pts',(5.81283217824947,-5.67720614651323,
82.1703165223916));
#173293=CARTESIAN_POINT('Ctrl Pts',(5.92828444223744,-5.55899577721508,
82.1767933543844));
#173294=CARTESIAN_POINT('Ctrl Pts',(6.04005138833563,-5.4373419236115,82.1832701863773));
#173295=CARTESIAN_POINT('Ctrl Pts',(6.14792370588864,-5.3125061570856,82.1897470183702));
#173296=CARTESIAN_POINT('Ctrl Pts',(6.30444885781006,-5.13136666028106,
82.1991450468417));
#173297=CARTESIAN_POINT('Ctrl Pts',(6.45286304564321,-4.94342492763543,
82.2085430753132));
#173298=CARTESIAN_POINT('Ctrl Pts',(6.59266451167577,-4.74936439947398,
82.2179411037848));
#173299=CARTESIAN_POINT('Ctrl Pts',(6.73266490349367,-4.55502773942305,
82.2273525048642));
#173300=CARTESIAN_POINT('Ctrl Pts',(6.86402803751655,-4.35455489830909,
82.2367639059436));
#173301=CARTESIAN_POINT('Ctrl Pts',(6.98629423363136,-4.14866007810102,
82.2461753070231));
#173302=CARTESIAN_POINT('Ctrl Pts',(7.1083763373526,-3.94307526729443,82.2555725376498));
#173303=CARTESIAN_POINT('Ctrl Pts',(7.22138886300046,-3.7320848268843,82.2649697682766));
#173304=CARTESIAN_POINT('Ctrl Pts',(7.32491838891015,-3.51642690217015,
82.2743669989033));
#173305=CARTESIAN_POINT('Ctrl Pts',(7.42818677473528,-3.30131294719024,
82.2837405262089));
#173306=CARTESIAN_POINT('Ctrl Pts',(7.52201990450268,-3.08155504962869,
82.2931140535145));
#173307=CARTESIAN_POINT('Ctrl Pts',(7.60605182487658,-2.85791238490469,
82.3024875808201));
#173308=CARTESIAN_POINT('Ctrl Pts',(7.68953804689525,-2.6357220425096,82.3118002369899));
#173309=CARTESIAN_POINT('Ctrl Pts',(7.76334990750397,-2.40969725823298,
82.3211128931597));
#173310=CARTESIAN_POINT('Ctrl Pts',(7.82717285021867,-2.18060834064712,
82.3304255493296));
#173311=CARTESIAN_POINT('Ctrl Pts',(7.86826770379246,-2.03310064007533,
82.3364218607719));
#173312=CARTESIAN_POINT('Ctrl Pts',(7.90522212284631,-1.88432309375023,
82.3424181722142));
#173313=CARTESIAN_POINT('Ctrl Pts',(7.93796211318074,-1.73448697089578,
82.3484144836565));
#173314=CARTESIAN_POINT('Ctrl Pts',(7.97744941790813,-1.55377144282478,
82.3556465620641));
#173315=CARTESIAN_POINT('Ctrl Pts',(8.01080108800573,-1.37152414881994,
82.3628786404717));
#173316=CARTESIAN_POINT('Ctrl Pts',(8.03789519688271,-1.18824592001399,
82.3701107188793));
#173317=CARTESIAN_POINT('Ctrl Pts',(8.06498051105206,-1.0050271830497,82.377340449765));
#173318=CARTESIAN_POINT('Ctrl Pts',(8.08581224529326,-0.820778563164806,
82.3845701806507));
#173319=CARTESIAN_POINT('Ctrl Pts',(8.10031960477432,-0.636010898498386,
82.3917999115364));
#173320=CARTESIAN_POINT('Ctrl Pts',(8.11482634946379,-0.451251063899659,
82.3990293360411));
#173321=CARTESIAN_POINT('Ctrl Pts',(8.1230092195426,-0.265972618188351,
82.4062587605459));
#173322=CARTESIAN_POINT('Ctrl Pts',(8.12484932289462,-0.0806910327038236,
82.4134881850507));
#173323=CARTESIAN_POINT('Ctrl Pts',(8.12512204060097,-0.0532308528357421,
82.4145596422963));
#173324=CARTESIAN_POINT('Ctrl Pts',(8.12525552921274,-0.0257706062289944,
82.4156310995419));
#173325=CARTESIAN_POINT('Ctrl Pts',(8.12524982465525,0.00168802838859176,
82.4167025567875));
#173326=CARTESIAN_POINT('',(8.13282513948647,-0.00629553435651024,78.4167025567875));
#173327=CARTESIAN_POINT('Ctrl Pts',(8.12524756561721,-0.00628966863631806,
78.4167025567875));
#173328=CARTESIAN_POINT('Ctrl Pts',(8.12540082558847,0.191697742214765,
78.4244812575649));
#173329=CARTESIAN_POINT('Ctrl Pts',(8.11831345843962,0.389951385898278,
78.4322599583424));
#173330=CARTESIAN_POINT('Ctrl Pts',(8.10395377987199,0.587895140478698,
78.4400386591199));
#173331=CARTESIAN_POINT('Ctrl Pts',(8.08960780372699,0.785650011375491,
78.447809937235));
#173332=CARTESIAN_POINT('Ctrl Pts',(8.06800336055709,0.983095236806884,
78.4555812153501));
#173333=CARTESIAN_POINT('Ctrl Pts',(8.03916077750979,1.17965315065415,78.4633524934652));
#173334=CARTESIAN_POINT('Ctrl Pts',(8.0103452233831,1.37602686642733,78.4711164889711));
#173335=CARTESIAN_POINT('Ctrl Pts',(7.97430509893499,1.57151458453547,78.4788804844771));
#173336=CARTESIAN_POINT('Ctrl Pts',(7.93111265724911,1.76554229077722,78.4866444799831));
#173337=CARTESIAN_POINT('Ctrl Pts',(7.88794352974413,1.95946526580065,78.4944042846818));
#173338=CARTESIAN_POINT('Ctrl Pts',(7.83762984852406,2.15192945898437,78.5021640893806));
#173339=CARTESIAN_POINT('Ctrl Pts',(7.78029529922124,2.34236901862535,78.5099238940794));
#173340=CARTESIAN_POINT('Ctrl Pts',(7.72298367973844,2.53273241572768,78.5176805953976));
#173341=CARTESIAN_POINT('Ctrl Pts',(7.65865688724969,2.72107245920761,78.5254372967158));
#173342=CARTESIAN_POINT('Ctrl Pts',(7.58748904662149,2.90683634384512,78.533193998034));
#173343=CARTESIAN_POINT('Ctrl Pts',(7.56546498063564,2.96432405201403,78.5355944376168));
#173344=CARTESIAN_POINT('Ctrl Pts',(7.54278611068146,3.02156515181753,78.5379948771995));
#173345=CARTESIAN_POINT('Ctrl Pts',(7.51945855803522,3.0785435771629,78.5403953167823));
#173346=CARTESIAN_POINT('Ctrl Pts',(7.44135943959123,3.26930361347196,78.548431831291));
#173347=CARTESIAN_POINT('Ctrl Pts',(7.35602819130241,3.45701454557353,78.5564683457996));
#173348=CARTESIAN_POINT('Ctrl Pts',(7.2637398644644,3.64112218195033,78.5645048603083));
#173349=CARTESIAN_POINT('Ctrl Pts',(7.17139578629167,3.82534103766342,78.5725462296716));
#173350=CARTESIAN_POINT('Ctrl Pts',(7.07208638634842,4.00595197258028,78.5805875990349));
#173351=CARTESIAN_POINT('Ctrl Pts',(6.96613217110615,4.18242634569694,78.5886289683981));
#173352=CARTESIAN_POINT('Ctrl Pts',(6.86010099407507,4.35902890421334,78.5966761787576));
#173353=CARTESIAN_POINT('Ctrl Pts',(6.74741553463572,4.53148863584257,78.6047233891171));
#173354=CARTESIAN_POINT('Ctrl Pts',(6.62843934565627,4.69930626831832,78.6127705994766));
#173355=CARTESIAN_POINT('Ctrl Pts',(6.5092877942703,4.86737125200056,78.6208296708496));
#173356=CARTESIAN_POINT('Ctrl Pts',(6.38382716446754,5.03078020351362,78.6288887422225));
#173357=CARTESIAN_POINT('Ctrl Pts',(6.25246208877077,5.18906594590821,78.6369478135954));
#173358=CARTESIAN_POINT('Ctrl Pts',(6.12099069287306,5.34747979672011,78.6450134075702));
#173359=CARTESIAN_POINT('Ctrl Pts',(5.98360552502437,5.50076192906777,78.653079001545));
#173360=CARTESIAN_POINT('Ctrl Pts',(5.84074836040636,5.64848175644662,78.6611445955198));
#173361=CARTESIAN_POINT('Ctrl Pts',(5.69766687740148,5.79643353770386,78.6692228543199));
#173362=CARTESIAN_POINT('Ctrl Pts',(5.54909645081852,5.93880533756818,78.6773011131199));
#173363=CARTESIAN_POINT('Ctrl Pts',(5.39551354793556,6.0752054382172,78.68537937192));
#173364=CARTESIAN_POINT('Ctrl Pts',(5.30879775500807,6.15221949812321,78.6899405086362));
#173365=CARTESIAN_POINT('Ctrl Pts',(5.22048458220785,6.22733057093386,78.6945016453524));
#173366=CARTESIAN_POINT('Ctrl Pts',(5.13066389792672,6.30047423048546,78.6990627820686));
#173367=CARTESIAN_POINT('Ctrl Pts',(4.97142564232424,6.43014668676428,78.7071489758008));
#173368=CARTESIAN_POINT('Ctrl Pts',(4.80713777818068,6.55388546943611,78.715235169533));
#173369=CARTESIAN_POINT('Ctrl Pts',(4.63826970675071,6.67129235530408,78.7233213632651));
#173370=CARTESIAN_POINT('Ctrl Pts',(4.46955225762668,6.7885945198015,78.7314003444962));
#173371=CARTESIAN_POINT('Ctrl Pts',(4.2962630058349,6.89957586860656,78.7394793257273));
#173372=CARTESIAN_POINT('Ctrl Pts',(4.11890376208171,7.00387887967868,78.7475583069584));
#173373=CARTESIAN_POINT('Ctrl Pts',(3.94167849500881,7.10810310054585,78.7556311853495));
#173374=CARTESIAN_POINT('Ctrl Pts',(3.76038963880158,7.2056588834096,78.7637040637406));
#173375=CARTESIAN_POINT('Ctrl Pts',(3.57556779496498,7.29623207594915,78.7717769421317));
#173376=CARTESIAN_POINT('Ctrl Pts',(3.39086036410816,7.38674919963541,78.7798448230504));
#173377=CARTESIAN_POINT('Ctrl Pts',(3.2026245909936,7.47029221426978,78.787912703969));
#173378=CARTESIAN_POINT('Ctrl Pts',(3.01141602940937,7.54659267883966,78.7959805848877));
#173379=CARTESIAN_POINT('Ctrl Pts',(2.82029979482945,7.62285630095193,78.8040445701478));
#173380=CARTESIAN_POINT('Ctrl Pts',(2.62621392846526,7.69188423081303,78.8121085554078));
#173381=CARTESIAN_POINT('Ctrl Pts',(2.42973490766022,7.75345573541227,78.8201725406679));
#173382=CARTESIAN_POINT('Ctrl Pts',(2.23052545764217,7.81588288675769,78.8283485895001));
#173383=CARTESIAN_POINT('Ctrl Pts',(2.02885614711122,7.87064469852979,78.8365246383323));
#173384=CARTESIAN_POINT('Ctrl Pts',(1.82534601807279,7.91756272326312,78.8447006871646));
#173385=CARTESIAN_POINT('Ctrl Pts',(1.62472036367283,7.9638157498803,78.8527608518115));
#173386=CARTESIAN_POINT('Ctrl Pts',(1.42230604679981,8.00244580329221,78.8608210164585));
#173387=CARTESIAN_POINT('Ctrl Pts',(1.2187090032898,8.03333280325173,78.8688811811054));
#173388=CARTESIAN_POINT('Ctrl Pts',(1.01512179656751,8.06421831090637,78.8769409563257));
#173389=CARTESIAN_POINT('Ctrl Pts',(0.810352290366901,8.087361463868,78.8850007315459));
#173390=CARTESIAN_POINT('Ctrl Pts',(0.605014417715229,8.10269369511502,
78.8930605067662));
#173391=CARTESIAN_POINT('Ctrl Pts',(0.399661041792254,8.11802708396505,
78.9011208905097));
#173392=CARTESIAN_POINT('Ctrl Pts',(0.193739529759944,8.1255483518748,78.9091812742532));
#173393=CARTESIAN_POINT('Ctrl Pts',(-0.0121326807149723,8.12524094169266,
78.9172416579968));
#173394=CARTESIAN_POINT('Ctrl Pts',(-0.223180078303388,8.12492580387595,
78.9255046625505));
#173395=CARTESIAN_POINT('Ctrl Pts',(-0.434175313038718,8.11638322957722,
78.9337676671043));
#173396=CARTESIAN_POINT('Ctrl Pts',(-0.644454750237635,8.09965219237197,
78.942030671658));
#173397=CARTESIAN_POINT('Ctrl Pts',(-0.849746511114368,8.08331800328096,
78.9500976837138));
#173398=CARTESIAN_POINT('Ctrl Pts',(-1.05435572752898,8.05917945067946,
78.9581646957695));
#173399=CARTESIAN_POINT('Ctrl Pts',(-1.25767116318497,8.02732525862712,
78.9662317078253));
#173400=CARTESIAN_POINT('Ctrl Pts',(-1.46839608946059,7.99431019388232,
78.974592708628));
#173401=CARTESIAN_POINT('Ctrl Pts',(-1.67773079525698,7.95300662129811,
78.9829537094307));
#173402=CARTESIAN_POINT('Ctrl Pts',(-1.88500718646095,7.90357105804019,
78.9913147102334));
#173403=CARTESIAN_POINT('Ctrl Pts',(-2.09228357766491,7.85413549478228,
78.9996757110361));
#173404=CARTESIAN_POINT('Ctrl Pts',(-2.29750129769483,7.79656806586894,
79.0080367118388));
#173405=CARTESIAN_POINT('Ctrl Pts',(-2.50001029116285,7.73108246667825,
79.0163977126415));
#173406=CARTESIAN_POINT('Ctrl Pts',(-2.68356041499135,7.67172762206325,
79.0239759574709));
#173407=CARTESIAN_POINT('Ctrl Pts',(-2.86525302554172,7.60574864884786,
79.0315542023004));
#173408=CARTESIAN_POINT('Ctrl Pts',(-3.04455396470433,7.53328472304765,
79.0391324471298));
#173409=CARTESIAN_POINT('Ctrl Pts',(-3.2237214813245,7.46087471955963,79.046705052788));
#173410=CARTESIAN_POINT('Ctrl Pts',(-3.40050052857907,7.38198950015648,
79.0542776584463));
#173411=CARTESIAN_POINT('Ctrl Pts',(-3.57437149736831,7.29681820804801,
79.0618502641045));
#173412=CARTESIAN_POINT('Ctrl Pts',(-3.74814610182904,7.21169412033732,
79.0694186728053));
#173413=CARTESIAN_POINT('Ctrl Pts',(-3.91901550605132,7.1202910535607,79.0769870815061));
#173414=CARTESIAN_POINT('Ctrl Pts',(-4.08647956659481,7.02284645384641,
79.0845554902068));
#173415=CARTESIAN_POINT('Ctrl Pts',(-4.25390316648401,6.92542539752555,
79.0921220703196));
#173416=CARTESIAN_POINT('Ctrl Pts',(-4.41792273901014,6.82196589129611,
79.0996886504324));
#173417=CARTESIAN_POINT('Ctrl Pts',(-4.57806215562732,6.71275163116534,
79.1072552305452));
#173418=CARTESIAN_POINT('Ctrl Pts',(-4.73817316423684,6.60355674514998,
79.114820468381));
#173419=CARTESIAN_POINT('Ctrl Pts',(-4.8944050849753,6.48860934697962,79.1223857062167));
#173420=CARTESIAN_POINT('Ctrl Pts',(-5.04631047429778,6.36823666013541,
79.1299509440525));
#173421=CARTESIAN_POINT('Ctrl Pts',(-5.19826868841348,6.24782211393176,
79.1375188126844));
#173422=CARTESIAN_POINT('Ctrl Pts',(-5.3458970747568,6.12197873603854,79.1450866813164));
#173423=CARTESIAN_POINT('Ctrl Pts',(-5.48878064983627,5.99107457310314,
79.1526545499483));
#173424=CARTESIAN_POINT('Ctrl Pts',(-5.62982038864289,5.86185965852084,
79.1601247592749));
#173425=CARTESIAN_POINT('Ctrl Pts',(-5.76623681665148,5.72771405851611,
79.1675949686015));
#173426=CARTESIAN_POINT('Ctrl Pts',(-5.89766614671137,5.58902689065231,
79.1750651779281));
#173427=CARTESIAN_POINT('Ctrl Pts',(-6.06139121157169,5.41626054128839,
79.1843710193712));
#173428=CARTESIAN_POINT('Ctrl Pts',(-6.21729831841948,5.23653277495086,
79.1936768608144));
#173429=CARTESIAN_POINT('Ctrl Pts',(-6.36489829365976,5.05052049534175,
79.2029827022575));
#173430=CARTESIAN_POINT('Ctrl Pts',(-6.51329070339016,4.86350955332969,
79.2123385048859));
#173431=CARTESIAN_POINT('Ctrl Pts',(-6.65328655720012,4.6701465054957,79.2216943075144));
#173432=CARTESIAN_POINT('Ctrl Pts',(-6.78443609563551,4.47114240734267,
79.2310501101429));
#173433=CARTESIAN_POINT('Ctrl Pts',(-6.91622229362762,4.27117225271375,
79.2404513300959));
#173434=CARTESIAN_POINT('Ctrl Pts',(-7.0390760764616,4.06550619474868,79.2498525500489));
#173435=CARTESIAN_POINT('Ctrl Pts',(-7.15258868013727,3.85488816118862,
79.259253770002));
#173436=CARTESIAN_POINT('Ctrl Pts',(-7.26622413813402,3.64404217641712,
79.2686651648647));
#173437=CARTESIAN_POINT('Ctrl Pts',(-7.37049818697081,3.42823353373309,
79.2780765597275));
#173438=CARTESIAN_POINT('Ctrl Pts',(-7.46504826856119,3.20823033938519,
79.2874879545903));
#173439=CARTESIAN_POINT('Ctrl Pts',(-7.55948744132022,2.9884852124738,79.296888309729));
#173440=CARTESIAN_POINT('Ctrl Pts',(-7.64422543575287,2.76455540382908,
79.3062886648678));
#173441=CARTESIAN_POINT('Ctrl Pts',(-7.71894840877369,2.53722742874779,
79.3156890200065));
#173442=CARTESIAN_POINT('Ctrl Pts',(-7.76675770782843,2.39177830239757,
79.3217035610758));
#173443=CARTESIAN_POINT('Ctrl Pts',(-7.81046810678153,2.2449384901348,79.327718102145));
#173444=CARTESIAN_POINT('Ctrl Pts',(-7.85000767910977,2.09691845344962,
79.3337326432142));
#173445=CARTESIAN_POINT('Ctrl Pts',(-7.9009055229794,1.90637767940598,79.3414749417335));
#173446=CARTESIAN_POINT('Ctrl Pts',(-7.94491300363429,1.71379089693561,
79.3492172402528));
#173447=CARTESIAN_POINT('Ctrl Pts',(-7.98186570632461,1.51970635607644,
79.356959538772));
#173448=CARTESIAN_POINT('Ctrl Pts',(-8.01879539082733,1.32574271231126,
79.3646970145404));
#173449=CARTESIAN_POINT('Ctrl Pts',(-8.04867898148121,1.1302835133879,79.3724344903088));
#173450=CARTESIAN_POINT('Ctrl Pts',(-8.07140237329596,0.933890406232127,
79.3801719660772));
#173451=CARTESIAN_POINT('Ctrl Pts',(-8.09411564909524,0.737584729497141,
79.3879059972707));
#173452=CARTESIAN_POINT('Ctrl Pts',(-8.10967503397298,0.540346322752834,
79.3956400284643));
#173453=CARTESIAN_POINT('Ctrl Pts',(-8.118017811087,0.342745359376757,79.4033740596578));
#173454=CARTESIAN_POINT('Ctrl Pts',(-8.12635952058831,0.1451696827003,79.4111071011389));
#173455=CARTESIAN_POINT('Ctrl Pts',(-8.12748643921373,-0.0527681057730007,
79.41884014262));
#173456=CARTESIAN_POINT('Ctrl Pts',(-8.12138783143314,-0.250494019788233,
79.4265731841011));
#173457=CARTESIAN_POINT('Ctrl Pts',(-8.1152898328989,-0.448200181132632,
79.4343054530572));
#173458=CARTESIAN_POINT('Ctrl Pts',(-8.10196776025479,-0.645694157064347,
79.4420377220132));
#173459=CARTESIAN_POINT('Ctrl Pts',(-8.08146299138581,-0.842403395862962,
79.4497699909693));
#173460=CARTESIAN_POINT('Ctrl Pts',(-8.06095033526488,-1.03918829975874,
79.4575052341775));
#173461=CARTESIAN_POINT('Ctrl Pts',(-8.03324949958436,-1.23518751166042,
79.4652404773857));
#173462=CARTESIAN_POINT('Ctrl Pts',(-7.99845367769798,-1.42983437090443,
79.472975720594));
#173463=CARTESIAN_POINT('Ctrl Pts',(-7.96932778711885,-1.5927637922132,
79.4794505165629));
#173464=CARTESIAN_POINT('Ctrl Pts',(-7.93523169286402,-1.75474569545111,
79.4859253125318));
#173465=CARTESIAN_POINT('Ctrl Pts',(-7.89624744735514,-1.91545394427466,
79.4924001085008));
#173466=CARTESIAN_POINT('Ctrl Pts',(-7.8455869558458,-2.12429622834947,
79.5008141830052));
#173467=CARTESIAN_POINT('Ctrl Pts',(-7.78664655913359,-2.33108810577066,
79.5092282575096));
#173468=CARTESIAN_POINT('Ctrl Pts',(-7.71961898120049,-2.53518645223365,
79.517642332014));
#173469=CARTESIAN_POINT('Ctrl Pts',(-7.65257268430924,-2.73934179774873,
79.5260587563379));
#173470=CARTESIAN_POINT('Ctrl Pts',(-7.57743477981321,-2.94080185974847,
79.5344751806617));
#173471=CARTESIAN_POINT('Ctrl Pts',(-7.49444727281426,-3.13894052787032,
79.5428916049856));
#173472=CARTESIAN_POINT('Ctrl Pts',(-7.41143918549133,-3.33712833300244,
79.5513101165241));
#173473=CARTESIAN_POINT('Ctrl Pts',(-7.32057771134345,-3.53199285640188,
79.5597286280626));
#173474=CARTESIAN_POINT('Ctrl Pts',(-7.2221526656362,-3.72292874451606,
79.5681471396011));
#173475=CARTESIAN_POINT('Ctrl Pts',(-7.12368981528036,-3.91393797030665,
79.5765688846547));
#173476=CARTESIAN_POINT('Ctrl Pts',(-7.01765770776236,-4.10101531008313,
79.5849906297083));
#173477=CARTESIAN_POINT('Ctrl Pts',(-6.90439238921444,-4.2835794959657,
79.593412374762));
#173478=CARTESIAN_POINT('Ctrl Pts',(-6.79111479301389,-4.46616347130972,
79.6018350327098));
#173479=CARTESIAN_POINT('Ctrl Pts',(-6.67060256204162,-4.64423309330062,
79.6102576906577));
#173480=CARTESIAN_POINT('Ctrl Pts',(-6.54323571841143,-4.81723508828507,
79.6186803486056));
#173481=CARTESIAN_POINT('Ctrl Pts',(-6.41584465327461,-4.99026998326805,
79.6271046083005));
#173482=CARTESIAN_POINT('Ctrl Pts',(-6.28159652782727,-5.15823511346599,
79.6355288679954));
#173483=CARTESIAN_POINT('Ctrl Pts',(-6.14091318052228,-5.32060831783244,
79.6439531276903));
#173484=CARTESIAN_POINT('Ctrl Pts',(-6.1013099343659,-5.36631739502537,
79.6463246097227));
#173485=CARTESIAN_POINT('Ctrl Pts',(-6.06119696865709,-5.41158353727088,
79.648696091755));
#173486=CARTESIAN_POINT('Ctrl Pts',(-6.0205842605687,-5.45639557985786,
79.6510675737873));
#173487=CARTESIAN_POINT('Ctrl Pts',(-5.87631386073357,-5.61558346970216,
79.6594918990075));
#173488=CARTESIAN_POINT('Ctrl Pts',(-5.7257193113277,-5.76905470810939,
79.6679162242276));
#173489=CARTESIAN_POINT('Ctrl Pts',(-5.56926842808729,-5.91632797758966,
79.6763405494478));
#173490=CARTESIAN_POINT('Ctrl Pts',(-5.4128445814735,-6.06357579644723,
79.6847634188414));
#173491=CARTESIAN_POINT('Ctrl Pts',(-5.25056661446976,-6.20462760484973,
79.6931862882351));
#173492=CARTESIAN_POINT('Ctrl Pts',(-5.08293824413027,-6.33903986175019,
79.7016091576288));
#173493=CARTESIAN_POINT('Ctrl Pts',(-4.91534412893088,-6.47342465127934,
79.7100303057949));
#173494=CARTESIAN_POINT('Ctrl Pts',(-4.74240199955845,-6.60117243374322,
79.718451453961));
#173495=CARTESIAN_POINT('Ctrl Pts',(-4.56464845453428,-6.72188009778647,
79.7268726021272));
#173496=CARTESIAN_POINT('Ctrl Pts',(-4.3869447811558,-6.84255389533297,
79.7352913876033));
#173497=CARTESIAN_POINT('Ctrl Pts',(-4.20443260646361,-6.95619137133587,
79.7437101730795));
#173498=CARTESIAN_POINT('Ctrl Pts',(-4.01767812023707,-7.06243230655475,
79.7521289585557));
#173499=CARTESIAN_POINT('Ctrl Pts',(-3.83097580262665,-7.16864356407927,
79.7605453923004));
#173500=CARTESIAN_POINT('Ctrl Pts',(-3.64003376881004,-7.26746227575448,
79.7689618260452));
#173501=CARTESIAN_POINT('Ctrl Pts',(-3.44544446140553,-7.3585732330303,
79.7773782597899));
#173502=CARTESIAN_POINT('Ctrl Pts',(-3.25092577860616,-7.44965112232582,
79.7857916388586));
#173503=CARTESIAN_POINT('Ctrl Pts',(-3.05276270453897,-7.53302673188149,
79.7942050179272));
#173504=CARTESIAN_POINT('Ctrl Pts',(-2.85157029193125,-7.60843179851638,
79.8026183969959));
#173505=CARTESIAN_POINT('Ctrl Pts',(-2.7948426134089,-7.62969281091529,
79.8049906110218));
#173506=CARTESIAN_POINT('Ctrl Pts',(-2.73787423246226,-7.65032045579075,
79.8073628250477));
#173507=CARTESIAN_POINT('Ctrl Pts',(-2.68067922986042,-7.67030940895444,
79.8097350390736));
#173508=CARTESIAN_POINT('Ctrl Pts',(-2.49418091383159,-7.73548828708402,
79.8174702239842));
#173509=CARTESIAN_POINT('Ctrl Pts',(-2.30518888622517,-7.79390142900383,
79.8252054088949));
#173510=CARTESIAN_POINT('Ctrl Pts',(-2.1142442949359,-7.84535905002639,
79.8329405938055));
#173511=CARTESIAN_POINT('Ctrl Pts',(-1.92335874843246,-7.89680075908103,
79.8406733868059));
#173512=CARTESIAN_POINT('Ctrl Pts',(-1.73052218134344,-7.94129113859473,
79.8484061798062));
#173513=CARTESIAN_POINT('Ctrl Pts',(-1.53629109203656,-7.97869019595504,
79.8561389728066));
#173514=CARTESIAN_POINT('Ctrl Pts',(-1.34208555454068,-8.01608433333242,
79.8638707485297));
#173515=CARTESIAN_POINT('Ctrl Pts',(-1.14648620721852,-8.04638894070733,
79.8716025242528));
#173516=CARTESIAN_POINT('Ctrl Pts',(-0.9500600678587,-8.06951506783154,
79.8793342999759));
#173517=CARTESIAN_POINT('Ctrl Pts',(-0.753563641862759,-8.0926494701155,
79.8870688423395));
#173518=CARTESIAN_POINT('Ctrl Pts',(-0.556240183493173,-8.10860021463751,
79.8948033847031));
#173519=CARTESIAN_POINT('Ctrl Pts',(-0.358662835275036,-8.11733013577078,
79.9025379270666));
#173520=CARTESIAN_POINT('Ctrl Pts',(-0.161052118446,-8.12606153129039,79.9102737757082));
#173521=CARTESIAN_POINT('Ctrl Pts',(0.0368122202687993,-8.12756966549348,
79.9180096243497));
#173522=CARTESIAN_POINT('Ctrl Pts',(0.234356526461537,-8.12186952499268,
79.9257454729913));
#173523=CARTESIAN_POINT('Ctrl Pts',(0.43206247235047,-8.11616472037883,
79.9334876514544));
#173524=CARTESIAN_POINT('Ctrl Pts',(0.629447509354175,-8.10323987465981,
79.9412298299176));
#173525=CARTESIAN_POINT('Ctrl Pts',(0.825941656388813,-8.08316200151535,
79.9489720083808));
#173526=CARTESIAN_POINT('Ctrl Pts',(0.99032169283829,-8.06636556473023,
79.9554488403739));
#173527=CARTESIAN_POINT('Ctrl Pts',(1.15407823778847,-8.04456408943727,
79.961925672367));
#173528=CARTESIAN_POINT('Ctrl Pts',(1.3168829979073,-8.01782431413427,79.9684025043601));
#173529=CARTESIAN_POINT('Ctrl Pts',(1.5531163559003,-7.97902430050325,79.9778005328316));
#173530=CARTESIAN_POINT('Ctrl Pts',(1.78748001050274,-7.92980496059317,
79.9871985613031));
#173531=CARTESIAN_POINT('Ctrl Pts',(2.01915084346335,-7.87036958686447,
79.9965965897746));
#173532=CARTESIAN_POINT('Ctrl Pts',(2.25115132463096,-7.81084964157304,
80.0060079908541));
#173533=CARTESIAN_POINT('Ctrl Pts',(2.48045128352638,-7.741084594051,80.0154193919336));
#173534=CARTESIAN_POINT('Ctrl Pts',(2.70624020151537,-7.66132831395457,
80.0248307930131));
#173535=CARTESIAN_POINT('Ctrl Pts',(2.93168915618036,-7.58169212039885,
80.0342280236399));
#173536=CARTESIAN_POINT('Ctrl Pts',(3.1536376025266,-7.49209477633976,80.0436252542666));
#173537=CARTESIAN_POINT('Ctrl Pts',(3.37129519995937,-7.3928381719899,80.0530224848934));
#173538=CARTESIAN_POINT('Ctrl Pts',(3.58840378373652,-7.29383192982284,
80.0623960121989));
#173539=CARTESIAN_POINT('Ctrl Pts',(3.80124309432122,-7.18521509110907,
80.0717695395045));
#173540=CARTESIAN_POINT('Ctrl Pts',(4.00904576453681,-7.06733610495139,
80.0811430668101));
#173541=CARTESIAN_POINT('Ctrl Pts',(4.21549897641626,-6.95022261800679,
80.0904557229798));
#173542=CARTESIAN_POINT('Ctrl Pts',(4.41698070153578,-6.82396689213371,
80.0997683791496));
#173543=CARTESIAN_POINT('Ctrl Pts',(4.61275590322929,-6.68895885319407,
80.1090810353193));
#173544=CARTESIAN_POINT('Ctrl Pts',(4.73881328800171,-6.60202874067335,
80.1150773467617));
#173545=CARTESIAN_POINT('Ctrl Pts',(4.86250514511262,-6.51147095877212,
80.121073658204));
#173546=CARTESIAN_POINT('Ctrl Pts',(4.98363930632188,-6.41740031687159,
80.1270699696464));
#173547=CARTESIAN_POINT('Ctrl Pts',(5.13651694433033,-6.29867825369696,
80.1346376278604));
#173548=CARTESIAN_POINT('Ctrl Pts',(5.28525813442047,-6.17440558564283,
80.1422052860744));
#173549=CARTESIAN_POINT('Ctrl Pts',(5.4294233883266,-6.04491929084187,80.1497729442884));
#173550=CARTESIAN_POINT('Ctrl Pts',(5.57354872546522,-5.91546884846848,
80.1573385071538));
#173551=CARTESIAN_POINT('Ctrl Pts',(5.71310037418531,-5.7808078971073,80.1649040700192));
#173552=CARTESIAN_POINT('Ctrl Pts',(5.84767217900044,-5.64131346846142,
80.1724696328847));
#173553=CARTESIAN_POINT('Ctrl Pts',(5.98223219405122,-5.50183126084836,
80.1800345329352));
#173554=CARTESIAN_POINT('Ctrl Pts',(6.11181297891524,-5.35751668399247,
80.1875994329857));
#173555=CARTESIAN_POINT('Ctrl Pts',(6.23604554107561,-5.20878331015324,
80.1951643330362));
#173556=CARTESIAN_POINT('Ctrl Pts',(6.36033907581099,-5.0599769388918,80.202732945893));
#173557=CARTESIAN_POINT('Ctrl Pts',(6.47927890533027,-4.90674771849094,
80.2103015587498));
#173558=CARTESIAN_POINT('Ctrl Pts',(6.59253627508182,-4.74954240156148,
80.2178701716066));
#173559=CARTESIAN_POINT('Ctrl Pts',(6.70581883128138,-4.59230212493312,
80.2254404675898));
#173560=CARTESIAN_POINT('Ctrl Pts',(6.81341620483991,-4.43108429539835,
80.233010763573));
#173561=CARTESIAN_POINT('Ctrl Pts',(6.91504341334367,-4.26636404378158,
80.2405810595562));
#173562=CARTESIAN_POINT('Ctrl Pts',(7.01677359918164,-4.10147688359129,
80.2481590264074));
#173563=CARTESIAN_POINT('Ctrl Pts',(7.11252135029389,-3.93308052975495,
80.2557369932586));
#173564=CARTESIAN_POINT('Ctrl Pts',(7.20204760538713,-3.7616748732762,80.2633149601098));
#173565=CARTESIAN_POINT('Ctrl Pts',(7.29034746383407,-3.59261725785024,
80.2707891183842));
#173566=CARTESIAN_POINT('Ctrl Pts',(7.37259510796375,-3.42063259496863,
80.2782632766586));
#173567=CARTESIAN_POINT('Ctrl Pts',(7.44860772744934,-3.24621787393913,
80.2857374349329));
#173568=CARTESIAN_POINT('Ctrl Pts',(7.54044114432775,-3.03550154953896,
80.2947672183724));
#173569=CARTESIAN_POINT('Ctrl Pts',(7.62332796704879,-2.82088908368092,
80.3037970018119));
#173570=CARTESIAN_POINT('Ctrl Pts',(7.69698348445964,-2.60310061320257,
80.3128267852514));
#173571=CARTESIAN_POINT('Ctrl Pts',(7.77051202053852,-2.38568760774083,
80.3218410014399));
#173572=CARTESIAN_POINT('Ctrl Pts',(7.83484100401659,-2.16510967085444,
80.3308552176283));
#173573=CARTESIAN_POINT('Ctrl Pts',(7.88973559610182,-1.94210189900115,
80.3398694338168));
#173574=CARTESIAN_POINT('Ctrl Pts',(7.94453711375102,-1.71947223948653,
80.3488683662942));
#173575=CARTESIAN_POINT('Ctrl Pts',(7.98993614758686,-1.49442110824226,
80.3578672987715));
#173576=CARTESIAN_POINT('Ctrl Pts',(8.02574813021303,-1.26769653816758,
80.3668662312489));
#173577=CARTESIAN_POINT('Ctrl Pts',(8.06141949001058,-1.04186224693322,
80.3758298276391));
#173578=CARTESIAN_POINT('Ctrl Pts',(8.08757889480169,-0.814367769798356,
80.3847934240293));
#173579=CARTESIAN_POINT('Ctrl Pts',(8.10409343111378,-0.585966912272722,
80.3937570204194));
#173580=CARTESIAN_POINT('Ctrl Pts',(8.11818505523042,-0.391075637619651,
80.4014055325349));
#173581=CARTESIAN_POINT('Ctrl Pts',(8.12525506186471,-0.195524715374751,
80.4090540446503));
#173582=CARTESIAN_POINT('Ctrl Pts',(8.12524999728007,0.000210238465518916,
80.4167025567657));
#173583=CARTESIAN_POINT('',(8.12952934429449,0.00742862902765984,76.4167025567875));
#173584=CARTESIAN_POINT('Ctrl Pts',(8.12952934429449,0.00742862902765984,
76.4167025567875));
#173585=CARTESIAN_POINT('Ctrl Pts',(8.13195251875862,0.526615112398015,
76.4370411272112));
#173586=CARTESIAN_POINT('Ctrl Pts',(7.83647938259965,3.73996568278205,76.5631580078259));
#173587=CARTESIAN_POINT('Ctrl Pts',(4.57239175033108,7.70877801686287,76.742164043536));
#173588=CARTESIAN_POINT('Ctrl Pts',(-0.99660367399542,8.39788261494146,
76.953720663918));
#173589=CARTESIAN_POINT('Ctrl Pts',(-4.87682214009191,6.92632775896648,
77.1123881292042));
#173590=CARTESIAN_POINT('Ctrl Pts',(-7.60342709026179,3.73828686763939,
77.2710555944908));
#173591=CARTESIAN_POINT('Ctrl Pts',(-8.45799212068,-0.346168247782079,77.4297230597773));
#173592=CARTESIAN_POINT('Ctrl Pts',(-7.27250765093393,-4.34712832670027,
77.5883905250636));
#173593=CARTESIAN_POINT('Ctrl Pts',(-4.29449854831541,-7.30169108010175,
77.7470579903501));
#173594=CARTESIAN_POINT('Ctrl Pts',(-0.307003826939667,-8.45123659280709,
77.9057254556364));
#173595=CARTESIAN_POINT('Ctrl Pts',(5.18705264259522,-7.30934400029921,
78.1172820760186));
#173596=CARTESIAN_POINT('Ctrl Pts',(7.9738707902656,-3.29181374846791,78.2876077764021));
#173597=CARTESIAN_POINT('Ctrl Pts',(8.1337744979333,-0.303304450377095,
78.4050443216903));
#173598=CARTESIAN_POINT('Ctrl Pts',(8.13282513948647,-0.00629553435651024,
78.4167025567875));
#173599=CARTESIAN_POINT('',(8.12524972840108,-0.00210085977713058,74.4167026551268));
#173600=CARTESIAN_POINT('Ctrl Pts',(8.12524972905207,-0.0020983420275516,
74.4167027534661));
#173601=CARTESIAN_POINT('Ctrl Pts',(8.12530621810546,0.21663990926585,74.4252463237542));
#173602=CARTESIAN_POINT('Ctrl Pts',(8.11652544175775,0.435225171804719,
74.4337898940423));
#173603=CARTESIAN_POINT('Ctrl Pts',(8.09897060024819,0.652964607628494,
74.4423334643304));
#173604=CARTESIAN_POINT('Ctrl Pts',(8.08139157394798,0.871004016691488,
74.4508888048448));
#173605=CARTESIAN_POINT('Ctrl Pts',(8.05501434439019,1.08819503484192,74.4594441453593));
#173606=CARTESIAN_POINT('Ctrl Pts',(8.01995378981406,1.30385151445515,74.4679994858738));
#173607=CARTESIAN_POINT('Ctrl Pts',(7.98385330648025,1.52590456644559,74.4768085857695));
#173608=CARTESIAN_POINT('Ctrl Pts',(7.93854656671959,1.74633038105455,74.4856176856651));
#173609=CARTESIAN_POINT('Ctrl Pts',(7.88421476674799,1.96439432759641,74.4944267855608));
#173610=CARTESIAN_POINT('Ctrl Pts',(7.83129931122844,2.17677369050512,74.5030062460966));
#173611=CARTESIAN_POINT('Ctrl Pts',(7.76982352019064,2.38691256644583,74.5115857066323));
#173612=CARTESIAN_POINT('Ctrl Pts',(7.70000508393201,2.59414904543306,74.5201651671681));
#173613=CARTESIAN_POINT('Ctrl Pts',(7.62738348873214,2.80970591685749,74.5290890867437));
#173614=CARTESIAN_POINT('Ctrl Pts',(7.54573566105335,3.02212226378135,74.5380130063193));
#173615=CARTESIAN_POINT('Ctrl Pts',(7.45536184516827,3.23067598500828,74.5469369258949));
#173616=CARTESIAN_POINT('Ctrl Pts',(7.36498802928315,3.43922970623527,74.5558608454704));
#173617=CARTESIAN_POINT('Ctrl Pts',(7.26588836458347,3.64392055211116,74.564784765046));
#173618=CARTESIAN_POINT('Ctrl Pts',(7.15841748436445,3.84405341820913,74.5737086846216));
#173619=CARTESIAN_POINT('Ctrl Pts',(7.06715258272108,4.01400742158951,74.581286929451));
#173620=CARTESIAN_POINT('Ctrl Pts',(6.96970326757686,4.18094771215279,74.5888651742805));
#173621=CARTESIAN_POINT('Ctrl Pts',(6.86630212036858,4.34437368953476,74.59644341911));
#173622=CARTESIAN_POINT('Ctrl Pts',(6.76297791667258,4.50767805735015,74.6040160247682));
#173623=CARTESIAN_POINT('Ctrl Pts',(6.65371088678339,4.66747300585524,74.6115886304264));
#173624=CARTESIAN_POINT('Ctrl Pts',(6.53878016623349,4.82328119646486,74.6191612360847));
#173625=CARTESIAN_POINT('Ctrl Pts',(6.42391314361848,4.97900303366146,74.6267296447855));
#173626=CARTESIAN_POINT('Ctrl Pts',(6.30338889389159,5.13074221496769,74.6342980534863));
#173627=CARTESIAN_POINT('Ctrl Pts',(6.17753058885142,5.27804920271733,74.6418664621871));
#173628=CARTESIAN_POINT('Ctrl Pts',(6.05170269218276,5.42532059992243,74.6494330422999));
#173629=CARTESIAN_POINT('Ctrl Pts',(5.92054353767196,5.56816165070676,74.6569996224128));
#173630=CARTESIAN_POINT('Ctrl Pts',(5.78441749887008,5.7061547263692,74.6645662025256));
#173631=CARTESIAN_POINT('Ctrl Pts',(5.64831560821166,5.8441233226843,74.6721314403613));
#173632=CARTESIAN_POINT('Ctrl Pts',(5.5072488475105,5.9772453960949,74.6796966781971));
#173633=CARTESIAN_POINT('Ctrl Pts',(5.36161927736592,6.10513933396103,74.6872619160328));
#173634=CARTESIAN_POINT('Ctrl Pts',(5.21593906483148,6.2330777466866,74.6948297846648));
#173635=CARTESIAN_POINT('Ctrl Pts',(5.06569314741027,6.35578414632546,74.7023976532968));
#173636=CARTESIAN_POINT('Ctrl Pts',(4.91131793613364,6.47291616605005,74.7099655219288));
#173637=CARTESIAN_POINT('Ctrl Pts',(4.75893485456602,6.5885366595753,74.7174357312551));
#173638=CARTESIAN_POINT('Ctrl Pts',(4.60252871783985,6.69872560740381,74.7249059405815));
#173639=CARTESIAN_POINT('Ctrl Pts',(4.44254749923095,6.80319478477405,74.7323761499079));
#173640=CARTESIAN_POINT('Ctrl Pts',(4.24325457593737,6.93333485954801,74.7416819913511));
#173641=CARTESIAN_POINT('Ctrl Pts',(4.03851277875083,7.05453672605251,74.7509878327943));
#173642=CARTESIAN_POINT('Ctrl Pts',(3.82907566883466,7.1664403356784,74.7602936742375));
#173643=CARTESIAN_POINT('Ctrl Pts',(3.61851413333113,7.27894473320685,74.7696494768659));
#173644=CARTESIAN_POINT('Ctrl Pts',(3.40320679896718,7.38205079083557,74.7790052794943));
#173645=CARTESIAN_POINT('Ctrl Pts',(3.18393376850058,7.47544335275853,74.7883610821227));
#173646=CARTESIAN_POINT('Ctrl Pts',(2.96359628693466,7.5692892846878,74.7977623020757));
#173647=CARTESIAN_POINT('Ctrl Pts',(2.73925456139049,7.65332719003012,74.8071635220286));
#173648=CARTESIAN_POINT('Ctrl Pts',(2.5117136941655,7.72728813239428,74.8165647419815));
#173649=CARTESIAN_POINT('Ctrl Pts',(2.28392656020113,7.80132912244544,74.8259761368442));
#173650=CARTESIAN_POINT('Ctrl Pts',(2.052933397635,7.8652713335794,74.8353875317069));
#173651=CARTESIAN_POINT('Ctrl Pts',(1.81955482203533,7.91889561821015,74.8447989265696));
#173652=CARTESIAN_POINT('Ctrl Pts',(1.58645000341915,7.97245700065563,74.8541992817083));
#173653=CARTESIAN_POINT('Ctrl Pts',(1.35096540119324,8.01572464461132,74.8635996368469));
#173654=CARTESIAN_POINT('Ctrl Pts',(1.11393101868102,8.04853062664983,74.8729999919856));
#173655=CARTESIAN_POINT('Ctrl Pts',(0.962271532682516,8.0695205704753,74.8790145330552));
#173656=CARTESIAN_POINT('Ctrl Pts',(0.809977857814596,8.08622883310838,
74.8850290741248));
#173657=CARTESIAN_POINT('Ctrl Pts',(0.657269933840611,8.09862233942102,
74.8910436151944));
#173658=CARTESIAN_POINT('Ctrl Pts',(0.460694614131297,8.11457604635598,
74.8987859137137));
#173659=CARTESIAN_POINT('Ctrl Pts',(0.263340261760429,8.123384379695,74.906528212233));
#173660=CARTESIAN_POINT('Ctrl Pts',(0.06577570720757,8.12498376114324,74.9142705107522));
#173661=CARTESIAN_POINT('Ctrl Pts',(-0.131665782517973,8.12658214632167,
74.9220079865206));
#173662=CARTESIAN_POINT('Ctrl Pts',(-0.329316861931104,8.12098051789449,
74.929745462289));
#173663=CARTESIAN_POINT('Ctrl Pts',(-0.526604529520342,8.10816719314474,
74.9374829380574));
#173664=CARTESIAN_POINT('Ctrl Pts',(-0.723804368448676,8.09535957263981,
74.945216969251));
#173665=CARTESIAN_POINT('Ctrl Pts',(-0.920640765975811,8.07534667275536,
74.9529510004445));
#173666=CARTESIAN_POINT('Ctrl Pts',(-1.11654153437862,8.0481688951281,74.9606850316381));
#173667=CARTESIAN_POINT('Ctrl Pts',(-1.3124172336526,8.02099459540046,74.9684180731192));
#173668=CARTESIAN_POINT('Ctrl Pts',(-1.50735719151998,7.98665728510766,
74.9761511146004));
#173669=CARTESIAN_POINT('Ctrl Pts',(-1.70079477764788,7.94524918972499,
74.9838841560815));
#173670=CARTESIAN_POINT('Ctrl Pts',(-1.89421303950434,7.90384523098036,
74.9916164250375));
#173671=CARTESIAN_POINT('Ctrl Pts',(-2.08612888376544,7.85537197165063,
74.9993486939936));
#173672=CARTESIAN_POINT('Ctrl Pts',(-2.2759864237333,7.79997265132909,75.0070809629496));
#173673=CARTESIAN_POINT('Ctrl Pts',(-2.46591699326275,7.74455202140838,
75.0148162061578));
#173674=CARTESIAN_POINT('Ctrl Pts',(-2.65378733713659,7.68220010679154,
75.0225514493661));
#173675=CARTESIAN_POINT('Ctrl Pts',(-2.83905664342013,7.61311007000109,
75.0302866925743));
#173676=CARTESIAN_POINT('Ctrl Pts',(-2.9941365711183,7.55527815965902,75.0367614885431));
#173677=CARTESIAN_POINT('Ctrl Pts',(-3.14739425040532,7.4927260665029,75.0432362845119));
#173678=CARTESIAN_POINT('Ctrl Pts',(-3.2985235105468,7.42559291995393,75.0497110804807));
#173679=CARTESIAN_POINT('Ctrl Pts',(-3.49491778470703,7.33835259616598,
75.0581251549851));
#173680=CARTESIAN_POINT('Ctrl Pts',(-3.68781206003829,7.24333339033684,
75.0665392294895));
#173681=CARTESIAN_POINT('Ctrl Pts',(-3.876608120588,7.14084007956285,75.0749533039939));
#173682=CARTESIAN_POINT('Ctrl Pts',(-4.06545690668342,7.03831814522687,
75.0833697283178));
#173683=CARTESIAN_POINT('Ctrl Pts',(-4.25020496110848,6.92831806495576,
75.0917861526417));
#173684=CARTESIAN_POINT('Ctrl Pts',(-4.43027963191671,6.811190053546,75.1002025769656));
#173685=CARTESIAN_POINT('Ctrl Pts',(-4.61039895998918,6.69403299520513,
75.1086210885042));
#173686=CARTESIAN_POINT('Ctrl Pts',(-4.78584236942369,6.56974462064712,
75.1170396000427));
#173687=CARTESIAN_POINT('Ctrl Pts',(-4.95606619123124,6.43871846493032,
75.1254581115812));
#173688=CARTESIAN_POINT('Ctrl Pts',(-5.12635539529663,6.30764198261525,
75.1338798566348));
#173689=CARTESIAN_POINT('Ctrl Pts',(-5.29142079539575,6.16982270757484,
75.1423016016885));
#173690=CARTESIAN_POINT('Ctrl Pts',(-5.45075069773424,6.02569534524022,
75.1507233467421));
#173691=CARTESIAN_POINT('Ctrl Pts',(-5.6100978709981,5.88155235989397,75.1591460046898));
#173692=CARTESIAN_POINT('Ctrl Pts',(-5.76370811147268,5.73110010132149,
75.1675686626375));
#173693=CARTESIAN_POINT('Ctrl Pts',(-5.9111051421337,5.57481152696129,75.1759913205852));
#173694=CARTESIAN_POINT('Ctrl Pts',(-6.05853020346894,5.4184932310111,75.1844155802801));
#173695=CARTESIAN_POINT('Ctrl Pts',(-6.19973951345155,5.25633659401228,
75.192839839975));
#173696=CARTESIAN_POINT('Ctrl Pts',(-6.33429489305838,5.08885014224967,
75.20126409967));
#173697=CARTESIAN_POINT('Ctrl Pts',(-6.37217307780808,5.04170165378735,
75.2036355817024));
#173698=CARTESIAN_POINT('Ctrl Pts',(-6.40952420877964,4.99413100456796,
75.2060070637348));
#173699=CARTESIAN_POINT('Ctrl Pts',(-6.44633908841539,4.94615000982258,
75.2083785457672));
#173700=CARTESIAN_POINT('Ctrl Pts',(-6.57711828671848,4.77570490478156,
75.2168028709873));
#173701=CARTESIAN_POINT('Ctrl Pts',(-6.70114073565114,4.60006159722525,
75.2252271962074));
#173702=CARTESIAN_POINT('Ctrl Pts',(-6.81801667296907,4.41976653338339,
75.2336515214275));
#173703=CARTESIAN_POINT('Ctrl Pts',(-6.93487241269567,4.2395026267335,75.2420743908212));
#173704=CARTESIAN_POINT('Ctrl Pts',(-7.04458396399692,4.05458879074625,
75.2504972602149));
#173705=CARTESIAN_POINT('Ctrl Pts',(-7.14680515950424,3.86560002775552,
75.2589201296086));
#173706=CARTESIAN_POINT('Ctrl Pts',(-7.24900546593935,3.6766498849345,75.2673412777748));
#173707=CARTESIAN_POINT('Ctrl Pts',(-7.34371834772962,3.48362671000325,
75.2757624259411));
#173708=CARTESIAN_POINT('Ctrl Pts',(-7.43064330195706,3.28713061522974,
75.2841835741073));
#173709=CARTESIAN_POINT('Ctrl Pts',(-7.51754386797469,3.09068965063179,
75.2926023595834));
#173710=CARTESIAN_POINT('Ctrl Pts',(-7.59666076382036,2.8907779534883,75.3010211450596));
#173711=CARTESIAN_POINT('Ctrl Pts',(-7.66774098444616,2.68801706801587,
75.3094399305357));
#173712=CARTESIAN_POINT('Ctrl Pts',(-7.73880134928791,2.48531282244016,
75.3178563642805));
#173713=CARTESIAN_POINT('Ctrl Pts',(-7.80182943402933,2.27976122651153,
75.3262727980252));
#173714=CARTESIAN_POINT('Ctrl Pts',(-7.85662121798895,2.07200159255388,
75.33468923177));
#173715=CARTESIAN_POINT('Ctrl Pts',(-7.91139311571642,1.86431736326486,
75.3431026108386));
#173716=CARTESIAN_POINT('Ctrl Pts',(-7.95793461498048,1.65442695129161,
75.3515159899072));
#173717=CARTESIAN_POINT('Ctrl Pts',(-7.99609193054374,1.44298350676414,
75.3599293689758));
#173718=CARTESIAN_POINT('Ctrl Pts',(-8.00685066593836,1.38336547449382,
75.3623015830018));
#173719=CARTESIAN_POINT('Ctrl Pts',(-8.01694316794742,1.32362405197726,
75.3646737970278));
#173720=CARTESIAN_POINT('Ctrl Pts',(-8.0263667199826,1.26377404580717,75.3670460110538));
#173721=CARTESIAN_POINT('Ctrl Pts',(-8.05709451971255,1.06861844030229,
75.3747811959645));
#173722=CARTESIAN_POINT('Ctrl Pts',(-8.08071938514722,0.872221018269008,
75.3825163808752));
#173723=CARTESIAN_POINT('Ctrl Pts',(-8.09715150632828,0.675148166009207,
75.3902515657859));
#173724=CARTESIAN_POINT('Ctrl Pts',(-8.11357854629147,0.478136253544567,
75.3979843587863));
#173725=CARTESIAN_POINT('Ctrl Pts',(-8.12281724193719,0.280449678433193,
75.4057171517867));
#173726=CARTESIAN_POINT('Ctrl Pts',(-8.12482951941,0.0826610127197688,75.4134499447871));
#173727=CARTESIAN_POINT('Ctrl Pts',(-8.12684153216034,-0.115101633170138,
75.4211817205102));
#173728=CARTESIAN_POINT('Ctrl Pts',(-8.12162901749148,-0.312965989718375,
75.4289134962333));
#173729=CARTESIAN_POINT('Ctrl Pts',(-8.10920600260128,-0.510358275993785,
75.4366452719565));
#173730=CARTESIAN_POINT('Ctrl Pts',(-8.09677854241716,-0.707821194618828,
75.4443798143201));
#173731=CARTESIAN_POINT('Ctrl Pts',(-8.07713544515563,-0.904811352251254,
75.4521143566838));
#173732=CARTESIAN_POINT('Ctrl Pts',(-8.0503427823418,-1.10075821563922,
75.4598488990474));
#173733=CARTESIAN_POINT('Ctrl Pts',(-8.02354559454599,-1.29673817226739,
75.4675847476889));
#173734=CARTESIAN_POINT('Ctrl Pts',(-7.98959649066467,-1.49167413444426,
75.4753205963305));
#173735=CARTESIAN_POINT('Ctrl Pts',(-7.94861294309523,-1.68500440455182,
75.483056444972));
#173736=CARTESIAN_POINT('Ctrl Pts',(-7.90759586093138,-1.8784928662406,
75.4907986234353));
#173737=CARTESIAN_POINT('Ctrl Pts',(-7.85953291581635,-2.07037266657687,
75.4985408018985));
#173738=CARTESIAN_POINT('Ctrl Pts',(-7.80459210839859,-2.2600950387146,
75.5062829803617));
#173739=CARTESIAN_POINT('Ctrl Pts',(-7.75863057691466,-2.41881004837783,
75.5127598123545));
#173740=CARTESIAN_POINT('Ctrl Pts',(-7.70785656533052,-2.5760153602587,
75.5192366443472));
#173741=CARTESIAN_POINT('Ctrl Pts',(-7.65239452295687,-2.73139993913738,
75.52571347634));
#173742=CARTESIAN_POINT('Ctrl Pts',(-7.57191785567642,-2.95686644775757,
75.5351115048115));
#173743=CARTESIAN_POINT('Ctrl Pts',(-7.48152510899277,-3.17862761966625,
75.5445095332829));
#173744=CARTESIAN_POINT('Ctrl Pts',(-7.38156369033432,-3.39591004710636,
75.5539075617544));
#173745=CARTESIAN_POINT('Ctrl Pts',(-7.28146003494381,-3.61350164925435,
75.5633189628337));
#173746=CARTESIAN_POINT('Ctrl Pts',(-7.17176048805549,-3.82660172531268,
75.5727303639131));
#173747=CARTESIAN_POINT('Ctrl Pts',(-7.05285996042488,-4.03445832065911,
75.5821417649925));
#173748=CARTESIAN_POINT('Ctrl Pts',(-6.93413845760611,-4.24200195282017,
75.5915389956191));
#173749=CARTESIAN_POINT('Ctrl Pts',(-6.80624368370452,-4.44431785359218,
75.6009362262457));
#173750=CARTESIAN_POINT('Ctrl Pts',(-6.66961418037348,-4.64068251957199,
75.6103334568724));
#173751=CARTESIAN_POINT('Ctrl Pts',(-6.53332930761853,-4.83655188061171,
75.6197069841778));
#173752=CARTESIAN_POINT('Ctrl Pts',(-6.3883537188307,-5.02649994834641,
75.6290805114832));
#173753=CARTESIAN_POINT('Ctrl Pts',(-6.23516764793593,-5.20983415903358,
75.6384540387886));
#173754=CARTESIAN_POINT('Ctrl Pts',(-6.08297635838614,-5.3919778081271,
75.6477666949584));
#173755=CARTESIAN_POINT('Ctrl Pts',(-5.92268088945874,-5.56759317338444,
75.6570793511282));
#173756=CARTESIAN_POINT('Ctrl Pts',(-5.75479649173734,-5.73602692646988,
75.6663920072979));
#173757=CARTESIAN_POINT('Ctrl Pts',(-5.6466976725834,-5.84447946917977,
75.6723883187408));
#173758=CARTESIAN_POINT('Ctrl Pts',(-5.53545343527797,-5.94995509218792,
75.6783846301837));
#173759=CARTESIAN_POINT('Ctrl Pts',(-5.42121114614727,-6.05228529329117,
75.6843809416266));
#173760=CARTESIAN_POINT('Ctrl Pts',(-5.27703141066134,-6.18143135154644,
75.6919485998406));
#173761=CARTESIAN_POINT('Ctrl Pts',(-5.12813153575109,-6.30551384389175,
75.6995162580546));
#173762=CARTESIAN_POINT('Ctrl Pts',(-4.97492175438106,-6.42416073119953,
75.7070839162686));
#173763=CARTESIAN_POINT('Ctrl Pts',(-4.82175439404575,-6.54277476731674,
75.7146494791341));
#173764=CARTESIAN_POINT('Ctrl Pts',(-4.6642797920895,-6.65595596814462,
75.7222150419996));
#173765=CARTESIAN_POINT('Ctrl Pts',(-4.50294161846877,-6.76337226116986,
75.729780604865));
#173766=CARTESIAN_POINT('Ctrl Pts',(-4.34161757959845,-6.87077914351156,
75.7373455049156));
#173767=CARTESIAN_POINT('Ctrl Pts',(-4.1764309492916,-6.97242192027236,
75.7449104049662));
#173768=CARTESIAN_POINT('Ctrl Pts',(-4.00785469237258,-7.06801162473061,
75.7524753050168));
#173769=CARTESIAN_POINT('Ctrl Pts',(-3.83919569926737,-7.16364824402569,
75.7600439178736));
#173770=CARTESIAN_POINT('Ctrl Pts',(-3.66714407468579,-7.25322567148377,
75.7676125307304));
#173771=CARTESIAN_POINT('Ctrl Pts',(-3.49219822177283,-7.33650046972987,
75.7751811435872));
#173772=CARTESIAN_POINT('Ctrl Pts',(-3.317213463978,-7.419793786827,75.7827514395705));
#173773=CARTESIAN_POINT('Ctrl Pts',(-3.13933353261881,-7.49678153505065,
75.7903217355537));
#173774=CARTESIAN_POINT('Ctrl Pts',(-2.95907691176168,-7.56726842346556,
75.797892031537));
#173775=CARTESIAN_POINT('Ctrl Pts',(-2.77863763956001,-7.63782673519286,
75.8054699983882));
#173776=CARTESIAN_POINT('Ctrl Pts',(-2.59581721296777,-7.70187090314973,
75.8130479652394));
#173777=CARTESIAN_POINT('Ctrl Pts',(-2.41115025259095,-7.75925524918021,
75.8206259320907));
#173778=CARTESIAN_POINT('Ctrl Pts',(-2.22901299639221,-7.81585350212932,
75.8281000903647));
#173779=CARTESIAN_POINT('Ctrl Pts',(-2.04507981757291,-7.86597320841395,
75.8355742486388));
#173780=CARTESIAN_POINT('Ctrl Pts',(-1.85987240872072,-7.90952351193037,
75.8430484069129));
#173781=CARTESIAN_POINT('Ctrl Pts',(-1.65978049137863,-7.95657380967729,
75.8511232386318));
#173782=CARTESIAN_POINT('Ctrl Pts',(-1.45777415622232,-7.99605722870673,
75.8591980703507));
#173783=CARTESIAN_POINT('Ctrl Pts',(-1.25445250182052,-8.02782887729778,
75.8672729020696));
#173784=CARTESIAN_POINT('Ctrl Pts',(-1.05126536469937,-8.05957950581706,
75.8753423914928));
#173785=CARTESIAN_POINT('Ctrl Pts',(-0.846764955638771,-8.08362848922263,
75.883411880916));
#173786=CARTESIAN_POINT('Ctrl Pts',(-0.641560898076209,-8.09988192361837,
75.8914813703392));
#173787=CARTESIAN_POINT('Ctrl Pts',(-0.436464648012926,-8.11612681899135,
75.8995466203166));
#173788=CARTESIAN_POINT('Ctrl Pts',(-0.23066580179146,-8.12458430800815,
75.907611870294));
#173789=CARTESIAN_POINT('Ctrl Pts',(-0.0247800730888524,-8.12521221325805,
75.9156771202714));
#173790=CARTESIAN_POINT('Ctrl Pts',(0.181025508580555,-8.12583987407748,
75.9237392306147));
#173791=CARTESIAN_POINT('Ctrl Pts',(0.386917588946715,-8.11864402912757,
75.931801340958));
#173792=CARTESIAN_POINT('Ctrl Pts',(0.592278846543603,-8.10363457532711,
75.9398634513013));
#173793=CARTESIAN_POINT('Ctrl Pts',(0.797588086386284,-8.08862892340285,
75.947923519522));
#173794=CARTESIAN_POINT('Ctrl Pts',(1.00236645601473,-8.06581363366268,
75.9559835877426));
#173795=CARTESIAN_POINT('Ctrl Pts',(1.20599952194076,-8.03525063178359,
75.9640436559632));
#173796=CARTESIAN_POINT('Ctrl Pts',(1.41268331489412,-8.00422975055449,
75.9722244760267));
#173797=CARTESIAN_POINT('Ctrl Pts',(1.61818688104359,-7.96522718414051,
75.9804052960902));
#173798=CARTESIAN_POINT('Ctrl Pts',(1.82187530932127,-7.91836207304172,
75.9885861161536));
#173799=CARTESIAN_POINT('Ctrl Pts',(2.02257670567079,-7.87218422525166,
75.9966469668553));
#173800=CARTESIAN_POINT('Ctrl Pts',(2.22151552496948,-7.81837294701084,
76.004707817557));
#173801=CARTESIAN_POINT('Ctrl Pts',(2.41809634264528,-7.75709337575522,
76.0127686682588));
#173802=CARTESIAN_POINT('Ctrl Pts',(2.61470976146192,-7.69580364184001,
76.0208308557793));
#173803=CARTESIAN_POINT('Ctrl Pts',(2.80896409611744,-7.62704323885842,
76.0288930432998));
#173804=CARTESIAN_POINT('Ctrl Pts',(3.00028009424158,-7.55102687841844,
76.0369552308203));
#173805=CARTESIAN_POINT('Ctrl Pts',(3.19165152102717,-7.4749884942839,76.0450197541426));
#173806=CARTESIAN_POINT('Ctrl Pts',(3.38008261892044,-7.39169007678637,
76.053084277465));
#173807=CARTESIAN_POINT('Ctrl Pts',(3.56501453744225,-7.30139431275461,
76.0611488007874));
#173808=CARTESIAN_POINT('Ctrl Pts',(3.75464791193204,-7.20880299281188,
76.0694183455122));
#173809=CARTESIAN_POINT('Ctrl Pts',(3.94060151628308,-7.10885398988861,
76.0776878902371));
#173810=CARTESIAN_POINT('Ctrl Pts',(4.12230025877587,-7.00188032881142,
76.085957434962));
#173811=CARTESIAN_POINT('Ctrl Pts',(4.2997336832766,-6.8974178391106,76.0940328548546));
#173812=CARTESIAN_POINT('Ctrl Pts',(4.4731095158356,-6.78625699138805,76.1021082747472));
#173813=CARTESIAN_POINT('Ctrl Pts',(4.64192191238647,-6.66875164643326,
76.1101836946399));
#173814=CARTESIAN_POINT('Ctrl Pts',(4.81682142488792,-6.54700923906974,
76.1185503017809));
#173815=CARTESIAN_POINT('Ctrl Pts',(4.9868219806478,-6.41845651367071,76.1269169089218));
#173816=CARTESIAN_POINT('Ctrl Pts',(5.15139851814492,-6.28353251521422,
76.1352835160628));
#173817=CARTESIAN_POINT('Ctrl Pts',(5.31597505564203,-6.14860851675773,
76.1436501232038));
#173818=CARTESIAN_POINT('Ctrl Pts',(5.47512731906034,-6.00731352220343,
76.1520167303447));
#173819=CARTESIAN_POINT('Ctrl Pts',(5.62837241333278,-5.86012896951377,
76.1603833374857));
#173820=CARTESIAN_POINT('Ctrl Pts',(5.77633035840448,-5.71802246968975,
76.1684612861188));
#173821=CARTESIAN_POINT('Ctrl Pts',(5.91906960610025,-5.57014972641378,
76.1765392347518));
#173822=CARTESIAN_POINT('Ctrl Pts',(6.05612875466844,-5.41691721086616,
76.1846171833849));
#173823=CARTESIAN_POINT('Ctrl Pts',(6.19302017067409,-5.26387222079763,
76.1926852462494));
#173824=CARTESIAN_POINT('Ctrl Pts',(6.32424513502683,-5.10548076675019,
76.2007533091139));
#173825=CARTESIAN_POINT('Ctrl Pts',(6.44937754428596,-4.94218745635574,
76.2088213719783));
#173826=CARTESIAN_POINT('Ctrl Pts',(6.57437222227587,-4.7790738803325,76.2168805544533));
#173827=CARTESIAN_POINT('Ctrl Pts',(6.69328752288442,-4.61106945295417,
76.2249397369282));
#173828=CARTESIAN_POINT('Ctrl Pts',(6.80573585024926,-4.43865374850663,
76.2329989194032));
#173829=CARTESIAN_POINT('Ctrl Pts',(6.91803974166775,-4.2664595060054,76.2410477501399));
#173830=CARTESIAN_POINT('Ctrl Pts',(7.0238930595349,-4.0898655533672,76.2490965808766));
#173831=CARTESIAN_POINT('Ctrl Pts',(7.12294994496738,-3.90938251441187,
76.2571454116133));
#173832=CARTESIAN_POINT('Ctrl Pts',(7.22193190421692,-3.72903599201603,
76.2651881542507));
#173833=CARTESIAN_POINT('Ctrl Pts',(7.31412752666964,-3.54480652240982,
76.273230896888));
#173834=CARTESIAN_POINT('Ctrl Pts',(7.39923483838501,-3.3572326950823,76.2812736395253));
#173835=CARTESIAN_POINT('Ctrl Pts',(7.48427282699343,-3.16981165369326,
76.2893098310462));
#173836=CARTESIAN_POINT('Ctrl Pts',(7.56223389198272,-2.97905197520006,
76.2973460225671));
#173837=CARTESIAN_POINT('Ctrl Pts',(7.63286237412736,-2.78551602762053,
76.305382214088));
#173838=CARTESIAN_POINT('Ctrl Pts',(7.67290587273076,-2.67578895702119,
76.3099384103161));
#173839=CARTESIAN_POINT('Ctrl Pts',(7.7105932046514,-2.56516990756974,76.3144946065442));
#173840=CARTESIAN_POINT('Ctrl Pts',(7.74588456348531,-2.45376443279708,
76.3190508027724));
#173841=CARTESIAN_POINT('Ctrl Pts',(7.80498441965225,-2.26720183637626,
76.3266807311924));
#173842=CARTESIAN_POINT('Ctrl Pts',(7.85733735241861,-2.07851109462117,
76.3343106596125));
#173843=CARTESIAN_POINT('Ctrl Pts',(7.90280004174291,-1.88823702503904,
76.3419405880325));
#173844=CARTESIAN_POINT('Ctrl Pts',(7.94828568129213,-1.69786690234703,
76.3495743681511));
#173845=CARTESIAN_POINT('Ctrl Pts',(7.98687404736717,-1.5059122071846,76.3572081482697));
#173846=CARTESIAN_POINT('Ctrl Pts',(8.01847276254194,-1.31292883237172,
76.3648419283882));
#173847=CARTESIAN_POINT('Ctrl Pts',(8.05008105541181,-1.1198869635374,76.3724780223357));
#173848=CARTESIAN_POINT('Ctrl Pts',(8.0746954299414,-0.925816151661797,
76.3801141162831));
#173849=CARTESIAN_POINT('Ctrl Pts',(8.09227536083693,-0.731277681111288,
76.3877502102305));
#173850=CARTESIAN_POINT('Ctrl Pts',(8.10986970331353,-0.536579732861084,
76.3953925640539));
#173851=CARTESIAN_POINT('Ctrl Pts',(8.12041807074284,-0.341413720418515,
76.4030349178773));
#173852=CARTESIAN_POINT('Ctrl Pts',(8.12393203108951,-0.146341780561353,
76.4106772717006));
#173853=CARTESIAN_POINT('Ctrl Pts',(8.12485550804272,-0.0950764209942109,
76.4126857000629));
#173854=CARTESIAN_POINT('Ctrl Pts',(8.1252934320321,-0.0438175393908651,
76.4146941284252));
#173855=CARTESIAN_POINT('Ctrl Pts',(8.12524660770978,0.00742471553402487,
76.4167025567875));
#173856=CARTESIAN_POINT('',(8.12524906564331,-0.0038966347636782,72.4167025567875));
#173857=CARTESIAN_POINT('Ctrl Pts',(8.12524906564331,-0.0038966347636782,
72.4167025567875));
#173858=CARTESIAN_POINT('Ctrl Pts',(8.12533820018677,0.181966400879045,
72.4239655139928));
#173859=CARTESIAN_POINT('Ctrl Pts',(8.11904571743255,0.367994713859331,
72.4312284711981));
#173860=CARTESIAN_POINT('Ctrl Pts',(8.10636402924909,0.55366938491884,72.4384914284034));
#173861=CARTESIAN_POINT('Ctrl Pts',(8.0936840973464,0.739318341984484,72.4457533797653));
#173862=CARTESIAN_POINT('Ctrl Pts',(8.07461673634665,0.924613365706575,
72.4530153311273));
#173863=CARTESIAN_POINT('Ctrl Pts',(8.049206453849,1.10903698126604,72.4602772824892));
#173864=CARTESIAN_POINT('Ctrl Pts',(8.02379836453089,1.2934446790921,72.4675386070669));
#173865=CARTESIAN_POINT('Ctrl Pts',(7.99204850192037,1.47698073328401,72.4747999316447));
#173866=CARTESIAN_POINT('Ctrl Pts',(7.95405299875925,1.65913485149008,72.4820612562225));
#173867=CARTESIAN_POINT('Ctrl Pts',(7.91604481293383,1.8413497716158,72.4893250045855));
#173868=CARTESIAN_POINT('Ctrl Pts',(7.87178691239364,2.02218145539832,72.4965887529485));
#173869=CARTESIAN_POINT('Ctrl Pts',(7.82142608333776,2.20113188732154,72.5038525013116));
#173870=CARTESIAN_POINT('Ctrl Pts',(7.80483468765621,2.26008718013709,72.5062455461736));
#173871=CARTESIAN_POINT('Ctrl Pts',(7.78758129581107,2.3188384138625,72.5086385910357));
#173872=CARTESIAN_POINT('Ctrl Pts',(7.76967232571523,2.37736819056597,72.5110316358978));
#173873=CARTESIAN_POINT('Ctrl Pts',(7.70002965467141,2.60497312616041,72.5203374773411));
#173874=CARTESIAN_POINT('Ctrl Pts',(7.62047679462563,2.82920612644778,72.5296433187843));
#173875=CARTESIAN_POINT('Ctrl Pts',(7.53136166697491,3.04930795488435,72.5389491602275));
#173876=CARTESIAN_POINT('Ctrl Pts',(7.44176809818251,3.27059146563297,72.548304962856));
#173877=CARTESIAN_POINT('Ctrl Pts',(7.3425093773523,3.48769930448531,72.5576607654845));
#173878=CARTESIAN_POINT('Ctrl Pts',(7.23398256648911,3.69988969973858,72.567016568113));
#173879=CARTESIAN_POINT('Ctrl Pts',(7.1249289170865,3.91311016375572,72.5764177880661));
#173880=CARTESIAN_POINT('Ctrl Pts',(7.00651701668263,4.12136529862264,72.5858190080192));
#173881=CARTESIAN_POINT('Ctrl Pts',(6.87919273380317,4.32393280402109,72.5952202279722));
#173882=CARTESIAN_POINT('Ctrl Pts',(6.75173064826658,4.52671954757161,72.6046316228351));
#173883=CARTESIAN_POINT('Ctrl Pts',(6.61533691549991,4.7238063233347,72.6140430176979));
#173884=CARTESIAN_POINT('Ctrl Pts',(6.47050121367161,4.91449912059959,72.6234544125607));
#173885=CARTESIAN_POINT('Ctrl Pts',(6.32583540655121,5.10496823201438,72.6328547676995));
#173886=CARTESIAN_POINT('Ctrl Pts',(6.17274744932352,5.28905833020603,72.6422551228383));
#173887=CARTESIAN_POINT('Ctrl Pts',(6.01176704613544,5.46610872060737,72.6516554779771));
#173888=CARTESIAN_POINT('Ctrl Pts',(5.90876846448565,5.5793892114667,72.6576700190462));
#173889=CARTESIAN_POINT('Ctrl Pts',(5.80253978676833,5.68978847537497,72.6636845601153));
#173890=CARTESIAN_POINT('Ctrl Pts',(5.69322869546497,5.79714020734657,72.6696991011844));
#173891=CARTESIAN_POINT('Ctrl Pts',(5.55251652963046,5.93533016164763,72.6774413997037));
#173892=CARTESIAN_POINT('Ctrl Pts',(5.4066283645938,6.06853290350363,72.6851836982229));
#173893=CARTESIAN_POINT('Ctrl Pts',(5.25596022344466,6.19633518235316,72.6929259967422));
#173894=CARTESIAN_POINT('Ctrl Pts',(5.10538593490379,6.32405785195602,72.7006634725106));
#173895=CARTESIAN_POINT('Ctrl Pts',(4.95003786704904,6.4463865290839,72.708400948279));
#173896=CARTESIAN_POINT('Ctrl Pts',(4.79034849363571,6.56294513705715,72.7161384240473));
#173897=CARTESIAN_POINT('Ctrl Pts',(4.6307302108482,6.6794518553886,72.7238724552409));
#173898=CARTESIAN_POINT('Ctrl Pts',(4.46677475637333,6.7901934126344,72.7316064864344));
#173899=CARTESIAN_POINT('Ctrl Pts',(4.29894734816104,6.89483424458044,72.739340517628));
#173900=CARTESIAN_POINT('Ctrl Pts',(4.13114141657244,6.99946168579493,72.7470735591091));
#173901=CARTESIAN_POINT('Ctrl Pts',(3.95946481370844,7.09798976341856,72.7548066005902));
#173902=CARTESIAN_POINT('Ctrl Pts',(3.78441169260494,7.19012626477275,72.7625396420713));
#173903=CARTESIAN_POINT('Ctrl Pts',(3.60937605917799,7.28225356175902,72.7702719110273));
#173904=CARTESIAN_POINT('Ctrl Pts',(3.43096489380225,7.36799039292066,72.7780041799833));
#173905=CARTESIAN_POINT('Ctrl Pts',(3.2496967837625,7.44709059808618,72.7857364489393));
#173906=CARTESIAN_POINT('Ctrl Pts',(3.06835894812452,7.52622122950332,72.7934716921475));
#173907=CARTESIAN_POINT('Ctrl Pts',(2.8841622963857,7.59870999312656,72.8012069353557));
#173908=CARTESIAN_POINT('Ctrl Pts',(2.697645825484,7.66435871829788,72.8089421785639));
#173909=CARTESIAN_POINT('Ctrl Pts',(2.5415219569212,7.71931007401683,72.8154169745329));
#173910=CARTESIAN_POINT('Ctrl Pts',(2.38377314301183,7.76946974238227,72.8218917705019));
#173911=CARTESIAN_POINT('Ctrl Pts',(2.22472360236408,7.81474839361986,72.8283665664708));
#173912=CARTESIAN_POINT('Ctrl Pts',(2.01803682932689,7.87358854036697,72.8367806409753));
#173913=CARTESIAN_POINT('Ctrl Pts',(1.80905368549032,7.92421359863214,72.8451947154797));
#173914=CARTESIAN_POINT('Ctrl Pts',(1.59842875182824,7.96647431978719,72.8536087899841));
#173915=CARTESIAN_POINT('Ctrl Pts',(1.38774499641717,8.00874684319893,72.862025214308));
#173916=CARTESIAN_POINT('Ctrl Pts',(1.17541879473009,8.04265031426947,72.8704416386319));
#173917=CARTESIAN_POINT('Ctrl Pts',(0.962114210042332,8.06808675023606,
72.8788580629558));
#173918=CARTESIAN_POINT('Ctrl Pts',(0.748756727303346,8.09352949426159,
72.8872765744944));
#173919=CARTESIAN_POINT('Ctrl Pts',(0.534420639260289,8.11050097995341,
72.8956950860329));
#173920=CARTESIAN_POINT('Ctrl Pts',(0.31977550978621,8.11895505504501,72.9041135975714));
#173921=CARTESIAN_POINT('Ctrl Pts',(0.10504793601485,8.12741237731153,72.9125353426251));
#173922=CARTESIAN_POINT('Ctrl Pts',(-0.109988652598161,8.12734573973279,
72.9209570876787));
#173923=CARTESIAN_POINT('Ctrl Pts',(-0.324662866439217,8.11876108686883,
72.9293788327324));
#173924=CARTESIAN_POINT('Ctrl Pts',(-0.53936035037808,8.11017550345196,
72.9378014906801));
#173925=CARTESIAN_POINT('Ctrl Pts',(-0.753695117504446,8.09307007479076,
72.9462241486279));
#173926=CARTESIAN_POINT('Ctrl Pts',(-0.966998464671324,8.06750280643418,
72.9546468065757));
#173927=CARTESIAN_POINT('Ctrl Pts',(-1.18034237599743,8.0419306759188,72.9630710662706));
#173928=CARTESIAN_POINT('Ctrl Pts',(-1.39265421346462,8.00789352238933,
72.9714953259656));
#173929=CARTESIAN_POINT('Ctrl Pts',(-1.60327173810763,7.96550107000717,
72.9799195856606));
#173930=CARTESIAN_POINT('Ctrl Pts',(-1.6625618945651,7.95356732831775,72.9822910676927));
#173931=CARTESIAN_POINT('Ctrl Pts',(-1.72171783872473,7.94097177664898,
72.9846625497249));
#173932=CARTESIAN_POINT('Ctrl Pts',(-1.7807249388753,7.92771759427438,72.9870340317571));
#173933=CARTESIAN_POINT('Ctrl Pts',(-1.99033858773114,7.88063414968803,
72.9954583569772));
#173934=CARTESIAN_POINT('Ctrl Pts',(-2.19809465750639,7.82523058662881,
73.0038826821972));
#173935=CARTESIAN_POINT('Ctrl Pts',(-2.40334379003392,7.76167676403787,
73.0123070074173));
#173936=CARTESIAN_POINT('Ctrl Pts',(-2.6085574530005,7.69813392432494,73.0207298768109));
#173937=CARTESIAN_POINT('Ctrl Pts',(-2.81126479202046,7.62644371624108,
73.0291527462045));
#173938=CARTESIAN_POINT('Ctrl Pts',(-3.01083162655915,7.54682585455708,
73.0375756155981));
#173939=CARTESIAN_POINT('Ctrl Pts',(-3.21035767928003,7.46722426291683,
73.0459967637642));
#173940=CARTESIAN_POINT('Ctrl Pts',(-3.40674426409017,7.37969835050973,
73.0544179119303));
#173941=CARTESIAN_POINT('Ctrl Pts',(-3.59937617500349,7.2845163678392,73.0628390600964));
#173942=CARTESIAN_POINT('Ctrl Pts',(-3.79195403990344,7.18936109002087,
73.0712578455725));
#173943=CARTESIAN_POINT('Ctrl Pts',(-3.9807790984489,7.0865541489707,73.0796766310486));
#173944=CARTESIAN_POINT('Ctrl Pts',(-4.16525888331298,6.97641068153834,
73.0880954165248));
#173945=CARTESIAN_POINT('Ctrl Pts',(-4.34968713498416,6.86629798194626,
73.0965118502695));
#173946=CARTESIAN_POINT('Ctrl Pts',(-4.52977231006664,6.74885298302943,
73.1049282840143));
#173947=CARTESIAN_POINT('Ctrl Pts',(-4.70494816856911,6.62443584719319,
73.113344717759));
#173948=CARTESIAN_POINT('Ctrl Pts',(-4.88006044841937,6.50006386754385,
73.1217580968276));
#173949=CARTESIAN_POINT('Ctrl Pts',(-5.05026675490292,6.36872495698999,
73.1301714758962));
#173950=CARTESIAN_POINT('Ctrl Pts',(-5.21503055399626,6.23082208728395,
73.1385848549649));
#173951=CARTESIAN_POINT('Ctrl Pts',(-5.26148691737217,6.19193936024744,
73.1409570689911));
#173952=CARTESIAN_POINT('Ctrl Pts',(-5.30751079024305,6.15253505479862,
73.1433292830174));
#173953=CARTESIAN_POINT('Ctrl Pts',(-5.35309060059216,6.11261879920153,
73.1457014970437));
#173954=CARTESIAN_POINT('Ctrl Pts',(-5.50171473709118,5.98246207026925,
73.1534366819544));
#173955=CARTESIAN_POINT('Ctrl Pts',(-5.64568073970341,5.84680119993373,
73.1611718668651));
#173956=CARTESIAN_POINT('Ctrl Pts',(-5.78455678274856,5.70601352869563,
73.1689070517758));
#173957=CARTESIAN_POINT('Ctrl Pts',(-5.92338988188977,5.56526939248415,
73.1766398447763));
#173958=CARTESIAN_POINT('Ctrl Pts',(-6.05713590802872,5.41940186364829,
73.1843726377767));
#173959=CARTESIAN_POINT('Ctrl Pts',(-6.18539879614912,5.26882617810618,
73.1921054307771));
#173960=CARTESIAN_POINT('Ctrl Pts',(-6.31364481081703,5.11827030134675,
73.1998372065003));
#173961=CARTESIAN_POINT('Ctrl Pts',(-6.43640889579381,4.96300777096174,
73.2075689822235));
#173962=CARTESIAN_POINT('Ctrl Pts',(-6.55333421547803,4.80348813080087,
73.2153007579467));
#173963=CARTESIAN_POINT('Ctrl Pts',(-6.67030137423394,4.64391141015755,
73.2230353003103));
#173964=CARTESIAN_POINT('Ctrl Pts',(-6.78142538102213,4.48007481903832,
73.2307698426739));
#173965=CARTESIAN_POINT('Ctrl Pts',(-6.88639144130183,4.31245875106822,
73.2385043850375));
#173966=CARTESIAN_POINT('Ctrl Pts',(-6.9913752291787,4.14481437461323,73.2462402336791));
#173967=CARTESIAN_POINT('Ctrl Pts',(-7.09019881717135,3.97338955301307,
73.2539760823207));
#173968=CARTESIAN_POINT('Ctrl Pts',(-7.18259253779685,3.79869082691459,
73.2617119309623));
#173969=CARTESIAN_POINT('Ctrl Pts',(-7.27506185914825,3.62384915440786,
73.2694541094256));
#173970=CARTESIAN_POINT('Ctrl Pts',(-7.36109064292379,3.44572854124775,
73.2771962878888));
#173971=CARTESIAN_POINT('Ctrl Pts',(-7.44045630233157,3.2648579717339,73.2849384663521));
#173972=CARTESIAN_POINT('Ctrl Pts',(-7.50685079897228,3.11354806629623,
73.2914152983447));
#173973=CARTESIAN_POINT('Ctrl Pts',(-7.56858298382625,2.96031410241079,
73.2978921303373));
#173974=CARTESIAN_POINT('Ctrl Pts',(-7.62554913898165,2.80547462855686,
73.30436896233));
#173975=CARTESIAN_POINT('Ctrl Pts',(-7.70820830764052,2.58079907955007,
73.3137669908014));
#173976=CARTESIAN_POINT('Ctrl Pts',(-7.7808798634525,2.35261557665354,73.3231650192727));
#173977=CARTESIAN_POINT('Ctrl Pts',(-7.8433350493158,2.12174052765041,73.3325630477441));
#173978=CARTESIAN_POINT('Ctrl Pts',(-7.90587910368191,1.8905369627738,73.3419744488235));
#173979=CARTESIAN_POINT('Ctrl Pts',(-7.95817769973159,1.65663422688744,
73.3513858499029));
#173980=CARTESIAN_POINT('Ctrl Pts',(-8.00005229852206,1.42086268985145,
73.3607972509823));
#173981=CARTESIAN_POINT('Ctrl Pts',(-8.04186384803645,1.18544614665803,
73.3701944816089));
#173982=CARTESIAN_POINT('Ctrl Pts',(-8.07328276631883,0.948166462592412,
73.3795917122355));
#173983=CARTESIAN_POINT('Ctrl Pts',(-8.09418224276287,0.709860115404616,
73.3889889428621));
#173984=CARTESIAN_POINT('Ctrl Pts',(-8.11502900293129,0.472154865718613,
73.3983624701677));
#173985=CARTESIAN_POINT('Ctrl Pts',(-8.12540929805967,0.233428161608197,
73.4077359974733));
#173986=CARTESIAN_POINT('Ctrl Pts',(-8.12524815165165,-0.00548056397160565,
73.4171095247788));
#173987=CARTESIAN_POINT('Ctrl Pts',(-8.12508805171894,-0.242837830319122,
73.4264221809486));
#173988=CARTESIAN_POINT('Ctrl Pts',(-8.11452295540435,-0.480374717166226,
73.4357348371184));
#173989=CARTESIAN_POINT('Ctrl Pts',(-8.09352990955081,-0.717259482827784,
73.4450474932882));
#173990=CARTESIAN_POINT('Ctrl Pts',(-8.08001273048008,-0.869786839692345,
73.451043804731));
#173991=CARTESIAN_POINT('Ctrl Pts',(-8.06217322375856,-1.02204366016996,
73.4570401161738));
#173992=CARTESIAN_POINT('Ctrl Pts',(-8.04001658451643,-1.17380615230997,
73.4630364276166));
#173993=CARTESIAN_POINT('Ctrl Pts',(-8.0120537486039,-1.36533834358738,
73.4706040858306));
#173994=CARTESIAN_POINT('Ctrl Pts',(-7.97722263444777,-1.5560067236132,
73.4781717440446));
#173995=CARTESIAN_POINT('Ctrl Pts',(-7.93559986926388,-1.74526281042113,
73.4857394022586));
#173996=CARTESIAN_POINT('Ctrl Pts',(-7.89398862867558,-1.9344664956201,
73.4933049651241));
#173997=CARTESIAN_POINT('Ctrl Pts',(-7.84558955766252,-2.12225830696251,
73.5008705279896));
#173998=CARTESIAN_POINT('Ctrl Pts',(-7.79053056235515,-2.30809902723222,
73.5084360908551));
#173999=CARTESIAN_POINT('Ctrl Pts',(-7.73547639073627,-2.493923466098,73.5160009909057));
#174000=CARTESIAN_POINT('Ctrl Pts',(-7.67376356141738,-2.67779680184264,
73.5235658909563));
#174001=CARTESIAN_POINT('Ctrl Pts',(-7.60557009024882,-2.85919414605103,
73.531130791007));
#174002=CARTESIAN_POINT('Ctrl Pts',(-7.53734315014629,-3.04068051895429,
73.5386994038638));
#174003=CARTESIAN_POINT('Ctrl Pts',(-7.46262934039782,-3.21968812679239,
73.5462680167206));
#174004=CARTESIAN_POINT('Ctrl Pts',(-7.38165537816871,-3.39571074157575,
73.5538366295774));
#174005=CARTESIAN_POINT('Ctrl Pts',(-7.30066340875383,-3.57177250069438,
73.5614069255607));
#174006=CARTESIAN_POINT('Ctrl Pts',(-7.21340867773382,-3.74484761523026,
73.568977221544));
#174007=CARTESIAN_POINT('Ctrl Pts',(-7.12016416680368,-3.91445395940033,
73.5765475175272));
#174008=CARTESIAN_POINT('Ctrl Pts',(-7.02682517260175,-4.08423216314854,
73.5841254843785));
#174009=CARTESIAN_POINT('Ctrl Pts',(-6.92748445960888,-4.25053425745538,
73.5917034512297));
#174010=CARTESIAN_POINT('Ctrl Pts',(-6.8224591849423,-4.41290587167871,
73.5992814180809));
#174011=CARTESIAN_POINT('Ctrl Pts',(-6.71887262392489,-4.57305319981126,
73.6067555763549));
#174012=CARTESIAN_POINT('Ctrl Pts',(-6.60975649933532,-4.72937680833569,
73.6142297346289));
#174013=CARTESIAN_POINT('Ctrl Pts',(-6.49545316497986,-4.88147270237713,
73.6217038929028));
#174014=CARTESIAN_POINT('Ctrl Pts',(-6.37196364870327,-5.0457920416925,
73.6297787246217));
#174015=CARTESIAN_POINT('Ctrl Pts',(-6.24215632176443,-5.20552794152128,
73.6378535563406));
#174016=CARTESIAN_POINT('Ctrl Pts',(-6.10639835220765,-5.36018532577519,
73.6459283880594));
#174017=CARTESIAN_POINT('Ctrl Pts',(-5.97073019990481,-5.51474038895284,
73.6539978774826));
#174018=CARTESIAN_POINT('Ctrl Pts',(-5.82911946395495,-5.66422339926768,
73.6620673669059));
#174019=CARTESIAN_POINT('Ctrl Pts',(-5.68197406005973,-5.80817168679683,
73.6701368563291));
#174020=CARTESIAN_POINT('Ctrl Pts',(-5.53490596154673,-5.95204434860411,
73.6782021063065));
#174021=CARTESIAN_POINT('Ctrl Pts',(-5.38230921987001,-6.09038786546068,
73.6862673562839));
#174022=CARTESIAN_POINT('Ctrl Pts',(-5.22462956665833,-6.22277538190955,
73.6943326062613));
#174023=CARTESIAN_POINT('Ctrl Pts',(-5.06701129485761,-6.3551113626505,
73.7023947166046));
#174024=CARTESIAN_POINT('Ctrl Pts',(-4.90431430020517,-6.48149576387487,
73.7104568269478));
#174025=CARTESIAN_POINT('Ctrl Pts',(-4.73701891142311,-6.60154068345563,
73.7185189372911));
#174026=CARTESIAN_POINT('Ctrl Pts',(-4.56976589835752,-6.72155519580572,
73.7265790055118));
#174027=CARTESIAN_POINT('Ctrl Pts',(-4.39791707172538,-6.83523324513132,
73.7346390737324));
#174028=CARTESIAN_POINT('Ctrl Pts',(-4.2219838762333,-6.94222872796093,
73.742699141953));
#174029=CARTESIAN_POINT('Ctrl Pts',(-4.04341493908372,-7.05082716269777,
73.7508799620165));
#174030=CARTESIAN_POINT('Ctrl Pts',(-3.86063854733434,-7.15254100888551,
73.7590607820799));
#174031=CARTESIAN_POINT('Ctrl Pts',(-3.67421852464841,-7.24705497396221,
73.7672416021434));
#174032=CARTESIAN_POINT('Ctrl Pts',(-3.49053229771513,-7.34018291905796,
73.7753024528451));
#174033=CARTESIAN_POINT('Ctrl Pts',(-3.30330887018905,-7.4263205744407,
73.7833633035468));
#174034=CARTESIAN_POINT('Ctrl Pts',(-3.11311121644029,-7.50521326256447,
73.7914241542485));
#174035=CARTESIAN_POINT('Ctrl Pts',(-2.92288202013944,-7.58411903432348,
73.799486341769));
#174036=CARTESIAN_POINT('Ctrl Pts',(-2.72967790653201,-7.65577732090503,
73.8075485292895));
#174037=CARTESIAN_POINT('Ctrl Pts',(-2.5340811935733,-7.71998186959517,
73.81561071681));
#174038=CARTESIAN_POINT('Ctrl Pts',(-2.33842781173114,-7.78420501982534,
73.8236752401323));
#174039=CARTESIAN_POINT('Ctrl Pts',(-2.14038074897869,-7.84097002617608,
73.8317397634547));
#174040=CARTESIAN_POINT('Ctrl Pts',(-1.94053739483727,-7.89012054291556,
73.8398042867771));
#174041=CARTESIAN_POINT('Ctrl Pts',(-1.7356134967979,-7.94052059511733,
73.848073831502));
#174042=CARTESIAN_POINT('Ctrl Pts',(-1.52880110969277,-7.98291378675044,
73.8563433762269));
#174043=CARTESIAN_POINT('Ctrl Pts',(-1.32075515694156,-8.01718737325705,
73.8646129209518));
#174044=CARTESIAN_POINT('Ctrl Pts',(-1.11759301424641,-8.05065639863557,
73.8726883408444));
#174045=CARTESIAN_POINT('Ctrl Pts',(-0.91325489095522,-8.07638274216671,
73.880763760737));
#174046=CARTESIAN_POINT('Ctrl Pts',(-0.708355890209745,-8.09431402252872,
73.8888391806297));
#174047=CARTESIAN_POINT('Ctrl Pts',(-0.496068545944349,-8.11289187734247,
73.8972057877707));
#174048=CARTESIAN_POINT('Ctrl Pts',(-0.283179502971089,-8.12310204624144,
73.9055723949118));
#174049=CARTESIAN_POINT('Ctrl Pts',(-0.0703731950607855,-8.12494524141037,
73.9139390020528));
#174050=CARTESIAN_POINT('Ctrl Pts',(0.142433112849518,-8.12678843657929,
73.9223056091939));
#174051=CARTESIAN_POINT('Ctrl Pts',(0.355156311837234,-8.12026470677724,
73.9306722163349));
#174052=CARTESIAN_POINT('Ctrl Pts',(0.567117184088067,-8.10543432901729,
73.939038823476));
#174053=CARTESIAN_POINT('Ctrl Pts',(0.771765138676577,-8.09111561801125,
73.947116772109));
#174054=CARTESIAN_POINT('Ctrl Pts',(0.976100380386021,-8.06902602697114,
73.9551947207421));
#174055=CARTESIAN_POINT('Ctrl Pts',(1.17950822345358,-8.03918204255292,
73.9632726693752));
#174056=CARTESIAN_POINT('Ctrl Pts',(1.38266713663346,-8.00937458111031,
73.9713407322397));
#174057=CARTESIAN_POINT('Ctrl Pts',(1.5849006036307,-7.97183168814913,73.9794087951043));
#174058=CARTESIAN_POINT('Ctrl Pts',(1.78559660822796,-7.92662174669542,
73.9874768579689));
#174059=CARTESIAN_POINT('Ctrl Pts',(1.98607170989304,-7.88146156711242,
73.9955360404437));
#174060=CARTESIAN_POINT('Ctrl Pts',(2.18501241658971,-7.82865123142644,
74.0035952229185));
#174061=CARTESIAN_POINT('Ctrl Pts',(2.38181387656983,-7.76831064130931,
74.0116544053933));
#174062=CARTESIAN_POINT('Ctrl Pts',(2.57836255195641,-7.70804755657017,
74.01970323613));
#174063=CARTESIAN_POINT('Ctrl Pts',(2.77277716191924,-7.64027360548962,
74.0277520668668));
#174064=CARTESIAN_POINT('Ctrl Pts',(2.96446500835067,-7.56515926975529,
74.0358008976035));
#174065=CARTESIAN_POINT('Ctrl Pts',(3.15600786296069,-7.49010175016531,
74.043843640241));
#174066=CARTESIAN_POINT('Ctrl Pts',(3.34482777245157,-7.40771502761441,
74.0518863828785));
#174067=CARTESIAN_POINT('Ctrl Pts',(3.53034781734139,-7.31821917211373,
74.059929125516));
#174068=CARTESIAN_POINT('Ctrl Pts',(3.71571674917015,-7.2287962143567,74.0679653170369));
#174069=CARTESIAN_POINT('Ctrl Pts',(3.89779089454204,-7.13227581143776,
74.0760015085577));
#174070=CARTESIAN_POINT('Ctrl Pts',(4.076013660801,-7.02892596343592,74.0840377000786));
#174071=CARTESIAN_POINT('Ctrl Pts',(4.1770587756715,-6.97033077112463,74.0885938963064));
#174072=CARTESIAN_POINT('Ctrl Pts',(4.27686625954618,-6.90954117291963,
74.0931500925343));
#174073=CARTESIAN_POINT('Ctrl Pts',(4.37533792322839,-6.84661271141135,
74.0977062887621));
#174074=CARTESIAN_POINT('Ctrl Pts',(4.54902863238394,-6.73561540826113,
74.1057428032707));
#174075=CARTESIAN_POINT('Ctrl Pts',(4.71842442093203,-6.61804890458617,
74.1137793177793));
#174076=CARTESIAN_POINT('Ctrl Pts',(4.88302931101169,-6.49428304821253,
74.1218158322879));
#174077=CARTESIAN_POINT('Ctrl Pts',(5.04773363882793,-6.37044242494334,
74.1298572016511));
#174078=CARTESIAN_POINT('Ctrl Pts',(5.20764104170037,-6.24039516724635,
74.1378985710143));
#174079=CARTESIAN_POINT('Ctrl Pts',(5.36228881921625,-6.10455126784994,
74.1459399403775));
#174080=CARTESIAN_POINT('Ctrl Pts',(5.51704892798421,-5.96860869574351,
74.153987150737));
#174081=CARTESIAN_POINT('Ctrl Pts',(5.66654155224571,-5.82686128979284,
74.1620343610965));
#174082=CARTESIAN_POINT('Ctrl Pts',(5.81034059418364,-5.67975613403266,
74.170081571456));
#174083=CARTESIAN_POINT('Ctrl Pts',(5.95435158564125,-5.53243415577711,
74.1781406428289));
#174084=CARTESIAN_POINT('Ctrl Pts',(6.09265200113154,-5.37973887051835,
74.1861997142018));
#174085=CARTESIAN_POINT('Ctrl Pts',(6.22485467574036,-5.2221520303811,74.1942587855747));
#174086=CARTESIAN_POINT('Ctrl Pts',(6.35716434845941,-5.06443764748314,
74.2023243795494));
#174087=CARTESIAN_POINT('Ctrl Pts',(6.48336623842568,-4.90182405822823,
74.2103899735242));
#174088=CARTESIAN_POINT('Ctrl Pts',(6.60311583106907,-4.7348230045045,74.2184555674989));
#174089=CARTESIAN_POINT('Ctrl Pts',(6.72305345793257,-4.56755972097103,
74.226533826299));
#174090=CARTESIAN_POINT('Ctrl Pts',(6.83651836201009,-4.39589546553531,
74.2346120850991));
#174091=CARTESIAN_POINT('Ctrl Pts',(6.94321048164746,-4.22036915092043,
74.2426903438991));
#174092=CARTESIAN_POINT('Ctrl Pts',(7.0034508572392,-4.12126369538565,74.2472514806157));
#174093=CARTESIAN_POINT('Ctrl Pts',(7.06153295399646,-4.02092746171593,
74.2518126173322));
#174094=CARTESIAN_POINT('Ctrl Pts',(7.11740948051487,-3.91946040280763,
74.2563737540487));
#174095=CARTESIAN_POINT('Ctrl Pts',(7.22059852415721,-3.73207780366742,
74.2647969572259));
#174096=CARTESIAN_POINT('Ctrl Pts',(7.31644555401899,-3.54050601147677,
74.2732201604031));
#174097=CARTESIAN_POINT('Ctrl Pts',(7.40462551799961,-3.3453263668421,74.2816433635803));
#174098=CARTESIAN_POINT('Ctrl Pts',(7.4927044203584,-3.15037041442214,74.2900569130614));
#174099=CARTESIAN_POINT('Ctrl Pts',(7.57313368175876,-2.95181510309204,
74.2984704625426));
#174100=CARTESIAN_POINT('Ctrl Pts',(7.64563451223645,-2.75026552678081,
74.3068840120237));
#174101=CARTESIAN_POINT('Ctrl Pts',(7.71805116954088,-2.54894994871891,
74.3152877934076));
#174102=CARTESIAN_POINT('Ctrl Pts',(7.78255767350349,-2.34464729292043,
74.3236915747915));
#174103=CARTESIAN_POINT('Ctrl Pts',(7.8389232237723,-2.13798275350932,74.3320953561754));
#174104=CARTESIAN_POINT('Ctrl Pts',(7.89519516524345,-1.93166143116894,
74.3404851810226));
#174105=CARTESIAN_POINT('Ctrl Pts',(7.94335307174294,-1.7229863121671,74.3488750058699));
#174106=CARTESIAN_POINT('Ctrl Pts',(7.9832158263263,-1.51259797460968,74.3572648307171));
#174107=CARTESIAN_POINT('Ctrl Pts',(8.02303601866255,-1.30243427281829,
74.3656456975833));
#174108=CARTESIAN_POINT('Ctrl Pts',(8.05457867863643,-1.09056126298045,
74.3740265644495));
#174109=CARTESIAN_POINT('Ctrl Pts',(8.07771312413821,-0.877632181853677,
74.3824074313157));
#174110=CARTESIAN_POINT('Ctrl Pts',(8.10081321161226,-0.66501933148655,
74.3907758513716));
#174111=CARTESIAN_POINT('Ctrl Pts',(8.11552997917101,-0.45135380484218,
74.3991442714274));
#174112=CARTESIAN_POINT('Ctrl Pts',(8.12178415220492,-0.237296749857492,
74.4075126914832));
#174113=CARTESIAN_POINT('Ctrl Pts',(8.12407351337415,-0.158940441673543,
74.410575979918));
#174114=CARTESIAN_POINT('Ctrl Pts',(8.12522942505247,-0.0805317558266113,
74.4136392683528));
#174115=CARTESIAN_POINT('Ctrl Pts',(8.12524972775009,-0.00210337752670956,
74.4167025567875));
#174116=CARTESIAN_POINT('',(8.12524985409108,0.00153983533466129,68.4161556904274));
#174117=CARTESIAN_POINT('Ctrl Pts',(8.12524912703364,-0.00376644912560897,
72.4136256277805));
#174118=CARTESIAN_POINT('Ctrl Pts',(8.12504495497945,-0.444220773542676,
72.3949776375295));
#174119=CARTESIAN_POINT('Ctrl Pts',(8.08902685308007,-0.883951672119959,
72.3762872520971));
#174120=CARTESIAN_POINT('Ctrl Pts',(8.01504119253789,-1.33380636191999,
72.3581502401893));
#174121=CARTESIAN_POINT('Ctrl Pts',(8.01249875253361,-1.34899535716882,
72.3575391098091));
#174122=CARTESIAN_POINT('Ctrl Pts',(8.00830498159974,-1.37361953614454,
72.3565504825373));
#174123=CARTESIAN_POINT('Ctrl Pts',(8.00668012898813,-1.38305915325922,
72.3561720026502));
#174124=CARTESIAN_POINT('Ctrl Pts',(8.00380322905308,-1.39959758255951,
72.3555098130235));
#174125=CARTESIAN_POINT('Ctrl Pts',(8.00255842169075,-1.4066976328787,72.355225826995));
#174126=CARTESIAN_POINT('Ctrl Pts',(8.0000346105114,-1.42098100930207,72.3546551326423));
#174127=CARTESIAN_POINT('Ctrl Pts',(7.99875537571469,-1.42816428960903,
72.3543684335725));
#174128=CARTESIAN_POINT('Ctrl Pts',(7.99627075941841,-1.44200808584983,
72.3538165102144));
#174129=CARTESIAN_POINT('Ctrl Pts',(7.99506672788509,-1.44866883537331,
72.3535512324763));
#174130=CARTESIAN_POINT('Ctrl Pts',(7.99220071414338,-1.46441133131637,
72.3529249126987));
#174131=CARTESIAN_POINT('Ctrl Pts',(7.99053157101026,-1.47349177671526,
72.352564161535));
#174132=CARTESIAN_POINT('Ctrl Pts',(7.9855296022346,-1.50044495913771,72.3514949314562));
#174133=CARTESIAN_POINT('Ctrl Pts',(7.98215224871541,-1.51830945103964,
72.3507883069983));
#174134=CARTESIAN_POINT('Ctrl Pts',(7.93918496767691,-1.74147833821821,
72.3419879767086));
#174135=CARTESIAN_POINT('Ctrl Pts',(7.89174591770249,-1.94518638619677,
72.3342784455922));
#174136=CARTESIAN_POINT('Ctrl Pts',(7.80616930297352,-2.25756236921412,
72.3227389680835));
#174137=CARTESIAN_POINT('Ctrl Pts',(7.77349272313415,-2.36763151194455,
72.3187263148649));
#174138=CARTESIAN_POINT('Ctrl Pts',(7.72019059084956,-2.53415661578989,
72.3126962252828));
#174139=CARTESIAN_POINT('Ctrl Pts',(7.7012536796923,-2.59113573193026,72.3106403080961));
#174140=CARTESIAN_POINT('Ctrl Pts',(7.65311041591386,-2.7308016777998,72.3056098318278));
#174141=CARTESIAN_POINT('Ctrl Pts',(7.62319363052296,-2.81323584978403,
72.3026484823864));
#174142=CARTESIAN_POINT('Ctrl Pts',(7.54814618143299,-3.01003130888968,
72.2955702977016));
#174143=CARTESIAN_POINT('Ctrl Pts',(7.50174295869586,-3.12388413911585,
72.2914681881237));
#174144=CARTESIAN_POINT('Ctrl Pts',(7.35398908633463,-3.46410610577125,
72.2790992305006));
#174145=CARTESIAN_POINT('Ctrl Pts',(7.24484276246993,-3.6869279749241,72.2708443731707));
#174146=CARTESIAN_POINT('Ctrl Pts',(6.94753331744447,-4.22952813186986,
72.2498282037025));
#174147=CARTESIAN_POINT('Ctrl Pts',(6.74735584827594,-4.54205792881767,
72.2368684506662));
#174148=CARTESIAN_POINT('Ctrl Pts',(6.4353746976905,-4.96276847347414,72.2175034197649));
#174149=CARTESIAN_POINT('Ctrl Pts',(6.34074444171681,-5.08311670814125,
72.2117242698427));
#174150=CARTESIAN_POINT('Ctrl Pts',(6.2280017313192,-5.21844945028411,72.2049236714721));
#174151=CARTESIAN_POINT('Ctrl Pts',(6.21315379241246,-5.23611880803534,
72.204029683142));
#174152=CARTESIAN_POINT('Ctrl Pts',(6.19054413417771,-5.26279319474105,
72.202670764606));
#174153=CARTESIAN_POINT('Ctrl Pts',(6.1828375498404,-5.27184490654455,72.2022079904825));
#174154=CARTESIAN_POINT('Ctrl Pts',(6.1689325866376,-5.28810445021449,72.2013737501251));
#174155=CARTESIAN_POINT('Ctrl Pts',(6.16274136365834,-5.29531838691089,
72.2010025650811));
#174156=CARTESIAN_POINT('Ctrl Pts',(6.15033126375604,-5.30972723873345,
72.2002590566208));
#174157=CARTESIAN_POINT('Ctrl Pts',(6.14411238660805,-5.31692213443908,
72.1998867333906));
#174158=CARTESIAN_POINT('Ctrl Pts',(6.12672227474124,-5.33697027659267,
72.1988463059439));
#174159=CARTESIAN_POINT('Ctrl Pts',(6.11552327162103,-5.34979931165965,
72.1981771052115));
#174160=CARTESIAN_POINT('Ctrl Pts',(6.07030913853198,-5.40126693413939,
72.1954785580249));
#174161=CARTESIAN_POINT('Ctrl Pts',(6.03596784940917,-5.43961667154546,
72.1934362681541));
#174162=CARTESIAN_POINT('Ctrl Pts',(5.40032434219047,-6.13602371317179,
72.1557623189628));
#174163=CARTESIAN_POINT('Ctrl Pts',(4.69519240538418,-6.69095410946617,
72.1151810558609));
#174164=CARTESIAN_POINT('Ctrl Pts',(3.749174347508,-7.21102644371547,72.0671412255708));
#174165=CARTESIAN_POINT('Ctrl Pts',(3.58089650030489,-7.29605342109991,
72.0588448934444));
#174166=CARTESIAN_POINT('Ctrl Pts',(3.27939061971709,-7.43545085977603,
72.0445708382571));
#174167=CARTESIAN_POINT('Ctrl Pts',(3.14739007965915,-7.49228078923422,
72.0385134903086));
#174168=CARTESIAN_POINT('Ctrl Pts',(2.96970122811621,-7.56325539578843,
72.030670574294));
#174169=CARTESIAN_POINT('Ctrl Pts',(2.92530236746905,-7.58053848604186,
72.0287368087081));
#174170=CARTESIAN_POINT('Ctrl Pts',(2.8498638239487,-7.60914285430796,72.025494010966));
#174171=CARTESIAN_POINT('Ctrl Pts',(2.81890448255758,-7.62066639839367,
72.0241751221225));
#174172=CARTESIAN_POINT('Ctrl Pts',(2.77666048163881,-7.63609760870184,
72.0223907379606));
#174173=CARTESIAN_POINT('Ctrl Pts',(2.76543649514764,-7.64016957359124,
72.0219180964252));
#174174=CARTESIAN_POINT('Ctrl Pts',(2.74762676266306,-7.6465864020851,72.0211703883204));
#174175=CARTESIAN_POINT('Ctrl Pts',(2.7410469220259,-7.64894752257462,72.0208946340961));
#174176=CARTESIAN_POINT('Ctrl Pts',(2.72735758045506,-7.65383989529039,
72.0203219287197));
#174177=CARTESIAN_POINT('Ctrl Pts',(2.72024758158589,-7.65636974092588,
72.0200250362779));
#174178=CARTESIAN_POINT('Ctrl Pts',(2.70395243103713,-7.66214223925022,
72.0193458634097));
#174179=CARTESIAN_POINT('Ctrl Pts',(2.69476494250921,-7.66537829134713,
72.0189638529471));
#174180=CARTESIAN_POINT('Ctrl Pts',(2.66644529609841,-7.67529593741482,
72.0177891127069));
#174181=CARTESIAN_POINT('Ctrl Pts',(2.64729386452627,-7.68192250986928,
72.0169985789499));
#174182=CARTESIAN_POINT('Ctrl Pts',(2.49536096016209,-7.73385705303818,
72.0107566485465));
#174183=CARTESIAN_POINT('Ctrl Pts',(2.36144690896471,-7.77579205445396,
72.0054332755426));
#174184=CARTESIAN_POINT('Ctrl Pts',(1.82242374767841,-7.92937587773068,
71.9845098408519));
#174185=CARTESIAN_POINT('Ctrl Pts',(1.41000022841712,-8.01299917827056,
71.9695884318297));
#174186=CARTESIAN_POINT('Ctrl Pts',(0.660770043793895,-8.10525052058009,
71.9424541737385));
#174187=CARTESIAN_POINT('Ctrl Pts',(0.326390879380124,-8.12558698148869,
71.9303412267286));
#174188=CARTESIAN_POINT('Ctrl Pts',(-0.177154645820925,-8.12507361174617,
71.9116302759429));
#174189=CARTESIAN_POINT('Ctrl Pts',(-0.345975732781222,-8.11963692453342,
71.9052812927844));
#174190=CARTESIAN_POINT('Ctrl Pts',(-0.621379669958194,-8.1021629022256,
71.8947717732055));
#174191=CARTESIAN_POINT('Ctrl Pts',(-0.728111544639003,-8.09326939223116,
71.8906616295401));
#174192=CARTESIAN_POINT('Ctrl Pts',(-0.870298233511019,-8.07858613602711,
71.8851348184977));
#174193=CARTESIAN_POINT('Ctrl Pts',(-0.905936297801803,-8.07466732308913,
71.8837452647594));
#174194=CARTESIAN_POINT('Ctrl Pts',(-0.964819651271658,-8.06779769112256,
71.8814422762498));
#174195=CARTESIAN_POINT('Ctrl Pts',(-0.98808026437187,-8.06498195476041,
71.8805306991771));
#174196=CARTESIAN_POINT('Ctrl Pts',(-1.03308054028227,-8.05933699285622,
71.8787636286209));
#174197=CARTESIAN_POINT('Ctrl Pts',(-1.05482160078324,-8.05652031304778,
71.8779083192658));
#174198=CARTESIAN_POINT('Ctrl Pts',(-1.10387830075651,-8.04996275690394,
71.875974682275));
#174199=CARTESIAN_POINT('Ctrl Pts',(-1.13118680485935,-8.0461707721552,
71.8748956731085));
#174200=CARTESIAN_POINT('Ctrl Pts',(-1.20115881839355,-8.03609138407347,
71.8721239078179));
#174201=CARTESIAN_POINT('Ctrl Pts',(-1.24379240730171,-8.02960320654094,
71.8704283579014));
#174202=CARTESIAN_POINT('Ctrl Pts',(-1.51488356943178,-7.98613644160722,
71.8596010771361));
#174203=CARTESIAN_POINT('Ctrl Pts',(-1.74171806207007,-7.93975188705933,
71.8503291373223));
#174204=CARTESIAN_POINT('Ctrl Pts',(-2.00682622234335,-7.8736322144272,
71.839190830929));
#174205=CARTESIAN_POINT('Ctrl Pts',(-2.04731575041621,-7.86320125134358,
71.8374814050575));
#174206=CARTESIAN_POINT('Ctrl Pts',(-2.30512055736173,-7.79465902595829,
71.8265437792783));
#174207=CARTESIAN_POINT('Ctrl Pts',(-2.52001868938172,-7.72785813238617,
71.817179932485));
#174208=CARTESIAN_POINT('Ctrl Pts',(-2.98688176645549,-7.56118693729032,
71.7963310852899));
#174209=CARTESIAN_POINT('Ctrl Pts',(-3.23718755319796,-7.45745428388846,
71.7848131890206));
#174210=CARTESIAN_POINT('Ctrl Pts',(-3.79231863603349,-7.1941701917563,
71.758770810249));
#174211=CARTESIAN_POINT('Ctrl Pts',(-4.09315265023061,-7.02736675993834,
71.7442911404142));
#174212=CARTESIAN_POINT('Ctrl Pts',(-4.40889168279579,-6.82512577658013,
71.7291961587856));
#174213=CARTESIAN_POINT('Ctrl Pts',(-4.43515730382158,-6.80808691605568,
71.727941394451));
#174214=CARTESIAN_POINT('Ctrl Pts',(-4.47467627769516,-6.78212466724629,
71.726055600984));
#174215=CARTESIAN_POINT('Ctrl Pts',(-4.48800273054334,-6.77331339058104,
71.7254200458083));
#174216=CARTESIAN_POINT('Ctrl Pts',(-4.51238662939472,-6.75708751666462,
71.7242579285532));
#174217=CARTESIAN_POINT('Ctrl Pts',(-4.52345199201722,-6.74968494667762,
71.7237308586995));
#174218=CARTESIAN_POINT('Ctrl Pts',(-4.54131252423564,-6.73767285786067,
71.7228806554447));
#174219=CARTESIAN_POINT('Ctrl Pts',(-4.54811896438835,-6.7330801917622,
71.7225567794492));
#174220=CARTESIAN_POINT('Ctrl Pts',(-4.56114862372824,-6.72425961708287,
71.7219370379099));
#174221=CARTESIAN_POINT('Ctrl Pts',(-4.56737295340548,-6.72003336826816,
71.7216410978728));
#174222=CARTESIAN_POINT('Ctrl Pts',(-4.58148511524971,-6.71042270729361,
71.720970397624));
#174223=CARTESIAN_POINT('Ctrl Pts',(-4.58936935065679,-6.7050330152836,
71.7205958817484));
#174224=CARTESIAN_POINT('Ctrl Pts',(-4.61316303340061,-6.68870593800675,
71.7194662626136));
#174225=CARTESIAN_POINT('Ctrl Pts',(-4.62904308682632,-6.67772569116637,
71.7187131941158));
#174226=CARTESIAN_POINT('Ctrl Pts',(-4.75764884901585,-6.58812216392219,
71.7126221985415));
#174227=CARTESIAN_POINT('Ctrl Pts',(-4.86839046867243,-6.50671585011454,
71.7074391774823));
#174228=CARTESIAN_POINT('Ctrl Pts',(-4.9914715805629,-6.41133628367439,
71.7017214669738));
#174229=CARTESIAN_POINT('Ctrl Pts',(-5.00587793636145,-6.40009434101028,
71.7010527860219));
#174230=CARTESIAN_POINT('Ctrl Pts',(-5.61092781592472,-5.92465332024203,
71.6729879854966));
#174231=CARTESIAN_POINT('Ctrl Pts',(-6.1344268456325,-5.38080118977403,
71.6492218693922));
#174232=CARTESIAN_POINT('Ctrl Pts',(-6.79573739469479,-4.46966222613106,
71.6101699234832));
#174233=CARTESIAN_POINT('Ctrl Pts',(-6.99447620919207,-4.1517704508491,
71.5967066866135));
#174234=CARTESIAN_POINT('Ctrl Pts',(-7.19870656213617,-3.76853932757851,
71.5801715980217));
#174235=CARTESIAN_POINT('Ctrl Pts',(-7.22625143129925,-3.71544814329774,
71.5778751307285));
#174236=CARTESIAN_POINT('Ctrl Pts',(-7.2610135149388,-3.64659708295576,
71.5748883933583));
#174237=CARTESIAN_POINT('Ctrl Pts',(-7.2687702309883,-3.63111096969571,
71.5742160575835));
#174238=CARTESIAN_POINT('Ctrl Pts',(-7.28120825193478,-3.6060791708597,
71.573128370759));
#174239=CARTESIAN_POINT('Ctrl Pts',(-7.28592045725938,-3.59654885744889,
71.5727140429054));
#174240=CARTESIAN_POINT('Ctrl Pts',(-7.29487211851472,-3.57835456242222,
71.5719226338914));
#174241=CARTESIAN_POINT('Ctrl Pts',(-7.29911488010529,-3.56969222288833,
71.5715456627836));
#174242=CARTESIAN_POINT('Ctrl Pts',(-7.30876951742276,-3.54989141489916,
71.570683546783));
#174243=CARTESIAN_POINT('Ctrl Pts',(-7.31417136800568,-3.53874809985087,
71.5701980726932));
#174244=CARTESIAN_POINT('Ctrl Pts',(-7.32813960641714,-3.50976482380475,
71.5689345813134));
#174245=CARTESIAN_POINT('Ctrl Pts',(-7.33666630611144,-3.49190588585062,
71.5681552619687));
#174246=CARTESIAN_POINT('Ctrl Pts',(-7.38873995946633,-3.38180632816902,
71.5633458704179));
#174247=CARTESIAN_POINT('Ctrl Pts',(-7.43061098676327,-3.28878574378801,
71.5592611610081));
#174248=CARTESIAN_POINT('Ctrl Pts',(-7.75767053619448,-2.52403856549157,
71.5254927951342));
#174249=CARTESIAN_POINT('Ctrl Pts',(-7.95288701129577,-1.81755561601874,
71.4927521215064));
#174250=CARTESIAN_POINT('Ctrl Pts',(-8.12210716901295,-0.572953641409007,
71.4361327713641));
#174251=CARTESIAN_POINT('Ctrl Pts',(-8.14217494269334,-0.04549467870958,
71.4125983856602));
#174252=CARTESIAN_POINT('Ctrl Pts',(-8.10938780181966,0.508234116331102,
71.39040356535));
#174253=CARTESIAN_POINT('Ctrl Pts',(-8.10758720757868,0.536192257884405,
71.3892892255849));
#174254=CARTESIAN_POINT('Ctrl Pts',(-8.10489076270286,0.574935099791029,
71.3877530911188));
#174255=CARTESIAN_POINT('Ctrl Pts',(-8.10411792962021,0.58572794767398,
71.3873260272872));
#174256=CARTESIAN_POINT('Ctrl Pts',(-8.102774312729,0.603980103466187,71.3866052254961));
#174257=CARTESIAN_POINT('Ctrl Pts',(-8.10221478379891,0.611440206476997,
71.3863110176697));
#174258=CARTESIAN_POINT('Ctrl Pts',(-8.10108497497928,0.626229860189176,
71.3857285289231));
#174259=CARTESIAN_POINT('Ctrl Pts',(-8.10051504896648,0.633559430173642,
71.3854402337814));
#174260=CARTESIAN_POINT('Ctrl Pts',(-8.09923367861765,0.649754167785704,
71.3848040625161));
#174261=CARTESIAN_POINT('Ctrl Pts',(-8.09851762452955,0.658618968296973,
71.3844563725896));
#174262=CARTESIAN_POINT('Ctrl Pts',(-8.0959488520343,0.689782885721233,
71.383235934421));
#174263=CARTESIAN_POINT('Ctrl Pts',(-8.09401856694579,0.712075624075153,
71.3823662473177));
#174264=CARTESIAN_POINT('Ctrl Pts',(-8.06057194931326,1.08062758120911,
71.3680395665487));
#174265=CARTESIAN_POINT('Ctrl Pts',(-8.00695192987167,1.42454425133131,
71.3553998141502));
#174266=CARTESIAN_POINT('Ctrl Pts',(-7.80412581306698,2.33651838338503,
71.321796061126));
#174267=CARTESIAN_POINT('Ctrl Pts',(-7.6151792680233,2.89356970676521,71.3010230017926));
#174268=CARTESIAN_POINT('Ctrl Pts',(-7.19727977051824,3.79244936429604,
71.2640615559556));
#174269=CARTESIAN_POINT('Ctrl Pts',(-6.99946542087125,4.14619936434816,
71.2485817615133));
#174270=CARTESIAN_POINT('Ctrl Pts',(-6.72293859285824,4.56410735578998,
71.2291846775868));
#174271=CARTESIAN_POINT('Ctrl Pts',(-6.66832016618217,4.64354231640478,
71.2254414632883));
#174272=CARTESIAN_POINT('Ctrl Pts',(-6.58496769142871,4.7602626286742,71.2198506667732));
#174273=CARTESIAN_POINT('Ctrl Pts',(-6.55730194331004,4.79830084412732,
71.2180140037653));
#174274=CARTESIAN_POINT('Ctrl Pts',(-6.50696437873559,4.86626256381853,
71.2147052452221));
#174275=CARTESIAN_POINT('Ctrl Pts',(-6.48441245812721,4.89627325893316,
71.213234441493));
#174276=CARTESIAN_POINT('Ctrl Pts',(-6.43567933738876,4.96019702038749,
71.2100802850006));
#174277=CARTESIAN_POINT('Ctrl Pts',(-6.40943625549527,4.99406146157451,
71.2083963065731));
#174278=CARTESIAN_POINT('Ctrl Pts',(-6.33786449468941,5.08492523309164,
71.203841896057));
#174279=CARTESIAN_POINT('Ctrl Pts',(-6.29203547093929,5.14152511566616,
71.2009661032967));
#174280=CARTESIAN_POINT('Ctrl Pts',(-5.99822354309752,5.49457714782154,
71.1827742683189));
#174281=CARTESIAN_POINT('Ctrl Pts',(-5.73011890938351,5.77362874985495,
71.167233074209));
#174282=CARTESIAN_POINT('Ctrl Pts',(-5.14356787094451,6.30287644120553,
71.1351914507845));
#174283=CARTESIAN_POINT('Ctrl Pts',(-4.82422803895731,6.55052431125194,
71.1187238430818));
#174284=CARTESIAN_POINT('Ctrl Pts',(-4.41676435507607,6.82049442112218,
71.0990870451804));
#174285=CARTESIAN_POINT('Ctrl Pts',(-4.34497857649999,6.86644834670042,
71.0956763271705));
#174286=CARTESIAN_POINT('Ctrl Pts',(-4.22266014119511,6.9420645203891,71.0899516161459));
#174287=CARTESIAN_POINT('Ctrl Pts',(-4.17250573162737,6.97232489772471,
71.0876284093376));
#174288=CARTESIAN_POINT('Ctrl Pts',(-4.10115155948183,7.01433035461302,
71.0843586340783));
#174289=CARTESIAN_POINT('Ctrl Pts',(-4.08021999499516,7.02652682602128,
71.0834037140385));
#174290=CARTESIAN_POINT('Ctrl Pts',(-4.04323723635568,7.04785507970407,
71.0817241538075));
#174291=CARTESIAN_POINT('Ctrl Pts',(-4.02720890193824,7.05702607594547,
71.0809987462373));
#174292=CARTESIAN_POINT('Ctrl Pts',(-3.99220257066058,7.0768976859255,71.079419695486));
#174293=CARTESIAN_POINT('Ctrl Pts',(-3.97321250001097,7.08757678311576,
71.0785664512056));
#174294=CARTESIAN_POINT('Ctrl Pts',(-3.9201492367624,7.11713671174759,71.0761911514856));
#174295=CARTESIAN_POINT('Ctrl Pts',(-3.88598279114167,7.13584912829217,
71.0746719087804));
#174296=CARTESIAN_POINT('Ctrl Pts',(-3.64083412099443,7.26783030831431,
71.0638373832864));
#174297=CARTESIAN_POINT('Ctrl Pts',(-3.42506772951328,7.37197016519568,
71.0546455920066));
#174298=CARTESIAN_POINT('Ctrl Pts',(-2.9794605640374,7.56325006901938,71.0360052580862));
#174299=CARTESIAN_POINT('Ctrl Pts',(-2.74963618815843,7.64979975102331,
71.0265651246789));
#174300=CARTESIAN_POINT('Ctrl Pts',(-2.46205102193899,7.74346442267606,
71.0148228872735));
#174301=CARTESIAN_POINT('Ctrl Pts',(-2.40766959437042,7.76054531492432,
71.0126058024549));
#174302=CARTESIAN_POINT('Ctrl Pts',(-2.31752015566504,7.78782195028811,
71.0089345345016));
#174303=CARTESIAN_POINT('Ctrl Pts',(-2.28185376234295,7.7983468630871,71.0074830912306));
#174304=CARTESIAN_POINT('Ctrl Pts',(-2.21181852071274,7.81849218666112,
71.0046346685808));
#174305=CARTESIAN_POINT('Ctrl Pts',(-2.17745603643589,7.82813173371456,
71.0032378815212));
#174306=CARTESIAN_POINT('Ctrl Pts',(-2.10163344559445,7.84886401523147,
71.0001572058916));
#174307=CARTESIAN_POINT('Ctrl Pts',(-2.06014673256705,7.85985527165133,
70.9984725190217));
#174308=CARTESIAN_POINT('Ctrl Pts',(-1.91599980027263,7.89682506429924,
70.9926215822871));
#174309=CARTESIAN_POINT('Ctrl Pts',(-1.81292075903311,7.92112488179225,
70.98844191024));
#174310=CARTESIAN_POINT('Ctrl Pts',(-1.53134751399616,7.98171861287944,
70.9770337665918));
#174311=CARTESIAN_POINT('Ctrl Pts',(-1.35206154163355,8.01403680447728,
70.9697785863781));
#174312=CARTESIAN_POINT('Ctrl Pts',(-0.972043262195311,8.06942298042583,
70.9544449962139));
#174313=CARTESIAN_POINT('Ctrl Pts',(-0.771227515012711,8.09108545248789,
70.946367644826));
#174314=CARTESIAN_POINT('Ctrl Pts',(-0.504546282224392,8.10983362781094,
70.9357374043058));
#174315=CARTESIAN_POINT('Ctrl Pts',(-0.439225760877315,8.11363354029947,
70.9331415143973));
#174316=CARTESIAN_POINT('Ctrl Pts',(-0.327234507077776,8.11879204502633,
70.9287083012134));
#174317=CARTESIAN_POINT('Ctrl Pts',(-0.28058494286654,8.12053808683788,
70.9268668374692));
#174318=CARTESIAN_POINT('Ctrl Pts',(-0.211503770181915,8.12252773124193,
70.9241489425652));
#174319=CARTESIAN_POINT('Ctrl Pts',(-0.189082215551901,8.1230806047658,
70.9232682351449));
#174320=CARTESIAN_POINT('Ctrl Pts',(-0.146857469901718,8.12394686670683,
70.9216124105504));
#174321=CARTESIAN_POINT('Ctrl Pts',(-0.127054949774831,8.12428069754005,
70.9208369716678));
#174322=CARTESIAN_POINT('Ctrl Pts',(-0.0815579850499752,8.1248812989825,
70.9190577094675));
#174323=CARTESIAN_POINT('Ctrl Pts',(-0.0558630755347635,8.12509859328326,
70.9180545622681));
#174324=CARTESIAN_POINT('Ctrl Pts',(0.0123321477511183,8.12535179092498,
70.9153961902816));
#174325=CARTESIAN_POINT('Ctrl Pts',(0.0548325363598336,8.12517613507318,
70.913743587966));
#174326=CARTESIAN_POINT('Ctrl Pts',(0.466865950002563,8.1202401666167,70.8977536317569));
#174327=CARTESIAN_POINT('Ctrl Pts',(0.835673794229557,8.09060688734209,
70.8836710363049));
#174328=CARTESIAN_POINT('Ctrl Pts',(1.36171574237481,8.01197628077325,70.8632572662452));
#174329=CARTESIAN_POINT('Ctrl Pts',(1.52149125407162,7.98317590727053,70.8570154963416));
#174330=CARTESIAN_POINT('Ctrl Pts',(1.82945705073294,7.91808168022554,70.8448565825756));
#174331=CARTESIAN_POINT('Ctrl Pts',(1.97770017857377,7.88236208344037,70.838945229761));
#174332=CARTESIAN_POINT('Ctrl Pts',(2.19036479600651,7.82474261310355,70.8303622292009));
#174333=CARTESIAN_POINT('Ctrl Pts',(2.25565485830422,7.80617166146281,70.8277130687633));
#174334=CARTESIAN_POINT('Ctrl Pts',(2.3725345149626,7.7713378843036,70.8229441925071));
#174335=CARTESIAN_POINT('Ctrl Pts',(2.42420903188614,7.75537381958172,70.8208264138433));
#174336=CARTESIAN_POINT('Ctrl Pts',(2.53919592216212,7.71858880518702,70.8160925735475));
#174337=CARTESIAN_POINT('Ctrl Pts',(2.6024192577888,7.69750238977082,70.813475199615));
#174338=CARTESIAN_POINT('Ctrl Pts',(2.82017536466298,7.62188630762233,70.8044097103626));
#174339=CARTESIAN_POINT('Ctrl Pts',(2.97331278707267,7.56346155516255,70.7979447823253));
#174340=CARTESIAN_POINT('Ctrl Pts',(3.2308281893675,7.45618434676361,70.7869312597258));
#174341=CARTESIAN_POINT('Ctrl Pts',(3.33612592249368,7.40966933736333,70.7823863691926));
#174342=CARTESIAN_POINT('Ctrl Pts',(3.47248358467956,7.34593762153586,70.77645327592));
#174343=CARTESIAN_POINT('Ctrl Pts',(3.50446886675525,7.33073255225362,70.7750580945332));
#174344=CARTESIAN_POINT('Ctrl Pts',(3.58421397240402,7.29218236606534,70.7715714814167));
#174345=CARTESIAN_POINT('Ctrl Pts',(3.63184610210123,7.26857670913078,70.769481520171));
#174346=CARTESIAN_POINT('Ctrl Pts',(3.7149371627918,7.2263775233482,70.7658240679228));
#174347=CARTESIAN_POINT('Ctrl Pts',(3.75049656320541,7.20798624934944,70.7642552031043));
#174348=CARTESIAN_POINT('Ctrl Pts',(3.83724584712964,7.16230388280299,70.7604178434199));
#174349=CARTESIAN_POINT('Ctrl Pts',(3.88828215720208,7.13472595809677,70.758151477773));
#174350=CARTESIAN_POINT('Ctrl Pts',(4.10309942568018,7.01565793411155,70.7485664893735));
#174351=CARTESIAN_POINT('Ctrl Pts',(4.26398133561234,6.91905662459237,70.7412735337428));
#174352=CARTESIAN_POINT('Ctrl Pts',(4.4726076200251,6.78374509481955,70.7315871315129));
#174353=CARTESIAN_POINT('Ctrl Pts',(4.52346361755219,6.7499402455907,70.7292073185378));
#174354=CARTESIAN_POINT('Ctrl Pts',(4.64547241950542,6.66684073964602,70.7234488329007));
#174355=CARTESIAN_POINT('Ctrl Pts',(4.71622785884208,6.61697620967572,70.7200682410466));
#174356=CARTESIAN_POINT('Ctrl Pts',(4.83167108467573,6.53282573646637,70.714477652273));
#174357=CARTESIAN_POINT('Ctrl Pts',(4.87682321037085,6.49918863573094,70.7122716593564));
#174358=CARTESIAN_POINT('Ctrl Pts',(4.96265734114744,6.43384639466952,70.7080389578296));
#174359=CARTESIAN_POINT('Ctrl Pts',(5.00339426095581,6.40221783162282,70.7060128543733));
#174360=CARTESIAN_POINT('Ctrl Pts',(5.11385168074785,6.31475938120592,70.7004700932477));
#174361=CARTESIAN_POINT('Ctrl Pts',(5.18295689963812,6.2581644842555,70.6969481139968));
#174362=CARTESIAN_POINT('Ctrl Pts',(5.60382537133273,5.90173366450811,70.6751454625246));
#174363=CARTESIAN_POINT('Ctrl Pts',(5.9304020742526,5.57347636726984,70.6566230950635));
#174364=CARTESIAN_POINT('Ctrl Pts',(6.30944666723935,5.12122337965189,70.6330358672515));
#174365=CARTESIAN_POINT('Ctrl Pts',(6.38927806623034,5.02127198022834,70.6279341022965));
#174366=CARTESIAN_POINT('Ctrl Pts',(6.49914869383377,4.87684560901156,70.6207317766775));
#174367=CARTESIAN_POINT('Ctrl Pts',(6.53115805922531,4.83389400885742,70.6186104661968));
#174368=CARTESIAN_POINT('Ctrl Pts',(6.58728505208385,4.75700496202787,70.6148510780976));
#174369=CARTESIAN_POINT('Ctrl Pts',(6.61157095301244,4.72319278933939,70.6132107125388));
#174370=CARTESIAN_POINT('Ctrl Pts',(6.64888530260346,4.67038992424895,70.6106695992693));
#174371=CARTESIAN_POINT('Ctrl Pts',(6.66209461606928,4.65152804389989,70.6097659103944));
#174372=CARTESIAN_POINT('Ctrl Pts',(6.6864211146216,4.6164754904999,70.6080941157472));
#174373=CARTESIAN_POINT('Ctrl Pts',(6.69756011913283,4.60030017828732,70.6073256274008));
#174374=CARTESIAN_POINT('Ctrl Pts',(6.72277274354714,4.56340242331729,70.6055794959634));
#174375=CARTESIAN_POINT('Ctrl Pts',(6.73680938663503,4.54265498684987,70.6046025975057));
#174376=CARTESIAN_POINT('Ctrl Pts',(6.78317023212566,4.4734419520957,70.6013593643055));
#174377=CARTESIAN_POINT('Ctrl Pts',(6.81506928648291,4.42469343445056,70.5991004475842));
#174378=CARTESIAN_POINT('Ctrl Pts',(6.98445761290257,4.15965419069249,70.5869398841881));
#174379=CARTESIAN_POINT('Ctrl Pts',(7.11218036556518,3.93729146884441,70.5771619352727));
#174380=CARTESIAN_POINT('Ctrl Pts',(7.3065276361628,3.55851768801626,70.5608651367569));
#174381=CARTESIAN_POINT('Ctrl Pts',(7.37913996320894,3.4053908853602,70.5543703537443));
#174382=CARTESIAN_POINT('Ctrl Pts',(7.49144532854843,3.14806761629204,70.5435453680393));
#174383=CARTESIAN_POINT('Ctrl Pts',(7.53387679306897,3.04512446454064,70.5392380281772));
#174384=CARTESIAN_POINT('Ctrl Pts',(7.59125404644554,2.89737370259024,70.5330784735375));
#174385=CARTESIAN_POINT('Ctrl Pts',(7.60794558758513,2.85325713557075,70.5312421718113));
#174386=CARTESIAN_POINT('Ctrl Pts',(7.63650474971762,2.77574114584565,70.5280199941431));
#174387=CARTESIAN_POINT('Ctrl Pts',(7.64853974192807,2.74240469417306,70.5266356631243));
#174388=CARTESIAN_POINT('Ctrl Pts',(7.67162879921967,2.67711454483264,70.5239268981184));
#174389=CARTESIAN_POINT('Ctrl Pts',(7.68270229111433,2.64516846646532,70.5226026667168));
#174390=CARTESIAN_POINT('Ctrl Pts',(7.71249874840557,2.55744256647578,70.5189691693249));
#174391=CARTESIAN_POINT('Ctrl Pts',(7.73081568700851,2.50152717171804,70.5166564341745));
#174392=CARTESIAN_POINT('Ctrl Pts',(7.84458082561739,2.14105224307255,70.5017657142116));
#174393=CARTESIAN_POINT('Ctrl Pts',(7.92262001831429,1.83129459579061,70.4890400931874));
#174394=CARTESIAN_POINT('Ctrl Pts',(8.0040754175095,1.40290158378793,70.4716500691821));
#174395=CARTESIAN_POINT('Ctrl Pts',(8.02343272710258,1.28758828974776,70.4669914170889));
#174396=CARTESIAN_POINT('Ctrl Pts',(8.05037215628687,1.10275897164459,70.4595774573658));
#174397=CARTESIAN_POINT('Ctrl Pts',(8.05955711576899,1.03349329748628,70.4568109495476));
#174398=CARTESIAN_POINT('Ctrl Pts',(8.07103589346378,0.937437546265412,
70.4529949806364));
#174399=CARTESIAN_POINT('Ctrl Pts',(8.07409182279171,0.910741890424098,
70.4519366489683));
#174400=CARTESIAN_POINT('Ctrl Pts',(8.07908818077056,0.865092318483335,
70.4501309695083));
#174401=CARTESIAN_POINT('Ctrl Pts',(8.08109446385744,0.846145862850543,
70.4493827341964));
#174402=CARTESIAN_POINT('Ctrl Pts',(8.08481742108188,0.809766434194584,
70.4479484614929));
#174403=CARTESIAN_POINT('Ctrl Pts',(8.08654438991563,0.792334678125103,
70.4472622914036));
#174404=CARTESIAN_POINT('Ctrl Pts',(8.091296918529,0.742728790426684,70.445312704527));
#174405=CARTESIAN_POINT('Ctrl Pts',(8.09418692589185,0.710541978090115,
70.4440513329304));
#174406=CARTESIAN_POINT('Ctrl Pts',(8.1062462310358,0.56659794473718,70.4384249761508));
#174407=CARTESIAN_POINT('Ctrl Pts',(8.11329359178476,0.454674335631456,
70.4340896728578));
#174408=CARTESIAN_POINT('Ctrl Pts',(8.12284981053059,0.228262825703277,
70.4253719529228));
#174409=CARTESIAN_POINT('Ctrl Pts',(8.12525961307041,0.113795876175322,
70.4209914133454));
#174410=CARTESIAN_POINT('Ctrl Pts',(8.12521102066953,-0.463152093049132,
70.3989788627655));
#174411=CARTESIAN_POINT('Ctrl Pts',(8.08568865400911,-0.924772150512832,
70.381553585682));
#174412=CARTESIAN_POINT('Ctrl Pts',(8.00536840918922,-1.3906364203307,70.3634517871324));
#174413=CARTESIAN_POINT('Ctrl Pts',(8.00360443098289,-1.40075305909931,
70.3630584547249));
#174414=CARTESIAN_POINT('Ctrl Pts',(7.96184204267193,-1.63761119523076,
70.3538438034098));
#174415=CARTESIAN_POINT('Ctrl Pts',(7.91224357439764,-1.86255160519841,
70.3449689048758));
#174416=CARTESIAN_POINT('Ctrl Pts',(7.83600451309022,-2.14969542717593,
70.3334186531768));
#174417=CARTESIAN_POINT('Ctrl Pts',(7.81805157208324,-2.21409726839991,
70.3308136797705));
#174418=CARTESIAN_POINT('Ctrl Pts',(7.7877663440834,-2.31777407627084,70.326595535779));
#174419=CARTESIAN_POINT('Ctrl Pts',(7.77592678248519,-2.35718984345461,
70.3249861104559));
#174420=CARTESIAN_POINT('Ctrl Pts',(7.7526120905287,-2.4327205276596,70.3218906733692));
#174421=CARTESIAN_POINT('Ctrl Pts',(7.74118275997524,-2.4688484882497,70.3204050305507));
#174422=CARTESIAN_POINT('Ctrl Pts',(7.71405078766447,-2.55257120005117,
70.3169503174575));
#174423=CARTESIAN_POINT('Ctrl Pts',(7.69815968671359,-2.6001032095624,70.3149799882836));
#174424=CARTESIAN_POINT('Ctrl Pts',(7.64463098599666,-2.75541980893398,
70.3085117226566));
#174425=CARTESIAN_POINT('Ctrl Pts',(7.60516155662379,-2.86255806788374,
70.3040021721219));
#174426=CARTESIAN_POINT('Ctrl Pts',(7.33791659911186,-3.54339676207545,
70.2750337620794));
#174427=CARTESIAN_POINT('Ctrl Pts',(7.0476618457027,-4.09036631971679,70.2503042843223));
#174428=CARTESIAN_POINT('Ctrl Pts',(6.45944268322675,-4.94705537190274,
70.206885575961));
#174429=CARTESIAN_POINT('Ctrl Pts',(6.19385657087972,-5.27578274585069,
70.1888842928901));
#174430=CARTESIAN_POINT('Ctrl Pts',(5.71598413270993,-5.78118165530637,
70.159648903071));
#174431=CARTESIAN_POINT('Ctrl Pts',(5.5180912241296,-5.97036155979792,70.148294836524));
#174432=CARTESIAN_POINT('Ctrl Pts',(5.29418462112617,-6.16374820610839,
70.1365249303017));
#174433=CARTESIAN_POINT('Ctrl Pts',(5.2772838595182,-6.17822448836411,70.135642875744));
#174434=CARTESIAN_POINT('Ctrl Pts',(5.25356075435809,-6.19837605374711,
70.1344138706803));
#174435=CARTESIAN_POINT('Ctrl Pts',(5.24678834259311,-6.2041097985284,70.1340640493713));
#174436=CARTESIAN_POINT('Ctrl Pts',(5.23439196123506,-6.2145701643817,70.1334256332464));
#174437=CARTESIAN_POINT('Ctrl Pts',(5.22877095286869,-6.21930027050853,
70.1331368635155));
#174438=CARTESIAN_POINT('Ctrl Pts',(5.21740836867921,-6.2288356482483,70.1325545822708));
#174439=CARTESIAN_POINT('Ctrl Pts',(5.21166654981927,-6.23364062105183,
70.1322610860705));
#174440=CARTESIAN_POINT('Ctrl Pts',(5.19758783855358,-6.24538917438899,
70.1315432878215));
#174441=CARTESIAN_POINT('Ctrl Pts',(5.18924364966388,-6.25232401791281,
70.131119440424));
#174442=CARTESIAN_POINT('Ctrl Pts',(5.15915753836315,-6.27722682501975,
70.1295969510889));
#174443=CARTESIAN_POINT('Ctrl Pts',(5.13733581759779,-6.29509839819479,
70.1285034534015));
#174444=CARTESIAN_POINT('Ctrl Pts',(5.01894048924274,-6.39103627032841,
70.1226306930314));
#174445=CARTESIAN_POINT('Ctrl Pts',(4.92068208345349,-6.46699280498969,
70.1179797515618));
#174446=CARTESIAN_POINT('Ctrl Pts',(4.7194201191621,-6.61533048007238,70.1088355778977));
#174447=CARTESIAN_POINT('Ctrl Pts',(4.61639659419257,-6.68763095760165,
70.1043445752153));
#174448=CARTESIAN_POINT('Ctrl Pts',(4.26847310631183,-6.91992621151057,
70.0896785612089));
#174449=CARTESIAN_POINT('Ctrl Pts',(4.01661312776997,-7.06909265258483,
70.0798588002836));
#174450=CARTESIAN_POINT('Ctrl Pts',(3.51428884849086,-7.33106733635283,
70.0609437903159));
#174451=CARTESIAN_POINT('Ctrl Pts',(3.26507234615863,-7.44540631990467,
70.05185297893));
#174452=CARTESIAN_POINT('Ctrl Pts',(2.52446720160884,-7.74084221022625,
70.024827851808));
#174453=CARTESIAN_POINT('Ctrl Pts',(2.02083343283141,-7.88731448839574,
70.0063602070289));
#174454=CARTESIAN_POINT('Ctrl Pts',(1.47462488986803,-7.99038362122791,
69.9849932148308));
#174455=CARTESIAN_POINT('Ctrl Pts',(1.4425746555034,-7.99623206980877,69.9837350627376));
#174456=CARTESIAN_POINT('Ctrl Pts',(1.39801453122952,-8.00408666961057,
69.9819795696626));
#174457=CARTESIAN_POINT('Ctrl Pts',(1.38553363883102,-8.00625658957399,
69.9814871914562));
#174458=CARTESIAN_POINT('Ctrl Pts',(1.3640379922249,-8.00994203976023,69.9806379943421));
#174459=CARTESIAN_POINT('Ctrl Pts',(1.35502564541722,-8.01147156420938,
69.9802815994345));
#174460=CARTESIAN_POINT('Ctrl Pts',(1.33642812894035,-8.01459555039709,
69.9795454156831));
#174461=CARTESIAN_POINT('Ctrl Pts',(1.32684264344161,-8.01618803291472,
69.9791655676479));
#174462=CARTESIAN_POINT('Ctrl Pts',(1.30453879484438,-8.01985237673453,
69.9782807734856));
#174463=CARTESIAN_POINT('Ctrl Pts',(1.29181833000483,-8.0219111820242,69.9777754341324));
#174464=CARTESIAN_POINT('Ctrl Pts',(1.25132490882108,-8.02836622228204,
69.9761644704218));
#174465=CARTESIAN_POINT('Ctrl Pts',(1.22353414337463,-8.0326485300445,69.9750554161045));
#174466=CARTESIAN_POINT('Ctrl Pts',(0.685409441237254,-8.11271131149232,
69.9535127482153));
#174467=CARTESIAN_POINT('Ctrl Pts',(0.169091766363293,-8.13985034820149,
69.9315661332443));
#174468=CARTESIAN_POINT('Ctrl Pts',(-1.12268340649487,-8.08475128496889,
69.8743495850356));
#174469=CARTESIAN_POINT('Ctrl Pts',(-1.89037987318308,-7.94041816769533,
69.838114659094));
#174470=CARTESIAN_POINT('Ctrl Pts',(-2.66449371236685,-7.67605521527749,
69.8050954500327));
#174471=CARTESIAN_POINT('Ctrl Pts',(-2.70298427949223,-7.66258614844077,
69.8034632276906));
#174472=CARTESIAN_POINT('Ctrl Pts',(-2.75397260833487,-7.64431171505664,
69.8013119894218));
#174473=CARTESIAN_POINT('Ctrl Pts',(-2.76656178318958,-7.63976456620548,
69.800781733742));
#174474=CARTESIAN_POINT('Ctrl Pts',(-2.78613575062367,-7.63263981665349,
69.7999585949431));
#174475=CARTESIAN_POINT('Ctrl Pts',(-2.79312829918805,-7.63008370179775,
69.7996648010626));
#174476=CARTESIAN_POINT('Ctrl Pts',(-2.80715708583404,-7.62493363215728,
69.7990758875457));
#174477=CARTESIAN_POINT('Ctrl Pts',(-2.81419326522917,-7.622339540177,69.7987807740736));
#174478=CARTESIAN_POINT('Ctrl Pts',(-2.82994463495543,-7.61650755685396,
69.7981206851073));
#174479=CARTESIAN_POINT('Ctrl Pts',(-2.83865788791283,-7.6132644375987,
69.7977559250275));
#174480=CARTESIAN_POINT('Ctrl Pts',(-2.86429221961688,-7.60367307719444,
69.7966838894245));
#174481=CARTESIAN_POINT('Ctrl Pts',(-2.88119776630638,-7.59728330536158,
69.7959782891976));
#174482=CARTESIAN_POINT('Ctrl Pts',(-3.01217327325884,-7.54727857692013,
69.7905216180425));
#174483=CARTESIAN_POINT('Ctrl Pts',(-3.12527129057741,-7.50115209177839,
69.7858682579696));
#174484=CARTESIAN_POINT('Ctrl Pts',(-3.53580520945711,-7.32282020534022,
69.769070096283));
#174485=CARTESIAN_POINT('Ctrl Pts',(-3.82627140615542,-7.17532412275545,
69.7573553566899));
#174486=CARTESIAN_POINT('Ctrl Pts',(-4.31543366197447,-6.88875969781271,
69.7369939457859));
#174487=CARTESIAN_POINT('Ctrl Pts',(-4.51820916486686,-6.7574967925622,
69.7283491849793));
#174488=CARTESIAN_POINT('Ctrl Pts',(-5.08240579768239,-6.35551189765814,
69.7032436953689));
#174489=CARTESIAN_POINT('Ctrl Pts',(-5.42749546570607,-6.06346784630231,
69.6865185591514));
#174490=CARTESIAN_POINT('Ctrl Pts',(-5.78489424545429,-5.70592928269897,
69.6670641678215));
#174491=CARTESIAN_POINT('Ctrl Pts',(-5.822860475225,-5.66717974231265,69.6649687097535));
#174492=CARTESIAN_POINT('Ctrl Pts',(-5.87963071179815,-5.60806546091758,
69.6617913833632));
#174493=CARTESIAN_POINT('Ctrl Pts',(-5.89872337670598,-5.58797978144977,
69.660715121027));
#174494=CARTESIAN_POINT('Ctrl Pts',(-5.93274761434856,-5.55181724297009,
69.6587833489756));
#174495=CARTESIAN_POINT('Ctrl Pts',(-5.94771756087288,-5.53577679879834,
69.6579285559876));
#174496=CARTESIAN_POINT('Ctrl Pts',(-5.97849766303341,-5.50252663626776,
69.6561609267104));
#174497=CARTESIAN_POINT('Ctrl Pts',(-5.99429893369876,-5.48530892277588,
69.6552479285773));
#174498=CARTESIAN_POINT('Ctrl Pts',(-6.0339603650917,-5.44171616413769,
69.6529419619288));
#174499=CARTESIAN_POINT('Ctrl Pts',(-6.05772198622704,-5.41525223955118,
69.6515472082112));
#174500=CARTESIAN_POINT('Ctrl Pts',(-6.15203516966994,-5.30881567487904,
69.6459568513787));
#174501=CARTESIAN_POINT('Ctrl Pts',(-6.22118216170835,-5.22761442520881,
69.641734832547));
#174502=CARTESIAN_POINT('Ctrl Pts',(-6.80567378693081,-4.5132036145341,
69.6049020913526));
#174503=CARTESIAN_POINT('Ctrl Pts',(-7.22443060215095,-3.80703758585675,
69.5698953363403));
#174504=CARTESIAN_POINT('Ctrl Pts',(-7.62326117383189,-2.82243333133104,
69.525297386777));
#174505=CARTESIAN_POINT('Ctrl Pts',(-7.70524212631386,-2.59026915367048,
69.5151134302322));
#174506=CARTESIAN_POINT('Ctrl Pts',(-7.78318193918576,-2.33287125718537,
69.5043889143253));
#174507=CARTESIAN_POINT('Ctrl Pts',(-7.78970998082622,-2.31097984152365,
69.5034812441314));
#174508=CARTESIAN_POINT('Ctrl Pts',(-7.79874055978895,-2.28022325310348,
69.5022124692848));
#174509=CARTESIAN_POINT('Ctrl Pts',(-7.80132044441033,-2.27138101765195,
69.501848456534));
#174510=CARTESIAN_POINT('Ctrl Pts',(-7.80601993238448,-2.25517164412501,
69.5011825489026));
#174511=CARTESIAN_POINT('Ctrl Pts',(-7.80814415422935,-2.24780586272768,
69.5008804764231));
#174512=CARTESIAN_POINT('Ctrl Pts',(-7.81242352860919,-2.23288778347482,
69.5002697603115));
#174513=CARTESIAN_POINT('Ctrl Pts',(-7.81457816214596,-2.22533534376384,
69.4999611372646));
#174514=CARTESIAN_POINT('Ctrl Pts',(-7.81984873207604,-2.20675884686842,
69.4992034178064));
#174515=CARTESIAN_POINT('Ctrl Pts',(-7.82295231619448,-2.19573128160686,
69.4987548159585));
#174516=CARTESIAN_POINT('Ctrl Pts',(-7.83415378797876,-2.1556053158934,
69.4971269457086));
#174517=CARTESIAN_POINT('Ctrl Pts',(-7.84211279301498,-2.12646815769041,
69.4959533920774));
#174518=CARTESIAN_POINT('Ctrl Pts',(-7.8858527843668,-1.9627542960068,69.4894095773776));
#174519=CARTESIAN_POINT('Ctrl Pts',(-7.91833107642896,-1.82732355148469,
69.4841980488634));
#174520=CARTESIAN_POINT('Ctrl Pts',(-7.96649898976188,-1.60096170352779,
69.475755305302));
#174521=CARTESIAN_POINT('Ctrl Pts',(-7.98414908211039,-1.51047960281127,
69.4724492669952));
#174522=CARTESIAN_POINT('Ctrl Pts',(-8.08425921272116,-0.946347622755314,
69.452172700937));
#174523=CARTESIAN_POINT('Ctrl Pts',(-8.12608706776378,-0.466441020489828,
69.4363477489438));
#174524=CARTESIAN_POINT('Ctrl Pts',(-8.12420806368213,0.596718049988053,
69.4003988978025));
#174525=CARTESIAN_POINT('Ctrl Pts',(-8.06057789775269,1.17721256588351,
69.3800983281423));
#174526=CARTESIAN_POINT('Ctrl Pts',(-7.92771808349984,1.78108723886922,
69.3563595479564));
#174527=CARTESIAN_POINT('Ctrl Pts',(-7.91974216543471,1.81622403842902,
69.3549692431946));
#174528=CARTESIAN_POINT('Ctrl Pts',(-7.90852037189623,1.86418022227607,
69.3530590537562));
#174529=CARTESIAN_POINT('Ctrl Pts',(-7.90547646684718,1.87704667070063,
69.352545310608));
#174530=CARTESIAN_POINT('Ctrl Pts',(-7.90024023707496,1.89894130311322,
69.3516689434141));
#174531=CARTESIAN_POINT('Ctrl Pts',(-7.89806380339156,1.90797327890583,
69.351306803821));
#174532=CARTESIAN_POINT('Ctrl Pts',(-7.89382236281962,1.9254432035057,69.3506051359127));
#174533=CARTESIAN_POINT('Ctrl Pts',(-7.89175930468227,1.93388161532513,
69.3502656674043));
#174534=CARTESIAN_POINT('Ctrl Pts',(-7.88682861845043,1.95391004334875,
69.3494586443778));
#174535=CARTESIAN_POINT('Ctrl Pts',(-7.883948972578,1.96549706452093,69.348990723491));
#174536=CARTESIAN_POINT('Ctrl Pts',(-7.87536771486809,1.99970374695952,
69.347606274945));
#174537=CARTESIAN_POINT('Ctrl Pts',(-7.86959424239913,2.02230516219376,
69.3466875522776));
#174538=CARTESIAN_POINT('Ctrl Pts',(-7.82346079782808,2.19971431373903,
69.3394445293105));
#174539=CARTESIAN_POINT('Ctrl Pts',(-7.77863554647648,2.353318377364,69.3329834798282));
#174540=CARTESIAN_POINT('Ctrl Pts',(-7.66990437118594,2.68874786390042,
69.3184425885165));
#174541=CARTESIAN_POINT('Ctrl Pts',(-7.60400611593848,2.86982286334984,
69.3103056836526));
#174542=CARTESIAN_POINT('Ctrl Pts',(-7.29689156039784,3.62862185723587,
69.2750327645425));
#174543=CARTESIAN_POINT('Ctrl Pts',(-6.99578450431915,4.17976247284559,
69.2462802276797));
#174544=CARTESIAN_POINT('Ctrl Pts',(-6.41412665823376,5.00243139365272,
69.2014013177315));
#174545=CARTESIAN_POINT('Ctrl Pts',(-6.17207815084648,5.2981970177237,69.1848421192762));
#174546=CARTESIAN_POINT('Ctrl Pts',(-5.8936089731106,5.59335654494038,69.1686386974851));
#174547=CARTESIAN_POINT('Ctrl Pts',(-5.87705304586395,5.61074965407702,
69.1676846751924));
#174548=CARTESIAN_POINT('Ctrl Pts',(-5.85390396730234,5.63485442608403,
69.1663632241873));
#174549=CARTESIAN_POINT('Ctrl Pts',(-5.84737600522581,5.64162830360981,
69.1659919511869));
#174550=CARTESIAN_POINT('Ctrl Pts',(-5.83609923825769,5.65328927951273,
69.1653529233625));
#174551=CARTESIAN_POINT('Ctrl Pts',(-5.83135603169067,5.6581817599575,69.1650848446888));
#174552=CARTESIAN_POINT('Ctrl Pts',(-5.82154115947836,5.66828006657245,
69.1645315697771));
#174553=CARTESIAN_POINT('Ctrl Pts',(-5.81646865180371,5.67348506718894,
69.1642464222294));
#174554=CARTESIAN_POINT('Ctrl Pts',(-5.80462613185168,5.68560433653809,
69.1635825351703));
#174555=CARTESIAN_POINT('Ctrl Pts',(-5.79785072916694,5.69251333995597,
69.1632040998581));
#174556=CARTESIAN_POINT('Ctrl Pts',(-5.77643571253208,5.71427273343935,
69.1620122990789));
#174557=CARTESIAN_POINT('Ctrl Pts',(-5.76175119704321,5.72907894573721,
69.1612014146334));
#174558=CARTESIAN_POINT('Ctrl Pts',(-5.62588778504759,5.86501760559962,
69.1537554811931));
#174559=CARTESIAN_POINT('Ctrl Pts',(-5.50095799946835,5.98234988834199,
69.1473199099218));
#174560=CARTESIAN_POINT('Ctrl Pts',(-5.22708447628595,6.22372871095469,
69.1338491205783));
#174561=CARTESIAN_POINT('Ctrl Pts',(-5.07722421852103,6.34657453499534,
69.1268489394979));
#174562=CARTESIAN_POINT('Ctrl Pts',(-4.68360841064116,6.64636275139911,
69.1090720866717));
#174563=CARTESIAN_POINT('Ctrl Pts',(-4.43415025674763,6.81532372194114,
69.0983571724786));
#174564=CARTESIAN_POINT('Ctrl Pts',(-3.88156971909406,7.14638530192673,
69.0750731776475));
#174565=CARTESIAN_POINT('Ctrl Pts',(-3.57638547463713,7.30389357314996,
69.0624704409213));
#174566=CARTESIAN_POINT('Ctrl Pts',(-2.96121531300906,7.57356373851832,
69.0371963198603));
#174567=CARTESIAN_POINT('Ctrl Pts',(-2.65254292039627,7.68711056539703,
69.024596737373));
#174568=CARTESIAN_POINT('Ctrl Pts',(-2.24388602237955,7.8098841672753,69.0080829800269));
#174569=CARTESIAN_POINT('Ctrl Pts',(-2.1494116824107,7.83641144922028,69.0042732327988));
#174570=CARTESIAN_POINT('Ctrl Pts',(-2.00866858150771,7.87319377271939,
68.9986031942153));
#174571=CARTESIAN_POINT('Ctrl Pts',(-1.96275286531232,7.88476574272989,
68.9967542892249));
#174572=CARTESIAN_POINT('Ctrl Pts',(-1.88023255802318,7.90479755121464,
68.9934322564218));
#174573=CARTESIAN_POINT('Ctrl Pts',(-1.84366542552282,7.91340613034307,
68.9919604636509));
#174574=CARTESIAN_POINT('Ctrl Pts',(-1.77285825178119,7.92955801857297,
68.9891107608784));
#174575=CARTESIAN_POINT('Ctrl Pts',(-1.73862647552142,7.93713391084969,
68.9877331690328));
#174576=CARTESIAN_POINT('Ctrl Pts',(-1.65580289577095,7.9549022181951,68.9844000091245));
#174577=CARTESIAN_POINT('Ctrl Pts',(-1.6071646971683,7.96487125672831,68.9824425363852));
#174578=CARTESIAN_POINT('Ctrl Pts',(-1.40798595367946,8.00379682227947,
68.9744248176684));
#174579=CARTESIAN_POINT('Ctrl Pts',(-1.25673307356647,8.02893574027641,
68.9683320555353));
#174580=CARTESIAN_POINT('Ctrl Pts',(-0.862835584914242,8.08299957998712,
68.9524377680066));
#174581=CARTESIAN_POINT('Ctrl Pts',(-0.619437882252064,8.10528601764408,
68.942587929458));
#174582=CARTESIAN_POINT('Ctrl Pts',(-0.146004578182886,8.12718336880894,
68.9233792791811));
#174583=CARTESIAN_POINT('Ctrl Pts',(0.0837468794542702,8.12806329111535,
68.9140353986946));
#174584=CARTESIAN_POINT('Ctrl Pts',(0.50732398423374,8.11172239437114,68.8968220247214));
#174585=CARTESIAN_POINT('Ctrl Pts',(0.701093165108121,8.09727654641522,
68.8889533412629));
#174586=CARTESIAN_POINT('Ctrl Pts',(1.01819559679323,8.06216713146995,68.8761361493206));
#174587=CARTESIAN_POINT('Ctrl Pts',(1.14190034348952,8.04557800554014,68.8711513789643));
#174588=CARTESIAN_POINT('Ctrl Pts',(1.29804345678392,8.02096489941695,68.8648919268133));
#174589=CARTESIAN_POINT('Ctrl Pts',(1.33087977954765,8.01558193538709,68.8635774219933));
#174590=CARTESIAN_POINT('Ctrl Pts',(1.38110339077879,8.0070314898736,68.8615700017127));
#174591=CARTESIAN_POINT('Ctrl Pts',(1.39851482991532,8.00400875372883,68.8608746620199));
#174592=CARTESIAN_POINT('Ctrl Pts',(1.43239101391131,7.99801371967724,68.8595229167905));
#174593=CARTESIAN_POINT('Ctrl Pts',(1.44885665619311,7.99504733374806,68.8588664002883));
#174594=CARTESIAN_POINT('Ctrl Pts',(1.46536577108706,7.99202044055815,68.8582085848539));
#174595=CARTESIAN_POINT('Ctrl Pts',(1.46541849174124,7.99201077385633,68.8582064841728));
#174596=CARTESIAN_POINT('Ctrl Pts',(1.46552380950545,7.99199146202823,68.858202287742));
#174597=CARTESIAN_POINT('Ctrl Pts',(1.46557640685287,7.99198181686093,68.8582001919829));
#174598=CARTESIAN_POINT('Ctrl Pts',(1.46568147969507,7.9919625477992,68.8581960053289));
#174599=CARTESIAN_POINT('Ctrl Pts',(1.46573395515897,7.99195292391292,68.8581939144351));
#174600=CARTESIAN_POINT('Ctrl Pts',(1.46583878540066,7.99193369720672,68.8581897374651));
#174601=CARTESIAN_POINT('Ctrl Pts',(1.46589114021679,7.99192409438223,68.8581876513873));
#174602=CARTESIAN_POINT('Ctrl Pts',(1.46599573060775,7.99190490954192,68.8581834839917));
#174603=CARTESIAN_POINT('Ctrl Pts',(1.46604796609892,7.99189532754387,68.8581814026771));
#174604=CARTESIAN_POINT('Ctrl Pts',(1.4661523191496,7.99187618412347,68.8581772447557));
#174605=CARTESIAN_POINT('Ctrl Pts',(1.46620443660733,7.99186662272217,68.8581751681529));
#174606=CARTESIAN_POINT('Ctrl Pts',(1.46630855482179,7.99184752027662,68.8581710196058));
#174607=CARTESIAN_POINT('Ctrl Pts',(1.46636055549897,7.99183797924932,68.8581689476647));
#174608=CARTESIAN_POINT('Ctrl Pts',(1.46646444154669,7.99181891730299,68.8581648083854));
#174609=CARTESIAN_POINT('Ctrl Pts',(1.46651632681758,7.99180939640456,68.8581627410511));
#174610=CARTESIAN_POINT('Ctrl Pts',(1.46661998268906,7.99179037460616,68.8581586109602));
#174611=CARTESIAN_POINT('Ctrl Pts',(1.46667175352282,7.9917808736657,68.8581565481942));
#174612=CARTESIAN_POINT('Ctrl Pts',(1.46677518263982,7.99176189140107,68.8581524271552));
#174613=CARTESIAN_POINT('Ctrl Pts',(1.46682684065998,7.99175241012745,68.8581503688927));
#174614=CARTESIAN_POINT('Ctrl Pts',(1.466930044307,7.99173346717444,68.8581462568544));
#174615=CARTESIAN_POINT('Ctrl Pts',(1.46698159033408,7.99172400542382,68.8581442030626));
#174616=CARTESIAN_POINT('Ctrl Pts',(1.46708457196305,7.99170510116225,68.8581400998872));
#174617=CARTESIAN_POINT('Ctrl Pts',(1.46713600741592,7.99169565868086,68.8581380505095));
#174618=CARTESIAN_POINT('Ctrl Pts',(1.46723876914309,7.99167679273547,68.8581339561127));
#174619=CARTESIAN_POINT('Ctrl Pts',(1.46729009532673,7.99166736929029,68.8581319110971));
#174620=CARTESIAN_POINT('Ctrl Pts',(1.46739263923941,7.99164854129095,68.8581278253954));
#174621=CARTESIAN_POINT('Ctrl Pts',(1.46744385723238,7.99163913669046,68.8581257846989));
#174622=CARTESIAN_POINT('Ctrl Pts',(1.46754618581056,7.99162034619471,68.8581217075936));
#174623=CARTESIAN_POINT('Ctrl Pts',(1.46759729666251,7.99161096025259,68.8581196711743));
#174624=CARTESIAN_POINT('Ctrl Pts',(1.46769941264952,7.9915922067694,68.8581156025559));
#174625=CARTESIAN_POINT('Ctrl Pts',(1.46775041764299,7.99158283925644,68.8581135703625));
#174626=CARTESIAN_POINT('Ctrl Pts',(1.46785232332801,7.99156412237797,68.8581095101397));
#174627=CARTESIAN_POINT('Ctrl Pts',(1.46790322378515,7.99155477305758,68.8581074821196));
#174628=CARTESIAN_POINT('Ctrl Pts',(1.46800492100919,7.99153609245808,68.858103430219));
#174629=CARTESIAN_POINT('Ctrl Pts',(1.46805571791023,7.99152676115637,68.8581014063331));
#174630=CARTESIAN_POINT('Ctrl Pts',(1.46815720941942,7.99150811634365,68.858097362645));
#174631=CARTESIAN_POINT('Ctrl Pts',(1.46820790399562,7.99149880284052,68.8580953428442));
#174632=CARTESIAN_POINT('Ctrl Pts',(1.46830919178887,7.99148019345943,68.858091307289));
#174633=CARTESIAN_POINT('Ctrl Pts',(1.46835978505242,7.99147089757492,68.8580892915328));
#174634=CARTESIAN_POINT('Ctrl Pts',(1.4684608719172,7.99145232312524,68.8580852639993));
#174635=CARTESIAN_POINT('Ctrl Pts',(1.46851136525732,7.99144304461001,68.8580832522324));
#174636=CARTESIAN_POINT('Ctrl Pts',(1.46861225274046,7.99142450481927,68.8580792326588));
#174637=CARTESIAN_POINT('Ctrl Pts',(1.46866264708611,7.99141524350846,68.8580772248441));
#174638=CARTESIAN_POINT('Ctrl Pts',(1.46876333781327,7.99139673790576,68.8580732131258));
#174639=CARTESIAN_POINT('Ctrl Pts',(1.468813634279,7.9913874936003,68.8580712092189));
#174640=CARTESIAN_POINT('Ctrl Pts',(1.46891413041804,7.99136902179866,68.8580672052694));
#174641=CARTESIAN_POINT('Ctrl Pts',(1.46896433005693,7.9913597943107,68.8580652052282));
#174642=CARTESIAN_POINT('Ctrl Pts',(1.46906463404821,7.99134135587287,68.8580612089501));
#174643=CARTESIAN_POINT('Ctrl Pts',(1.46911473808841,7.99133214498226,68.8580592127256));
#174644=CARTESIAN_POINT('Ctrl Pts',(1.4692148519933,7.99131373954044,68.8580552240368));
#174645=CARTESIAN_POINT('Ctrl Pts',(1.46926486165812,7.99130454502781,68.8580532315803));
#174646=CARTESIAN_POINT('Ctrl Pts',(1.46936478718811,7.99128617227837,68.8580492504124));
#174647=CARTESIAN_POINT('Ctrl Pts',(1.46941470336609,7.99127699398584,68.8580472616885));
#174648=CARTESIAN_POINT('Ctrl Pts',(1.46951444294607,7.99125865349378,68.8580432879448));
#174649=CARTESIAN_POINT('Ctrl Pts',(1.46956426659665,7.99124949125033,68.8580413029151));
#174650=CARTESIAN_POINT('Ctrl Pts',(1.46966382280698,7.99123118255187,68.8580373364927));
#174651=CARTESIAN_POINT('Ctrl Pts',(1.46971355520909,7.99122203612762,68.8580353551063));
#174652=CARTESIAN_POINT('Ctrl Pts',(1.46981292962969,7.99120375894277,68.8580313959421));
#174653=CARTESIAN_POINT('Ctrl Pts',(1.4698625717242,7.99119462816994,68.8580294181615));
#174654=CARTESIAN_POINT('Ctrl Pts',(1.469961766682,7.99117638208116,68.8580254661628));
#174655=CARTESIAN_POINT('Ctrl Pts',(1.47001131950453,7.99116726677443,68.8580234919465));
#174656=CARTESIAN_POINT('Ctrl Pts',(1.47011033726559,7.99114905137518,68.858019547023));
#174657=CARTESIAN_POINT('Ctrl Pts',(1.47015980200424,7.99113995132111,68.8580175763238));
#174658=CARTESIAN_POINT('Ctrl Pts',(1.47025864426745,7.991121766309,68.8580136384076));
#174659=CARTESIAN_POINT('Ctrl Pts',(1.47030802186855,7.99111268133854,68.8580116711876));
#174660=CARTESIAN_POINT('Ctrl Pts',(1.47040669086932,7.99109452631231,68.8580077401897));
#174661=CARTESIAN_POINT('Ctrl Pts',(1.47045598235759,7.99108545624189,68.8580057764081));
#174662=CARTESIAN_POINT('Ctrl Pts',(1.47055448006977,7.99106733084824,68.8580018522496));
#174663=CARTESIAN_POINT('Ctrl Pts',(1.47060368638651,7.99105827550955,68.8579998918689));
#174664=CARTESIAN_POINT('Ctrl Pts',(1.47070201509097,7.99104017933849,68.8579959744589));
#174665=CARTESIAN_POINT('Ctrl Pts',(1.47075113733859,7.9910311385335,68.8579940174351));
#174666=CARTESIAN_POINT('Ctrl Pts',(1.47084929892892,7.99101307124614,68.8579901066981));
#174667=CARTESIAN_POINT('Ctrl Pts',(1.47089833816698,7.9910040447846,68.857988152989));
#174668=CARTESIAN_POINT('Ctrl Pts',(1.47099633439392,7.99098600606819,68.8579842488551));
#174669=CARTESIAN_POINT('Ctrl Pts',(1.47104529147504,7.99097699379789,68.8579822984266));
#174670=CARTESIAN_POINT('Ctrl Pts',(1.47114312476577,7.99095898321498,68.8579784007991));
#174671=CARTESIAN_POINT('Ctrl Pts',(1.47119200082598,7.99094998493142,68.857976453606));
#174672=CARTESIAN_POINT('Ctrl Pts',(1.47128967285355,7.99093200218324,68.8579725624181));
#174673=CARTESIAN_POINT('Ctrl Pts',(1.47133846886116,7.99092301771272,68.8579706184217));
#174674=CARTESIAN_POINT('Ctrl Pts',(1.47143598152897,7.99090506245792,68.8579667335976));
#174675=CARTESIAN_POINT('Ctrl Pts',(1.47148469837034,7.99089609164177,68.8579647927625));
#174676=CARTESIAN_POINT('Ctrl Pts',(1.47158205389726,7.99087816348075,68.8579609142136));
#174677=CARTESIAN_POINT('Ctrl Pts',(1.47163069262779,7.99086920612907,68.8579589764979));
#174678=CARTESIAN_POINT('Ctrl Pts',(1.47172789262735,7.99085130477353,68.8579551041598));
#174679=CARTESIAN_POINT('Ctrl Pts',(1.47177645405722,7.99084236074151,68.8579531695311));
#174680=CARTESIAN_POINT('Ctrl Pts',(1.47187350094922,7.99082448575452,68.8579493033074));
#174681=CARTESIAN_POINT('Ctrl Pts',(1.47192198622288,7.9908155548357,68.85794737172));
#174682=CARTESIAN_POINT('Ctrl Pts',(1.47201888142288,7.99079770596513,68.8579435115543));
#174683=CARTESIAN_POINT('Ctrl Pts',(1.47206729136785,7.99078878801136,68.8579415829752));
#174684=CARTESIAN_POINT('Ctrl Pts',(1.47216403713483,7.99077096484954,68.8579377287773));
#174685=CARTESIAN_POINT('Ctrl Pts',(1.47221237281052,7.99076205966986,68.8579358031644));
#174686=CARTESIAN_POINT('Ctrl Pts',(1.47230897074345,7.99074426193059,68.8579319548706));
#174687=CARTESIAN_POINT('Ctrl Pts',(1.47235723302641,7.99073536936765,68.8579300321887));
#174688=CARTESIAN_POINT('Ctrl Pts',(1.47245368517003,7.99071759668244,68.8579261897175));
#174689=CARTESIAN_POINT('Ctrl Pts',(1.47250187504069,7.99070871655967,68.8579242699277));
#174690=CARTESIAN_POINT('Ctrl Pts',(1.47259818306337,7.99069096862921,68.8579204332125));
#174691=CARTESIAN_POINT('Ctrl Pts',(1.47264630134839,7.99068210079834,68.8579185162818));
#174692=CARTESIAN_POINT('Ctrl Pts',(1.47274246731365,7.99066437725036,68.8579146852403));
#174693=CARTESIAN_POINT('Ctrl Pts',(1.4727905149483,7.99065552154298,68.8579127711314));
#174694=CARTESIAN_POINT('Ctrl Pts',(1.47288654070747,7.99063782204418,68.8579089456898));
#174695=CARTESIAN_POINT('Ctrl Pts',(1.47293451864807,7.99062897828795,68.8579070343645));
#174696=CARTESIAN_POINT('Ctrl Pts',(1.47303040614765,7.9906113024873,68.8579032144452));
#174697=CARTESIAN_POINT('Ctrl Pts',(1.47307831550587,7.99060247048116,68.8579013058593));
#174698=CARTESIAN_POINT('Ctrl Pts',(1.47317406575616,7.99058481820011,68.857897491422));
#174699=CARTESIAN_POINT('Ctrl Pts',(1.47322190703322,7.99057599785548,68.8578955855553));
#174700=CARTESIAN_POINT('Ctrl Pts',(1.47331752296717,7.99055836856085,68.8578917764831));
#174701=CARTESIAN_POINT('Ctrl Pts',(1.47336529738919,7.99054955965541,68.8578898732869));
#174702=CARTESIAN_POINT('Ctrl Pts',(1.47346078006895,7.99053195315882,68.8578860695374));
#174703=CARTESIAN_POINT('Ctrl Pts',(1.47350848845103,7.99052315554596,68.8578841689791));
#174704=CARTESIAN_POINT('Ctrl Pts',(1.47360383959436,7.990505571538,68.8578803704838));
#174705=CARTESIAN_POINT('Ctrl Pts',(1.47365148260562,7.99049678509799,68.8578784725368));
#174706=CARTESIAN_POINT('Ctrl Pts',(1.47374670470366,7.99047922312647,68.8578746791964));
#174707=CARTESIAN_POINT('Ctrl Pts',(1.47379428351258,7.99047044764739,68.857872783814));
#174708=CARTESIAN_POINT('Ctrl Pts',(1.47388937762626,7.99045290752376,68.8578689955862));
#174709=CARTESIAN_POINT('Ctrl Pts',(1.47393689298121,7.99044414287112,68.8578671027387));
#174710=CARTESIAN_POINT('Ctrl Pts',(1.47403186113397,7.99042662422917,68.8578633195427));
#174711=CARTESIAN_POINT('Ctrl Pts',(1.47407931392535,7.99041787024219,68.8578614291945));
#174712=CARTESIAN_POINT('Ctrl Pts',(1.47417415777903,7.99040037278226,68.8578576509642));
#174713=CARTESIAN_POINT('Ctrl Pts',(1.47422154883355,7.99039162931187,68.8578557630824));
#174714=CARTESIAN_POINT('Ctrl Pts',(1.4743162703113,7.99037415268596,68.857851989741));
#174715=CARTESIAN_POINT('Ctrl Pts',(1.47436360060736,7.99036541955501,68.8578501042866));
#174716=CARTESIAN_POINT('Ctrl Pts',(1.47445820106574,7.99034796351952,68.8578463357801));
#174717=CARTESIAN_POINT('Ctrl Pts',(1.47450547132981,7.9903392405973,68.857844452724));
#174718=CARTESIAN_POINT('Ctrl Pts',(1.49288185894259,7.98694802258996,68.8571124131317));
#174719=CARTESIAN_POINT('Ctrl Pts',(1.51119932016105,7.98350246306801,68.8563832422862));
#174720=CARTESIAN_POINT('Ctrl Pts',(1.55546114101503,7.97501891430162,68.8546223212223));
#174721=CARTESIAN_POINT('Ctrl Pts',(1.58139312247707,7.96991730470969,68.853591492964));
#174722=CARTESIAN_POINT('Ctrl Pts',(1.65170706747173,7.95572772528308,68.8507980196084));
#174723=CARTESIAN_POINT('Ctrl Pts',(1.69603876069255,7.94639493275195,68.849038506292));
#174724=CARTESIAN_POINT('Ctrl Pts',(1.84292256960197,7.91418750140257,68.8432101401496));
#174725=CARTESIAN_POINT('Ctrl Pts',(1.94510929488157,7.88969438350205,68.8391575098413));
#174726=CARTESIAN_POINT('Ctrl Pts',(2.36154539459447,7.78129633786341,68.8225906315874));
#174727=CARTESIAN_POINT('Ctrl Pts',(2.67109307344107,7.68054232349897,68.8101392688014));
#174728=CARTESIAN_POINT('Ctrl Pts',(3.03429394351043,7.53770375575407,68.7950031265807));
#174729=CARTESIAN_POINT('Ctrl Pts',(3.09453230953841,7.51317425415586,68.7924754702189));
#174730=CARTESIAN_POINT('Ctrl Pts',(3.19023663475632,7.47285648895061,68.7884297585868));
#174731=CARTESIAN_POINT('Ctrl Pts',(3.22589529380331,7.45753266372646,68.7869156704604));
#174732=CARTESIAN_POINT('Ctrl Pts',(3.29251281890573,7.42833747619856,68.7840740483638));
#174733=CARTESIAN_POINT('Ctrl Pts',(3.32349728312093,7.41452656095403,68.7827470659134));
#174734=CARTESIAN_POINT('Ctrl Pts',(3.3547245645171,7.40037234132297,68.7814041705394));
#174735=CARTESIAN_POINT('Ctrl Pts',(3.35505482968569,7.40022261717816,68.7813899672191));
#174736=CARTESIAN_POINT('Ctrl Pts',(3.35571081124885,7.39992517811352,68.7813617549607));
#174737=CARTESIAN_POINT('Ctrl Pts',(3.35603652789243,7.39977746380677,68.7813477460289));
#174738=CARTESIAN_POINT('Ctrl Pts',(3.35668349730532,7.39948400808205,68.7813199189465));
#174739=CARTESIAN_POINT('Ctrl Pts',(3.35700475036275,7.39933826723619,68.7813061008));
#174740=CARTESIAN_POINT('Ctrl Pts',(3.35764287582884,7.39904872277399,68.7812786517574));
#174741=CARTESIAN_POINT('Ctrl Pts',(3.3579597484739,7.3989049197308,68.7812650208671));
#174742=CARTESIAN_POINT('Ctrl Pts',(3.35858919449595,7.39861921597219,68.7812379428836));
#174743=CARTESIAN_POINT('Ctrl Pts',(3.35890176811458,7.39847731580591,68.7812244957954));
#174744=CARTESIAN_POINT('Ctrl Pts',(3.35952269566285,7.39819538364034,68.7811977820384));
#174745=CARTESIAN_POINT('Ctrl Pts',(3.35983104986385,7.39805535215586,68.7811845153729));
#174746=CARTESIAN_POINT('Ctrl Pts',(3.3604436165455,7.39777712385026,68.7811581591512));
#174747=CARTESIAN_POINT('Ctrl Pts',(3.36074782925585,7.39763892754274,68.7811450695997));
#174748=CARTESIAN_POINT('Ctrl Pts',(3.36135218925008,7.39736433677668,68.7811190643663));
#174749=CARTESIAN_POINT('Ctrl Pts',(3.36165233673397,7.3972279428258,68.7811061486899));
#174750=CARTESIAN_POINT('Ctrl Pts',(3.36224864085068,7.39695692467045,68.7810804880395));
#174751=CARTESIAN_POINT('Ctrl Pts',(3.36254479770947,7.39682230094311,68.7810677430693));
#174752=CARTESIAN_POINT('Ctrl Pts',(3.36313319352195,7.39655479180632,68.7810424207326));
#174753=CARTESIAN_POINT('Ctrl Pts',(3.36342543271977,7.39642190684766,68.7810298433688));
#174754=CARTESIAN_POINT('Ctrl Pts',(3.4060567742504,7.37703383311753,68.7791950079598));
#174755=CARTESIAN_POINT('Ctrl Pts',(3.44822964998529,7.35741552327589,68.7773695894421));
#174756=CARTESIAN_POINT('Ctrl Pts',(3.59006026043245,7.28995031233638,68.7711948094611));
#174757=CARTESIAN_POINT('Ctrl Pts',(3.68890873341837,7.24043232769752,68.7668310458188));
#174758=CARTESIAN_POINT('Ctrl Pts',(3.93610346373034,7.11022403658889,68.7557619955943));
#174759=CARTESIAN_POINT('Ctrl Pts',(4.08300137027764,7.02689799338167,68.7490374499538));
#174760=CARTESIAN_POINT('Ctrl Pts',(4.44541235920284,6.8061212850139,68.7320969216525));
#174761=CARTESIAN_POINT('Ctrl Pts',(4.65723765563184,6.662966027469,68.7218664317003));
#174762=CARTESIAN_POINT('Ctrl Pts',(4.90960813340563,6.47448618992539,68.7093850524794));
#174763=CARTESIAN_POINT('Ctrl Pts',(4.9568592080705,6.43838258485717,68.7070352090695));
#174764=CARTESIAN_POINT('Ctrl Pts',(5.02360181144587,6.38621561044771,68.7037000809295));
#174765=CARTESIAN_POINT('Ctrl Pts',(5.04342119368483,6.37057514330391,68.7027076787084));
#174766=CARTESIAN_POINT('Ctrl Pts',(5.07768947766798,6.34327217549735,68.7009884944066));
#174767=CARTESIAN_POINT('Ctrl Pts',(5.09217183743392,6.33165209915655,68.700260889157));
#174768=CARTESIAN_POINT('Ctrl Pts',(5.12295462150942,6.30677927628258,68.6987119345327));
#174769=CARTESIAN_POINT('Ctrl Pts',(5.13924374350542,6.29351274267405,68.697890837169));
#174770=CARTESIAN_POINT('Ctrl Pts',(5.1555872470373,6.28009615527412,68.6970654281444));
#174771=CARTESIAN_POINT('Ctrl Pts',(5.15569322855992,6.2800091492197,68.6970600756081));
#174772=CARTESIAN_POINT('Ctrl Pts',(5.15590553630268,6.27983484513326,68.6970493529933));
#174773=CARTESIAN_POINT('Ctrl Pts',(5.1560118634934,6.27974754627461,68.6970439828652));
#174774=CARTESIAN_POINT('Ctrl Pts',(5.15622487119661,6.27957264940916,68.6970332246297));
#174775=CARTESIAN_POINT('Ctrl Pts',(5.1563315515814,6.27948505147677,68.6970278365282));
#174776=CARTESIAN_POINT('Ctrl Pts',(5.156545272635,6.27930955065525,68.697017041993));
#174777=CARTESIAN_POINT('Ctrl Pts',(5.15665231330758,6.27922164773185,68.6970116355585));
#174778=CARTESIAN_POINT('Ctrl Pts',(5.15686676228843,6.27904553079711,68.6970008039843));
#174779=CARTESIAN_POINT('Ctrl Pts',(5.15697417051611,6.27895731682004,68.6969953788482));
#174780=CARTESIAN_POINT('Ctrl Pts',(5.15718936183999,6.27878057174157,68.6969845095039));
#174781=CARTESIAN_POINT('Ctrl Pts',(5.15729714490241,6.27869204063525,68.6969790652971));
#174782=CARTESIAN_POINT('Ctrl Pts',(5.15751309320959,6.27851465519246,68.6969681574403));
#174783=CARTESIAN_POINT('Ctrl Pts',(5.15762125846492,6.27842580081388,68.6969626937894));
#174784=CARTESIAN_POINT('Ctrl Pts',(5.15783797836242,6.27824776280772,68.6969517466792));
#174785=CARTESIAN_POINT('Ctrl Pts',(5.15794653311332,6.27815857905661,68.6969462632139));
#174786=CARTESIAN_POINT('Ctrl Pts',(5.15816403977227,6.27797987581868,68.6969352760807));
#174787=CARTESIAN_POINT('Ctrl Pts',(5.15827299159601,6.27789035636617,68.6969297724165));
#174788=CARTESIAN_POINT('Ctrl Pts',(5.15849129966275,6.27771097565327,68.6969187445172));
#174789=CARTESIAN_POINT('Ctrl Pts',(5.15860065596855,6.27762111430554,68.6969132202784));
#174790=CARTESIAN_POINT('Ctrl Pts',(5.15881978092106,6.27744104318508,68.6969021508278));
#174791=CARTESIAN_POINT('Ctrl Pts',(5.15892954942596,6.27735083349231,68.6968966056227));
#174792=CARTESIAN_POINT('Ctrl Pts',(5.18800649302797,6.25345361075834,68.6954276987711));
#174793=CARTESIAN_POINT('Ctrl Pts',(5.2168086270516,6.22944629965759,68.6939676604643));
#174794=CARTESIAN_POINT('Ctrl Pts',(5.28210558538231,6.17424916107911,68.6906447536481));
#174795=CARTESIAN_POINT('Ctrl Pts',(5.31849228133803,6.14293350142099,68.6887837565319));
#174796=CARTESIAN_POINT('Ctrl Pts',(5.43553123371574,6.04038625232833,68.6827634459872));
#174797=CARTESIAN_POINT('Ctrl Pts',(5.51504687034231,5.96787433877879,68.6786195231253));
#174798=CARTESIAN_POINT('Ctrl Pts',(5.74935971908633,5.74551625739629,68.6662059149627));
#174799=CARTESIAN_POINT('Ctrl Pts',(5.8996613873873,5.5910723565407,68.6579659858858));
#174800=CARTESIAN_POINT('Ctrl Pts',(6.14589564198877,5.31705331723577,68.6438313971806));
#174801=CARTESIAN_POINT('Ctrl Pts',(6.24490908088331,5.20040377445726,68.6379526604064));
#174802=CARTESIAN_POINT('Ctrl Pts',(6.4252530284798,4.97535421014705,68.6268252387107));
#174803=CARTESIAN_POINT('Ctrl Pts',(6.50728041476446,4.8675791932999,68.6215835161743));
#174804=CARTESIAN_POINT('Ctrl Pts',(6.63600402948093,4.68937773932993,68.6130394889167));
#174805=CARTESIAN_POINT('Ctrl Pts',(6.68436302244405,4.62018440568612,68.6097509392193));
#174806=CARTESIAN_POINT('Ctrl Pts',(6.76009305283663,4.50814949090166,68.6044699526556));
#174807=CARTESIAN_POINT('Ctrl Pts',(6.78815553460128,4.46578261135981,68.6024827005488));
#174808=CARTESIAN_POINT('Ctrl Pts',(6.84449976555352,4.37895951116253,68.5984296651954));
#174809=CARTESIAN_POINT('Ctrl Pts',(6.87275025218304,4.3344858276652,68.5963637782265));
#174810=CARTESIAN_POINT('Ctrl Pts',(6.93139591858326,4.24014718693536,68.5920027948546));
#174811=CARTESIAN_POINT('Ctrl Pts',(6.96169011666517,4.19022293451664,68.5897072406829));
#174812=CARTESIAN_POINT('Ctrl Pts',(7.00735887954088,4.11309917103806,68.5861798497595));
#174813=CARTESIAN_POINT('Ctrl Pts',(7.02311916856769,4.08613024735513,68.5849498667983));
#174814=CARTESIAN_POINT('Ctrl Pts',(7.07722596024238,3.99230514915065,68.5806828966483));
#174815=CARTESIAN_POINT('Ctrl Pts',(7.11477641183433,3.92499481180254,68.5776429897638));
#174816=CARTESIAN_POINT('Ctrl Pts',(7.24831491145606,3.67740793101818,68.5665410162272));
#174817=CARTESIAN_POINT('Ctrl Pts',(7.33845478342522,3.49406351712362,68.5584701306853));
#174818=CARTESIAN_POINT('Ctrl Pts',(7.43548303308128,3.27634617986965,68.5490947127222));
#174819=CARTESIAN_POINT('Ctrl Pts',(7.44917855609185,3.24508722105226,68.5477535867909));
#174820=CARTESIAN_POINT('Ctrl Pts',(7.47705193014619,3.18036207357472,68.5449872780222));
#174821=CARTESIAN_POINT('Ctrl Pts',(7.49120296097507,3.14688523636605,68.543562440069));
#174822=CARTESIAN_POINT('Ctrl Pts',(7.52066919614788,3.07585229118556,68.5405512278604));
#174823=CARTESIAN_POINT('Ctrl Pts',(7.53592875312049,3.03827423292664,68.5389652197135));
#174824=CARTESIAN_POINT('Ctrl Pts',(7.57487957637518,2.9402552895227,68.534844624304));
#174825=CARTESIAN_POINT('Ctrl Pts',(7.59812900545402,2.87964188948989,68.5323125717301));
#174826=CARTESIAN_POINT('Ctrl Pts',(7.68342064584085,2.64905164434503,68.5227305708916));
#174827=CARTESIAN_POINT('Ctrl Pts',(7.74050542177605,2.47729757651487,68.5156958446344));
#174828=CARTESIAN_POINT('Ctrl Pts',(7.82077818122245,2.20580046442253,68.5046598428428));
#174829=CARTESIAN_POINT('Ctrl Pts',(7.84789708810768,2.10728219182212,68.5006723989076));
#174830=CARTESIAN_POINT('Ctrl Pts',(7.88615138613055,1.95731206573724,68.4946185195247));
#174831=CARTESIAN_POINT('Ctrl Pts',(7.8986567719548,1.90622018308294,68.4925588976306));
#174832=CARTESIAN_POINT('Ctrl Pts',(7.92233418071596,1.8052482237899,68.4884926036413));
#174833=CARTESIAN_POINT('Ctrl Pts',(7.93353336705345,1.75537697194322,68.4864861717446));
#174834=CARTESIAN_POINT('Ctrl Pts',(7.95545027779596,1.65328168089871,68.4823814780289));
#174835=CARTESIAN_POINT('Ctrl Pts',(7.96612607420632,1.6010511496219,68.4802830756631));
#174836=CARTESIAN_POINT('Ctrl Pts',(7.99001105265801,1.47803762170106,68.4753431823402));
#174837=CARTESIAN_POINT('Ctrl Pts',(8.00279485494536,1.40717670504677,68.4724993422498));
#174838=CARTESIAN_POINT('Ctrl Pts',(8.0881702828961,0.895070953656037,68.451952704868));
#174839=CARTESIAN_POINT('Ctrl Pts',(8.12516511525461,0.448681294685467,
68.4340257735927));
#174840=CARTESIAN_POINT('Ctrl Pts',(8.12524985409108,0.00153983533466129,
68.4161556904274));
#174841=CARTESIAN_POINT('',(8.12524976787349,0.00315471203378172,64.4160553597947));
#174842=CARTESIAN_POINT('Ctrl Pts',(8.12524985424774,0.00153900849306533,
68.4161556573826));
#174843=CARTESIAN_POINT('Ctrl Pts',(8.12528237179811,-0.170138550527305,
68.4092945351027));
#174844=CARTESIAN_POINT('Ctrl Pts',(8.11987384283798,-0.341777092234551,
68.4024537844651));
#174845=CARTESIAN_POINT('Ctrl Pts',(8.10701627146785,-0.544971023882323,
68.3944096543118));
#174846=CARTESIAN_POINT('Ctrl Pts',(8.10481302331182,-0.576812024049769,
68.3931507326559));
#174847=CARTESIAN_POINT('Ctrl Pts',(8.10078293599201,-0.630461975753339,
68.3910326129349));
#174848=CARTESIAN_POINT('Ctrl Pts',(8.09905549502474,-0.652277986337368,
68.3901721681756));
#174849=CARTESIAN_POINT('Ctrl Pts',(8.0956879270921,-0.692729758567754,
68.3885784377277));
#174850=CARTESIAN_POINT('Ctrl Pts',(8.09407153657532,-0.711367341657171,
68.3878448295472));
#174851=CARTESIAN_POINT('Ctrl Pts',(8.09061230082685,-0.749714626254643,
68.3863369087451));
#174852=CARTESIAN_POINT('Ctrl Pts',(8.08876176397404,-0.769423519400977,
68.3855627149282));
#174853=CARTESIAN_POINT('Ctrl Pts',(8.08453844555367,-0.812703450460102,
68.3838645289267));
#174854=CARTESIAN_POINT('Ctrl Pts',(8.08213456390817,-0.836271291250548,
68.3829410391522));
#174855=CARTESIAN_POINT('Ctrl Pts',(8.07245465411354,-0.927231385424134,
68.3793808909721));
#174856=CARTESIAN_POINT('Ctrl Pts',(8.06443845589282,-0.994542450136126,
68.3767549491114));
#174857=CARTESIAN_POINT('Ctrl Pts',(8.05060544007279,-1.09949505721077,
68.3726671091484));
#174858=CARTESIAN_POINT('Ctrl Pts',(8.04536468118677,-1.1372090807838,68.3711995072183));
#174859=CARTESIAN_POINT('Ctrl Pts',(7.99945485684791,-1.45137474617261,
68.3589791156529));
#174860=CARTESIAN_POINT('Ctrl Pts',(7.94481481446527,-1.72559724645603,
68.3483363392331));
#174861=CARTESIAN_POINT('Ctrl Pts',(7.83788003959037,-2.14746140446812,
68.3316412044999));
#174862=CARTESIAN_POINT('Ctrl Pts',(7.79526973845258,-2.29732955351505,
68.3256469802612));
#174863=CARTESIAN_POINT('Ctrl Pts',(7.72685277196014,-2.51406983012027,
68.3168486942218));
#174864=CARTESIAN_POINT('Ctrl Pts',(7.70442831998608,-2.58197309237309,
68.3140735520567));
#174865=CARTESIAN_POINT('Ctrl Pts',(7.67986724905146,-2.65317567027084,
68.3111420947519));
#174866=CARTESIAN_POINT('Ctrl Pts',(7.6786213741955,-2.65677923285041,68.3109936755857));
#174867=CARTESIAN_POINT('Ctrl Pts',(7.67618647920419,-2.66380589201568,
68.3107041563119));
#174868=CARTESIAN_POINT('Ctrl Pts',(7.67499770467241,-2.66722907286134,
68.3105630583767));
#174869=CARTESIAN_POINT('Ctrl Pts',(7.67265798727234,-2.67395197894404,
68.3102858472728));
#174870=CARTESIAN_POINT('Ctrl Pts',(7.67150720478222,-2.67725175923315,
68.3101497355337));
#174871=CARTESIAN_POINT('Ctrl Pts',(7.65951940125848,-2.71155467204993,
68.3087342708662));
#174872=CARTESIAN_POINT('Ctrl Pts',(7.64849665170215,-2.74249250831835,
68.3074533000525));
#174873=CARTESIAN_POINT('Ctrl Pts',(7.62598414968093,-2.80448744221619,
68.3048774178709));
#174874=CARTESIAN_POINT('Ctrl Pts',(7.61449150591817,-2.8355428337931,68.3035825028963));
#174875=CARTESIAN_POINT('Ctrl Pts',(7.58723475371147,-2.90783515408737,
68.3005572421608));
#174876=CARTESIAN_POINT('Ctrl Pts',(7.57132378381058,-2.94901553597965,
68.2988256225012));
#174877=CARTESIAN_POINT('Ctrl Pts',(7.52070865324648,-3.0769061929997,68.2934214048425));
#174878=CARTESIAN_POINT('Ctrl Pts',(7.48484469518878,-3.16314875957572,
68.2897388545074));
#174879=CARTESIAN_POINT('Ctrl Pts',(7.3212545348328,-3.53816585473537,68.2735557268121));
#174880=CARTESIAN_POINT('Ctrl Pts',(7.17824490486902,-3.81997147494461,
68.2609332763151));
#174881=CARTESIAN_POINT('Ctrl Pts',(6.97790492517623,-4.16356246973784,
68.2450940582139));
#174882=CARTESIAN_POINT('Ctrl Pts',(6.9355373091331,-4.23376096600011,68.2418341586656));
#174883=CARTESIAN_POINT('Ctrl Pts',(6.87156676215497,-4.336215284512,68.2370471372909));
#174884=CARTESIAN_POINT('Ctrl Pts',(6.8507836059003,-4.36897662642505,68.2355119437941));
#174885=CARTESIAN_POINT('Ctrl Pts',(6.81281772358389,-4.42788675532222,
68.2327442325536));
#174886=CARTESIAN_POINT('Ctrl Pts',(6.79571709024347,-4.454087526402,68.2315106710721));
#174887=CARTESIAN_POINT('Ctrl Pts',(6.76831536793371,-4.49554596307694,
68.229555075291));
#174888=CARTESIAN_POINT('Ctrl Pts',(6.75811305171226,-4.51086847610355,
68.2288315057182));
#174889=CARTESIAN_POINT('Ctrl Pts',(6.737706362303,-4.541291963691,68.2273933424948));
#174890=CARTESIAN_POINT('Ctrl Pts',(6.72750306847714,-4.55639355102487,
68.2266787381253));
#174891=CARTESIAN_POINT('Ctrl Pts',(6.70484993590334,-4.58967978954676,
68.2251021344501));
#174892=CARTESIAN_POINT('Ctrl Pts',(6.6923767577114,-4.60784836675312,68.2242405590758));
#174893=CARTESIAN_POINT('Ctrl Pts',(6.64894834335656,-4.6705583855664,68.2212628677662));
#174894=CARTESIAN_POINT('Ctrl Pts',(6.61762098529057,-4.71484064012608,
68.2191533299401));
#174895=CARTESIAN_POINT('Ctrl Pts',(6.39191163066633,-5.02720648675815,
68.2042125084047));
#174896=CARTESIAN_POINT('Ctrl Pts',(6.18174124685891,-5.28350466912997,
68.1916299791438));
#174897=CARTESIAN_POINT('Ctrl Pts',(5.8434269320696,-5.64815868404763,68.1727365288103));
#174898=CARTESIAN_POINT('Ctrl Pts',(5.72662288744624,-5.76655226479261,
68.1664276887652));
#174899=CARTESIAN_POINT('Ctrl Pts',(5.35059155554883,-6.12500031618885,
68.1466632182802));
#174900=CARTESIAN_POINT('Ctrl Pts',(5.07929713680077,-6.35178659747735,
68.1331591686982));
#174901=CARTESIAN_POINT('Ctrl Pts',(4.72423193329506,-6.61126398044991,
68.1161094882838));
#174902=CARTESIAN_POINT('Ctrl Pts',(4.6535401965327,-6.6612117730507,68.1127443077749));
#174903=CARTESIAN_POINT('Ctrl Pts',(4.55091880344635,-6.73128873186888,
68.1078982831813));
#174904=CARTESIAN_POINT('Ctrl Pts',(4.51962563584827,-6.7523398943051,68.1064256699359));
#174905=CARTESIAN_POINT('Ctrl Pts',(4.45622553410183,-6.7943514515029,68.1034522069703));
#174906=CARTESIAN_POINT('Ctrl Pts',(4.4241145178227,-6.8153039828961,68.101951332318));
#174907=CARTESIAN_POINT('Ctrl Pts',(4.36211694310375,-6.85513477839087,
68.0990631826074));
#174908=CARTESIAN_POINT('Ctrl Pts',(4.33225310799632,-6.87404684701336,
68.0976762180631));
#174909=CARTESIAN_POINT('Ctrl Pts',(4.26116988288377,-6.91841497431566,
68.0943847644017));
#174910=CARTESIAN_POINT('Ctrl Pts',(4.21984439854455,-6.94369842078232,
68.0924789995474));
#174911=CARTESIAN_POINT('Ctrl Pts',(4.06728370560869,-7.03517198171976,
68.0854715048558));
#174912=CARTESIAN_POINT('Ctrl Pts',(3.95469796582418,-7.0990707289956,68.0803541086279));
#174913=CARTESIAN_POINT('Ctrl Pts',(3.47688779510555,-7.35535977581938,
68.0588569931837));
#174914=CARTESIAN_POINT('Ctrl Pts',(3.09881441516549,-7.52245985305122,
68.0423935515526));
#174915=CARTESIAN_POINT('Ctrl Pts',(2.21016307782089,-7.83681167644055,
68.0037393787933));
#174916=CARTESIAN_POINT('Ctrl Pts',(1.6945644242408,-7.96422242321409,67.9812694531593));
#174917=CARTESIAN_POINT('Ctrl Pts',(0.921593806983284,-8.07672619712227,
67.9482699891821));
#174918=CARTESIAN_POINT('Ctrl Pts',(0.67135801296593,-8.1013656798774,67.9377170400963));
#174919=CARTESIAN_POINT('Ctrl Pts',(0.352061973250933,-8.1179073393984,
67.9246595686243));
#174920=CARTESIAN_POINT('Ctrl Pts',(0.283702650057588,-8.12058374054772,
67.9218881940336));
#174921=CARTESIAN_POINT('Ctrl Pts',(0.187527340314437,-8.12313325342106,
67.9180299109739));
#174922=CARTESIAN_POINT('Ctrl Pts',(0.15973414087787,-8.12372730844027,
67.9169197177845));
#174923=CARTESIAN_POINT('Ctrl Pts',(0.111169665544383,-8.12451600502814,
67.9149887947233));
#174924=CARTESIAN_POINT('Ctrl Pts',(0.0903997446909679,-8.12477365261168,
67.914165850343));
#174925=CARTESIAN_POINT('Ctrl Pts',(0.0600104991025161,-8.12503408140102,
67.9129661809404));
#174926=CARTESIAN_POINT('Ctrl Pts',(0.0503918816739662,-8.12509942974085,
67.9125871155027));
#174927=CARTESIAN_POINT('Ctrl Pts',(0.0335144987093047,-8.12518412284654,
67.9119231459339));
#174928=CARTESIAN_POINT('Ctrl Pts',(0.0262557905068431,-8.1252108210004,
67.9116379592979));
#174929=CARTESIAN_POINT('Ctrl Pts',(0.0121661504554965,-8.12524376302789,
67.911085136558));
#174930=CARTESIAN_POINT('Ctrl Pts',(0.00533522940645123,-8.12525111978136,
67.9108174570436));
#174931=CARTESIAN_POINT('Ctrl Pts',(-0.0109660751142631,-8.12524811901701,
67.9101794894724));
#174932=CARTESIAN_POINT('Ctrl Pts',(-0.0204364602350505,-8.12522981844067,
67.9098095191954));
#174933=CARTESIAN_POINT('Ctrl Pts',(-0.0542969048736042,-8.12510518658287,
67.9084891472156));
#174934=CARTESIAN_POINT('Ctrl Pts',(-0.0786866475893341,-8.12490559181954,
67.9075425714146));
#174935=CARTESIAN_POINT('Ctrl Pts',(-0.512123510969814,-8.11940665590536,
67.8908050070238));
#174936=CARTESIAN_POINT('Ctrl Pts',(-0.920202038761973,-8.08333301032376,
67.8765166026161));
#174937=CARTESIAN_POINT('Ctrl Pts',(-1.67960378625187,-7.95792978515934,
67.8504518717959));
#174938=CARTESIAN_POINT('Ctrl Pts',(-2.03107546700232,-7.87556046562825,
67.8385918448277));
#174939=CARTESIAN_POINT('Ctrl Pts',(-2.93263516201177,-7.59988518097128,
67.8068520556476));
#174940=CARTESIAN_POINT('Ctrl Pts',(-3.46938307923615,-7.37033869787014,
67.7865082791149));
#174941=CARTESIAN_POINT('Ctrl Pts',(-4.00173824143169,-7.07153341752101,
67.7629940937613));
#174942=CARTESIAN_POINT('Ctrl Pts',(-4.02642609084264,-7.05750570269801,
67.761895992281));
#174943=CARTESIAN_POINT('Ctrl Pts',(-4.06225479286396,-7.03689853169093,
67.7602910874559));
#174944=CARTESIAN_POINT('Ctrl Pts',(-4.07345437557699,-7.03042135264311,
67.7597878039503));
#174945=CARTESIAN_POINT('Ctrl Pts',(-4.093045280803,-7.0190285986269,67.7589045955394));
#174946=CARTESIAN_POINT('Ctrl Pts',(-4.10144335032669,-7.0141246483289,
67.758525072208));
#174947=CARTESIAN_POINT('Ctrl Pts',(-4.11770548553439,-7.00458938050265,
67.7577883739759));
#174948=CARTESIAN_POINT('Ctrl Pts',(-4.12557059474589,-6.99995986575535,
67.7574312617242));
#174949=CARTESIAN_POINT('Ctrl Pts',(-4.1442861747106,-6.98890111050983,
67.7565795483498));
#174950=CARTESIAN_POINT('Ctrl Pts',(-4.15512949370236,-6.98245984730412,
67.7560845310902));
#174951=CARTESIAN_POINT('Ctrl Pts',(-4.19364163322253,-6.95946098004096,
67.7543208191451));
#174952=CARTESIAN_POINT('Ctrl Pts',(-4.22122666817874,-6.94276405096403,
67.7530472891322));
#174953=CARTESIAN_POINT('Ctrl Pts',(-4.67677196270482,-6.66330874395816,
67.7318444279279));
#174954=CARTESIAN_POINT('Ctrl Pts',(-5.07951291141891,-6.36162888214538,
67.710488533981));
#174955=CARTESIAN_POINT('Ctrl Pts',(-5.64190296136223,-5.85272167400217,
67.6769527046995));
#174956=CARTESIAN_POINT('Ctrl Pts',(-5.82375524306836,-5.67179777825154,
67.6654332765996));
#174957=CARTESIAN_POINT('Ctrl Pts',(-6.36389153071405,-5.08100700429423,
67.6294739318485));
#174958=CARTESIAN_POINT('Ctrl Pts',(-6.68983719728844,-4.64349362207447,
67.605100792816));
#174959=CARTESIAN_POINT('Ctrl Pts',(-6.97934853272343,-4.16037732323915,
67.5825268228573));
#174960=CARTESIAN_POINT('Ctrl Pts',(-6.98901572345644,-4.14411687078104,
67.581771489877));
#174961=CARTESIAN_POINT('Ctrl Pts',(-7.00628165217253,-4.11484289567279,
67.580419388186));
#174962=CARTESIAN_POINT('Ctrl Pts',(-7.01390111922076,-4.10184174969319,
67.5798216205588));
#174963=CARTESIAN_POINT('Ctrl Pts',(-7.0260047268843,-4.0810569500542,67.5788702148473));
#174964=CARTESIAN_POINT('Ctrl Pts',(-7.03051218262687,-4.07328696541042,
67.5785154929436));
#174965=CARTESIAN_POINT('Ctrl Pts',(-7.03838572416256,-4.05966249401794,
67.5778951214279));
#174966=CARTESIAN_POINT('Ctrl Pts',(-7.04175740807506,-4.05381126516518,
67.5776292173625));
#174967=CARTESIAN_POINT('Ctrl Pts',(-7.04936853689389,-4.04056474474278,
67.5770284107597));
#174968=CARTESIAN_POINT('Ctrl Pts',(-7.05360365082833,-4.03316696444838,
67.5766937020005));
#174969=CARTESIAN_POINT('Ctrl Pts',(-7.06501154578945,-4.01316703892286,
67.5757910058133));
#174970=CARTESIAN_POINT('Ctrl Pts',(-7.07216226468644,-4.00055230307849,
67.5752239841448));
#174971=CARTESIAN_POINT('Ctrl Pts',(-7.10393023166592,-3.94415839453911,
67.5726993125262));
#174972=CARTESIAN_POINT('Ctrl Pts',(-7.12817529161501,-3.90017016480807,
67.5707573579752));
#174973=CARTESIAN_POINT('Ctrl Pts',(-7.15512691781651,-3.85018044470134,
67.5685784957784));
#174974=CARTESIAN_POINT('Ctrl Pts',(-7.15823562059561,-3.84439767286311,
67.5683268683799));
#174975=CARTESIAN_POINT('Ctrl Pts',(-7.19074635742421,-3.78374543566969,
67.5656920521144));
#174976=CARTESIAN_POINT('Ctrl Pts',(-7.21952429242536,-3.72854286372604,
67.5633313505425));
#174977=CARTESIAN_POINT('Ctrl Pts',(-7.30448361988949,-3.56089942096104,
67.5562610450679));
#174978=CARTESIAN_POINT('Ctrl Pts',(-7.3586938873596,-3.44747894752531,
67.5516100735348));
#174979=CARTESIAN_POINT('Ctrl Pts',(-7.55990469990789,-3.00010651399587,
67.5336431996009));
#174980=CARTESIAN_POINT('Ctrl Pts',(-7.68697892380179,-2.65766123365706,
67.520677545651));
#174981=CARTESIAN_POINT('Ctrl Pts',(-7.92752083770743,-1.84565710448643,
67.4901801584177));
#174982=CARTESIAN_POINT('Ctrl Pts',(-8.02302685049483,-1.37224137682229,
67.4725395280405));
#174983=CARTESIAN_POINT('Ctrl Pts',(-8.08285062260947,-0.831315734765007,
67.4517599623032));
#174984=CARTESIAN_POINT('Ctrl Pts',(-8.08898033100149,-0.76938751113298,
67.449373280676));
#174985=CARTESIAN_POINT('Ctrl Pts',(-8.09875036260817,-0.657593560786433,
67.4450504339902));
#174986=CARTESIAN_POINT('Ctrl Pts',(-8.10264296999869,-0.607752891722415,
67.4431180653179));
#174987=CARTESIAN_POINT('Ctrl Pts',(-8.10786522389545,-0.531872765917759,
67.4401683223207));
#174988=CARTESIAN_POINT('Ctrl Pts',(-8.10952991239581,-0.505857411798655,
67.4391556173412));
#174989=CARTESIAN_POINT('Ctrl Pts',(-8.11236055631888,-0.458008525922321,
67.4372904597392));
#174990=CARTESIAN_POINT('Ctrl Pts',(-8.11356363657743,-0.436177390521669,
67.436438514337));
#174991=CARTESIAN_POINT('Ctrl Pts',(-8.11573929955384,-0.393568105432536,
67.434773824817));
#174992=CARTESIAN_POINT('Ctrl Pts',(-8.11672024076189,-0.372790506428888,
67.4339611826753));
#174993=CARTESIAN_POINT('Ctrl Pts',(-8.11911203607947,-0.317633774258172,
67.4318014025331));
#174994=CARTESIAN_POINT('Ctrl Pts',(-8.12038431223899,-0.28324913788809,
67.4304523994076));
#174995=CARTESIAN_POINT('Ctrl Pts',(-8.12418770521429,-0.159125849185185,
67.4255723975308));
#174996=CARTESIAN_POINT('Ctrl Pts',(-8.12544991887554,-0.0693556589142267,
67.422023492796));
#174997=CARTESIAN_POINT('Ctrl Pts',(-8.12364523334291,0.648873426885906,
67.3934434558375));
#174998=CARTESIAN_POINT('Ctrl Pts',(-8.04915847923988,1.27498319445882,
67.3671476166185));
#174999=CARTESIAN_POINT('Ctrl Pts',(-7.80688433222686,2.2901336481186,67.3228579568412));
#175000=CARTESIAN_POINT('Ctrl Pts',(-7.67964844082461,2.6861077945585,67.3052027981136));
#175001=CARTESIAN_POINT('Ctrl Pts',(-7.50307558741761,3.11869198044984,
67.2863626793351));
#175002=CARTESIAN_POINT('Ctrl Pts',(-7.48299505549403,3.16657039627257,
67.2842844535992));
#175003=CARTESIAN_POINT('Ctrl Pts',(-7.45690258042211,3.22714867952234,
67.2816664668417));
#175004=CARTESIAN_POINT('Ctrl Pts',(-7.45131495144626,3.24002935031666,
67.2811104730396));
#175005=CARTESIAN_POINT('Ctrl Pts',(-7.44232244705243,3.26061268448294,
67.2802231245441));
#175006=CARTESIAN_POINT('Ctrl Pts',(-7.43893894735494,3.26832462008929,
67.2798909171762));
#175007=CARTESIAN_POINT('Ctrl Pts',(-7.43251301171878,3.28290943913169,
67.2792631452908));
#175008=CARTESIAN_POINT('Ctrl Pts',(-7.42947301845861,3.28978338547856,
67.2789674813435));
#175009=CARTESIAN_POINT('Ctrl Pts',(-7.42257632304926,3.30531968211885,
67.2782997202027));
#175010=CARTESIAN_POINT('Ctrl Pts',(-7.41871398279387,3.313979528444,67.2779278588823));
#175011=CARTESIAN_POINT('Ctrl Pts',(-7.40733106292205,3.33938182212979,
67.2768381140802));
#175012=CARTESIAN_POINT('Ctrl Pts',(-7.39976887360642,3.35610563809094,
67.2761220146158));
#175013=CARTESIAN_POINT('Ctrl Pts',(-7.3442575638069,3.47776938096674,67.2709229699835));
#175014=CARTESIAN_POINT('Ctrl Pts',(-7.29413864732273,3.58169533223031,
67.2665464193172));
#175015=CARTESIAN_POINT('Ctrl Pts',(-6.92624758302988,4.3047725925774,67.2364877210908));
#175016=CARTESIAN_POINT('Ctrl Pts',(-6.5322776545076,4.88195575864787,67.2141925393082));
#175017=CARTESIAN_POINT('Ctrl Pts',(-5.72851076755715,5.78506503095518,
67.1729244295603));
#175018=CARTESIAN_POINT('Ctrl Pts',(-5.35200186662086,6.13504840745117,
67.1547320846952));
#175019=CARTESIAN_POINT('Ctrl Pts',(-4.92273492565188,6.46429875265236,
67.1338894137622));
#175020=CARTESIAN_POINT('Ctrl Pts',(-4.90034498303991,6.48128818525221,
67.1328023098433));
#175021=CARTESIAN_POINT('Ctrl Pts',(-4.86756380388422,6.50589549297222,
67.1312105824569));
#175022=CARTESIAN_POINT('Ctrl Pts',(-4.8572417819325,6.51360543941619,67.1307093714129));
#175023=CARTESIAN_POINT('Ctrl Pts',(-4.83910306677747,6.52708690627988,
67.1298285649592));
#175024=CARTESIAN_POINT('Ctrl Pts',(-4.83129426495378,6.53286902498781,
67.1294493617748));
#175025=CARTESIAN_POINT('Ctrl Pts',(-4.81611834134668,6.54406412402888,
67.1287123749738));
#175026=CARTESIAN_POINT('Ctrl Pts',(-4.80875241648433,6.5494787070103,67.1283546511884));
#175027=CARTESIAN_POINT('Ctrl Pts',(-4.79115549978447,6.56236825297716,
67.1275000255716));
#175028=CARTESIAN_POINT('Ctrl Pts',(-4.78091614438116,6.56983172763534,
67.1270027032725));
#175029=CARTESIAN_POINT('Ctrl Pts',(-4.74427406650383,6.59640914370292,
67.1252228816519));
#175030=CARTESIAN_POINT('Ctrl Pts',(-4.71777400173205,6.61538800433101,
67.1239354528301));
#175031=CARTESIAN_POINT('Ctrl Pts',(-4.26146317939659,6.93805316163785,
67.1017613747089));
#175032=CARTESIAN_POINT('Ctrl Pts',(-3.80331990871621,7.19939476466031,
67.0793045265722));
#175033=CARTESIAN_POINT('Ctrl Pts',(-3.07124324612625,7.52750801859559,
67.0436601736648));
#175034=CARTESIAN_POINT('Ctrl Pts',(-2.81371562270016,7.62751013974738,
67.0311853636322));
#175035=CARTESIAN_POINT('Ctrl Pts',(-2.23350135862769,7.81942576983251,
67.0036286497536));
#175036=CARTESIAN_POINT('Ctrl Pts',(-1.90918175208397,7.90487132480282,
66.988583617878));
#175037=CARTESIAN_POINT('Ctrl Pts',(-1.50483030809981,7.9850563451124,66.970841124326));
#175038=CARTESIAN_POINT('Ctrl Pts',(-1.42894622558409,7.99898445276284,
66.9675550811182));
#175039=CARTESIAN_POINT('Ctrl Pts',(-1.26057291326981,8.02741588921456,
66.9603748289545));
#175040=CARTESIAN_POINT('Ctrl Pts',(-1.16800677360788,8.0414060445731,66.9565009404886));
#175041=CARTESIAN_POINT('Ctrl Pts',(-1.02180670860129,8.06092439468,66.9505169889738));
#175042=CARTESIAN_POINT('Ctrl Pts',(-0.968327462287127,8.0675233480576,
66.9483570071883));
#175043=CARTESIAN_POINT('Ctrl Pts',(-0.901075449670824,8.07514340375013,
66.9456732948217));
#175044=CARTESIAN_POINT('Ctrl Pts',(-0.887360828707382,8.07666197881792,
66.9451276958735));
#175045=CARTESIAN_POINT('Ctrl Pts',(-0.865554460247878,8.07902031299955,
66.9442627790811));
#175046=CARTESIAN_POINT('Ctrl Pts',(-0.857465243867065,8.0798828641092,
66.9439424987562));
#175047=CARTESIAN_POINT('Ctrl Pts',(-0.842241128180823,8.08148308758662,
66.9433407663423));
#175048=CARTESIAN_POINT('Ctrl Pts',(-0.835106525419513,8.08222346292072,
66.9430592025743));
#175049=CARTESIAN_POINT('Ctrl Pts',(-0.819083943237819,8.0838647232487,
66.9424278287786));
#175050=CARTESIAN_POINT('Ctrl Pts',(-0.810195431557844,8.08476040049189,
66.9420782308996));
#175051=CARTESIAN_POINT('Ctrl Pts',(-0.787598524540116,8.08699980532536,
66.9411910908572));
#175052=CARTESIAN_POINT('Ctrl Pts',(-0.773888125860028,8.08832334039418,
66.9406543523265));
#175053=CARTESIAN_POINT('Ctrl Pts',(-0.697694262053483,8.09548321688525,
66.9376796439581));
#175054=CARTESIAN_POINT('Ctrl Pts',(-0.635147207728117,8.10063047358791,
66.9352681500204));
#175055=CARTESIAN_POINT('Ctrl Pts',(0.168378862335905,8.15739204640914,
66.904612617782));
#175056=CARTESIAN_POINT('Ctrl Pts',(0.913042336930171,8.10789647634058,
66.8792462508587));
#175057=CARTESIAN_POINT('Ctrl Pts',(1.93143524335923,7.89793545264935,66.8411471898703));
#175058=CARTESIAN_POINT('Ctrl Pts',(2.21868846126042,7.82209940607559,66.8300713915483));
#175059=CARTESIAN_POINT('Ctrl Pts',(2.76815282729282,7.64432964409433,66.808134051918));
#175060=CARTESIAN_POINT('Ctrl Pts',(3.03050839307999,7.54416725991463,66.7973378179631));
#175061=CARTESIAN_POINT('Ctrl Pts',(3.35722349828693,7.39963577098459,66.7834777094646));
#175062=CARTESIAN_POINT('Ctrl Pts',(3.42685684990023,7.36764624488402,66.7804969147674));
#175063=CARTESIAN_POINT('Ctrl Pts',(3.53498910736567,7.3161056924747,66.7758230250501));
#175064=CARTESIAN_POINT('Ctrl Pts',(3.57380252720547,7.29722453882304,66.7741361565688));
#175065=CARTESIAN_POINT('Ctrl Pts',(3.64605904881325,7.26135990660095,66.7709779944127));
#175066=CARTESIAN_POINT('Ctrl Pts',(3.67953859658884,7.24445235914449,66.7695074528438));
#175067=CARTESIAN_POINT('Ctrl Pts',(3.75432431601573,7.20603256776671,66.7662059383096));
#175068=CARTESIAN_POINT('Ctrl Pts',(3.79556497944784,7.1843957922146,66.7643738154981));
#175069=CARTESIAN_POINT('Ctrl Pts',(3.91606353853653,7.11984948401743,66.7589858665454));
#175070=CARTESIAN_POINT('Ctrl Pts',(3.9947958291383,7.07597459109165,66.7554208248923));
#175071=CARTESIAN_POINT('Ctrl Pts',(4.61584434226886,6.71621537012863,66.7269272717926));
#175072=CARTESIAN_POINT('Ctrl Pts',(5.12062435597174,6.33977408667381,66.7013594027734));
#175073=CARTESIAN_POINT('Ctrl Pts',(5.70083759731357,5.79216076383939,66.6690256663079));
#175074=CARTESIAN_POINT('Ctrl Pts',(5.82095447296992,5.67143419109782,66.6621515817681));
#175075=CARTESIAN_POINT('Ctrl Pts',(5.98111482082203,5.50000842620154,66.6527607321199));
#175076=CARTESIAN_POINT('Ctrl Pts',(6.02447930591811,5.45247433561489,66.6501940450774));
#175077=CARTESIAN_POINT('Ctrl Pts',(6.09875713143947,5.36908645007551,66.6457578067695));
#175078=CARTESIAN_POINT('Ctrl Pts',(6.12993011411289,5.33346835557321,66.6438834202816));
#175079=CARTESIAN_POINT('Ctrl Pts',(6.17530749811607,5.28069698466522,66.6411371328361));
#175080=CARTESIAN_POINT('Ctrl Pts',(6.18975533884231,5.26375457191609,66.6402600296525));
#175081=CARTESIAN_POINT('Ctrl Pts',(6.21609387538912,5.23261001498598,66.6386561856895));
#175082=CARTESIAN_POINT('Ctrl Pts',(6.2280059656783,5.21842623125739,66.6379289514342));
#175083=CARTESIAN_POINT('Ctrl Pts',(6.25477770937037,5.18632674848314,66.636290085895));
#175084=CARTESIAN_POINT('Ctrl Pts',(6.26960910197254,5.16838766440655,66.6353790382456));
#175085=CARTESIAN_POINT('Ctrl Pts',(6.30791479290245,5.12164807629578,66.6330173878932));
#175086=CARTESIAN_POINT('Ctrl Pts',(6.33126903934526,5.0927497899076,66.6315690019332));
#175087=CARTESIAN_POINT('Ctrl Pts',(6.49067129220682,4.89271599919196,66.6216188195317));
#175088=CARTESIAN_POINT('Ctrl Pts',(6.61996362658758,4.71630864829569,66.6132184609574));
#175089=CARTESIAN_POINT('Ctrl Pts',(6.84009164238777,4.38904683280956,66.5980576517333));
#175090=CARTESIAN_POINT('Ctrl Pts',(6.9334388927404,4.24004841252845,66.5913032211815));
#175091=CARTESIAN_POINT('Ctrl Pts',(7.07767457367433,3.99230603314086,66.5802320487235));
#175092=CARTESIAN_POINT('Ctrl Pts',(7.13150126140866,3.89534008052208,66.5759373569923));
#175093=CARTESIAN_POINT('Ctrl Pts',(7.20524250760718,3.7558443976771,66.5698017332538));
#175094=CARTESIAN_POINT('Ctrl Pts',(7.22679945369571,3.71419659773013,66.5679752323476));
#175095=CARTESIAN_POINT('Ctrl Pts',(7.26399454420735,3.64078618166893,66.5647643115575));
#175096=CARTESIAN_POINT('Ctrl Pts',(7.27978791652459,3.60910357834949,66.5633813049974));
#175097=CARTESIAN_POINT('Ctrl Pts',(7.31241338045087,3.54256912553104,66.5604823963732));
#175098=CARTESIAN_POINT('Ctrl Pts',(7.32920451778435,3.50769818811195,66.5589661686231));
#175099=CARTESIAN_POINT('Ctrl Pts',(7.37324690396006,3.41453627810188,66.5549231781983));
#175100=CARTESIAN_POINT('Ctrl Pts',(7.40005587672126,3.35603946070945,66.5523926111522));
#175101=CARTESIAN_POINT('Ctrl Pts',(7.56533041145752,2.98380091849978,66.5363372753369));
#175102=CARTESIAN_POINT('Ctrl Pts',(7.68450946102702,2.66187903549099,66.5226431027337));
#175103=CARTESIAN_POINT('Ctrl Pts',(7.83512182606183,2.15951533923086,66.5016970093936));
#175104=CARTESIAN_POINT('Ctrl Pts',(7.88141179793418,1.98393285100065,66.4944568374496));
#175105=CARTESIAN_POINT('Ctrl Pts',(7.93145751486333,1.7645288671942,66.4855625941377));
#175106=CARTESIAN_POINT('Ctrl Pts',(7.94079210969303,1.72203401078657,66.4838470465938));
#175107=CARTESIAN_POINT('Ctrl Pts',(7.95431498374099,1.65802322615973,66.4812747143047));
#175108=CARTESIAN_POINT('Ctrl Pts',(7.95875820721297,1.63656215374422,66.4804143018794));
#175109=CARTESIAN_POINT('Ctrl Pts',(7.96707320447535,1.59556533448844,66.4787745163987));
#175110=CARTESIAN_POINT('Ctrl Pts',(7.97096007350897,1.57603289680016,66.4779948997055));
#175111=CARTESIAN_POINT('Ctrl Pts',(7.97976232870652,1.53093387838883,66.4761983843436));
#175112=CARTESIAN_POINT('Ctrl Pts',(7.98462673092698,1.50535754454683,66.475182191451));
#175113=CARTESIAN_POINT('Ctrl Pts',(7.99750618916814,1.43582001312951,66.4724259462639));
#175114=CARTESIAN_POINT('Ctrl Pts',(8.00528167202,1.3918152665049,66.4706888922711));
#175115=CARTESIAN_POINT('Ctrl Pts',(8.05157034817105,1.11661778278855,66.4598640027488));
#175116=CARTESIAN_POINT('Ctrl Pts',(8.08042845631781,0.883910871926848,
66.4508764259574));
#175117=CARTESIAN_POINT('Ctrl Pts',(8.11659211714811,0.433495816651327,
66.4335543104261));
#175118=CARTESIAN_POINT('Ctrl Pts',(8.12528685465822,0.216100174615363,
66.4252264970346));
#175119=CARTESIAN_POINT('Ctrl Pts',(8.12521409019402,-0.211923570187139,
66.4087511185072));
#175120=CARTESIAN_POINT('Ctrl Pts',(8.11699493825367,-0.422382964632793,
66.4006125534617));
#175121=CARTESIAN_POINT('Ctrl Pts',(8.09538390981195,-0.699256483068275,
66.3898052595378));
#175122=CARTESIAN_POINT('Ctrl Pts',(8.08932606281942,-0.766161911063918,
66.3871861588197));
#175123=CARTESIAN_POINT('Ctrl Pts',(8.07676727611018,-0.888019704309546,
66.382400906296));
#175124=CARTESIAN_POINT('Ctrl Pts',(8.07053331029202,-0.942995592617735,
66.3802364799513));
#175125=CARTESIAN_POINT('Ctrl Pts',(8.05643536843777,-1.05691655480052,
66.3757393629398));
#175126=CARTESIAN_POINT('Ctrl Pts',(8.04848479322796,-1.11584763840538,
66.3734063245012));
#175127=CARTESIAN_POINT('Ctrl Pts',(8.0236705920712,-1.28568315175161,66.366663100997));
#175128=CARTESIAN_POINT('Ctrl Pts',(8.00515628565184,-1.39633220505732,
66.3622455509408));
#175129=CARTESIAN_POINT('Ctrl Pts',(7.96560317565574,-1.60595261680053,
66.3538327016816));
#175130=CARTESIAN_POINT('Ctrl Pts',(7.94499505202998,-1.70498426553291,
66.3498393545942));
#175131=CARTESIAN_POINT('Ctrl Pts',(7.89078443591569,-1.94311063898959,
66.3401975497372));
#175132=CARTESIAN_POINT('Ctrl Pts',(7.85534604560827,-2.08175327420229,
66.3345506808625));
#175133=CARTESIAN_POINT('Ctrl Pts',(7.80378797100673,-2.26333107199899,
66.3271268925674));
#175134=CARTESIAN_POINT('Ctrl Pts',(7.79094019770234,-2.3071681975563,66.3253324659611));
#175135=CARTESIAN_POINT('Ctrl Pts',(7.76524205126199,-2.39218819962183,
66.3218490623778));
#175136=CARTESIAN_POINT('Ctrl Pts',(7.75243201312976,-2.43338167807495,
66.3201598926861));
#175137=CARTESIAN_POINT('Ctrl Pts',(7.70626740455601,-2.57776868670368,
66.3142313315006));
#175138=CARTESIAN_POINT('Ctrl Pts',(7.67117540937297,-2.68039487733141,
66.3100031626101));
#175139=CARTESIAN_POINT('Ctrl Pts',(7.56586223670502,-2.96935306622828,
66.2980227777913));
#175140=CARTESIAN_POINT('Ctrl Pts',(7.49083224236327,-3.15384863120235,
66.2902819749781));
#175141=CARTESIAN_POINT('Ctrl Pts',(7.37643109916493,-3.4079738740167,66.2794060088474));
#175142=CARTESIAN_POINT('Ctrl Pts',(7.34269625096009,-3.4800622686869,66.2762962317874));
#175143=CARTESIAN_POINT('Ctrl Pts',(7.28367215345462,-3.60151102884986,
66.2710103044029));
#175144=CARTESIAN_POINT('Ctrl Pts',(7.25892666212905,-3.65112933474513,
66.2688372431872));
#175145=CARTESIAN_POINT('Ctrl Pts',(7.20607788168896,-3.75443751282017,
66.2642827663701));
#175146=CARTESIAN_POINT('Ctrl Pts',(7.17787789358002,-3.80807410429185,
66.2619008915859));
#175147=CARTESIAN_POINT('Ctrl Pts',(7.09808609249884,-3.95580277367275,
66.2552901750498));
#175148=CARTESIAN_POINT('Ctrl Pts',(7.04522653103298,-4.04919555946854,
66.2510534063102));
#175149=CARTESIAN_POINT('Ctrl Pts',(6.9215124827327,-4.25801466173364,66.2414413001707));
#175150=CARTESIAN_POINT('Ctrl Pts',(6.84959071805755,-4.3727714922219,66.2360597871468));
#175151=CARTESIAN_POINT('Ctrl Pts',(6.53770099839623,-4.84382672177588,
66.2135404342653));
#175152=CARTESIAN_POINT('Ctrl Pts',(6.2725408675276,-5.18260759031173,66.1962574664917));
#175153=CARTESIAN_POINT('Ctrl Pts',(5.9340245562,-5.55085881413701,66.1764179372877));
#175154=CARTESIAN_POINT('Ctrl Pts',(5.88552494959952,-5.60225643702847,
66.173623663906));
#175155=CARTESIAN_POINT('Ctrl Pts',(5.81819010225182,-5.67177517281152,
66.1698122825605));
#175156=CARTESIAN_POINT('Ctrl Pts',(5.79992899526413,-5.69044755125468,
66.1687853421284));
#175157=CARTESIAN_POINT('Ctrl Pts',(5.76840539906206,-5.72237172808484,
66.1670242276754));
#175158=CARTESIAN_POINT('Ctrl Pts',(5.75518650853229,-5.73566624700747,
66.1662892149316));
#175159=CARTESIAN_POINT('Ctrl Pts',(5.72778720485934,-5.76303222101129,
66.1647729869279));
#175160=CARTESIAN_POINT('Ctrl Pts',(5.71360065269636,-5.77709738806742,
66.1639919078419));
#175161=CARTESIAN_POINT('Ctrl Pts',(5.67769241136163,-5.81243673973807,
66.162025014844));
#175162=CARTESIAN_POINT('Ctrl Pts',(5.65590289376746,-5.83364161049239,
66.1608407218886));
#175163=CARTESIAN_POINT('Ctrl Pts',(5.55067145053681,-5.93490572302008,
66.155163386764));
#175164=CARTESIAN_POINT('Ctrl Pts',(5.46564512663863,-6.01330053341449,
66.1507021741328));
#175165=CARTESIAN_POINT('Ctrl Pts',(5.15134202941808,-6.29091442219426,
66.1345828077174));
#175166=CARTESIAN_POINT('Ctrl Pts',(4.91261590221555,-6.47905357528902,
66.1230221806197));
#175167=CARTESIAN_POINT('Ctrl Pts',(4.54107957367375,-6.73949461958504,
66.1055822575981));
#175168=CARTESIAN_POINT('Ctrl Pts',(4.41588098621987,-6.82218336721901,
66.0997942969035));
#175169=CARTESIAN_POINT('Ctrl Pts',(4.24308419578413,-6.92955834317883,
66.0918973619693));
#175170=CARTESIAN_POINT('Ctrl Pts',(4.19742538294049,-6.95731000049822,
66.0898192229814));
#175171=CARTESIAN_POINT('Ctrl Pts',(4.1232537544949,-7.00139596624113,66.0864560319566));
#175172=CARTESIAN_POINT('Ctrl Pts',(4.094909689487,-7.01801123014745,66.0851737748835));
#175173=CARTESIAN_POINT('Ctrl Pts',(4.03525291537851,-7.05249752029697,
66.0824809209811));
#175174=CARTESIAN_POINT('Ctrl Pts',(4.00392046844352,-7.07033296499898,
66.0810700107101));
#175175=CARTESIAN_POINT('Ctrl Pts',(3.92796405792192,-7.11290298887246,
66.0776576076076));
#175176=CARTESIAN_POINT('Ctrl Pts',(3.88322388049436,-7.13742690554507,
66.0756541715074));
#175177=CARTESIAN_POINT('Ctrl Pts',(3.71135679690996,-7.2295399099169,66.0679822541809));
#175178=CARTESIAN_POINT('Ctrl Pts',(3.58267349414296,-7.29416661469247,
66.0622874990506));
#175179=CARTESIAN_POINT('Ctrl Pts',(3.17560203757542,-7.48523188214039,
66.0444301608095));
#175180=CARTESIAN_POINT('Ctrl Pts',(2.89175369627808,-7.59940154113746,
66.0321913243133));
#175181=CARTESIAN_POINT('Ctrl Pts',(2.53477966330553,-7.72008011783607,
66.0172307782375));
#175182=CARTESIAN_POINT('Ctrl Pts',(2.46711333358603,-7.74196983099114,
66.0144142150904));
#175183=CARTESIAN_POINT('Ctrl Pts',(2.37525429729774,-7.77035913429486,
66.0106207974673));
#175184=CARTESIAN_POINT('Ctrl Pts',(2.35130643850876,-7.77763923633915,
66.0096346003467));
#175185=CARTESIAN_POINT('Ctrl Pts',(2.31033218790532,-7.78988878722828,
66.0079521948445));
#175186=CARTESIAN_POINT('Ctrl Pts',(2.29332248590119,-7.79491334870117,
66.0072552298158));
#175187=CARTESIAN_POINT('Ctrl Pts',(2.25821560996518,-7.8051588440548,66.005819850931));
#175188=CARTESIAN_POINT('Ctrl Pts',(2.24011645835406,-7.8103726274337,66.0050815573951));
#175189=CARTESIAN_POINT('Ctrl Pts',(2.19475620293195,-7.82326881469741,
66.0032356071258));
#175190=CARTESIAN_POINT('Ctrl Pts',(2.16747275199456,-7.83087170219616,
66.0021291939289));
#175191=CARTESIAN_POINT('Ctrl Pts',(2.05507102089112,-7.86156146807002,
65.997586096076));
#175192=CARTESIAN_POINT('Ctrl Pts',(1.96961876925467,-7.88340457949319,
65.9941677224519));
#175193=CARTESIAN_POINT('Ctrl Pts',(1.39816802030431,-8.01960581908799,
65.9714986999136));
#175194=CARTESIAN_POINT('Ctrl Pts',(0.902866426919166,-8.09035209126938,
65.9527310908568));
#175195=CARTESIAN_POINT('Ctrl Pts',(0.290640563331582,-8.12084633362458,
65.929376276916));
#175196=CARTESIAN_POINT('Ctrl Pts',(0.176967400717827,-8.1241183801935,
65.9250352451172));
#175197=CARTESIAN_POINT('Ctrl Pts',(-0.17221644250915,-8.12683722238152,
65.9116611181454));
#175198=CARTESIAN_POINT('Ctrl Pts',(-0.407661965790738,-8.11843279466399,
65.9025865897993));
#175199=CARTESIAN_POINT('Ctrl Pts',(-0.709506812354297,-8.09449308979185,
65.8908154373219));
#175200=CARTESIAN_POINT('Ctrl Pts',(-0.776537880727611,-8.08833772507705,
65.8881928263365));
#175201=CARTESIAN_POINT('Ctrl Pts',(-0.884513901156566,-8.07706781409081,
65.8839532090205));
#175202=CARTESIAN_POINT('Ctrl Pts',(-0.925510025313442,-8.07247300978378,
65.8823400203701));
#175203=CARTESIAN_POINT('Ctrl Pts',(-1.00406236014561,-8.06306268486193,
65.879242034595));
#175204=CARTESIAN_POINT('Ctrl Pts',(-1.04162342017547,-8.05829645291117,
65.8777576197378));
#175205=CARTESIAN_POINT('Ctrl Pts',(-1.12860651991741,-8.04664058980043,
65.8743127481626));
#175206=CARTESIAN_POINT('Ctrl Pts',(-1.17800110157287,-8.03955787588657,
65.8723510553864));
#175207=CARTESIAN_POINT('Ctrl Pts',(-1.33886403808096,-8.01497732958864,
65.8659441085504));
#175208=CARTESIAN_POINT('Ctrl Pts',(-1.45003325117336,-7.99561266216185,
65.8614875386447));
#175209=CARTESIAN_POINT('Ctrl Pts',(-2.14166742442192,-7.86023707560376,
65.8335770948069));
#175210=CARTESIAN_POINT('Ctrl Pts',(-2.70838026960999,-7.68340436469641,
65.8098940618716));
#175211=CARTESIAN_POINT('Ctrl Pts',(-3.55252128438107,-7.31489158181805,
65.77150808314));
#175212=CARTESIAN_POINT('Ctrl Pts',(-3.8459185068589,-7.16498073331512,
65.7575626268181));
#175213=CARTESIAN_POINT('Ctrl Pts',(-4.46864879847514,-6.79750156815182,
65.7269634608765));
#175214=CARTESIAN_POINT('Ctrl Pts',(-4.79289827014357,-6.57289871458698,
65.7103468082767));
#175215=CARTESIAN_POINT('Ctrl Pts',(-5.11649168966103,-6.31202598791034,
65.6938132369453));
#175216=CARTESIAN_POINT('Ctrl Pts',(-5.13334579690712,-6.29832677960305,
65.6929523697108));
#175217=CARTESIAN_POINT('Ctrl Pts',(-5.15705283204414,-6.27889906091169,
65.6917420926312));
#175218=CARTESIAN_POINT('Ctrl Pts',(-5.16395147489601,-6.27322664147535,
65.6913899820534));
#175219=CARTESIAN_POINT('Ctrl Pts',(-5.17651930719527,-6.26285794337134,
65.6907486711045));
#175220=CARTESIAN_POINT('Ctrl Pts',(-5.18219148882733,-6.25816531662345,
65.6904592902064));
#175221=CARTESIAN_POINT('Ctrl Pts',(-5.19360646722319,-6.24869548203223,
65.6898770583545));
#175222=CARTESIAN_POINT('Ctrl Pts',(-5.19934906997312,-6.24391804979842,
65.689584219249));
#175223=CARTESIAN_POINT('Ctrl Pts',(-5.21335235794006,-6.23223560787106,
65.6888703166078));
#175224=CARTESIAN_POINT('Ctrl Pts',(-5.22160593682087,-6.22532207376202,
65.6884496962123));
#175225=CARTESIAN_POINT('Ctrl Pts',(-5.25102079105293,-6.20058333940167,
65.6869512847883));
#175226=CARTESIAN_POINT('Ctrl Pts',(-5.27210488589027,-6.18266634995624,
65.6858784212792));
#175227=CARTESIAN_POINT('Ctrl Pts',(-5.69304264548774,-5.82123992251527,
65.6644900534577));
#175228=CARTESIAN_POINT('Ctrl Pts',(-6.05863507432376,-5.43971904231667,
65.6466661385943));
#175229=CARTESIAN_POINT('Ctrl Pts',(-6.57424450685164,-4.78465457191867,
65.6188089320896));
#175230=CARTESIAN_POINT('Ctrl Pts',(-6.75001803475049,-4.53330615418877,
65.6086603655937));
#175231=CARTESIAN_POINT('Ctrl Pts',(-7.17801341021492,-3.84100494506177,
65.581007867879));
#175232=CARTESIAN_POINT('Ctrl Pts',(-7.40380680392797,-3.38537584130643,
65.5630447193436));
#175233=CARTESIAN_POINT('Ctrl Pts',(-7.59726689937952,-2.88136740909345,
65.5422913732803));
#175234=CARTESIAN_POINT('Ctrl Pts',(-7.60872398657461,-2.85097557929176,
65.5410370420098));
#175235=CARTESIAN_POINT('Ctrl Pts',(-7.62439017416096,-2.80865129463363,
65.5392860452217));
#175236=CARTESIAN_POINT('Ctrl Pts',(-7.62875415348125,-2.79677630258508,
65.5387943090215));
#175237=CARTESIAN_POINT('Ctrl Pts',(-7.63622197236423,-2.77630780585556,
65.5379459249085));
#175238=CARTESIAN_POINT('Ctrl Pts',(-7.63933908974433,-2.76771915397871,
65.5375896991179));
#175239=CARTESIAN_POINT('Ctrl Pts',(-7.64574211796224,-2.74998354397871,
65.5368535895245));
#175240=CARTESIAN_POINT('Ctrl Pts',(-7.64902611610913,-2.74083591279153,
65.5364736458324));
#175241=CARTESIAN_POINT('Ctrl Pts',(-7.65663102158317,-2.7195322028468,
65.53558815841));
#175242=CARTESIAN_POINT('Ctrl Pts',(-7.66093940027064,-2.70737169714791,
65.5350822195579));
#175243=CARTESIAN_POINT('Ctrl Pts',(-7.67457278516681,-2.66859801109404,
65.5334674653374));
#175244=CARTESIAN_POINT('Ctrl Pts',(-7.68378816868808,-2.64194665709101,
65.532355197167));
#175245=CARTESIAN_POINT('Ctrl Pts',(-7.86539384528741,-2.10774574820757,
65.5100127789457));
#175246=CARTESIAN_POINT('Ctrl Pts',(-7.98725817670137,-1.58448422945002,
65.4871424845212));
#175247=CARTESIAN_POINT('Ctrl Pts',(-8.1323200153023,-0.474689868414925,
65.4374942058783));
#175248=CARTESIAN_POINT('Ctrl Pts',(-8.14541724627627,0.11016935005052,
65.4107024834253));
#175249=CARTESIAN_POINT('Ctrl Pts',(-8.07867718978711,0.891666298386771,
65.3770688398252));
#175250=CARTESIAN_POINT('Ctrl Pts',(-8.05414508560277,1.09126581436165,
65.368694457187));
#175251=CARTESIAN_POINT('Ctrl Pts',(-8.01892898912319,1.31030437846695,
65.3598397965051));
#175252=CARTESIAN_POINT('Ctrl Pts',(-8.01555041022097,1.33081603872916,
65.3590134768446));
#175253=CARTESIAN_POINT('Ctrl Pts',(-8.01047380964964,1.3609157619988,65.3578048528227));
#175254=CARTESIAN_POINT('Ctrl Pts',(-8.00883722825762,1.37051399799154,
65.3574200365076));
#175255=CARTESIAN_POINT('Ctrl Pts',(-8.00589774452284,1.38756843376153,
65.3567373024246));
#175256=CARTESIAN_POINT('Ctrl Pts',(-8.00460167072762,1.39502578743407,
65.3564391115006));
#175257=CARTESIAN_POINT('Ctrl Pts',(-8.00187959949421,1.41055935570605,
65.3558186886657));
#175258=CARTESIAN_POINT('Ctrl Pts',(-8.00045179083238,1.41863524697295,
65.3554965285343));
#175259=CARTESIAN_POINT('Ctrl Pts',(-7.99753086362955,1.43501176898227,
65.3548440274901));
#175260=CARTESIAN_POINT('Ctrl Pts',(-7.99603704325914,1.44331226535306,
65.3545137141916));
#175261=CARTESIAN_POINT('Ctrl Pts',(-7.98998427507912,1.47664699295352,
65.3531887761207));
#175262=CARTESIAN_POINT('Ctrl Pts',(-7.98532063552413,1.50166221996321,
65.3521981297017));
#175263=CARTESIAN_POINT('Ctrl Pts',(-7.97375262244783,1.56213362192292,
65.3498113650114));
#175264=CARTESIAN_POINT('Ctrl Pts',(-7.96672914681945,1.59756661296886,
65.3484195235397));
#175265=CARTESIAN_POINT('Ctrl Pts',(-7.86692894604569,2.08402103143757,
65.3293908341882));
#175266=CARTESIAN_POINT('Ctrl Pts',(-7.73620633673433,2.52643571023312,
65.3129779518931));
#175267=CARTESIAN_POINT('Ctrl Pts',(-7.35803688400547,3.49491385757805,
65.2756551601418));
#175268=CARTESIAN_POINT('Ctrl Pts',(-7.09030629034492,4.01031793990886,
65.2547006226584));
#175269=CARTESIAN_POINT('Ctrl Pts',(-6.72003636824551,4.56825851802383,
65.2291262086479));
#175270=CARTESIAN_POINT('Ctrl Pts',(-6.66874851808954,4.64280815600138,
65.2256480126999));
#175271=CARTESIAN_POINT('Ctrl Pts',(-6.59620316492399,4.74457387976865,
65.2208139647307));
#175272=CARTESIAN_POINT('Ctrl Pts',(-6.57600094180632,4.77253487055945,
65.2194766195567));
#175273=CARTESIAN_POINT('Ctrl Pts',(-6.54332271204319,4.81716190283916,
65.2173274439717));
#175274=CARTESIAN_POINT('Ctrl Pts',(-6.53095960310399,4.83391017410198,
65.2165175143791));
#175275=CARTESIAN_POINT('Ctrl Pts',(-6.50678342642775,4.86639952391509,
65.2149398307756));
#175276=CARTESIAN_POINT('Ctrl Pts',(-6.49497724629585,4.88214557879501,
65.214172202156));
#175277=CARTESIAN_POINT('Ctrl Pts',(-6.46885533116981,4.91672226116835,
65.2124798627619));
#175278=CARTESIAN_POINT('Ctrl Pts',(-6.45451434601867,4.93553357206189,
65.2115547327507));
#175279=CARTESIAN_POINT('Ctrl Pts',(-6.41445567749221,4.98760599982247,
65.2089812793721));
#175280=CARTESIAN_POINT('Ctrl Pts',(-6.38856175005407,5.02073042327874,
65.2073299110334));
#175281=CARTESIAN_POINT('Ctrl Pts',(-6.33043040879614,5.09391621568159,
65.2036482762663));
#175282=CARTESIAN_POINT('Ctrl Pts',(-6.29806750408878,5.13387545892998,
65.2016157237437));
#175283=CARTESIAN_POINT('Ctrl Pts',(-5.97465714367341,5.52553724375952,
65.1814637391716));
#175284=CARTESIAN_POINT('Ctrl Pts',(-5.65485624178699,5.85240525089714,
65.1627293753417));
#175285=CARTESIAN_POINT('Ctrl Pts',(-4.87586664836254,6.52483658010809,
65.1194447066968));
#175286=CARTESIAN_POINT('Ctrl Pts',(-4.40408307581055,6.85212460011129,
65.0946992205918));
#175287=CARTESIAN_POINT('Ctrl Pts',(-3.84855357837986,7.15625678623129,
65.0689230406342));
#175288=CARTESIAN_POINT('Ctrl Pts',(-3.79495697475135,7.18482272543686,
65.0664699839276));
#175289=CARTESIAN_POINT('Ctrl Pts',(-3.71373590099987,7.2269495361896,65.0628079214012));
#175290=CARTESIAN_POINT('Ctrl Pts',(-3.68634691082636,7.24095852932249,
65.0615823896207));
#175291=CARTESIAN_POINT('Ctrl Pts',(-3.64824415396597,7.2601752057576,65.0598910191015));
#175292=CARTESIAN_POINT('Ctrl Pts',(-3.63759768017609,7.26551529791332,
65.0594198856143));
#175293=CARTESIAN_POINT('Ctrl Pts',(-3.62053489209693,7.27402679972451,
65.0586671896804));
#175294=CARTESIAN_POINT('Ctrl Pts',(-3.61412608281881,7.27721316479831,
65.0583850112067));
#175295=CARTESIAN_POINT('Ctrl Pts',(-3.60091268675825,7.28376090943299,
65.0578043417398));
#175296=CARTESIAN_POINT('Ctrl Pts',(-3.59410758244709,7.2871212319881,65.0575058952136));
#175297=CARTESIAN_POINT('Ctrl Pts',(-3.57828924690416,7.29490468957244,
65.056813586907));
#175298=CARTESIAN_POINT('Ctrl Pts',(-3.56927249435045,7.2993206688475,65.0564200307715));
#175299=CARTESIAN_POINT('Ctrl Pts',(-3.5410239304411,7.31309062189298,65.0551904625854));
#175300=CARTESIAN_POINT('Ctrl Pts',(-3.52176326475132,7.32238543361087,
65.0543570364865));
#175301=CARTESIAN_POINT('Ctrl Pts',(-3.35426453493117,7.40240320267688,
65.0471532159475));
#175302=CARTESIAN_POINT('Ctrl Pts',(-3.20395650283865,7.46868973780232,
65.0410087725186));
#175303=CARTESIAN_POINT('Ctrl Pts',(-2.69949267515121,7.67312716574129,
65.0212422503882));
#175304=CARTESIAN_POINT('Ctrl Pts',(-2.33764703225545,7.7909933326566,65.008376930653));
#175305=CARTESIAN_POINT('Ctrl Pts',(-1.71906298429799,7.94548953476738,
64.9869189938467));
#175306=CARTESIAN_POINT('Ctrl Pts',(-1.46643687724503,7.99597042042751,
64.9783012521853));
#175307=CARTESIAN_POINT('Ctrl Pts',(-0.707475819954939,8.11044631883014,
64.9521167343787));
#175308=CARTESIAN_POINT('Ctrl Pts',(-0.197119007150179,8.13885357084496,
64.9340526506436));
#175309=CARTESIAN_POINT('Ctrl Pts',(0.344775467129954,8.11799606352015,
64.9132014133074));
#175310=CARTESIAN_POINT('Ctrl Pts',(0.377033714500188,8.1165618188947,64.9119542311904));
#175311=CARTESIAN_POINT('Ctrl Pts',(0.421886141373222,8.11429965592282,
64.910211686451));
#175312=CARTESIAN_POINT('Ctrl Pts',(0.434488410269032,8.11363461353964,
64.9097211533254));
#175313=CARTESIAN_POINT('Ctrl Pts',(0.456203697186414,8.11243792446836,
64.9088742932131));
#175314=CARTESIAN_POINT('Ctrl Pts',(0.465317478449534,8.11192027421732,
64.9085183819724));
#175315=CARTESIAN_POINT('Ctrl Pts',(0.484137683759807,8.11081949129409,
64.9077824005763));
#175316=CARTESIAN_POINT('Ctrl Pts',(0.493843970354896,8.11023429065843,
64.9074022695735));
#175317=CARTESIAN_POINT('Ctrl Pts',(0.516454981119869,8.10883031128891,
64.9065154395649));
#175318=CARTESIAN_POINT('Ctrl Pts',(0.529358831163944,8.10799814940859,
64.9060083439557));
#175319=CARTESIAN_POINT('Ctrl Pts',(0.570554391291529,8.10524270882468,
64.9043862531092));
#175320=CARTESIAN_POINT('Ctrl Pts',(0.598837900124074,8.10320213446807,
64.9032677768537));
#175321=CARTESIAN_POINT('Ctrl Pts',(1.19545697479929,8.0570170773446,64.8795717415941));
#175322=CARTESIAN_POINT('Ctrl Pts',(1.75751587621444,7.95334038131988,64.8551312043109));
#175323=CARTESIAN_POINT('Ctrl Pts',(2.62510588459359,7.69679208170392,64.8147642484918));
#175324=CARTESIAN_POINT('Ctrl Pts',(2.94000145813439,7.58209572280094,64.7995588971635));
#175325=CARTESIAN_POINT('Ctrl Pts',(3.65023213176778,7.27248710499434,64.7648018577684));
#175326=CARTESIAN_POINT('Ctrl Pts',(4.03866740606205,7.06417368211481,64.7454453496932));
#175327=CARTESIAN_POINT('Ctrl Pts',(4.43308363825827,6.80942894844569,64.7266367975115));
#175328=CARTESIAN_POINT('Ctrl Pts',(4.45771115355224,6.79333235257426,64.7254656118682));
#175329=CARTESIAN_POINT('Ctrl Pts',(4.49175698062641,6.77081506781141,64.7238502475973));
#175330=CARTESIAN_POINT('Ctrl Pts',(4.50124982769582,6.76450792341948,64.7234002464539));
#175331=CARTESIAN_POINT('Ctrl Pts',(4.51641850197298,6.75438363300913,64.7226817825234));
#175332=CARTESIAN_POINT('Ctrl Pts',(4.52210281269807,6.7505792713384,64.7224126794892));
#175333=CARTESIAN_POINT('Ctrl Pts',(4.53380568988196,6.74272542448886,64.721858911851));
#175334=CARTESIAN_POINT('Ctrl Pts',(4.53982365151768,6.73867504760398,64.7215742917754));
#175335=CARTESIAN_POINT('Ctrl Pts',(4.55378358990197,6.7292521514178,64.7209143694076));
#175336=CARTESIAN_POINT('Ctrl Pts',(4.56172150688043,6.72387361538723,64.7205393602484));
#175337=CARTESIAN_POINT('Ctrl Pts',(4.57835700324922,6.71255879673595,64.7197539110081));
#175338=CARTESIAN_POINT('Ctrl Pts',(4.58705260508955,6.70661962901463,64.7193436092958));
#175339=CARTESIAN_POINT('Ctrl Pts',(4.6383984918679,6.67140338926205,64.7169222675484));
#175340=CARTESIAN_POINT('Ctrl Pts',(4.68078048878368,6.64173606134519,64.7149294048499));
#175341=CARTESIAN_POINT('Ctrl Pts',(4.86677868482135,6.50887293516043,64.7061963888022));
#175342=CARTESIAN_POINT('Ctrl Pts',(5.00729134661894,6.40140601812458,64.6996321227779));
#175343=CARTESIAN_POINT('Ctrl Pts',(5.48888260889117,6.00750803362267,64.6768818301142));
#175344=CARTESIAN_POINT('Ctrl Pts',(5.80982237052869,5.69771614418732,64.6611970011749));
#175345=CARTESIAN_POINT('Ctrl Pts',(6.24265027949436,5.20512022940595,64.6375007784001));
#175346=CARTESIAN_POINT('Ctrl Pts',(6.37533831363412,5.04172766620706,64.6298269637827));
#175347=CARTESIAN_POINT('Ctrl Pts',(6.7672236856133,4.51891595382675,64.6056555662988));
#175348=CARTESIAN_POINT('Ctrl Pts',(7.00347298490783,4.1433382764389,64.5887815533345));
#175349=CARTESIAN_POINT('Ctrl Pts',(7.25983449841712,3.65063540870118,64.5673172911544));
#175350=CARTESIAN_POINT('Ctrl Pts',(7.30966788503088,3.549801535146,64.5629553586286));
#175351=CARTESIAN_POINT('Ctrl Pts',(7.37831507482546,3.403319750806,64.5566533604685));
#175352=CARTESIAN_POINT('Ctrl Pts',(7.39883139843843,3.35848367256796,64.554728999357));
#175353=CARTESIAN_POINT('Ctrl Pts',(7.43439306359846,3.27886010707587,64.551318836131));
#175354=CARTESIAN_POINT('Ctrl Pts',(7.44960550853401,3.24414882208678,64.5498346224841));
#175355=CARTESIAN_POINT('Ctrl Pts',(7.47836546326555,3.17725614963081,64.5469786441879));
#175356=CARTESIAN_POINT('Ctrl Pts',(7.49194948211848,3.145091348337,64.5456072525477));
#175357=CARTESIAN_POINT('Ctrl Pts',(7.52071459765309,3.07573617509593,64.5426539458711));
#175358=CARTESIAN_POINT('Ctrl Pts',(7.53582807019887,3.0385187770293,64.5410714420403));
#175359=CARTESIAN_POINT('Ctrl Pts',(7.57175603477389,2.94812798647438,64.5372330910199));
#175360=CARTESIAN_POINT('Ctrl Pts',(7.59228714338808,2.8948443758837,64.5349747086733));
#175361=CARTESIAN_POINT('Ctrl Pts',(7.7769340225401,2.40015713159284,64.514042895066));
#175362=CARTESIAN_POINT('Ctrl Pts',(7.90294210862582,1.94549302343782,64.4950225567952));
#175363=CARTESIAN_POINT('Ctrl Pts',(7.99033216260217,1.47456587650895,64.4755584402205));
#175364=CARTESIAN_POINT('Ctrl Pts',(7.99179170308602,1.46663491276828,64.4752307202717));
#175365=CARTESIAN_POINT('Ctrl Pts',(8.02475806137802,1.28598935728686,64.4677679779035));
#175366=CARTESIAN_POINT('Ctrl Pts',(8.05067070566752,1.1123003414602,64.4606297618435));
#175367=CARTESIAN_POINT('Ctrl Pts',(8.09853278855276,0.700435081823796,
64.4438321144453));
#175368=CARTESIAN_POINT('Ctrl Pts',(8.11563527370661,0.461855513389096,
64.4342021022195));
#175369=CARTESIAN_POINT('Ctrl Pts',(8.12324142796484,0.184654997777823,
64.4232056083949));
#175370=CARTESIAN_POINT('Ctrl Pts',(8.1240202554274,0.146436607636499,64.4216937683884));
#175371=CARTESIAN_POINT('Ctrl Pts',(8.12479443884191,0.0883121799698593,
64.4194014691192));
#175372=CARTESIAN_POINT('Ctrl Pts',(8.12498639216542,0.0684094130669633,
64.4186177988583));
#175373=CARTESIAN_POINT('Ctrl Pts',(8.12516785655924,0.0380128452778828,
64.4174228851264));
#175374=CARTESIAN_POINT('Ctrl Pts',(8.12521017267948,0.0275195205149921,
64.417010732583));
#175375=CARTESIAN_POINT('Ctrl Pts',(8.12524185021268,0.0124023266316113,
64.4164174421896));
#175376=CARTESIAN_POINT('Ctrl Pts',(8.12524759234423,0.00777851422042358,
64.4162360399775));
#175377=CARTESIAN_POINT('Ctrl Pts',(8.12524938758068,0.00315469804922955,
64.4160547003486));
#175378=CARTESIAN_POINT('',(8.12524999535401,-0.000274771867375941,60.4167025044555));
#175379=CARTESIAN_POINT('Ctrl Pts',(8.12524938756529,0.0031547376877246,
64.4160547019031));
#175380=CARTESIAN_POINT('Ctrl Pts',(8.12525204940757,-0.00370102481534387,
64.4157858284478));
#175381=CARTESIAN_POINT('Ctrl Pts',(8.12524603432191,-0.0105567958430449,
64.4155170925646));
#175382=CARTESIAN_POINT('Ctrl Pts',(8.12519813422269,-0.0329084438924019,
64.4146413753845));
#175383=CARTESIAN_POINT('Ctrl Pts',(8.12512059715649,-0.048404228318903,
64.4140349442452));
#175384=CARTESIAN_POINT('Ctrl Pts',(8.12471932175839,-0.0994273318824331,
64.4120401975096));
#175385=CARTESIAN_POINT('Ctrl Pts',(8.12420689032392,-0.13495285100877,
64.410654606361));
#175386=CARTESIAN_POINT('Ctrl Pts',(8.11947477656758,-0.360448517205846,
64.4018763343925));
#175387=CARTESIAN_POINT('Ctrl Pts',(8.10882517728109,-0.550226757232409,
64.3945617889879));
#175388=CARTESIAN_POINT('Ctrl Pts',(8.07513697308051,-0.918860305201467,
64.3803278025321));
#175389=CARTESIAN_POINT('Ctrl Pts',(8.05278017884501,-1.09766688401897,
64.3734116579737));
#175390=CARTESIAN_POINT('Ctrl Pts',(8.00415582295705,-1.40355555064036,
64.3614663920084));
#175391=CARTESIAN_POINT('Ctrl Pts',(7.98075471087268,-1.53102334966457,
64.356454671678));
#175392=CARTESIAN_POINT('Ctrl Pts',(7.94632772561076,-1.69620039633607,
64.349898106299));
#175393=CARTESIAN_POINT('Ctrl Pts',(7.93806317250455,-1.73446624753435,
64.348374831546));
#175394=CARTESIAN_POINT('Ctrl Pts',(7.9223281029886,-1.80485246180425,64.3455643941418));
#175395=CARTESIAN_POINT('Ctrl Pts',(7.91493795418629,-1.8369899710248,64.3442778938508));
#175396=CARTESIAN_POINT('Ctrl Pts',(7.89925646041881,-1.90333223292204,
64.3416150432594));
#175397=CARTESIAN_POINT('Ctrl Pts',(7.89093810213413,-1.93752989000181,
64.3402384993482));
#175398=CARTESIAN_POINT('Ctrl Pts',(7.87144005493255,-2.01547963905902,
64.3370915458013));
#175399=CARTESIAN_POINT('Ctrl Pts',(7.86011729518225,-2.05919469662068,
64.33531999881));
#175400=CARTESIAN_POINT('Ctrl Pts',(7.82290836486081,-2.19807138964046,
64.3296699459717));
#175401=CARTESIAN_POINT('Ctrl Pts',(7.79565398966512,-2.29285668554399,
64.3257804125679));
#175402=CARTESIAN_POINT('Ctrl Pts',(7.67686491772103,-2.67934590069931,
64.309779680942));
#175403=CARTESIAN_POINT('Ctrl Pts',(7.57062835689682,-2.9662656681853,64.2975559304686));
#175404=CARTESIAN_POINT('Ctrl Pts',(7.39952224714856,-3.35883482445798,
64.2804585812234));
#175405=CARTESIAN_POINT('Ctrl Pts',(7.3480301193725,-3.47003667282726,64.2755736441374));
#175406=CARTESIAN_POINT('Ctrl Pts',(7.27227122521564,-3.62438965903496,
64.2687520887739));
#175407=CARTESIAN_POINT('Ctrl Pts',(7.25009545692704,-3.66854808821287,
64.2667957655264));
#175408=CARTESIAN_POINT('Ctrl Pts',(7.21499875400296,-3.736874538536,64.2637629173039));
#175409=CARTESIAN_POINT('Ctrl Pts',(7.20235608084728,-3.76118401961452,
64.2626827218337));
#175410=CARTESIAN_POINT('Ctrl Pts',(7.18075844045299,-3.80220399056128,
64.2608583554564));
#175411=CARTESIAN_POINT('Ctrl Pts',(7.17186752600412,-3.81894791253493,
64.260113203913));
#175412=CARTESIAN_POINT('Ctrl Pts',(7.15407559281999,-3.85217352162106,
64.2586337764102));
#175413=CARTESIAN_POINT('Ctrl Pts',(7.14517602069198,-3.86865584725983,
64.2578994780146));
#175414=CARTESIAN_POINT('Ctrl Pts',(7.12714118232302,-3.90178249117635,
64.2564227114513));
#175415=CARTESIAN_POINT('Ctrl Pts',(7.11800441306719,-3.91842585988836,
64.2556802726238));
#175416=CARTESIAN_POINT('Ctrl Pts',(7.09571828303957,-3.95868668763129,
64.2538829126784));
#175417=CARTESIAN_POINT('Ctrl Pts',(7.08250922400596,-3.98227087752909,
64.2528288918872));
#175418=CARTESIAN_POINT('Ctrl Pts',(7.03118857839778,-4.0728385636086,64.248775921879));
#175419=CARTESIAN_POINT('Ctrl Pts',(6.99224224111277,-4.13934479879885,
64.2457884052512));
#175420=CARTESIAN_POINT('Ctrl Pts',(6.7339240821858,-4.5664071052158,64.2264978092489));
#175421=CARTESIAN_POINT('Ctrl Pts',(6.48768755617069,-4.90996159105387,
64.2104504594844));
#175422=CARTESIAN_POINT('Ctrl Pts',(6.12907874093593,-5.33593916333049,
64.1890069140588));
#175423=CARTESIAN_POINT('Ctrl Pts',(6.03972662018785,-5.4368699595074,64.1838019477991));
#175424=CARTESIAN_POINT('Ctrl Pts',(5.9267833840165,-5.55822701518685,64.1773740221034));
#175425=CARTESIAN_POINT('Ctrl Pts',(5.90553117334658,-5.58080194855463,
64.1761708503687));
#175426=CARTESIAN_POINT('Ctrl Pts',(5.87193317930073,-5.61608423694732,
64.1742785014447));
#175427=CARTESIAN_POINT('Ctrl Pts',(5.85967413836101,-5.62887381364428,
64.1735900494471));
#175428=CARTESIAN_POINT('Ctrl Pts',(5.83991486298699,-5.6493537104712,64.1724835967761));
#175429=CARTESIAN_POINT('Ctrl Pts',(5.8324410301001,-5.65706943418077,64.1720658179839));
#175430=CARTESIAN_POINT('Ctrl Pts',(5.82071279407045,-5.669129307266,64.1714113593207));
#175431=CARTESIAN_POINT('Ctrl Pts',(5.81646877575139,-5.67348354313539,
64.1711747667798));
#175432=CARTESIAN_POINT('Ctrl Pts',(5.80688973725717,-5.68328930491495,
64.170641282479));
#175433=CARTESIAN_POINT('Ctrl Pts',(5.80155192073177,-5.68873808985793,
64.1703443674562));
#175434=CARTESIAN_POINT('Ctrl Pts',(5.79194368959671,-5.69851847923192,
64.1698105616407));
#175435=CARTESIAN_POINT('Ctrl Pts',(5.78767606791372,-5.70285282069132,
64.1695736945061));
#175436=CARTESIAN_POINT('Ctrl Pts',(5.78004590347647,-5.71058488837986,
64.1691506038999));
#175437=CARTESIAN_POINT('Ctrl Pts',(5.77668522135747,-5.71398444756537,
64.168964396173));
#175438=CARTESIAN_POINT('Ctrl Pts',(5.77070977335725,-5.72001836107062,
64.1686335604088));
#175439=CARTESIAN_POINT('Ctrl Pts',(5.76809619847496,-5.72265389346899,
64.168488942439));
#175440=CARTESIAN_POINT('Ctrl Pts',(5.76346984884242,-5.72731272142231,
64.1682331005509));
#175441=CARTESIAN_POINT('Ctrl Pts',(5.76145781210566,-5.72933674929343,
64.1681218828647));
#175442=CARTESIAN_POINT('Ctrl Pts',(5.75790885942168,-5.73290309266949,
64.1679257983797));
#175443=CARTESIAN_POINT('Ctrl Pts',(5.75637238903329,-5.73444585135656,
64.1678409353406));
#175444=CARTESIAN_POINT('Ctrl Pts',(5.71813460267077,-5.77280927939729,
64.1657296901173));
#175445=CARTESIAN_POINT('Ctrl Pts',(5.68108144517901,-5.80927739912985,
64.1637003779826));
#175446=CARTESIAN_POINT('Ctrl Pts',(5.60593469460557,-5.88183106590527,
64.1596171476276));
#175447=CARTESIAN_POINT('Ctrl Pts',(5.56783641332856,-5.91790825709693,
64.1575632710034));
#175448=CARTESIAN_POINT('Ctrl Pts',(5.48305435021858,-5.99664920821727,
64.1530278682194));
#175449=CARTESIAN_POINT('Ctrl Pts',(5.43621650970671,-6.03914205477017,
64.1505452543575));
#175450=CARTESIAN_POINT('Ctrl Pts',(5.27342822128735,-6.18340051557863,
64.1419947395129));
#175451=CARTESIAN_POINT('Ctrl Pts',(5.15507877583407,-6.28240794851399,
64.1359113623838));
#175452=CARTESIAN_POINT('Ctrl Pts',(4.93314086003644,-6.45757794478466,
64.1247504614391));
#175453=CARTESIAN_POINT('Ctrl Pts',(4.83042503823626,-6.53476745256651,
64.1196765853492));
#175454=CARTESIAN_POINT('Ctrl Pts',(4.66299862665205,-6.65448082229071,
64.1115617008048));
#175455=CARTESIAN_POINT('Ctrl Pts',(4.59943550084666,-6.69857181366465,
64.1085155644984));
#175456=CARTESIAN_POINT('Ctrl Pts',(4.50427363148722,-6.7625883056649,64.1040092861141));
#175457=CARTESIAN_POINT('Ctrl Pts',(4.47315155761274,-6.78321433375243,
64.1025439978163));
#175458=CARTESIAN_POINT('Ctrl Pts',(4.40251628902125,-6.82933003919344,
64.099237843005));
#175459=CARTESIAN_POINT('Ctrl Pts',(4.36292177808266,-6.85469270185865,
64.0973980327873));
#175460=CARTESIAN_POINT('Ctrl Pts',(4.19784317407485,-6.958425680721,64.0897784624167));
#175461=CARTESIAN_POINT('Ctrl Pts',(4.07045016611131,-7.03370535256267,
64.084019063757));
#175462=CARTESIAN_POINT('Ctrl Pts',(3.77697888693032,-7.19648029311263,
64.0709534203922));
#175463=CARTESIAN_POINT('Ctrl Pts',(3.60978196664744,-7.28178356681184,
64.0636501735826));
#175464=CARTESIAN_POINT('Ctrl Pts',(3.3913140943643,-7.38387015225066,64.0542255174533));
#175465=CARTESIAN_POINT('Ctrl Pts',(3.34262320686156,-7.40603941313536,
64.0521324573302));
#175466=CARTESIAN_POINT('Ctrl Pts',(3.24877503240178,-7.44765501977847,
64.0481109177716));
#175467=CARTESIAN_POINT('Ctrl Pts',(3.20365318231655,-7.4671755553558,64.0461829345451));
#175468=CARTESIAN_POINT('Ctrl Pts',(3.09936060646691,-7.51117510599718,
64.0417381805705));
#175469=CARTESIAN_POINT('Ctrl Pts',(3.04007217246704,-7.53536653291677,
64.0392198491847));
#175470=CARTESIAN_POINT('Ctrl Pts',(2.86206881262391,-7.60555438327485,
64.0316811236387));
#175471=CARTESIAN_POINT('Ctrl Pts',(2.74255294244948,-7.64946392738869,
64.0266483374526));
#175472=CARTESIAN_POINT('Ctrl Pts',(2.25776655844223,-7.81474954326695,
64.0063298713251));
#175473=CARTESIAN_POINT('Ctrl Pts',(1.8851152814601,-7.91291066159002,63.9909038048653));
#175474=CARTESIAN_POINT('Ctrl Pts',(1.37368334320369,-8.00943604647141,
63.9700926781856));
#175475=CARTESIAN_POINT('Ctrl Pts',(1.23983811073659,-8.03124358790862,
63.9646816320136));
#175476=CARTESIAN_POINT('Ctrl Pts',(1.05048490881522,-8.05724852629485,
63.957093360949));
#175477=CARTESIAN_POINT('Ctrl Pts',(0.995384196476443,-8.06424098776294,
63.9548931929893));
#175478=CARTESIAN_POINT('Ctrl Pts',(0.909396319193509,-8.07425839542534,
63.9514737343896));
#175479=CARTESIAN_POINT('Ctrl Pts',(0.878556319360719,-8.07767225787237,
63.9502501359119));
#175480=CARTESIAN_POINT('Ctrl Pts',(0.826275490750182,-8.08315658179095,
63.9481809433575));
#175481=CARTESIAN_POINT('Ctrl Pts',(0.804844644263694,-8.08531858461841,
63.9473341902665));
#175482=CARTESIAN_POINT('Ctrl Pts',(0.764802366292209,-8.08919737820714,
63.9457549088741));
#175483=CARTESIAN_POINT('Ctrl Pts',(0.746193122989615,-8.09093521843988,
63.9450220930727));
#175484=CARTESIAN_POINT('Ctrl Pts',(0.707759744308294,-8.0943906284182,
63.9435110663978));
#175485=CARTESIAN_POINT('Ctrl Pts',(0.687934940217948,-8.09609961794608,
63.942732987854));
#175486=CARTESIAN_POINT('Ctrl Pts',(0.643666690664774,-8.09975197157235,
63.9409986803755));
#175487=CARTESIAN_POINT('Ctrl Pts',(0.619220314132326,-8.10165754759993,
63.9400430471894));
#175488=CARTESIAN_POINT('Ctrl Pts',(0.52066865764252,-8.10889090127148,
63.9361981806767));
#175489=CARTESIAN_POINT('Ctrl Pts',(0.446500092807692,-8.11331284414584,
63.9333218985643));
#175490=CARTESIAN_POINT('Ctrl Pts',(0.125294502595008,-8.12804524212464,
63.9209153883458));
#175491=CARTESIAN_POINT('Ctrl Pts',(-0.122082025730928,-8.12809424394012,
63.9114834068664));
#175492=CARTESIAN_POINT('Ctrl Pts',(-0.531230597173478,-8.10949011156463,
63.8958015585012));
#175493=CARTESIAN_POINT('Ctrl Pts',(-0.69312617299227,-8.09725949964694,
63.8895763427644));
#175494=CARTESIAN_POINT('Ctrl Pts',(-0.928650146515136,-8.0723509178624,
63.8804424902982));
#175495=CARTESIAN_POINT('Ctrl Pts',(-1.00264285739792,-8.06349475420231,
63.8775619364667));
#175496=CARTESIAN_POINT('Ctrl Pts',(-1.13618574810246,-8.04564448522457,
63.872339003689));
#175497=CARTESIAN_POINT('Ctrl Pts',(-1.19577776775611,-8.0370037151075,
63.8699996291643));
#175498=CARTESIAN_POINT('Ctrl Pts',(-1.2878575355839,-8.02260547297953,
63.8663700168485));
#175499=CARTESIAN_POINT('Ctrl Pts',(-1.32041564458816,-8.01731115299748,
63.865083751183));
#175500=CARTESIAN_POINT('Ctrl Pts',(-1.38473825371414,-8.00644911668935,
63.8625366319962));
#175501=CARTESIAN_POINT('Ctrl Pts',(-1.41650364793955,-8.0008902565102,
63.8612758761062));
#175502=CARTESIAN_POINT('Ctrl Pts',(-1.48996925976643,-7.98758274206336,
63.8583531952647));
#175503=CARTESIAN_POINT('Ctrl Pts',(-1.53164353265685,-7.97969639315823,
63.8566901354077));
#175504=CARTESIAN_POINT('Ctrl Pts',(-1.65263821544259,-7.95581685323283,
63.8518463519944));
#175505=CARTESIAN_POINT('Ctrl Pts',(-1.7317835384288,-7.93896470136714,
63.848658628572));
#175506=CARTESIAN_POINT('Ctrl Pts',(-2.09291836372321,-7.85641209705464,
63.8340232325431));
#175507=CARTESIAN_POINT('Ctrl Pts',(-2.37152029756464,-7.77685068071387,
63.8224691814695));
#175508=CARTESIAN_POINT('Ctrl Pts',(-2.79714929864855,-7.63029771565671,
63.8045205684309));
#175509=CARTESIAN_POINT('Ctrl Pts',(-2.9474390112876,-7.57351248576873,
63.7981255740526));
#175510=CARTESIAN_POINT('Ctrl Pts',(-3.12730734936599,-7.49938575999014,
63.790439559224));
#175511=CARTESIAN_POINT('Ctrl Pts',(-3.15858611875411,-7.48626554287471,
63.7891018124664));
#175512=CARTESIAN_POINT('Ctrl Pts',(-3.20612307748125,-7.46597468927721,
63.7870675055553));
#175513=CARTESIAN_POINT('Ctrl Pts',(-3.22244135791033,-7.45894596748951,
63.7863689574048));
#175514=CARTESIAN_POINT('Ctrl Pts',(-3.25468018323636,-7.44493429699319,
63.7849885600082));
#175515=CARTESIAN_POINT('Ctrl Pts',(-3.27060164000678,-7.43795366324794,
63.7843066788492));
#175516=CARTESIAN_POINT('Ctrl Pts',(-3.3078954115363,-7.42145961269543,
63.7827092202604));
#175517=CARTESIAN_POINT('Ctrl Pts',(-3.32924930814989,-7.41190487568663,
63.7817943418073));
#175518=CARTESIAN_POINT('Ctrl Pts',(-3.39697023209044,-7.38125164353628,
63.7788919046525));
#175519=CARTESIAN_POINT('Ctrl Pts',(-3.44318042365743,-7.35980918259458,
63.7769098546716));
#175520=CARTESIAN_POINT('Ctrl Pts',(-3.87464215715951,-7.15464920109376,
63.7583769411999));
#175521=CARTESIAN_POINT('Ctrl Pts',(-4.24506479953309,-6.94127473179555,
63.7422494402626));
#175522=CARTESIAN_POINT('Ctrl Pts',(-4.84852728871508,-6.52721324974982,
63.714449338336));
#175523=CARTESIAN_POINT('Ctrl Pts',(-5.09012257526372,-6.34061343858149,
63.7028440259401));
#175524=CARTESIAN_POINT('Ctrl Pts',(-5.41118586621761,-6.06243388068201,
63.6865064216333));
#175525=CARTESIAN_POINT('Ctrl Pts',(-5.49997353340321,-5.98200032070825,
63.6818830476362));
#175526=CARTESIAN_POINT('Ctrl Pts',(-5.65288329967631,-5.83719485623575,
63.6737206436038));
#175527=CARTESIAN_POINT('Ctrl Pts',(-5.71776503104696,-5.77365536606747,
63.6701905117093));
#175528=CARTESIAN_POINT('Ctrl Pts',(-5.80803529048837,-5.68223834361919,
63.6651802468827));
#175529=CARTESIAN_POINT('Ctrl Pts',(-5.83431600503003,-5.65525094684929,
63.6637093804543));
#175530=CARTESIAN_POINT('Ctrl Pts',(-5.88694846925146,-5.60044582380717,
63.6607386431695));
#175531=CARTESIAN_POINT('Ctrl Pts',(-5.91329301984136,-5.5726224845497,
63.6592387453951));
#175532=CARTESIAN_POINT('Ctrl Pts',(-5.96358378557714,-5.51875056893912,
63.656350253589));
#175533=CARTESIAN_POINT('Ctrl Pts',(-5.98755861018893,-5.49272985779891,
63.6549619646227));
#175534=CARTESIAN_POINT('Ctrl Pts',(-6.04404719283613,-5.43061149356175,
63.6516638397119));
#175535=CARTESIAN_POINT('Ctrl Pts',(-6.07640863765134,-5.39437723100798,
63.6497527156917));
#175536=CARTESIAN_POINT('Ctrl Pts',(-6.17476433658124,-5.28224276866908,
63.6438766874999));
#175537=CARTESIAN_POINT('Ctrl Pts',(-6.23967564193039,-5.20540593989818,
63.6399033600526));
#175538=CARTESIAN_POINT('Ctrl Pts',(-6.56490242714283,-4.80560147872492,
63.6194947523112));
#175539=CARTESIAN_POINT('Ctrl Pts',(-6.80162929359192,-4.46425539471723,
63.6029886710398));
#175540=CARTESIAN_POINT('Ctrl Pts',(-7.20251664628805,-3.77977075460938,
63.5705558172725));
#175541=CARTESIAN_POINT('Ctrl Pts',(-7.37072190454711,-3.44025474152612,
63.5547351218701));
#175542=CARTESIAN_POINT('Ctrl Pts',(-7.66828907220903,-2.71665612943567,
63.5216660775127));
#175543=CARTESIAN_POINT('Ctrl Pts',(-7.7938542466089,-2.33210619624823,
63.504436103179));
#175544=CARTESIAN_POINT('Ctrl Pts',(-7.91927117879069,-1.82196566220897,
63.482861504689));
#175545=CARTESIAN_POINT('Ctrl Pts',(-7.94560058857013,-1.70348105245745,
63.4779417661207));
#175546=CARTESIAN_POINT('Ctrl Pts',(-7.9732636753246,-1.56434461232731,
63.4723022967545));
#175547=CARTESIAN_POINT('Ctrl Pts',(-7.97718464863456,-1.54422562895212,
63.4714901912393));
#175548=CARTESIAN_POINT('Ctrl Pts',(-7.98284803600176,-1.51456884711066,
63.4702982397127));
#175549=CARTESIAN_POINT('Ctrl Pts',(-7.9846495614056,-1.50504250474424,
63.4699161428485));
#175550=CARTESIAN_POINT('Ctrl Pts',(-7.98777228687909,-1.48836632601237,
63.4692486632953));
#175551=CARTESIAN_POINT('Ctrl Pts',(-7.98910094674253,-1.48121790789082,
63.4689629889867));
#175552=CARTESIAN_POINT('Ctrl Pts',(-7.99165531064304,-1.4673715693478,
63.4684105231899));
#175553=CARTESIAN_POINT('Ctrl Pts',(-7.99288219344804,-1.46067387484599,
63.4681436848806));
#175554=CARTESIAN_POINT('Ctrl Pts',(-7.99578057124931,-1.4447382984189,
63.4675097661155));
#175555=CARTESIAN_POINT('Ctrl Pts',(-7.99744448054419,-1.43549903380843,
63.4671429940331));
#175556=CARTESIAN_POINT('Ctrl Pts',(-8.00239079824824,-1.40775785143915,
63.466044092619));
#175557=CARTESIAN_POINT('Ctrl Pts',(-8.0056250550691,-1.38924732924432,
63.4653139686099));
#175558=CARTESIAN_POINT('Ctrl Pts',(-8.05104951925469,-1.12384394578858,
63.4548918939583));
#175559=CARTESIAN_POINT('Ctrl Pts',(-8.08186510898217,-0.875145046226254,
63.4457563378864));
#175560=CARTESIAN_POINT('Ctrl Pts',(-8.13987571169031,-0.123724830521734,
63.4192581857281));
#175561=CARTESIAN_POINT('Ctrl Pts',(-8.13192134988833,0.380501029881913,
63.4028745511142));
#175562=CARTESIAN_POINT('Ctrl Pts',(-8.01189465542595,1.48125066983262,
63.3656839765176));
#175563=CARTESIAN_POINT('Ctrl Pts',(-7.87967257195023,2.0724918143441,63.3446719436477));
#175564=CARTESIAN_POINT('Ctrl Pts',(-7.67391061298761,2.67050429610845,
63.3203132846228));
#175565=CARTESIAN_POINT('Ctrl Pts',(-7.66451114472503,2.69736282033,63.3192128460829));
#175566=CARTESIAN_POINT('Ctrl Pts',(-7.65062936392473,2.73637087719036,
63.3176051481124));
#175567=CARTESIAN_POINT('Ctrl Pts',(-7.64625874428789,2.74856006942296,
63.3171014259841));
#175568=CARTESIAN_POINT('Ctrl Pts',(-7.63855409512638,2.76988691287619,
63.3162177087356));
#175569=CARTESIAN_POINT('Ctrl Pts',(-7.63523275558756,2.7790291364945,63.3158381166157));
#175570=CARTESIAN_POINT('Ctrl Pts',(-7.62876438297412,2.79673466483496,
63.3151014766595));
#175571=CARTESIAN_POINT('Ctrl Pts',(-7.6256193266851,2.80529867933497,63.3147444919888));
#175572=CARTESIAN_POINT('Ctrl Pts',(-7.61809634583897,2.82567768656041,
63.3138933873048));
#175573=CARTESIAN_POINT('Ctrl Pts',(-7.61370535524593,2.83748781223489,
63.3133988525227));
#175574=CARTESIAN_POINT('Ctrl Pts',(-7.59800515431709,2.87941665499392,
63.3116384943998));
#175575=CARTESIAN_POINT('Ctrl Pts',(-7.58654462174147,2.90947817855706,
63.3103678597336));
#175576=CARTESIAN_POINT('Ctrl Pts',(-7.39731528067532,3.39711511563414,
63.2896165249454));
#175577=CARTESIAN_POINT('Ctrl Pts',(-7.17863979560322,3.83766805284282,
63.2687758373457));
#175578=CARTESIAN_POINT('Ctrl Pts',(-6.64247001345833,4.70969677116121,
63.2235801981561));
#175579=CARTESIAN_POINT('Ctrl Pts',(-6.31939339008014,5.13506570441792,
63.1991886686126));
#175580=CARTESIAN_POINT('Ctrl Pts',(-5.78028346325522,5.71625220931396,
63.1644909113297));
#175581=CARTESIAN_POINT('Ctrl Pts',(-5.59450124224049,5.89820323550877,
63.1534092167543));
#175582=CARTESIAN_POINT('Ctrl Pts',(-5.36818891090053,6.09951490315464,
63.1411744746036));
#175583=CARTESIAN_POINT('Ctrl Pts',(-5.33585423308989,6.12782130460805,
63.1394540399324));
#175584=CARTESIAN_POINT('Ctrl Pts',(-5.29335428758745,6.16443510346981,
63.1372265058798));
#175585=CARTESIAN_POINT('Ctrl Pts',(-5.28339172345201,6.17297591588093,
63.1367067371201));
#175586=CARTESIAN_POINT('Ctrl Pts',(-5.26715767014812,6.1868251267358,63.1358635867649));
#175587=CARTESIAN_POINT('Ctrl Pts',(-5.26089876643083,6.19214819275304,
63.1355394351994));
#175588=CARTESIAN_POINT('Ctrl Pts',(-5.24886217047174,6.20235364170421,
63.1349177944893));
#175589=CARTESIAN_POINT('Ctrl Pts',(-5.2430857156204,6.20723746609683,63.1346202313172));
#175590=CARTESIAN_POINT('Ctrl Pts',(-5.22988143408974,6.21836971905312,
63.1339417676677));
#175591=CARTESIAN_POINT('Ctrl Pts',(-5.22244920631241,6.2246129249912,63.1335611303777));
#175592=CARTESIAN_POINT('Ctrl Pts',(-5.2027880126816,6.24106868252852,63.132557433755));
#175593=CARTESIAN_POINT('Ctrl Pts',(-5.19054013321589,6.25125863604428,
63.1319354840345));
#175594=CARTESIAN_POINT('Ctrl Pts',(-5.11025100102791,6.3176586990242,63.1278794069582));
#175595=CARTESIAN_POINT('Ctrl Pts',(-5.04132635515106,6.37279420225621,
63.1244957924265));
#175596=CARTESIAN_POINT('Ctrl Pts',(-4.54164333825795,6.75932921596949,
63.1005685158073));
#175597=CARTESIAN_POINT('Ctrl Pts',(-4.07946894131787,7.04791161659307,
63.0814870743557));
#175598=CARTESIAN_POINT('Ctrl Pts',(-3.33112898753213,7.41672437088348,
63.0513920394419));
#175599=CARTESIAN_POINT('Ctrl Pts',(-3.06363186422011,7.53116018788785,
63.0407974046997));
#175600=CARTESIAN_POINT('Ctrl Pts',(-2.5706637747521,7.71143353272238,63.0212294327299));
#175601=CARTESIAN_POINT('Ctrl Pts',(-2.34737804935643,7.78230880486546,
63.0123534670956));
#175602=CARTESIAN_POINT('Ctrl Pts',(-2.07726331331589,7.85536443242926,
63.0015620714131));
#175603=CARTESIAN_POINT('Ctrl Pts',(-2.03307852239784,7.86691584566017,
62.9997953163534));
#175604=CARTESIAN_POINT('Ctrl Pts',(-1.96401611110322,7.88435042384482,
62.9970314634466));
#175605=CARTESIAN_POINT('Ctrl Pts',(-1.93920400436303,7.89048976386617,
62.9960380220522));
#175606=CARTESIAN_POINT('Ctrl Pts',(-1.89322872803482,7.90163562009407,
62.9941963931268));
#175607=CARTESIAN_POINT('Ctrl Pts',(-1.87207358696403,7.90667445708102,
62.9933486625261));
#175608=CARTESIAN_POINT('Ctrl Pts',(-1.82689224060276,7.91724447949351,
62.991537419877));
#175609=CARTESIAN_POINT('Ctrl Pts',(-1.80286055595851,7.92275136658977,
62.9905735750719));
#175610=CARTESIAN_POINT('Ctrl Pts',(-1.73832481455643,7.93723097002044,
62.9879837321676));
#175611=CARTESIAN_POINT('Ctrl Pts',(-1.69777660589826,7.94600297002463,
62.9863549419748));
#175612=CARTESIAN_POINT('Ctrl Pts',(-1.51324324699864,7.98444702922659,
62.9789332451494));
#175613=CARTESIAN_POINT('Ctrl Pts',(-1.36853878936757,8.01051806358963,
62.9730875467613));
#175614=CARTESIAN_POINT('Ctrl Pts',(-1.0941736298121,8.05229829755306,62.9619289755147));
#175615=CARTESIAN_POINT('Ctrl Pts',(-0.964685657689746,8.06883537719088,
62.9566316024408));
#175616=CARTESIAN_POINT('Ctrl Pts',(-0.606834356168358,8.10579971070932,
62.9418956805752));
#175617=CARTESIAN_POINT('Ctrl Pts',(-0.377922659050299,8.11969250849721,
62.9323590304124));
#175618=CARTESIAN_POINT('Ctrl Pts',(0.119685701681321,8.12880292136515,
62.9114326169932));
#175619=CARTESIAN_POINT('Ctrl Pts',(0.388183179612827,8.12041085485493,
62.900015800063));
#175620=CARTESIAN_POINT('Ctrl Pts',(1.00315989691236,8.07061522847358,62.8738589285822));
#175621=CARTESIAN_POINT('Ctrl Pts',(1.34839545407884,8.02016251701541,62.8591632117109));
#175622=CARTESIAN_POINT('Ctrl Pts',(1.72017800583175,7.94113780508695,62.8438598016724));
#175623=CARTESIAN_POINT('Ctrl Pts',(1.7509855809573,7.93440177558938,62.8425958151784));
#175624=CARTESIAN_POINT('Ctrl Pts',(1.80443779045928,7.92238804902876,62.8404107099278));
#175625=CARTESIAN_POINT('Ctrl Pts',(1.82710034318673,7.91719220985915,62.839486766264));
#175626=CARTESIAN_POINT('Ctrl Pts',(1.85977389630223,7.90955338754597,62.8381585456323));
#175627=CARTESIAN_POINT('Ctrl Pts',(1.86980293496711,7.9071885472248,62.8377513796489));
#175628=CARTESIAN_POINT('Ctrl Pts',(1.88725282252336,7.90303882062074,62.837043882874));
#175629=CARTESIAN_POINT('Ctrl Pts',(1.89467569426125,7.90126254660898,62.836743224662));
#175630=CARTESIAN_POINT('Ctrl Pts',(1.90897917882951,7.89781844444394,62.836164460185));
#175631=CARTESIAN_POINT('Ctrl Pts',(1.91586013372285,7.89615207775169,62.8358862974823));
#175632=CARTESIAN_POINT('Ctrl Pts',(1.93212057916416,7.89219176570665,62.8352296023997));
#175633=CARTESIAN_POINT('Ctrl Pts',(1.94149818815987,7.88989008703565,62.8348513766385));
#175634=CARTESIAN_POINT('Ctrl Pts',(1.96932747033105,7.88300693451832,62.8337304643152));
#175635=CARTESIAN_POINT('Ctrl Pts',(1.98776726804379,7.87837739075315,62.8329897314686));
#175636=CARTESIAN_POINT('Ctrl Pts',(2.22054577885077,7.81906612739816,62.8236654189386));
#175637=CARTESIAN_POINT('Ctrl Pts',(2.4325736746376,7.75572063302635,62.8155031024213));
#175638=CARTESIAN_POINT('Ctrl Pts',(3.11200976243386,7.52212474382858,62.789897959343));
#175639=CARTESIAN_POINT('Ctrl Pts',(3.56644896326103,7.31761251325884,62.7735395429903));
#175640=CARTESIAN_POINT('Ctrl Pts',(4.49196538899508,6.79427659383245,62.7376094089114));
#175641=CARTESIAN_POINT('Ctrl Pts',(4.9540993098378,6.46504235961165,62.7179404884031));
#175642=CARTESIAN_POINT('Ctrl Pts',(5.41923087030591,6.05430540045263,62.6942711520381));
#175643=CARTESIAN_POINT('Ctrl Pts',(5.45984842508369,6.01770156678796,62.6921695839031));
#175644=CARTESIAN_POINT('Ctrl Pts',(5.5124295755443,5.96934574661173,62.6894024422877));
#175645=CARTESIAN_POINT('Ctrl Pts',(5.52473097594945,5.95796241237925,62.6887516879447));
#175646=CARTESIAN_POINT('Ctrl Pts',(5.54468630420597,5.93938142713052,62.6876904933898));
#175647=CARTESIAN_POINT('Ctrl Pts',(5.55236167238611,5.93220682436324,62.6872809865011));
#175648=CARTESIAN_POINT('Ctrl Pts',(5.56708175938493,5.91839352755375,62.6864930289483));
#175649=CARTESIAN_POINT('Ctrl Pts',(5.57412857543158,5.911757089601,62.6861146702385));
#175650=CARTESIAN_POINT('Ctrl Pts',(5.59019569895153,5.89657138224248,62.6852493616479));
#175651=CARTESIAN_POINT('Ctrl Pts',(5.59920827467962,5.88801398720893,62.6847620801637));
#175652=CARTESIAN_POINT('Ctrl Pts',(5.62294822765948,5.86536922460854,62.6834734901238));
#175653=CARTESIAN_POINT('Ctrl Pts',(5.63764225517208,5.85124710701203,62.6826707559272));
#175654=CARTESIAN_POINT('Ctrl Pts',(5.73222596136949,5.75965768359682,62.6774701048535));
#175655=CARTESIAN_POINT('Ctrl Pts',(5.81056812256743,5.68061334685429,62.6730068867596));
#175656=CARTESIAN_POINT('Ctrl Pts',(6.54783702410524,4.90552330799002,62.629457466984));
#175657=CARTESIAN_POINT('Ctrl Pts',(7.08027475571478,4.09967731532907,62.5847303324922));
#175658=CARTESIAN_POINT('Ctrl Pts',(7.56706264271846,2.97191484942539,62.5307991778134));
#175659=CARTESIAN_POINT('Ctrl Pts',(7.66172198382725,2.71859464217452,62.5192544220422));
#175660=CARTESIAN_POINT('Ctrl Pts',(7.75641443257763,2.42064381551627,62.5066462132521));
#175661=CARTESIAN_POINT('Ctrl Pts',(7.76892684435691,2.3801800605182,62.5049539791719));
#175662=CARTESIAN_POINT('Ctrl Pts',(7.78477544105883,2.32747069559257,62.5027734304126));
#175663=CARTESIAN_POINT('Ctrl Pts',(7.7883999663594,2.31531303998063,62.5022721169757));
#175664=CARTESIAN_POINT('Ctrl Pts',(7.79423145439123,2.29558397642976,62.5014611869925));
#175665=CARTESIAN_POINT('Ctrl Pts',(7.79645588507414,2.28801778623926,62.5011508072324));
#175666=CARTESIAN_POINT('Ctrl Pts',(7.80069628430694,2.27351648376464,62.5005570946048));
#175667=CARTESIAN_POINT('Ctrl Pts',(7.80271402817571,2.26658190165376,62.5002736858765));
#175668=CARTESIAN_POINT('Ctrl Pts',(7.80732801053588,2.25064539035918,62.4996235240274));
#175669=CARTESIAN_POINT('Ctrl Pts',(7.80991793351598,2.24164163280765,62.4992570367442));
#175670=CARTESIAN_POINT('Ctrl Pts',(7.8178953759522,2.21372674641611,62.4981233384743));
#175671=CARTESIAN_POINT('Ctrl Pts',(7.82322984634526,2.1948004457798,62.4973583053059));
#175672=CARTESIAN_POINT('Ctrl Pts',(7.86655399893867,2.03892472871585,62.4910859259758));
#175673=CARTESIAN_POINT('Ctrl Pts',(7.90101451191266,1.90101500873938,62.4857160076361));
#175674=CARTESIAN_POINT('Ctrl Pts',(8.06032380931102,1.18397563950439,62.4584198726444));
#175675=CARTESIAN_POINT('Ctrl Pts',(8.12518544520022,0.593344303021297,
62.4378250394779));
#175676=CARTESIAN_POINT('Ctrl Pts',(8.12531225746491,-0.571359736175462,
62.3954537244734));
#175677=CARTESIAN_POINT('Ctrl Pts',(8.06492182068399,-1.14198041541291,
62.3738694867536));
#175678=CARTESIAN_POINT('Ctrl Pts',(7.9202586513955,-1.81748889944684,62.3471936005567));
#175679=CARTESIAN_POINT('Ctrl Pts',(7.89287697418633,-1.93293965873061,
62.34259541739));
#175680=CARTESIAN_POINT('Ctrl Pts',(7.8511016152355,-2.09334933675133,62.3361410732562));
#175681=CARTESIAN_POINT('Ctrl Pts',(7.83882943857648,-2.1388457230221,62.3343030290089));
#175682=CARTESIAN_POINT('Ctrl Pts',(7.81580821770263,-2.22133135436604,
62.3309563601047));
#175683=CARTESIAN_POINT('Ctrl Pts',(7.80519056780994,-2.25835587721572,
62.3294489165132));
#175684=CARTESIAN_POINT('Ctrl Pts',(7.78322840658023,-2.33293420686602,
62.3264014384356));
#175685=CARTESIAN_POINT('Ctrl Pts',(7.7718743741075,-2.37048415745722,62.3248613568242));
#175686=CARTESIAN_POINT('Ctrl Pts',(7.74317078945072,-2.46298895674056,
62.3210527992961));
#175687=CARTESIAN_POINT('Ctrl Pts',(7.72550770352769,-2.51784414738833,
62.3187815840866));
#175688=CARTESIAN_POINT('Ctrl Pts',(7.65531858141025,-2.72813165456218,
62.3100236453473));
#175689=CARTESIAN_POINT('Ctrl Pts',(7.59867342313778,-2.8821460828094,62.3035005081099));
#175690=CARTESIAN_POINT('Ctrl Pts',(7.38599250098703,-3.41045312062028,
62.2807167141194));
#175691=CARTESIAN_POINT('Ctrl Pts',(7.2066420450918,-3.77470215026916,62.264263832392));
#175692=CARTESIAN_POINT('Ctrl Pts',(6.92298713874376,-4.25622794409802,
62.2415507475766));
#175693=CARTESIAN_POINT('Ctrl Pts',(6.84138542441196,-4.38619117662682,
62.2353188670386));
#175694=CARTESIAN_POINT('Ctrl Pts',(6.65387746531277,-4.66685090764606,
62.2216618800794));
#175695=CARTESIAN_POINT('Ctrl Pts',(6.54642724378459,-4.81641721516844,
62.2142511119096));
#175696=CARTESIAN_POINT('Ctrl Pts',(6.39921731363512,-5.00728937323294,
62.2046551407293));
#175697=CARTESIAN_POINT('Ctrl Pts',(6.36397352008132,-5.05200655279165,
62.2023966849957));
#175698=CARTESIAN_POINT('Ctrl Pts',(6.31415493373948,-5.11386751144847,
62.1992592772701));
#175699=CARTESIAN_POINT('Ctrl Pts',(6.29997471125366,-5.13132654339272,
62.198372328782));
#175700=CARTESIAN_POINT('Ctrl Pts',(6.27389841592312,-5.16316127890511,
62.1967524778462));
#175701=CARTESIAN_POINT('Ctrl Pts',(6.26202500489671,-5.17755526910597,
62.1960191066999));
#175702=CARTESIAN_POINT('Ctrl Pts',(6.23694484477089,-5.20774716648288,
62.1944786360966));
#175703=CARTESIAN_POINT('Ctrl Pts',(6.22372740342606,-5.22353603974208,
62.1936717627748));
#175704=CARTESIAN_POINT('Ctrl Pts',(6.18831232026624,-5.26551582220743,
62.1915226459226));
#175705=CARTESIAN_POINT('Ctrl Pts',(6.16600841098385,-5.29161662809608,
62.1901824797457));
#175706=CARTESIAN_POINT('Ctrl Pts',(6.02934098069599,-5.4495122330022,62.1820473844686));
#175707=CARTESIAN_POINT('Ctrl Pts',(5.91092053211543,-5.57773752900278,
62.1753208757816));
#175708=CARTESIAN_POINT('Ctrl Pts',(5.56831406656756,-5.92553598374877,
62.1565383245833));
#175709=CARTESIAN_POINT('Ctrl Pts',(5.33540944962258,-6.13608205130694,
62.144516491761));
#175710=CARTESIAN_POINT('Ctrl Pts',(5.04423671565151,-6.37016097234567,
62.1300179431059));
#175711=CARTESIAN_POINT('Ctrl Pts',(4.99714332621086,-6.40717046669309,
62.1276890158747));
#175712=CARTESIAN_POINT('Ctrl Pts',(4.9226796036295,-6.46436920916488,62.124029815501));
#175713=CARTESIAN_POINT('Ctrl Pts',(4.8955842930863,-6.48491311991678,62.1227030830682));
#175714=CARTESIAN_POINT('Ctrl Pts',(4.84004767897333,-6.52647505380922,
62.1199930452544));
#175715=CARTESIAN_POINT('Ctrl Pts',(4.81159651055969,-6.54747868817897,
62.1186096301913));
#175716=CARTESIAN_POINT('Ctrl Pts',(4.74534694402768,-6.59572138182043,
62.1153993321513));
#175717=CARTESIAN_POINT('Ctrl Pts',(4.70744961659883,-6.62282237793359,
62.1135711378423));
#175718=CARTESIAN_POINT('Ctrl Pts',(4.58131145250874,-6.71139612614134,
62.1075123800936));
#175719=CARTESIAN_POINT('Ctrl Pts',(4.49208381136442,-6.7714426340591,62.103268355296));
#175720=CARTESIAN_POINT('Ctrl Pts',(4.26676196698893,-6.91666089700728,
62.0926514134573));
#175721=CARTESIAN_POINT('Ctrl Pts',(4.12928627651811,-6.99960354903399,
62.086261571181));
#175722=CARTESIAN_POINT('Ctrl Pts',(3.78279343433746,-7.19488927112636,
62.0703891672577));
#175723=CARTESIAN_POINT('Ctrl Pts',(3.57114030165288,-7.30225411112304,
62.0608924530032));
#175724=CARTESIAN_POINT('Ctrl Pts',(3.27815767084971,-7.43508612343448,
62.0481123647284));
#175725=CARTESIAN_POINT('Ctrl Pts',(3.20068201581274,-7.46876550654912,
62.0447668893427));
#175726=CARTESIAN_POINT('Ctrl Pts',(3.09898395766114,-7.51110149238733,
62.0404263355929));
#175727=CARTESIAN_POINT('Ctrl Pts',(3.07522632662997,-7.5208596746376,62.0394159295113));
#175728=CARTESIAN_POINT('Ctrl Pts',(3.0346935048254,-7.53728390835473,62.037698452646));
#175729=CARTESIAN_POINT('Ctrl Pts',(3.01794169170144,-7.54400698103875,
62.0369904960387));
#175730=CARTESIAN_POINT('Ctrl Pts',(2.98196926235409,-7.55830494789312,
62.0354740970303));
#175731=CARTESIAN_POINT('Ctrl Pts',(2.96274185863672,-7.5658624788938,62.0346659207762));
#175732=CARTESIAN_POINT('Ctrl Pts',(2.91502799716843,-7.58440713042021,
62.032665931966));
#175733=CARTESIAN_POINT('Ctrl Pts',(2.88650799762047,-7.59530719155618,
62.0314753589515));
#175734=CARTESIAN_POINT('Ctrl Pts',(2.77617384271997,-7.63676460149921,
62.0268869698048));
#175735=CARTESIAN_POINT('Ctrl Pts',(2.69393005716837,-7.66616304398773,
62.0235037932779));
#175736=CARTESIAN_POINT('Ctrl Pts',(2.53324846378231,-7.72069432954278,
62.0169513329304));
#175737=CARTESIAN_POINT('Ctrl Pts',(2.45487094351724,-7.74597169227038,
62.0137812529695));
#175738=CARTESIAN_POINT('Ctrl Pts',(2.12872368156943,-7.8457092115773,62.0006739371023));
#175739=CARTESIAN_POINT('Ctrl Pts',(1.87785249931966,-7.90950617504113,
61.9907871897118));
#175740=CARTESIAN_POINT('Ctrl Pts',(1.3714804935247,-8.01282360825074,61.9709363988586));
#175741=CARTESIAN_POINT('Ctrl Pts',(1.1162828344953,-8.05234197028682,61.9609835006251));
#175742=CARTESIAN_POINT('Ctrl Pts',(0.78095028817407,-8.0880199317794,61.9478681832114));
#175743=CARTESIAN_POINT('Ctrl Pts',(0.702142483920749,-8.09524215925793,
61.9447836955023));
#175744=CARTESIAN_POINT('Ctrl Pts',(0.568260862463784,-8.10554180646614,
61.9395380810763));
#175745=CARTESIAN_POINT('Ctrl Pts',(0.513238168799655,-8.10921173352463,
61.9373806566744));
#175746=CARTESIAN_POINT('Ctrl Pts',(0.398391891898013,-8.11569823152074,
61.9328738532247));
#175747=CARTESIAN_POINT('Ctrl Pts',(0.338565899703413,-8.11841406833795,
61.9305240581155));
#175748=CARTESIAN_POINT('Ctrl Pts',(0.162614985591844,-8.12445315920515,
61.9236068139472));
#175749=CARTESIAN_POINT('Ctrl Pts',(0.046442743288885,-8.12594767860219,
61.9190313378358));
#175750=CARTESIAN_POINT('Ctrl Pts',(-0.306702637332613,-8.12291729740619,
61.9051017399361));
#175751=CARTESIAN_POINT('Ctrl Pts',(-0.543481870822225,-8.11051660733493,
61.8957308207934));
#175752=CARTESIAN_POINT('Ctrl Pts',(-0.825419238152854,-8.08334769458556,
61.8845899582229));
#175753=CARTESIAN_POINT('Ctrl Pts',(-0.871419998375232,-8.078518061831,
61.8827729047744));
#175754=CARTESIAN_POINT('Ctrl Pts',(-0.959825596665691,-8.06847244073484,
61.8792831720209));
#175755=CARTESIAN_POINT('Ctrl Pts',(-1.00223544949722,-8.06331425764931,
61.8776101989663));
#175756=CARTESIAN_POINT('Ctrl Pts',(-1.14664729274457,-8.0445929449074,
61.8719145879527));
#175757=CARTESIAN_POINT('Ctrl Pts',(-1.24843169712396,-8.02942675979171,
61.8679019667794));
#175758=CARTESIAN_POINT('Ctrl Pts',(-1.54561554432345,-7.97935784802296,
61.8561607164715));
#175759=CARTESIAN_POINT('Ctrl Pts',(-1.74005619463509,-7.93922435869023,
61.8484449843567));
#175760=CARTESIAN_POINT('Ctrl Pts',(-2.01370625907561,-7.87220475345948,
61.8374526241279));
#175761=CARTESIAN_POINT('Ctrl Pts',(-2.09427140311719,-7.85115582589881,
61.8341999260927));
#175762=CARTESIAN_POINT('Ctrl Pts',(-2.22834613981786,-7.81391606660522,
61.8287537009817));
#175763=CARTESIAN_POINT('Ctrl Pts',(-2.28203784649393,-7.7984045840702,
61.8265637382998));
#175764=CARTESIAN_POINT('Ctrl Pts',(-2.39258791821276,-7.76522730340484,
61.8220343642352));
#175765=CARTESIAN_POINT('Ctrl Pts',(-2.4494207461888,-7.74748797961997,
61.8196946682721));
#175766=CARTESIAN_POINT('Ctrl Pts',(-2.60249712413585,-7.69785525494417,
61.8133602274957));
#175767=CARTESIAN_POINT('Ctrl Pts',(-2.69834673310783,-7.6647825500432,
61.8093587108608));
#175768=CARTESIAN_POINT('Ctrl Pts',(-3.12289377704863,-7.50934272681272,
61.7914640469587));
#175769=CARTESIAN_POINT('Ctrl Pts',(-3.44407959679674,-7.36756432997102,
61.7774480702845));
#175770=CARTESIAN_POINT('Ctrl Pts',(-3.98374446877178,-7.08632117156818,
61.7530861434291));
#175771=CARTESIAN_POINT('Ctrl Pts',(-4.20659552217092,-6.95634415889652,
61.7427698769314));
#175772=CARTESIAN_POINT('Ctrl Pts',(-4.46003845374512,-6.791885278389,61.7308234533547));
#175773=CARTESIAN_POINT('Ctrl Pts',(-4.49698930193048,-6.7674763310802,
61.7290762995698));
#175774=CARTESIAN_POINT('Ctrl Pts',(-4.55525181108142,-6.72830146036634,
61.7263137215263));
#175775=CARTESIAN_POINT('Ctrl Pts',(-4.57669543941068,-6.7137335712442,
61.7252952677873));
#175776=CARTESIAN_POINT('Ctrl Pts',(-4.61447452854532,-6.68780295186171,
61.7234982001473));
#175777=CARTESIAN_POINT('Ctrl Pts',(-4.63083863865992,-6.67648238248094,
61.7227188695024));
#175778=CARTESIAN_POINT('Ctrl Pts',(-4.66519472401123,-6.65252802048314,
61.7210808459859));
#175779=CARTESIAN_POINT('Ctrl Pts',(-4.68317727619349,-6.63988113448914,
61.7202224409685));
#175780=CARTESIAN_POINT('Ctrl Pts',(-4.73693808579128,-6.60174483752643,
61.717652869569));
#175781=CARTESIAN_POINT('Ctrl Pts',(-4.77256123059647,-6.5760380672491,
61.7159457256849));
#175782=CARTESIAN_POINT('Ctrl Pts',(-4.85654681896081,-6.5143895383639,
61.7119073301713));
#175783=CARTESIAN_POINT('Ctrl Pts',(-4.90472147275561,-6.47819615344555,
61.7095800121605));
#175784=CARTESIAN_POINT('Ctrl Pts',(-5.08931854848621,-6.33626969529422,
61.7006082172586));
#175785=CARTESIAN_POINT('Ctrl Pts',(-5.22276188287721,-6.22673557689064,
61.6940060646147));
#175786=CARTESIAN_POINT('Ctrl Pts',(-5.56354347062184,-5.92834481329625,
61.6766734579828));
#175787=CARTESIAN_POINT('Ctrl Pts',(-5.76476847883351,-5.73286406727149,
61.6659446193856));
#175788=CARTESIAN_POINT('Ctrl Pts',(-6.00262996547609,-5.47657958061562,
61.652404952417));
#175789=CARTESIAN_POINT('Ctrl Pts',(-6.04912250091376,-5.42518269725157,
61.6497147129244));
#175790=CARTESIAN_POINT('Ctrl Pts',(-6.12146995540695,-5.3431171797327,
61.6454560625029));
#175791=CARTESIAN_POINT('Ctrl Pts',(-6.14776514359542,-5.31284098530027,
61.6438926687732));
#175792=CARTESIAN_POINT('Ctrl Pts',(-6.1964469889122,-5.25594349399365,
61.6409685746474));
#175793=CARTESIAN_POINT('Ctrl Pts',(-6.21888893714445,-5.22937067683744,
61.6396085262119));
#175794=CARTESIAN_POINT('Ctrl Pts',(-6.26944326411468,-5.16872517156314,
61.6365169514494));
#175795=CARTESIAN_POINT('Ctrl Pts',(-6.29744977109725,-5.13456571688859,
61.6347843242804));
#175796=CARTESIAN_POINT('Ctrl Pts',(-6.38389496117759,-5.02735752053206,
61.6293731591286));
#175797=CARTESIAN_POINT('Ctrl Pts',(-6.44135133999584,-4.95352715216749,
61.6256846313344));
#175798=CARTESIAN_POINT('Ctrl Pts',(-6.57804371246188,-4.77147917450536,
61.6166799861609));
#175799=CARTESIAN_POINT('Ctrl Pts',(-6.65589974403492,-4.66226026696053,
61.6113527434064));
#175800=CARTESIAN_POINT('Ctrl Pts',(-6.8109787738291,-4.43290372672422,
61.6003274637109));
#175801=CARTESIAN_POINT('Ctrl Pts',(-6.88781038445357,-4.31255554272703,
61.594629493107));
#175802=CARTESIAN_POINT('Ctrl Pts',(-7.04155796220453,-4.057128254136,61.5827435935202));
#175803=CARTESIAN_POINT('Ctrl Pts',(-7.11785046002824,-3.92173860166251,
61.5765591373405));
#175804=CARTESIAN_POINT('Ctrl Pts',(-7.20598200657805,-3.7542851571309,
61.5690831787386));
#175805=CARTESIAN_POINT('Ctrl Pts',(-7.22156222153079,-3.72422781448013,
61.5677479563913));
#175806=CARTESIAN_POINT('Ctrl Pts',(-7.24535112640807,-3.67762365350201,
61.5656885457635));
#175807=CARTESIAN_POINT('Ctrl Pts',(-7.2536919857583,-3.66114480183142,
61.5649624404453));
#175808=CARTESIAN_POINT('Ctrl Pts',(-7.26946435218926,-3.62971820535078,
61.5635817760801));
#175809=CARTESIAN_POINT('Ctrl Pts',(-7.27690612471744,-3.61477571536043,
61.562927056102));
#175810=CARTESIAN_POINT('Ctrl Pts',(-7.29498961651387,-3.57818334004305,
61.5613281079596));
#175811=CARTESIAN_POINT('Ctrl Pts',(-7.30558108080675,-3.55650876532049,
61.5603847438999));
#175812=CARTESIAN_POINT('Ctrl Pts',(-7.34128920710725,-3.48260237703531,
61.5571802417162));
#175813=CARTESIAN_POINT('Ctrl Pts',(-7.36594360049633,-3.43014890166331,
61.5549265616023));
#175814=CARTESIAN_POINT('Ctrl Pts',(-7.42496324921254,-3.30101032549842,
61.5494237355752));
#175815=CARTESIAN_POINT('Ctrl Pts',(-7.45870425400993,-3.22404706107066,
61.5461831614131));
#175816=CARTESIAN_POINT('Ctrl Pts',(-7.64685488975612,-2.77610504818729,
61.5275134563248));
#175817=CARTESIAN_POINT('Ctrl Pts',(-7.77476992081399,-2.39459972790696,
61.5123492254595));
#175818=CARTESIAN_POINT('Ctrl Pts',(-7.97017323991821,-1.6272973329033,
61.482232868238));
#175819=CARTESIAN_POINT('Ctrl Pts',(-8.03907875170318,-1.24296508113117,
61.4673242886985));
#175820=CARTESIAN_POINT('Ctrl Pts',(-8.08780429090186,-0.782584465608853,
61.4493419320412));
#175821=CARTESIAN_POINT('Ctrl Pts',(-8.09450888817357,-0.709889057082839,
61.4464994618613));
#175822=CARTESIAN_POINT('Ctrl Pts',(-8.10359536137866,-0.594364031135042,
61.441976010416));
#175823=CARTESIAN_POINT('Ctrl Pts',(-8.10661928465596,-0.551588741911865,
61.4402997564319));
#175824=CARTESIAN_POINT('Ctrl Pts',(-8.1116548188829,-0.471330579643435,
61.437151806774));
#175825=CARTESIAN_POINT('Ctrl Pts',(-8.1137455781137,-0.433853776364693,
61.4356807033261));
#175826=CARTESIAN_POINT('Ctrl Pts',(-8.11786818376271,-0.349443158880844,
61.4323644819724));
#175827=CARTESIAN_POINT('Ctrl Pts',(-8.11975282665341,-0.302503528540085,
61.4305184322093));
#175828=CARTESIAN_POINT('Ctrl Pts',(-8.12425218016602,-0.159516862081264,
61.4248887483838));
#175829=CARTESIAN_POINT('Ctrl Pts',(-8.12557041786649,-0.0634377752123971,
61.4210972420416));
#175830=CARTESIAN_POINT('Ctrl Pts',(-8.12356828760708,0.434934049148002,
61.4013830069805));
#175831=CARTESIAN_POINT('Ctrl Pts',(-8.09207729568715,0.836542689192359,
61.3854020371046));
#175832=CARTESIAN_POINT('Ctrl Pts',(-7.94312641934823,1.80580367579763,
61.3454643083025));
#175833=CARTESIAN_POINT('Ctrl Pts',(-7.79449744559859,2.36641543206504,
61.3210105496806));
#175834=CARTESIAN_POINT('Ctrl Pts',(-7.45926099603663,3.24159150537307,
61.2813935792335));
#175835=CARTESIAN_POINT('Ctrl Pts',(-7.3088143056645,3.56787654615489,61.2663223215167));
#175836=CARTESIAN_POINT('Ctrl Pts',(-7.12661772412565,3.90275613116896,
61.2511555210289));
#175837=CARTESIAN_POINT('Ctrl Pts',(-7.11587144578774,3.92231553855636,
61.2502709091544));
#175838=CARTESIAN_POINT('Ctrl Pts',(-7.10073471219003,3.94959909810885,
61.2490389504922));
#175839=CARTESIAN_POINT('Ctrl Pts',(-7.09641201802787,3.95736060523233,
61.2486887147537));
#175840=CARTESIAN_POINT('Ctrl Pts',(-7.08849021999816,3.97152967674962,
61.248049775112));
#175841=CARTESIAN_POINT('Ctrl Pts',(-7.08489513882653,3.97793947221306,
61.2477608952793));
#175842=CARTESIAN_POINT('Ctrl Pts',(-7.07762150663957,3.99086674547418,
61.2471786258198));
#175843=CARTESIAN_POINT('Ctrl Pts',(-7.07394263697814,3.99738403716737,
61.246885250874));
#175844=CARTESIAN_POINT('Ctrl Pts',(-7.06491585727204,4.01332391877098,
61.2461681691995));
#175845=CARTESIAN_POINT('Ctrl Pts',(-7.05955808581796,4.02274092898861,
61.2457449149994));
#175846=CARTESIAN_POINT('Ctrl Pts',(-7.04023377764377,4.05654851815236,
61.2442268740445));
#175847=CARTESIAN_POINT('Ctrl Pts',(-7.02615943859548,4.08087749074562,
61.2431371911178));
#175848=CARTESIAN_POINT('Ctrl Pts',(-6.74597066269945,4.55946664879856,
61.2217633867272));
#175849=CARTESIAN_POINT('Ctrl Pts',(-6.43644439311334,4.98689027910571,
61.2039625492203));
#175850=CARTESIAN_POINT('Ctrl Pts',(-5.60872534562217,5.92325868789787,
61.162200081619));
#175851=CARTESIAN_POINT('Ctrl Pts',(-5.05954832784191,6.39872730018576,
61.1383400024782));
#175852=CARTESIAN_POINT('Ctrl Pts',(-4.3646357413689,6.85428640341238,61.107215830422));
#175853=CARTESIAN_POINT('Ctrl Pts',(-4.27340048671877,6.91153633511982,
61.1031206324968));
#175854=CARTESIAN_POINT('Ctrl Pts',(-4.16377144545252,6.97732765980867,
61.0981827127597));
#175855=CARTESIAN_POINT('Ctrl Pts',(-4.14644828723428,6.98763626104161,
61.0974019498304));
#175856=CARTESIAN_POINT('Ctrl Pts',(-4.11844052257241,7.00416219367493,
61.0961387900911));
#175857=CARTESIAN_POINT('Ctrl Pts',(-4.10777973140671,7.01041981980389,
61.0956577902534));
#175858=CARTESIAN_POINT('Ctrl Pts',(-4.08875390511109,7.02152921940628,
61.0947990151759));
#175859=CARTESIAN_POINT('Ctrl Pts',(-4.0803943998404,7.02639044008455,61.094421567099));
#175860=CARTESIAN_POINT('Ctrl Pts',(-4.06308993406297,7.03641203966904,
61.0936399784184));
#175861=CARTESIAN_POINT('Ctrl Pts',(-4.05414377642814,7.04157031090248,
61.0932357662378));
#175862=CARTESIAN_POINT('Ctrl Pts',(-4.03102394421308,7.05484232634771,
61.0921907737771));
#175863=CARTESIAN_POINT('Ctrl Pts',(-4.0168356276749,7.06293039926917,61.0915491141526));
#175864=CARTESIAN_POINT('Ctrl Pts',(-3.98592294802465,7.08042894707689,
61.0901502928308));
#175865=CARTESIAN_POINT('Ctrl Pts',(-3.96918945675955,7.08982304944259,
61.0893925763861));
#175866=CARTESIAN_POINT('Ctrl Pts',(-3.92063466039204,7.11685570550575,
61.0871924160428));
#175867=CARTESIAN_POINT('Ctrl Pts',(-3.88872815607519,7.1343398124449,61.0857447419105));
#175868=CARTESIAN_POINT('Ctrl Pts',(-3.56948260151329,7.30650192572491,
61.0712401536745));
#175869=CARTESIAN_POINT('Ctrl Pts',(-3.27321314273342,7.44393866513744,
61.0576050810417));
#175870=CARTESIAN_POINT('Ctrl Pts',(-2.58247179560257,7.71514166658305,
61.0255476920333));
#175871=CARTESIAN_POINT('Ctrl Pts',(-2.18436564951852,7.83716049459927,
61.0068720976049));
#175872=CARTESIAN_POINT('Ctrl Pts',(-1.26458408332123,8.04351480764306,
60.964533921876));
#175873=CARTESIAN_POINT('Ctrl Pts',(-0.740383610719197,8.1085952819358,
60.9409806207243));
#175874=CARTESIAN_POINT('Ctrl Pts',(-0.1825648725882,8.12325767747229,60.9185733810647));
#175875=CARTESIAN_POINT('Ctrl Pts',(-0.151624703333772,8.12389409172628,
60.9173384552744));
#175876=CARTESIAN_POINT('Ctrl Pts',(-0.108733545335255,8.12453120865442,
60.9156366988931));
#175877=CARTESIAN_POINT('Ctrl Pts',(-0.0967853111397488,8.12468232916457,
60.9151637330466));
#175878=CARTESIAN_POINT('Ctrl Pts',(-0.0776770240843752,8.12488185204107,
60.9144090362036));
#175879=CARTESIAN_POINT('Ctrl Pts',(-0.070517192407656,8.12494714787237,
60.9141266339489));
#175880=CARTESIAN_POINT('Ctrl Pts',(-0.0557722640516926,8.12506212609247,
60.9135458257129));
#175881=CARTESIAN_POINT('Ctrl Pts',(-0.0481871645174521,8.12511065130447,
60.9132474653224));
#175882=CARTESIAN_POINT('Ctrl Pts',(-0.0305899512860504,8.12519858593376,
60.9125562314602));
#175883=CARTESIAN_POINT('Ctrl Pts',(-0.0205777981007368,8.12523011128357,
60.9121636615602));
#175884=CARTESIAN_POINT('Ctrl Pts',(0.0111078971516225,8.12527131348465,
60.9109234918231));
#175885=CARTESIAN_POINT('Ctrl Pts',(0.0327815299780469,8.12521277783753,
60.9100784569328));
#175886=CARTESIAN_POINT('Ctrl Pts',(0.518396730850356,8.12195814959084,
60.8912135749861));
#175887=CARTESIAN_POINT('Ctrl Pts',(0.981254947947732,8.07911744903377,
60.8745905294104));
#175888=CARTESIAN_POINT('Ctrl Pts',(1.83850391449729,7.92497464002435,60.8433212049468));
#175889=CARTESIAN_POINT('Ctrl Pts',(2.2330717166765,7.82295990687601,60.8287294406177));
#175890=CARTESIAN_POINT('Ctrl Pts',(2.87554546160043,7.60425876813392,60.8035885545911));
#175891=CARTESIAN_POINT('Ctrl Pts',(3.12819743219707,7.50385805839592,60.7933336200218));
#175892=CARTESIAN_POINT('Ctrl Pts',(3.42011051805385,7.37054639615745,60.7809705478439));
#175893=CARTESIAN_POINT('Ctrl Pts',(3.4646953526693,7.34969361257639,60.7790679521608));
#175894=CARTESIAN_POINT('Ctrl Pts',(3.53276679155353,7.31709885217607,60.7761410123672));
#175895=CARTESIAN_POINT('Ctrl Pts',(3.55639068008394,7.30564590844781,60.7751211171078));
#175896=CARTESIAN_POINT('Ctrl Pts',(3.5995829255423,7.28444700775809,60.7732488793961));
#175897=CARTESIAN_POINT('Ctrl Pts',(3.61916829301732,7.27473616764047,60.7723970684399));
#175898=CARTESIAN_POINT('Ctrl Pts',(3.65988955042922,7.25434055743921,60.7706200470351));
#175899=CARTESIAN_POINT('Ctrl Pts',(3.68101842361429,7.24364216430808,60.7696946295668));
#175900=CARTESIAN_POINT('Ctrl Pts',(3.73506221449023,7.21598011075325,60.7673186619841));
#175901=CARTESIAN_POINT('Ctrl Pts',(3.76790841166634,7.19888358605946,60.7658660939672));
#175902=CARTESIAN_POINT('Ctrl Pts',(3.90602873709278,7.12578736285463,60.7597205080133));
#175903=CARTESIAN_POINT('Ctrl Pts',(4.01017890308169,7.06769909188581,60.7549937797083));
#175904=CARTESIAN_POINT('Ctrl Pts',(4.2728839759304,6.91350235844712,60.7428109601154));
#175905=CARTESIAN_POINT('Ctrl Pts',(4.42949409816638,6.81422272803062,60.7352977337067));
#175906=CARTESIAN_POINT('Ctrl Pts',(4.96727551700171,6.44692925676997,60.7085560816244));
#175907=CARTESIAN_POINT('Ctrl Pts',(5.32865914823077,6.15159164251842,60.6887909456451));
#175908=CARTESIAN_POINT('Ctrl Pts',(5.94531495419874,5.55231416255085,60.6523221694996));
#175909=CARTESIAN_POINT('Ctrl Pts',(6.20756351610341,5.25748439611811,60.6356834160601));
#175910=CARTESIAN_POINT('Ctrl Pts',(6.46005269871621,4.92826944339104,60.6191368695381));
#175911=CARTESIAN_POINT('Ctrl Pts',(6.47265301497333,4.91170882013923,60.6183096824065));
#175912=CARTESIAN_POINT('Ctrl Pts',(6.4912694697758,4.88704512735089,60.6170855916737));
#175913=CARTESIAN_POINT('Ctrl Pts',(6.49733430545904,4.87897902539082,60.6166864983251));
#175914=CARTESIAN_POINT('Ctrl Pts',(6.50769768075396,4.86514236526821,60.6160040335542));
#175915=CARTESIAN_POINT('Ctrl Pts',(6.51200360423369,4.85937736724523,60.6157203221113));
#175916=CARTESIAN_POINT('Ctrl Pts',(6.52082443768452,4.84753478960648,60.6151388299771));
#175917=CARTESIAN_POINT('Ctrl Pts',(6.52533852323877,4.84145660324821,60.6148410879811));
#175918=CARTESIAN_POINT('Ctrl Pts',(6.53574575209892,4.82740234213295,60.6141542841525));
#175919=CARTESIAN_POINT('Ctrl Pts',(6.54163280889005,4.81942176030033,60.6137655124283));
#175920=CARTESIAN_POINT('Ctrl Pts',(6.56004136314681,4.79437097586078,60.6125490472261));
#175921=CARTESIAN_POINT('Ctrl Pts',(6.57251082754709,4.77726251875835,60.6117238888044));
#175922=CARTESIAN_POINT('Ctrl Pts',(6.76887688357308,4.50561864708963,60.5987133809843));
#175923=CARTESIAN_POINT('Ctrl Pts',(6.93792910374296,4.24068738920564,60.5873947578006));
#175924=CARTESIAN_POINT('Ctrl Pts',(7.4397684916167,3.34354093246848,60.5516780980573));
#175925=CARTESIAN_POINT('Ctrl Pts',(7.70467034127299,2.67722706093914,60.5288058451769));
#175926=CARTESIAN_POINT('Ctrl Pts',(7.89231785046553,1.93234034338486,60.5014377636945));
#175927=CARTESIAN_POINT('Ctrl Pts',(7.90502134347635,1.87969617604864,60.4994959447511));
#175928=CARTESIAN_POINT('Ctrl Pts',(7.97060789579515,1.5954697078088,60.4889638419832));
#175929=CARTESIAN_POINT('Ctrl Pts',(8.0138397396152,1.36179164406858,60.4801287633887));
#175930=CARTESIAN_POINT('Ctrl Pts',(8.05030829620179,1.10130577618197,60.469996262894));
#175931=CARTESIAN_POINT('Ctrl Pts',(8.05372561464904,1.07603056952247,60.4690102117594));
#175932=CARTESIAN_POINT('Ctrl Pts',(8.05865928521796,1.03819941428734,60.4675299132235));
#175933=CARTESIAN_POINT('Ctrl Pts',(8.06026543203758,1.02565523566158,60.4670383471084));
#175934=CARTESIAN_POINT('Ctrl Pts',(8.06298135964844,1.00404313390011,60.466190179523));
#175935=CARTESIAN_POINT('Ctrl Pts',(8.06410514757114,0.994976979138242,
60.4658339967926));
#175936=CARTESIAN_POINT('Ctrl Pts',(8.06633167306843,0.976762920415431,
60.465117649003));
#175937=CARTESIAN_POINT('Ctrl Pts',(8.06743414470222,0.967614997243684,
60.4647574765578));
#175938=CARTESIAN_POINT('Ctrl Pts',(8.06963369641106,0.949098802184107,
60.4640276615495));
#175939=CARTESIAN_POINT('Ctrl Pts',(8.07073002879028,0.939730457217788,
60.4636579972944));
#175940=CARTESIAN_POINT('Ctrl Pts',(8.07321103190454,0.918205262005532,
60.4628076869764));
#175941=CARTESIAN_POINT('Ctrl Pts',(8.07458455921479,0.906047163976217,
60.4623267091662));
#175942=CARTESIAN_POINT('Ctrl Pts',(8.07803815102685,0.874845236051451,
60.4610905531158));
#175943=CARTESIAN_POINT('Ctrl Pts',(8.08007833166224,0.855797116500719,
60.4603341873944));
#175944=CARTESIAN_POINT('Ctrl Pts',(8.11085524543148,0.558524385973172,
60.4485029571617));
#175945=CARTESIAN_POINT('Ctrl Pts',(8.12527172054597,0.279029717082663,
60.437000513906));
#175946=CARTESIAN_POINT('Ctrl Pts',(8.12524997543795,-0.000631779635134194,
60.4251159836211));
#175947=CARTESIAN_POINT('',(8.13321556035325,-0.00564624965199908,58.4167025567876));
#175948=CARTESIAN_POINT('Ctrl Pts',(8.12524804204743,-0.00564071843287404,
58.4167025567876));
#175949=CARTESIAN_POINT('Ctrl Pts',(8.12538636330396,0.193605978980111,
58.4245358486659));
#175950=CARTESIAN_POINT('Ctrl Pts',(8.11819169268104,0.393119237488508,
58.4323691405441));
#175951=CARTESIAN_POINT('Ctrl Pts',(8.10363182462515,0.592316480795924,
58.4402024324224));
#175952=CARTESIAN_POINT('Ctrl Pts',(8.08908683718342,0.791310138651282,
58.4480277184455));
#175953=CARTESIAN_POINT('Ctrl Pts',(8.06719166999482,0.989988084929009,
58.4558530044687));
#175954=CARTESIAN_POINT('Ctrl Pts',(8.03796611065937,1.18776612445018,58.4636782904918));
#175955=CARTESIAN_POINT('Ctrl Pts',(8.00877136902933,1.38533561140653,58.4714953249241));
#175956=CARTESIAN_POINT('Ctrl Pts',(7.97226169411772,1.5820067454906,58.4793123593564));
#175957=CARTESIAN_POINT('Ctrl Pts',(7.92850878668791,1.77719891455983,58.4871293937886));
#175958=CARTESIAN_POINT('Ctrl Pts',(7.88478257898052,1.97227196979093,58.494941657963));
#175959=CARTESIAN_POINT('Ctrl Pts',(7.83382201664854,2.16586752378011,58.5027539221375));
#175960=CARTESIAN_POINT('Ctrl Pts',(7.7757502551909,2.35741288946139,58.5105661863119));
#175961=CARTESIAN_POINT('Ctrl Pts',(7.71770715655588,2.54886371296411,58.5183745945409));
#175962=CARTESIAN_POINT('Ctrl Pts',(7.65255995253317,2.73826603678667,58.5261830027699));
#175963=CARTESIAN_POINT('Ctrl Pts',(7.58048229823073,2.92505994617384,58.533991410999));
#175964=CARTESIAN_POINT('Ctrl Pts',(7.53647218251617,3.03911501145677,58.5387591708967));
#175965=CARTESIAN_POINT('Ctrl Pts',(7.48987921437218,3.15219785171096,58.5435269307944));
#175966=CARTESIAN_POINT('Ctrl Pts',(7.44075200433562,3.2641839979504,58.5482946906921));
#175967=CARTESIAN_POINT('Ctrl Pts',(7.35794340140681,3.45294733929565,58.5563312052008));
#175968=CARTESIAN_POINT('Ctrl Pts',(7.26798055620304,3.63848305674189,58.5643677197096));
#175969=CARTESIAN_POINT('Ctrl Pts',(7.17115218707309,3.82024395455799,58.5724042342183));
#175970=CARTESIAN_POINT('Ctrl Pts',(7.07426532397069,4.00211465404734,58.5804456035816));
#175971=CARTESIAN_POINT('Ctrl Pts',(6.97050481102578,4.18020570571134,58.588486972945));
#175972=CARTESIAN_POINT('Ctrl Pts',(6.86020417375442,4.35399658439259,58.5965283423083));
#175973=CARTESIAN_POINT('Ctrl Pts',(6.74982341759097,4.52791369926795,58.6045755526679));
#175974=CARTESIAN_POINT('Ctrl Pts',(6.6328932283692,4.69752414308522,58.6126227630274));
#175975=CARTESIAN_POINT('Ctrl Pts',(6.50978943598929,4.86233781853773,58.620669973387));
#175976=CARTESIAN_POINT('Ctrl Pts',(6.38650419741034,5.02739441757839,58.62872904476));
#175977=CARTESIAN_POINT('Ctrl Pts',(6.2570273581813,5.18763986421855,58.636788116133));
#175978=CARTESIAN_POINT('Ctrl Pts',(6.12177501879248,5.34261716593921,58.6448471875059));
#175979=CARTESIAN_POINT('Ctrl Pts',(5.98641321304975,5.49771989839352,58.6529127814808));
#175980=CARTESIAN_POINT('Ctrl Pts',(5.84526679511342,5.64754574778535,58.6609783754556));
#175981=CARTESIAN_POINT('Ctrl Pts',(5.69878808873808,5.79167522243409,58.6690439694304));
#175982=CARTESIAN_POINT('Ctrl Pts',(5.55207937732762,5.93603101328741,58.6771222282305));
#175983=CARTESIAN_POINT('Ctrl Pts',(5.40002187451157,6.07467233789709,58.6852004870307));
#175984=CARTESIAN_POINT('Ctrl Pts',(5.24310162096852,6.20721942214848,58.6932787458308));
#175985=CARTESIAN_POINT('Ctrl Pts',(5.15450149715187,6.28205799659028,58.6978398825468));
#175986=CARTESIAN_POINT('Ctrl Pts',(5.06435170617298,6.3549545324053,58.7024010192627));
#175987=CARTESIAN_POINT('Ctrl Pts',(4.97274368742692,6.42584685326811,58.7069621559787));
#175988=CARTESIAN_POINT('Ctrl Pts',(4.81033676276519,6.55152803239476,58.7150483497109));
#175989=CARTESIAN_POINT('Ctrl Pts',(4.64302902299906,6.67115206366083,58.723134543443));
#175990=CARTESIAN_POINT('Ctrl Pts',(4.47129960638425,6.78433249424349,58.7312207371752));
#175991=CARTESIAN_POINT('Ctrl Pts',(4.2997233642602,6.89741197325267,58.7392997184063));
#175992=CARTESIAN_POINT('Ctrl Pts',(4.12373357235079,7.00405913783073,58.7473786996374));
#175993=CARTESIAN_POINT('Ctrl Pts',(3.94384075842282,7.10392902798887,58.7554576808684));
#175994=CARTESIAN_POINT('Ctrl Pts',(3.76408383502655,7.20372347670954,58.7635305592595));
#175995=CARTESIAN_POINT('Ctrl Pts',(3.58043004481467,7.29675070657168,58.7716034376506));
#175996=CARTESIAN_POINT('Ctrl Pts',(3.39341762130824,7.3827098283689,58.7796763160417));
#175997=CARTESIAN_POINT('Ctrl Pts',(3.20652096684773,7.46861573762905,58.7877441969604));
#175998=CARTESIAN_POINT('Ctrl Pts',(3.01627011257903,7.54746213275558,58.7958120778791));
#175999=CARTESIAN_POINT('Ctrl Pts',(2.82322710233959,7.61899444094266,58.8038799587978));
#176000=CARTESIAN_POINT('Ctrl Pts',(2.63027730488765,7.69049220902475,58.8119439440578));
#176001=CARTESIAN_POINT('Ctrl Pts',(2.43453833700815,7.75468282419935,58.8200079293179));
#176002=CARTESIAN_POINT('Ctrl Pts',(2.2365919758216,7.81135992617101,58.8280719145779));
#176003=CARTESIAN_POINT('Ctrl Pts',(2.03589479408909,7.8688246583656,58.8362479634101));
#176004=CARTESIAN_POINT('Ctrl Pts',(1.83292871753126,7.91856537212488,58.8444240122423));
#176005=CARTESIAN_POINT('Ctrl Pts',(1.62831702554787,7.96041903588064,58.8526000610746));
#176006=CARTESIAN_POINT('Ctrl Pts',(1.42660542133468,8.00167948183336,58.8606602257215));
#176007=CARTESIAN_POINT('Ctrl Pts',(1.2232948623812,8.03527491782727,58.8687203903684));
#176008=CARTESIAN_POINT('Ctrl Pts',(1.01899407762534,8.06110033632286,58.8767805550154));
#176009=CARTESIAN_POINT('Ctrl Pts',(0.814703163657677,8.08692450706388,
58.8848403302356));
#176010=CARTESIAN_POINT('Ctrl Pts',(0.609422433575708,8.10497936945029,
58.8929001054559));
#176011=CARTESIAN_POINT('Ctrl Pts',(0.403767332793357,8.11521161174919,
58.9009598806762));
#176012=CARTESIAN_POINT('Ctrl Pts',(0.198096704788882,8.12544462659542,
58.9090202644197));
#176013=CARTESIAN_POINT('Ctrl Pts',(-0.00794803388750687,8.12785382821346,
58.9170806481632));
#176014=CARTESIAN_POINT('Ctrl Pts',(-0.213749224837953,8.12243798569008,
58.9251410319068));
#176015=CARTESIAN_POINT('Ctrl Pts',(-0.42472381762285,8.11688600046745,
58.9334040364605));
#176016=CARTESIAN_POINT('Ctrl Pts',(-0.635442107449402,8.10311040649792,
58.9416670410142));
#176017=CARTESIAN_POINT('Ctrl Pts',(-0.845241631071249,8.08116663283242,
58.9499300455679));
#176018=CARTESIAN_POINT('Ctrl Pts',(-1.05006486157437,8.05974334962373,
58.9579970576237));
#176019=CARTESIAN_POINT('Ctrl Pts',(-1.25401209977637,8.03053504270057,
58.9660640696795));
#176020=CARTESIAN_POINT('Ctrl Pts',(-1.45647449919524,7.9936455760619,58.9741310817353));
#176021=CARTESIAN_POINT('Ctrl Pts',(-1.66631530175634,7.95541173457959,
58.982492082538));
#176022=CARTESIAN_POINT('Ctrl Pts',(-1.87456064031404,7.90892643445054,
58.9908530833407));
#176023=CARTESIAN_POINT('Ctrl Pts',(-2.08054651029981,7.85436272277893,
58.9992140841433));
#176024=CARTESIAN_POINT('Ctrl Pts',(-2.28653238028559,7.79979901110732,
59.007575084946));
#176025=CARTESIAN_POINT('Ctrl Pts',(-2.49025842832984,7.73715702172116,
59.0159360857487));
#176026=CARTESIAN_POINT('Ctrl Pts',(-2.69108010185902,7.66666651471671,
59.0242970865514));
#176027=CARTESIAN_POINT('Ctrl Pts',(-2.87310087245517,7.60277532120567,
59.0318753313809));
#176028=CARTESIAN_POINT('Ctrl Pts',(-3.05310033015549,7.53230813123251,
59.0394535762103));
#176029=CARTESIAN_POINT('Ctrl Pts',(-3.23054793484947,7.45541733259379,
59.0470318210397));
#176030=CARTESIAN_POINT('Ctrl Pts',(-3.40786349611596,7.37858375041967,
59.054604426698));
#176031=CARTESIAN_POINT('Ctrl Pts',(-3.5826306470187,7.29533621379642,59.0621770323562));
#176032=CARTESIAN_POINT('Ctrl Pts',(-3.75433463186656,7.20587670130897,
59.0697496380144));
#176033=CARTESIAN_POINT('Ctrl Pts',(-3.9259434533907,7.11646676987552,59.0773180467152));
#176034=CARTESIAN_POINT('Ctrl Pts',(-4.09449216222265,7.02085188261255,
59.084886455416));
#176035=CARTESIAN_POINT('Ctrl Pts',(-4.25948666092877,6.91928182312802,
59.0924548641167));
#176036=CARTESIAN_POINT('Ctrl Pts',(-4.42444129564691,6.81773630378066,
59.1000214442295));
#176037=CARTESIAN_POINT('Ctrl Pts',(-4.5858431126521,6.71023866162834,59.1075880243423));
#176038=CARTESIAN_POINT('Ctrl Pts',(-4.7432231696582,6.59708432000968,59.1151546044551));
#176039=CARTESIAN_POINT('Ctrl Pts',(-4.9005753081548,6.48395005145887,59.1227198422908));
#176040=CARTESIAN_POINT('Ctrl Pts',(-5.05390680998816,6.36516129799542,
59.1302850801266));
#176041=CARTESIAN_POINT('Ctrl Pts',(-5.20277848913424,6.24105628523746,
59.1378503179623));
#176042=CARTESIAN_POINT('Ctrl Pts',(-5.35170193810663,6.1169081152115,59.1454181865943));
#176043=CARTESIAN_POINT('Ctrl Pts',(-5.49616218113374,5.9874402257623,59.1529860552263));
#176044=CARTESIAN_POINT('Ctrl Pts',(-5.63575349523875,5.85303084763818,
59.1605539238582));
#176045=CARTESIAN_POINT('Ctrl Pts',(-5.77354345794196,5.7203559507979,59.1680241331848));
#176046=CARTESIAN_POINT('Ctrl Pts',(-5.90658918307767,5.58286660992183,
59.1754943425114));
#176047=CARTESIAN_POINT('Ctrl Pts',(-6.03453665110089,5.44096084979667,
59.182964551838));
#176048=CARTESIAN_POINT('Ctrl Pts',(-6.19392426641852,5.26418501315344,
59.1922703932813));
#176049=CARTESIAN_POINT('Ctrl Pts',(-6.34532358992774,5.08064389841133,
59.2015762347245));
#176050=CARTESIAN_POINT('Ctrl Pts',(-6.4882623953925,4.89102633922939,59.2108820761678));
#176051=CARTESIAN_POINT('Ctrl Pts',(-6.63196861046514,4.70039076162852,
59.2202378787963));
#176052=CARTESIAN_POINT('Ctrl Pts',(-6.76712323346971,4.50361338683149,
59.2295936814247));
#176053=CARTESIAN_POINT('Ctrl Pts',(-6.89329428761988,4.30141621175714,
59.2389494840532));
#176054=CARTESIAN_POINT('Ctrl Pts',(-7.02007783349853,4.0982374795571,59.2483507040063));
#176055=CARTESIAN_POINT('Ctrl Pts',(-7.13779037612417,3.88958624743861,
59.2577519239594));
#176056=CARTESIAN_POINT('Ctrl Pts',(-7.24604173723519,3.67621635717289,
59.2671531439124));
#176057=CARTESIAN_POINT('Ctrl Pts',(-7.3544102584414,3.46261553737062,59.2765645387752));
#176058=CARTESIAN_POINT('Ctrl Pts',(-7.45329710928877,3.2442858823815,59.285975933638));
#176059=CARTESIAN_POINT('Ctrl Pts',(-7.542358903169,3.02200425848266,59.2953873285008));
#176060=CARTESIAN_POINT('Ctrl Pts',(-7.63131622607169,2.7999833746557,59.3047876836396));
#176061=CARTESIAN_POINT('Ctrl Pts',(-7.71047151882323,2.57401982332461,
59.3141880387784));
#176062=CARTESIAN_POINT('Ctrl Pts',(-7.77953055161956,2.34490766532882,
59.3235883939172));
#176063=CARTESIAN_POINT('Ctrl Pts',(-7.82371594491667,2.19831698196304,
59.3296029349862));
#176064=CARTESIAN_POINT('Ctrl Pts',(-7.86376919165637,2.05043775128498,
59.3356174760553));
#176065=CARTESIAN_POINT('Ctrl Pts',(-7.8996236098685,1.90148215476986,59.3416320171243));
#176066=CARTESIAN_POINT('Ctrl Pts',(-7.9457776897635,1.70973706880325,59.3493743156435));
#176067=CARTESIAN_POINT('Ctrl Pts',(-7.98499275830769,1.51611758234971,
59.3571166141628));
#176068=CARTESIAN_POINT('Ctrl Pts',(-8.01711805569086,1.32117585643077,
59.364858912682));
#176069=CARTESIAN_POINT('Ctrl Pts',(-8.04922334192284,1.12635556155427,
59.3725963884504));
#176070=CARTESIAN_POINT('Ctrl Pts',(-8.07424759310664,0.930215014276329,
59.3803338642187));
#176071=CARTESIAN_POINT('Ctrl Pts',(-8.0920906761317,0.733318519991388,
59.3880713399871));
#176072=CARTESIAN_POINT('Ctrl Pts',(-8.10992581576069,0.536509680224317,
59.3958053711806));
#176073=CARTESIAN_POINT('Ctrl Pts',(-8.12058612244261,0.338945914785465,
59.4035394023741));
#176074=CARTESIAN_POINT('Ctrl Pts',(-8.12402304696773,0.141198777746593,
59.4112734335676));
#176075=CARTESIAN_POINT('Ctrl Pts',(-8.12745953167473,-0.0565230538854145,
59.4190064750487));
#176076=CARTESIAN_POINT('Ctrl Pts',(-8.12367446159159,-0.254427857503845,
59.4267395165298));
#176077=CARTESIAN_POINT('Ctrl Pts',(-8.1126713474277,-0.451941557201383,
59.4344725580108));
#176078=CARTESIAN_POINT('Ctrl Pts',(-8.10166933246672,-0.64943552542729,
59.4422048269668));
#176079=CARTESIAN_POINT('Ctrl Pts',(-8.08345073299006,-0.846538114910816,
59.4499370959228));
#176080=CARTESIAN_POINT('Ctrl Pts',(-8.05807112147902,-1.04267797698327,
59.4576693648787));
#176081=CARTESIAN_POINT('Ctrl Pts',(-8.03268174758566,-1.23889328514048,
59.4654046080869));
#176082=CARTESIAN_POINT('Ctrl Pts',(-8.00012590370554,-1.4341447752558,
59.4731398512951));
#176083=CARTESIAN_POINT('Ctrl Pts',(-7.96051081565275,-1.62786827365595,
59.4808750945033));
#176084=CARTESIAN_POINT('Ctrl Pts',(-7.92735095169755,-1.79002479450765,
59.4873498904725));
#176085=CARTESIAN_POINT('Ctrl Pts',(-7.8892459262511,-1.95111075807356,
59.4938246864417));
#176086=CARTESIAN_POINT('Ctrl Pts',(-7.84628585923914,-2.1108021644872,
59.5002994824109));
#176087=CARTESIAN_POINT('Ctrl Pts',(-7.79045874031913,-2.31832304972874,
59.5087135569154));
#176088=CARTESIAN_POINT('Ctrl Pts',(-7.72640514464444,-2.52358870154097,
59.5171276314198));
#176089=CARTESIAN_POINT('Ctrl Pts',(-7.65433369538427,-2.7259609759138,
59.5255417059243));
#176090=CARTESIAN_POINT('Ctrl Pts',(-7.58224211855191,-2.9283897672931,
59.5339581302482));
#176091=CARTESIAN_POINT('Ctrl Pts',(-7.50212830660131,-3.12792331937895,
59.5423745545721));
#176092=CARTESIAN_POINT('Ctrl Pts',(-7.41424972646203,-3.32394171972941,
59.550790978896));
#176093=CARTESIAN_POINT('Ctrl Pts',(-7.32634935304548,-3.52000873128116,
59.5592094904346));
#176094=CARTESIAN_POINT('Ctrl Pts',(-7.23068047512863,-3.71255860991952,
59.5676280019733));
#176095=CARTESIAN_POINT('Ctrl Pts',(-7.1275478400223,-3.90099337998586,
59.5760465135119));
#176096=CARTESIAN_POINT('Ctrl Pts',(-7.02437559210323,-4.08950052705732,
59.5844682585656));
#176097=CARTESIAN_POINT('Ctrl Pts',(-6.91373398380659,-4.27388917474599,
59.5928900036192));
#176098=CARTESIAN_POINT('Ctrl Pts',(-6.79597338141109,-4.45358657282553,
59.6013117486728));
#176099=CARTESIAN_POINT('Ctrl Pts',(-6.67820001408728,-4.63330344961323,
59.6097344066207));
#176100=CARTESIAN_POINT('Ctrl Pts',(-6.55330625912476,-4.80832784237316,
59.6181570645685));
#176101=CARTESIAN_POINT('Ctrl Pts',(-6.42168575059229,-4.97811607770851,
59.6265797225164));
#176102=CARTESIAN_POINT('Ctrl Pts',(-6.29004021162703,-5.14793660187985,
59.6350039822113));
#176103=CARTESIAN_POINT('Ctrl Pts',(-6.15166552523974,-5.31251877076992,
59.6434282419063));
#176104=CARTESIAN_POINT('Ctrl Pts',(-6.00699635693191,-5.47135105164225,
59.6518525016013));
#176105=CARTESIAN_POINT('Ctrl Pts',(-5.96627107712832,-5.5160633366165,
59.6542239836332));
#176106=CARTESIAN_POINT('Ctrl Pts',(-5.9250472257413,-5.56032017481485,
59.6565954656652));
#176107=CARTESIAN_POINT('Ctrl Pts',(-5.88333505391349,-5.60411065253825,
59.6589669476971));
#176108=CARTESIAN_POINT('Ctrl Pts',(-5.73515897820208,-5.75966959033143,
59.6673912729172));
#176109=CARTESIAN_POINT('Ctrl Pts',(-5.58080255360596,-5.90935670906184,
59.6758155981372));
#176110=CARTESIAN_POINT('Ctrl Pts',(-5.42074539525802,-6.05270244785657,
59.6842399233572));
#176111=CARTESIAN_POINT('Ctrl Pts',(-5.26071589674424,-6.19602341475479,
59.6926627927509));
#176112=CARTESIAN_POINT('Ctrl Pts',(-5.09498782864397,-6.33300501451064,
59.7010856621445));
#176113=CARTESIAN_POINT('Ctrl Pts',(-4.92407575896629,-6.46321634191991,
59.7095085315381));
#176114=CARTESIAN_POINT('Ctrl Pts',(-4.75319861545562,-6.59340106042684,
59.7179296797043));
#176115=CARTESIAN_POINT('Ctrl Pts',(-4.57713979565663,-6.71681810952512,
59.7263508278705));
#176116=CARTESIAN_POINT('Ctrl Pts',(-4.39644573569564,-6.83307781717606,
59.7347719760367));
#176117=CARTESIAN_POINT('Ctrl Pts',(-4.215802372392,-6.94930490627517,59.7431907615128));
#176118=CARTESIAN_POINT('Ctrl Pts',(-4.03052658815115,-7.05837852195163,
59.751609546989));
#176119=CARTESIAN_POINT('Ctrl Pts',(-3.84119333691809,-7.15995260535404,
59.7600283324651));
#176120=CARTESIAN_POINT('Ctrl Pts',(-3.65191297466052,-7.26149831471663,
59.7684447662099));
#176121=CARTESIAN_POINT('Ctrl Pts',(-3.45857764080911,-7.35554854991029,
59.7768611999547));
#176122=CARTESIAN_POINT('Ctrl Pts',(-3.26178741716566,-7.44180290035417,
59.7852776336994));
#176123=CARTESIAN_POINT('Ctrl Pts',(-3.06506861693375,-7.5280259454829,
59.793691012768));
#176124=CARTESIAN_POINT('Ctrl Pts',(-2.86489767249388,-7.60645865035784,
59.8021043918366));
#176125=CARTESIAN_POINT('Ctrl Pts',(-2.66189610388929,-7.67684809636084,
59.8105177709052));
#176126=CARTESIAN_POINT('Ctrl Pts',(-2.6046583205384,-7.69669491768445,
59.8128899849314));
#176127=CARTESIAN_POINT('Ctrl Pts',(-2.54719562530409,-7.71590259370242,
59.8152621989575));
#176128=CARTESIAN_POINT('Ctrl Pts',(-2.48952222673452,-7.73446615126699,
59.8176344129837));
#176129=CARTESIAN_POINT('Ctrl Pts',(-2.30146398348853,-7.7949971778854,
59.8253695978944));
#176130=CARTESIAN_POINT('Ctrl Pts',(-2.11108068195695,-7.84870267244674,
59.8331047828051));
#176131=CARTESIAN_POINT('Ctrl Pts',(-1.91891801273629,-7.89540633678193,
59.8408399677158));
#176132=CARTESIAN_POINT('Ctrl Pts',(-1.72681476496072,-7.9420955591902,
59.8485727607162));
#176133=CARTESIAN_POINT('Ctrl Pts',(-1.5329335881136,-7.98178717972852,
59.8563055537166));
#176134=CARTESIAN_POINT('Ctrl Pts',(-1.3378342829939,-8.01435505787872,
59.864038346717));
#176135=CARTESIAN_POINT('Ctrl Pts',(-1.14276064390407,-8.04691865160498,
59.8717701224401));
#176136=CARTESIAN_POINT('Ctrl Pts',(-0.946469544243333,-8.07236031221967,
59.8795018981632));
#176137=CARTESIAN_POINT('Ctrl Pts',(-0.749530034423728,-8.09060518688168,
59.8872336738863));
#176138=CARTESIAN_POINT('Ctrl Pts',(-0.552520054268652,-8.10885659005816,
59.8949682162499));
#176139=CARTESIAN_POINT('Ctrl Pts',(-0.35486155216785,-8.11990602540112,
59.9027027586136));
#176140=CARTESIAN_POINT('Ctrl Pts',(-0.157128416396801,-8.12373056072521,
59.9104373009772));
#176141=CARTESIAN_POINT('Ctrl Pts',(0.0406381142961575,-8.12755574197067,
59.9181731496188));
#176142=CARTESIAN_POINT('Ctrl Pts',(0.238478950284186,-8.12415359266938,
59.9259089982604));
#176143=CARTESIAN_POINT('Ctrl Pts',(0.435820985675838,-8.11355332951874,
59.9336448469019));
#176144=CARTESIAN_POINT('Ctrl Pts',(0.633324495256172,-8.10294439275282,
59.9413870253652));
#176145=CARTESIAN_POINT('Ctrl Pts',(0.830328036174533,-8.08512560110551,
59.9491292038284));
#176146=CARTESIAN_POINT('Ctrl Pts',(1.02626346573561,-8.06017809117121,
59.9568713822916));
#176147=CARTESIAN_POINT('Ctrl Pts',(1.19017609894768,-8.03930788890827,
59.9633482142844));
#176148=CARTESIAN_POINT('Ctrl Pts',(1.35334123727867,-8.01344966063173,
59.9698250462772));
#176149=CARTESIAN_POINT('Ctrl Pts',(1.51543234453711,-7.98267827058255,
59.97630187827));
#176150=CARTESIAN_POINT('Ctrl Pts',(1.75063017623512,-7.93802829353992,
59.9856999067414));
#176151=CARTESIAN_POINT('Ctrl Pts',(1.98370033438577,-7.88300859344652,
59.9950979352128));
#176152=CARTESIAN_POINT('Ctrl Pts',(2.21382499870229,-7.81784282507782,
60.0044959636842));
#176153=CARTESIAN_POINT('Ctrl Pts',(2.44427711115741,-7.75258433127435,
60.0139073647636));
#176154=CARTESIAN_POINT('Ctrl Pts',(2.67177531021364,-7.67715090081817,
60.023318765843));
#176155=CARTESIAN_POINT('Ctrl Pts',(2.89551562634762,-7.59181643745927,
60.0327301669224));
#176156=CARTESIAN_POINT('Ctrl Pts',(3.1189190636738,-7.50661045953731,60.0421273975491));
#176157=CARTESIAN_POINT('Ctrl Pts',(3.33857589388081,-7.41153326016449,
60.0515246281758));
#176158=CARTESIAN_POINT('Ctrl Pts',(3.55370351085696,-7.30690624816159,
60.0609218588024));
#176159=CARTESIAN_POINT('Ctrl Pts',(3.76828849573501,-7.20254314451151,
60.0702953861081));
#176160=CARTESIAN_POINT('Ctrl Pts',(3.97836704400503,-7.08867834160937,
60.0796689134137));
#176161=CARTESIAN_POINT('Ctrl Pts',(4.18318067121494,-6.96567922276598,
60.0890424407194));
#176162=CARTESIAN_POINT('Ctrl Pts',(4.38666425075851,-6.84347885297659,
60.0983550968892));
#176163=CARTESIAN_POINT('Ctrl Pts',(4.58495101820729,-6.71226242211352,
60.107667753059));
#176164=CARTESIAN_POINT('Ctrl Pts',(4.77731583887187,-6.5724379752238,60.1169804092288));
#176165=CARTESIAN_POINT('Ctrl Pts',(4.90117731880401,-6.4824066334087,60.1229767206713));
#176166=CARTESIAN_POINT('Ctrl Pts',(5.0225839822251,-6.3888074375956,60.1289730321139));
#176167=CARTESIAN_POINT('Ctrl Pts',(5.1413465689545,-6.29175993028976,60.1349693435564));
#176168=CARTESIAN_POINT('Ctrl Pts',(5.29123115610279,-6.16928090750249,
60.1425370017704));
#176169=CARTESIAN_POINT('Ctrl Pts',(5.43684283592682,-6.04135563105719,
60.1501046599844));
#176170=CARTESIAN_POINT('Ctrl Pts',(5.57775061728474,-5.9083318808171,60.1576723181984));
#176171=CARTESIAN_POINT('Ctrl Pts',(5.71861938381086,-5.77534496246231,
60.1652378810639));
#176172=CARTESIAN_POINT('Ctrl Pts',(5.85478657630854,-5.63726263133551,
60.1728034439293));
#176173=CARTESIAN_POINT('Ctrl Pts',(5.98585552004352,-5.4944718814154,60.1803690067948));
#176174=CARTESIAN_POINT('Ctrl Pts',(6.1169129809003,-5.35169364131449,60.1879339068455));
#176175=CARTESIAN_POINT('Ctrl Pts',(6.24287283401844,-5.20420807489195,
60.1954988068961));
#176176=CARTESIAN_POINT('Ctrl Pts',(6.36337646291,-5.0524377832669,60.2030637069468));
#176177=CARTESIAN_POINT('Ctrl Pts',(6.48393923423736,-4.90059300372137,
60.2106323198036));
#176178=CARTESIAN_POINT('Ctrl Pts',(6.59904019996351,-4.74445958410859,
60.2182009326604));
#176179=CARTESIAN_POINT('Ctrl Pts',(6.70836179251535,-4.58449229721463,
60.2257695455173));
#176180=CARTESIAN_POINT('Ctrl Pts',(6.81770769626733,-4.42448943640853,
60.2333398415005));
#176181=CARTESIAN_POINT('Ctrl Pts',(6.92127146867148,-4.26065131995747,
60.2409101374837));
#176182=CARTESIAN_POINT('Ctrl Pts',(7.0187800049933,-4.09346000395829,60.248480433467));
#176183=CARTESIAN_POINT('Ctrl Pts',(7.1163873452605,-3.92609927549251,60.2560584003182));
#176184=CARTESIAN_POINT('Ctrl Pts',(7.20792701552237,-3.75537888246008,
60.2636363671695));
#176185=CARTESIAN_POINT('Ctrl Pts',(7.29317243242582,-3.58180449402309,
60.2712143340207));
#176186=CARTESIAN_POINT('Ctrl Pts',(7.37725009475724,-3.410607855535,60.2786884922948));
#176187=CARTESIAN_POINT('Ctrl Pts',(7.45520477439366,-3.23663525093396,
60.2861626505689));
#176188=CARTESIAN_POINT('Ctrl Pts',(7.52686604962493,-3.06038805276448,
60.293636808843));
#176189=CARTESIAN_POINT('Ctrl Pts',(7.61514203613323,-2.84327783197196,
60.3028438553662));
#176190=CARTESIAN_POINT('Ctrl Pts',(7.69401223489476,-2.62236632347889,
60.3120509018894));
#176191=CARTESIAN_POINT('Ctrl Pts',(7.76320154708332,-2.39841391379036,
60.3212579484126));
#176192=CARTESIAN_POINT('Ctrl Pts',(7.83225976266042,-2.17488583845505,
60.3304475498628));
#176193=CARTESIAN_POINT('Ctrl Pts',(7.89167371237667,-1.94832846441916,
60.339637151313));
#176194=CARTESIAN_POINT('Ctrl Pts',(7.94121874032326,-1.71951518773132,
60.3488267527632));
#176195=CARTESIAN_POINT('Ctrl Pts',(7.99065588289186,-1.49120015693954,
60.357996343656));
#176196=CARTESIAN_POINT('Ctrl Pts',(8.0302669900568,-1.26063912489709,60.3671659345488));
#176197=CARTESIAN_POINT('Ctrl Pts',(8.05987815615349,-1.02861638644337,
60.3763355254416));
#176198=CARTESIAN_POINT('Ctrl Pts',(8.08934617123157,-0.797715329291968,
60.3854607872367));
#176199=CARTESIAN_POINT('Ctrl Pts',(8.10891065581527,-0.565366758546668,
60.3945860490317));
#176200=CARTESIAN_POINT('Ctrl Pts',(8.11844970807552,-0.332358089939839,
60.4037113108267));
#176201=CARTESIAN_POINT('Ctrl Pts',(8.12297647043886,-0.221783701352419,
60.408041708703));
#176202=CARTESIAN_POINT('Ctrl Pts',(8.12524624889688,-0.11106086174646,
60.4123721065793));
#176203=CARTESIAN_POINT('Ctrl Pts',(8.12524999535401,-0.000274771867375941,
60.4167025044555));
#176204=CARTESIAN_POINT('',(8.12839272166354,0.00745291351919315,56.4167025567876));
#176205=CARTESIAN_POINT('Ctrl Pts',(8.12839272166354,0.00745291351919315,
56.4167025567876));
#176206=CARTESIAN_POINT('Ctrl Pts',(8.13117600423807,0.594204244290565,
56.4396742518479));
#176207=CARTESIAN_POINT('Ctrl Pts',(7.79071024475799,3.87609837964483,56.5684242570992));
#176208=CARTESIAN_POINT('Ctrl Pts',(4.37969769441631,7.81986399754792,56.7500634174461));
#176209=CARTESIAN_POINT('Ctrl Pts',(-1.20468243196269,8.37056697778818,
56.9616200378278));
#176210=CARTESIAN_POINT('Ctrl Pts',(-5.04719085376719,6.80318123386091,
57.1202875031144));
#176211=CARTESIAN_POINT('Ctrl Pts',(-7.69384797429684,3.54846383209959,
57.2789549684008));
#176212=CARTESIAN_POINT('Ctrl Pts',(-8.44679792397339,-0.555938847163704,
57.4376224336872));
#176213=CARTESIAN_POINT('Ctrl Pts',(-7.16239838939218,-4.52625027291816,
57.5962898989736));
#176214=CARTESIAN_POINT('Ctrl Pts',(-4.11199154401565,-7.40600674808037,
57.7549573642601));
#176215=CARTESIAN_POINT('Ctrl Pts',(-0.0971997372447445,-8.45625233235956,
57.9136248295464));
#176216=CARTESIAN_POINT('Ctrl Pts',(5.36683002199323,-7.17838145731046,
58.1251814499284));
#176217=CARTESIAN_POINT('Ctrl Pts',(8.01157082499094,-3.15609430642058,
58.2928740256754));
#176218=CARTESIAN_POINT('Ctrl Pts',(8.13406518936454,-0.235442656146994,
58.407677446327));
#176219=CARTESIAN_POINT('Ctrl Pts',(8.13353216142055,-0.00564646944313244,
58.4167025567876));
#176220=CARTESIAN_POINT('',(8.12524955238746,-0.00269701298808146,54.4167028280926));
#176221=CARTESIAN_POINT('Ctrl Pts',(8.12524955469297,-0.00269006721165242,
54.4167030993976));
#176222=CARTESIAN_POINT('Ctrl Pts',(8.12532117721707,0.213643145395203,
54.4251531671901));
#176223=CARTESIAN_POINT('Ctrl Pts',(8.1167486902665,0.42985406284176,54.4336032349825));
#176224=CARTESIAN_POINT('Ctrl Pts',(8.09958770519598,0.645264727331433,
54.442053302775));
#176225=CARTESIAN_POINT('Ctrl Pts',(8.0824089990312,0.860897833171388,54.450512096433));
#176226=CARTESIAN_POINT('Ctrl Pts',(8.05662409774357,1.07572878194088,54.458970890091));
#176227=CARTESIAN_POINT('Ctrl Pts',(8.02234035055661,1.28908605699205,54.467429683749));
#176228=CARTESIAN_POINT('Ctrl Pts',(7.98802355053444,1.50264902901132,54.475896632499));
#176229=CARTESIAN_POINT('Ctrl Pts',(7.94519157648052,1.71473523844329,54.484363581249));
#176230=CARTESIAN_POINT('Ctrl Pts',(7.8940028471983,1.92468350928801,54.492830529999));
#176231=CARTESIAN_POINT('Ctrl Pts',(7.84274283670313,2.13492413682158,54.5013092691253));
#176232=CARTESIAN_POINT('Ctrl Pts',(7.78310286112371,2.34302062537099,54.5097880082515));
#176233=CARTESIAN_POINT('Ctrl Pts',(7.71529177581499,2.54832501391434,54.5182667473777));
#176234=CARTESIAN_POINT('Ctrl Pts',(7.64743704724449,2.75376153650533,54.5267509434264));
#176235=CARTESIAN_POINT('Ctrl Pts',(7.57140079006321,2.95640213063907,54.535235139475));
#176236=CARTESIAN_POINT('Ctrl Pts',(7.48744068584734,3.15561714065853,54.5437193355236));
#176237=CARTESIAN_POINT('Ctrl Pts',(7.40340079297167,3.35502146795923,54.5522115942425));
#176238=CARTESIAN_POINT('Ctrl Pts',(7.31142210103964,3.5509934704558,54.5607038529614));
#176239=CARTESIAN_POINT('Ctrl Pts',(7.21180989403962,3.74292474072513,54.5691961116802));
#176240=CARTESIAN_POINT('Ctrl Pts',(7.16328015026766,3.8364311055424,54.5733334272973));
#176241=CARTESIAN_POINT('Ctrl Pts',(7.11293928072038,3.92897876777759,54.5774707429144));
#176242=CARTESIAN_POINT('Ctrl Pts',(7.0608264780951,4.02049959690723,54.5816080585314));
#176243=CARTESIAN_POINT('Ctrl Pts',(6.96537197072242,4.18813739834589,54.5891863388038));
#176244=CARTESIAN_POINT('Ctrl Pts',(6.86380968578961,4.35260891314493,54.5967646190762));
#176245=CARTESIAN_POINT('Ctrl Pts',(6.75638455891372,4.51341946361872,54.6043428993485));
#176246=CARTESIAN_POINT('Ctrl Pts',(6.64903936949063,4.6741103513454,54.6119155404521));
#176247=CARTESIAN_POINT('Ctrl Pts',(6.5358402198108,4.83114539062414,54.6194881815556));
#176248=CARTESIAN_POINT('Ctrl Pts',(6.41707800793653,4.98405431376478,54.6270608226592));
#176249=CARTESIAN_POINT('Ctrl Pts',(6.29838161732412,5.13687849060345,54.6346292667982));
#176250=CARTESIAN_POINT('Ctrl Pts',(6.17412852431732,5.28558081247401,54.6421977109373));
#176251=CARTESIAN_POINT('Ctrl Pts',(6.04465295973988,5.42971989690149,54.6497661550763));
#176252=CARTESIAN_POINT('Ctrl Pts',(5.91520867859788,5.57382415494487,54.6573327705542));
#176253=CARTESIAN_POINT('Ctrl Pts',(5.78054467676714,5.71336709163324,54.6648993860321));
#176254=CARTESIAN_POINT('Ctrl Pts',(5.64103558225979,5.84794024611905,54.67246600151));
#176255=CARTESIAN_POINT('Ctrl Pts',(5.50155123616915,5.98248952780635,54.6800312746972));
#176256=CARTESIAN_POINT('Ctrl Pts',(5.35722377501494,6.11207052907319,54.6875965478845));
#176257=CARTESIAN_POINT('Ctrl Pts',(5.20846460849133,6.236311729267,54.6951618210717));
#176258=CARTESIAN_POINT('Ctrl Pts',(5.05965371435143,6.36059613151204,54.7027297249106));
#176259=CARTESIAN_POINT('Ctrl Pts',(4.90640831666732,6.47953678467443,54.7102976287495));
#176260=CARTESIAN_POINT('Ctrl Pts',(4.74917319109061,6.59280225424107,54.7178655325884));
#176261=CARTESIAN_POINT('Ctrl Pts',(4.59397223275593,6.70460239659791,54.7253355296649));
#176262=CARTESIAN_POINT('Ctrl Pts',(4.43488446612516,6.81087314914783,54.7328055267414));
#176263=CARTESIAN_POINT('Ctrl Pts',(4.27236483638971,6.91133751652173,54.7402755238179));
#176264=CARTESIAN_POINT('Ctrl Pts',(4.06990534011865,7.036491414822,54.749581303358));
#176265=CARTESIAN_POINT('Ctrl Pts',(3.86222049824272,7.15257477844018,54.7588870828981));
#176266=CARTESIAN_POINT('Ctrl Pts',(3.65007256103867,7.25924637008916,54.7681928624382));
#176267=CARTESIAN_POINT('Ctrl Pts',(3.43678578333663,7.3664905901132,54.7775485967351));
#176268=CARTESIAN_POINT('Ctrl Pts',(3.21898792955849,7.46422174700156,54.786904331032));
#176269=CARTESIAN_POINT('Ctrl Pts',(2.99746666849595,7.55214414148431,54.7962600653289));
#176270=CARTESIAN_POINT('Ctrl Pts',(2.77487016322118,7.6404933033362,54.8056612115158));
#176271=CARTESIAN_POINT('Ctrl Pts',(2.54851406480698,7.71893825665806,54.8150623577028));
#176272=CARTESIAN_POINT('Ctrl Pts',(2.31920988599594,7.7872301280493,54.8244635038897));
#176273=CARTESIAN_POINT('Ctrl Pts',(2.08965755173713,7.85559590563803,54.8338748240981));
#176274=CARTESIAN_POINT('Ctrl Pts',(1.85715079420815,7.91378662327403,54.8432861443065));
#176275=CARTESIAN_POINT('Ctrl Pts',(1.62251539912165,7.96160356599807,54.852697464515));
#176276=CARTESIAN_POINT('Ctrl Pts',(1.38815517534784,8.00936443086184,54.8620977474912));
#176277=CARTESIAN_POINT('Ctrl Pts',(1.15167134041322,8.04677583537968,54.8714980304675));
#176278=CARTESIAN_POINT('Ctrl Pts',(0.913897794378005,8.07369050583009,
54.8808983134437));
#176279=CARTESIAN_POINT('Ctrl Pts',(0.761755334774513,8.09091220365991,
54.8869132053306));
#176280=CARTESIAN_POINT('Ctrl Pts',(0.609085056009594,8.103837301339,54.8929280972176));
#176281=CARTESIAN_POINT('Ctrl Pts',(0.456107690708852,8.11243818694332,
54.8989429891045));
#176282=CARTESIAN_POINT('Ctrl Pts',(0.259196678160573,8.12350916525328,
54.9066853008478));
#176283=CARTESIAN_POINT('Ctrl Pts',(0.061684181500173,8.12741761380081,
54.914427612591));
#176284=CARTESIAN_POINT('Ctrl Pts',(-0.135859564528569,8.12411408962393,
54.9221699243343));
#176285=CARTESIAN_POINT('Ctrl Pts',(-0.333280259637731,8.12081262322765,
54.9299074133555));
#176286=CARTESIAN_POINT('Ctrl Pts',(-0.530731813611958,8.11030813480075,
54.9376449023768));
#176287=CARTESIAN_POINT('Ctrl Pts',(-0.727641109789703,8.0926031644857,
54.945382391398));
#176288=CARTESIAN_POINT('Ctrl Pts',(-0.92446274644691,8.07490607601899,
54.9531164358659));
#176289=CARTESIAN_POINT('Ctrl Pts',(-1.12074225497299,8.05001492133607,
54.9608504803337));
#176290=CARTESIAN_POINT('Ctrl Pts',(-1.31590862474052,8.01798428869959,
54.9685845248016));
#176291=CARTESIAN_POINT('Ctrl Pts',(-1.51105001943296,7.98595775496323,
54.9763175795583));
#176292=CARTESIAN_POINT('Ctrl Pts',(-1.70507820945395,7.94679361266297,
54.9840506343149));
#176293=CARTESIAN_POINT('Ctrl Pts',(-1.89742902587127,7.90059812003377,
54.9917836890716));
#176294=CARTESIAN_POINT('Ctrl Pts',(-2.08976062681534,7.85440724224464,
54.9995159713111));
#176295=CARTESIAN_POINT('Ctrl Pts',(-2.28041484514974,7.80118649929966,
55.0072482535506));
#176296=CARTESIAN_POINT('Ctrl Pts',(-2.4688395181715,7.74109288124194,55.0149805357901));
#176297=CARTESIAN_POINT('Ctrl Pts',(-2.65733666855023,7.68097614823576,
55.0227157922441));
#176298=CARTESIAN_POINT('Ctrl Pts',(-2.84360222324174,7.61398136575718,
55.030451048698));
#176299=CARTESIAN_POINT('Ctrl Pts',(-3.02710032847934,7.54031505733151,
55.0381863051519));
#176300=CARTESIAN_POINT('Ctrl Pts',(-3.18069551964057,7.4786534357571,55.0446610215648));
#176301=CARTESIAN_POINT('Ctrl Pts',(-3.3323519420771,7.41231841846424,55.0511357379778));
#176302=CARTESIAN_POINT('Ctrl Pts',(-3.48176698343969,7.34145668348791,
55.0576104543907));
#176303=CARTESIAN_POINT('Ctrl Pts',(-3.67593586605389,7.24936994459615,
55.0660245232801));
#176304=CARTESIAN_POINT('Ctrl Pts',(-3.86641280821176,7.14959357787699,
55.0744385921696));
#176305=CARTESIAN_POINT('Ctrl Pts',(-4.05260734156805,7.04244711002992,
55.082852661059));
#176306=CARTESIAN_POINT('Ctrl Pts',(-4.23885387189586,6.93527072029557,
55.0912690796742));
#176307=CARTESIAN_POINT('Ctrl Pts',(-4.42081537713161,6.82072025230835,
55.0996854982895));
#176308=CARTESIAN_POINT('Ctrl Pts',(-4.5979280725388,6.69916002214155,55.1081019169047));
#176309=CARTESIAN_POINT('Ctrl Pts',(-4.77508468938182,6.5775696467622,55.1165204226724));
#176310=CARTESIAN_POINT('Ctrl Pts',(-4.94738987823115,6.44896618817717,
55.12493892844));
#176311=CARTESIAN_POINT('Ctrl Pts',(-5.11430990332206,6.31375655020701,
55.1333574342077));
#176312=CARTESIAN_POINT('Ctrl Pts',(-5.28129404125881,6.17849497913493,
55.1417791734661));
#176313=CARTESIAN_POINT('Ctrl Pts',(-5.44288867607268,6.03662232332008,
55.1502009127246));
#176314=CARTESIAN_POINT('Ctrl Pts',(-5.59859305894425,5.88858585085088,
55.158622651983));
#176315=CARTESIAN_POINT('Ctrl Pts',(-5.75431431990311,5.7405333314827,55.1670453041435));
#176316=CARTESIAN_POINT('Ctrl Pts',(-5.90414386489438,5.58631584549195,
55.1754679563039));
#176317=CARTESIAN_POINT('Ctrl Pts',(-6.04761730014841,5.42641802236481,
55.1838906084644));
#176318=CARTESIAN_POINT('Ctrl Pts',(-6.19111802100276,5.2664897900676,55.1923148624345));
#176319=CARTESIAN_POINT('Ctrl Pts',(-6.32826004101571,5.10087925898032,
55.2007391164045));
#176320=CARTESIAN_POINT('Ctrl Pts',(-6.45861793529407,4.9301056711188,55.2091633703746));
#176321=CARTESIAN_POINT('Ctrl Pts',(-6.4953150588272,4.88203110314082,55.2115348868088));
#176322=CARTESIAN_POINT('Ctrl Pts',(-6.5314747998295,4.83354757078024,55.2139064032431));
#176323=CARTESIAN_POINT('Ctrl Pts',(-6.56708825636936,4.78466711439318,
55.2162779196773));
#176324=CARTESIAN_POINT('Ctrl Pts',(-6.69359774332266,4.6110293364188,55.2247022445406));
#176325=CARTESIAN_POINT('Ctrl Pts',(-6.8132235736821,4.43236261921473,55.2331265694039));
#176326=CARTESIAN_POINT('Ctrl Pts',(-6.92558966475159,4.24922291224947,
55.2415508942672));
#176327=CARTESIAN_POINT('Ctrl Pts',(-7.0379363373458,4.06611485445737,55.2499737632861));
#176328=CARTESIAN_POINT('Ctrl Pts',(-7.14302563848885,3.87853557566106,
55.258396632305));
#176329=CARTESIAN_POINT('Ctrl Pts',(-7.2405257755269,3.68706849087871,55.2668195013239));
#176330=CARTESIAN_POINT('Ctrl Pts',(-7.33800598806478,3.49564053307689,
55.2752406490995));
#176331=CARTESIAN_POINT('Ctrl Pts',(-7.42790001379247,3.30032659087973,
55.2836617968751));
#176332=CARTESIAN_POINT('Ctrl Pts',(-7.50992233352312,3.10173404839142,
55.2920829446507));
#176333=CARTESIAN_POINT('Ctrl Pts',(-7.59192164037156,2.90319722472215,
55.3005017297172));
#176334=CARTESIAN_POINT('Ctrl Pts',(-7.66605355161384,2.70138388175668,
55.3089205147837));
#176335=CARTESIAN_POINT('Ctrl Pts',(-7.73208056312027,2.4969216503362,55.3173392998502));
#176336=CARTESIAN_POINT('Ctrl Pts',(-7.79808913034733,2.29251653430581,
55.3257557331758));
#176337=CARTESIAN_POINT('Ctrl Pts',(-7.85599723723042,2.08546425817583,
55.3341721665014));
#176338=CARTESIAN_POINT('Ctrl Pts',(-7.90561678982064,1.8764089999267,55.342588599827));
#176339=CARTESIAN_POINT('Ctrl Pts',(-7.95521833333483,1.66742961684867,
55.3510019784659));
#176340=CARTESIAN_POINT('Ctrl Pts',(-7.99653726911623,1.45644895996967,
55.3594153571048));
#176341=CARTESIAN_POINT('Ctrl Pts',(-8.02943606656307,1.24412379427298,
55.3678287357437));
#176342=CARTESIAN_POINT('Ctrl Pts',(-8.03871213393285,1.18425709110593,
55.3702009521503));
#176343=CARTESIAN_POINT('Ctrl Pts',(-8.04731910989908,1.12428356740809,
55.3725731685569));
#176344=CARTESIAN_POINT('Ctrl Pts',(-8.05525464611378,1.06421809266818,
55.3749453849636));
#176345=CARTESIAN_POINT('Ctrl Pts',(-8.0811303839952,0.868360063917399,
55.3826805711281));
#176346=CARTESIAN_POINT('Ctrl Pts',(-8.0998745576842,0.67143685392728,55.3904157572926));
#176347=CARTESIAN_POINT('Ctrl Pts',(-8.11141143931543,0.47401690333016,
55.3981509434571));
#176348=CARTESIAN_POINT('Ctrl Pts',(-8.12294475347403,0.276657999582231,
55.4058837377218));
#176349=CARTESIAN_POINT('Ctrl Pts',(-8.1272751931843,0.0788030133886556,
55.4136165319865));
#176350=CARTESIAN_POINT('Ctrl Pts',(-8.12437890424811,-0.118974714574983,
55.4213493262512));
#176351=CARTESIAN_POINT('Ctrl Pts',(-8.12148299632561,-0.316726424409161,
55.4290811032485));
#176352=CARTESIAN_POINT('Ctrl Pts',(-8.11136225933815,-0.514400543104047,
55.4368128802457));
#176353=CARTESIAN_POINT('Ctrl Pts',(-8.09404495409557,-0.711423814318956,
55.444544657243));
#176354=CARTESIAN_POINT('Ctrl Pts',(-8.07672145222333,-0.908517586124225,
55.4522792008923));
#176355=CARTESIAN_POINT('Ctrl Pts',(-8.05219626393886,-1.10495969247385,
55.4600137445417));
#176356=CARTESIAN_POINT('Ctrl Pts',(-8.02054959776511,-1.30018141514555,
55.467748288191));
#176357=CARTESIAN_POINT('Ctrl Pts',(-7.9888975867931,-1.49543610876966,
55.4754841381257));
#176358=CARTESIAN_POINT('Ctrl Pts',(-7.95012176548351,-1.68946966039589,
55.4832199880604));
#176359=CARTESIAN_POINT('Ctrl Pts',(-7.90435350815507,-1.88172346018661,
55.490955837995));
#176360=CARTESIAN_POINT('Ctrl Pts',(-7.85854780113553,-2.07413457086995,
55.4986980177575));
#176361=CARTESIAN_POINT('Ctrl Pts',(-7.8057383160175,-2.26476267798658,
55.5064401975201));
#176362=CARTESIAN_POINT('Ctrl Pts',(-7.74610661894578,-2.45306335230551,
55.5141823772826));
#176363=CARTESIAN_POINT('Ctrl Pts',(-7.69622092294884,-2.61058880699442,
55.5206592016051));
#176364=CARTESIAN_POINT('Ctrl Pts',(-7.6415617019312,-2.76648561514557,
55.5271360259276));
#176365=CARTESIAN_POINT('Ctrl Pts',(-7.58226108443207,-2.92044592656789,
55.5336128502501));
#176366=CARTESIAN_POINT('Ctrl Pts',(-7.49621448058495,-3.14384599361324,
55.5430108761084));
#176367=CARTESIAN_POINT('Ctrl Pts',(-7.40034680045617,-3.36329580948709,
55.5524089019666));
#176368=CARTESIAN_POINT('Ctrl Pts',(-7.29502453550529,-3.5780308255905,
55.5618069278249));
#176369=CARTESIAN_POINT('Ctrl Pts',(-7.18955240745439,-3.79307138824867,
55.5712183261385));
#176370=CARTESIAN_POINT('Ctrl Pts',(-7.07459880091788,-4.00338369818199,
55.5806297244521));
#176371=CARTESIAN_POINT('Ctrl Pts',(-6.95057716370891,-4.20822583208509,
55.5900411227658));
#176372=CARTESIAN_POINT('Ctrl Pts',(-6.82674226255766,-4.41275954067304,
55.599438350589));
#176373=CARTESIAN_POINT('Ctrl Pts',(-6.69386664112265,-4.6118395053296,
55.6088355784123));
#176374=CARTESIAN_POINT('Ctrl Pts',(-6.55240665869331,-4.80475332786311,
55.6182328062355));
#176375=CARTESIAN_POINT('Ctrl Pts',(-6.41130349015302,-4.99718055107653,
55.6276063308082));
#176376=CARTESIAN_POINT('Ctrl Pts',(-6.26165921735419,-5.18347265648011,
55.6369798553809));
#176377=CARTESIAN_POINT('Ctrl Pts',(-6.10397111129621,-5.36294921055209,
55.6463533799536));
#176378=CARTESIAN_POINT('Ctrl Pts',(-5.94730701916723,-5.54126025825905,
55.6556660336086));
#176379=CARTESIAN_POINT('Ctrl Pts',(-5.78270323996381,-5.71284393894928,
55.6649786872636));
#176380=CARTESIAN_POINT('Ctrl Pts',(-5.61069107700621,-5.87705991129093,
55.6742913409186));
#176381=CARTESIAN_POINT('Ctrl Pts',(-5.49993415966061,-5.98279693920071,
55.6802876657912));
#176382=CARTESIAN_POINT('Ctrl Pts',(-5.38610664811779,-6.0854799000411,
55.6862839906638));
#176383=CARTESIAN_POINT('Ctrl Pts',(-5.26936004560861,-6.18494399911944,
55.6922803155364));
#176384=CARTESIAN_POINT('Ctrl Pts',(-5.12202005641906,-6.31047261381124,
55.6998479742341));
#176385=CARTESIAN_POINT('Ctrl Pts',(-4.97008702844688,-6.43082209503759,
55.7074156329318));
#176386=CARTESIAN_POINT('Ctrl Pts',(-4.81398030021903,-6.54563069777108,
55.7149832916295));
#176387=CARTESIAN_POINT('Ctrl Pts',(-4.65791679505825,-6.66040751212495,
55.7225488549825));
#176388=CARTESIAN_POINT('Ctrl Pts',(-4.49768218492731,-6.76964628300164,
55.7301144183354));
#176389=CARTESIAN_POINT('Ctrl Pts',(-4.33372824331128,-6.87302604939237,
55.7376799816883));
#176390=CARTESIAN_POINT('Ctrl Pts',(-4.16978866553457,-6.97639675878613,
55.7452448822299));
#176391=CARTESIAN_POINT('Ctrl Pts',(-4.00213071628905,-7.0739092899868,
55.7528097827714));
#176392=CARTESIAN_POINT('Ctrl Pts',(-3.83123438527392,-7.16528650143138,
55.760374683313));
#176393=CARTESIAN_POINT('Ctrl Pts',(-3.66025417929713,-7.25670856029932,
55.7679432966654));
#176394=CARTESIAN_POINT('Ctrl Pts',(-3.48603273945837,-7.34198910719033,
55.7755119100177));
#176395=CARTESIAN_POINT('Ctrl Pts',(-3.30907435617335,-7.42089714709858,
55.7830805233701));
#176396=CARTESIAN_POINT('Ctrl Pts',(-3.13207662038864,-7.49982273479723,
55.7906508198518));
#176397=CARTESIAN_POINT('Ctrl Pts',(-2.95234106915857,-7.57237285329657,
55.7982211163335));
#176398=CARTESIAN_POINT('Ctrl Pts',(-2.77039087292521,-7.63836513749589,
55.8057914128153));
#176399=CARTESIAN_POINT('Ctrl Pts',(-2.58825630921775,-7.70442429071213,
55.8133693801678));
#176400=CARTESIAN_POINT('Ctrl Pts',(-2.40390296661676,-7.76391221895912,
55.8209473475203));
#176401=CARTESIAN_POINT('Ctrl Pts',(-2.21786891603798,-7.81669655505269,
55.8285253148728));
#176402=CARTESIAN_POINT('Ctrl Pts',(-2.03438338178489,-7.86875778834944,
55.8359994701895));
#176403=CARTESIAN_POINT('Ctrl Pts',(-1.84926323846872,-7.91429791085689,
55.8434736255062));
#176404=CARTESIAN_POINT('Ctrl Pts',(-1.66303227187805,-7.95323903986245,
55.850947780823));
#176405=CARTESIAN_POINT('Ctrl Pts',(-1.46183445975847,-7.99530975506528,
55.8590226124404));
#176406=CARTESIAN_POINT('Ctrl Pts',(-1.2589105843238,-8.0297684172589,55.8670974440578));
#176407=CARTESIAN_POINT('Ctrl Pts',(-1.05486315500429,-8.05648504539755,
55.8751722756752));
#176408=CARTESIAN_POINT('Ctrl Pts',(-0.850950723195874,-8.08318399785014,
55.8832417649946));
#176409=CARTESIAN_POINT('Ctrl Pts',(-0.645916532928484,-8.10215108926084,
55.8913112543141));
#176410=CARTESIAN_POINT('Ctrl Pts',(-0.440372350046428,-8.11330757187317,
55.8993807436335));
#176411=CARTESIAN_POINT('Ctrl Pts',(-0.234936153408985,-8.12445819323153,
55.907445993505));
#176412=CARTESIAN_POINT('Ctrl Pts',(-0.0289908141246323,-8.12780637205476,
55.9155112433766));
#176413=CARTESIAN_POINT('Ctrl Pts',(0.176847097141084,-8.12332522226783,
55.9235764932482));
#176414=CARTESIAN_POINT('Ctrl Pts',(0.382604879940012,-8.11884581690038,
55.9316386034838));
#176415=CARTESIAN_POINT('Ctrl Pts',(0.588255001873923,-8.10654316857554,
55.9397007137194));
#176416=CARTESIAN_POINT('Ctrl Pts',(0.793180577158063,-8.086442489409,55.947762823955));
#176417=CARTESIAN_POINT('Ctrl Pts',(0.998054245006541,-8.06634690172364,
55.9558228920664));
#176418=CARTESIAN_POINT('Ctrl Pts',(1.20220341731265,-8.03845725418866,
55.9638829601779));
#176419=CARTESIAN_POINT('Ctrl Pts',(1.40501538642423,-8.00285069999504,
55.9719430282893));
#176420=CARTESIAN_POINT('Ctrl Pts',(1.61086578575788,-7.96671070573456,
55.9801238484187));
#176421=CARTESIAN_POINT('Ctrl Pts',(1.81533826366942,-7.92262077005964,
55.9883046685482));
#176422=CARTESIAN_POINT('Ctrl Pts',(2.0178010609234,-7.87071575150802,55.9964854886776));
#176423=CARTESIAN_POINT('Ctrl Pts',(2.21729479539547,-7.81957190617372,
56.0045463392674));
#176424=CARTESIAN_POINT('Ctrl Pts',(2.41483707918783,-7.76084071773865,
56.0126071898573));
#176425=CARTESIAN_POINT('Ctrl Pts',(2.60983676881351,-7.69470204768508,
56.0206680404471));
#176426=CARTESIAN_POINT('Ctrl Pts',(2.80486879734938,-7.62855240913965,
56.0287302278551));
#176427=CARTESIAN_POINT('Ctrl Pts',(2.99735709055459,-7.55499294051914,
56.0367924152631));
#176428=CARTESIAN_POINT('Ctrl Pts',(3.18672790230071,-7.47425266091521,
56.0448546026711));
#176429=CARTESIAN_POINT('Ctrl Pts',(3.37615357913105,-7.39348898899332,
56.0529191258804));
#176430=CARTESIAN_POINT('Ctrl Pts',(3.56245968161549,-7.30554048087805,
56.0609836490897));
#176431=CARTESIAN_POINT('Ctrl Pts',(3.74509404969466,-7.2106836098557,56.069048172299));
#176432=CARTESIAN_POINT('Ctrl Pts',(3.93237147111605,-7.11341522386678,
56.0773177172237));
#176433=CARTESIAN_POINT('Ctrl Pts',(4.11578768127097,-7.00888273012241,
56.0855872621484));
#176434=CARTESIAN_POINT('Ctrl Pts',(4.29477602916872,-6.89743332129987,
56.0938568070732));
#176435=CARTESIAN_POINT('Ctrl Pts',(4.46956267802646,-6.78860015470516,
56.101932226853));
#176436=CARTESIAN_POINT('Ctrl Pts',(4.64012677096593,-6.67317137814245,
56.1100076466328));
#176437=CARTESIAN_POINT('Ctrl Pts',(4.80597140041664,-6.55151329548199,
56.1180830664126));
#176438=CARTESIAN_POINT('Ctrl Pts',(4.97779614240671,-6.42546840193691,
56.1264496739098));
#176439=CARTESIAN_POINT('Ctrl Pts',(5.14455444401536,-6.29273684981324,
56.134816281407));
#176440=CARTESIAN_POINT('Ctrl Pts',(5.30573229981658,-6.15377057788012,
56.1431828889042));
#176441=CARTESIAN_POINT('Ctrl Pts',(5.46691015561774,-6.01480430594705,
56.1515494964014));
#176442=CARTESIAN_POINT('Ctrl Pts',(5.62250731674663,-5.86960359742682,
56.1599161038986));
#176443=CARTESIAN_POINT('Ctrl Pts',(5.77205298320038,-5.71866172470689,
56.1682827113957));
#176444=CARTESIAN_POINT('Ctrl Pts',(5.91643912919243,-5.57292754338514,
56.1763606600264));
#176445=CARTESIAN_POINT('Ctrl Pts',(6.05546510078527,-5.42155839124349,
56.184438608657));
#176446=CARTESIAN_POINT('Ctrl Pts',(6.18867972450313,-5.26497206355587,
56.1925165572876));
#176447=CARTESIAN_POINT('Ctrl Pts',(6.32173132057101,-5.10857736573825,
56.2005846201494));
#176448=CARTESIAN_POINT('Ctrl Pts',(6.44898554226959,-4.94697845792061,
56.2086526830111));
#176449=CARTESIAN_POINT('Ctrl Pts',(6.57002744988545,-4.78063038419115,
56.2167207458728));
#176450=CARTESIAN_POINT('Ctrl Pts',(6.69093612857618,-4.61446540717174,
56.2247799283446));
#176451=CARTESIAN_POINT('Ctrl Pts',(6.80564593991808,-4.44356193885165,
56.2328391108164));
#176452=CARTESIAN_POINT('Ctrl Pts',(6.91378130758381,-4.2684090236767,56.2408982932882));
#176453=CARTESIAN_POINT('Ctrl Pts',(7.02177777914472,-4.09348108630681,
56.2489471240214));
#176454=CARTESIAN_POINT('Ctrl Pts',(7.12321648869526,-3.91431485850987,
56.2569959547546));
#176455=CARTESIAN_POINT('Ctrl Pts',(7.21776435450075,-3.73142938904092,
56.2650447854878));
#176456=CARTESIAN_POINT('Ctrl Pts',(7.31224070472476,-3.54868225332053,
56.2730875281216));
#176457=CARTESIAN_POINT('Ctrl Pts',(7.39983645606923,-3.36222176263079,
56.2811302707554));
#176458=CARTESIAN_POINT('Ctrl Pts',(7.48026309217137,-3.17259383382097,
56.2891730133891));
#176459=CARTESIAN_POINT('Ctrl Pts',(7.56062421774698,-2.98312036410657,
56.2972092049059));
#176460=CARTESIAN_POINT('Ctrl Pts',(7.63382775364498,-2.79048489256754,
56.3052453964226));
#176461=CARTESIAN_POINT('Ctrl Pts',(7.69963207399846,-2.59525595800378,
56.3132815879393));
#176462=CARTESIAN_POINT('Ctrl Pts',(7.73694046776287,-2.48456903158642,
56.317837784187));
#176463=CARTESIAN_POINT('Ctrl Pts',(7.77187128670256,-2.37304886704202,
56.3223939804346));
#176464=CARTESIAN_POINT('Ctrl Pts',(7.80438735588229,-2.26080197316009,
56.3269501766823));
#176465=CARTESIAN_POINT('Ctrl Pts',(7.85866325892142,-2.07343918047128,
56.3345553907196));
#176466=CARTESIAN_POINT('Ctrl Pts',(7.90618641271472,-1.88412563235468,
56.3421606047569));
#176467=CARTESIAN_POINT('Ctrl Pts',(7.94682714905332,-1.69340657420746,
56.3497658187942));
#176468=CARTESIAN_POINT('Ctrl Pts',(7.9874729292636,-1.50266384615311,56.3573719767053));
#176469=CARTESIAN_POINT('Ctrl Pts',(8.02123452283479,-1.31051561809717,
56.3649781346163));
#176470=CARTESIAN_POINT('Ctrl Pts',(8.04803359127215,-1.11751638746601,
56.3725842925274));
#176471=CARTESIAN_POINT('Ctrl Pts',(8.07485448690262,-0.924359963629182,
56.3801966454701));
#176472=CARTESIAN_POINT('Ctrl Pts',(8.09470148545109,-0.730351513950841,
56.3878089984128));
#176473=CARTESIAN_POINT('Ctrl Pts',(8.10754817391848,-0.53605052941974,
56.3954213513555));
#176474=CARTESIAN_POINT('Ctrl Pts',(8.11951963742666,-0.354986969590803,
56.4025150864995));
#176475=CARTESIAN_POINT('Ctrl Pts',(8.12541265295082,-0.173669645053181,
56.4096088216436));
#176476=CARTESIAN_POINT('Ctrl Pts',(8.12524658453948,0.00745002882984703,
56.4167025567876));
#176477=CARTESIAN_POINT('',(8.12524979689129,-0.00180012532809755,52.4166320361364));
#176478=CARTESIAN_POINT('Ctrl Pts',(8.12524979923223,-0.00180626037467281,
52.41679142628));
#176479=CARTESIAN_POINT('Ctrl Pts',(8.12529142980181,0.185463959284471,
52.4241148867614));
#176480=CARTESIAN_POINT('Ctrl Pts',(8.11885447565195,0.372914385266139,
52.4314383472427));
#176481=CARTESIAN_POINT('Ctrl Pts',(8.10592778611965,0.560019900283289,
52.4387618077241));
#176482=CARTESIAN_POINT('Ctrl Pts',(8.09300372005407,0.747087442307473,
52.4460837819119));
#176483=CARTESIAN_POINT('Ctrl Pts',(8.07359255433145,0.933809827599829,
52.4534057560997));
#176484=CARTESIAN_POINT('Ctrl Pts',(8.04773524373084,1.11966289985534,52.4607277302875));
#176485=CARTESIAN_POINT('Ctrl Pts',(8.02188165943195,1.30548918879088,52.4680486493043));
#176486=CARTESIAN_POINT('Ctrl Pts',(7.98958383553074,1.49044603221675,52.4753695683211));
#176487=CARTESIAN_POINT('Ctrl Pts',(7.95093442865585,1.67401591202566,52.4826904873379));
#176488=CARTESIAN_POINT('Ctrl Pts',(7.91227199465363,1.85764766569988,52.4900138739358));
#176489=CARTESIAN_POINT('Ctrl Pts',(7.86725378425988,2.03989114479142,52.4973372605336));
#176490=CARTESIAN_POINT('Ctrl Pts',(7.8160232871797,2.22024042318949,52.5046606471314));
#176491=CARTESIAN_POINT('Ctrl Pts',(7.78274734470621,2.33738338597818,52.5094174346902));
#176492=CARTESIAN_POINT('Ctrl Pts',(7.74685150652963,2.4537274576232,52.514174222249));
#176493=CARTESIAN_POINT('Ctrl Pts',(7.70838622756085,2.56913785719065,52.5189310098078));
#176494=CARTESIAN_POINT('Ctrl Pts',(7.63379529391426,2.79293889768875,52.5281552565747));
#176495=CARTESIAN_POINT('Ctrl Pts',(7.54954791469676,3.01320771803129,52.5373795033417));
#176496=CARTESIAN_POINT('Ctrl Pts',(7.4559985125789,3.22920636425132,52.5466037501086));
#176497=CARTESIAN_POINT('Ctrl Pts',(7.36202586583066,3.44618225100003,52.5558697300436));
#176498=CARTESIAN_POINT('Ctrl Pts',(7.25866691095433,3.65884919165463,52.5651357099785));
#176499=CARTESIAN_POINT('Ctrl Pts',(7.1463242493121,3.86648901281173,52.5744016899135));
#176500=CARTESIAN_POINT('Ctrl Pts',(7.03351765094578,4.07498631532998,52.5837059351727));
#176501=CARTESIAN_POINT('Ctrl Pts',(6.91165304755985,4.2784148422899,52.5930101804319));
#176502=CARTESIAN_POINT('Ctrl Pts',(6.7811806751285,4.47607821801225,52.6023144256911));
#176503=CARTESIAN_POINT('Ctrl Pts',(6.65058492372394,4.67392851073386,52.6116274693511));
#176504=CARTESIAN_POINT('Ctrl Pts',(6.51136516903268,4.86600269982851,52.6209405130112));
#176505=CARTESIAN_POINT('Ctrl Pts',(6.36401470585195,5.05163383334541,52.6302535566712));
#176506=CARTESIAN_POINT('Ctrl Pts',(6.21679692851287,5.23709781012148,52.6395582141408));
#176507=CARTESIAN_POINT('Ctrl Pts',(6.06146312303957,5.41613028144629,52.6488628716105));
#176508=CARTESIAN_POINT('Ctrl Pts',(5.89854619522163,5.58809809732581,52.6581675290801));
#176509=CARTESIAN_POINT('Ctrl Pts',(5.78513954772361,5.70780507767257,52.6646445110849));
#176510=CARTESIAN_POINT('Ctrl Pts',(5.66805929710808,5.82408949441311,52.6711214930897));
#176511=CARTESIAN_POINT('Ctrl Pts',(5.54749678423229,5.93674717260491,52.6775984750944));
#176512=CARTESIAN_POINT('Ctrl Pts',(5.40290965348903,6.07185426400015,52.6853661320685));
#176513=CARTESIAN_POINT('Ctrl Pts',(5.2532451898613,6.20180571678652,52.6931337890425));
#176514=CARTESIAN_POINT('Ctrl Pts',(5.09891321461151,6.3261972457678,52.7009014460165));
#176515=CARTESIAN_POINT('Ctrl Pts',(4.94467551481463,6.45051278876035,52.7086643580284));
#176516=CARTESIAN_POINT('Ctrl Pts',(4.78577625325051,6.56927495205543,52.7164272700403));
#176517=CARTESIAN_POINT('Ctrl Pts',(4.62266063250388,6.68211764631534,52.7241901820522));
#176518=CARTESIAN_POINT('Ctrl Pts',(4.4596160671024,6.79491118478899,52.7319497124358));
#176519=CARTESIAN_POINT('Ctrl Pts',(4.29235908890434,6.90179019128051,52.7397092428194));
#176520=CARTESIAN_POINT('Ctrl Pts',(4.1213665088273,7.00242998268577,52.747468773203));
#176521=CARTESIAN_POINT('Ctrl Pts',(3.95039498770512,7.10305737958349,52.7552273479452));
#176522=CARTESIAN_POINT('Ctrl Pts',(3.77568907959939,7.19744690792926,52.7629859226873));
#176523=CARTESIAN_POINT('Ctrl Pts',(3.59775334397401,7.28531800530518,52.7707444974295));
#176524=CARTESIAN_POINT('Ctrl Pts',(3.4198345896975,7.37318071667726,52.7785023317298));
#176525=CARTESIAN_POINT('Ctrl Pts',(3.2386869381476,7.45452608415542,52.7862601660301));
#176526=CARTESIAN_POINT('Ctrl Pts',(3.0548381577906,7.5291202269725,52.7940180003304));
#176527=CARTESIAN_POINT('Ctrl Pts',(2.87091998578194,7.60374252450873,52.8017787627379));
#176528=CARTESIAN_POINT('Ctrl Pts',(2.68429897349192,7.67160837433803,52.8095395251454));
#176529=CARTESIAN_POINT('Ctrl Pts',(2.4955220439955,7.73253239827888,52.8173002875529));
#176530=CARTESIAN_POINT('Ctrl Pts',(2.34174515461608,7.78216085083975,52.8236221718288));
#176531=CARTESIAN_POINT('Ctrl Pts',(2.18653809678768,7.82718383344977,52.8299440561048));
#176532=CARTESIAN_POINT('Ctrl Pts',(2.03020328100823,7.86752579914953,52.8362659403807));
#176533=CARTESIAN_POINT('Ctrl Pts',(1.8225771514488,7.92110341175808,52.8446619483792));
#176534=CARTESIAN_POINT('Ctrl Pts',(1.61286290931407,7.96644911872512,52.8530579563777));
#176535=CARTESIAN_POINT('Ctrl Pts',(1.40171550536911,8.00342934025832,52.8614539643762));
#176536=CARTESIAN_POINT('Ctrl Pts',(1.19051779013239,8.04041837327905,52.8698519729393));
#176537=CARTESIAN_POINT('Ctrl Pts',(0.977886494570286,8.06903789590412,
52.8782499815023));
#176538=CARTESIAN_POINT('Ctrl Pts',(0.764484866176533,8.0892057985866,52.8866479900654));
#176539=CARTESIAN_POINT('Ctrl Pts',(0.551036542337206,8.1093781143057,52.8950478362374));
#176540=CARTESIAN_POINT('Ctrl Pts',(0.336817815055019,8.12109509325748,
52.9034476824095));
#176541=CARTESIAN_POINT('Ctrl Pts',(0.122496212510106,8.12432657150245,
52.9118475285815));
#176542=CARTESIAN_POINT('Ctrl Pts',(-0.0919039381742978,8.12755923407322,
52.9202504532687));
#176543=CARTESIAN_POINT('Ctrl Pts',(-0.306406772346929,8.12230017603941,
52.9286533779558));
#176544=CARTESIAN_POINT('Ctrl Pts',(-0.520344185914271,8.10857135941253,
52.937056302643));
#176545=CARTESIAN_POINT('Ctrl Pts',(-0.734304306751976,8.09484108561206,
52.9454601192147));
#176546=CARTESIAN_POINT('Ctrl Pts',(-0.947698620842927,8.07263927854439,
52.9538639357865));
#176547=CARTESIAN_POINT('Ctrl Pts',(-1.15986297180958,8.04203988109516,
52.9622677523582));
#176548=CARTESIAN_POINT('Ctrl Pts',(-1.37207112322722,8.01143416652713,
52.970673303863));
#176549=CARTESIAN_POINT('Ctrl Pts',(-1.58304853993314,7.97242743636115,
52.9790788553679));
#176550=CARTESIAN_POINT('Ctrl Pts',(-1.79213879196529,7.92514517929061,
52.9874844068727));
#176551=CARTESIAN_POINT('Ctrl Pts',(-1.85390404454704,7.91117800233131,
52.9899674064709));
#176552=CARTESIAN_POINT('Ctrl Pts',(-1.91550468941563,7.89648903272553,
52.9924504060691));
#176553=CARTESIAN_POINT('Ctrl Pts',(-1.97692399346394,7.8810823550174,52.9949334056673));
#176554=CARTESIAN_POINT('Ctrl Pts',(-2.18546791597217,7.82877031645138,
53.0033642155539));
#176555=CARTESIAN_POINT('Ctrl Pts',(-2.39194333430613,7.76817430305625,
53.0117950254405));
#176556=CARTESIAN_POINT('Ctrl Pts',(-2.5957044001731,7.69948090649117,53.020225835327));
#176557=CARTESIAN_POINT('Ctrl Pts',(-2.79943222349145,7.63079871689325,
53.0286552697712));
#176558=CARTESIAN_POINT('Ctrl Pts',(-3.00044632993504,7.55402186671484,
53.0370847042154));
#176559=CARTESIAN_POINT('Ctrl Pts',(-3.1981173121605,7.46938640185118,53.0455141386595));
#176560=CARTESIAN_POINT('Ctrl Pts',(-3.39574895585102,7.3847677803054,53.0539418955606));
#176561=CARTESIAN_POINT('Ctrl Pts',(-3.59003856248263,7.29229377063194,
53.0623696524616));
#176562=CARTESIAN_POINT('Ctrl Pts',(-3.78037692044528,7.19224845940855,
53.0707974093626));
#176563=CARTESIAN_POINT('Ctrl Pts',(-3.97066168704092,7.09223131678475,
53.0792227933577));
#176564=CARTESIAN_POINT('Ctrl Pts',(-4.15699719452033,6.98464725259868,
53.0876481773528));
#176565=CARTESIAN_POINT('Ctrl Pts',(-4.33879814483341,6.86982665144399,
53.096073561348));
#176566=CARTESIAN_POINT('Ctrl Pts',(-4.52054763823719,6.75503854909224,
53.1044965606239));
#176567=CARTESIAN_POINT('Ctrl Pts',(-4.69776491502061,6.63301813953614,
53.1129195598998));
#176568=CARTESIAN_POINT('Ctrl Pts',(-4.86989202172793,6.50414016294319,
53.1213425591757));
#176569=CARTESIAN_POINT('Ctrl Pts',(-5.04195466287281,6.3753104541182,53.1297624038445));
#176570=CARTESIAN_POINT('Ctrl Pts',(-5.20893073079048,6.23962846456765,
53.1381822485134));
#176571=CARTESIAN_POINT('Ctrl Pts',(-5.37029303830708,6.09751098770724,
53.1466020931822));
#176572=CARTESIAN_POINT('Ctrl Pts',(-5.41500245102512,6.05813383064257,
53.148935019106));
#176573=CARTESIAN_POINT('Ctrl Pts',(-5.4592810817868,6.01826286209088,53.1512679450297));
#176574=CARTESIAN_POINT('Ctrl Pts',(-5.50311816005396,5.9779075000358,53.1536008709535));
#176575=CARTESIAN_POINT('Ctrl Pts',(-5.64845632790801,5.84411267118276,
53.1613354918019));
#176576=CARTESIAN_POINT('Ctrl Pts',(-5.78900199474849,5.70493168866682,
53.1690701126502));
#176577=CARTESIAN_POINT('Ctrl Pts',(-5.92433287199729,5.56075242968722,
53.1768047334986));
#176578=CARTESIAN_POINT('Ctrl Pts',(-6.05962189912813,5.41661775712514,
53.1845369624701));
#176579=CARTESIAN_POINT('Ctrl Pts',(-6.18969910655291,5.26748814351576,
53.1922691914416));
#176580=CARTESIAN_POINT('Ctrl Pts',(-6.31417889455817,5.11378846355773,
53.2000014204131));
#176581=CARTESIAN_POINT('Ctrl Pts',(-6.4386423110938,4.96010899804321,53.2077326324489));
#176582=CARTESIAN_POINT('Ctrl Pts',(-6.55750955281092,4.80186093838473,
53.2154638444846));
#176583=CARTESIAN_POINT('Ctrl Pts',(-6.67043508813259,4.63950248383483,
53.2231950565203));
#176584=CARTESIAN_POINT('Ctrl Pts',(-6.78340106456531,4.47708588516128,
53.2309290372726));
#176585=CARTESIAN_POINT('Ctrl Pts',(-6.89042087788212,4.31055623859291,
53.2386630180249));
#176586=CARTESIAN_POINT('Ctrl Pts',(-6.99119178996117,4.14040154073002,
53.2463969987773));
#176587=CARTESIAN_POINT('Ctrl Pts',(-7.09197973207841,3.97021808713849,
53.2541322865534));
#176588=CARTESIAN_POINT('Ctrl Pts',(-7.18651649518555,3.79640866959065,
53.2618675743296));
#176589=CARTESIAN_POINT('Ctrl Pts',(-7.27454510353943,3.6194863032025,53.2696028621058));
#176590=CARTESIAN_POINT('Ctrl Pts',(-7.36264578837941,3.44241907547074,
53.277344483418));
#176591=CARTESIAN_POINT('Ctrl Pts',(-7.44422752112627,3.26223412640846,
53.2850861047302));
#176592=CARTESIAN_POINT('Ctrl Pts',(-7.5190809496,3.07946573870573,53.2928277260425));
#176593=CARTESIAN_POINT('Ctrl Pts',(-7.58173777845746,2.92647758809798,
53.2993079294417));
#176594=CARTESIAN_POINT('Ctrl Pts',(-7.63968110812795,2.77167975125065,
53.3057881328409));
#176595=CARTESIAN_POINT('Ctrl Pts',(-7.69281501789776,2.61539378734957,
53.3122683362401));
#176596=CARTESIAN_POINT('Ctrl Pts',(-7.76986127328381,2.38877300336918,
53.321664885604));
#176597=CARTESIAN_POINT('Ctrl Pts',(-7.83683934975107,2.15889379270417,
53.3310614349679));
#176598=CARTESIAN_POINT('Ctrl Pts',(-7.8935407830906,1.92657765693091,53.3404579843318));
#176599=CARTESIAN_POINT('Ctrl Pts',(-7.95032228177454,1.69393347880798,
53.3498678021074));
#176600=CARTESIAN_POINT('Ctrl Pts',(-7.99679810175101,1.45884552910251,
53.359277619883));
#176601=CARTESIAN_POINT('Ctrl Pts',(-8.0328103301751,1.22214801146677,53.3686874376586));
#176602=CARTESIAN_POINT('Ctrl Pts',(-8.06876814688821,0.985808125598951,
53.3780830379223));
#176603=CARTESIAN_POINT('Ctrl Pts',(-8.09429396780832,0.747863569393553,
53.3874786381861));
#176604=CARTESIAN_POINT('Ctrl Pts',(-8.10928174435626,0.509153368986473,
53.3968742384498));
#176605=CARTESIAN_POINT('Ctrl Pts',(-8.12423175226499,0.271044709402109,
53.4062461621504));
#176606=CARTESIAN_POINT('Ctrl Pts',(-8.12869673648614,0.0321742965836574,
53.4156180858511));
#176607=CARTESIAN_POINT('Ctrl Pts',(-8.12262253898462,-0.206617162111417,
53.4249900095518));
#176608=CARTESIAN_POINT('Ctrl Pts',(-8.11658772510818,-0.443860354837681,
53.4343011679696));
#176609=CARTESIAN_POINT('Ctrl Pts',(-8.1001499332365,-0.681025568421049,
53.4436123263874));
#176610=CARTESIAN_POINT('Ctrl Pts',(-8.07330682219572,-0.91728104591125,
53.4529234848052));
#176611=CARTESIAN_POINT('Ctrl Pts',(-8.05599760400982,-1.06962544449004,
53.458927590379));
#176612=CARTESIAN_POINT('Ctrl Pts',(-8.03436283170225,-1.22159142398268,
53.4649316959528));
#176613=CARTESIAN_POINT('Ctrl Pts',(-8.00841329672666,-1.3729544898909,
53.4709358015266));
#176614=CARTESIAN_POINT('Ctrl Pts',(-7.97570399173204,-1.56374714541908,
53.4785039572033));
#176615=CARTESIAN_POINT('Ctrl Pts',(-7.93614904893175,-1.75350540783528,
53.4860721128799));
#176616=CARTESIAN_POINT('Ctrl Pts',(-7.88983874489199,-1.94168281191886,
53.4936402685566));
#176617=CARTESIAN_POINT('Ctrl Pts',(-7.84354123413481,-2.12980823174636,
53.5012063335203));
#176618=CARTESIAN_POINT('Ctrl Pts',(-7.79049216315058,-2.31635330559633,
53.508772398484));
#176619=CARTESIAN_POINT('Ctrl Pts',(-7.73083284066094,-2.50078210811303,
53.5163384634477));
#176620=CARTESIAN_POINT('Ctrl Pts',(-7.67117870900688,-2.68519486385699,
53.5239038701036));
#176621=CARTESIAN_POINT('Ctrl Pts',(-7.60491558457017,-2.86749136525201,
53.5314692767595));
#176622=CARTESIAN_POINT('Ctrl Pts',(-7.53223451333963,-3.04715125954641,
53.5390346834153));
#176623=CARTESIAN_POINT('Ctrl Pts',(-7.45951771598275,-3.22689946503346,
53.5466038088204));
#176624=CARTESIAN_POINT('Ctrl Pts',(-7.38037680440389,-3.40400813173496,
53.5541729342254));
#176625=CARTESIAN_POINT('Ctrl Pts',(-7.29505104634859,-3.57797677377431,
53.5617420596305));
#176626=CARTESIAN_POINT('Ctrl Pts',(-7.20970627224065,-3.75198418718738,
53.5693128719222));
#176627=CARTESIAN_POINT('Ctrl Pts',(-7.11817407806062,-3.9228498569337,
53.576883684214));
#176628=CARTESIAN_POINT('Ctrl Pts',(-7.02073938188642,-4.09009854332742,
53.5844544965058));
#176629=CARTESIAN_POINT('Ctrl Pts',(-6.9232059119717,-4.25751677690504,
53.5920329836554));
#176630=CARTESIAN_POINT('Ctrl Pts',(-6.81975818026263,-4.42131038948132,
53.5996114708051));
#176631=CARTESIAN_POINT('Ctrl Pts',(-6.71072457615695,-4.58103298672506,
53.6071899579548));
#176632=CARTESIAN_POINT('Ctrl Pts',(-6.60323593554964,-4.7384923772755,
53.6146610609075));
#176633=CARTESIAN_POINT('Ctrl Pts',(-6.49031892947357,-4.89199512838687,
53.6221321638602));
#176634=CARTESIAN_POINT('Ctrl Pts',(-6.37232536909627,-5.04114639272379,
53.6296032668129));
#176635=CARTESIAN_POINT('Ctrl Pts',(-6.24479984339853,-5.20234665935044,
53.6376779136711));
#176636=CARTESIAN_POINT('Ctrl Pts',(-6.11107242724856,-5.35880848322185,
53.6457525605292));
#176637=CARTESIAN_POINT('Ctrl Pts',(-5.97152241968435,-5.5100460573127,
53.6538272073874));
#176638=CARTESIAN_POINT('Ctrl Pts',(-5.83206481307636,-5.66118349169946,
53.6618965077386));
#176639=CARTESIAN_POINT('Ctrl Pts',(-5.68679251715282,-5.80710334209315,
53.6699658080898));
#176640=CARTESIAN_POINT('Ctrl Pts',(-5.53612476371952,-5.94735320651392,
53.678035108441));
#176641=CARTESIAN_POINT('Ctrl Pts',(-5.38553623836849,-6.08752932106094,
53.6861001655803));
#176642=CARTESIAN_POINT('Ctrl Pts',(-5.22955814501596,-6.22204118025769,
53.6941652227197));
#176643=CARTESIAN_POINT('Ctrl Pts',(-5.06864663283712,-6.3504731220539,
53.7022302798591));
#176644=CARTESIAN_POINT('Ctrl Pts',(-4.90779782796481,-6.47885501385036,
53.7102921940411));
#176645=CARTESIAN_POINT('Ctrl Pts',(-4.74201968601487,-6.60116151651033,
53.7183541082232));
#176646=CARTESIAN_POINT('Ctrl Pts',(-4.57180197775206,-6.71701676629754,
53.7264160224053));
#176647=CARTESIAN_POINT('Ctrl Pts',(-4.4016274473332,-6.83284262795619,
53.7344758915823));
#176648=CARTESIAN_POINT('Ctrl Pts',(-4.22701585865114,-6.94222032293446,
53.7425357607594));
#176649=CARTESIAN_POINT('Ctrl Pts',(-4.0484870533218,-7.04481654421077,
53.7505956299364));
#176650=CARTESIAN_POINT('Ctrl Pts',(-3.86727648178455,-7.14895391218758,
53.7587765702468));
#176651=CARTESIAN_POINT('Ctrl Pts',(-3.68203034285036,-7.24610425315686,
53.7669575105572));
#176652=CARTESIAN_POINT('Ctrl Pts',(-3.49332014501591,-7.3359663253675,
53.7751384508675));
#176653=CARTESIAN_POINT('Ctrl Pts',(-3.30738476615581,-7.42450705413245,
53.7831990975814));
#176654=CARTESIAN_POINT('Ctrl Pts',(-3.11808680048448,-7.50597225396094,
53.7912597442952));
#176655=CARTESIAN_POINT('Ctrl Pts',(-2.92599533830767,-7.58012129472225,
53.7993203910091));
#176656=CARTESIAN_POINT('Ctrl Pts',(-2.73387204916043,-7.65428262098184,
53.8073823732636));
#176657=CARTESIAN_POINT('Ctrl Pts',(-2.53895463601142,-7.72112525625011,
53.8154443555182));
#176658=CARTESIAN_POINT('Ctrl Pts',(-2.34183032616524,-7.78045745994108,
53.8235063377727));
#176659=CARTESIAN_POINT('Ctrl Pts',(-2.14464892525096,-7.83980684740246,
53.8315706549355));
#176660=CARTESIAN_POINT('Ctrl Pts',(-1.94525965622814,-7.8916413735799,
53.8396349720983));
#176661=CARTESIAN_POINT('Ctrl Pts',(-1.7442635756675,-7.93581956329021,
53.8476992892611));
#176662=CARTESIAN_POINT('Ctrl Pts',(-1.53814329739408,-7.98112403256795,
53.8559691982715));
#176663=CARTESIAN_POINT('Ctrl Pts',(-1.33033353834054,-8.01837652543524,
53.8642391072819));
#176664=CARTESIAN_POINT('Ctrl Pts',(-1.12149192529827,-8.04748056375353,
53.8725090162922));
#176665=CARTESIAN_POINT('Ctrl Pts',(-0.917566984062273,-8.07589941772295,
53.8805842302518));
#176666=CARTESIAN_POINT('Ctrl Pts',(-0.712658547025337,-8.09654916905283,
53.8886594442113));
#176667=CARTESIAN_POINT('Ctrl Pts',(-0.507382800075561,-8.10939271811937,
53.8967346581708));
#176668=CARTESIAN_POINT('Ctrl Pts',(-0.294683193115528,-8.12270075805598,
53.9051019147067));
#176669=CARTESIAN_POINT('Ctrl Pts',(-0.0815895931428846,-8.12762743478942,
53.9134691712425));
#176670=CARTESIAN_POINT('Ctrl Pts',(0.131213614354412,-8.12419045504893,
53.9218364277783));
#176671=CARTESIAN_POINT('Ctrl Pts',(0.344016821851631,-8.12075347530843,
53.9302036843141));
#176672=CARTESIAN_POINT('Ctrl Pts',(0.556529264119323,-8.10895289716088,
53.9385709408499));
#176673=CARTESIAN_POINT('Ctrl Pts',(0.768073252409577,-8.08886586867609,
53.9469381973857));
#176674=CARTESIAN_POINT('Ctrl Pts',(0.972307163530668,-8.06947296404473,
53.9550163164638));
#176675=CARTESIAN_POINT('Ctrl Pts',(1.17603556407372,-8.04231901093511,
53.9630944355419));
#176676=CARTESIAN_POINT('Ctrl Pts',(1.37864434331301,-8.00743575292059,
53.97117255462));
#176677=CARTESIAN_POINT('Ctrl Pts',(1.58100514933681,-7.97259518858248,
53.979240786875));
#176678=CARTESIAN_POINT('Ctrl Pts',(1.78224875691176,-7.93004422929355,
53.9873090191299));
#176679=CARTESIAN_POINT('Ctrl Pts',(1.98176501262701,-7.87986643270223,
53.9953772513849));
#176680=CARTESIAN_POINT('Ctrl Pts',(2.18106163449512,-7.82974387342714,
54.0034366018729));
#176681=CARTESIAN_POINT('Ctrl Pts',(2.37863439093669,-7.77201129082964,
54.0114959523609));
#176682=CARTESIAN_POINT('Ctrl Pts',(2.57388156976952,-7.70680356745264,
54.0195553028489));
#176683=CARTESIAN_POINT('Ctrl Pts',(2.76887789789266,-7.64167962200158,
54.0276042988017));
#176684=CARTESIAN_POINT('Ctrl Pts',(2.96155431105262,-7.56909979483945,
54.0356532947545));
#176685=CARTESIAN_POINT('Ctrl Pts',(3.15132250263827,-7.48924923118904,
54.0437022907072));
#176686=CARTESIAN_POINT('Ctrl Pts',(3.34094711543319,-7.40945908254956,
54.0517451967822));
#176687=CARTESIAN_POINT('Ctrl Pts',(3.52766760279783,-7.32240928431047,
54.0597881028571));
#176688=CARTESIAN_POINT('Ctrl Pts',(3.71091266240122,-7.22833416317551,
54.0678310089321));
#176689=CARTESIAN_POINT('Ctrl Pts',(3.89400838944722,-7.13433570701835,
54.0758673605725));
#176690=CARTESIAN_POINT('Ctrl Pts',(4.07363405838302,-7.0333234921172,54.083903712213));
#176691=CARTESIAN_POINT('Ctrl Pts',(4.24923987684056,-6.92557925603108,
54.0919400638535));
#176692=CARTESIAN_POINT('Ctrl Pts',(4.3487775266202,-6.86450720197548,54.0964952634598));
#176693=CARTESIAN_POINT('Ctrl Pts',(4.44702402957637,-6.80127308141812,
54.101050463066));
#176694=CARTESIAN_POINT('Ctrl Pts',(4.54388266994327,-6.73593481591748,
54.1056056626723));
#176695=CARTESIAN_POINT('Ctrl Pts',(4.71476441173592,-6.62066253280297,
54.1136421211646));
#176696=CARTESIAN_POINT('Ctrl Pts',(4.88118962102054,-6.49892972876899,
54.121678579657));
#176697=CARTESIAN_POINT('Ctrl Pts',(5.04267165464983,-6.37111843759721,
54.1297150381493));
#176698=CARTESIAN_POINT('Ctrl Pts',(5.2042512233777,-6.24322994844493,54.1377563506601));
#176699=CARTESIAN_POINT('Ctrl Pts',(5.3608814122162,-6.10925584351674,54.1457976631709));
#176700=CARTESIAN_POINT('Ctrl Pts',(5.51210984118968,-5.96961746355325,
54.1538389756816));
#176701=CARTESIAN_POINT('Ctrl Pts',(5.66344810492306,-5.82987766649482,
54.1618861284675));
#176702=CARTESIAN_POINT('Ctrl Pts',(5.80937654981052,-5.68446560085876,
54.1699332812534));
#176703=CARTESIAN_POINT('Ctrl Pts',(5.94948030747646,-5.53383877913423,
54.1779804340393));
#176704=CARTESIAN_POINT('Ctrl Pts',(6.08979055673919,-5.38298995641946,
54.1860394471026));
#176705=CARTESIAN_POINT('Ctrl Pts',(6.22425874553431,-5.22691124793029,
54.1940984601659));
#176706=CARTESIAN_POINT('Ctrl Pts',(6.35250978663326,-5.06609385752264,
54.2021574732292));
#176707=CARTESIAN_POINT('Ctrl Pts',(6.48086462185065,-4.90514631691017,
54.2102230084863));
#176708=CARTESIAN_POINT('Ctrl Pts',(6.60299208143421,-4.7394526949591,54.2182885437435));
#176709=CARTESIAN_POINT('Ctrl Pts',(6.71856045953086,-4.56953311774063,
54.2263540790006));
#176710=CARTESIAN_POINT('Ctrl Pts',(6.83431030468434,-4.39934673046492,
54.2344322788722));
#176711=CARTESIAN_POINT('Ctrl Pts',(6.94348031450639,-4.22492139177615,
54.2425104787438));
#176712=CARTESIAN_POINT('Ctrl Pts',(7.04578389662639,-4.04680328710703,
54.2505886786153));
#176713=CARTESIAN_POINT('Ctrl Pts',(7.10355122967148,-3.9462260867729,54.2551501617297));
#176714=CARTESIAN_POINT('Ctrl Pts',(7.15913007684663,-3.84447186092738,
54.2597116448442));
#176715=CARTESIAN_POINT('Ctrl Pts',(7.21247563134185,-3.74164172921459,
54.2642731279586));
#176716=CARTESIAN_POINT('Ctrl Pts',(7.31207324622793,-3.54965505002594,
54.2727895421723));
#176717=CARTESIAN_POINT('Ctrl Pts',(7.40405480498203,-3.35358662842629,
54.2813059563859));
#176718=CARTESIAN_POINT('Ctrl Pts',(7.48810513339414,-3.1540401192338,54.2898223705996));
#176719=CARTESIAN_POINT('Ctrl Pts',(7.57205211902636,-2.95473895936195,
54.2983283135881));
#176720=CARTESIAN_POINT('Ctrl Pts',(7.64808723974097,-2.75196847756056,
54.3068342565765));
#176721=CARTESIAN_POINT('Ctrl Pts',(7.71594230646601,-2.54635462687113,
54.315340199565));
#176722=CARTESIAN_POINT('Ctrl Pts',(7.7836627303163,-2.34114876988477,54.3238292644532));
#176723=CARTESIAN_POINT('Ctrl Pts',(7.84323542574184,-2.13311104534834,
54.3323183293414));
#176724=CARTESIAN_POINT('Ctrl Pts',(7.89444118896209,-1.92288477983439,
54.3408073942297));
#176725=CARTESIAN_POINT('Ctrl Pts',(7.94558245025501,-1.71292332824858,
54.3492857657699));
#176726=CARTESIAN_POINT('Ctrl Pts',(7.98837774946234,-1.50077907902443,
54.3577641373101));
#176727=CARTESIAN_POINT('Ctrl Pts',(8.02265754136298,-1.28711053779843,
54.3662425088503));
#176728=CARTESIAN_POINT('Ctrl Pts',(8.0568660294448,-1.07388643867972,54.3747032449198));
#176729=CARTESIAN_POINT('Ctrl Pts',(8.08259432589578,-0.859144623191298,
54.3831639809892));
#176730=CARTESIAN_POINT('Ctrl Pts',(8.09972385147236,-0.643553488367279,
54.3916247170586));
#176731=CARTESIAN_POINT('Ctrl Pts',(8.11664796987523,-0.430547595351899,
54.3999839969683));
#176732=CARTESIAN_POINT('Ctrl Pts',(8.12517833118536,-0.216712883417576,
54.4083432768779));
#176733=CARTESIAN_POINT('Ctrl Pts',(8.12524955008195,-0.0027039587645105,
54.4167025567876));
#176734=CARTESIAN_POINT('',(8.12524999842753,0.000155745727534607,50.4167086581892));
#176735=CARTESIAN_POINT('Ctrl Pts',(8.12524999842753,0.000155745727534607,
50.4167086581892));
#176736=CARTESIAN_POINT('Ctrl Pts',(8.12520464167094,2.24634946216138,50.5047042175299));
#176737=CARTESIAN_POINT('Ctrl Pts',(7.14394733579225,4.47538755847567,50.5926997768706));
#176738=CARTESIAN_POINT('Ctrl Pts',(3.83078204044946,7.50935546634353,50.7686929293524));
#176739=CARTESIAN_POINT('Ctrl Pts',(1.52412477697767,8.29110090552131,50.8566905224936));
#176740=CARTESIAN_POINT('Ctrl Pts',(-2.95101623932526,7.89663306204436,
51.032685708776));
#176741=CARTESIAN_POINT('Ctrl Pts',(-5.08535169588699,6.72342983085812,
51.1206833019172));
#176742=CARTESIAN_POINT('Ctrl Pts',(-7.81671694684382,3.15661951052992,
51.2966784881996));
#176743=CARTESIAN_POINT('Ctrl Pts',(-8.39290461146695,0.790229551554735,
51.3846760813408));
#176744=CARTESIAN_POINT('Ctrl Pts',(-7.60701611462514,-3.63299000730349,
51.5606712676232));
#176745=CARTESIAN_POINT('Ctrl Pts',(-6.25093680401409,-5.65606750609959,
51.6486688607644));
#176746=CARTESIAN_POINT('Ctrl Pts',(-2.45807268688641,-8.0636957548829,
51.8246640470468));
#176747=CARTESIAN_POINT('Ctrl Pts',(-0.0502299510463028,-8.42987470330084,
51.912661640188));
#176748=CARTESIAN_POINT('Ctrl Pts',(4.28689960880906,-7.25863639434614,
52.0886568264704));
#176749=CARTESIAN_POINT('Ctrl Pts',(6.18309125557085,-5.7301564626646,52.1766544196116));
#176750=CARTESIAN_POINT('Ctrl Pts',(7.81022974018296,-2.58694001339646,
52.3153120205474));
#176751=CARTESIAN_POINT('Ctrl Pts',(8.12495798447121,-1.29495785838389,
52.3659720283419));
#176752=CARTESIAN_POINT('Ctrl Pts',(8.12524979689129,-0.00180012532809755,
52.4166320361364));
#176753=CARTESIAN_POINT('',(8.12524962724961,0.00113542683362771,48.4167025567876));
#176754=CARTESIAN_POINT('Ctrl Pts',(8.12524824860312,0.00533489193623286,
48.4167025567876));
#176755=CARTESIAN_POINT('Ctrl Pts',(8.12509405526136,0.240177358298132,
48.4258982129203));
#176756=CARTESIAN_POINT('Ctrl Pts',(8.11475436208719,0.474765486234928,
48.4350938690529));
#176757=CARTESIAN_POINT('Ctrl Pts',(8.09431945547053,0.708293805769365,
48.4442895251855));
#176758=CARTESIAN_POINT('Ctrl Pts',(8.0737852173659,0.94295727683138,48.4535298802358));
#176759=CARTESIAN_POINT('Ctrl Pts',(8.04305742039561,1.17655052682022,48.462770235286));
#176760=CARTESIAN_POINT('Ctrl Pts',(8.00227883614591,1.40826879219532,48.4720105903362));
#176761=CARTESIAN_POINT('Ctrl Pts',(7.96144009132553,1.64032891110307,48.4812645776653));
#176762=CARTESIAN_POINT('Ctrl Pts',(7.91052092462163,1.87050843279415,48.4905185649944));
#176763=CARTESIAN_POINT('Ctrl Pts',(7.84971528909508,2.09801273653117,48.4997725523235));
#176764=CARTESIAN_POINT('Ctrl Pts',(7.78890031216287,2.32555199114029,48.5090279613177));
#176765=CARTESIAN_POINT('Ctrl Pts',(7.71819586053827,2.55041513008745,48.5182833703119));
#176766=CARTESIAN_POINT('Ctrl Pts',(7.63784592382679,2.77182200120833,48.5275387793061));
#176767=CARTESIAN_POINT('Ctrl Pts',(7.56635283748268,2.96882353228684,48.5357739787531));
#176768=CARTESIAN_POINT('Ctrl Pts',(7.48722417490742,3.1630889238551,48.5440091782001));
#176769=CARTESIAN_POINT('Ctrl Pts',(7.4006648329993,3.35407924654553,48.5522443776471));
#176770=CARTESIAN_POINT('Ctrl Pts',(7.31732883794868,3.53795736109197,48.5601729099721));
#176771=CARTESIAN_POINT('Ctrl Pts',(7.22706578225808,3.71888253593403,48.5681014422972));
#176772=CARTESIAN_POINT('Ctrl Pts',(7.13011092176217,3.89630668786067,48.5760299746223));
#176773=CARTESIAN_POINT('Ctrl Pts',(7.03322245478509,4.07360934186849,48.583953077584));
#176774=CARTESIAN_POINT('Ctrl Pts',(6.92965147418736,4.24741545864518,48.5918761805458));
#176775=CARTESIAN_POINT('Ctrl Pts',(6.81968041450227,4.41719895483033,48.5997992835076));
#176776=CARTESIAN_POINT('Ctrl Pts',(6.70976771037649,4.58689235630411,48.6077181821168));
#176777=CARTESIAN_POINT('Ctrl Pts',(6.59346187718006,4.75256711206116,48.6156370807261));
#176778=CARTESIAN_POINT('Ctrl Pts',(6.47109036267713,4.91372334188313,48.6235559793353));
#176779=CARTESIAN_POINT('Ctrl Pts',(6.3487604732,5.07482475394583,48.6314721843082));
#176780=CARTESIAN_POINT('Ctrl Pts',(6.22036921596723,5.23141043754099,48.6393883892811));
#176781=CARTESIAN_POINT('Ctrl Pts',(6.08628654583634,5.38301064874216,48.647304594254));
#176782=CARTESIAN_POINT('Ctrl Pts',(5.95223227009314,5.53457875590508,48.6552191228299));
#176783=CARTESIAN_POINT('Ctrl Pts',(5.81248920625189,5.68116324623945,48.6631336514057));
#176784=CARTESIAN_POINT('Ctrl Pts',(5.66746688746875,5.82232828359457,48.6710481799816));
#176785=CARTESIAN_POINT('Ctrl Pts',(5.52242962534958,5.96350786682515,48.6789635240833));
#176786=CARTESIAN_POINT('Ctrl Pts',(5.37211225842041,6.09926664600249,48.6868788681851));
#176787=CARTESIAN_POINT('Ctrl Pts',(5.2169608776247,6.22920594970445,48.6947942122868));
#176788=CARTESIAN_POINT('Ctrl Pts',(5.11165180460258,6.3174023134868,48.7001667558358));
#176789=CARTESIAN_POINT('Ctrl Pts',(5.00411644590343,6.40291840952884,48.7055392993848));
#176790=CARTESIAN_POINT('Ctrl Pts',(4.89450297224217,6.48564015477367,48.7109118429337));
#176791=CARTESIAN_POINT('Ctrl Pts',(4.72941840659802,6.6102241399986,48.71900322065));
#176792=CARTESIAN_POINT('Ctrl Pts',(4.55956536848283,6.72850849743512,48.7270945983663));
#176793=CARTESIAN_POINT('Ctrl Pts',(4.38545483821631,6.84013694486193,48.7351859760825));
#176794=CARTESIAN_POINT('Ctrl Pts',(4.21133698669297,6.95177008620663,48.743277694037));
#176795=CARTESIAN_POINT('Ctrl Pts',(4.0329615488586,7.05674659121316,48.7513694119915));
#176796=CARTESIAN_POINT('Ctrl Pts',(3.85086745973168,7.15475417957037,48.7594611299459));
#176797=CARTESIAN_POINT('Ctrl Pts',(3.66874498380537,7.25277704641225,48.7675541093251));
#176798=CARTESIAN_POINT('Ctrl Pts',(3.48290297530535,7.34382868226941,48.7756470887042));
#176799=CARTESIAN_POINT('Ctrl Pts',(3.29390445147555,7.42764303309264,48.7837400680833));
#176800=CARTESIAN_POINT('Ctrl Pts',(3.10479503248428,7.51150656210931,48.79183779603));
#176801=CARTESIAN_POINT('Ctrl Pts',(2.91252568231339,7.5881241929646,48.7999355239767));
#176802=CARTESIAN_POINT('Ctrl Pts',(2.71768000648576,7.65727777639335,48.8080332519233));
#176803=CARTESIAN_POINT('Ctrl Pts',(2.52277499100083,7.72645242033538,48.8161334460084));
#176804=CARTESIAN_POINT('Ctrl Pts',(2.32529238051981,7.78815838282438,48.8242336400934));
#176805=CARTESIAN_POINT('Ctrl Pts',(2.12583148881044,7.84222723744231,48.8323338341784));
#176806=CARTESIAN_POINT('Ctrl Pts',(1.92621631634278,7.89633791371168,48.8404402936726));
#176807=CARTESIAN_POINT('Ctrl Pts',(1.72462010761914,7.94279960123247,48.8485467531668));
#176808=CARTESIAN_POINT('Ctrl Pts',(1.52165420994225,7.98149459862406,48.8566532126609));
#176809=CARTESIAN_POINT('Ctrl Pts',(1.41377494853402,8.00206154009835,48.8609619111806));
#176810=CARTESIAN_POINT('Ctrl Pts',(1.30550889176043,8.02043520376885,48.8652706097003));
#176811=CARTESIAN_POINT('Ctrl Pts',(1.19694860265409,8.03660386015787,48.86957930822));
#176812=CARTESIAN_POINT('Ctrl Pts',(0.978053846880687,8.06920541382536,
48.8782671213967));
#176813=CARTESIAN_POINT('Ctrl Pts',(0.757838365444617,8.0928577768821,48.8869549345734));
#176814=CARTESIAN_POINT('Ctrl Pts',(0.537011557224253,8.1074845759895,48.8956427477501));
#176815=CARTESIAN_POINT('Ctrl Pts',(0.316234220785276,8.12210809825829,
48.904328614598));
#176816=CARTESIAN_POINT('Ctrl Pts',(0.0948460474159337,8.12771008307366,
48.9130144814458));
#176817=CARTESIAN_POINT('Ctrl Pts',(-0.126440066090956,8.12426614976312,
48.9217003482936));
#176818=CARTESIAN_POINT('Ctrl Pts',(-0.352643206937182,8.12074569147786,
48.9305792170614));
#176819=CARTESIAN_POINT('Ctrl Pts',(-0.578739470335517,8.10777262911778,
48.9394580858291));
#176820=CARTESIAN_POINT('Ctrl Pts',(-0.803966609970434,8.08537724862314,
48.9483369545969));
#176821=CARTESIAN_POINT('Ctrl Pts',(-1.02394625691664,8.06350365069696,
48.9570089575357));
#176822=CARTESIAN_POINT('Ctrl Pts',(-1.2430965929378,8.0326418826472,48.9656809604745));
#176823=CARTESIAN_POINT('Ctrl Pts',(-1.46071001826149,7.99287268790455,
48.9743529634133));
#176824=CARTESIAN_POINT('Ctrl Pts',(-1.68611001525814,7.95168048497764,
48.9833352650955));
#176825=CARTESIAN_POINT('Ctrl Pts',(-1.90986086182544,7.90093167741484,
48.9923175667777));
#176826=CARTESIAN_POINT('Ctrl Pts',(-2.13118291449833,7.84077463950153,
49.00129986846));
#176827=CARTESIAN_POINT('Ctrl Pts',(-2.35250496717114,7.78061760158825,
49.0102821701422));
#176828=CARTESIAN_POINT('Ctrl Pts',(-2.57139796323687,7.71105235475339,
49.0192644718244));
#176829=CARTESIAN_POINT('Ctrl Pts',(-2.7870929229118,7.63228672165525,49.0282467735066));
#176830=CARTESIAN_POINT('Ctrl Pts',(-2.97744349581197,7.56277613407511,
49.0361736452043));
#176831=CARTESIAN_POINT('Ctrl Pts',(-3.16523267751558,7.48612560747436,
49.0441005169019));
#176832=CARTESIAN_POINT('Ctrl Pts',(-3.34990292770109,7.4025561759084,49.0520273885996));
#176833=CARTESIAN_POINT('Ctrl Pts',(-3.53456242783743,7.31899160909731,
49.0599537988571));
#176834=CARTESIAN_POINT('Ctrl Pts',(-3.716103055548,7.22850907745022,49.0678802091146));
#176835=CARTESIAN_POINT('Ctrl Pts',(-3.89398852514512,7.13137721120809,
49.0758066193722));
#176836=CARTESIAN_POINT('Ctrl Pts',(-4.07189066434111,7.03423624276525,
49.0837337724114));
#176837=CARTESIAN_POINT('Ctrl Pts',(-4.24613667118519,6.93044485765078,
49.0916609254507));
#176838=CARTESIAN_POINT('Ctrl Pts',(-4.41621572419633,6.82031716563541,
49.09958807849));
#176839=CARTESIAN_POINT('Ctrl Pts',(-4.58639777019186,6.71012278475117,
49.107520031892));
#176840=CARTESIAN_POINT('Ctrl Pts',(-4.75240754060323,6.59358461043873,
49.115451985294));
#176841=CARTESIAN_POINT('Ctrl Pts',(-4.91376315920374,6.47106012781152,
49.1233839386961));
#176842=CARTESIAN_POINT('Ctrl Pts',(-5.07517035288604,6.34849648193565,
49.1313184274368));
#176843=CARTESIAN_POINT('Ctrl Pts',(-5.23192016811001,6.219942919279,49.1392529161775));
#176844=CARTESIAN_POINT('Ctrl Pts',(-5.38356408656067,6.08579701340705,
49.1471874049182));
#176845=CARTESIAN_POINT('Ctrl Pts',(-5.53534800335026,5.95152726343908,
49.1551292188142));
#176846=CARTESIAN_POINT('Ctrl Pts',(-5.68201636049718,5.81165508017606,
49.1630710327102));
#176847=CARTESIAN_POINT('Ctrl Pts',(-5.82315689846523,5.66661550648681,
49.1710128466061));
#176848=CARTESIAN_POINT('Ctrl Pts',(-5.91735582569032,5.56981431496942,
49.1763133106684));
#176849=CARTESIAN_POINT('Ctrl Pts',(-6.00909322572258,5.47071211191697,
49.1816137747306));
#176850=CARTESIAN_POINT('Ctrl Pts',(-6.09825655253652,5.3694463943637,49.1869142387928));
#176851=CARTESIAN_POINT('Ctrl Pts',(-6.23208145070166,5.2174570639581,49.1948696851484));
#176852=CARTESIAN_POINT('Ctrl Pts',(-6.36033685696158,5.06033019130039,
49.202825131504));
#176853=CARTESIAN_POINT('Ctrl Pts',(-6.48261644312577,4.8985070801026,49.2107805778595));
#176854=CARTESIAN_POINT('Ctrl Pts',(-6.60480242608076,4.7368078420958,49.218729934439));
#176855=CARTESIAN_POINT('Ctrl Pts',(-6.72102150762917,4.57041979332046,
49.2266792910184));
#176856=CARTESIAN_POINT('Ctrl Pts',(-6.83090671507786,4.39981829311214,
49.2346286475978));
#176857=CARTESIAN_POINT('Ctrl Pts',(-6.94072590306755,4.22931929094708,
49.242573228173));
#176858=CARTESIAN_POINT('Ctrl Pts',(-7.04421862370558,4.05461216063073,
49.2505178087481));
#176859=CARTESIAN_POINT('Ctrl Pts',(-7.14106017126255,3.87620267696462,
49.2584623893232));
#176860=CARTESIAN_POINT('Ctrl Pts',(-7.23785947669766,3.69787101521831,
49.2664035044856));
#176861=CARTESIAN_POINT('Ctrl Pts',(-7.32801323521957,3.51584050984272,
49.2743446196479));
#176862=CARTESIAN_POINT('Ctrl Pts',(-7.41124157611675,3.33064346079531,
49.2822857348102));
#176863=CARTESIAN_POINT('Ctrl Pts',(-7.49444730802118,3.14549672055728,
49.2902246927673));
#176864=CARTESIAN_POINT('Ctrl Pts',(-7.57073123781064,2.95718545319507,
49.2981636507244));
#176865=CARTESIAN_POINT('Ctrl Pts',(-7.63986053311785,2.76626437583399,
49.3061026086814));
#176866=CARTESIAN_POINT('Ctrl Pts',(-7.71175143377586,2.56771630522097,
49.3143587153766));
#176867=CARTESIAN_POINT('Ctrl Pts',(-7.77590415649592,2.36634596511415,
49.3226148220718));
#176868=CARTESIAN_POINT('Ctrl Pts',(-7.83211284222034,2.16279818504346,
49.330870928767));
#176869=CARTESIAN_POINT('Ctrl Pts',(-7.88617341184988,1.96702934975347,
49.3388115134847));
#176870=CARTESIAN_POINT('Ctrl Pts',(-7.93288578425423,1.76924675451631,
49.3467520982024));
#176871=CARTESIAN_POINT('Ctrl Pts',(-7.97211821269964,1.5700378228701,49.35469268292));
#176872=CARTESIAN_POINT('Ctrl Pts',(-8.01136013437536,1.37078068782833,
49.3626351890533));
#176873=CARTESIAN_POINT('Ctrl Pts',(-8.04311843908364,1.17009685298631,
49.3705776951866));
#176874=CARTESIAN_POINT('Ctrl Pts',(-8.06731275359214,0.968582726580205,
49.3785202013198));
#176875=CARTESIAN_POINT('Ctrl Pts',(-8.09151653536827,0.766989747426939,
49.3864658153664));
#176876=CARTESIAN_POINT('Ctrl Pts',(-8.10815038611567,0.564566157414711,
49.3944114294129));
#176877=CARTESIAN_POINT('Ctrl Pts',(-8.11718588958296,0.36191269175768,
49.4023570434594));
#176878=CARTESIAN_POINT('Ctrl Pts',(-8.12622627820231,0.159149659102155,
49.4103069533964));
#176879=CARTESIAN_POINT('Ctrl Pts',(-8.1276601137808,-0.0438431668199141,
49.4182568633334));
#176880=CARTESIAN_POINT('Ctrl Pts',(-8.12151108857014,-0.246465414880581,
49.4262067732703));
#176881=CARTESIAN_POINT('Ctrl Pts',(-8.11535469856938,-0.449330346988657,
49.4341662049471));
#176882=CARTESIAN_POINT('Ctrl Pts',(-8.1015973137944,-0.651823483752154,
49.4421256366238));
#176883=CARTESIAN_POINT('Ctrl Pts',(-8.08031458130745,-0.853348597942344,
49.4500850683006));
#176884=CARTESIAN_POINT('Ctrl Pts',(-8.05901692913426,-1.05501498588464,
49.4580500797224));
#176885=CARTESIAN_POINT('Ctrl Pts',(-8.0301834536962,-1.25571167114033,
49.4660150911443));
#176886=CARTESIAN_POINT('Ctrl Pts',(-7.99394096336068,-1.45485237629254,
49.4739801025662));
#176887=CARTESIAN_POINT('Ctrl Pts',(-7.95765074415915,-1.6542553360511,
49.4819556033601));
#176888=CARTESIAN_POINT('Ctrl Pts',(-7.9139320897016,-1.85209790024651,
49.489931104154));
#176889=CARTESIAN_POINT('Ctrl Pts',(-7.86296203991051,-2.04780749130046,
49.4979066049478));
#176890=CARTESIAN_POINT('Ctrl Pts',(-7.84945062821162,-2.09968722987224,
49.5000207930872));
#176891=CARTESIAN_POINT('Ctrl Pts',(-7.83542992459351,-2.15141718538454,
49.5021349812266));
#176892=CARTESIAN_POINT('Ctrl Pts',(-7.82090379551784,-2.20298692319193,
49.5042491693659));
#176893=CARTESIAN_POINT('Ctrl Pts',(-7.76804293468209,-2.39065018292006,
49.5119427403395));
#176894=CARTESIAN_POINT('Ctrl Pts',(-7.70832839993634,-2.5767471830493,
49.5196363113131));
#176895=CARTESIAN_POINT('Ctrl Pts',(-7.64186410911351,-2.76072463319737,
49.5273298822867));
#176896=CARTESIAN_POINT('Ctrl Pts',(-7.57548016190044,-2.94447968704398,
49.5350141530894));
#176897=CARTESIAN_POINT('Ctrl Pts',(-7.50236281859812,-3.12611995856152,
49.5426984238921));
#176898=CARTESIAN_POINT('Ctrl Pts',(-7.42266685376287,-3.30510277306924,
49.5503826946948));
#176899=CARTESIAN_POINT('Ctrl Pts',(-7.34305114840654,-3.48390533921112,
49.5580592268927));
#176900=CARTESIAN_POINT('Ctrl Pts',(-7.25687015394062,-3.66005545187811,
49.5657357590907));
#176901=CARTESIAN_POINT('Ctrl Pts',(-7.16432829059914,-3.83302592047339,
49.5734122912886));
#176902=CARTESIAN_POINT('Ctrl Pts',(-7.07186098524913,-4.00585703234666,
49.5810826387524));
#176903=CARTESIAN_POINT('Ctrl Pts',(-6.97304318171762,-4.17551328660332,
49.5887529862162));
#176904=CARTESIAN_POINT('Ctrl Pts',(-6.86812726052436,-4.34148770535426,
49.5964233336801));
#176905=CARTESIAN_POINT('Ctrl Pts',(-6.76327476256909,-4.50736179009542,
49.6040890443045));
#176906=CARTESIAN_POINT('Ctrl Pts',(-6.65233167795167,-4.669558169658,49.611754754929));
#176907=CARTESIAN_POINT('Ctrl Pts',(-6.53559620385363,-4.82759462078932,
49.6194204655534));
#176908=CARTESIAN_POINT('Ctrl Pts',(-6.41890783646469,-4.98556729887146,
49.6270830828045));
#176909=CARTESIAN_POINT('Ctrl Pts',(-6.29643194718965,-5.13938310428014,
49.6347457000557));
#176910=CARTESIAN_POINT('Ctrl Pts',(-6.16850996881306,-5.28858887862858,
49.6424083173068));
#176911=CARTESIAN_POINT('Ctrl Pts',(-6.04058987852066,-5.43779245075135,
49.6500708214604));
#176912=CARTESIAN_POINT('Ctrl Pts',(-5.90722408351136,-5.58238584811721,
49.6577333256139));
#176913=CARTESIAN_POINT('Ctrl Pts',(-5.76879447776803,-5.7219487795482,
49.6653958297675));
#176914=CARTESIAN_POINT('Ctrl Pts',(-5.63035960384037,-5.86151702229424,
49.6730586255312));
#176915=CARTESIAN_POINT('Ctrl Pts',(-5.48686078699429,-5.99605416267736,
49.680721421295));
#176916=CARTESIAN_POINT('Ctrl Pts',(-5.33871686536881,-6.12517671532231,
49.6883842170587));
#176917=CARTESIAN_POINT('Ctrl Pts',(-5.19054034300347,-6.25432768284047,
49.6960486991071));
#176918=CARTESIAN_POINT('Ctrl Pts',(-5.03771695023212,-6.37806145431482,
49.7037131811554));
#176919=CARTESIAN_POINT('Ctrl Pts',(-4.88069872336345,-6.49603475469908,
49.7113776632037));
#176920=CARTESIAN_POINT('Ctrl Pts',(-4.72361735401347,-6.61405549624393,
49.7190452274064));
#176921=CARTESIAN_POINT('Ctrl Pts',(-4.56233807763212,-6.72631093904359,
49.7267127916091));
#176922=CARTESIAN_POINT('Ctrl Pts',(-4.3973420624435,-6.83250103171343,
49.7343803558118));
#176923=CARTESIAN_POINT('Ctrl Pts',(-4.23215008656796,-6.93881724308669,
49.7420570265445));
#176924=CARTESIAN_POINT('Ctrl Pts',(-4.06323285690005,-7.03905352323911,
49.7497336972771));
#176925=CARTESIAN_POINT('Ctrl Pts',(-3.89109725091988,-7.13295519026888,
49.7574103680097));
#176926=CARTESIAN_POINT('Ctrl Pts',(-3.71885251649102,-7.22691638794133,
49.7650919055052));
#176927=CARTESIAN_POINT('Ctrl Pts',(-3.54338566076395,-7.31453481388569,
49.7727734430006));
#176928=CARTESIAN_POINT('Ctrl Pts',(-3.36522360387869,-7.39560394142342,
49.780454980496));
#176929=CARTESIAN_POINT('Ctrl Pts',(-3.18678481962152,-7.47679898828989,
49.788148449217));
#176930=CARTESIAN_POINT('Ctrl Pts',(-3.00564280229518,-7.55142428215892,
49.795841917938));
#176931=CARTESIAN_POINT('Ctrl Pts',(-2.82234092344189,-7.61932275693616,
49.803535386659));
#176932=CARTESIAN_POINT('Ctrl Pts',(-2.67900015934634,-7.6724188807532,
49.8095516244189));
#176933=CARTESIAN_POINT('Ctrl Pts',(-2.53433894520927,-7.72140246568362,
49.8155678621787));
#176934=CARTESIAN_POINT('Ctrl Pts',(-2.38862097292405,-7.76622027824394,
49.8215840999386));
#176935=CARTESIAN_POINT('Ctrl Pts',(-2.1962582923516,-7.82538439112784,
49.8295261513157));
#176936=CARTESIAN_POINT('Ctrl Pts',(-2.00145107000579,-7.87747278895808,
49.8374682026927));
#176937=CARTESIAN_POINT('Ctrl Pts',(-1.80475697291493,-7.92228122646596,
49.8454102540698));
#176938=CARTESIAN_POINT('Ctrl Pts',(-1.60828922623835,-7.96703809959776,
49.8533431659422));
#176939=CARTESIAN_POINT('Ctrl Pts',(-1.40993925436718,-8.00453163140133,
49.8612760778146));
#176940=CARTESIAN_POINT('Ctrl Pts',(-1.21028139561434,-8.03460680468745,
49.8692089896869));
#176941=CARTESIAN_POINT('Ctrl Pts',(-1.01081919040248,-8.0646525059849,
49.8771341277491));
#176942=CARTESIAN_POINT('Ctrl Pts',(-0.810051980740767,-8.08729428572821,
49.8850592658113));
#176943=CARTESIAN_POINT('Ctrl Pts',(-0.608566267360869,-8.10242770166636,
49.8929844038735));
#176944=CARTESIAN_POINT('Ctrl Pts',(-0.407243597863957,-8.11754887152088,
49.9009031288493));
#176945=CARTESIAN_POINT('Ctrl Pts',(-0.205203915256688,-8.12517376165031,
49.9088218538251));
#176946=CARTESIAN_POINT('Ctrl Pts',(-0.00304126880216057,-8.12524943082882,
49.916740578801));
#176947=CARTESIAN_POINT('Ctrl Pts',(0.198992286934878,-8.12532505168887,
49.9246542472844));
#176948=CARTESIAN_POINT('Ctrl Pts',(0.401148316694656,-8.11786105996389,
49.9325679157677));
#176949=CARTESIAN_POINT('Ctrl Pts',(0.602829902214262,-8.10285651307589,
49.9404815842511));
#176950=CARTESIAN_POINT('Ctrl Pts',(0.813547487829065,-8.0871797130084,
49.9487498111787));
#176951=CARTESIAN_POINT('Ctrl Pts',(1.0237467640609,-8.06327110342906,49.9570180381062));
#176952=CARTESIAN_POINT('Ctrl Pts',(1.23274817861052,-8.03119041553819,
49.9652862650337));
#176953=CARTESIAN_POINT('Ctrl Pts',(1.43264913325689,-8.00050660342659,
49.9731944720648));
#176954=CARTESIAN_POINT('Ctrl Pts',(1.63145396338488,-7.96234732507618,
49.9811026790958));
#176955=CARTESIAN_POINT('Ctrl Pts',(1.82857437159921,-7.91681775273566,
49.9890108861269));
#176956=CARTESIAN_POINT('Ctrl Pts',(2.02567888788894,-7.87129185100712,
49.9969184555952));
#176957=CARTESIAN_POINT('Ctrl Pts',(2.22109892714147,-7.81839691460787,
50.0048260250635));
#176958=CARTESIAN_POINT('Ctrl Pts',(2.4142575022211,-7.75828900437907,50.0127335945318));
#176959=CARTESIAN_POINT('Ctrl Pts',(2.60743037754448,-7.69817664413935,
50.0206417494268));
#176960=CARTESIAN_POINT('Ctrl Pts',(2.79834113580858,-7.63085034532393,
50.0285499043217));
#176961=CARTESIAN_POINT('Ctrl Pts',(2.98642867148884,-7.55651582097261,
50.0364580592166));
#176962=CARTESIAN_POINT('Ctrl Pts',(3.1745592206354,-7.48216429716651,50.0443680226161));
#176963=CARTESIAN_POINT('Ctrl Pts',(3.35986494964294,-7.40080147664705,
50.0522779860155));
#176964=CARTESIAN_POINT('Ctrl Pts',(3.54180507075917,-7.31268106806557,
50.0601879494149));
#176965=CARTESIAN_POINT('Ctrl Pts',(3.72388341191931,-7.22449371434484,
50.0681039220193));
#176966=CARTESIAN_POINT('Ctrl Pts',(3.90259073642823,-7.12953866306084,
50.0760198946238));
#176967=CARTESIAN_POINT('Ctrl Pts',(4.07741025868074,-7.02811590292199,
50.0839358672282));
#176968=CARTESIAN_POINT('Ctrl Pts',(4.25230714285979,-6.92664826072411,
50.0918553428447));
#176969=CARTESIAN_POINT('Ctrl Pts',(4.42331250995822,-6.81870737797382,
50.0997748184612));
#176970=CARTESIAN_POINT('Ctrl Pts',(4.58993838759777,-6.70463669116801,
50.1076942940777));
#176971=CARTESIAN_POINT('Ctrl Pts',(4.75672701053396,-6.5904545902888,50.1156215047316));
#176972=CARTESIAN_POINT('Ctrl Pts',(4.91912733013389,-6.47013092322236,
50.1235487153856));
#176973=CARTESIAN_POINT('Ctrl Pts',(5.07668346350215,-6.34405017113703,
50.1314759260395));
#176974=CARTESIAN_POINT('Ctrl Pts',(5.12599491373206,-6.30458979216928,
50.1339569608635));
#176975=CARTESIAN_POINT('Ctrl Pts',(5.17483211521669,-6.26456576137527,
50.1364379956876));
#176976=CARTESIAN_POINT('Ctrl Pts',(5.22318182438274,-6.22399061631183,
50.1389190305116));
#176977=CARTESIAN_POINT('Ctrl Pts',(5.381146124221,-6.09142675002737,50.1470248689046));
#176978=CARTESIAN_POINT('Ctrl Pts',(5.53418169031714,-5.95274456759449,
50.1551307072977));
#176979=CARTESIAN_POINT('Ctrl Pts',(5.68180697082179,-5.80833514088339,
50.1632365456907));
#176980=CARTESIAN_POINT('Ctrl Pts',(5.82930838711782,-5.66404688013585,
50.171335582923));
#176981=CARTESIAN_POINT('Ctrl Pts',(5.97140834685528,-5.51404117448959,
50.1794346201553));
#176982=CARTESIAN_POINT('Ctrl Pts',(6.10765932867919,-5.35874846277543,
50.1875336573877));
#176983=CARTESIAN_POINT('Ctrl Pts',(6.24381173869352,-5.20356809875523,
50.1956268353099));
#176984=CARTESIAN_POINT('Ctrl Pts',(6.37412340357326,-5.04310859039263,
50.2037200132321));
#176985=CARTESIAN_POINT('Ctrl Pts',(6.49818410722792,-4.87783669991836,
50.2118131911543));
#176986=CARTESIAN_POINT('Ctrl Pts',(6.62215384031421,-4.71268599913084,
50.2199004345543));
#176987=CARTESIAN_POINT('Ctrl Pts',(6.73988157087455,-4.54273020667023,
50.2279876779544));
#176988=CARTESIAN_POINT('Ctrl Pts',(6.85099752114733,-4.36846889970996,
50.2360749213544));
#176989=CARTESIAN_POINT('Ctrl Pts',(6.96206384269067,-4.19428542466521,
50.2441585526753));
#176990=CARTESIAN_POINT('Ctrl Pts',(7.06652410506711,-4.01580053289428,
50.2522421839961));
#176991=CARTESIAN_POINT('Ctrl Pts',(7.16405146167329,-3.83354329791602,
50.260325815317));
#176992=CARTESIAN_POINT('Ctrl Pts',(7.26154376603157,-3.65135156789968,
50.2684065413048));
#176993=CARTESIAN_POINT('Ctrl Pts',(7.35210798796967,-3.465390474538,50.2764872672926));
#176994=CARTESIAN_POINT('Ctrl Pts',(7.43546262163905,-3.27621476168894,
50.2845679932804));
#176995=CARTESIAN_POINT('Ctrl Pts',(7.48022561735247,-3.17462386925059,
50.2889074941195));
#176996=CARTESIAN_POINT('Ctrl Pts',(7.52291023104088,-3.07210634064467,
50.2932469949587));
#176997=CARTESIAN_POINT('Ctrl Pts',(7.56347845227602,-2.96875079190833,
50.2975864957978));
#176998=CARTESIAN_POINT('Ctrl Pts',(7.63905678384256,-2.77620007871927,
50.305670957558));
#176999=CARTESIAN_POINT('Ctrl Pts',(7.70726142573685,-2.58080430198568,
50.3137554193181));
#177000=CARTESIAN_POINT('Ctrl Pts',(7.76789915218257,-2.38315553920035,
50.3218398810783));
#177001=CARTESIAN_POINT('Ctrl Pts',(7.82858569751626,-2.18534765117446,
50.3299308515659));
#177002=CARTESIAN_POINT('Ctrl Pts',(7.88169305932133,-1.98528345031682,
50.3380218220535));
#177003=CARTESIAN_POINT('Ctrl Pts',(7.9270780998098,-1.78356955625953,50.3461127925411));
#177004=CARTESIAN_POINT('Ctrl Pts',(7.97248100561706,-1.58177625976075,
50.3542069479497));
#177005=CARTESIAN_POINT('Ctrl Pts',(8.01015546311294,-1.37833228028703,
50.3623011033582));
#177006=CARTESIAN_POINT('Ctrl Pts',(8.04000967540918,-1.17385347545031,
50.3703952587668));
#177007=CARTESIAN_POINT('Ctrl Pts',(8.06989506292854,-0.969161143882411,
50.3784978664868));
#177008=CARTESIAN_POINT('Ctrl Pts',(8.09194384218465,-0.763432136862623,
50.3866004742068));
#177009=CARTESIAN_POINT('Ctrl Pts',(8.10611605649862,-0.557288113165248,
50.3947030819268));
#177010=CARTESIAN_POINT('Ctrl Pts',(8.11887801713983,-0.37165714128154,
50.4019994125159));
#177011=CARTESIAN_POINT('Ctrl Pts',(8.12525366522605,-0.185689847070898,
50.409295743105));
#177012=CARTESIAN_POINT('Ctrl Pts',(8.12524999841854,0.000160310478422246,
50.416592073694));
#177013=CARTESIAN_POINT('',(8.12525,4.14113188185183E-13,46.4167025567876));
#177014=CARTESIAN_POINT('Ctrl Pts',(8.12525,4.14112967973255E-13,46.4167025567876));
#177015=CARTESIAN_POINT('Ctrl Pts',(8.12524999999989,2.24624642433447,46.5047001499288));
#177016=CARTESIAN_POINT('Ctrl Pts',(7.14398562317582,4.47535249753478,46.59269774307));
#177017=CARTESIAN_POINT('Ctrl Pts',(3.83078204044914,7.50935546634369,46.7686929293524));
#177018=CARTESIAN_POINT('Ctrl Pts',(1.52412477697731,8.29110090552138,46.8566905224936));
#177019=CARTESIAN_POINT('Ctrl Pts',(-2.9510162393256,7.89663306204424,47.032685708776));
#177020=CARTESIAN_POINT('Ctrl Pts',(-5.08535169588728,6.7234298308579,47.1206833019172));
#177021=CARTESIAN_POINT('Ctrl Pts',(-7.81671694684396,3.15661951052958,
47.2966784881996));
#177022=CARTESIAN_POINT('Ctrl Pts',(-8.39290461146698,0.790229551554374,
47.3846760813408));
#177023=CARTESIAN_POINT('Ctrl Pts',(-7.60701611462498,-3.63299000730381,
47.5606712676232));
#177024=CARTESIAN_POINT('Ctrl Pts',(-6.25093680401385,-5.65606750609986,
47.6486688607644));
#177025=CARTESIAN_POINT('Ctrl Pts',(-2.45807268688606,-8.06369575488301,
47.8246640470468));
#177026=CARTESIAN_POINT('Ctrl Pts',(-0.0502299510459392,-8.42987470330084,
47.912661640188));
#177027=CARTESIAN_POINT('Ctrl Pts',(4.28689960880937,-7.25863639434595,
48.0886568264704));
#177028=CARTESIAN_POINT('Ctrl Pts',(6.1830912555711,-5.73015646266433,48.1766544196116));
#177029=CARTESIAN_POINT('Ctrl Pts',(7.81050559202892,-2.58640713800313,
48.3153355274311));
#177030=CARTESIAN_POINT('Ctrl Pts',(8.12525000000004,-1.29375883538159,
48.3660190421093));
#177031=CARTESIAN_POINT('Ctrl Pts',(8.12525,2.38922734780257E-13,48.4167025567876));
#177032=CARTESIAN_POINT('',(8.12525,5.33559741527911E-13,42.4167025567876));
#177033=CARTESIAN_POINT('Ctrl Pts',(8.12524980845225,-0.00176429777071613,
46.4169402126099));
#177034=CARTESIAN_POINT('Ctrl Pts',(8.12524336551536,-0.0314364271678197,
46.4157867211515));
#177035=CARTESIAN_POINT('Ctrl Pts',(8.12507438574217,-0.0611082895719105,
46.4146319165874));
#177036=CARTESIAN_POINT('Ctrl Pts',(8.12437406859321,-0.123787156037501,
46.4121895060278));
#177037=CARTESIAN_POINT('Ctrl Pts',(8.1238041070432,-0.156793138196381,
46.4109016018563));
#177038=CARTESIAN_POINT('Ctrl Pts',(8.1222235994471,-0.224437375940562,
46.4082582697045));
#177039=CARTESIAN_POINT('Ctrl Pts',(8.12119256875095,-0.259074480346016,
46.406902695888));
#177040=CARTESIAN_POINT('Ctrl Pts',(8.11826360209412,-0.340050718864486,
46.4037285183971));
#177041=CARTESIAN_POINT('Ctrl Pts',(8.11619043274539,-0.386382246215232,
46.4019084990561));
#177042=CARTESIAN_POINT('Ctrl Pts',(8.10816968998069,-0.536784525350514,
46.3959872082714));
#177043=CARTESIAN_POINT('Ctrl Pts',(8.10061612005149,-0.640758594942385,
46.3918732211905));
#177044=CARTESIAN_POINT('Ctrl Pts',(8.08072228816024,-0.85694361806308,
46.3832762487718));
#177045=CARTESIAN_POINT('Ctrl Pts',(8.06803990408777,-0.969101100063071,
46.3787917803781));
#177046=CARTESIAN_POINT('Ctrl Pts',(8.03316353031277,-1.22892661807609,
46.3683533355293));
#177047=CARTESIAN_POINT('Ctrl Pts',(8.00922716218528,-1.37632012200615,
46.36239396653));
#177048=CARTESIAN_POINT('Ctrl Pts',(7.95287798781533,-1.67162239496777,
46.3504093054814));
#177049=CARTESIAN_POINT('Ctrl Pts',(7.92036464764697,-1.8194543570788,46.3443865170123));
#177050=CARTESIAN_POINT('Ctrl Pts',(7.87759736522188,-1.99092740557492,
46.3374041968547));
#177051=CARTESIAN_POINT('Ctrl Pts',(7.87133774666267,-2.01553324614104,
46.3364023665107));
#177052=CARTESIAN_POINT('Ctrl Pts',(7.86023131383483,-2.05835040207013,
46.3346595165833));
#177053=CARTESIAN_POINT('Ctrl Pts',(7.85543628679765,-2.0765749279254,46.3339178415516));
#177054=CARTESIAN_POINT('Ctrl Pts',(7.84594759615601,-2.11213551717461,
46.3324710580468));
#177055=CARTESIAN_POINT('Ctrl Pts',(7.84125976796006,-2.12947302831123,
46.3317658714593));
#177056=CARTESIAN_POINT('Ctrl Pts',(7.83182091250608,-2.16392798625774,
46.330364943579));
#177057=CARTESIAN_POINT('Ctrl Pts',(7.8270711730163,-2.18104561840115,46.3296692059075));
#177058=CARTESIAN_POINT('Ctrl Pts',(7.81311361609309,-2.23071458181794,
46.327651138887));
#177059=CARTESIAN_POINT('Ctrl Pts',(7.80375859356496,-2.26322419412593,
46.326331103278));
#177060=CARTESIAN_POINT('Ctrl Pts',(7.7571464083772,-2.42148039431153,46.3199074389535));
#177061=CARTESIAN_POINT('Ctrl Pts',(7.71705112061419,-2.54637201197463,
46.3148448902823));
#177062=CARTESIAN_POINT('Ctrl Pts',(7.65788772160375,-2.71640056833077,
46.3079325100559));
#177063=CARTESIAN_POINT('Ctrl Pts',(7.64140921612542,-2.76241590314978,
46.3060597455096));
#177064=CARTESIAN_POINT('Ctrl Pts',(7.50902671784351,-3.12183611318082,
46.2914073490015));
#177065=CARTESIAN_POINT('Ctrl Pts',(7.3743039082081,-3.4279713168692,46.2787735834716));
#177066=CARTESIAN_POINT('Ctrl Pts',(7.09796167809606,-3.96368421756942,
46.2558516907867));
#177067=CARTESIAN_POINT('Ctrl Pts',(6.96304550455104,-4.19617055669198,
46.2456047079432));
#177068=CARTESIAN_POINT('Ctrl Pts',(6.75747299275486,-4.51310954346834,
46.2310572037499));
#177069=CARTESIAN_POINT('Ctrl Pts',(6.6962436596425,-4.60346821379332,46.2268402812932));
#177070=CARTESIAN_POINT('Ctrl Pts',(6.59800694296685,-4.74233150138394,
46.2202427902082));
#177071=CARTESIAN_POINT('Ctrl Pts',(6.56224193997055,-4.79169952766249,
46.2178735694056));
#177072=CARTESIAN_POINT('Ctrl Pts',(6.50107200302626,-4.87416563644041,
46.2138746312995));
#177073=CARTESIAN_POINT('Ctrl Pts',(6.47596148784595,-4.90747905070353,
46.2122476227983));
#177074=CARTESIAN_POINT('Ctrl Pts',(6.42926783382067,-4.96844371676085,
46.2092484063285));
#177075=CARTESIAN_POINT('Ctrl Pts',(6.40776002280285,-4.99615145157797,
46.2078769008142));
#177076=CARTESIAN_POINT('Ctrl Pts',(6.36285554445283,-5.05323332654042,
46.2050337632221));
#177077=CARTESIAN_POINT('Ctrl Pts',(6.33943328737875,-5.08258628224926,
46.2035619339907));
#177078=CARTESIAN_POINT('Ctrl Pts',(6.2861213898629,-5.14845531641048,46.2002366431198));
#177079=CARTESIAN_POINT('Ctrl Pts',(6.25611544707481,-5.18487548223448,
46.1983822276097));
#177080=CARTESIAN_POINT('Ctrl Pts',(6.16331715168767,-5.29553235236255,
46.1926988024806));
#177081=CARTESIAN_POINT('Ctrl Pts',(6.09950832993655,-5.36890484046775,
46.1888617021973));
#177082=CARTESIAN_POINT('Ctrl Pts',(5.81876339123752,-5.68026144051294,
46.1722764913487));
#177083=CARTESIAN_POINT('Ctrl Pts',(5.58910503477557,-5.9063759593944,46.1594931154483));
#177084=CARTESIAN_POINT('Ctrl Pts',(5.05323131775854,-6.37466652749516,
46.1307515848629));
#177085=CARTESIAN_POINT('Ctrl Pts',(4.74177109018703,-6.60962220355473,
46.1146780262004));
#177086=CARTESIAN_POINT('Ctrl Pts',(4.22328341220484,-6.94518070483189,
46.0887254352519));
#177087=CARTESIAN_POINT('Ctrl Pts',(4.02677134496226,-7.06093255776235,
46.0790649838876));
#177088=CARTESIAN_POINT('Ctrl Pts',(3.58504144300756,-7.29668077770954,
46.0578742679747));
#177089=CARTESIAN_POINT('Ctrl Pts',(3.33810983977917,-7.41290098746993,
46.0463600053154));
#177090=CARTESIAN_POINT('Ctrl Pts',(2.96889379203362,-7.56447798537479,
46.0299487237922));
#177091=CARTESIAN_POINT('Ctrl Pts',(2.85088241532768,-7.6097390692465,46.0248204765168));
#177092=CARTESIAN_POINT('Ctrl Pts',(2.71176121135175,-7.65940560144486,
46.0189464140556));
#177093=CARTESIAN_POINT('Ctrl Pts',(2.69163353955806,-7.66650193594872,
46.0181007308151));
#177094=CARTESIAN_POINT('Ctrl Pts',(2.66232836974136,-7.67670431091013,
46.0168757190071));
#177095=CARTESIAN_POINT('Ctrl Pts',(2.6531729943345,-7.67987333805801,46.016493894785));
#177096=CARTESIAN_POINT('Ctrl Pts',(2.63713778230002,-7.68539164455165,
46.0158267272965));
#177097=CARTESIAN_POINT('Ctrl Pts',(2.63026042928107,-7.68774807649121,
46.0155410932482));
#177098=CARTESIAN_POINT('Ctrl Pts',(2.61693347656547,-7.69229439987594,
46.0149885866469));
#177099=CARTESIAN_POINT('Ctrl Pts',(2.6104842696778,-7.69448541705252,46.0147216675835));
#177100=CARTESIAN_POINT('Ctrl Pts',(2.59337811418094,-7.70027298377651,
46.0140148896106));
#177101=CARTESIAN_POINT('Ctrl Pts',(2.58271641696357,-7.70385552687754,
46.0135756220414));
#177102=CARTESIAN_POINT('Ctrl Pts',(2.54499834494907,-7.7164424516538,46.0120260971338));
#177103=CARTESIAN_POINT('Ctrl Pts',(2.51790183900885,-7.72532659781437,
46.0109210629608));
#177104=CARTESIAN_POINT('Ctrl Pts',(2.06627088260679,-7.87077448163264,
45.9926448166083));
#177105=CARTESIAN_POINT('Ctrl Pts',(1.6312345633962,-7.97230598977856,45.977250272847));
#177106=CARTESIAN_POINT('Ctrl Pts',(0.951560163103997,-8.07293937603262,
45.9541233936049));
#177107=CARTESIAN_POINT('Ctrl Pts',(0.711605282612934,-8.0976191636857,
45.9461308768391));
#177108=CARTESIAN_POINT('Ctrl Pts',(0.0869932142115497,-8.13388017662535,
45.9252111373475));
#177109=CARTESIAN_POINT('Ctrl Pts',(-0.298005582694259,-8.12888357574144,
45.9121859310117));
#177110=CARTESIAN_POINT('Ctrl Pts',(-0.806047737852952,-8.08614091774465,
45.8939740572312));
#177111=CARTESIAN_POINT('Ctrl Pts',(-0.93064487404062,-8.07274963355612,
45.8894277785557));
#177112=CARTESIAN_POINT('Ctrl Pts',(-1.21033957582965,-8.03612765574105,
45.8790098018641));
#177113=CARTESIAN_POINT('Ctrl Pts',(-1.36517191603069,-8.01127780957283,
45.8730940842373));
#177114=CARTESIAN_POINT('Ctrl Pts',(-1.54198906310983,-7.97762472193629,
45.866145295766));
#177115=CARTESIAN_POINT('Ctrl Pts',(-1.56477535075435,-7.97318660046487,
45.8652461221294));
#177116=CARTESIAN_POINT('Ctrl Pts',(-1.59922863863991,-7.966322697293,45.8638809043011));
#177117=CARTESIAN_POINT('Ctrl Pts',(-1.6109099166797,-7.96396878415137,
45.863417046909));
#177118=CARTESIAN_POINT('Ctrl Pts',(-1.63109493542001,-7.95985504166606,
45.8626137985644));
#177119=CARTESIAN_POINT('Ctrl Pts',(-1.63960112481182,-7.95810725761027,
45.8622747747221));
#177120=CARTESIAN_POINT('Ctrl Pts',(-1.65721164054363,-7.95445935561626,
45.8615717937013));
#177121=CARTESIAN_POINT('Ctrl Pts',(-1.66631553719116,-7.95255723598064,
45.861207775972));
#177122=CARTESIAN_POINT('Ctrl Pts',(-1.69105450889051,-7.94734406133373,
45.8602169383449));
#177123=CARTESIAN_POINT('Ctrl Pts',(-1.7066830758271,-7.94400250858541,
45.8595891903008));
#177124=CARTESIAN_POINT('Ctrl Pts',(-1.76535837372883,-7.93127596754589,
45.8572256012656));
#177125=CARTESIAN_POINT('Ctrl Pts',(-1.8083380212938,-7.92158710028727,
45.8554805117701));
#177126=CARTESIAN_POINT('Ctrl Pts',(-2.52960066047031,-7.75281767647352,
45.8259606724177));
#177127=CARTESIAN_POINT('Ctrl Pts',(-3.18463676915089,-7.50752101775611,
45.7953227894909));
#177128=CARTESIAN_POINT('Ctrl Pts',(-4.17441324213938,-6.98377828490047,
45.745028943772));
#177129=CARTESIAN_POINT('Ctrl Pts',(-4.53254600500595,-6.75684391358903,
45.7259416974196));
#177130=CARTESIAN_POINT('Ctrl Pts',(-4.96828512188053,-6.43043485913772,
45.7027486366266));
#177131=CARTESIAN_POINT('Ctrl Pts',(-5.06356531824567,-6.35567918774564,
45.6976813709935));
#177132=CARTESIAN_POINT('Ctrl Pts',(-5.2078560671055,-6.23716519663319,
45.6900550319017));
#177133=CARTESIAN_POINT('Ctrl Pts',(-5.25806279163667,-6.19489872400199,
45.6874118741333));
#177134=CARTESIAN_POINT('Ctrl Pts',(-5.31861179395697,-6.14265918378931,
45.6842314930712));
#177135=CARTESIAN_POINT('Ctrl Pts',(-5.32944625192273,-6.13326144188078,
45.6836626784716));
#177136=CARTESIAN_POINT('Ctrl Pts',(-5.3469881773048,-6.11796410471686,
45.6827420695414));
#177137=CARTESIAN_POINT('Ctrl Pts',(-5.35371086910122,-6.11208207452541,
45.6823893434816));
#177138=CARTESIAN_POINT('Ctrl Pts',(-5.36599298429608,-6.10130000671119,
45.681745054542));
#177139=CARTESIAN_POINT('Ctrl Pts',(-5.37155542465681,-6.09640343150863,
45.6814533114156));
#177140=CARTESIAN_POINT('Ctrl Pts',(-5.38371780423885,-6.08566740996543,
45.6808154987705));
#177141=CARTESIAN_POINT('Ctrl Pts',(-5.3903149628298,-6.07982481841757,
45.6804695919525));
#177142=CARTESIAN_POINT('Ctrl Pts',(-5.40840198695145,-6.06375396461244,
45.6795213627768));
#177143=CARTESIAN_POINT('Ctrl Pts',(-5.41987236313527,-6.053503759563,45.6789201534425));
#177144=CARTESIAN_POINT('Ctrl Pts',(-5.47654511129033,-6.00256942036892,
45.6759500318758));
#177145=CARTESIAN_POINT('Ctrl Pts',(-5.52131947526164,-5.9614106947656,
45.6736045147556));
#177146=CARTESIAN_POINT('Ctrl Pts',(-6.00117080475262,-5.51026446347943,
45.6484327917287));
#177147=CARTESIAN_POINT('Ctrl Pts',(-6.39022140888337,-5.05393303340372,
45.6275606749244));
#177148=CARTESIAN_POINT('Ctrl Pts',(-6.97133207312041,-4.19664947714925,
45.5901382393326));
#177149=CARTESIAN_POINT('Ctrl Pts',(-7.18726695421699,-3.8150367556271,
45.5740219014664));
#177150=CARTESIAN_POINT('Ctrl Pts',(-7.39631084374373,-3.36419061593246,
45.5550296700606));
#177151=CARTESIAN_POINT('Ctrl Pts',(-7.4206268995964,-3.31020980121936,
45.552757459196));
#177152=CARTESIAN_POINT('Ctrl Pts',(-7.45810354760932,-3.22452429177211,
45.5491531704004));
#177153=CARTESIAN_POINT('Ctrl Pts',(-7.4716569826887,-3.19299347819154,
45.547827379621));
#177154=CARTESIAN_POINT('Ctrl Pts',(-7.4943258370972,-3.13932175199636,
45.5455715045057));
#177155=CARTESIAN_POINT('Ctrl Pts',(-7.50354392024658,-3.11722463846776,
45.5446429947826));
#177156=CARTESIAN_POINT('Ctrl Pts',(-7.52155028395054,-3.07351802965036,
45.5428069768942));
#177157=CARTESIAN_POINT('Ctrl Pts',(-7.53034343937526,-3.05191078388361,
45.541899550129));
#177158=CARTESIAN_POINT('Ctrl Pts',(-7.53906851689393,-3.03020353517938,
45.5409881811403));
#177159=CARTESIAN_POINT('Ctrl Pts',(-7.53909363080346,-3.03014105166963,
45.5409855578006));
#177160=CARTESIAN_POINT('Ctrl Pts',(-7.53914408064139,-3.03001552775656,
45.5409802877447));
#177161=CARTESIAN_POINT('Ctrl Pts',(-7.53916941659177,-3.02995248725839,
45.5409776410244));
#177162=CARTESIAN_POINT('Ctrl Pts',(-7.53922031114152,-3.0298258476799,
45.5409723241366));
#177163=CARTESIAN_POINT('Ctrl Pts',(-7.53924586976819,-3.02976224849103,
45.5409696539645));
#177164=CARTESIAN_POINT('Ctrl Pts',(-7.53929721060149,-3.02963448909234,
45.5409642900706));
#177165=CARTESIAN_POINT('Ctrl Pts',(-7.53932299267492,-3.02957032917286,
45.5409615963611));
#177166=CARTESIAN_POINT('Ctrl Pts',(-7.53937478087994,-3.02944144699925,
45.5409561853373));
#177167=CARTESIAN_POINT('Ctrl Pts',(-7.53940078701182,-3.02937672470275,
45.5409534680213));
#177168=CARTESIAN_POINT('Ctrl Pts',(-7.53945302395908,-3.02924671609373,
45.5409480097142));
#177169=CARTESIAN_POINT('Ctrl Pts',(-7.53947925478269,-3.02918142971857,
45.5409452687204));
#177170=CARTESIAN_POINT('Ctrl Pts',(-7.53953193019778,-3.02905031999472,
45.5409397641933));
#177171=CARTESIAN_POINT('Ctrl Pts',(-7.5395583748154,-3.02898449654486,
45.5409370006561));
#177172=CARTESIAN_POINT('Ctrl Pts',(-7.53961153635078,-3.02885216683859,
45.5409314449186));
#177173=CARTESIAN_POINT('Ctrl Pts',(-7.53963821879948,-3.02878574634356,
45.5409286563194));
#177174=CARTESIAN_POINT('Ctrl Pts',(-7.53969180895005,-3.02865233953581,
45.5409230553705));
#177175=CARTESIAN_POINT('Ctrl Pts',(-7.53971871790345,-3.02858535006354,
45.5409202428882));
#177176=CARTESIAN_POINT('Ctrl Pts',(-7.53977276148186,-3.02845080412888,
45.5409145941242));
#177177=CARTESIAN_POINT('Ctrl Pts',(-7.53979989743318,-3.02838324432005,
45.540911757702));
#177178=CARTESIAN_POINT('Ctrl Pts',(-7.53985439568391,-3.02824755589569,
45.5409060609818));
#177179=CARTESIAN_POINT('Ctrl Pts',(-7.53988175919209,-3.02817942422567,
45.5409032005557));
#177180=CARTESIAN_POINT('Ctrl Pts',(-7.53993671313527,-3.02804259050424,
45.5408974557618));
#177181=CARTESIAN_POINT('Ctrl Pts',(-7.53996430472478,-3.02797388553272,
45.5408945712714));
#177182=CARTESIAN_POINT('Ctrl Pts',(-7.54001972393283,-3.02783588240704,
45.540888777392));
#177183=CARTESIAN_POINT('Ctrl Pts',(-7.54004755267668,-3.02776658139969,
45.5408858678827));
#177184=CARTESIAN_POINT('Ctrl Pts',(-7.54010885584952,-3.02761391404568,
45.5408794583566));
#177185=CARTESIAN_POINT('Ctrl Pts',(-7.54014235661827,-3.02753048085637,
45.5408759555342));
#177186=CARTESIAN_POINT('Ctrl Pts',(-7.54021050534136,-3.02736074928107,
45.540868829606));
#177187=CARTESIAN_POINT('Ctrl Pts',(-7.54024515321194,-3.02727445082401,
45.5408652064975));
#177188=CARTESIAN_POINT('Ctrl Pts',(-7.54031562566087,-3.02709891433387,
45.5408578368753));
#177189=CARTESIAN_POINT('Ctrl Pts',(-7.5403514501167,-3.02700967630925,
45.5408540903622));
#177190=CARTESIAN_POINT('Ctrl Pts',(-7.54042430538776,-3.02682818592322,
45.5408464707928));
#177191=CARTESIAN_POINT('Ctrl Pts',(-7.54046133604598,-3.02673593363831,
45.5408425977401));
#177192=CARTESIAN_POINT('Ctrl Pts',(-7.54053663329123,-3.02654834011407,
45.5408347219597));
#177193=CARTESIAN_POINT('Ctrl Pts',(-7.54057489978158,-3.02645299878228,
45.5408307192285));
#177194=CARTESIAN_POINT('Ctrl Pts',(-7.540652698301,-3.02625915238135,45.5408225809526));
#177195=CARTESIAN_POINT('Ctrl Pts',(-7.5406922302526,-3.02616064715243,
45.5408184454014));
#177196=CARTESIAN_POINT('Ctrl Pts',(-7.54077258936141,-3.02596039796529,
45.5408100383383));
#177197=CARTESIAN_POINT('Ctrl Pts',(-7.54081341638606,-3.02585865396432,
45.5408057668248));
#177198=CARTESIAN_POINT('Ctrl Pts',(-7.54089639528232,-3.02565185223482,
45.5407970846893));
#177199=CARTESIAN_POINT('Ctrl Pts',(-7.54093854695903,-3.02554679459784,
45.5407926740715));
#177200=CARTESIAN_POINT('Ctrl Pts',(-7.5491502900155,-3.0050788427179,45.5399333725441));
#177201=CARTESIAN_POINT('Ctrl Pts',(-7.55723736107177,-2.98468296767218,
45.5390773367234));
#177202=CARTESIAN_POINT('Ctrl Pts',(-7.57535143104456,-2.93845302631693,
45.5371374191445));
#177203=CARTESIAN_POINT('Ctrl Pts',(-7.58532906588683,-2.91259994601593,
45.5360528387105));
#177204=CARTESIAN_POINT('Ctrl Pts',(-7.61444622904872,-2.83598990586738,
45.5328393192778));
#177205=CARTESIAN_POINT('Ctrl Pts',(-7.63320985289154,-2.7850919906294,
45.53070484145));
#177206=CARTESIAN_POINT('Ctrl Pts',(-7.80497507508968,-2.30438600085963,
45.5105417701189));
#177207=CARTESIAN_POINT('Ctrl Pts',(-7.92202125832042,-1.86262356676084,
45.4919151453754));
#177208=CARTESIAN_POINT('Ctrl Pts',(-8.0440196866528,-1.17197978190414,
45.4624982583085));
#177209=CARTESIAN_POINT('Ctrl Pts',(-8.07571645024059,-0.928757313290472,
45.4520980391277));
#177210=CARTESIAN_POINT('Ctrl Pts',(-8.12970213534692,-0.290186252796987,
45.4249028951722));
#177211=CARTESIAN_POINT('Ctrl Pts',(-8.13418974339782,0.106027200574754,
45.4081196394064));
#177212=CARTESIAN_POINT('Ctrl Pts',(-8.10666456771426,0.551584987354708,
45.3901266501115));
#177213=CARTESIAN_POINT('Ctrl Pts',(-8.1030661332201,0.602142656589539,
45.3880983345551));
#177214=CARTESIAN_POINT('Ctrl Pts',(-8.09787649840437,0.66654153460252,
45.3855341621121));
#177215=CARTESIAN_POINT('Ctrl Pts',(-8.09672249047119,0.680416281329202,
45.3849828626505));
#177216=CARTESIAN_POINT('Ctrl Pts',(-8.0948154706107,0.702652501605304,
45.3841012392303));
#177217=CARTESIAN_POINT('Ctrl Pts',(-8.09408515436585,0.711015861822725,
45.383770081619));
#177218=CARTESIAN_POINT('Ctrl Pts',(-8.09267600877235,0.72686941246166,
45.3831431795118));
#177219=CARTESIAN_POINT('Ctrl Pts',(-8.09199973945508,0.734359818384843,
45.3828473391157));
#177220=CARTESIAN_POINT('Ctrl Pts',(-8.09044330900325,0.751335727411188,
45.3821776798022));
#177221=CARTESIAN_POINT('Ctrl Pts',(-8.08955686338025,0.760820653363481,
45.3818041022267));
#177222=CARTESIAN_POINT('Ctrl Pts',(-8.08689442566711,0.788777844420601,
45.3807047171814));
#177223=CARTESIAN_POINT('Ctrl Pts',(-8.08507182116498,0.807245683606145,
45.3799807425165));
#177224=CARTESIAN_POINT('Ctrl Pts',(-8.07085962259609,0.946374713739244,
45.3745443357744));
#177225=CARTESIAN_POINT('Ctrl Pts',(-8.05583420975066,1.06674096627667,
45.3699504409275));
#177226=CARTESIAN_POINT('Ctrl Pts',(-8.03641889366127,1.19824630978568,
45.3650373395693));
#177227=CARTESIAN_POINT('Ctrl Pts',(-8.03469534084682,1.20974941000309,
45.3646084182519));
#177228=CARTESIAN_POINT('Ctrl Pts',(-8.0277410386084,1.25549237527572,45.3629060046652));
#177229=CARTESIAN_POINT('Ctrl Pts',(-8.02231603376223,1.28970259457657,
45.3616399963894));
#177230=CARTESIAN_POINT('Ctrl Pts',(-8.00039206781983,1.42246206109011,
45.3567519599135));
#177231=CARTESIAN_POINT('Ctrl Pts',(-7.98229427654372,1.52074009796005,
45.3531869732088));
#177232=CARTESIAN_POINT('Ctrl Pts',(-7.83294448115052,2.2554096044385,45.3268019615254));
#177233=CARTESIAN_POINT('Ctrl Pts',(-7.62758768314559,2.87434716211447,
45.3059136198857));
#177234=CARTESIAN_POINT('Ctrl Pts',(-7.18360442274106,3.81697195364983,
45.2697024173584));
#177235=CARTESIAN_POINT('Ctrl Pts',(-6.991072983905,4.15912352909268,45.255540693643));
#177236=CARTESIAN_POINT('Ctrl Pts',(-6.7535741850353,4.51778422284777,45.2390338878057));
#177237=CARTESIAN_POINT('Ctrl Pts',(-6.73232038208992,4.54939565037014,
45.2375643656091));
#177238=CARTESIAN_POINT('Ctrl Pts',(-6.70262734549773,4.59289524179344,
45.2355215356989));
#177239=CARTESIAN_POINT('Ctrl Pts',(-6.6943770870959,4.60491209990383,45.2349550010346));
#177240=CARTESIAN_POINT('Ctrl Pts',(-6.68039415329947,4.62516185252005,
45.233996589977));
#177241=CARTESIAN_POINT('Ctrl Pts',(-6.67467847251796,4.63340646750193,
45.233605325962));
#177242=CARTESIAN_POINT('Ctrl Pts',(-6.66333719892671,4.64970121488785,
45.2328299396103));
#177243=CARTESIAN_POINT('Ctrl Pts',(-6.65771225028756,4.65775177589896,
45.2324458408619));
#177244=CARTESIAN_POINT('Ctrl Pts',(-6.64528126898984,4.67547476695927,
45.2315980217185));
#177245=CARTESIAN_POINT('Ctrl Pts',(-6.63846869124513,4.68514256713675,
45.2311340644658));
#177246=CARTESIAN_POINT('Ctrl Pts',(-6.61459166362652,4.71887007143144,
45.2295103000987));
#177247=CARTESIAN_POINT('Ctrl Pts',(-6.59741742187913,4.74285156492032,
45.2283465016564));
#177248=CARTESIAN_POINT('Ctrl Pts',(-6.41718535115487,4.9916479521449,45.2161753308082));
#177249=CARTESIAN_POINT('Ctrl Pts',(-6.242845461206,5.20803985701046,45.2047491767878));
#177250=CARTESIAN_POINT('Ctrl Pts',(-5.97721703900751,5.50519544344796,
45.1878086820734));
#177251=CARTESIAN_POINT('Ctrl Pts',(-5.89465495528056,5.59350892050967,
45.182602900367));
#177252=CARTESIAN_POINT('Ctrl Pts',(-5.42941418854369,6.06941506633686,
45.153622969414));
#177253=CARTESIAN_POINT('Ctrl Pts',(-5.01048674582911,6.41960287061624,
45.1287035164661));
#177254=CARTESIAN_POINT('Ctrl Pts',(-4.24805436883545,6.93653458664437,
45.0875440716594));
#177255=CARTESIAN_POINT('Ctrl Pts',(-3.92204468498437,7.12594497405542,
45.0710824623263));
#177256=CARTESIAN_POINT('Ctrl Pts',(-3.54042037364813,7.31351313601746,
45.0538769648425));
#177257=CARTESIAN_POINT('Ctrl Pts',(-3.49660021335185,7.33456459657802,
45.051931136617));
#177258=CARTESIAN_POINT('Ctrl Pts',(-3.44052797024926,7.36088530685993,
45.049475902821));
#177259=CARTESIAN_POINT('Ctrl Pts',(-3.42844852594054,7.36651925421631,
45.0489490146779));
#177260=CARTESIAN_POINT('Ctrl Pts',(-3.4090694708078,7.37549980594561,45.0481069013155));
#177261=CARTESIAN_POINT('Ctrl Pts',(-3.40177869902302,7.37886534148689,
45.0477908001003));
#177262=CARTESIAN_POINT('Ctrl Pts',(-3.38795125511701,7.38522345894802,
45.0471926312692));
#177263=CARTESIAN_POINT('Ctrl Pts',(-3.38141558069347,7.38821818280482,
45.0469104667181));
#177264=CARTESIAN_POINT('Ctrl Pts',(-3.36659825835626,7.39498387657562,
45.0462720215924));
#177265=CARTESIAN_POINT('Ctrl Pts',(-3.35831422474455,7.39874961981613,
45.0459159736402));
#177266=CARTESIAN_POINT('Ctrl Pts',(-3.33698435895785,7.40840251348089,
45.0450014683825));
#177267=CARTESIAN_POINT('Ctrl Pts',(-3.32392923518722,7.41426913838569,
45.0444439022422));
#177268=CARTESIAN_POINT('Ctrl Pts',(-3.2468858711594,7.44864598547684,45.0411658633859));
#177269=CARTESIAN_POINT('Ctrl Pts',(-3.18254548809281,7.4763627140695,45.0384785198737));
#177270=CARTESIAN_POINT('Ctrl Pts',(-2.44331803344873,7.7835369077003,45.0080920308414));
#177271=CARTESIAN_POINT('Ctrl Pts',(-1.73401533819079,7.97161566454119,
44.9831039707371));
#177272=CARTESIAN_POINT('Ctrl Pts',(-0.712458494096431,8.09947202621859,
44.9453992624519));
#177273=CARTESIAN_POINT('Ctrl Pts',(-0.414033940448249,8.12019772104746,
44.9342518477751));
#177274=CARTESIAN_POINT('Ctrl Pts',(0.0822609033961705,8.12723205720843,
44.9154013165454));
#177275=CARTESIAN_POINT('Ctrl Pts',(0.279709784340779,8.12283374114866,
44.9078264745174));
#177276=CARTESIAN_POINT('Ctrl Pts',(0.609571087942919,8.10344372815655,
44.8950799401636));
#177277=CARTESIAN_POINT('Ctrl Pts',(0.742131558063892,8.09238020800831,
44.8899287518685));
#177278=CARTESIAN_POINT('Ctrl Pts',(0.927038347820043,8.07236613493958,
44.8826877445129));
#177279=CARTESIAN_POINT('Ctrl Pts',(0.979659804493552,8.06614912752745,
44.8806207634749));
#177280=CARTESIAN_POINT('Ctrl Pts',(1.07025126604122,8.05454655223554,44.8770504252935));
#177281=CARTESIAN_POINT('Ctrl Pts',(1.10825096604494,8.04940604747869,44.8755491880151));
#177282=CARTESIAN_POINT('Ctrl Pts',(1.18116793908095,8.03901589347521,44.8726611590434));
#177283=CARTESIAN_POINT('Ctrl Pts',(1.21609019998089,8.03380724504245,44.8712747511448));
#177284=CARTESIAN_POINT('Ctrl Pts',(1.3079946995373,8.01948672563891,44.8676172489392));
#177285=CARTESIAN_POINT('Ctrl Pts',(1.3649156022477,8.00999518273489,44.8653429331886));
#177286=CARTESIAN_POINT('Ctrl Pts',(1.57085445535829,7.97339602694035,44.8570797287275));
#177287=CARTESIAN_POINT('Ctrl Pts',(1.71920691171149,7.94272967368668,44.8510605860194));
#177288=CARTESIAN_POINT('Ctrl Pts',(2.35131172397897,7.79352565555383,44.8251008319314));
#177289=CARTESIAN_POINT('Ctrl Pts',(2.82445890418429,7.63479694414776,44.8048301902614));
#177290=CARTESIAN_POINT('Ctrl Pts',(3.30695751754261,7.42189886193524,44.7834265270393));
#177291=CARTESIAN_POINT('Ctrl Pts',(3.33377254799363,7.40989280225078,44.7822346758421));
#177292=CARTESIAN_POINT('Ctrl Pts',(3.5218987488572,7.32443398875131,44.7738572087877));
#177293=CARTESIAN_POINT('Ctrl Pts',(3.68083531292024,7.2458647991905,44.7666970574187));
#177294=CARTESIAN_POINT('Ctrl Pts',(3.8952686160866,7.13098368279333,44.7569561587073));
#177295=CARTESIAN_POINT('Ctrl Pts',(3.95307928976165,7.09909924649732,44.7543218199998));
#177296=CARTESIAN_POINT('Ctrl Pts',(4.05248077617866,7.04268540303238,44.7497805730705));
#177297=CARTESIAN_POINT('Ctrl Pts',(4.09425328211408,7.01848332897948,44.7478685277292));
#177298=CARTESIAN_POINT('Ctrl Pts',(4.15512191629435,6.98248901915033,44.7450779768425));
#177299=CARTESIAN_POINT('Ctrl Pts',(4.17438867873645,6.97098774985198,44.744194030144));
#177300=CARTESIAN_POINT('Ctrl Pts',(4.20946027062326,6.94985426818393,44.7425838799892));
#177301=CARTESIAN_POINT('Ctrl Pts',(4.22528025939768,6.94024760736314,44.7418571582128));
#177302=CARTESIAN_POINT('Ctrl Pts',(4.26077861781979,6.91852492661886,44.7402253075828));
#177303=CARTESIAN_POINT('Ctrl Pts',(4.2804384178785,6.90637883021331,44.7393207420655));
#177304=CARTESIAN_POINT('Ctrl Pts',(4.33108051684267,6.8747921377427,44.7369880785158));
#177305=CARTESIAN_POINT('Ctrl Pts',(4.36198390488628,6.85522587610914,44.7355621098359));
#177306=CARTESIAN_POINT('Ctrl Pts',(4.58181546129759,6.71395269309282,44.7253954249804));
#177307=CARTESIAN_POINT('Ctrl Pts',(4.765756592046,6.58466096047464,44.7167626730908));
#177308=CARTESIAN_POINT('Ctrl Pts',(5.12668048785489,6.3079131543629,44.6992800782621));
#177309=CARTESIAN_POINT('Ctrl Pts',(5.30322850355997,6.16022626206441,44.6904374838974));
#177310=CARTESIAN_POINT('Ctrl Pts',(5.52648635794501,5.95674579546528,44.6787315525291));
#177311=CARTESIAN_POINT('Ctrl Pts',(5.5790551078985,5.90753890917359,44.6759350755949));
#177312=CARTESIAN_POINT('Ctrl Pts',(5.65994973397002,5.82977472070196,44.6715653994652));
#177313=CARTESIAN_POINT('Ctrl Pts',(5.6887294563797,5.80169470438309,44.6699973698012));
#177314=CARTESIAN_POINT('Ctrl Pts',(5.74224262745843,5.74870154523371,44.6670559263607));
#177315=CARTESIAN_POINT('Ctrl Pts',(5.76702536670895,5.72383946827723,44.66568310852));
#177316=CARTESIAN_POINT('Ctrl Pts',(5.82263150179234,5.66732755997899,44.6625784607601));
#177317=CARTESIAN_POINT('Ctrl Pts',(5.85335941919497,5.63558539706276,44.6608456116069));
#177318=CARTESIAN_POINT('Ctrl Pts',(5.94787501936967,5.53634312551023,44.6554610279046));
#177319=CARTESIAN_POINT('Ctrl Pts',(6.01076511112856,5.46799918161962,44.6517997115051));
#177320=CARTESIAN_POINT('Ctrl Pts',(6.19955859871954,5.25563963057183,44.6405614512073));
#177321=CARTESIAN_POINT('Ctrl Pts',(6.32155909416401,5.10824473013339,44.632948244177));
#177322=CARTESIAN_POINT('Ctrl Pts',(6.56778108748063,4.78842662361782,44.6168372472003));
#177323=CARTESIAN_POINT('Ctrl Pts',(6.6906733655091,4.61515634978962,44.608340014486));
#177324=CARTESIAN_POINT('Ctrl Pts',(6.86061903507362,4.35446494656249,44.5959635610578));
#177325=CARTESIAN_POINT('Ctrl Pts',(6.91308570474049,4.27067966809851,44.5920451139746));
#177326=CARTESIAN_POINT('Ctrl Pts',(6.97896116666159,4.1610852830678,44.5870060102031));
#177327=CARTESIAN_POINT('Ctrl Pts',(6.99377813402844,4.13613311204955,44.5858644220904));
#177328=CARTESIAN_POINT('Ctrl Pts',(7.01850027108073,4.09398768829716,44.5839461880536));
#177329=CARTESIAN_POINT('Ctrl Pts',(7.02847668828978,4.07683660354645,44.5831683248027));
#177330=CARTESIAN_POINT('Ctrl Pts',(7.04788451219962,4.04318841533717,44.5816474740091));
#177331=CARTESIAN_POINT('Ctrl Pts',(7.05732106851708,4.02669442567495,44.5809044070354));
#177332=CARTESIAN_POINT('Ctrl Pts',(7.08007106588813,3.98660447898564,44.5791040313858));
#177333=CARTESIAN_POINT('Ctrl Pts',(7.09332453617936,3.96297471622389,44.578047629301));
#177334=CARTESIAN_POINT('Ctrl Pts',(7.14408116358562,3.87140975788872,44.573971594418));
#177335=CARTESIAN_POINT('Ctrl Pts',(7.18072874295299,3.80300460682597,44.5709635611151));
#177336=CARTESIAN_POINT('Ctrl Pts',(7.41007777652969,3.35977086776508,44.5516760744117));
#177337=CARTESIAN_POINT('Ctrl Pts',(7.57434875249141,2.97095255935598,44.5356505910524));
#177338=CARTESIAN_POINT('Ctrl Pts',(7.77141585486654,2.38019025982771,44.5116677081881));
#177339=CARTESIAN_POINT('Ctrl Pts',(7.82799672897575,2.18693301614099,44.5038827246096));
#177340=CARTESIAN_POINT('Ctrl Pts',(7.8954304854544,1.92023697181414,44.4931762732301));
#177341=CARTESIAN_POINT('Ctrl Pts',(7.91254358578328,1.84845516938181,44.4902984279291));
#177342=CARTESIAN_POINT('Ctrl Pts',(7.9407035610943,1.7227712067595,44.4852647755205));
#177343=CARTESIAN_POINT('Ctrl Pts',(7.95218513525367,1.66897130712437,44.4831117497081));
#177344=CARTESIAN_POINT('Ctrl Pts',(7.97553790769001,1.55382944139232,44.4785070305282));
#177345=CARTESIAN_POINT('Ctrl Pts',(7.987249697207,1.49245873970389,44.4760546117448));
#177346=CARTESIAN_POINT('Ctrl Pts',(8.0225000196189,1.2954293794884,44.4681870697772));
#177347=CARTESIAN_POINT('Ctrl Pts',(8.04329871172858,1.15930558064328,44.4627601131665));
#177348=CARTESIAN_POINT('Ctrl Pts',(8.0760634814595,0.901068015869555,44.4524869881328));
#177349=CARTESIAN_POINT('Ctrl Pts',(8.08874250723559,0.779082527618561,
44.4476435785835));
#177350=CARTESIAN_POINT('Ctrl Pts',(8.10413182001569,0.589341440954557,
44.4401333083677));
#177351=CARTESIAN_POINT('Ctrl Pts',(8.10876331086594,0.521759993070642,
44.4374629606468));
#177352=CARTESIAN_POINT('Ctrl Pts',(8.11550502768295,0.401325983249336,
44.4327149325259));
#177353=CARTESIAN_POINT('Ctrl Pts',(8.11794525130967,0.348495798446415,
44.4306357991851));
#177354=CARTESIAN_POINT('Ctrl Pts',(8.12132811894089,0.255585713392512,
44.4269871001163));
#177355=CARTESIAN_POINT('Ctrl Pts',(8.12249022303476,0.215515792835325,
44.42541620068));
#177356=CARTESIAN_POINT('Ctrl Pts',(8.12461687105055,0.117045429389527,
44.421561277003));
#177357=CARTESIAN_POINT('Ctrl Pts',(8.12524832282328,0.0586400636367198,
44.4192794311841));
#177358=CARTESIAN_POINT('Ctrl Pts',(8.12525491974489,-0.171553006934017,
44.410296314558));
#177359=CARTESIAN_POINT('Ctrl Pts',(8.11981193981901,-0.343296123938928,
44.4036160078732));
#177360=CARTESIAN_POINT('Ctrl Pts',(8.10033598238096,-0.650111030153366,
44.3916430139931));
#177361=CARTESIAN_POINT('Ctrl Pts',(8.08835417673415,-0.78524766315252,
44.3863561626108));
#177362=CARTESIAN_POINT('Ctrl Pts',(8.06596022829843,-0.981750063222547,
44.3786252009258));
#177363=CARTESIAN_POINT('Ctrl Pts',(8.05821758982036,-1.04339677695893,
44.3761936553276));
#177364=CARTESIAN_POINT('Ctrl Pts',(8.04227813131998,-1.15951889108442,
44.3715993920579));
#177365=CARTESIAN_POINT('Ctrl Pts',(8.03423284598387,-1.2140115943198,44.3694375866352));
#177366=CARTESIAN_POINT('Ctrl Pts',(8.01401510338441,-1.34193486943712,
44.3643472006735));
#177367=CARTESIAN_POINT('Ctrl Pts',(8.00138653255227,-1.4152882248396,44.3614162290669));
#177368=CARTESIAN_POINT('Ctrl Pts',(7.94969598499687,-1.69268363622646,
44.3502812531698));
#177369=CARTESIAN_POINT('Ctrl Pts',(7.90382202973324,-1.89537332521706,
44.3420377557613));
#177370=CARTESIAN_POINT('Ctrl Pts',(7.79383566644714,-2.30729384807574,
44.325038503748));
#177371=CARTESIAN_POINT('Ctrl Pts',(7.72893873707275,-2.51614478645766,
44.3162852211738));
#177372=CARTESIAN_POINT('Ctrl Pts',(7.64671444242232,-2.74739241303451,
44.3064612791299));
#177373=CARTESIAN_POINT('Ctrl Pts',(7.63760438971574,-2.77261717916063,
44.3053879175072));
#177374=CARTESIAN_POINT('Ctrl Pts',(7.62689254112645,-2.80182371496526,
44.3041431628281));
#177375=CARTESIAN_POINT('Ctrl Pts',(7.62541228004832,-2.80584987533635,
44.3039715283971));
#177376=CARTESIAN_POINT('Ctrl Pts',(7.55279043406486,-3.00289202582133,
44.2955695528571));
#177377=CARTESIAN_POINT('Ctrl Pts',(7.47434704800034,-3.19313975625692,
44.2873564015562));
#177378=CARTESIAN_POINT('Ctrl Pts',(7.37020801602888,-3.42077648508081,
44.2774576128583));
#177379=CARTESIAN_POINT('Ctrl Pts',(7.35131418261996,-3.46119311497737,
44.2756973656458));
#177380=CARTESIAN_POINT('Ctrl Pts',(7.32087766773431,-3.52492758916795,
44.2729181437735));
#177381=CARTESIAN_POINT('Ctrl Pts',(7.30955425994735,-3.54834903336843,
44.2718960850059));
#177382=CARTESIAN_POINT('Ctrl Pts',(7.28936547854264,-3.5896009498445,44.2700948542616));
#177383=CARTESIAN_POINT('Ctrl Pts',(7.28054668615404,-3.60745395161059,
44.2693149550847));
#177384=CARTESIAN_POINT('Ctrl Pts',(7.26187857555311,-3.64489889565543,
44.2676785468383));
#177385=CARTESIAN_POINT('Ctrl Pts',(7.25201542904595,-3.66448367805545,
44.2668223161907));
#177386=CARTESIAN_POINT('Ctrl Pts',(7.22231308479321,-3.72287262706274,
44.264268424304));
#177387=CARTESIAN_POINT('Ctrl Pts',(7.20224081943805,-3.76155740398518,
44.2625747104102));
#177388=CARTESIAN_POINT('Ctrl Pts',(7.09661686954593,-3.96117857944336,
44.2538199189667));
#177389=CARTESIAN_POINT('Ctrl Pts',(7.00597820713182,-4.11936614395862,
44.2468304139154));
#177390=CARTESIAN_POINT('Ctrl Pts',(6.73024944483812,-4.56511859569667,
44.2267619975062));
#177391=CARTESIAN_POINT('Ctrl Pts',(6.53223439153364,-4.84422097220849,
44.2137151685589));
#177392=CARTESIAN_POINT('Ctrl Pts',(6.27669275257601,-5.16013278170267,
44.1979691883851));
#177393=CARTESIAN_POINT('Ctrl Pts',(6.23556078490337,-5.20976236227084,
44.195465505402));
#177394=CARTESIAN_POINT('Ctrl Pts',(6.16877857623918,-5.288417353187,44.191447282888));
#177395=CARTESIAN_POINT('Ctrl Pts',(6.14350367106949,-5.31775797247312,
44.189936922008));
#177396=CARTESIAN_POINT('Ctrl Pts',(6.09472873888611,-5.37356696079795,
44.1870416611897));
#177397=CARTESIAN_POINT('Ctrl Pts',(6.07126360448104,-5.40006467711225,
44.1856571777615));
#177398=CARTESIAN_POINT('Ctrl Pts',(6.01634083454644,-5.46127503365843,
44.1824357568248));
#177399=CARTESIAN_POINT('Ctrl Pts',(5.98475467598516,-5.49587058385891,
44.1805974177579));
#177400=CARTESIAN_POINT('Ctrl Pts',(5.87763019720732,-5.61118273672971,
44.1744097361266));
#177401=CARTESIAN_POINT('Ctrl Pts',(5.80074461844093,-5.69063001950176,
44.1700457494245));
#177402=CARTESIAN_POINT('Ctrl Pts',(5.59812717404535,-5.89162396064811,
44.1587398292857));
#177403=CARTESIAN_POINT('Ctrl Pts',(5.47005007425579,-6.01072476703551,
44.1517769658818));
#177404=CARTESIAN_POINT('Ctrl Pts',(5.17240468109232,-6.27011160082396,
44.1360318594264));
#177405=CARTESIAN_POINT('Ctrl Pts',(5.0007775741833,-6.40783069546567,44.1272487564396));
#177406=CARTESIAN_POINT('Ctrl Pts',(4.79384480209525,-6.56049715136603,
44.1170763769369));
#177407=CARTESIAN_POINT('Ctrl Pts',(4.76376435824148,-6.58237191409718,
44.1156076896143));
#177408=CARTESIAN_POINT('Ctrl Pts',(4.71460758325386,-6.6176056982552,44.1132245446566));
#177409=CARTESIAN_POINT('Ctrl Pts',(4.69562219348293,-6.63109056359063,
44.1123081903321));
#177410=CARTESIAN_POINT('Ctrl Pts',(4.66143152540633,-6.65515490476045,
44.1106654326722));
#177411=CARTESIAN_POINT('Ctrl Pts',(4.64624755393757,-6.66576434796622,
44.1099385237624));
#177412=CARTESIAN_POINT('Ctrl Pts',(4.6127407961705,-6.68900629439616,44.1083403673681));
#177413=CARTESIAN_POINT('Ctrl Pts',(4.59440217029388,-6.701615593223,44.1074695761782));
#177414=CARTESIAN_POINT('Ctrl Pts',(4.53694925374254,-6.74077248604679,
44.1047533091371));
#177415=CARTESIAN_POINT('Ctrl Pts',(4.49765482980891,-6.76705425670424,
44.1029125610495));
#177416=CARTESIAN_POINT('Ctrl Pts',(4.42874355548889,-6.8122796369159,44.0997121020318));
#177417=CARTESIAN_POINT('Ctrl Pts',(4.3992290443109,-6.83137666671693,44.0983500860251));
#177418=CARTESIAN_POINT('Ctrl Pts',(4.2736831408696,-6.9114586745001,44.0925915281276));
#177419=CARTESIAN_POINT('Ctrl Pts',(4.17649989330501,-6.97061529791405,
44.08822014177));
#177420=CARTESIAN_POINT('Ctrl Pts',(3.64928677856101,-7.27655140765172,
44.0648878450016));
#177421=CARTESIAN_POINT('Ctrl Pts',(3.19859017648461,-7.48562086624576,
44.0462431902046));
#177422=CARTESIAN_POINT('Ctrl Pts',(2.70831348368903,-7.66063573743803,
44.0263297441983));
#177423=CARTESIAN_POINT('Ctrl Pts',(2.68493375579961,-7.66886122917032,
44.0253810849795));
#177424=CARTESIAN_POINT('Ctrl Pts',(2.43999692083465,-7.75377789297895,
44.0154515978058));
#177425=CARTESIAN_POINT('Ctrl Pts',(2.21525949889722,-7.82095131979762,
44.0064163569928));
#177426=CARTESIAN_POINT('Ctrl Pts',(1.92275573253107,-7.89475881853295,
43.9946886352603));
#177427=CARTESIAN_POINT('Ctrl Pts',(1.85737498222384,-7.91039597764122,
43.9920694442624));
#177428=CARTESIAN_POINT('Ctrl Pts',(1.75158962550293,-7.93431292189322,
43.9878339908805));
#177429=CARTESIAN_POINT('Ctrl Pts',(1.71130273932041,-7.9430995637086,43.9862215320902));
#177430=CARTESIAN_POINT('Ctrl Pts',(1.63389254221699,-7.95936660056042,
43.9831240453414));
#177431=CARTESIAN_POINT('Ctrl Pts',(1.59678036329107,-7.96689487707838,
43.9816393970757));
#177432=CARTESIAN_POINT('Ctrl Pts',(1.51060492211509,-7.98374939516942,
43.9781926407273));
#177433=CARTESIAN_POINT('Ctrl Pts',(1.46150563849806,-7.99288326456616,
43.9762292922099));
#177434=CARTESIAN_POINT('Ctrl Pts',(1.30096065853655,-8.02122044401922,
43.9698106284283));
#177435=CARTESIAN_POINT('Ctrl Pts',(1.18919822655473,-8.03854983126021,
43.9653439406352));
#177436=CARTESIAN_POINT('Ctrl Pts',(0.485852237943699,-8.13261799363731,
43.9372409537668));
#177437=CARTESIAN_POINT('Ctrl Pts',(-0.112287566390233,-8.14634140401478,
43.9133683576055));
#177438=CARTESIAN_POINT('Ctrl Pts',(-1.14061059040513,-8.05658535462587,
43.870329392652));
#177439=CARTESIAN_POINT('Ctrl Pts',(-1.5709495469569,-7.98383744375511,
43.8517450237294));
#177440=CARTESIAN_POINT('Ctrl Pts',(-2.26669337639057,-7.80777085755481,
43.8215563886968));
#177441=CARTESIAN_POINT('Ctrl Pts',(-2.53625593626694,-7.72441604295968,
43.8098408578113));
#177442=CARTESIAN_POINT('Ctrl Pts',(-2.82190011867859,-7.61951871943386,
43.7977349152253));
#177443=CARTESIAN_POINT('Ctrl Pts',(-2.84282141182087,-7.61173779290116,
43.7968501330194));
#177444=CARTESIAN_POINT('Ctrl Pts',(-2.87202511825347,-7.60073932069382,
43.7956179776585));
#177445=CARTESIAN_POINT('Ctrl Pts',(-2.88033461846911,-7.59759428947356,
43.7952677143421));
#177446=CARTESIAN_POINT('Ctrl Pts',(-2.89550816017897,-7.59182284233145,
43.7946287398531));
#177447=CARTESIAN_POINT('Ctrl Pts',(-2.90237382297885,-7.58920073309052,
43.7943398526833));
#177448=CARTESIAN_POINT('Ctrl Pts',(-2.916223484814,-7.58388977734259,43.7937575839575));
#177449=CARTESIAN_POINT('Ctrl Pts',(-2.92320734657849,-7.58120058946147,
43.7934642170405));
#177450=CARTESIAN_POINT('Ctrl Pts',(-2.94029193037083,-7.57459492577229,
43.7927471828576));
#177451=CARTESIAN_POINT('Ctrl Pts',(-2.95038857148898,-7.57066788361836,
43.7923239679799));
#177452=CARTESIAN_POINT('Ctrl Pts',(-2.98664546640152,-7.55648238351508,
43.7908062215602));
#177453=CARTESIAN_POINT('Ctrl Pts',(-3.01276051441887,-7.54610835226529,
43.789716791176));
#177454=CARTESIAN_POINT('Ctrl Pts',(-3.09035711888323,-7.51481658287512,
43.7864921238135));
#177455=CARTESIAN_POINT('Ctrl Pts',(-3.14167608255709,-7.49350698273366,
43.7843766759602));
#177456=CARTESIAN_POINT('Ctrl Pts',(-3.33172440629778,-7.41229601884797,
43.7766033458235));
#177457=CARTESIAN_POINT('Ctrl Pts',(-3.46899534253118,-7.34905399182183,
43.7711056209107));
#177458=CARTESIAN_POINT('Ctrl Pts',(-3.89962638709474,-7.13590176015911,
43.7540358132553));
#177459=CARTESIAN_POINT('Ctrl Pts',(-4.18567940677025,-6.97196420692852,
43.7429590886332));
#177460=CARTESIAN_POINT('Ctrl Pts',(-4.6924009418013,-6.63910484374846,
43.7227108822087));
#177461=CARTESIAN_POINT('Ctrl Pts',(-4.91588129332239,-6.47537251974482,
43.7135302269684));
#177462=CARTESIAN_POINT('Ctrl Pts',(-5.53930228835542,-5.96771844354783,
43.6862958692775));
#177463=CARTESIAN_POINT('Ctrl Pts',(-5.91463767426695,-5.595937654131,43.6677090831581));
#177464=CARTESIAN_POINT('Ctrl Pts',(-6.2721373199752,-5.16536966161726,
43.6461965781401));
#177465=CARTESIAN_POINT('Ctrl Pts',(-6.292810882002,-5.14016356508407,43.6449376498866));
#177466=CARTESIAN_POINT('Ctrl Pts',(-6.3213087555192,-5.10498812409495,
43.6431812435748));
#177467=CARTESIAN_POINT('Ctrl Pts',(-6.32926239133614,-5.09512371877596,
43.6426887351025));
#177468=CARTESIAN_POINT('Ctrl Pts',(-6.34291455475529,-5.07811048441957,
43.6418393729979));
#177469=CARTESIAN_POINT('Ctrl Pts',(-6.34862416229896,-5.07097055661881,
43.641482943747));
#177470=CARTESIAN_POINT('Ctrl Pts',(-6.36037715505396,-5.05622234641789,
43.6407467447852));
#177471=CARTESIAN_POINT('Ctrl Pts',(-6.36641896637513,-5.04861283074464,
43.6403669160241));
#177472=CARTESIAN_POINT('Ctrl Pts',(-6.38043982209358,-5.0308887097145,
43.6394822618939));
#177473=CARTESIAN_POINT('Ctrl Pts',(-6.38840847881102,-5.02076594145754,
43.6389770436812));
#177474=CARTESIAN_POINT('Ctrl Pts',(-6.41368302088845,-4.98850152015256,
43.6373668452527));
#177475=CARTESIAN_POINT('Ctrl Pts',(-6.43089803964644,-4.96628912704614,
43.636258439679));
#177476=CARTESIAN_POINT('Ctrl Pts',(-6.75962287167571,-4.53756299518346,
43.6148664524412));
#177477=CARTESIAN_POINT('Ctrl Pts',(-7.0320853861352,-4.10263838288007,
43.5930931606757));
#177478=CARTESIAN_POINT('Ctrl Pts',(-7.53545778628034,-3.09979480313859,
43.5434612772505));
#177479=CARTESIAN_POINT('Ctrl Pts',(-7.74685067876847,-2.52549925227883,
43.5153755186125));
#177480=CARTESIAN_POINT('Ctrl Pts',(-7.93918042723531,-1.74025005816425,
43.4807326997601));
#177481=CARTESIAN_POINT('Ctrl Pts',(-7.97931233656667,-1.54584935029852,
43.4724715200992));
#177482=CARTESIAN_POINT('Ctrl Pts',(-8.01573678266102,-1.32969227894562,
43.4637227558245));
#177483=CARTESIAN_POINT('Ctrl Pts',(-8.0191048387637,-1.30922699381565,
43.4628983384693));
#177484=CARTESIAN_POINT('Ctrl Pts',(-8.02393742399501,-1.27914440365713,
43.4616919651483));
#177485=CARTESIAN_POINT('Ctrl Pts',(-8.02546308471682,-1.26953710718351,
43.4613075107311));
#177486=CARTESIAN_POINT('Ctrl Pts',(-8.02814497463701,-1.25245083727079,
43.4606251926377));
#177487=CARTESIAN_POINT('Ctrl Pts',(-8.02930801338898,-1.24497295560636,
43.4603270569537));
#177488=CARTESIAN_POINT('Ctrl Pts',(-8.03171030010472,-1.2293838072931,
43.4597065239183));
#177489=CARTESIAN_POINT('Ctrl Pts',(-8.03294771233321,-1.22127226365777,
43.4593841989911));
#177490=CARTESIAN_POINT('Ctrl Pts',(-8.0361248147711,-1.2002318283528,43.4585495451517));
#177491=CARTESIAN_POINT('Ctrl Pts',(-8.03804559635771,-1.18730007734661,
43.4580379456097));
#177492=CARTESIAN_POINT('Ctrl Pts',(-8.04608915636332,-1.13223221305118,
43.4558651127093));
#177493=CARTESIAN_POINT('Ctrl Pts',(-8.05191194838266,-1.09005254432804,
43.4542150961298));
#177494=CARTESIAN_POINT('Ctrl Pts',(-8.0940406148127,-0.766099145188816,
43.4416406689747));
#177495=CARTESIAN_POINT('Ctrl Pts',(-8.1158786617702,-0.482627865515014,
43.4312005377163));
#177496=CARTESIAN_POINT('Ctrl Pts',(-8.135225930706,0.308743104068866,43.4025211807722));
#177497=CARTESIAN_POINT('Ctrl Pts',(-8.10007344109652,0.816113456656182,
43.3845960547325));
#177498=CARTESIAN_POINT('Ctrl Pts',(-7.96596000923648,1.63265612685865,
43.3541518463842));
#177499=CARTESIAN_POINT('Ctrl Pts',(-7.89549106150435,1.94506885710805,
43.3421312063749));
#177500=CARTESIAN_POINT('Ctrl Pts',(-7.79381481825625,2.29746112418802,
43.3280077892873));
#177501=CARTESIAN_POINT('Ctrl Pts',(-7.78045501164359,2.3423058742983,43.3262001139419));
#177502=CARTESIAN_POINT('Ctrl Pts',(-7.75837642384178,2.41414316938138,
43.323287689265));
#177503=CARTESIAN_POINT('Ctrl Pts',(-7.74990232284037,2.44120993645363,
43.3221865233557));
#177504=CARTESIAN_POINT('Ctrl Pts',(-7.73457284415657,2.48928884623968,
43.3202237203911));
#177505=CARTESIAN_POINT('Ctrl Pts',(-7.72777310736054,2.51031847338947,
43.3193628732917));
#177506=CARTESIAN_POINT('Ctrl Pts',(-7.72086420084677,2.53139162522534,
43.3184979200565));
#177507=CARTESIAN_POINT('Ctrl Pts',(-7.72084072433549,2.53146322857538,
43.3184949810506));
#177508=CARTESIAN_POINT('Ctrl Pts',(-7.72079409662351,2.53160543639102,
43.3184891439847));
#177509=CARTESIAN_POINT('Ctrl Pts',(-7.72077095418529,2.53167601423059,
43.3184862470185));
#177510=CARTESIAN_POINT('Ctrl Pts',(-7.72072500094861,2.53181615201227,
43.3184804948148));
#177511=CARTESIAN_POINT('Ctrl Pts',(-7.72070219094693,2.53188570961862,
43.318477639674));
#177512=CARTESIAN_POINT('Ctrl Pts',(-7.72065689865357,2.53202381919728,
43.31847197062));
#177513=CARTESIAN_POINT('Ctrl Pts',(-7.72063441699642,2.53209236932629,
43.3184691567832));
#177514=CARTESIAN_POINT('Ctrl Pts',(-7.72058977699565,2.532228477628,43.3184635697781));
#177515=CARTESIAN_POINT('Ctrl Pts',(-7.72056761945206,2.53229603345048,
43.318460796707));
#177516=CARTESIAN_POINT('Ctrl Pts',(-7.72052362358933,2.53243016587103,
43.3184552907126));
#177517=CARTESIAN_POINT('Ctrl Pts',(-7.72050178604294,2.53249674019989,
43.3184525578832));
#177518=CARTESIAN_POINT('Ctrl Pts',(-7.72045842606367,2.53262892242341,
43.3184471318493));
#177519=CARTESIAN_POINT('Ctrl Pts',(-7.72043690442406,2.53269452798417,
43.3184444387413));
#177520=CARTESIAN_POINT('Ctrl Pts',(-7.72039417215233,2.53282478543858,
43.3184390916282));
#177521=CARTESIAN_POINT('Ctrl Pts',(-7.72037296235442,2.53288943487141,
43.3184364377248));
#177522=CARTESIAN_POINT('Ctrl Pts',(-7.72033084971694,2.53301779265579,
43.3184311685061));
#177523=CARTESIAN_POINT('Ctrl Pts',(-7.72030994774276,2.53308149844944,
43.3184285532965));
#177524=CARTESIAN_POINT('Ctrl Pts',(-7.72026844669099,2.53320798157188,
43.3184233609494));
#177525=CARTESIAN_POINT('Ctrl Pts',(-7.72024784853508,2.53327075616923,
43.3184207839247));
#177526=CARTESIAN_POINT('Ctrl Pts',(-7.7202069511716,2.53339538916199,43.3184156674459));
#177527=CARTESIAN_POINT('Ctrl Pts',(-7.72018665289644,2.5334572447914,43.318413128106));
#177528=CARTESIAN_POINT('Ctrl Pts',(-7.72014635131495,2.53358005219907,
43.3184080864914));
#177529=CARTESIAN_POINT('Ctrl Pts',(-7.72012634900176,2.53364100102445,
43.3184055843386));
#177530=CARTESIAN_POINT('Ctrl Pts',(-7.72009318223559,2.53374205906787,
43.3184014355359));
#177531=CARTESIAN_POINT('Ctrl Pts',(-7.72008001920702,2.53378216532449,
43.3183997890185));
#177532=CARTESIAN_POINT('Ctrl Pts',(-7.72005377507706,2.53386212612016,
43.3183965063012));
#177533=CARTESIAN_POINT('Ctrl Pts',(-7.72004066806906,2.53390205959654,
43.3183948668604));
#177534=CARTESIAN_POINT('Ctrl Pts',(-7.72001450106194,2.53398178123842,
43.3183915939277));
#177535=CARTESIAN_POINT('Ctrl Pts',(-7.72000144123687,2.5340215688813,43.3183899604572));
#177536=CARTESIAN_POINT('Ctrl Pts',(-7.71997536851898,2.5341009991124,43.3183866994548));
#177537=CARTESIAN_POINT('Ctrl Pts',(-7.71996235576821,2.53414064127546,
43.3183850719403));
#177538=CARTESIAN_POINT('Ctrl Pts',(-7.71993637702291,2.53421978110579,
43.3183818228271));
#177539=CARTESIAN_POINT('Ctrl Pts',(-7.71992341121742,2.53425927820475,
43.3183802012517));
#177540=CARTESIAN_POINT('Ctrl Pts',(-7.7198975261035,2.53433812871883,43.3183769639835));
#177541=CARTESIAN_POINT('Ctrl Pts',(-7.71988460704875,2.53437748136872,
43.3183753483221));
#177542=CARTESIAN_POINT('Ctrl Pts',(-7.71985881545119,2.5344560429617,43.3183721228831));
#177543=CARTESIAN_POINT('Ctrl Pts',(-7.71984594304755,2.53449525148833,
43.3183705131226));
#177544=CARTESIAN_POINT('Ctrl Pts',(-7.71982024462464,2.53457352524555,
43.3183672994685));
#177545=CARTESIAN_POINT('Ctrl Pts',(-7.71980741873576,2.5346125900864,43.318365695591));
#177546=CARTESIAN_POINT('Ctrl Pts',(-7.71978181325614,2.53469057675676,
43.3183624936915));
#177547=CARTESIAN_POINT('Ctrl Pts',(-7.7197690337824,2.53472949823728,43.3183608956839));
#177548=CARTESIAN_POINT('Ctrl Pts',(-7.71974352086098,2.53480719903753,
43.3183577054894));
#177549=CARTESIAN_POINT('Ctrl Pts',(-7.71973078762226,2.53484597772815,
43.3183561133283));
#177550=CARTESIAN_POINT('Ctrl Pts',(-7.71970536708742,2.53492339322454,
43.3183529348159));
#177551=CARTESIAN_POINT('Ctrl Pts',(-7.71969267995611,2.53496202953565,
43.3183513484848));
#177552=CARTESIAN_POINT('Ctrl Pts',(-7.71966735153383,2.535039160606,43.3183481816187));
#177553=CARTESIAN_POINT('Ctrl Pts',(-7.71965471038453,2.53507765494102,
43.3183466011012));
#177554=CARTESIAN_POINT('Ctrl Pts',(-7.71962947381584,2.53515450241696,
43.3183434458477));
#177555=CARTESIAN_POINT('Ctrl Pts',(-7.71961687854283,2.53519285511932,
43.3183418711298));
#177556=CARTESIAN_POINT('Ctrl Pts',(-7.71959173348298,2.53526942009338,
43.3183387274443));
#177557=CARTESIAN_POINT('Ctrl Pts',(-7.7195791839334,2.5353076316498,43.3183371585062));
#177558=CARTESIAN_POINT('Ctrl Pts',(-7.71955413011865,2.53538391496745,
43.3183340263545));
#177559=CARTESIAN_POINT('Ctrl Pts',(-7.71954162612672,2.53542198590384,
43.3183324631747));
#177560=CARTESIAN_POINT('Ctrl Pts',(-7.71951666337221,2.53549798817011,
43.3183293425322));
#177561=CARTESIAN_POINT('Ctrl Pts',(-7.71950420482444,2.53553591885301,
43.3183277850959));
#177562=CARTESIAN_POINT('Ctrl Pts',(-7.71947933281627,2.53561164106546,
43.3183246759219));
#177563=CARTESIAN_POINT('Ctrl Pts',(-7.71946691957511,2.53564943193453,
43.3183231242113));
#177564=CARTESIAN_POINT('Ctrl Pts',(-7.71944213804101,2.53572487496364,
43.3183200264705));
#177565=CARTESIAN_POINT('Ctrl Pts',(-7.71942976996171,2.53576252648026,
43.3183184804667));
#177566=CARTESIAN_POINT('Ctrl Pts',(-7.71940507867793,2.53583769104856,
43.3183153941297));
#177567=CARTESIAN_POINT('Ctrl Pts',(-7.71939275564967,2.53587520357067,
43.3183138538182));
#177568=CARTESIAN_POINT('Ctrl Pts',(-7.7193681543073,2.53595009065952,43.318310778845));
#177569=CARTESIAN_POINT('Ctrl Pts',(-7.71935587620204,2.53598746459734,
43.3183092442092));
#177570=CARTESIAN_POINT('Ctrl Pts',(-7.71933136448927,2.53606207519662,
43.3183061805595));
#177571=CARTESIAN_POINT('Ctrl Pts',(-7.71931913114104,2.53609931107565,
43.3183046515779));
#177572=CARTESIAN_POINT('Ctrl Pts',(-7.7192947088611,2.53617364582477,43.3183015992259));
#177573=CARTESIAN_POINT('Ctrl Pts',(-7.71928252014296,2.53621074405155,
43.3183000758819));
#177574=CARTESIAN_POINT('Ctrl Pts',(-7.71925818702915,2.53628480380246,
43.3182970347928));
#177575=CARTESIAN_POINT('Ctrl Pts',(-7.71924604282186,2.53632176475996,
43.318295517071));
#177576=CARTESIAN_POINT('Ctrl Pts',(-7.71922179861044,2.5363955503553,43.3182924872105));
#177577=CARTESIAN_POINT('Ctrl Pts',(-7.71920969881315,2.53643237437031,
43.3182909750976));
#177578=CARTESIAN_POINT('Ctrl Pts',(-7.71918554310673,2.53650588705915,
43.3182879564148));
#177579=CARTESIAN_POINT('Ctrl Pts',(-7.71917348752128,2.53654257475454,
43.3182864498853));
#177580=CARTESIAN_POINT('Ctrl Pts',(-7.71914942016059,2.53661581506093,
43.318283442359));
#177581=CARTESIAN_POINT('Ctrl Pts',(-7.71913740863179,2.53665236692852,
43.3182819413929));
#177582=CARTESIAN_POINT('Ctrl Pts',(-7.71911342952066,2.53672533518425,
43.3182789450098));
#177583=CARTESIAN_POINT('Ctrl Pts',(-7.71910146204209,2.53676175126314,
43.3182774496056));
#177584=CARTESIAN_POINT('Ctrl Pts',(-7.71907757056455,2.53683444938142,
43.3182744642875));
#177585=CARTESIAN_POINT('Ctrl Pts',(-7.71906564690765,2.53687073038643,
43.318272974416));
#177586=CARTESIAN_POINT('Ctrl Pts',(-7.71904184298302,2.53694315865129,
43.3182700001514));
#177587=CARTESIAN_POINT('Ctrl Pts',(-7.71902996300926,2.53697930502313,
43.3182685157948));
#177588=CARTESIAN_POINT('Ctrl Pts',(-7.71900624643302,2.53705146409521,
43.318265552557));
#177589=CARTESIAN_POINT('Ctrl Pts',(-7.71899441006016,2.53708747610323,
43.3182640737043));
#177590=CARTESIAN_POINT('Ctrl Pts',(-7.71897078042849,2.53715936724918,
43.3182611214415));
#177591=CARTESIAN_POINT('Ctrl Pts',(-7.71895898748708,2.53719524542784,
43.3182596480709));
#177592=CARTESIAN_POINT('Ctrl Pts',(-7.71893544458174,2.53726686934943,
43.3182567067546));
#177593=CARTESIAN_POINT('Ctrl Pts',(-7.71892369491311,2.53730261420029,
43.3182552388457));
#177594=CARTESIAN_POINT('Ctrl Pts',(-7.71890023856532,2.53737397144851,
43.3182523084536));
#177595=CARTESIAN_POINT('Ctrl Pts',(-7.71888853208125,2.53740958325863,
43.3182508459947));
#177596=CARTESIAN_POINT('Ctrl Pts',(-7.7188651619421,2.5374806749322,43.318247926482));
#177597=CARTESIAN_POINT('Ctrl Pts',(-7.71885349851508,2.53751615410806,
43.3182464694566));
#177598=CARTESIAN_POINT('Ctrl Pts',(-7.71883021431867,2.53758698105279,
43.3182435607888));
#177599=CARTESIAN_POINT('Ctrl Pts',(-7.71881859382518,2.53762232798861,
43.3182421091808));
#177600=CARTESIAN_POINT('Ctrl Pts',(-7.71879539527648,2.5376928911387,43.31823921132));
#177601=CARTESIAN_POINT('Ctrl Pts',(-7.71878381757113,2.53772810629498,
43.3182377651107));
#177602=CARTESIAN_POINT('Ctrl Pts',(-7.71876070436158,2.53779840662545,
43.318234878017));
#177603=CARTESIAN_POINT('Ctrl Pts',(-7.71874916924161,2.53783349063708,
43.3182334371804));
#177604=CARTESIAN_POINT('Ctrl Pts',(-7.71872614136112,2.53790352821487,
43.3182305608513));
#177605=CARTESIAN_POINT('Ctrl Pts',(-7.71871464880682,2.53793848115988,
43.3182291253844));
#177606=CARTESIAN_POINT('Ctrl Pts',(-7.71869170572183,2.53800825764377,
43.3182262597522));
#177607=CARTESIAN_POINT('Ctrl Pts',(-7.71868025555603,2.53804308007896,
43.3182248296323));
#177608=CARTESIAN_POINT('Ctrl Pts',(-7.7186573969895,2.53811259634722,43.3182219746612));
#177609=CARTESIAN_POINT('Ctrl Pts',(-7.71864598897575,2.53814728900938,
43.3182205498581));
#177610=CARTESIAN_POINT('Ctrl Pts',(-7.71862321504526,2.53821654473994,
43.3182177055615));
#177611=CARTESIAN_POINT('Ctrl Pts',(-7.71861184922293,2.53825110752712,
43.3182162860796));
#177612=CARTESIAN_POINT('Ctrl Pts',(-7.71141079274784,2.56014859472355,
43.3173169597234));
#177613=CARTESIAN_POINT('Ctrl Pts',(-7.70412826127212,2.58198082307861,
43.3164177782825));
#177614=CARTESIAN_POINT('Ctrl Pts',(-7.68565837342603,2.63657762841191,
43.3141625901609));
#177615=CARTESIAN_POINT('Ctrl Pts',(-7.67435419912403,2.66930212477082,
43.3128049217041));
#177616=CARTESIAN_POINT('Ctrl Pts',(-7.64958810192927,2.73953970964014,
43.3098775430473));
#177617=CARTESIAN_POINT('Ctrl Pts',(-7.63605863938204,2.77702797589849,
43.308306840452));
#177618=CARTESIAN_POINT('Ctrl Pts',(-7.59694764146552,2.8829519267926,43.3038443211235));
#177619=CARTESIAN_POINT('Ctrl Pts',(-7.57071828992925,2.95114379165832,
43.3009423080302));
#177620=CARTESIAN_POINT('Ctrl Pts',(-7.48094835357156,3.17545393848171,
43.2912937299656));
#177621=CARTESIAN_POINT('Ctrl Pts',(-7.41347117972893,3.32994576680014,
43.2844811355807));
#177622=CARTESIAN_POINT('Ctrl Pts',(-7.1943775174643,3.79183991538978,43.2635658903136));
#177623=CARTESIAN_POINT('Ctrl Pts',(-7.02808095223314,4.09184314423419,
43.2492081026081));
#177624=CARTESIAN_POINT('Ctrl Pts',(-6.66461197122455,4.65967297660361,
43.2206645242936));
#177625=CARTESIAN_POINT('Ctrl Pts',(-6.46895192405148,4.92770412172795,
43.2065172092838));
#177626=CARTESIAN_POINT('Ctrl Pts',(-6.19097616872694,5.2633037017996,43.1882993655216));
#177627=CARTESIAN_POINT('Ctrl Pts',(-6.12294815635756,5.34228961493669,
43.1839734291377));
#177628=CARTESIAN_POINT('Ctrl Pts',(-5.999762065711,5.47987344974748,43.1763941295349));
#177629=CARTESIAN_POINT('Ctrl Pts',(-5.94521789091443,5.53900194349548,
43.1731218052866));
#177630=CARTESIAN_POINT('Ctrl Pts',(-5.85993637499657,5.62873991630223,
43.168143008614));
#177631=CARTESIAN_POINT('Ctrl Pts',(-5.829817479223,5.65992893978231,43.1664102191611));
#177632=CARTESIAN_POINT('Ctrl Pts',(-5.78985835986735,5.70065042615432,
43.1641462327998));
#177633=CARTESIAN_POINT('Ctrl Pts',(-5.78024191196769,5.71040090977648,
43.1636040150442));
#177634=CARTESIAN_POINT('Ctrl Pts',(-5.765312195909,5.7254623639638,43.1627663281378));
#177635=CARTESIAN_POINT('Ctrl Pts',(-5.76001615936766,5.73079033308376,
43.1624699722669));
#177636=CARTESIAN_POINT('Ctrl Pts',(-5.74942422089966,5.74141662040014,
43.1618788719523));
#177637=CARTESIAN_POINT('Ctrl Pts',(-5.7441283658279,5.74671497450538,43.1615841256178));
#177638=CARTESIAN_POINT('Ctrl Pts',(-5.73232278041858,5.75849350719814,
43.1609288603418));
#177639=CARTESIAN_POINT('Ctrl Pts',(-5.72580936789303,5.76496999252924,
43.1605685405306));
#177640=CARTESIAN_POINT('Ctrl Pts',(-5.70732064493873,5.78329165210559,
43.1595491930477));
#177641=CARTESIAN_POINT('Ctrl Pts',(-5.69531942288969,5.79511069386634,
43.1588916021998));
#177642=CARTESIAN_POINT('Ctrl Pts',(-5.61000194549167,5.87861202412645,
43.1542460794458));
#177643=CARTESIAN_POINT('Ctrl Pts',(-5.53537483730188,5.94893501386298,
43.1503402883846));
#177644=CARTESIAN_POINT('Ctrl Pts',(-5.39356506901399,6.0775860160203,43.1432026924547));
#177645=CARTESIAN_POINT('Ctrl Pts',(-5.3267232241019,6.13625425928232,43.1399475758287));
#177646=CARTESIAN_POINT('Ctrl Pts',(-4.93736629972774,6.46684228061812,
43.1215289968502));
#177647=CARTESIAN_POINT('Ctrl Pts',(-4.59501171187625,6.71442759288274,
43.1074102534538));
#177648=CARTESIAN_POINT('Ctrl Pts',(-3.64554784453508,7.29428987859576,
43.0700097649961));
#177649=CARTESIAN_POINT('Ctrl Pts',(-3.01270579241394,7.57761180737288,
43.0465535127301));
#177650=CARTESIAN_POINT('Ctrl Pts',(-2.30997551292859,7.79009619240129,
43.0184483907628));
#177651=CARTESIAN_POINT('Ctrl Pts',(-2.26817382354244,7.80236970377461,
43.0167703832019));
#177652=CARTESIAN_POINT('Ctrl Pts',(-2.21097676559589,7.81866499880751,
43.0144654916384));
#177653=CARTESIAN_POINT('Ctrl Pts',(-2.19566499349843,7.82297870727617,
43.0138476024746));
#177654=CARTESIAN_POINT('Ctrl Pts',(-2.17139543113407,7.82973918282014,
43.0128668405602));
#177655=CARTESIAN_POINT('Ctrl Pts',(-2.16244591177299,7.83221561675182,
43.0125048807498));
#177656=CARTESIAN_POINT('Ctrl Pts',(-2.14511448355381,7.83697945024005,
43.0118033340963));
#177657=CARTESIAN_POINT('Ctrl Pts',(-2.1367331095607,7.83926875856409,43.0114638064462));
#177658=CARTESIAN_POINT('Ctrl Pts',(-2.11681478141822,7.84467498116884,
43.0106562876363));
#177659=CARTESIAN_POINT('Ctrl Pts',(-2.10527460572266,7.84777989064726,
43.0101879287998));
#177660=CARTESIAN_POINT('Ctrl Pts',(-2.07113658515394,7.85688408099155,
43.0088009338999));
#177661=CARTESIAN_POINT('Ctrl Pts',(-2.04851973565767,7.86281127193661,
43.0078800906289));
#177662=CARTESIAN_POINT('Ctrl Pts',(-1.86945097426594,7.90891471323045,
43.0005737026299));
#177663=CARTESIAN_POINT('Ctrl Pts',(-1.71186424149105,7.94451358068654,
42.9940487045344));
#177664=CARTESIAN_POINT('Ctrl Pts',(-1.34718749593792,8.01553981971223,
42.9787213989851));
#177665=CARTESIAN_POINT('Ctrl Pts',(-1.1395794686277,8.04767940722128,42.9698282733234));
#177666=CARTESIAN_POINT('Ctrl Pts',(-0.659246859878672,8.10307939567049,
42.9489161580937));
#177667=CARTESIAN_POINT('Ctrl Pts',(-0.386128024018008,8.12067704402824,
42.9367758549409));
#177668=CARTESIAN_POINT('Ctrl Pts',(0.15911113577437,8.12823727385243,42.9122975236471));
#177669=CARTESIAN_POINT('Ctrl Pts',(0.430891913528653,8.11836738840273,
42.8999773817311));
#177670=CARTESIAN_POINT('Ctrl Pts',(1.13116826917909,8.05766742681217,42.868457823685));
#177671=CARTESIAN_POINT('Ctrl Pts',(1.55709080156417,7.98630833263183,42.8495032297364));
#177672=CARTESIAN_POINT('Ctrl Pts',(2.00690392570419,7.87356842741467,42.8308946782213));
#177673=CARTESIAN_POINT('Ctrl Pts',(2.03837159261542,7.86548056025775,42.829599978799));
#177674=CARTESIAN_POINT('Ctrl Pts',(2.08127639483327,7.85417832863333,42.8278433961798));
#177675=CARTESIAN_POINT('Ctrl Pts',(2.09275595372134,7.85112738209627,42.8273742583536));
#177676=CARTESIAN_POINT('Ctrl Pts',(2.11092626501703,7.84625553665721,42.8266329794712));
#177677=CARTESIAN_POINT('Ctrl Pts',(2.11762141972482,7.84445123421721,42.8263601209435));
#177678=CARTESIAN_POINT('Ctrl Pts',(2.13057891356626,7.84094147285557,42.8258325676889));
#177679=CARTESIAN_POINT('Ctrl Pts',(2.1368415324452,7.83923707724237,42.8255778279998));
#177680=CARTESIAN_POINT('Ctrl Pts',(2.15171885206167,7.83516900544632,42.8249732253256));
#177681=CARTESIAN_POINT('Ctrl Pts',(2.16033172097101,7.8327986198037,42.8246236440325));
#177682=CARTESIAN_POINT('Ctrl Pts',(2.18580009454235,7.82574415353778,42.8235911813598));
#177683=CARTESIAN_POINT('Ctrl Pts',(2.20264446128824,7.82101981796767,42.8229099538309));
#177684=CARTESIAN_POINT('Ctrl Pts',(2.33028326768221,7.78477593201482,42.8177594111088));
#177685=CARTESIAN_POINT('Ctrl Pts',(2.44041450187959,7.75095703001012,42.8133808375343));
#177686=CARTESIAN_POINT('Ctrl Pts',(2.80946250071686,7.62898435703066,42.7988259573468));
#177687=CARTESIAN_POINT('Ctrl Pts',(3.06464376725408,7.53010294695429,42.788952647525));
#177688=CARTESIAN_POINT('Ctrl Pts',(3.78596785004583,7.20783908608765,42.7605983443867));
#177689=CARTESIAN_POINT('Ctrl Pts',(4.23639902806167,6.95265530020107,42.7422317071644));
#177690=CARTESIAN_POINT('Ctrl Pts',(5.00240361006941,6.41644662906668,42.7075275221651));
#177691=CARTESIAN_POINT('Ctrl Pts',(5.32618550505402,6.15032931690788,42.6915642532777));
#177692=CARTESIAN_POINT('Ctrl Pts',(5.70842868503499,5.78324824074013,42.6710815152664));
#177693=CARTESIAN_POINT('Ctrl Pts',(5.78724640700374,5.70437525018435,42.6667569547309));
#177694=CARTESIAN_POINT('Ctrl Pts',(5.8984332466823,5.58843343788272,42.6604987736079));
#177695=CARTESIAN_POINT('Ctrl Pts',(5.9321282397313,5.5526532013677,42.6585805493182));
#177696=CARTESIAN_POINT('Ctrl Pts',(5.99121129525999,5.48876209068082,42.6551774196928));
#177697=CARTESIAN_POINT('Ctrl Pts',(6.01673134874103,5.46077521387005,42.6536940813364));
#177698=CARTESIAN_POINT('Ctrl Pts',(6.06540148505567,5.40664514131769,42.6508388318612));
#177699=CARTESIAN_POINT('Ctrl Pts',(6.08858056437309,5.38052911521294,42.649467290668));
#177700=CARTESIAN_POINT('Ctrl Pts',(6.13810761446642,5.32399678521263,42.6465109754763));
#177701=CARTESIAN_POINT('Ctrl Pts',(6.16439941714729,5.29353253180919,42.6449256039618));
#177702=CARTESIAN_POINT('Ctrl Pts',(6.26465236088444,5.17560985699768,42.6388177138522));
#177703=CARTESIAN_POINT('Ctrl Pts',(6.33698691704785,5.08678710342411,42.6342773421413));
#177704=CARTESIAN_POINT('Ctrl Pts',(6.50770199983884,4.86786373601786,42.6232225498849));
#177705=CARTESIAN_POINT('Ctrl Pts',(6.60408954305541,4.7362731146837,42.6166892592864));
#177706=CARTESIAN_POINT('Ctrl Pts',(7.01237905660326,4.14214742259587,42.5876595647853));
#177707=CARTESIAN_POINT('Ctrl Pts',(7.28012406102139,3.65111381113903,42.56481333148));
#177708=CARTESIAN_POINT('Ctrl Pts',(7.54380157565832,3.02099870177545,42.5373708478235));
#177709=CARTESIAN_POINT('Ctrl Pts',(7.5894739181055,2.90435220511297,42.5323676853423));
#177710=CARTESIAN_POINT('Ctrl Pts',(7.6438398765672,2.75545021810583,42.5260906180345));
#177711=CARTESIAN_POINT('Ctrl Pts',(7.65505593485097,2.72413520487855,42.5247765736869));
#177712=CARTESIAN_POINT('Ctrl Pts',(7.67193533832621,2.67608070758901,42.5227696872137));
#177713=CARTESIAN_POINT('Ctrl Pts',(7.67773685304264,2.65939026993549,42.5220744229651));
#177714=CARTESIAN_POINT('Ctrl Pts',(7.68931090816715,2.62573919064727,42.5206761850738));
#177715=CARTESIAN_POINT('Ctrl Pts',(7.69508187228439,2.60877816636048,42.5199732275087));
#177716=CARTESIAN_POINT('Ctrl Pts',(7.70682845157251,2.57387652143945,42.5185302093478));
#177717=CARTESIAN_POINT('Ctrl Pts',(7.71279763185633,2.55593384548913,42.5177902574539));
#177718=CARTESIAN_POINT('Ctrl Pts',(7.72171367713446,2.52881756630794,42.516674689839));
#177719=CARTESIAN_POINT('Ctrl Pts',(7.72470694055985,2.51965931787174,42.5162983823247));
#177720=CARTESIAN_POINT('Ctrl Pts',(7.74835368152359,2.446871089066,42.5133111330687));
#177721=CARTESIAN_POINT('Ctrl Pts',(7.76823701919188,2.38299320471857,42.5107112547795));
#177722=CARTESIAN_POINT('Ctrl Pts',(7.82714155320064,2.18517803078143,42.5027136546651));
#177723=CARTESIAN_POINT('Ctrl Pts',(7.86350425565667,2.05047536182246,42.4973425384259));
#177724=CARTESIAN_POINT('Ctrl Pts',(7.96321135834686,1.63931856032761,42.4810720365312));
#177725=CARTESIAN_POINT('Ctrl Pts',(8.01556850876955,1.36042668233816,42.4701953982874));
#177726=CARTESIAN_POINT('Ctrl Pts',(8.06217324061677,1.01270633249905,42.4565928005351));
#177727=CARTESIAN_POINT('Ctrl Pts',(8.07028003231253,0.945934255082753,
42.4539793868732));
#177728=CARTESIAN_POINT('Ctrl Pts',(8.08180445319509,0.840039136813365,
42.449830204852));
#177729=CARTESIAN_POINT('Ctrl Pts',(8.0857691160484,0.800978626131609,42.4482987727469));
#177730=CARTESIAN_POINT('Ctrl Pts',(8.09265244415706,0.727894232208515,
42.4454311311958));
#177731=CARTESIAN_POINT('Ctrl Pts',(8.09564002075744,0.693877684027413,
42.4440955026879));
#177732=CARTESIAN_POINT('Ctrl Pts',(8.10118006138048,0.625883461946875,
42.4414237038685));
#177733=CARTESIAN_POINT('Ctrl Pts',(8.10373340690565,0.591906542886768,
42.4400875677428));
#177734=CARTESIAN_POINT('Ctrl Pts',(8.10909802289794,0.513962775514821,
42.4370198522718));
#177735=CARTESIAN_POINT('Ctrl Pts',(8.11176556218601,0.469987153224875,
42.4352871662012));
#177736=CARTESIAN_POINT('Ctrl Pts',(8.12151370489216,0.284309626197095,
42.427962665018));
#177737=CARTESIAN_POINT('Ctrl Pts',(8.12523976146772,0.142458731127623,
42.4223452556673));
#177738=CARTESIAN_POINT('Ctrl Pts',(8.12524997892878,0.000585164857848444,
42.4167054960774));
#177739=CARTESIAN_POINT('',(8.12525,7.08749465366809E-13,40.4167025567876));
#177740=CARTESIAN_POINT('Ctrl Pts',(8.12525,7.08750173002854E-13,40.4167025567876));
#177741=CARTESIAN_POINT('Ctrl Pts',(8.1252499999998,2.24624642433485,40.5047001499288));
#177742=CARTESIAN_POINT('Ctrl Pts',(7.14398562317558,4.47535249753519,40.59269774307));
#177743=CARTESIAN_POINT('Ctrl Pts',(3.83078204044859,7.50935546634399,40.7686929293524));
#177744=CARTESIAN_POINT('Ctrl Pts',(1.52412477697662,8.29110090552153,40.8566905224937));
#177745=CARTESIAN_POINT('Ctrl Pts',(-2.95101623932641,7.89663306204396,
41.032685708776));
#177746=CARTESIAN_POINT('Ctrl Pts',(-5.08535169588805,6.72342983085734,
41.1206833019173));
#177747=CARTESIAN_POINT('Ctrl Pts',(-7.81671694684439,3.15661951052857,
41.2966784881996));
#177748=CARTESIAN_POINT('Ctrl Pts',(-8.39290461146711,0.79022955155319,
41.3846760813409));
#177749=CARTESIAN_POINT('Ctrl Pts',(-7.60701611462442,-3.63299000730503,
41.5606712676232));
#177750=CARTESIAN_POINT('Ctrl Pts',(-6.2509368040129,-5.65606750610093,
41.6486688607645));
#177751=CARTESIAN_POINT('Ctrl Pts',(-2.45807268688456,-8.06369575488349,
41.8246640470469));
#177752=CARTESIAN_POINT('Ctrl Pts',(-0.05022995104427,-8.42987470330087,
41.9126616401881));
#177753=CARTESIAN_POINT('Ctrl Pts',(4.28689960881094,-7.25863639434505,
42.0886568264705));
#177754=CARTESIAN_POINT('Ctrl Pts',(6.18309125557241,-5.73015646266294,
42.1766544196117));
#177755=CARTESIAN_POINT('Ctrl Pts',(7.81050559202928,-2.58640713800177,
42.3153355274311));
#177756=CARTESIAN_POINT('Ctrl Pts',(8.12525000000008,-1.29375883538076,
42.3660190421094));
#177757=CARTESIAN_POINT('Ctrl Pts',(8.12525,5.33559939809858E-13,42.4167025567876));
#177758=CARTESIAN_POINT('',(8.11892105081991,0.00515126165398824,36.4167025567876));
#177759=CARTESIAN_POINT('Ctrl Pts',(8.1252485711882,-0.00481859980626085,
40.4188459864349));
#177760=CARTESIAN_POINT('Ctrl Pts',(8.1251819769692,-0.117111507396714,
40.4144052047108));
#177761=CARTESIAN_POINT('Ctrl Pts',(8.12278751819628,-0.22939079092564,
40.4099448085709));
#177762=CARTESIAN_POINT('Ctrl Pts',(8.09547973049322,-0.878385878674702,
40.3840313152647));
#177763=CARTESIAN_POINT('Ctrl Pts',(8.01970496545542,-1.41161764218638,
40.3621556303063));
#177764=CARTESIAN_POINT('Ctrl Pts',(7.8469380395891,-2.11681216089531,40.3327010699118));
#177765=CARTESIAN_POINT('Ctrl Pts',(7.79563605181829,-2.29856265439132,
40.3250679245549));
#177766=CARTESIAN_POINT('Ctrl Pts',(7.7170919871729,-2.54379630369786,40.3147517221167));
#177767=CARTESIAN_POINT('Ctrl Pts',(7.69530536892766,-2.60896220197726,
40.3120088286049));
#177768=CARTESIAN_POINT('Ctrl Pts',(7.66125444458475,-2.70667258326552,
40.307896309049));
#177769=CARTESIAN_POINT('Ctrl Pts',(7.64960356275784,-2.73942721905045,
40.3065177399438));
#177770=CARTESIAN_POINT('Ctrl Pts',(7.63028340929652,-2.79265835540521,
40.3042778008842));
#177771=CARTESIAN_POINT('Ctrl Pts',(7.62274109165079,-2.81318038005924,
40.3034143517969));
#177772=CARTESIAN_POINT('Ctrl Pts',(7.60916018908447,-2.84967724958447,
40.3018790702057));
#177773=CARTESIAN_POINT('Ctrl Pts',(7.6031539028261,-2.86566396210636,40.3012066760006));
#177774=CARTESIAN_POINT('Ctrl Pts',(7.59052060888832,-2.89897021809782,
40.2998060900536));
#177775=CARTESIAN_POINT('Ctrl Pts',(7.58388462978731,-2.91628622814618,
40.2990780542807));
#177776=CARTESIAN_POINT('Ctrl Pts',(7.56870242196635,-2.95550059683324,
40.2974294016943));
#177777=CARTESIAN_POINT('Ctrl Pts',(7.56012031828319,-2.9773849111008,40.2965093965113));
#177778=CARTESIAN_POINT('Ctrl Pts',(7.53743130477847,-3.03451114060876,
40.2941074784629));
#177779=CARTESIAN_POINT('Ctrl Pts',(7.52317215334946,-3.06969205429657,
40.2926279063032));
#177780=CARTESIAN_POINT('Ctrl Pts',(7.43791680690272,-3.27587596353569,
40.2839498226564));
#177781=CARTESIAN_POINT('Ctrl Pts',(7.36133807237399,-3.44451344136854,
40.276822830029));
#177782=CARTESIAN_POINT('Ctrl Pts',(7.18896156513465,-3.79204936111791,
40.2619058705827));
#177783=CARTESIAN_POINT('Ctrl Pts',(7.09208997161504,-3.97027281562581,
40.2541220989433));
#177784=CARTESIAN_POINT('Ctrl Pts',(6.93023358092275,-4.24319057357566,
40.2418710136692));
#177785=CARTESIAN_POINT('Ctrl Pts',(6.86973823107639,-4.34044929648943,
40.2374366352345));
#177786=CARTESIAN_POINT('Ctrl Pts',(6.78131951340159,-4.47611900089402,
40.2311401753544));
#177787=CARTESIAN_POINT('Ctrl Pts',(6.75508426352783,-4.51561426856414,
40.2292936188642));
#177788=CARTESIAN_POINT('Ctrl Pts',(6.70963802069234,-4.58274785551292,
40.2261307267005));
#177789=CARTESIAN_POINT('Ctrl Pts',(6.69059820030894,-4.6105006224167,40.2248160463785));
#177790=CARTESIAN_POINT('Ctrl Pts',(6.65025131904567,-4.66853465648938,
40.2220515368519));
#177791=CARTESIAN_POINT('Ctrl Pts',(6.62890859924075,-4.69879018647623,
40.2206013874757));
#177792=CARTESIAN_POINT('Ctrl Pts',(6.57387199283709,-4.77568899243237,
40.2168924205391));
#177793=CARTESIAN_POINT('Ctrl Pts',(6.53988815231436,-4.822122068366,40.2146308123889));
#177794=CARTESIAN_POINT('Ctrl Pts',(6.36557719683538,-5.05505564789734,
40.2031711204747));
#177795=CARTESIAN_POINT('Ctrl Pts',(6.21775544279945,-5.23580705588439,
40.1938993689842));
#177796=CARTESIAN_POINT('Ctrl Pts',(5.94837388922065,-5.53767498081775,
40.1777566921731));
#177797=CARTESIAN_POINT('Ctrl Pts',(5.8303790990267,-5.6617731878283,40.1709096303088));
#177798=CARTESIAN_POINT('Ctrl Pts',(5.63621283063207,-5.85347130840994,
40.1600262849563));
#177799=CARTESIAN_POINT('Ctrl Pts',(5.56253882696945,-5.92352795451505,
40.1559792936496));
#177800=CARTESIAN_POINT('Ctrl Pts',(5.45512319602477,-6.02189788605954,
40.1502062101591));
#177801=CARTESIAN_POINT('Ctrl Pts',(5.42243604516287,-6.05134783309196,
40.1484658181077));
#177802=CARTESIAN_POINT('Ctrl Pts',(5.37051791042152,-6.09736575027585,
40.1457283196326));
#177803=CARTESIAN_POINT('Ctrl Pts',(5.35144579075298,-6.11411151956304,
40.1447283216727));
#177804=CARTESIAN_POINT('Ctrl Pts',(5.31831846615572,-6.1429243358456,40.1430013238426));
#177805=CARTESIAN_POINT('Ctrl Pts',(5.30429988785251,-6.15503317679096,
40.1422735611404));
#177806=CARTESIAN_POINT('Ctrl Pts',(5.27676631023246,-6.17865195614285,
40.1408502386042));
#177807=CARTESIAN_POINT('Ctrl Pts',(5.26325478457163,-6.19016572984544,
40.1401545903957));
#177808=CARTESIAN_POINT('Ctrl Pts',(5.23268152857093,-6.21604609681591,
40.1385866999178));
#177809=CARTESIAN_POINT('Ctrl Pts',(5.2155981426956,-6.23038691217221,40.1377149301721));
#177810=CARTESIAN_POINT('Ctrl Pts',(5.16907263965613,-6.26911774497663,
40.1353520502838));
#177811=CARTESIAN_POINT('Ctrl Pts',(5.13951701783502,-6.29337064671277,
40.1338632365727));
#177812=CARTESIAN_POINT('Ctrl Pts',(4.97315107578598,-6.42793444380456,
40.125547264049));
#177813=CARTESIAN_POINT('Ctrl Pts',(4.83295985692925,-6.53399364949683,
40.1187807203424));
#177814=CARTESIAN_POINT('Ctrl Pts',(4.68016225860993,-6.6419799630296,40.1115959796777));
#177815=CARTESIAN_POINT('Ctrl Pts',(4.67087203141289,-6.6485164557599,40.1111598739999));
#177816=CARTESIAN_POINT('Ctrl Pts',(4.64096565903866,-6.66946459874231,
40.1097583047798));
#177817=CARTESIAN_POINT('Ctrl Pts',(4.62029628046534,-6.68380000929254,
40.1087931448782));
#177818=CARTESIAN_POINT('Ctrl Pts',(4.58336915500097,-6.70915796078588,
40.1070748082565));
#177819=CARTESIAN_POINT('Ctrl Pts',(4.56713738390945,-6.72021796303621,
40.1063215337671));
#177820=CARTESIAN_POINT('Ctrl Pts',(4.31249044281815,-6.89238054166912,
40.0945348456375));
#177821=CARTESIAN_POINT('Ctrl Pts',(4.06572372624255,-7.04076507792674,
40.0835270349664));
#177822=CARTESIAN_POINT('Ctrl Pts',(3.65930398638107,-7.25664683608995,
40.0657745856703));
#177823=CARTESIAN_POINT('Ctrl Pts',(3.50446420412401,-7.33267746359716,
40.0590951308392));
#177824=CARTESIAN_POINT('Ctrl Pts',(3.28305051318219,-7.43278160218562,
40.0496334060862));
#177825=CARTESIAN_POINT('Ctrl Pts',(3.21840185453257,-7.4610021083678,40.0468813884373));
#177826=CARTESIAN_POINT('Ctrl Pts',(3.10487426610065,-7.50880915987454,
40.0420659194891));
#177827=CARTESIAN_POINT('Ctrl Pts',(3.0561570490982,-7.52876904119957,40.0400049796456));
#177828=CARTESIAN_POINT('Ctrl Pts',(2.95302932740019,-7.56985546714256,
40.0356534523509));
#177829=CARTESIAN_POINT('Ctrl Pts',(2.89857819416075,-7.59087204647968,
40.0333623599727));
#177830=CARTESIAN_POINT('Ctrl Pts',(2.72695079120161,-7.65499934472716,
40.0261611326993));
#177831=CARTESIAN_POINT('Ctrl Pts',(2.6090047966837,-7.69599697012235,40.0212413762091));
#177832=CARTESIAN_POINT('Ctrl Pts',(2.34541753594677,-7.78086285281284,
40.0103154403997));
#177833=CARTESIAN_POINT('Ctrl Pts',(2.19939393744849,-7.82339290015442,
40.0043081043583));
#177834=CARTESIAN_POINT('Ctrl Pts',(1.99353865432809,-7.87712985526717,
39.9959176202091));
#177835=CARTESIAN_POINT('Ctrl Pts',(1.93464415275881,-7.89180100807817,
39.9935260622607));
#177836=CARTESIAN_POINT('Ctrl Pts',(1.87427880792064,-7.90612220565004,
39.9910849200648));
#177837=CARTESIAN_POINT('Ctrl Pts',(1.8729668150793,-7.90643312057372,39.9910318686688));
#177838=CARTESIAN_POINT('Ctrl Pts',(1.87034324980781,-7.9070541611145,39.9909257926807));
#177839=CARTESIAN_POINT('Ctrl Pts',(1.86903167747601,-7.90736428701065,
39.9908727680883));
#177840=CARTESIAN_POINT('Ctrl Pts',(1.86640865832378,-7.90798382005548,
39.9907667337977));
#177841=CARTESIAN_POINT('Ctrl Pts',(1.86509721158565,-7.90829322733173,
39.9907137241008));
#177842=CARTESIAN_POINT('Ctrl Pts',(1.86247413720249,-7.90891139578969,
39.9906077072349));
#177843=CARTESIAN_POINT('Ctrl Pts',(1.86116250958926,-7.90922015694973,
39.9905547000674));
#177844=CARTESIAN_POINT('Ctrl Pts',(1.85853875577263,-7.90983710783268,
39.9904486754479));
#177845=CARTESIAN_POINT('Ctrl Pts',(1.85722662956809,-7.91014529737471,
39.9903956579986));
#177846=CARTESIAN_POINT('Ctrl Pts',(1.85550300436084,-7.91054968645628,
39.9903260201186));
#177847=CARTESIAN_POINT('Ctrl Pts',(1.85509157451694,-7.91064618038513,
39.9903093980224));
#177848=CARTESIAN_POINT('Ctrl Pts',(1.85423286767628,-7.91084750491217,
39.9902747065918));
#177849=CARTESIAN_POINT('Ctrl Pts',(1.85378558932523,-7.91095232967285,
39.9902566372911));
#177850=CARTESIAN_POINT('Ctrl Pts',(1.85285235375731,-7.9111709605331,39.9902189373286));
#177851=CARTESIAN_POINT('Ctrl Pts',(1.85236639493926,-7.91128475979129,
39.990199306706));
#177852=CARTESIAN_POINT('Ctrl Pts',(1.85135278869658,-7.91152202221167,
39.9901583628404));
#177853=CARTESIAN_POINT('Ctrl Pts',(1.85082513940203,-7.91164547736515,
39.9901370496435));
#177854=CARTESIAN_POINT('Ctrl Pts',(1.84972495949717,-7.91190277255842,
39.9900926120434));
#177855=CARTESIAN_POINT('Ctrl Pts',(1.84915242669486,-7.91203660324274,
39.9900694876938));
#177856=CARTESIAN_POINT('Ctrl Pts',(1.84795909969006,-7.91231540920709,
39.9900212917084));
#177857=CARTESIAN_POINT('Ctrl Pts',(1.8473383029026,-7.9124603735837,39.989996220134));
#177858=CARTESIAN_POINT('Ctrl Pts',(1.84604487648848,-7.912762245483,39.9899439859762));
#177859=CARTESIAN_POINT('Ctrl Pts',(1.84537224392627,-7.91291914029817,
39.9899168234676));
#177860=CARTESIAN_POINT('Ctrl Pts',(1.8439713798153,-7.91324571032853,39.9898602559539));
#177861=CARTESIAN_POINT('Ctrl Pts',(1.84324314483148,-7.91341537078919,
39.9898308510351));
#177862=CARTESIAN_POINT('Ctrl Pts',(1.84172711196871,-7.91376834774494,
39.9897696393416));
#177863=CARTESIAN_POINT('Ctrl Pts',(1.84093931010477,-7.9139516471382,39.989737832667));
#177864=CARTESIAN_POINT('Ctrl Pts',(1.83929997896678,-7.91433281547642,
39.9896716501324));
#177865=CARTESIAN_POINT('Ctrl Pts',(1.83844844510834,-7.91453066463407,
39.9896372743897));
#177866=CARTESIAN_POINT('Ctrl Pts',(1.83667728213165,-7.91494188323866,
39.9895657783293));
#177867=CARTESIAN_POINT('Ctrl Pts',(1.83575764772262,-7.91515522984686,
39.9895286581475));
#177868=CARTESIAN_POINT('Ctrl Pts',(1.83384570951133,-7.91559843054879,
39.9894514896615));
#177869=CARTESIAN_POINT('Ctrl Pts',(1.83285339960373,-7.91582825834169,
39.9894114415142));
#177870=CARTESIAN_POINT('Ctrl Pts',(1.83079132645743,-7.91630544427434,
39.9893282252746));
#177871=CARTESIAN_POINT('Ctrl Pts',(1.82972155624718,-7.91655277217829,
39.9892850573654));
#177872=CARTESIAN_POINT('Ctrl Pts',(1.82749956446088,-7.91706601606434,
39.9891954013589));
#177873=CARTESIAN_POINT('Ctrl Pts',(1.82634733488476,-7.9173318973746,39.9891489134723));
#177874=CARTESIAN_POINT('Ctrl Pts',(1.82395520666374,-7.91788333997653,
39.9890524086529));
#177875=CARTESIAN_POINT('Ctrl Pts',(1.82271529889148,-7.91816886158542,
39.9890023919636));
#177876=CARTESIAN_POINT('Ctrl Pts',(1.82014236976715,-7.91876071030438,
39.9888986118119));
#177877=CARTESIAN_POINT('Ctrl Pts',(1.81880933801753,-7.91906699209084,
39.9888448486304));
#177878=CARTESIAN_POINT('Ctrl Pts',(1.81604448062742,-7.91970151992816,
39.9887333485743));
#177879=CARTESIAN_POINT('Ctrl Pts',(1.81461264317271,-7.92002971431345,
39.9886756120234));
#177880=CARTESIAN_POINT('Ctrl Pts',(1.81164424725919,-7.92070925917188,
39.9885559287147));
#177881=CARTESIAN_POINT('Ctrl Pts',(1.81010767539403,-7.92106055086305,
39.9884939823291));
#177882=CARTESIAN_POINT('Ctrl Pts',(1.80692362382067,-7.92178751516963,
39.9883656327704));
#177883=CARTESIAN_POINT('Ctrl Pts',(1.80527612891062,-7.92216312102983,
39.9882992300239));
#177884=CARTESIAN_POINT('Ctrl Pts',(1.76803700737578,-7.93064090172793,
39.9867984781306));
#177885=CARTESIAN_POINT('Ctrl Pts',(1.73239121354811,-7.93850367946046,
39.9853656918028));
#177886=CARTESIAN_POINT('Ctrl Pts',(1.65057425568284,-7.95597361443739,
39.9820861760189));
#177887=CARTESIAN_POINT('Ctrl Pts',(1.60436999730531,-7.96541954065471,
39.9802406517647));
#177888=CARTESIAN_POINT('Ctrl Pts',(1.39331777883707,-8.00665586283508,
39.9718353305307));
#177889=CARTESIAN_POINT('Ctrl Pts',(1.22759079173065,-8.03373473305531,
39.9653028489402));
#177890=CARTESIAN_POINT('Ctrl Pts',(0.903846226043641,-8.07638046380758,
39.9525894849163));
#177891=CARTESIAN_POINT('Ctrl Pts',(0.745976017161152,-8.09248904478588,
39.9464118006412));
#177892=CARTESIAN_POINT('Ctrl Pts',(0.532732046101728,-8.10795445732032,
39.9380593152625));
#177893=CARTESIAN_POINT('Ctrl Pts',(0.477688964854494,-8.11138349153013,
39.9359027156763));
#177894=CARTESIAN_POINT('Ctrl Pts',(0.382351215999723,-8.11634897647779,
39.932164683451));
#177895=CARTESIAN_POINT('Ctrl Pts',(0.34207209574314,-8.11814632980938,
39.9305845830816));
#177896=CARTESIAN_POINT('Ctrl Pts',(0.274014037820888,-8.12067583130098,
39.9279128300663));
#177897=CARTESIAN_POINT('Ctrl Pts',(0.246241666479283,-8.1215654087346,
39.9268220323059));
#177898=CARTESIAN_POINT('Ctrl Pts',(0.209379042880324,-8.122556900316,39.9253733660159));
#177899=CARTESIAN_POINT('Ctrl Pts',(0.200292375896853,-8.12278604584081,
39.9250162012173));
#177900=CARTESIAN_POINT('Ctrl Pts',(0.119515140179965,-8.12468744181302,
39.9218405076695));
#177901=CARTESIAN_POINT('Ctrl Pts',(0.0478059584587918,-8.12542579961906,
39.9190169058176));
#177902=CARTESIAN_POINT('Ctrl Pts',(-0.205672567958882,-8.12468009736984,
39.9090159528562));
#177903=CARTESIAN_POINT('Ctrl Pts',(-0.387371165912396,-8.11804597769241,
39.9018094927786));
#177904=CARTESIAN_POINT('Ctrl Pts',(-0.725351555175829,-8.09433230679333,
39.888317085699));
#177905=CARTESIAN_POINT('Ctrl Pts',(-0.881658147361512,-8.07880120349797,
39.882042347435));
#177906=CARTESIAN_POINT('Ctrl Pts',(-1.06783522663328,-8.05483433608878,
39.8745308909834));
#177907=CARTESIAN_POINT('Ctrl Pts',(-1.09823246219525,-8.0507461586496,
39.8733033137494));
#177908=CARTESIAN_POINT('Ctrl Pts',(-1.3453650205405,-8.01608317129101,
39.8633139249273));
#177909=CARTESIAN_POINT('Ctrl Pts',(-1.5608080161246,-7.97693396640702,
39.854546195635));
#177910=CARTESIAN_POINT('Ctrl Pts',(-1.84579645032834,-7.91315832151464,
39.8429235172893));
#177911=CARTESIAN_POINT('Ctrl Pts',(-1.91696667652322,-7.89621922300006,
39.8400191463585));
#177912=CARTESIAN_POINT('Ctrl Pts',(-2.02403149014228,-7.86920407591601,
39.8356505863755));
#177913=CARTESIAN_POINT('Ctrl Pts',(-2.06010120358055,-7.85983837680962,
39.8341789491582));
#177914=CARTESIAN_POINT('Ctrl Pts',(-2.11928562700564,-7.84403541740643,
39.8317649678267));
#177915=CARTESIAN_POINT('Ctrl Pts',(-2.14243846378034,-7.83774333800429,
39.8308208080423));
#177916=CARTESIAN_POINT('Ctrl Pts',(-2.16563225108831,-7.83132967769123,
39.8298752577217));
#177917=CARTESIAN_POINT('Ctrl Pts',(-2.1657013597474,-7.83131056643966,
39.8298724403441));
#177918=CARTESIAN_POINT('Ctrl Pts',(-2.16583972556701,-7.83127230089845,
39.8298667995399));
#177919=CARTESIAN_POINT('Ctrl Pts',(-2.16590898294062,-7.83125314654562,
39.8298639761046));
#177920=CARTESIAN_POINT('Ctrl Pts',(-2.16604764546928,-7.83121479498823,
39.8298583232143));
#177921=CARTESIAN_POINT('Ctrl Pts',(-2.16611705050937,-7.83119559781124,
39.8298554937641));
#177922=CARTESIAN_POINT('Ctrl Pts',(-2.16625600772886,-7.83115716077045,
39.8298498288703));
#177923=CARTESIAN_POINT('Ctrl Pts',(-2.1663255596686,-7.83113792096871,
39.8298469934364));
#177924=CARTESIAN_POINT('Ctrl Pts',(-2.16646480963405,-7.83109939895714,
39.8298413166183));
#177925=CARTESIAN_POINT('Ctrl Pts',(-2.16653450781359,-7.83108011670054,
39.8298384752278));
#177926=CARTESIAN_POINT('Ctrl Pts',(-2.16667404941672,-7.83104150999953,
39.8298327865306));
#177927=CARTESIAN_POINT('Ctrl Pts',(-2.16674389281416,-7.83102218555816,
39.8298299392251));
#177928=CARTESIAN_POINT('Ctrl Pts',(-2.16688372403984,-7.83098349470005,
39.8298242387311));
#177929=CARTESIAN_POINT('Ctrl Pts',(-2.16695371191143,-7.83096412826713,
39.829821385541));
#177930=CARTESIAN_POINT('Ctrl Pts',(-2.16709383120357,-7.83092535365741,
39.8298156733138));
#177931=CARTESIAN_POINT('Ctrl Pts',(-2.16716396271781,-7.83090594545052,
39.8298128142729));
#177932=CARTESIAN_POINT('Ctrl Pts',(-2.16730436858667,-7.83086708747645,
39.8298070903732));
#177933=CARTESIAN_POINT('Ctrl Pts',(-2.16737464284022,-7.8308476377331,
39.8298042255185));
#177934=CARTESIAN_POINT('Ctrl Pts',(-2.16751533335053,-7.83080869690536,
39.8297984900253));
#177935=CARTESIAN_POINT('Ctrl Pts',(-2.16758574963143,-7.83078920581017,
39.8297956193858));
#177936=CARTESIAN_POINT('Ctrl Pts',(-2.16772672343646,-7.83075018247673,
39.829789872354));
#177937=CARTESIAN_POINT('Ctrl Pts',(-2.16779728083816,-7.83073065026824,
39.8297869959668));
#177938=CARTESIAN_POINT('Ctrl Pts',(-2.16793853602321,-7.83069154493438,
39.8297812374746));
#177939=CARTESIAN_POINT('Ctrl Pts',(-2.16800923383181,-7.8306719717979,
39.8297783553687));
#177940=CARTESIAN_POINT('Ctrl Pts',(-2.16815076902445,-7.83063278481895,
39.8297725854722));
#177941=CARTESIAN_POINT('Ctrl Pts',(-2.16822160635381,-7.83061317098751,
39.8297696976838));
#177942=CARTESIAN_POINT('Ctrl Pts',(-2.16836341965642,-7.83057390286432,
39.8297639164604));
#177943=CARTESIAN_POINT('Ctrl Pts',(-2.16843439580468,-7.83055424852003,
39.8297610230182));
#177944=CARTESIAN_POINT('Ctrl Pts',(-2.16857648597554,-7.830514899572,39.8297552305184));
#177945=CARTESIAN_POINT('Ctrl Pts',(-2.16864760000675,-7.83049520496182,
39.8297523314606));
#177946=CARTESIAN_POINT('Ctrl Pts',(-2.16878996522908,-7.83045577566771,
39.8297465277587));
#177947=CARTESIAN_POINT('Ctrl Pts',(-2.16886121638479,-7.83043604098955,
39.8297436231162));
#177948=CARTESIAN_POINT('Ctrl Pts',(-2.16900385509695,-7.83039653175762,
39.829737808276));
#177949=CARTESIAN_POINT('Ctrl Pts',(-2.16907524258471,-7.83037675721885,
39.8297348980811));
#177950=CARTESIAN_POINT('Ctrl Pts',(-2.16921815312932,-7.83033716848402,
39.8297290721702));
#177951=CARTESIAN_POINT('Ctrl Pts',(-2.16928967619349,-7.83031735428191,
39.8297261564538));
#177952=CARTESIAN_POINT('Ctrl Pts',(-2.16943285704856,-7.83027768644172,
39.8297203195342));
#177953=CARTESIAN_POINT('Ctrl Pts',(-2.16950451488789,-7.83025783278623,
39.829717398329));
#177954=CARTESIAN_POINT('Ctrl Pts',(-2.16964796454732,-7.83021808623396,
39.8297115504623));
#177955=CARTESIAN_POINT('Ctrl Pts',(-2.16971975633641,-7.8301981933418,
39.829708623802));
#177956=CARTESIAN_POINT('Ctrl Pts',(-2.16986347300943,-7.83015836854977,
39.8297027650612));
#177957=CARTESIAN_POINT('Ctrl Pts',(-2.16993539805907,-7.8301384366,39.829699832974));
#177958=CARTESIAN_POINT('Ctrl Pts',(-2.17007938066475,-7.83009853384393,
39.8296939634032));
#177959=CARTESIAN_POINT('Ctrl Pts',(-2.17015143800203,-7.83007856309429,
39.8296910259287));
#177960=CARTESIAN_POINT('Ctrl Pts',(-2.17029568439011,-7.8300385829464,
39.8296851456157));
#177961=CARTESIAN_POINT('Ctrl Pts',(-2.170367873445,-7.83001857354307,39.8296822027772));
#177962=CARTESIAN_POINT('Ctrl Pts',(-2.17051238243866,-7.82997851630594,
39.8296763117701));
#177963=CARTESIAN_POINT('Ctrl Pts',(-2.17058470235686,-7.82995846847392,
39.8296733636023));
#177964=CARTESIAN_POINT('Ctrl Pts',(-2.17072947229866,-7.82991833458347,
39.8296674619687));
#177965=CARTESIAN_POINT('Ctrl Pts',(-2.17080192233333,-7.82989824851807,
39.8296645085023));
#177966=CARTESIAN_POINT('Ctrl Pts',(-2.17094695165827,-7.82985803838475,
39.8296585963061));
#177967=CARTESIAN_POINT('Ctrl Pts',(-2.17101953107432,-7.82983791427808,
39.829655637571));
#177968=CARTESIAN_POINT('Ctrl Pts',(-2.17116481847131,-7.82979762824209,
39.8296497148656));
#177969=CARTESIAN_POINT('Ctrl Pts',(-2.17123752641904,-7.8297774663181,
39.8296467508966));
#177970=CARTESIAN_POINT('Ctrl Pts',(-2.17138307014348,-7.82973710483994,
39.8296408177533));
#177971=CARTESIAN_POINT('Ctrl Pts',(-2.17145590593814,-7.82971690527694,
39.8296378485782));
#177972=CARTESIAN_POINT('Ctrl Pts',(-2.17160170465256,-7.82967646870439,
39.8296319050515));
#177973=CARTESIAN_POINT('Ctrl Pts',(-2.17167466749546,-7.82965623171232,
39.829628930703));
#177974=CARTESIAN_POINT('Ctrl Pts',(-2.17182071953564,-7.82961572048391,
39.8296229768609));
#177975=CARTESIAN_POINT('Ctrl Pts',(-2.17189380874019,-7.82959544624172,
39.829619997367));
#177976=CARTESIAN_POINT('Ctrl Pts',(-2.17204011275934,-7.82955486070807,
39.8296140332644));
#177977=CARTESIAN_POINT('Ctrl Pts',(-2.17211332754264,-7.82953454942148,
39.829611048657));
#177978=CARTESIAN_POINT('Ctrl Pts',(-2.17225988202463,-7.82949388998032,
39.8296050743558));
#177979=CARTESIAN_POINT('Ctrl Pts',(-2.17233322164535,-7.82947354184358,
39.8296020846652));
#177980=CARTESIAN_POINT('Ctrl Pts',(-2.17248002498705,-7.82943280891692,
39.8295961002309));
#177981=CARTESIAN_POINT('Ctrl Pts',(-2.17255348877729,-7.829412424104,39.8295931054844));
#177982=CARTESIAN_POINT('Ctrl Pts',(-2.17270053972405,-7.8293716180173,
39.8295871109681));
#177983=CARTESIAN_POINT('Ctrl Pts',(-2.17277412688221,-7.82935119673931,
39.8295841111983));
#177984=CARTESIAN_POINT('Ctrl Pts',(-2.17292142379105,-7.82931031792593,
39.8295781066672));
#177985=CARTESIAN_POINT('Ctrl Pts',(-2.17299513365084,-7.82928986035652,
39.8295751019014));
#177986=CARTESIAN_POINT('Ctrl Pts',(-2.17314267522118,-7.82924890915493,
39.8295690874084));
#177987=CARTESIAN_POINT('Ctrl Pts',(-2.1732165070184,-7.82922841549497,
39.8295660776777));
#177988=CARTESIAN_POINT('Ctrl Pts',(-2.1733642919015,-7.82918739225713,
39.829560053278));
#177989=CARTESIAN_POINT('Ctrl Pts',(-2.17343824485432,-7.82916686271247,
39.8295570386144));
#177990=CARTESIAN_POINT('Ctrl Pts',(-2.17356513994918,-7.82913163434596,
39.8295518657899));
#177991=CARTESIAN_POINT('Ctrl Pts',(-2.17361808209445,-7.82911693607337,
39.8295497076274));
#177992=CARTESIAN_POINT('Ctrl Pts',(-2.17372457475787,-7.82908736946283,
39.8295453665055));
#177993=CARTESIAN_POINT('Ctrl Pts',(-2.1737781252814,-7.82907250111,39.8295431835458));
#177994=CARTESIAN_POINT('Ctrl Pts',(-2.17388583901435,-7.8290425931012,
39.8295387926538));
#177995=CARTESIAN_POINT('Ctrl Pts',(-2.17394000228027,-7.82902755341591,
39.8295365847192));
#177996=CARTESIAN_POINT('Ctrl Pts',(-2.17404894592648,-7.82899730147151,
39.8295321436969));
#177997=CARTESIAN_POINT('Ctrl Pts',(-2.17410372625624,-7.82898208921256,
39.8295299106112));
#177998=CARTESIAN_POINT('Ctrl Pts',(-2.17421390831106,-7.82895149089026,
39.8295254191125));
#177999=CARTESIAN_POINT('Ctrl Pts',(-2.17426931014589,-7.8289361047823,
39.829523160695));
#178000=CARTESIAN_POINT('Ctrl Pts',(-2.17438073957824,-7.82890515750653,
39.8295186183544));
#178001=CARTESIAN_POINT('Ctrl Pts',(-2.17443676714711,-7.8288895963323,
39.8295163344327));
#178002=CARTESIAN_POINT('Ctrl Pts',(-2.17454945247657,-7.82885829765053,
39.8295117409033));
#178003=CARTESIAN_POINT('Ctrl Pts',(-2.17460611008935,-7.8288425601694,
39.8295094313017));
#178004=CARTESIAN_POINT('Ctrl Pts',(-2.17472005965025,-7.82881090767879,
39.829504786244));
#178005=CARTESIAN_POINT('Ctrl Pts',(-2.17477735171328,-7.82879499262247,
39.8295024507831));
#178006=CARTESIAN_POINT('Ctrl Pts',(-2.17489257446465,-7.82876298374484,
39.8294977538321));
#178007=CARTESIAN_POINT('Ctrl Pts',(-2.1749505050794,-7.8287468899288,39.8294953923449));
#178008=CARTESIAN_POINT('Ctrl Pts',(-2.17506700910107,-7.82871452232841,
39.8294906431713));
#178009=CARTESIAN_POINT('Ctrl Pts',(-2.17512558261446,-7.82869824849903,
39.8294882554807));
#178010=CARTESIAN_POINT('Ctrl Pts',(-2.17524337663283,-7.82866551965869,
39.8294834537293));
#178011=CARTESIAN_POINT('Ctrl Pts',(-2.17530259714821,-7.8286490646291,
39.8294810396681));
#178012=CARTESIAN_POINT('Ctrl Pts',(-2.17542168936825,-7.82861597217462,
39.8294761850045));
#178013=CARTESIAN_POINT('Ctrl Pts',(-2.17548156108439,-7.82859933473053,
39.8294737444018));
#178014=CARTESIAN_POINT('Ctrl Pts',(-2.175601959962,-7.82856587621615,39.8294688364816));
#178015=CARTESIAN_POINT('Ctrl Pts',(-2.17566248695237,-7.82854905517712,
39.8294663691713));
#178016=CARTESIAN_POINT('Ctrl Pts',(-2.17578420035632,-7.82851522831838,
39.8294614076742));
#178017=CARTESIAN_POINT('Ctrl Pts',(-2.17584538688022,-7.82849822245142,
39.8294589134828));
#178018=CARTESIAN_POINT('Ctrl Pts',(-2.17596842337759,-7.82846402476786,
39.8294538980597));
#178019=CARTESIAN_POINT('Ctrl Pts',(-2.17603027338683,-7.82844683292446,
39.8294513768264));
#178020=CARTESIAN_POINT('Ctrl Pts',(-2.17615464106193,-7.8284122620679,
39.8294463071479));
#178021=CARTESIAN_POINT('Ctrl Pts',(-2.17621715854566,-7.82839488308822,
39.8294437587102));
#178022=CARTESIAN_POINT('Ctrl Pts',(-2.17634286507707,-7.82835993682135,
39.8294386344637));
#178023=CARTESIAN_POINT('Ctrl Pts',(-2.17640605419629,-7.82834236949683,
39.8294360586521));
#178024=CARTESIAN_POINT('Ctrl Pts',(-2.17653310785606,-7.8283070454154,
39.8294308795007));
#178025=CARTESIAN_POINT('Ctrl Pts',(-2.17659697250595,-7.82828928861037,
39.8294282761566));
#178026=CARTESIAN_POINT('Ctrl Pts',(-2.17672538122505,-7.82825358440302,
39.8294230417773));
#178027=CARTESIAN_POINT('Ctrl Pts',(-2.17678992528318,-7.82823563698575,
39.8294204107426));
#178028=CARTESIAN_POINT('Ctrl Pts',(-2.17691969669401,-7.82819955042213,
39.8294151208246));
#178029=CARTESIAN_POINT('Ctrl Pts',(-2.17698492412455,-7.82818141123582,
39.8294124619381));
#178030=CARTESIAN_POINT('Ctrl Pts',(-2.1771160662694,-7.82814493996965,
39.8294071161538));
#178031=CARTESIAN_POINT('Ctrl Pts',(-2.17718198081471,-7.82812660791818,
39.8294044292629));
#178032=CARTESIAN_POINT('Ctrl Pts',(-2.17731450095326,-7.8280897498188,
39.8293990273167));
#178033=CARTESIAN_POINT('Ctrl Pts',(-2.17738110658052,-7.82807122374252,
39.82939631226));
#178034=CARTESIAN_POINT('Ctrl Pts',(-2.17751501257517,-7.82803397650965,
39.8293908538317));
#178035=CARTESIAN_POINT('Ctrl Pts',(-2.17758231299994,-7.82801525531789,
39.8293881104578));
#178036=CARTESIAN_POINT('Ctrl Pts',(-2.17771761244208,-7.8279776167246,
39.8293825952384));
#178037=CARTESIAN_POINT('Ctrl Pts',(-2.17778561133009,-7.82795869933952,
39.829379823398));
#178038=CARTESIAN_POINT('Ctrl Pts',(-2.1779223113467,-7.82792066728601,
39.8293742510972));
#178039=CARTESIAN_POINT('Ctrl Pts',(-2.17799101250686,-7.82790155258895,
39.8293714506353));
#178040=CARTESIAN_POINT('Ctrl Pts',(-2.17812912067033,-7.82786312484948,
39.8293658209447));
#178041=CARTESIAN_POINT('Ctrl Pts',(-2.17819852769838,-7.82784381178003,
39.8293629917149));
#178042=CARTESIAN_POINT('Ctrl Pts',(-2.17833805122705,-7.82780498622528,
39.8293573043406));
#178043=CARTESIAN_POINT('Ctrl Pts',(-2.178408167723,-7.82778547372082,39.8293544461963));
#178044=CARTESIAN_POINT('Ctrl Pts',(-2.17854911369094,-7.82774624825957,
39.8293487008504));
#178045=CARTESIAN_POINT('Ctrl Pts',(-2.17861994326358,-7.827726535254,39.8293458136447));
#178046=CARTESIAN_POINT('Ctrl Pts',(-2.17876231903963,-7.82768690771089,
39.829340010027));
#178047=CARTESIAN_POINT('Ctrl Pts',(-2.17883386508615,-7.82766699319594,
39.8293370936215));
#178048=CARTESIAN_POINT('Ctrl Pts',(-2.17897767725032,-7.82762696161307,
39.8293312314643));
#178049=CARTESIAN_POINT('Ctrl Pts',(-2.17904994339091,-7.82760684451737,
39.8293282857117));
#178050=CARTESIAN_POINT('Ctrl Pts',(-2.17919519912821,-7.82756640676634,
39.8293223647224));
#178051=CARTESIAN_POINT('Ctrl Pts',(-2.17926818871999,-7.82754608609068,
39.8293193894859));
#178052=CARTESIAN_POINT('Ctrl Pts',(-2.17941489469947,-7.82750524018461,
39.8293134093931));
#178053=CARTESIAN_POINT('Ctrl Pts',(-2.17948861115696,-7.82748471491273,
39.8293104045338));
#178054=CARTESIAN_POINT('Ctrl Pts',(-2.17963677435974,-7.82744345877572,
39.8293043650532));
#178055=CARTESIAN_POINT('Ctrl Pts',(-2.17971122089749,-7.827422727946,39.8293013304403));
#178056=CARTESIAN_POINT('Ctrl Pts',(-2.17986084748517,-7.82738105972819,
39.8292952313211));
#178057=CARTESIAN_POINT('Ctrl Pts',(-2.1799360275581,-7.82736012231101,
39.8292921668139));
#178058=CARTESIAN_POINT('Ctrl Pts',(-2.18008712435711,-7.8273180399753,
39.8292860077783));
#178059=CARTESIAN_POINT('Ctrl Pts',(-2.18016304113141,-7.82729689502034,
39.8292829132479));
#178060=CARTESIAN_POINT('Ctrl Pts',(-2.18031561457832,-7.82725439663604,
39.8292766940339));
#178061=CARTESIAN_POINT('Ctrl Pts',(-2.1803922711972,-7.82723304319832,
39.8292735693524));
#178062=CARTESIAN_POINT('Ctrl Pts',(-2.18054632750404,-7.82719012689511,
39.8292672897072));
#178063=CARTESIAN_POINT('Ctrl Pts',(-2.18062372713733,-7.82716856402118,
39.8292641347456));
#178064=CARTESIAN_POINT('Ctrl Pts',(-2.18077927237866,-7.82712522796489,
39.8292577944219));
#178065=CARTESIAN_POINT('Ctrl Pts',(-2.18085741820314,-7.82710345469824,
39.8292546090509));
#178066=CARTESIAN_POINT('Ctrl Pts',(-2.18101445892962,-7.82705969691989,
39.8292482077822));
#178067=CARTESIAN_POINT('Ctrl Pts',(-2.18109335380842,-7.82703771239033,
39.8292449918853));
#178068=CARTESIAN_POINT('Ctrl Pts',(-2.18125189566308,-7.82699353117163,
39.8292385294419));
#178069=CARTESIAN_POINT('Ctrl Pts',(-2.18133154268146,-7.82697133444599,
39.8292352828936));
#178070=CARTESIAN_POINT('Ctrl Pts',(-2.18149159181669,-7.82692672792455,
39.8292287590251));
#178071=CARTESIAN_POINT('Ctrl Pts',(-2.18157199383644,-7.82690431813084,
39.829225481709));
#178072=CARTESIAN_POINT('Ctrl Pts',(-2.18173355587189,-7.82685928459056,
39.8292188961868));
#178073=CARTESIAN_POINT('Ctrl Pts',(-2.181814715832,-7.82683666083416,39.8292155879832));
#178074=CARTESIAN_POINT('Ctrl Pts',(-2.1819777965221,-7.82679119851917,
39.8292089405733));
#178075=CARTESIAN_POINT('Ctrl Pts',(-2.18205971725393,-7.8267683599344,
39.829205601367));
#178076=CARTESIAN_POINT('Ctrl Pts',(-2.18222432225902,-7.82672246711287,
39.8291988918389));
#178077=CARTESIAN_POINT('Ctrl Pts',(-2.18230700650684,-7.82669941285721,
39.8291955215183));
#178078=CARTESIAN_POINT('Ctrl Pts',(-2.18247314122627,-7.82665308786786,
39.8291887496526));
#178079=CARTESIAN_POINT('Ctrl Pts',(-2.18255659173976,-7.82662981709617,
39.8291853481058));
#178080=CARTESIAN_POINT('Ctrl Pts',(-2.1827242616678,-7.82658305824907,
39.8291785136788));
#178081=CARTESIAN_POINT('Ctrl Pts',(-2.18280848107302,-7.8265595701496,
39.8291750807991));
#178082=CARTESIAN_POINT('Ctrl Pts',(-2.18297769139592,-7.8265123758385,
39.8291681836));
#178083=CARTESIAN_POINT('Ctrl Pts',(-2.18306268232895,-7.82648866959559,
39.82916471928));
#178084=CARTESIAN_POINT('Ctrl Pts',(-2.18323343819188,-7.8264410382235,
39.8291577590994));
#178085=CARTESIAN_POINT('Ctrl Pts',(-2.18331920323313,-7.82641711303592,
39.8291542632344));
#178086=CARTESIAN_POINT('Ctrl Pts',(-2.18349151003716,-7.82636904293224,
39.8291472398527));
#178087=CARTESIAN_POINT('Ctrl Pts',(-2.1835780515284,-7.82634489806422,
39.8291437123472));
#178088=CARTESIAN_POINT('Ctrl Pts',(-2.18375191356705,-7.82629638786513,
39.8291366255899));
#178089=CARTESIAN_POINT('Ctrl Pts',(-2.18383923420451,-7.82627202248092,
39.8291330663345));
#178090=CARTESIAN_POINT('Ctrl Pts',(-2.18401465689354,-7.8262230705073,
39.8291259159812));
#178091=CARTESIAN_POINT('Ctrl Pts',(-2.18410275890438,-7.8261984839009,
39.8291223248852));
#178092=CARTESIAN_POINT('Ctrl Pts',(-2.18427974664506,-7.82614908875446,
39.8291151107572));
#178093=CARTESIAN_POINT('Ctrl Pts',(-2.18436863244871,-7.82612428016514,
39.8291114877222));
#178094=CARTESIAN_POINT('Ctrl Pts',(-2.18454719004913,-7.82607444033188,
39.8291042096239));
#178095=CARTESIAN_POINT('Ctrl Pts',(-2.18463686187345,-7.82604940905124,
39.8291005545595));
#178096=CARTESIAN_POINT('Ctrl Pts',(-2.18481699381708,-7.82599912310556,
39.8290932123086));
#178097=CARTESIAN_POINT('Ctrl Pts',(-2.18490745387324,-7.82597386842877,
39.8290895251248));
#178098=CARTESIAN_POINT('Ctrl Pts',(-2.18508916441082,-7.82592313500779,
39.8290821185486));
#178099=CARTESIAN_POINT('Ctrl Pts',(-2.18518041493717,-7.82589765622135,
39.8290783991545));
#178100=CARTESIAN_POINT('Ctrl Pts',(-2.18536370855264,-7.82584647389493,
39.8290709280708));
#178101=CARTESIAN_POINT('Ctrl Pts',(-2.18545575159851,-7.82582077033697,
39.8290671763831));
#178102=CARTESIAN_POINT('Ctrl Pts',(-2.18564063231989,-7.82576913780003,
39.8290596406282));
#178103=CARTESIAN_POINT('Ctrl Pts',(-2.18573346998756,-7.82574320879284,
39.8290558565614));
#178104=CARTESIAN_POINT('Ctrl Pts',(-2.18591994196658,-7.82569112470357,
39.8290482559666));
#178105=CARTESIAN_POINT('Ctrl Pts',(-2.1860135762373,-7.82566496960211,
39.8290444394403));
#178106=CARTESIAN_POINT('Ctrl Pts',(-2.18620164333323,-7.8256124326982,
39.8290367738488));
#178107=CARTESIAN_POINT('Ctrl Pts',(-2.18629607619411,-7.82558605085471,
39.8290329247823));
#178108=CARTESIAN_POINT('Ctrl Pts',(-2.18648574237248,-7.82553305984195,
39.8290251940331));
#178109=CARTESIAN_POINT('Ctrl Pts',(-2.18658097567478,-7.82550645064551,
39.8290213123511));
#178110=CARTESIAN_POINT('Ctrl Pts',(-2.18677224462759,-7.82545300430393,
39.8290135162943));
#178111=CARTESIAN_POINT('Ctrl Pts',(-2.18686828021034,-7.82542616714597,
39.8290096019222));
#178112=CARTESIAN_POINT('Ctrl Pts',(-2.18706115544613,-7.82537226430469,
39.8290017404152));
#178113=CARTESIAN_POINT('Ctrl Pts',(-2.18715799515145,-7.82534519857466,
39.8289977932782));
#178114=CARTESIAN_POINT('Ctrl Pts',(-2.18735248031133,-7.82529083802356,
39.8289898661732));
#178115=CARTESIAN_POINT('Ctrl Pts',(-2.18745012583376,-7.82526354315109,
39.8289858862025));
#178116=CARTESIAN_POINT('Ctrl Pts',(-2.1876462243892,-7.82520872372528,
39.8289778933587));
#178117=CARTESIAN_POINT('Ctrl Pts',(-2.18774467735244,-7.82518119915869,
39.8289738804884));
#178118=CARTESIAN_POINT('Ctrl Pts',(-2.1879423924795,-7.82512591977371,
39.8289658217768));
#178119=CARTESIAN_POINT('Ctrl Pts',(-2.18804165453847,-7.82509816495153,
39.8289617759398));
#178120=CARTESIAN_POINT('Ctrl Pts',(-2.18824098937266,-7.82504242453209,
39.8289536512331));
#178121=CARTESIAN_POINT('Ctrl Pts',(-2.18834106213754,-7.82501443890428,
39.8289495723641));
#178122=CARTESIAN_POINT('Ctrl Pts',(-2.18854201987731,-7.82495823635534,
39.8289413815327));
#178123=CARTESIAN_POINT('Ctrl Pts',(-2.18864290482272,-7.82493001940868,
39.8289372695717));
#178124=CARTESIAN_POINT('Ctrl Pts',(-2.18884548831427,-7.82487335373156,
39.8289290125002));
#178125=CARTESIAN_POINT('Ctrl Pts',(-2.18894718694298,-7.82484490494389,
39.8289248673864));
#178126=CARTESIAN_POINT('Ctrl Pts',(-2.18915139921468,-7.82478777508681,
39.8289165439519));
#178127=CARTESIAN_POINT('Ctrl Pts',(-2.1892539128725,-7.82475909397881,
39.8289123656308));
#178128=CARTESIAN_POINT('Ctrl Pts',(-2.1894597565891,-7.82470149898959,
39.8289039757253));
#178129=CARTESIAN_POINT('Ctrl Pts',(-2.1895630866467,-7.82467258507391,
39.8288997641412));
#178130=CARTESIAN_POINT('Ctrl Pts',(-2.1897705644194,-7.82461452401322,
39.828891307659));
#178131=CARTESIAN_POINT('Ctrl Pts',(-2.18987471220733,-7.8245853768127,
39.828887062758));
#178132=CARTESIAN_POINT('Ctrl Pts',(-2.190083826865,-7.82452684867818,39.8288785395843));
#178133=CARTESIAN_POINT('Ctrl Pts',(-2.19018879350566,-7.82449746777283,
39.8288742613211));
#178134=CARTESIAN_POINT('Ctrl Pts',(-2.19039954697668,-7.82443847181203,
39.828865671378));
#178135=CARTESIAN_POINT('Ctrl Pts',(-2.19050533386394,-7.82440885670487,
39.828861359696));
#178136=CARTESIAN_POINT('Ctrl Pts',(-2.19071772889649,-7.8243493919338,
39.8288527028721));
#178137=CARTESIAN_POINT('Ctrl Pts',(-2.19082433707031,-7.82431954222581,
39.8288483577293));
#178138=CARTESIAN_POINT('Ctrl Pts',(-2.21080074354796,-7.81872581693615,
39.8280341593126));
#178139=CARTESIAN_POINT('Ctrl Pts',(-2.23064931950368,-7.81308626249394,
39.8272254034176));
#178140=CARTESIAN_POINT('Ctrl Pts',(-2.26783679034714,-7.8023669668516,
39.8257107047351));
#178141=CARTESIAN_POINT('Ctrl Pts',(-2.28518064861989,-7.79730488056071,
39.825004493789));
#178142=CARTESIAN_POINT('Ctrl Pts',(-2.33265394550703,-7.78327702770808,
39.8230721870066));
#178143=CARTESIAN_POINT('Ctrl Pts',(-2.36274850212809,-7.77419418642854,
39.8218479991728));
#178144=CARTESIAN_POINT('Ctrl Pts',(-2.50354086373117,-7.73080857813394,
39.8161222314859));
#178145=CARTESIAN_POINT('Ctrl Pts',(-2.61355021155178,-7.6943143865977,
39.8116521764866));
#178146=CARTESIAN_POINT('Ctrl Pts',(-3.02176321312957,-7.54912965435448,
39.7950005510652));
#178147=CARTESIAN_POINT('Ctrl Pts',(-3.31429661051441,-7.42535188935789,
39.7829240683185));
#178148=CARTESIAN_POINT('Ctrl Pts',(-3.68355772473503,-7.24292887832528,
39.767079830347));
#178149=CARTESIAN_POINT('Ctrl Pts',(-3.76753836991228,-7.19960212234876,
39.7634354675164));
#178150=CARTESIAN_POINT('Ctrl Pts',(-3.91598720521225,-7.11970655789409,
39.7569106956654));
#178151=CARTESIAN_POINT('Ctrl Pts',(-3.9807469209437,-7.08370179507006,
39.7540355427547));
#178152=CARTESIAN_POINT('Ctrl Pts',(-4.08028154438181,-7.02656705409377,
39.7495687932789));
#178153=CARTESIAN_POINT('Ctrl Pts',(-4.11540557468927,-7.00605302483863,
39.7479832149848));
#178154=CARTESIAN_POINT('Ctrl Pts',(-4.17862274511229,-6.96849188993833,
39.7451120882393));
#178155=CARTESIAN_POINT('Ctrl Pts',(-4.20676935586562,-6.95153643765855,
39.7438274632443));
#178156=CARTESIAN_POINT('Ctrl Pts',(-4.27005236105911,-6.91288980170372,
39.7409247364454));
#178157=CARTESIAN_POINT('Ctrl Pts',(-4.30512778280207,-6.89110058942634,
39.7393057048506));
#178158=CARTESIAN_POINT('Ctrl Pts',(-4.40567795364597,-6.82757046108686,
39.7346346850221));
#178159=CARTESIAN_POINT('Ctrl Pts',(-4.47072221078912,-6.785157289266,39.7315763171149));
#178160=CARTESIAN_POINT('Ctrl Pts',(-4.64483531312543,-6.66803329234237,
39.7232884877699));
#178161=CARTESIAN_POINT('Ctrl Pts',(-4.75270461248176,-6.59158262676681,
39.7180441076068));
#178162=CARTESIAN_POINT('Ctrl Pts',(-5.04186857747583,-6.37585258856342,
39.7036902037643));
#178163=CARTESIAN_POINT('Ctrl Pts',(-5.21922735953489,-6.23150065531565,
39.6945538642326));
#178164=CARTESIAN_POINT('Ctrl Pts',(-5.44162917706752,-6.03432446338089,
39.6827292205568));
#178165=CARTESIAN_POINT('Ctrl Pts',(-5.49241576650423,-5.98813568194523,
39.6800029015519));
#178166=CARTESIAN_POINT('Ctrl Pts',(-5.56791879952114,-5.9176993575639,
39.6759139053764));
#178167=CARTESIAN_POINT('Ctrl Pts',(-5.59307544350426,-5.89392844716465,
39.6745453805691));
#178168=CARTESIAN_POINT('Ctrl Pts',(-5.63686501069081,-5.85201816168369,
39.6721530789692));
#178169=CARTESIAN_POINT('Ctrl Pts',(-5.65556414987715,-5.83394873703186,
39.6711282232715));
#178170=CARTESIAN_POINT('Ctrl Pts',(-5.68856969444956,-5.80174687219388,
39.6693137029558));
#178171=CARTESIAN_POINT('Ctrl Pts',(-5.70291096838506,-5.78765051014218,
39.6685233886861));
#178172=CARTESIAN_POINT('Ctrl Pts',(-5.73045188577533,-5.76037816248689,
39.6670021805882));
#178173=CARTESIAN_POINT('Ctrl Pts',(-5.74365877919381,-5.7472096901385,
39.6662711493347));
#178174=CARTESIAN_POINT('Ctrl Pts',(-5.77682943181101,-5.71390700000489,
39.6644312369548));
#178175=CARTESIAN_POINT('Ctrl Pts',(-5.79673336005715,-5.69371353783658,
39.6633236240303));
#178176=CARTESIAN_POINT('Ctrl Pts',(-5.8731262452021,-5.61539360085841,
39.6590577573738));
#178177=CARTESIAN_POINT('Ctrl Pts',(-5.92885029447873,-5.55652693334649,
39.655914627342));
#178178=CARTESIAN_POINT('Ctrl Pts',(-6.2672918596412,-5.18810997591716,
39.6365957456872));
#178179=CARTESIAN_POINT('Ctrl Pts',(-6.52658519441173,-4.85789336847288,
39.620770287007));
#178180=CARTESIAN_POINT('Ctrl Pts',(-6.99462319292796,-4.15630089341364,
39.5887171053279));
#178181=CARTESIAN_POINT('Ctrl Pts',(-7.20201354171842,-3.78557541896965,
39.5725300128041));
#178182=CARTESIAN_POINT('Ctrl Pts',(-7.4018062149867,-3.35198302043742,
39.5539859670726));
#178183=CARTESIAN_POINT('Ctrl Pts',(-7.4236235778997,-3.3033828655158,39.5519130455387));
#178184=CARTESIAN_POINT('Ctrl Pts',(-7.46045253399993,-3.21913517609428,
39.5483286639629));
#178185=CARTESIAN_POINT('Ctrl Pts',(-7.47569045822439,-3.1835884556694,
39.546819039659));
#178186=CARTESIAN_POINT('Ctrl Pts',(-7.50549377912414,-3.11266989951469,
39.5438124010645));
#178187=CARTESIAN_POINT('Ctrl Pts',(-7.52006433329674,-3.07730128257048,
39.5423154668215));
#178188=CARTESIAN_POINT('Ctrl Pts',(-7.54844025853394,-3.00701627285619,
39.539345562679));
#178189=CARTESIAN_POINT('Ctrl Pts',(-7.56225445162001,-2.97210443971392,
39.5378726966557));
#178190=CARTESIAN_POINT('Ctrl Pts',(-7.59288346851263,-2.89310125603126,
39.5345447924184));
#178191=CARTESIAN_POINT('Ctrl Pts',(-7.60955715573164,-2.84895667188855,
39.5326888154104));
#178192=CARTESIAN_POINT('Ctrl Pts',(-7.66694852514242,-2.6929105804216,
39.5261402518591));
#178193=CARTESIAN_POINT('Ctrl Pts',(-7.70558977749548,-2.58026219475194,
39.5214345800578));
#178194=CARTESIAN_POINT('Ctrl Pts',(-7.93100723669749,-1.87281958140106,
39.4920136738859));
#178195=CARTESIAN_POINT('Ctrl Pts',(-8.05127663399291,-1.25905660289138,
39.4669951067845));
#178196=CARTESIAN_POINT('Ctrl Pts',(-8.14033006716474,-0.127718535303896,
39.4195089625374));
#178197=CARTESIAN_POINT('Ctrl Pts',(-8.13223161532385,0.384803107321045,
39.3975519182653));
#178198=CARTESIAN_POINT('Ctrl Pts',(-8.05880298280382,1.04875732503032,
39.3698639516156));
#178199=CARTESIAN_POINT('Ctrl Pts',(-8.0370995506624,1.20384018408007,39.3634622230776));
#178200=CARTESIAN_POINT('Ctrl Pts',(-8.00591166621803,1.38779199831945,
39.3560140780603));
#178201=CARTESIAN_POINT('Ctrl Pts',(-8.00073110030372,1.41735321167889,
39.3548216879439));
#178202=CARTESIAN_POINT('Ctrl Pts',(-7.99340680751234,1.45782674158068,
39.353195959149));
#178203=CARTESIAN_POINT('Ctrl Pts',(-7.99140431983574,1.46876417347065,
39.3527573118923));
#178204=CARTESIAN_POINT('Ctrl Pts',(-7.98800569133949,1.48711450017874,
39.3520225568526));
#178205=CARTESIAN_POINT('Ctrl Pts',(-7.98662167113063,1.4945296063384,39.3517259784986));
#178206=CARTESIAN_POINT('Ctrl Pts',(-7.98387773655974,1.50911800574823,
39.3511431488239));
#178207=CARTESIAN_POINT('Ctrl Pts',(-7.98251847571596,1.51629141424244,
39.3508568718564));
#178208=CARTESIAN_POINT('Ctrl Pts',(-7.97952028349018,1.53199840587013,
39.3502307340822));
#178209=CARTESIAN_POINT('Ctrl Pts',(-7.97787732642742,1.54053121859241,
39.349891036781));
#178210=CARTESIAN_POINT('Ctrl Pts',(-7.97218250784277,1.56985422008605,
39.3487252589104));
#178211=CARTESIAN_POINT('Ctrl Pts',(-7.96806301912931,1.59063130400415,
39.347901987745));
#178212=CARTESIAN_POINT('Ctrl Pts',(-7.90966495723687,1.879247652144,39.3365064246268));
#178213=CARTESIAN_POINT('Ctrl Pts',(-7.84198957560371,2.14419451368648,
39.3265982952413));
#178214=CARTESIAN_POINT('Ctrl Pts',(-7.62116266974008,2.85674971452128,
39.3005436146682));
#178215=CARTESIAN_POINT('Ctrl Pts',(-7.44209265334162,3.29521284361814,
39.2851093655004));
#178216=CARTESIAN_POINT('Ctrl Pts',(-6.94639615476124,4.25921113486542,
39.2487269731623));
#178217=CARTESIAN_POINT('Ctrl Pts',(-6.60647419115726,4.76945478166142,
39.2274971347593));
#178218=CARTESIAN_POINT('Ctrl Pts',(-6.1942304959262,5.25851755566576,39.2028609958781));
#178219=CARTESIAN_POINT('Ctrl Pts',(-6.17576484996748,5.28019193005629,
39.2017598645026));
#178220=CARTESIAN_POINT('Ctrl Pts',(-6.14873421471051,5.31158383965963,
39.2001513385859));
#178221=CARTESIAN_POINT('Ctrl Pts',(-6.14025922797868,5.32137876308843,
39.1996474865322));
#178222=CARTESIAN_POINT('Ctrl Pts',(-6.12537852284956,5.33849418249886,
39.1987636185115));
#178223=CARTESIAN_POINT('Ctrl Pts',(-6.11898300182386,5.34582352938619,
39.1983840059675));
#178224=CARTESIAN_POINT('Ctrl Pts',(-6.10656431222097,5.36000401864025,
39.1976473830777));
#178225=CARTESIAN_POINT('Ctrl Pts',(-6.10054273522479,5.36685653937149,
39.1972904360502));
#178226=CARTESIAN_POINT('Ctrl Pts',(-6.08617890577347,5.38314708687933,
39.1964395110524));
#178227=CARTESIAN_POINT('Ctrl Pts',(-6.07782623232217,5.39257587058624,
39.1959451187171));
#178228=CARTESIAN_POINT('Ctrl Pts',(-6.04807675668433,5.42600117620617,
39.1941857499752));
#178229=CARTESIAN_POINT('Ctrl Pts',(-6.02655962286843,5.44988993486056,
39.1929159693117));
#178230=CARTESIAN_POINT('Ctrl Pts',(-5.67630873194198,5.83413481687002,
39.172289487356));
#178231=CARTESIAN_POINT('Ctrl Pts',(-5.31596416505834,6.1642548336654,39.1515908810326));
#178232=CARTESIAN_POINT('Ctrl Pts',(-4.80596876738529,6.553319860956,39.1232821619198));
#178233=CARTESIAN_POINT('Ctrl Pts',(-4.68108033619358,6.64310337415656,
39.1164264849211));
#178234=CARTESIAN_POINT('Ctrl Pts',(-4.47782224747682,6.78064850313609,
39.1054333653861));
#178235=CARTESIAN_POINT('Ctrl Pts',(-4.40105982948991,6.830721665907,39.1013177998181));
#178236=CARTESIAN_POINT('Ctrl Pts',(-4.02643373674881,7.06615840036962,
39.0814404921693));
#178237=CARTESIAN_POINT('Ctrl Pts',(-3.7176128548317,7.23340398818993,39.065665669073));
#178238=CARTESIAN_POINT('Ctrl Pts',(-3.21207764323464,7.4662285892181,39.0416262750269));
#178239=CARTESIAN_POINT('Ctrl Pts',(-3.02199307797236,7.54516986998229,
39.0329685035316));
#178240=CARTESIAN_POINT('Ctrl Pts',(-2.79364619224551,7.62998417493303,
39.0231550531384));
#178241=CARTESIAN_POINT('Ctrl Pts',(-2.75810527558184,7.64290343483283,
39.0216433411657));
#178242=CARTESIAN_POINT('Ctrl Pts',(-2.71069127494805,7.65976480006877,
39.0196460350253));
#178243=CARTESIAN_POINT('Ctrl Pts',(-2.69889779933894,7.66392814759418,
39.0191508293896));
#178244=CARTESIAN_POINT('Ctrl Pts',(-2.67946956959745,7.67073631868657,
39.0183375982761));
#178245=CARTESIAN_POINT('Ctrl Pts',(-2.67184042521701,7.67339700445627,
39.0180189035023));
#178246=CARTESIAN_POINT('Ctrl Pts',(-2.6570130716723,7.6785432922786,39.0174007530652));
#178247=CARTESIAN_POINT('Ctrl Pts',(-2.64981531387917,7.68103016250182,
39.0171012451035));
#178248=CARTESIAN_POINT('Ctrl Pts',(-2.63313331164547,7.68676765894157,
39.0164083754198));
#178249=CARTESIAN_POINT('Ctrl Pts',(-2.62364651481158,7.69001086123238,
39.0160153157868));
#178250=CARTESIAN_POINT('Ctrl Pts',(-2.5937980755633,7.70015332965275,39.0147815971318));
#178251=CARTESIAN_POINT('Ctrl Pts',(-2.57341494957766,7.70698937749371,
39.0139434468122));
#178252=CARTESIAN_POINT('Ctrl Pts',(-2.37318488798664,7.77325917847878,
39.0057506887219));
#178253=CARTESIAN_POINT('Ctrl Pts',(-2.19133161432705,7.82647020614236,
38.9986300272372));
#178254=CARTESIAN_POINT('Ctrl Pts',(-1.59997415219955,7.97727334479463,
38.9761003291139));
#178255=CARTESIAN_POINT('Ctrl Pts',(-1.1846960634733,8.04942993408061,38.9611945069414));
#178256=CARTESIAN_POINT('Ctrl Pts',(-0.466645763163058,8.11739846189286,
38.9352016274706));
#178257=CARTESIAN_POINT('Ctrl Pts',(-0.166270535428642,8.12909976743459,
38.9242725170387));
#178258=CARTESIAN_POINT('Ctrl Pts',(0.372946335110583,8.12020209798196,
38.9041827851706));
#178259=CARTESIAN_POINT('Ctrl Pts',(0.611538127078164,8.10572554099386,
38.8951304917143));
#178260=CARTESIAN_POINT('Ctrl Pts',(0.894796380222606,8.07596028686548,
38.8841469783617));
#178261=CARTESIAN_POINT('Ctrl Pts',(0.940411408907324,8.07077576570451,
38.8823710529108));
#178262=CARTESIAN_POINT('Ctrl Pts',(1.01140198766865,8.06209709233737,38.8795960123034));
#178263=CARTESIAN_POINT('Ctrl Pts',(1.03680923264027,8.05886903452129,38.8786006036997));
#178264=CARTESIAN_POINT('Ctrl Pts',(1.08376294110711,8.05267772003594,38.8767569378992));
#178265=CARTESIAN_POINT('Ctrl Pts',(1.10531363264755,8.04974796776937,38.8759091437725));
#178266=CARTESIAN_POINT('Ctrl Pts',(1.15122654221731,8.0433183928796,38.8740995060946));
#178267=CARTESIAN_POINT('Ctrl Pts',(1.1755851650669,8.03979432788134,38.8731373350038));
#178268=CARTESIAN_POINT('Ctrl Pts',(1.24076640661903,8.03006172458242,38.8705568025145));
#178269=CARTESIAN_POINT('Ctrl Pts',(1.28155821572863,8.02365260260789,38.8689356848157));
#178270=CARTESIAN_POINT('Ctrl Pts',(1.46536826638818,7.99333528642364,38.8616010472481));
#178271=CARTESIAN_POINT('Ctrl Pts',(1.60777737506264,7.96591260974251,38.8558362765378));
#178272=CARTESIAN_POINT('Ctrl Pts',(1.88024380044932,7.90584152130384,38.8446220005729));
#178273=CARTESIAN_POINT('Ctrl Pts',(2.01037725672817,7.87375571543561,38.8391835136085));
#178274=CARTESIAN_POINT('Ctrl Pts',(2.36067167923866,7.77813632074388,38.8243078955258));
#178275=CARTESIAN_POINT('Ctrl Pts',(2.5790313095104,7.70848675196743,38.8147756178591));
#178276=CARTESIAN_POINT('Ctrl Pts',(3.04706937102918,7.53708184172281,38.7938161458616));
#178277=CARTESIAN_POINT('Ctrl Pts',(3.29522364002373,7.43194003210416,38.7823610311762));
#178278=CARTESIAN_POINT('Ctrl Pts',(3.78529660430662,7.19491936498721,38.7592837995907));
#178279=CARTESIAN_POINT('Ctrl Pts',(4.02666577315459,7.0626698419597,38.7476782488455));
#178280=CARTESIAN_POINT('Ctrl Pts',(4.35602448774592,6.85982708395537,38.7318200207872));
#178281=CARTESIAN_POINT('Ctrl Pts',(4.44996492774435,6.79926395421352,38.7272953178517));
#178282=CARTESIAN_POINT('Ctrl Pts',(4.55729241029078,6.72689276440429,38.7221465314803));
#178283=CARTESIAN_POINT('Ctrl Pts',(4.57192437164105,6.7169567456133,38.7214450553498));
#178284=CARTESIAN_POINT('Ctrl Pts',(4.59413157391607,6.70177048157487,38.7203812348059));
#178285=CARTESIAN_POINT('Ctrl Pts',(4.60173046936383,6.69655502436361,38.7200173622722));
#178286=CARTESIAN_POINT('Ctrl Pts',(4.61549132842539,6.68707585631193,38.7193587130828));
#178287=CARTESIAN_POINT('Ctrl Pts',(4.62165629382854,6.68281653294731,38.7190637387434));
#178288=CARTESIAN_POINT('Ctrl Pts',(4.63397042472076,6.67428361255352,38.718474769448));
#178289=CARTESIAN_POINT('Ctrl Pts',(4.6401195918153,6.67001003088353,38.7181807742692));
#178290=CARTESIAN_POINT('Ctrl Pts',(4.65742011509124,6.65795091606179,38.7173539591712));
#178291=CARTESIAN_POINT('Ctrl Pts',(4.66855787503468,6.65014585550233,38.7168220608693));
#178292=CARTESIAN_POINT('Ctrl Pts',(4.71436446408398,6.61787396437697,38.7146362753966));
#178293=CARTESIAN_POINT('Ctrl Pts',(4.74886137634211,6.59316341589212,38.7129943441616));
#178294=CARTESIAN_POINT('Ctrl Pts',(5.42577333761911,6.10021423977058,38.6808821688189));
#178295=CARTESIAN_POINT('Ctrl Pts',(5.99628020856969,5.54043843477751,38.6557683994322));
#178296=CARTESIAN_POINT('Ctrl Pts',(6.69034224076001,4.62433826554945,38.616440448427));
#178297=CARTESIAN_POINT('Ctrl Pts',(6.88556393405946,4.32829877959735,38.6039893486984));
#178298=CARTESIAN_POINT('Ctrl Pts',(7.13490096290407,3.89040867536051,38.5853271585033));
#178299=CARTESIAN_POINT('Ctrl Pts',(7.20535340390675,3.75832024706725,38.579671258999));
#178300=CARTESIAN_POINT('Ctrl Pts',(7.2823530659317,3.60382409685525,38.5730055821192));
#178301=CARTESIAN_POINT('Ctrl Pts',(7.29250338161553,3.58323997478331,38.57211649349));
#178302=CARTESIAN_POINT('Ctrl Pts',(7.30776695201863,3.55195304356195,38.5707635452649));
#178303=CARTESIAN_POINT('Ctrl Pts',(7.31294424068456,3.54128151661286,38.5703017973906));
#178304=CARTESIAN_POINT('Ctrl Pts',(7.32226615092641,3.52195939609975,38.5694652358078));
#178305=CARTESIAN_POINT('Ctrl Pts',(7.32641886046876,3.51331271778877,38.5690906890524));
#178306=CARTESIAN_POINT('Ctrl Pts',(7.33467399100099,3.49604578728306,38.5683423673731));
#178307=CARTESIAN_POINT('Ctrl Pts',(7.33877655070547,3.48742561772021,38.5679685977979));
#178308=CARTESIAN_POINT('Ctrl Pts',(7.35023305430371,3.46324383408953,38.5669195529469));
#178309=CARTESIAN_POINT('Ctrl Pts',(7.357552738207,3.44766609564364,38.5662431565377));
#178310=CARTESIAN_POINT('Ctrl Pts',(7.38714904733828,3.38415577281091,38.5634829593133));
#178311=CARTESIAN_POINT('Ctrl Pts',(7.4090069631374,3.33603013089226,38.5613855175646));
#178312=CARTESIAN_POINT('Ctrl Pts',(7.81088301153502,2.42776552140212,38.5216849519242));
#178313=CARTESIAN_POINT('Ctrl Pts',(8.03915329819708,1.50839263913174,38.4785037434441));
#178314=CARTESIAN_POINT('Ctrl Pts',(8.11850364623492,0.381530010391947,
38.4281981582461));
#178315=CARTESIAN_POINT('Ctrl Pts',(8.1251981936157,0.191901387828279,38.4198586473823));
#178316=CARTESIAN_POINT('Ctrl Pts',(8.12530306403275,-0.194326991398393,
38.4033160972334));
#178317=CARTESIAN_POINT('Ctrl Pts',(8.11822602146989,-0.390818134096953,
38.3951409940692));
#178318=CARTESIAN_POINT('Ctrl Pts',(8.10272852959197,-0.604814845761113,
38.3865972702528));
#178319=CARTESIAN_POINT('Ctrl Pts',(8.10137078755534,-0.622737498371618,
38.3858842035754));
#178320=CARTESIAN_POINT('Ctrl Pts',(8.09922980642979,-0.649806406752644,
38.3848108126932));
#178321=CARTESIAN_POINT('Ctrl Pts',(8.09849052636613,-0.658956006821622,
38.3844486102723));
#178322=CARTESIAN_POINT('Ctrl Pts',(8.09718030352606,-0.67483651734461,
38.3838209935984));
#178323=CARTESIAN_POINT('Ctrl Pts',(8.0966164701167,-0.68156799307307,38.3835552822289));
#178324=CARTESIAN_POINT('Ctrl Pts',(8.09542535404545,-0.69557837460763,
38.3830029125989));
#178325=CARTESIAN_POINT('Ctrl Pts',(8.09479664715481,-0.702857154612624,
38.3827163132664));
#178326=CARTESIAN_POINT('Ctrl Pts',(8.09329245903785,-0.720001972001027,
38.3820420988152));
#178327=CARTESIAN_POINT('Ctrl Pts',(8.09240875190378,-0.729867289602332,
38.3816548167233));
#178328=CARTESIAN_POINT('Ctrl Pts',(8.0894560857593,-0.762164866655926,
38.3803890337384));
#178329=CARTESIAN_POINT('Ctrl Pts',(8.08731186458667,-0.784590252826219,
38.3795135051035));
#178330=CARTESIAN_POINT('Ctrl Pts',(8.04959315081964,-1.16247888389211,
38.3648124580738));
#178331=CARTESIAN_POINT('Ctrl Pts',(7.99070460628798,-1.51524869881281,
38.3518484376183));
#178332=CARTESIAN_POINT('Ctrl Pts',(7.76002544546271,-2.49451799077964,
38.3156875430688));
#178333=CARTESIAN_POINT('Ctrl Pts',(7.53617333959681,-3.10591474188473,
38.2926583529603));
#178334=CARTESIAN_POINT('Ctrl Pts',(7.09240338266829,-3.97823448761708,
38.2558383317433));
#178335=CARTESIAN_POINT('Ctrl Pts',(6.92504051766862,-4.26290253188216,
38.2431887587551));
#178336=CARTESIAN_POINT('Ctrl Pts',(6.68596845706459,-4.61813526113775,
38.2266177051951));
#178337=CARTESIAN_POINT('Ctrl Pts',(6.629618049335,-4.69867128156877,38.222801620362));
#178338=CARTESIAN_POINT('Ctrl Pts',(6.5439579866085,-4.81648693133922,38.2171240403336));
#178339=CARTESIAN_POINT('Ctrl Pts',(6.51576054539933,-4.85456455103081,
38.2152739764911));
#178340=CARTESIAN_POINT('Ctrl Pts',(6.46461056187599,-4.92238857501888,
38.2119506819065));
#178341=CARTESIAN_POINT('Ctrl Pts',(6.44178165851802,-4.95222657511283,
38.2104787902989));
#178342=CARTESIAN_POINT('Ctrl Pts',(6.39261892962319,-5.01556842865307,
38.2073326169962));
#178343=CARTESIAN_POINT('Ctrl Pts',(6.36622681929078,-5.04902559985828,
38.2056577436812));
#178344=CARTESIAN_POINT('Ctrl Pts',(6.29347563904454,-5.13977463228924,
38.201078300959));
#178345=CARTESIAN_POINT('Ctrl Pts',(6.24659849945455,-5.1966456466147,38.1981681408436));
#178346=CARTESIAN_POINT('Ctrl Pts',(5.92853419942872,-5.57199584455395,
38.1786822707243));
#178347=CARTESIAN_POINT('Ctrl Pts',(5.63388052916184,-5.86975559237063,
38.1618398356592));
#178348=CARTESIAN_POINT('Ctrl Pts',(4.98793605025122,-6.42886540178347,
38.1271601353612));
#178349=CARTESIAN_POINT('Ctrl Pts',(4.635808550968,-6.6872343296369,38.1093687099196));
#178350=CARTESIAN_POINT('Ctrl Pts',(4.2027030661909,-6.95429876935298,38.08906144608));
#178351=CARTESIAN_POINT('Ctrl Pts',(4.14024314918993,-6.99166441277781,
38.0861691646487));
#178352=CARTESIAN_POINT('Ctrl Pts',(4.05608685828283,-7.04048633233219,
38.0823231776387));
#178353=CARTESIAN_POINT('Ctrl Pts',(4.03482888471358,-7.05269056997144,
38.0813559692687));
#178354=CARTESIAN_POINT('Ctrl Pts',(3.99862959878405,-7.07325540452159,
38.0797163663507));
#178355=CARTESIAN_POINT('Ctrl Pts',(3.9837165839922,-7.08166526080852,38.0790430386715));
#178356=CARTESIAN_POINT('Ctrl Pts',(3.9518331056948,-7.09951263980306,38.0776079672001));
#178357=CARTESIAN_POINT('Ctrl Pts',(3.93485520347087,-7.10893656949247,
38.0768464742973));
#178358=CARTESIAN_POINT('Ctrl Pts',(3.89265383398506,-7.13216379752461,
38.074960018663));
#178359=CARTESIAN_POINT('Ctrl Pts',(3.86739053135358,-7.14589426130388,
38.0738363263668));
#178360=CARTESIAN_POINT('Ctrl Pts',(3.76718489166121,-7.19966841833148,
38.0693999879081));
#178361=CARTESIAN_POINT('Ctrl Pts',(3.69168882356309,-7.23866984759135,
38.0661031788969));
#178362=CARTESIAN_POINT('Ctrl Pts',(3.53881857215696,-7.31462921584078,
38.0595012597281));
#178363=CARTESIAN_POINT('Ctrl Pts',(3.46144338978405,-7.35156086953082,
38.0561967567631));
#178364=CARTESIAN_POINT('Ctrl Pts',(3.12042697096105,-7.50775250016901,
38.0417594496031));
#178365=CARTESIAN_POINT('Ctrl Pts',(2.85110864840801,-7.61410474270099,
38.0306748309688));
#178366=CARTESIAN_POINT('Ctrl Pts',(2.49958217425814,-7.73164842399371,
38.0163262144808));
#178367=CARTESIAN_POINT('Ctrl Pts',(2.4220894585606,-7.75627365082814,38.0131711528636));
#178368=CARTESIAN_POINT('Ctrl Pts',(2.30355733940408,-7.7919905384352,38.0083529839391));
#178369=CARTESIAN_POINT('Ctrl Pts',(2.26277870120508,-7.80393013163419,
38.0066967918507));
#178370=CARTESIAN_POINT('Ctrl Pts',(2.18822927863056,-7.82512403381542,
38.0036710009939));
#178371=CARTESIAN_POINT('Ctrl Pts',(2.15448870355277,-7.83448096155193,
38.0023022828169));
#178372=CARTESIAN_POINT('Ctrl Pts',(2.0805848968681,-7.85446242204418,37.9993055923255));
#178373=CARTESIAN_POINT('Ctrl Pts',(2.0403985538727,-7.86499759549781,37.9976769210452));
#178374=CARTESIAN_POINT('Ctrl Pts',(1.92401868187338,-7.89455551698002,
37.9929621209266));
#178375=CARTESIAN_POINT('Ctrl Pts',(1.84762818350918,-7.91278236053515,
37.9898696026554));
#178376=CARTESIAN_POINT('Ctrl Pts',(1.71673107361407,-7.94201563689225,
37.9845731132626));
#178377=CARTESIAN_POINT('Ctrl Pts',(1.66235356184399,-7.95357520588922,
37.9823736185903));
#178378=CARTESIAN_POINT('Ctrl Pts',(1.43070741043288,-8.00033915452698,
37.9730071196873));
#178379=CARTESIAN_POINT('Ctrl Pts',(1.25241025727234,-8.03018169061828,
37.9658042810544));
#178380=CARTESIAN_POINT('Ctrl Pts',(0.806402868076624,-8.0896157855723,
37.9478358823616));
#178381=CARTESIAN_POINT('Ctrl Pts',(0.537933932950174,-8.11189237201577,
37.9370595542143));
#178382=CARTESIAN_POINT('Ctrl Pts',(0.229100257388967,-8.12211688850682,
37.924854738887));
#178383=CARTESIAN_POINT('Ctrl Pts',(0.189336934210476,-8.12314109366498,
37.9232871390134));
#178384=CARTESIAN_POINT('Ctrl Pts',(0.128256249534165,-8.12426564204894,
37.9208858886481));
#178385=CARTESIAN_POINT('Ctrl Pts',(0.106943524038269,-8.12457414109394,
37.9200493183069));
#178386=CARTESIAN_POINT('Ctrl Pts',(0.0655187816009979,-8.12501072899457,
37.9184257591139));
#178387=CARTESIAN_POINT('Ctrl Pts',(0.0454070909787996,-8.12514801442794,
37.917638624657));
#178388=CARTESIAN_POINT('Ctrl Pts',(-0.00238489442532232,-8.12529679839415,
37.915770527126));
#178389=CARTESIAN_POINT('Ctrl Pts',(-0.0300651776680895,-8.12524152518288,
37.9146904645797));
#178390=CARTESIAN_POINT('Ctrl Pts',(-0.124701342575879,-8.12456894581731,
37.9110035177865));
#178391=CARTESIAN_POINT('Ctrl Pts',(-0.19164988562061,-8.12326543896288,
37.9084049675273));
#178392=CARTESIAN_POINT('Ctrl Pts',(-0.687696142308071,-8.1074714453238,
37.8891985523274));
#178393=CARTESIAN_POINT('Ctrl Pts',(-1.11506257674444,-8.0598176923586,
37.8728801079191));
#178394=CARTESIAN_POINT('Ctrl Pts',(-1.73677604599634,-7.94007733791922,
37.8485063210257));
#178395=CARTESIAN_POINT('Ctrl Pts',(-1.93536873457752,-7.89402088552531,
37.8406283630125));
#178396=CARTESIAN_POINT('Ctrl Pts',(-2.19815186944007,-7.82256435002126,
37.8300330313126));
#178397=CARTESIAN_POINT('Ctrl Pts',(-2.26405537785717,-7.80374511643277,
37.8273614133427));
#178398=CARTESIAN_POINT('Ctrl Pts',(-2.37809651167119,-7.76961358315815,
37.8227120533384));
#178399=CARTESIAN_POINT('Ctrl Pts',(-2.42634414940916,-7.75468195982484,
37.8207367841108));
#178400=CARTESIAN_POINT('Ctrl Pts',(-2.52929458623334,-7.72176611601376,
37.8165039011953));
#178401=CARTESIAN_POINT('Ctrl Pts',(-2.58395176566452,-7.70364824604006,
37.8142456209746));
#178402=CARTESIAN_POINT('Ctrl Pts',(-2.72960265991232,-7.65364311095802,
37.8081979401269));
#178403=CARTESIAN_POINT('Ctrl Pts',(-2.82022894836474,-7.6207146728734,
37.8044035581415));
#178404=CARTESIAN_POINT('Ctrl Pts',(-3.04507782880851,-7.53445706123394,
37.7949119447178));
#178405=CARTESIAN_POINT('Ctrl Pts',(-3.1785050998285,-7.479147504975,37.7892091446805));
#178406=CARTESIAN_POINT('Ctrl Pts',(-3.42461792422765,-7.36935040389043,
37.7785706455184));
#178407=CARTESIAN_POINT('Ctrl Pts',(-3.53765710650911,-7.31575803791595,
37.773635939523));
#178408=CARTESIAN_POINT('Ctrl Pts',(-3.69004523030179,-7.23915201102149,
37.7669279919342));
#178409=CARTESIAN_POINT('Ctrl Pts',(-3.7305041767151,-7.21838584766392,
37.7651416289053));
#178410=CARTESIAN_POINT('Ctrl Pts',(-3.80914010237132,-7.17718705299606,
37.7616600405768));
#178411=CARTESIAN_POINT('Ctrl Pts',(-3.84733230485705,-7.15678674141199,
37.7599646592506));
#178412=CARTESIAN_POINT('Ctrl Pts',(-3.98262712480989,-7.08312320570872,
37.753940008585));
#178413=CARTESIAN_POINT('Ctrl Pts',(-4.07880194526745,-7.02818098858735,
37.7496224809905));
#178414=CARTESIAN_POINT('Ctrl Pts',(-4.38345385296372,-6.8457809721673,
37.73579129896));
#178415=CARTESIAN_POINT('Ctrl Pts',(-4.58731545109521,-6.71088081352194,
37.7262952494593));
#178416=CARTESIAN_POINT('Ctrl Pts',(-4.83447285745584,-6.53079925521143,
37.7143402980482));
#178417=CARTESIAN_POINT('Ctrl Pts',(-4.88374560459725,-6.49403538330858,
37.7119341361101));
#178418=CARTESIAN_POINT('Ctrl Pts',(-4.97649313243812,-6.42318108006872,
37.7073589339506));
#178419=CARTESIAN_POINT('Ctrl Pts',(-5.02004674185723,-6.38919946223021,
37.7051907140946));
#178420=CARTESIAN_POINT('Ctrl Pts',(-5.12248485360041,-6.30758057132354,
37.7000421754501));
#178421=CARTESIAN_POINT('Ctrl Pts',(-5.18105638535243,-6.25955896199597,
37.6970592819009));
#178422=CARTESIAN_POINT('Ctrl Pts',(-5.4086378096875,-6.06758667695662,
37.6853080290312));
#178423=CARTESIAN_POINT('Ctrl Pts',(-5.57238863410537,-5.91755475100201,
37.6764937704057));
#178424=CARTESIAN_POINT('Ctrl Pts',(-5.87594308056476,-5.61564527162143,
37.6594122447874));
#178425=CARTESIAN_POINT('Ctrl Pts',(-6.0165124841956,-5.46477409508698,
37.6511574605115));
#178426=CARTESIAN_POINT('Ctrl Pts',(-6.30171123252783,-5.13431560608808,
37.6336860043781));
#178427=CARTESIAN_POINT('Ctrl Pts',(-6.444746455658,-4.95358517693716,37.6244778103));
#178428=CARTESIAN_POINT('Ctrl Pts',(-6.60909871605692,-4.72673005949495,
37.6133986925933));
#178429=CARTESIAN_POINT('Ctrl Pts',(-6.63791768817087,-4.6861723934592,
37.6114358750152));
#178430=CARTESIAN_POINT('Ctrl Pts',(-6.6806488929502,-4.62485052324696,
37.6084961248085));
#178431=CARTESIAN_POINT('Ctrl Pts',(-6.69484071648923,-4.60428276502318,
37.6075147802132));
#178432=CARTESIAN_POINT('Ctrl Pts',(-6.72006386873803,-4.56736446673624,
37.6057618232111));
#178433=CARTESIAN_POINT('Ctrl Pts',(-6.73113096112512,-4.55103862424891,
37.6049895946091));
#178434=CARTESIAN_POINT('Ctrl Pts',(-6.75497548820163,-4.51558664827104,
37.6033191874099));
#178435=CARTESIAN_POINT('Ctrl Pts',(-6.76773130968638,-4.49644632427089,
37.6024214589137));
#178436=CARTESIAN_POINT('Ctrl Pts',(-6.80811223630881,-4.43529294964012,
37.5995659454713));
#178437=CARTESIAN_POINT('Ctrl Pts',(-6.83542876999993,-4.39307743500752,
37.5976136567261));
#178438=CARTESIAN_POINT('Ctrl Pts',(-6.90115011089745,-4.28941315114365,
37.5928611064934));
#178439=CARTESIAN_POINT('Ctrl Pts',(-6.93912824112716,-4.22769882934905,
37.5900668407345));
#178440=CARTESIAN_POINT('Ctrl Pts',(-7.1046934159661,-3.95041335404007,
37.5776442808977));
#178441=CARTESIAN_POINT('Ctrl Pts',(-7.22309701559356,-3.72951804601877,
37.5680944432444));
#178442=CARTESIAN_POINT('Ctrl Pts',(-7.41925984880203,-3.31904611005962,
37.550655796394));
#178443=CARTESIAN_POINT('Ctrl Pts',(-7.50041820856906,-3.1313270518481,
37.5427918180161));
#178444=CARTESIAN_POINT('Ctrl Pts',(-7.59524941694852,-2.88707278317949,
37.5326279248495));
#178445=CARTESIAN_POINT('Ctrl Pts',(-7.61551777827767,-2.83317699507591,
37.5303895952474));
#178446=CARTESIAN_POINT('Ctrl Pts',(-7.64670015806661,-2.74750660141824,
37.5268373426887));
#178447=CARTESIAN_POINT('Ctrl Pts',(-7.65799295421377,-2.71587181883277,
37.5255268564697));
#178448=CARTESIAN_POINT('Ctrl Pts',(-7.68082991192148,-2.65062304618199,
37.5228261671469));
#178449=CARTESIAN_POINT('Ctrl Pts',(-7.692350339879,-2.61700151061444,37.5214357831341));
#178450=CARTESIAN_POINT('Ctrl Pts',(-7.71887350205123,-2.53790705239747,
37.5181675486405));
#178451=CARTESIAN_POINT('Ctrl Pts',(-7.73369556827182,-2.49237500759929,
37.5162881645062));
#178452=CARTESIAN_POINT('Ctrl Pts',(-7.78362248806716,-2.33426933516128,
37.5097685944556));
#178453=CARTESIAN_POINT('Ctrl Pts',(-7.81667845274167,-2.22106505550809,
37.5051114846297));
#178454=CARTESIAN_POINT('Ctrl Pts',(-7.87422443180798,-2.00676076768006,
37.4963159468717));
#178455=CARTESIAN_POINT('Ctrl Pts',(-7.89925983462117,-1.90583133551186,
37.4921821412222));
#178456=CARTESIAN_POINT('Ctrl Pts',(-7.95395165523837,-1.66570947667068,
37.482373756228));
#178457=CARTESIAN_POINT('Ctrl Pts',(-7.98190207549247,-1.52616321537475,
37.476694091203));
#178458=CARTESIAN_POINT('Ctrl Pts',(-8.03202753252847,-1.23660619738642,
37.4649792258475));
#178459=CARTESIAN_POINT('Ctrl Pts',(-8.05369761241732,-1.08656179414735,
37.4589471566957));
#178460=CARTESIAN_POINT('Ctrl Pts',(-8.07505458824178,-0.902399591329861,
37.4516226785151));
#178461=CARTESIAN_POINT('Ctrl Pts',(-8.07874116122626,-0.868776662209606,
37.4502886834988));
#178462=CARTESIAN_POINT('Ctrl Pts',(-8.08411540477477,-0.81676592974232,
37.4482307325988));
#178463=CARTESIAN_POINT('Ctrl Pts',(-8.08595051860162,-0.798393809419776,
37.4475048638575));
#178464=CARTESIAN_POINT('Ctrl Pts',(-8.08932561298056,-0.763398573696936,
37.4461243938638));
#178465=CARTESIAN_POINT('Ctrl Pts',(-8.09087701609042,-0.746776651994654,
37.4454696323381));
#178466=CARTESIAN_POINT('Ctrl Pts',(-8.09454642366884,-0.706107982780919,
37.4438700224355));
#178467=CARTESIAN_POINT('Ctrl Pts',(-8.0966085163781,-0.682056322335849,
37.442926040087));
#178468=CARTESIAN_POINT('Ctrl Pts',(-8.10326462236594,-0.600133460629295,
37.4397171739875));
#178469=CARTESIAN_POINT('Ctrl Pts',(-8.10734561813163,-0.542222107185787,
37.4374597754607));
#178470=CARTESIAN_POINT('Ctrl Pts',(-8.11582498784977,-0.400205711281178,
37.4319460653837));
#178471=CARTESIAN_POINT('Ctrl Pts',(-8.11953706568488,-0.316066234122284,
37.4286983690644));
#178472=CARTESIAN_POINT('Ctrl Pts',(-8.13341522268754,0.170028859495288,
37.4100122569928));
#178473=CARTESIAN_POINT('Ctrl Pts',(-8.11504142195906,0.572242905391769,
37.3948386913516));
#178474=CARTESIAN_POINT('Ctrl Pts',(-8.02040776561461,1.35809115875314,
37.3647320158234));
#178475=CARTESIAN_POINT('Ctrl Pts',(-7.94610990120337,1.74088513977439,
37.3498428923332));
#178476=CARTESIAN_POINT('Ctrl Pts',(-7.82579951276028,2.18672945908209,
37.3319055269939));
#178477=CARTESIAN_POINT('Ctrl Pts',(-7.80601487142752,2.25633674140283,
37.3290880041147));
#178478=CARTESIAN_POINT('Ctrl Pts',(-7.77322970878715,2.36608679634183,
37.3246170148992));
#178479=CARTESIAN_POINT('Ctrl Pts',(-7.76084171098822,2.40640868416693,
37.3229682280847));
#178480=CARTESIAN_POINT('Ctrl Pts',(-7.73707727742894,2.48166730563065,
37.3198790379777));
#178481=CARTESIAN_POINT('Ctrl Pts',(-7.72577674844785,2.51662691635659,
37.318439224322));
#178482=CARTESIAN_POINT('Ctrl Pts',(-7.69980642164302,2.5951456876696,37.3151944131068));
#178483=CARTESIAN_POINT('Ctrl Pts',(-7.68500335385168,2.63865941416542,
37.3133885219715));
#178484=CARTESIAN_POINT('Ctrl Pts',(-7.63989872617744,2.76764490848981,
37.3080121925767));
#178485=CARTESIAN_POINT('Ctrl Pts',(-7.60853473568339,2.85273727055215,
37.3044348722191));
#178486=CARTESIAN_POINT('Ctrl Pts',(-7.44440862655155,3.27604596334917,
37.2864829278164));
#178487=CARTESIAN_POINT('Ctrl Pts',(-7.29049172156961,3.60560945604558,
37.2720616140364));
#178488=CARTESIAN_POINT('Ctrl Pts',(-6.98398079870945,4.16141277402086,
37.2463444282087));
#178489=CARTESIAN_POINT('Ctrl Pts',(-6.84109986260679,4.39234441302397,
37.2351863685049));
#178490=CARTESIAN_POINT('Ctrl Pts',(-6.43369110442789,4.98257404325643,
37.2052698070201));
#178491=CARTESIAN_POINT('Ctrl Pts',(-6.15069180496686,5.32798251608046,
37.1862400322237));
#178492=CARTESIAN_POINT('Ctrl Pts',(-5.71326178205887,5.78031016722106,
37.1598078433099));
#178493=CARTESIAN_POINT('Ctrl Pts',(-5.58129108446918,5.90783707758814,
37.1521707301604));
#178494=CARTESIAN_POINT('Ctrl Pts',(-5.37732554496077,6.09199465435793,
37.1409756237096));
#178495=CARTESIAN_POINT('Ctrl Pts',(-5.30850856854674,6.15205383290401,
37.1372963428697));
#178496=CARTESIAN_POINT('Ctrl Pts',(-5.22675544019093,6.22100948333098,
37.1330522728761));
#178497=CARTESIAN_POINT('Ctrl Pts',(-5.21478948634788,6.23104341506426,
37.132434205476));
#178498=CARTESIAN_POINT('Ctrl Pts',(-5.19557971513977,6.24705748470578,
37.1314470711861));
#178499=CARTESIAN_POINT('Ctrl Pts',(-5.18835435632236,6.25305964050697,
37.1310769285995));
#178500=CARTESIAN_POINT('Ctrl Pts',(-5.17553471412573,6.26367148962491,
37.1304222554507));
#178501=CARTESIAN_POINT('Ctrl Pts',(-5.16994464690103,6.26828624549559,
37.13013747176));
#178502=CARTESIAN_POINT('Ctrl Pts',(-5.15832444728088,6.27785292458736,
37.1295469293536));
#178503=CARTESIAN_POINT('Ctrl Pts',(-5.15229333989172,6.28280365652295,
37.1292412313205));
#178504=CARTESIAN_POINT('Ctrl Pts',(-5.13672792651202,6.29554329195237,
37.1284543621582));
#178505=CARTESIAN_POINT('Ctrl Pts',(-5.12718301125246,6.30331924490339,
37.1279738626732));
#178506=CARTESIAN_POINT('Ctrl Pts',(-5.08728165438416,6.33567507135007,
37.1259737356764));
#178507=CARTESIAN_POINT('Ctrl Pts',(-5.05676550222269,6.36005785902611,
37.1244646255642));
#178508=CARTESIAN_POINT('Ctrl Pts',(-4.843991490142,6.5275674400667,37.1140913687883));
#178509=CARTESIAN_POINT('Ctrl Pts',(-4.65585324261567,6.66306446823743,
37.1056859838987));
#178510=CARTESIAN_POINT('Ctrl Pts',(-3.99321458678843,7.09850809267342,
37.077854293084));
#178511=CARTESIAN_POINT('Ctrl Pts',(-3.49357627801123,7.35727921880065,
37.0597437380901));
#178512=CARTESIAN_POINT('Ctrl Pts',(-2.47487979833628,7.75751686430239,
37.0227001854279));
#178513=CARTESIAN_POINT('Ctrl Pts',(-1.96057718935779,7.90317386145941,
37.0039182551235));
#178514=CARTESIAN_POINT('Ctrl Pts',(-1.40362232001673,8.00316166898179,
36.9821668922066));
#178515=CARTESIAN_POINT('Ctrl Pts',(-1.37147098397941,8.00873395911033,
36.980906780968));
#178516=CARTESIAN_POINT('Ctrl Pts',(-1.32678424706177,8.01620183211323,
36.9791489961083));
#178517=CARTESIAN_POINT('Ctrl Pts',(-1.31427648243856,8.01826200478602,
36.9786563025079));
#178518=CARTESIAN_POINT('Ctrl Pts',(-1.29273869721206,8.02175777650204,
36.9778067059103));
#178519=CARTESIAN_POINT('Ctrl Pts',(-1.28371096440708,8.02320742118287,
36.9774502278366));
#178520=CARTESIAN_POINT('Ctrl Pts',(-1.2650854019114,8.02616601395783,36.9767140071667));
#178521=CARTESIAN_POINT('Ctrl Pts',(-1.25548727579643,8.02767299142703,
36.976334205721));
#178522=CARTESIAN_POINT('Ctrl Pts',(-1.23316018731623,8.03113748937763,
36.9754497502369));
#178523=CARTESIAN_POINT('Ctrl Pts',(-1.22042924411967,8.03308196641377,
36.9749447038983));
#178524=CARTESIAN_POINT('Ctrl Pts',(-1.1799263826769,8.03916971708846,36.9733355908616));
#178525=CARTESIAN_POINT('Ctrl Pts',(-1.15213772341481,8.04319927987422,
36.9722281053273));
#178526=CARTESIAN_POINT('Ctrl Pts',(-0.850959933323492,8.08527947499498,
36.960186727106));
#178527=CARTESIAN_POINT('Ctrl Pts',(-0.575841607544147,8.10951696116799,
36.9488375274159));
#178528=CARTESIAN_POINT('Ctrl Pts',(0.108004096137983,8.13478632827817,
36.9197876448925));
#178529=CARTESIAN_POINT('Ctrl Pts',(0.516575916144777,8.11908378719154,
36.9016721629172));
#178530=CARTESIAN_POINT('Ctrl Pts',(1.53296812704108,8.00297396181324,36.8557705926273));
#178531=CARTESIAN_POINT('Ctrl Pts',(2.13392119096461,7.8641062988252,36.8278357264556));
#178532=CARTESIAN_POINT('Ctrl Pts',(2.74694008390008,7.64691212990139,36.8016568879921));
#178533=CARTESIAN_POINT('Ctrl Pts',(2.78028635316732,7.63485119681187,36.8002398167166));
#178534=CARTESIAN_POINT('Ctrl Pts',(2.82541572252063,7.61819358214124,36.7983303093581));
#178535=CARTESIAN_POINT('Ctrl Pts',(2.83726828853964,7.61378723903433,36.7978295847397));
#178536=CARTESIAN_POINT('Ctrl Pts',(2.85594416764985,7.60679457581252,36.7970417699991));
#178537=CARTESIAN_POINT('Ctrl Pts',(2.86277433597345,7.60422671342119,36.7967538961836));
#178538=CARTESIAN_POINT('Ctrl Pts',(2.8759408279522,7.59925640026952,36.7961994246806));
#178539=CARTESIAN_POINT('Ctrl Pts',(2.88227762066764,7.59685521782957,36.7959327742801));
#178540=CARTESIAN_POINT('Ctrl Pts',(2.89725171354938,7.59115969573271,36.7953031433129));
#178541=CARTESIAN_POINT('Ctrl Pts',(2.90588642051966,7.58785853384698,36.7949404446646));
#178542=CARTESIAN_POINT('Ctrl Pts',(2.93114843639161,7.5781510880231,36.7938803703278));
#178543=CARTESIAN_POINT('Ctrl Pts',(2.9477603858686,7.57170481348814,36.7931846138128));
#178544=CARTESIAN_POINT('Ctrl Pts',(3.07158038497103,7.52318715932068,36.7880078309173));
#178545=CARTESIAN_POINT('Ctrl Pts',(3.17790712970326,7.47889421805786,36.783613597906));
#178546=CARTESIAN_POINT('Ctrl Pts',(3.53446288756006,7.32138494224311,36.7689569950812));
#178547=CARTESIAN_POINT('Ctrl Pts',(3.77988831775344,7.19774683603318,36.7589969941373));
#178548=CARTESIAN_POINT('Ctrl Pts',(4.33586462258877,6.88136813430985,36.7359634571538));
#178549=CARTESIAN_POINT('Ctrl Pts',(4.64061076973154,6.67964670464074,36.7229576760477));
#178550=CARTESIAN_POINT('Ctrl Pts',(5.00087770235044,6.40458369834443,36.7064221848967));
#178551=CARTESIAN_POINT('Ctrl Pts',(5.07011888369741,6.34991058396381,36.7031882560278));
#178552=CARTESIAN_POINT('Ctrl Pts',(5.37332611482754,6.10237533113688,36.6887542385641));
#178553=CARTESIAN_POINT('Ctrl Pts',(5.59727087153957,5.89764070327418,36.6773458144166));
#178554=CARTESIAN_POINT('Ctrl Pts',(5.84451849769205,5.64480614569987,36.6637264080394));
#178555=CARTESIAN_POINT('Ctrl Pts',(5.87945526296628,5.60840785351286,36.6617766270597));
#178556=CARTESIAN_POINT('Ctrl Pts',(5.93226733494533,5.55235063404496,36.6587902128289));
#178557=CARTESIAN_POINT('Ctrl Pts',(5.95038908197754,5.53292536208915,36.6577583077418));
#178558=CARTESIAN_POINT('Ctrl Pts',(5.98295131327453,5.49767587784272,36.6558911460154));
#178559=CARTESIAN_POINT('Ctrl Pts',(5.99742512976749,5.48188273161136,36.6550565069261));
#178560=CARTESIAN_POINT('Ctrl Pts',(6.0255434587052,5.45095668299506,36.6534258568991));
#178561=CARTESIAN_POINT('Ctrl Pts',(6.03919386736983,5.43582929843389,36.6526299448002));
#178562=CARTESIAN_POINT('Ctrl Pts',(6.07494585337241,5.39590804671453,36.6505338727248));
#178563=CARTESIAN_POINT('Ctrl Pts',(6.09695250358661,5.37102978248296,36.6492320085259));
#178564=CARTESIAN_POINT('Ctrl Pts',(6.17728191408485,5.27908842896727,36.6444359053918));
#178565=CARTESIAN_POINT('Ctrl Pts',(6.2346552404826,5.21120525557357,36.6409240257727));
#178566=CARTESIAN_POINT('Ctrl Pts',(6.56839075168565,4.80293292186313,36.6199515541404));
#178567=CARTESIAN_POINT('Ctrl Pts',(6.81793057208248,4.44158822725121,36.601937187932));
#178568=CARTESIAN_POINT('Ctrl Pts',(7.34050343706632,3.53624976299989,36.5579718189738));
#178569=CARTESIAN_POINT('Ctrl Pts',(7.58405867599734,2.9782708836275,36.5316849932689));
#178570=CARTESIAN_POINT('Ctrl Pts',(7.77870714222655,2.34822476958046,36.5050808676723));
#178571=CARTESIAN_POINT('Ctrl Pts',(7.79371911470639,2.29790923968159,36.5029780492243));
#178572=CARTESIAN_POINT('Ctrl Pts',(7.81227328950041,2.23344710535848,36.5003144284647));
#178573=CARTESIAN_POINT('Ctrl Pts',(7.81626640876989,2.2194322140264,36.4997371528914));
#178574=CARTESIAN_POINT('Ctrl Pts',(7.82256266058574,2.19710613331562,36.498820521354));
#178575=CARTESIAN_POINT('Ctrl Pts',(7.82489029215667,2.18880192257014,36.4984802351187));
#178576=CARTESIAN_POINT('Ctrl Pts',(7.8292150485915,2.17327757172662,36.4978453282286));
#178577=CARTESIAN_POINT('Ctrl Pts',(7.83121541708501,2.16605834929088,36.4975505818709));
#178578=CARTESIAN_POINT('Ctrl Pts',(7.83564627788241,2.14998124163357,36.4968953163169));
#178579=CARTESIAN_POINT('Ctrl Pts',(7.83807174189637,2.14112197252275,36.496534996252));
#178580=CARTESIAN_POINT('Ctrl Pts',(7.84508416622161,2.1153367378781,36.4954885245381));
#178581=CARTESIAN_POINT('Ctrl Pts',(7.84963137678619,2.09839994864755,36.4948039813032));
#178582=CARTESIAN_POINT('Ctrl Pts',(7.88364621727185,1.97004857797567,36.4896383087437));
#178583=CARTESIAN_POINT('Ctrl Pts',(7.91079350474151,1.85804100352943,36.4852629932323));
#178584=CARTESIAN_POINT('Ctrl Pts',(7.95695899968721,1.64815694583263,36.4772948993053));
#178585=CARTESIAN_POINT('Ctrl Pts',(7.97657444123336,1.55044476404425,36.4736732144773));
#178586=CARTESIAN_POINT('Ctrl Pts',(8.08115054270371,0.974828388749765,
36.4527439956508));
#178587=CARTESIAN_POINT('Ctrl Pts',(8.12494782763725,0.490438023465154,
36.4367273681874));
#178588=CARTESIAN_POINT('Ctrl Pts',(8.12524844182851,0.00503200391154854,
36.4203543227145));
#178589=CARTESIAN_POINT('',(8.120871211716,-0.00172117854340554,34.4167025567877));
#178590=CARTESIAN_POINT('Ctrl Pts',(8.120871211716,-0.00172117854340554,
34.4167025567877));
#178591=CARTESIAN_POINT('Ctrl Pts',(8.12076539718447,0.119070448189721,
34.4214150269101));
#178592=CARTESIAN_POINT('Ctrl Pts',(8.08738294886854,1.59563522457119,34.479016652128));
#178593=CARTESIAN_POINT('Ctrl Pts',(6.87712117603644,5.73415005919172,34.6423965875369));
#178594=CARTESIAN_POINT('Ctrl Pts',(1.64131973131669,8.81124817329271,34.8539532079189));
#178595=CARTESIAN_POINT('Ctrl Pts',(-3.82482145636865,7.54243940143105,
35.0655098283007));
#178596=CARTESIAN_POINT('Ctrl Pts',(-6.96195299981451,4.82582851322905,
35.2241772935872));
#178597=CARTESIAN_POINT('Ctrl Pts',(-8.42537801125605,0.894369939753666,
35.3828447588736));
#178598=CARTESIAN_POINT('Ctrl Pts',(-7.82264342903586,-3.23476629007719,
35.54151222416));
#178599=CARTESIAN_POINT('Ctrl Pts',(-5.33310408397497,-6.58368385109594,
35.7001796894465));
#178600=CARTESIAN_POINT('Ctrl Pts',(-1.52043507705952,-8.3334079215629,
35.8588471547329));
#178601=CARTESIAN_POINT('Ctrl Pts',(2.61913853473312,-8.04100520042323,
36.0175146200193));
#178602=CARTESIAN_POINT('Ctrl Pts',(6.80819671928331,-5.43726497504425,
36.2034664207042));
#178603=CARTESIAN_POINT('Ctrl Pts',(8.10078544928885,-2.03703630869931,
36.3365290662937));
#178604=CARTESIAN_POINT('Ctrl Pts',(8.11892105081991,0.00515126165398824,
36.4167025567876));
#178605=CARTESIAN_POINT('',(8.12588319212562,-0.00333877610576572,32.4167025567876));
#178606=CARTESIAN_POINT('Ctrl Pts',(8.12524931413266,-0.00333851565694556,
32.4167025567876));
#178607=CARTESIAN_POINT('Ctrl Pts',(8.12533264120618,0.199462164817699,
32.4246762945215));
#178608=CARTESIAN_POINT('Ctrl Pts',(8.11781906538481,0.402445848508343,
32.4326500322554));
#178609=CARTESIAN_POINT('Ctrl Pts',(8.10269393801063,0.605011164711699,
32.4406237699892));
#178610=CARTESIAN_POINT('Ctrl Pts',(8.08758128338672,0.807409437918437,
32.4485909322784));
#178611=CARTESIAN_POINT('Ctrl Pts',(8.06486961318257,1.00938970431921,32.4565580945675));
#178612=CARTESIAN_POINT('Ctrl Pts',(8.03459632854458,1.21035094077627,32.4645252568566));
#178613=CARTESIAN_POINT('Ctrl Pts',(8.00434310015103,1.41117903913057,32.4724871408498));
#178614=CARTESIAN_POINT('Ctrl Pts',(7.96653829317832,1.61098912868181,32.4804490248431));
#178615=CARTESIAN_POINT('Ctrl Pts',(7.92127114606062,1.80918517379715,32.4884109088363));
#178616=CARTESIAN_POINT('Ctrl Pts',(7.87458221998924,2.01360628462991,32.4966228646766));
#178617=CARTESIAN_POINT('Ctrl Pts',(7.8199545913438,2.21630995564091,32.5048348205169));
#178618=CARTESIAN_POINT('Ctrl Pts',(7.75754347982598,2.4166519652423,32.5130467763573));
#178619=CARTESIAN_POINT('Ctrl Pts',(7.69708101937612,2.61073873180324,32.5210023317566));
#178620=CARTESIAN_POINT('Ctrl Pts',(7.62931389273452,2.80260874993346,32.5289578871559));
#178621=CARTESIAN_POINT('Ctrl Pts',(7.55443431239011,2.99169012136667,32.5369134425552));
#178622=CARTESIAN_POINT('Ctrl Pts',(7.47956462708131,3.18074650645654,32.5448679466598));
#178623=CARTESIAN_POINT('Ctrl Pts',(7.39758448288845,3.3670146732867,32.5528224507644));
#178624=CARTESIAN_POINT('Ctrl Pts',(7.30873478426675,3.54994132567698,32.5607769548691));
#178625=CARTESIAN_POINT('Ctrl Pts',(7.21988377005464,3.73287068664765,32.5687315767554));
#178626=CARTESIAN_POINT('Ctrl Pts',(7.12416314297998,3.91245813848594,32.5766861986417));
#178627=CARTESIAN_POINT('Ctrl Pts',(7.02186064015138,4.08817327333284,32.5846408205281));
#178628=CARTESIAN_POINT('Ctrl Pts',(6.91954158903092,4.2639168315834,32.5925967291415));
#178629=CARTESIAN_POINT('Ctrl Pts',(6.81063870605211,4.43578653992892,32.600552637755));
#178630=CARTESIAN_POINT('Ctrl Pts',(6.69548431629431,4.60327897620347,32.6085085463684));
#178631=CARTESIAN_POINT('Ctrl Pts',(6.58025746384561,4.77087680969878,32.6164694613611));
#178632=CARTESIAN_POINT('Ctrl Pts',(6.4587714325685,4.9340915968601,32.6244303763538));
#178633=CARTESIAN_POINT('Ctrl Pts',(6.33140089099655,5.09245032572612,32.6323912913465));
#178634=CARTESIAN_POINT('Ctrl Pts',(6.20398294524252,5.25086799181519,32.6403551691959));
#178635=CARTESIAN_POINT('Ctrl Pts',(6.07067633399234,5.40442574385364,32.6483190470453));
#178636=CARTESIAN_POINT('Ctrl Pts',(5.93189469190031,5.55268519967636,32.6562829248947));
#178637=CARTESIAN_POINT('Ctrl Pts',(5.79299791080893,5.70106765768533,32.6642534099071));
#178638=CARTESIAN_POINT('Ctrl Pts',(5.64861725715567,5.84414280526376,32.6722238949195));
#178639=CARTESIAN_POINT('Ctrl Pts',(5.49920245619378,5.98150983517475,32.6801943799319));
#178640=CARTESIAN_POINT('Ctrl Pts',(5.4660628260617,6.01197731586801,32.681962202956));
#178641=CARTESIAN_POINT('Ctrl Pts',(5.43267567652258,6.04216415184208,32.6837300259801));
#178642=CARTESIAN_POINT('Ctrl Pts',(5.39904612847492,6.072066243471,32.6854978490042));
#178643=CARTESIAN_POINT('Ctrl Pts',(5.25488410256312,6.2002495334193,32.6930760938337));
#178644=CARTESIAN_POINT('Ctrl Pts',(5.10595192852175,6.32347549322777,32.7006543386631));
#178645=CARTESIAN_POINT('Ctrl Pts',(4.95264020853747,6.44135409112695,32.7082325834926));
#178646=CARTESIAN_POINT('Ctrl Pts',(4.79944257183473,6.5591449724623,32.7158051891509));
#178647=CARTESIAN_POINT('Ctrl Pts',(4.64187216176423,6.67159618525623,32.7233777948091));
#178648=CARTESIAN_POINT('Ctrl Pts',(4.48035529049402,6.77835555525396,32.7309504004674));
#178649=CARTESIAN_POINT('Ctrl Pts',(4.31892793655416,6.88505575611526,32.7385188091681));
#178650=CARTESIAN_POINT('Ctrl Pts',(4.15355877926477,6.98607018940402,32.7460872178689));
#178651=CARTESIAN_POINT('Ctrl Pts',(3.98470591506945,7.08108793427327,32.7536556265696));
#178652=CARTESIAN_POINT('Ctrl Pts',(3.81589384707356,7.17608272209712,32.7612222066825));
#178653=CARTESIAN_POINT('Ctrl Pts',(3.64360006343698,7.26508351828062,32.7687887867953));
#178654=CARTESIAN_POINT('Ctrl Pts',(3.46831037012406,7.3478235375511,32.7763553669081));
#178655=CARTESIAN_POINT('Ctrl Pts',(3.29305177240959,7.43054887911654,32.7839206047438));
#178656=CARTESIAN_POINT('Ctrl Pts',(3.11479865672792,7.50701550028967,32.7914858425796));
#178657=CARTESIAN_POINT('Ctrl Pts',(2.93405982546309,7.57700339864669,32.7990510804153));
#178658=CARTESIAN_POINT('Ctrl Pts',(2.75325814263375,7.64701563515439,32.8066189490473));
#178659=CARTESIAN_POINT('Ctrl Pts',(2.56996935946642,7.71054451188793,32.8141868176793));
#178660=CARTESIAN_POINT('Ctrl Pts',(2.38472103070679,7.76741869401957,32.8217546863112));
#178661=CARTESIAN_POINT('Ctrl Pts',(2.20186323275607,7.82355894518661,32.8292248956377));
#178662=CARTESIAN_POINT('Ctrl Pts',(2.01709650532465,7.87321516599391,32.8366951049643));
#178663=CARTESIAN_POINT('Ctrl Pts',(1.83094063365424,7.91627083660822,32.8441653142908));
#178664=CARTESIAN_POINT('Ctrl Pts',(1.59904123836584,7.96990644793545,32.853471155734));
#178665=CARTESIAN_POINT('Ctrl Pts',(1.36510048989128,8.01327489456442,32.8627769971773));
#178666=CARTESIAN_POINT('Ctrl Pts',(1.12994981778146,8.04629734547485,32.8720828386205));
#178667=CARTESIAN_POINT('Ctrl Pts',(0.893536669155535,8.07949708726183,
32.881438641249));
#178668=CARTESIAN_POINT('Ctrl Pts',(0.655900623007412,8.10223949089091,
32.8907944438775));
#178669=CARTESIAN_POINT('Ctrl Pts',(0.417882586364596,8.11449700884246,
32.900150246506));
#178670=CARTESIAN_POINT('Ctrl Pts',(0.178709101831053,8.12681403036552,
32.909551466459));
#178671=CARTESIAN_POINT('Ctrl Pts',(-0.0608500475701027,8.12854414403122,
32.918952686412));
#178672=CARTESIAN_POINT('Ctrl Pts',(-0.299946381647792,8.11971180095922,
32.928353906365));
#178673=CARTESIAN_POINT('Ctrl Pts',(-0.539301488910411,8.11086989867103,
32.9377653012278));
#178674=CARTESIAN_POINT('Ctrl Pts',(-0.778192742263481,8.0914426860629,
32.9471766960906));
#178675=CARTESIAN_POINT('Ctrl Pts',(-1.01577422354322,8.06150670093905,
32.9565880909534));
#178676=CARTESIAN_POINT('Ctrl Pts',(-1.25307701775994,8.03160583122793,
32.9659884460921));
#178677=CARTESIAN_POINT('Ctrl Pts',(-1.48907307527489,7.99122083726528,
32.9753888012308));
#178678=CARTESIAN_POINT('Ctrl Pts',(-1.72292528536935,7.9404795839757,32.9847891563696));
#178679=CARTESIAN_POINT('Ctrl Pts',(-1.87254875182174,7.90801428374929,
32.9908036974388));
#178680=CARTESIAN_POINT('Ctrl Pts',(-2.02129470894103,7.8713104735582,32.996818238508));
#178681=CARTESIAN_POINT('Ctrl Pts',(-2.16894526312187,7.83041276102871,
33.0028327795772));
#178682=CARTESIAN_POINT('Ctrl Pts',(-2.35901041586562,7.77776663300085,
33.0105750780965));
#178683=CARTESIAN_POINT('Ctrl Pts',(-2.54734889156301,7.71814326754754,
33.0183173766158));
#178684=CARTESIAN_POINT('Ctrl Pts',(-2.73340470777657,7.65167865673964,
33.0260596751351));
#178685=CARTESIAN_POINT('Ctrl Pts',(-2.91934462806418,7.58525544736582,
33.0337971509035));
#178686=CARTESIAN_POINT('Ctrl Pts',(-3.10300438871746,7.51199959605789,
33.0415346266719));
#178687=CARTESIAN_POINT('Ctrl Pts',(-3.28384194403098,7.43209725778147,
33.0492721024402));
#178688=CARTESIAN_POINT('Ctrl Pts',(-3.46459899395702,7.35223049048305,
33.0570061336338));
#178689=CARTESIAN_POINT('Ctrl Pts',(-3.64253601833489,7.2657232716565,33.0647401648274));
#178690=CARTESIAN_POINT('Ctrl Pts',(-3.81712965369039,7.17281038153229,
33.072474196021));
#178691=CARTESIAN_POINT('Ctrl Pts',(-3.99170094655791,7.07990938133252,
33.0802072375021));
#178692=CARTESIAN_POINT('Ctrl Pts',(-4.16292938732278,6.98060450167136,
33.0879402789832));
#178693=CARTESIAN_POINT('Ctrl Pts',(-4.33031465918097,6.87517727153144,
33.0956733204643));
#178694=CARTESIAN_POINT('Ctrl Pts',(-4.49768320937557,6.76976057349303,
33.1034055894204));
#178695=CARTESIAN_POINT('Ctrl Pts',(-4.66120905830741,6.65822293464464,
33.1111378583764));
#178696=CARTESIAN_POINT('Ctrl Pts',(-4.82041952696814,6.54089008824673,
33.1188701273325));
#178697=CARTESIAN_POINT('Ctrl Pts',(-4.97969123665482,6.42351210923942,
33.1266053705407));
#178698=CARTESIAN_POINT('Ctrl Pts',(-5.13464396491998,6.30033467881232,
33.1343406137489));
#178699=CARTESIAN_POINT('Ctrl Pts',(-5.28483636192333,6.17172521991971,
33.1420758569572));
#178700=CARTESIAN_POINT('Ctrl Pts',(-5.41055511445368,6.06407249542646,
33.1485506529259));
#178701=CARTESIAN_POINT('Ctrl Pts',(-5.53293900276645,5.95261459081656,
33.1550254488947));
#178702=CARTESIAN_POINT('Ctrl Pts',(-5.6517484076503,5.83758747250286,33.1615002448635));
#178703=CARTESIAN_POINT('Ctrl Pts',(-5.80614264483297,5.68810836178156,
33.1699143193679));
#178704=CARTESIAN_POINT('Ctrl Pts',(-5.95457441705346,5.53252925030719,
33.1783283938722));
#178705=CARTESIAN_POINT('Ctrl Pts',(-6.09658687204909,5.37134211106113,
33.1867424683766));
#178706=CARTESIAN_POINT('Ctrl Pts',(-6.23863898721543,5.21010995668271,
33.1951588927004));
#178707=CARTESIAN_POINT('Ctrl Pts',(-6.37426803170842,5.04326684605947,
33.2035753170243));
#178708=CARTESIAN_POINT('Ctrl Pts',(-6.50305678842,4.87133862188665,33.2119917413481));
#178709=CARTESIAN_POINT('Ctrl Pts',(-6.63187748384527,4.69936776071301,
33.2204102528865));
#178710=CARTESIAN_POINT('Ctrl Pts',(-6.75385434666259,4.52230947963071,
33.2288287644249));
#178711=CARTESIAN_POINT('Ctrl Pts',(-6.86861227674034,4.34072032666375,
33.2372472759632));
#178712=CARTESIAN_POINT('Ctrl Pts',(-6.98341428486049,4.15906142606036,
33.2456690210168));
#178713=CARTESIAN_POINT('Ctrl Pts',(-7.0909916771743,3.97286839841154,33.2540907660704));
#178714=CARTESIAN_POINT('Ctrl Pts',(-7.1910135405162,3.78272544901326,33.2625125111239));
#178715=CARTESIAN_POINT('Ctrl Pts',(-7.29104624595438,3.59256188863962,
33.2709351690716));
#178716=CARTESIAN_POINT('Ctrl Pts',(-7.38352166699777,3.39844778665161,
33.2793578270193));
#178717=CARTESIAN_POINT('Ctrl Pts',(-7.46815530497601,3.2009910814088,33.287780484967));
#178718=CARTESIAN_POINT('Ctrl Pts',(-7.55280503783703,3.00349682558206,
33.2962047446618));
#178719=CARTESIAN_POINT('Ctrl Pts',(-7.62960990449206,2.80265893920064,
33.3046290043567));
#178720=CARTESIAN_POINT('Ctrl Pts',(-7.69833341527587,2.59910565190163,
33.3130532640516));
#178721=CARTESIAN_POINT('Ctrl Pts',(-7.71767951534411,2.54180412262302,
33.3154247460844));
#178722=CARTESIAN_POINT('Ctrl Pts',(-7.73638549978518,2.48428751806916,
33.3177962281173));
#178723=CARTESIAN_POINT('Ctrl Pts',(-7.75444679713097,2.42657009644585,
33.3201677101501));
#178724=CARTESIAN_POINT('Ctrl Pts',(-7.81860677837113,2.22153783227988,
33.3285920353703));
#178725=CARTESIAN_POINT('Ctrl Pts',(-7.87463413800463,2.01394911798742,
33.3370163605904));
#178726=CARTESIAN_POINT('Ctrl Pts',(-7.92235089313825,1.80445113219825,
33.3454406858106));
#178727=CARTESIAN_POINT('Ctrl Pts',(-7.97005940223307,1.59498935022292,
33.3538635552043));
#178728=CARTESIAN_POINT('Ctrl Pts',(-8.00946011672307,1.38361921295956,
33.362286424598));
#178729=CARTESIAN_POINT('Ctrl Pts',(-8.04042581154511,1.17099971457691,
33.3707092939918));
#178730=CARTESIAN_POINT('Ctrl Pts',(-8.07138517847581,0.958423665343055,
33.3791304421581));
#178731=CARTESIAN_POINT('Ctrl Pts',(-8.09391292985907,0.744599025845439,
33.3875515903245));
#178732=CARTESIAN_POINT('Ctrl Pts',(-8.10793335615874,0.530192657991854,
33.3959727384908));
#178733=CARTESIAN_POINT('Ctrl Pts',(-8.12194984879967,0.315846445333534,
33.404391523967));
#178734=CARTESIAN_POINT('Ctrl Pts',(-8.12746376636122,0.100919093475446,
33.4128103094432));
#178735=CARTESIAN_POINT('Ctrl Pts',(-8.12445137104079,-0.11391875215882,
33.4212290949194));
#178736=CARTESIAN_POINT('Ctrl Pts',(-8.1214398172128,-0.328696584281594,
33.4296455286643));
#178737=CARTESIAN_POINT('Ctrl Pts',(-8.10990670965498,-0.543384696404741,
33.4380619624092));
#178738=CARTESIAN_POINT('Ctrl Pts',(-8.08988041762325,-0.757312611182398,
33.4464783961542));
#178739=CARTESIAN_POINT('Ctrl Pts',(-8.0698613939715,-0.971162882561556,
33.4548917752228));
#178740=CARTESIAN_POINT('Ctrl Pts',(-8.041355366176,-1.18425324501899,33.4633051542915));
#178741=CARTESIAN_POINT('Ctrl Pts',(-8.00444263315897,-1.39591751008687,
33.4717185333602));
#178742=CARTESIAN_POINT('Ctrl Pts',(-7.99403481695767,-1.45559780431469,
33.4740907473856));
#178743=CARTESIAN_POINT('Ctrl Pts',(-7.98295898412734,-1.51516475896524,
33.476462961411));
#178744=CARTESIAN_POINT('Ctrl Pts',(-7.97121767767481,-1.57460353664807,
33.4788351754364));
#178745=CARTESIAN_POINT('Ctrl Pts',(-7.93293227191862,-1.76841823098716,
33.486570360347));
#178746=CARTESIAN_POINT('Ctrl Pts',(-7.88755027022448,-1.96095538472589,
33.4943055452577));
#178747=CARTESIAN_POINT('Ctrl Pts',(-7.83518219328127,-2.15165228617173,
33.5020407301683));
#178748=CARTESIAN_POINT('Ctrl Pts',(-7.78283030984125,-2.34229021942431,
33.5097735231687));
#178749=CARTESIAN_POINT('Ctrl Pts',(-7.72349674658826,-2.53108869332655,
33.517506316169));
#178750=CARTESIAN_POINT('Ctrl Pts',(-7.657342730468,-2.71749698631828,33.5252391091694));
#178751=CARTESIAN_POINT('Ctrl Pts',(-7.59119741715084,-2.90388075661636,
33.5329708848925));
#178752=CARTESIAN_POINT('Ctrl Pts',(-7.51823355702077,-3.08787463971037,
33.5407026606156));
#178753=CARTESIAN_POINT('Ctrl Pts',(-7.43866171381144,-3.26894470280179,
33.5484344363387));
#178754=CARTESIAN_POINT('Ctrl Pts',(-7.35906139762417,-3.45007955770527,
33.5561689787023));
#178755=CARTESIAN_POINT('Ctrl Pts',(-7.27284851266753,-3.6282881768599,
33.5639035210659));
#178756=CARTESIAN_POINT('Ctrl Pts',(-7.18028137304695,-3.80305758125945,
33.5716380634294));
#178757=CARTESIAN_POINT('Ctrl Pts',(-7.08769859986825,-3.9778565022634,
33.579373912071));
#178758=CARTESIAN_POINT('Ctrl Pts',(-6.98875960585026,-4.14921474241172,
33.5871097607126));
#178759=CARTESIAN_POINT('Ctrl Pts',(-6.88376792891641,-4.316645302005,33.5948456093541));
#178760=CARTESIAN_POINT('Ctrl Pts',(-6.77869034303867,-4.48421286086308,
33.6025877878173));
#178761=CARTESIAN_POINT('Ctrl Pts',(-6.6675503734878,-4.64784602265518,
33.6103299662805));
#178762=CARTESIAN_POINT('Ctrl Pts',(-6.55069455383339,-4.80708731196735,
33.6180721447437));
#178763=CARTESIAN_POINT('Ctrl Pts',(-6.45293711838823,-4.94030292849529,
33.6245489767368));
#178764=CARTESIAN_POINT('Ctrl Pts',(-6.35118031518691,-5.07044540173571,
33.6310258087299));
#178765=CARTESIAN_POINT('Ctrl Pts',(-6.2456480000629,-5.19726549464334,
33.637502640723));
#178766=CARTESIAN_POINT('Ctrl Pts',(-6.09251824414858,-5.38128429352174,
33.6469006691946));
#178767=CARTESIAN_POINT('Ctrl Pts',(-5.93135238108043,-5.55841258206398,
33.6562986976661));
#178768=CARTESIAN_POINT('Ctrl Pts',(-5.76274268177044,-5.72804367530497,
33.6656967261376));
#178769=CARTESIAN_POINT('Ctrl Pts',(-5.59389306497075,-5.89791613939373,
33.6751081272171));
#178770=CARTESIAN_POINT('Ctrl Pts',(-5.41757845098032,-6.06027004263627,
33.6845195282966));
#178771=CARTESIAN_POINT('Ctrl Pts',(-5.23442833419645,-6.21453518588972,
33.693930929376));
#178772=CARTESIAN_POINT('Ctrl Pts',(-5.05155398082456,-6.36856805693391,
33.7033281600028));
#178773=CARTESIAN_POINT('Ctrl Pts',(-4.86186472487565,-6.51453648871021,
33.7127253906295));
#178774=CARTESIAN_POINT('Ctrl Pts',(-4.66602124068028,-6.65191200663542,
33.7221226212562));
#178775=CARTESIAN_POINT('Ctrl Pts',(-4.47067174680851,-6.78894101225855,
33.7314961485618));
#178776=CARTESIAN_POINT('Ctrl Pts',(-4.26919905109153,-6.9174203594827,
33.7408696758674));
#178777=CARTESIAN_POINT('Ctrl Pts',(-4.06229233142146,-7.03686496790825,
33.750243203173));
#178778=CARTESIAN_POINT('Ctrl Pts',(-3.85672925183439,-7.15553391006335,
33.7595558593429));
#178779=CARTESIAN_POINT('Ctrl Pts',(-3.64580252352251,-7.26528503378603,
33.7688685155128));
#178780=CARTESIAN_POINT('Ctrl Pts',(-3.43022070587989,-7.3656821456979,
33.7781811716827));
#178781=CARTESIAN_POINT('Ctrl Pts',(-3.29141007051721,-7.43032668318932,
33.7841774831249));
#178782=CARTESIAN_POINT('Ctrl Pts',(-3.15067013035487,-7.49109391630273,
33.7901737945671));
#178783=CARTESIAN_POINT('Ctrl Pts',(-3.00819722507071,-7.54787632500539,
33.7961701060093));
#178784=CARTESIAN_POINT('Ctrl Pts',(-2.82838897756056,-7.61953869040649,
33.8037377642233));
#178785=CARTESIAN_POINT('Ctrl Pts',(-2.64589067218342,-7.68482273278492,
33.8113054224373));
#178786=CARTESIAN_POINT('Ctrl Pts',(-2.4612154913732,-7.74352025034639,
33.8188730806513));
#178787=CARTESIAN_POINT('Ctrl Pts',(-2.27659144380121,-7.80220151562026,
33.8264386435167));
#178788=CARTESIAN_POINT('Ctrl Pts',(-2.08979207012664,-7.85429977352598,
33.8340042063822));
#178789=CARTESIAN_POINT('Ctrl Pts',(-1.90134819948848,-7.89965585242812,
33.8415697692476));
#178790=CARTESIAN_POINT('Ctrl Pts',(-1.71292083831543,-7.94500795770884,
33.8491346692982));
#178791=CARTESIAN_POINT('Ctrl Pts',(-1.52284962459433,-7.98361897446067,
33.8566995693488));
#178792=CARTESIAN_POINT('Ctrl Pts',(-1.33167806492943,-8.01538028379726,
33.8642644693994));
#178793=CARTESIAN_POINT('Ctrl Pts',(-1.14041267944472,-8.04715718138815,
33.8718330822562));
#178794=CARTESIAN_POINT('Ctrl Pts',(-0.948046231811912,-8.07207759181744,
33.879401695113));
#178795=CARTESIAN_POINT('Ctrl Pts',(-0.755130451195359,-8.0900843978402,
33.8869703079698));
#178796=CARTESIAN_POINT('Ctrl Pts',(-0.562171769501025,-8.10809520826003,
33.894540603953));
#178797=CARTESIAN_POINT('Ctrl Pts',(-0.36866387859067,-8.11918932886303,
33.9021108999362));
#178798=CARTESIAN_POINT('Ctrl Pts',(-0.17516079945972,-8.12336175833827,
33.9096811959194));
#178799=CARTESIAN_POINT('Ctrl Pts',(0.0185383534548096,-8.12753841567405,
33.9172591627707));
#178800=CARTESIAN_POINT('Ctrl Pts',(0.212232316991425,-8.12477937273059,
33.9248371296218));
#178801=CARTESIAN_POINT('Ctrl Pts',(0.405368986399675,-8.11513176401747,
33.9324150964731));
#178802=CARTESIAN_POINT('Ctrl Pts',(0.595859927315845,-8.10561631536143,
33.9398892547473));
#178803=CARTESIAN_POINT('Ctrl Pts',(0.785808414656637,-8.08939992281175,
33.9473634130216));
#178804=CARTESIAN_POINT('Ctrl Pts',(0.974693342529583,-8.06657674918726,
33.9548375712958));
#178805=CARTESIAN_POINT('Ctrl Pts',(1.17875832895955,-8.04191935238796,
33.9629124030147));
#178806=CARTESIAN_POINT('Ctrl Pts',(1.38201771513442,-8.00949834448808,
33.9709872347336));
#178807=CARTESIAN_POINT('Ctrl Pts',(1.58385912450158,-7.96938378020742,
33.9790620664525));
#178808=CARTESIAN_POINT('Ctrl Pts',(1.78556699591701,-7.92929575565795,
33.9871315558757));
#178809=CARTESIAN_POINT('Ctrl Pts',(1.98585845150732,-7.88152438633841,
33.9952010452989));
#178810=CARTESIAN_POINT('Ctrl Pts',(2.18412877315489,-7.82619122337149,
34.0032705347222));
#178811=CARTESIAN_POINT('Ctrl Pts',(2.38229493006097,-7.77088713063841,
34.0113357846996));
#178812=CARTESIAN_POINT('Ctrl Pts',(2.57844176615795,-7.70802925192821,
34.019401034677));
#178813=CARTESIAN_POINT('Ctrl Pts',(2.77197663982588,-7.6377898027348,34.0274662846545));
#178814=CARTESIAN_POINT('Ctrl Pts',(2.96543617439079,-7.56757769629878,
34.0355283949977));
#178815=CARTESIAN_POINT('Ctrl Pts',(3.15628547712697,-7.48998985841786,
34.043590505341));
#178816=CARTESIAN_POINT('Ctrl Pts',(3.34394831142824,-7.40524795351217,
34.0516526156843));
#178817=CARTESIAN_POINT('Ctrl Pts',(3.53156361096603,-7.32052751362603,
34.059712683905));
#178818=CARTESIAN_POINT('Ctrl Pts',(3.71599376363942,-7.2286567516874,34.0677727521257));
#178819=CARTESIAN_POINT('Ctrl Pts',(3.8966831435325,-7.12990519161438,34.0758328203465));
#178820=CARTESIAN_POINT('Ctrl Pts',(4.08007951981587,-7.02967418589374,
34.0840136404099));
#178821=CARTESIAN_POINT('Ctrl Pts',(4.25962184019905,-6.92235470453889,
34.0921944604733));
#178822=CARTESIAN_POINT('Ctrl Pts',(4.43475493420291,-6.80827703872742,
34.1003752805367));
#178823=CARTESIAN_POINT('Ctrl Pts',(4.60731975200248,-6.69587228891284,
34.1084361312384));
#178824=CARTESIAN_POINT('Ctrl Pts',(4.77560351615612,-6.57690640215509,
34.1164969819402));
#178825=CARTESIAN_POINT('Ctrl Pts',(4.93910395641602,-6.45173927481695,
34.1245578326419));
#178826=CARTESIAN_POINT('Ctrl Pts',(5.10263151173733,-6.32655138964882,
34.1326200201624));
#178827=CARTESIAN_POINT('Ctrl Pts',(5.26137390929089,-6.19516040529427,
34.1406822076829));
#178828=CARTESIAN_POINT('Ctrl Pts',(5.41486111847034,-6.05796720279816,
34.1487443952034));
#178829=CARTESIAN_POINT('Ctrl Pts',(5.56839279643728,-5.92073425226441,
34.1568089185258));
#178830=CARTESIAN_POINT('Ctrl Pts',(5.716666013082,-5.77769594188403,34.1648734418481));
#178831=CARTESIAN_POINT('Ctrl Pts',(5.85924639888388,-5.62929118092733,
34.1729379651705));
#178832=CARTESIAN_POINT('Ctrl Pts',(6.00545155325516,-5.47711358045951,
34.1812075098953));
#178833=CARTESIAN_POINT('Ctrl Pts',(6.14567034559919,-5.31929331423924,
34.1894770546201));
#178834=CARTESIAN_POINT('Ctrl Pts',(6.27947735424209,-5.15634092356787,
34.197746599345));
#178835=CARTESIAN_POINT('Ctrl Pts',(6.41014328753384,-4.99721378646835,
34.2058220192376));
#178836=CARTESIAN_POINT('Ctrl Pts',(6.53469492018589,-4.83319304331193,
34.2138974391303));
#178837=CARTESIAN_POINT('Ctrl Pts',(6.65277901944452,-4.66478497692431,
34.2219728590229));
#178838=CARTESIAN_POINT('Ctrl Pts',(6.77512105010348,-4.49030437411188,
34.2303394661638));
#178839=CARTESIAN_POINT('Ctrl Pts',(6.89052025400354,-4.31111448626926,
34.2387060733048));
#178840=CARTESIAN_POINT('Ctrl Pts',(6.99863465908814,-4.12780819214147,
34.2470726804457));
#178841=CARTESIAN_POINT('Ctrl Pts',(7.10674906417275,-3.94450189801367,
34.2554392875867));
#178842=CARTESIAN_POINT('Ctrl Pts',(7.20757852552032,-3.75707954566137,
34.2638058947276));
#178843=CARTESIAN_POINT('Ctrl Pts',(7.30083524784917,-3.56615931307942,
34.2721725018686));
#178844=CARTESIAN_POINT('Ctrl Pts',(7.39190886085651,-3.37970846060229,
34.280343249477));
#178845=CARTESIAN_POINT('Ctrl Pts',(7.4759325855816,-3.18956949062817,34.2885139970854));
#178846=CARTESIAN_POINT('Ctrl Pts',(7.55260879493786,-2.99629570522125,
34.2966847446939));
#178847=CARTESIAN_POINT('Ctrl Pts',(7.62918229596141,-2.80328081143694,
34.3048445475273));
#178848=CARTESIAN_POINT('Ctrl Pts',(7.69842779444841,-2.60713975455653,
34.3130043503606));
#178849=CARTESIAN_POINT('Ctrl Pts',(7.76009405630176,-2.4084492520811,34.321164153194));
#178850=CARTESIAN_POINT('Ctrl Pts',(7.82165318383096,-2.2101039395371,34.3293097797998));
#178851=CARTESIAN_POINT('Ctrl Pts',(7.87565925711571,-2.00921830639751,
34.3374554064056));
#178852=CARTESIAN_POINT('Ctrl Pts',(7.92190957329863,-1.80638763142893,
34.3456010330114));
#178853=CARTESIAN_POINT('Ctrl Pts',(7.9681129779998,-1.60376268667573,34.3537383975458));
#178854=CARTESIAN_POINT('Ctrl Pts',(8.00657624106007,-1.39919692676357,
34.3618757620802));
#178855=CARTESIAN_POINT('Ctrl Pts',(8.03714624980014,-1.19330118655077,
34.3700131266146));
#178856=CARTESIAN_POINT('Ctrl Pts',(8.06767649776054,-0.987673243944254,
34.378139907313));
#178857=CARTESIAN_POINT('Ctrl Pts',(8.09033393005807,-0.780719070800755,
34.3862666880114));
#178858=CARTESIAN_POINT('Ctrl Pts',(8.10501632571067,-0.573060138609772,
34.3943934687099));
#178859=CARTESIAN_POINT('Ctrl Pts',(8.1184513582358,-0.383043156767717,
34.4018298275706));
#178860=CARTESIAN_POINT('Ctrl Pts',(8.12520938963273,-0.192436394347444,
34.4092661864313));
#178861=CARTESIAN_POINT('Ctrl Pts',(8.12524981744152,-0.00172240138687737,
34.416702545292));
#178862=CARTESIAN_POINT('',(8.12804752138608,0.000138485945550895,30.4167025567876));
#178863=CARTESIAN_POINT('Ctrl Pts',(8.12804752138608,0.000138485945550895,
30.4167025567876));
#178864=CARTESIAN_POINT('Ctrl Pts',(8.13188959766799,0.403006519365657,
30.4325194828565));
#178865=CARTESIAN_POINT('Ctrl Pts',(8.01567158785024,2.15330402273085,30.5012255640209));
#178866=CARTESIAN_POINT('Ctrl Pts',(6.73558121933894,5.11366765981583,30.6228208002808));
#178867=CARTESIAN_POINT('Ctrl Pts',(3.50109731423418,7.71360667956193,30.7814882655671));
#178868=CARTESIAN_POINT('Ctrl Pts',(-0.62887488263501,8.44934367887132,
30.9401557308536));
#178869=CARTESIAN_POINT('Ctrl Pts',(-4.5833286137765,7.11692082205467,31.09882319614));
#178870=CARTESIAN_POINT('Ctrl Pts',(-7.43229334537612,4.06791197667428,
31.2574906614265));
#178871=CARTESIAN_POINT('Ctrl Pts',(-8.47097384492051,0.00353968824748415,
31.4161581267129));
#178872=CARTESIAN_POINT('Ctrl Pts',(-7.44199729007049,-4.01675585914069,
31.5748255919993));
#178873=CARTESIAN_POINT('Ctrl Pts',(-3.67416070295655,-8.17511883464782,
31.7863822123813));
#178874=CARTESIAN_POINT('Ctrl Pts',(2.38173522129231,-8.63148943733773,
31.9979388327631));
#178875=CARTESIAN_POINT('Ctrl Pts',(6.72405806064641,-5.12185486701296,
32.2094954531451));
#178876=CARTESIAN_POINT('Ctrl Pts',(8.00961219341287,-2.17106617787569,
32.3314536427881));
#178877=CARTESIAN_POINT('Ctrl Pts',(8.12957810661569,-0.414884693015649,
32.4005226773356));
#178878=CARTESIAN_POINT('Ctrl Pts',(8.12588319212562,-0.00333877610576572,
32.4167025567876));
#178879=CARTESIAN_POINT('',(8.12524926709318,0.00223483220777574,28.4167025567876));
#178880=CARTESIAN_POINT('Ctrl Pts',(8.1252482522699,0.00532930435881126,
28.4167025567876));
#178881=CARTESIAN_POINT('Ctrl Pts',(8.12509106864763,0.244977083153327,
28.4260839083502));
#178882=CARTESIAN_POINT('Ctrl Pts',(8.11432752923275,0.484323489608783,
28.4354652599127));
#178883=CARTESIAN_POINT('Ctrl Pts',(8.09306141022359,0.722526520516521,
28.4448466114753));
#178884=CARTESIAN_POINT('Ctrl Pts',(8.07128129778416,0.966486821610978,
28.4544547064821));
#178885=CARTESIAN_POINT('Ctrl Pts',(8.03848466495988,1.20924773715741,28.464062801489));
#178886=CARTESIAN_POINT('Ctrl Pts',(7.99483706199556,1.44991996835765,28.4736708964958));
#178887=CARTESIAN_POINT('Ctrl Pts',(7.95184974422027,1.6869513968819,28.4831336437081));
#178888=CARTESIAN_POINT('Ctrl Pts',(7.89833745508182,1.92195688380524,28.4925963909204));
#178889=CARTESIAN_POINT('Ctrl Pts',(7.8345091458018,2.15410167049931,28.5020591381326));
#178890=CARTESIAN_POINT('Ctrl Pts',(7.76921023230268,2.39159507298165,28.5117399070367));
#178891=CARTESIAN_POINT('Ctrl Pts',(7.6931142730173,2.62609435745481,28.5214206759408));
#178892=CARTESIAN_POINT('Ctrl Pts',(7.60649905761435,2.85672183612825,28.5311014448449));
#178893=CARTESIAN_POINT('Ctrl Pts',(7.51988384221139,3.08734931480173,28.540782213749));
#178894=CARTESIAN_POINT('Ctrl Pts',(7.42274934721133,3.31410495540211,28.5504629826531));
#178895=CARTESIAN_POINT('Ctrl Pts',(7.31542809573566,3.53612773222649,28.5601437515572));
#178896=CARTESIAN_POINT('Ctrl Pts',(7.22959677648631,3.71369282372714,28.5678860500765));
#178897=CARTESIAN_POINT('Ctrl Pts',(7.13721021316495,3.88830969019066,28.5756283485958));
#178898=CARTESIAN_POINT('Ctrl Pts',(7.03850176295656,4.05945568954231,28.583370647115));
#178899=CARTESIAN_POINT('Ctrl Pts',(6.93985479917425,4.23049508043424,28.5911081228834));
#178900=CARTESIAN_POINT('Ctrl Pts',(6.83489396518796,4.39806760432478,28.5988455986518));
#178901=CARTESIAN_POINT('Ctrl Pts',(6.72389947446002,4.56167331358311,28.6065830744202));
#178902=CARTESIAN_POINT('Ctrl Pts',(6.61295439633667,4.72520618873798,28.6143171056137));
#178903=CARTESIAN_POINT('Ctrl Pts',(6.49598120900059,4.884775474622,28.6220511368073));
#178904=CARTESIAN_POINT('Ctrl Pts',(6.37330461960953,5.03990831148383,28.6297851680008));
#178905=CARTESIAN_POINT('Ctrl Pts',(6.25064372895854,5.19502129622804,28.6375182094819));
#178906=CARTESIAN_POINT('Ctrl Pts',(6.12228110297427,5.34569868106632,28.645251250963));
#178907=CARTESIAN_POINT('Ctrl Pts',(5.98858331476219,5.49149865197579,28.6529842924441));
#178908=CARTESIAN_POINT('Ctrl Pts',(5.8548988828592,5.63728405757716,28.6607165614002));
#178909=CARTESIAN_POINT('Ctrl Pts',(5.71588059186604,5.77819276177285,28.6684488303562));
#178910=CARTESIAN_POINT('Ctrl Pts',(5.57193355532975,5.91381805752344,28.6761810993123));
#178911=CARTESIAN_POINT('Ctrl Pts',(5.42793114891565,6.04949552215667,28.6839163425205));
#178912=CARTESIAN_POINT('Ctrl Pts',(5.27899646657123,6.17988527542889,28.6916515857287));
#178913=CARTESIAN_POINT('Ctrl Pts',(5.12557002731086,6.30461889868313,28.699386828937));
#178914=CARTESIAN_POINT('Ctrl Pts',(4.99714421525889,6.40902734962442,28.7058616249058));
#178915=CARTESIAN_POINT('Ctrl Pts',(4.86557192918227,6.50947342548462,28.7123364208746));
#178916=CARTESIAN_POINT('Ctrl Pts',(4.73112823130852,6.60576363650831,28.7188112168435));
#178917=CARTESIAN_POINT('Ctrl Pts',(4.55641704411399,6.73089391296767,28.7272252913479));
#178918=CARTESIAN_POINT('Ctrl Pts',(4.3767721993223,6.84906573986351,28.7356393658523));
#178919=CARTESIAN_POINT('Ctrl Pts',(4.19275952876206,6.95991775069756,28.7440534403567));
#178920=CARTESIAN_POINT('Ctrl Pts',(4.00869546852586,7.07080071944825,28.7524698646806));
#178921=CARTESIAN_POINT('Ctrl Pts',(3.82026137354079,7.17435965494173,28.7608862890045));
#178922=CARTESIAN_POINT('Ctrl Pts',(3.62804930012442,7.27027825040876,28.7693027133284));
#178923=CARTESIAN_POINT('Ctrl Pts',(3.43578955945314,7.36622063301913,28.7777212248669));
#178924=CARTESIAN_POINT('Ctrl Pts',(3.23975020606864,7.45451877506325,28.7861397364054));
#178925=CARTESIAN_POINT('Ctrl Pts',(3.04054596310806,7.53490330453731,28.7945582479439));
#178926=CARTESIAN_POINT('Ctrl Pts',(2.84126520662993,7.61531870937334,28.8029799929975));
#178927=CARTESIAN_POINT('Ctrl Pts',(2.63881737573806,7.6878143275157,28.8114017380511));
#178928=CARTESIAN_POINT('Ctrl Pts',(2.43383649091729,7.75216921241916,28.8198234831048));
#178929=CARTESIAN_POINT('Ctrl Pts',(2.22883338672855,7.81653107321633,28.8282461410525));
#178930=CARTESIAN_POINT('Ctrl Pts',(2.02129693312102,7.87275036272454,28.8366687990003));
#178931=CARTESIAN_POINT('Ctrl Pts',(1.81187618825483,7.92065604864491,28.8450914569481));
#178932=CARTESIAN_POINT('Ctrl Pts',(1.60241561758895,7.96857084484827,28.853515716643));
#178933=CARTESIAN_POINT('Ctrl Pts',(1.39107029708886,8.0081688201962,28.861939976338));
#178934=CARTESIAN_POINT('Ctrl Pts',(1.1785006509006,8.03932980902804,28.8703642360329));
#178935=CARTESIAN_POINT('Ctrl Pts',(1.11866095995868,8.04810182316354,28.8727357180653));
#178936=CARTESIAN_POINT('Ctrl Pts',(1.05872430008753,8.05620555411314,28.8751072000976));
#178937=CARTESIAN_POINT('Ctrl Pts',(0.998705517653771,8.06363905761586,
28.87747868213));
#178938=CARTESIAN_POINT('Ctrl Pts',(0.78549802308374,8.09004543564329,28.8859030073501));
#178939=CARTESIAN_POINT('Ctrl Pts',(0.571231764690501,8.10799285447874,
28.8943273325702));
#178940=CARTESIAN_POINT('Ctrl Pts',(0.356575332115341,8.11742210280005,
28.9027516577903));
#178941=CARTESIAN_POINT('Ctrl Pts',(0.141955994797125,8.12684972163193,
28.911174527184));
#178942=CARTESIAN_POINT('Ctrl Pts',(-0.0730531184909462,8.12776209849467,
28.9195973965777));
#178943=CARTESIAN_POINT('Ctrl Pts',(-0.287780883101245,8.12015207528908,
28.9280202659714));
#178944=CARTESIAN_POINT('Ctrl Pts',(-0.502464767732327,8.1125436072045,
28.9364414141376));
#178945=CARTESIAN_POINT('Ctrl Pts',(-0.716867154888951,8.09641622618733,
28.9448625623037));
#178946=CARTESIAN_POINT('Ctrl Pts',(-0.930318404587091,8.07181486585183,
28.9532837104699));
#178947=CARTESIAN_POINT('Ctrl Pts',(-1.14370976706711,8.0472204078279,28.9617024959461));
#178948=CARTESIAN_POINT('Ctrl Pts',(-1.35615026307032,8.01415674921051,
28.9701212814222));
#178949=CARTESIAN_POINT('Ctrl Pts',(-1.56697583717458,7.97272063277091,
28.9785400668984));
#178950=CARTESIAN_POINT('Ctrl Pts',(-1.77774251856639,7.93129609123299,
28.9869565006432));
#178951=CARTESIAN_POINT('Ctrl Pts',(-1.9868949199916,7.88150381237641,28.995372934388));
#178952=CARTESIAN_POINT('Ctrl Pts',(-2.19377848254012,7.82349177362921,
29.0037893681328));
#178953=CARTESIAN_POINT('Ctrl Pts',(-2.40058695838251,7.76550078987958,
29.0122027472015));
#178954=CARTESIAN_POINT('Ctrl Pts',(-2.60512798586169,7.69929607501525,
29.0206161262701));
#178955=CARTESIAN_POINT('Ctrl Pts',(-2.80676052500101,7.62507592865776,
29.0290295053387));
#178956=CARTESIAN_POINT('Ctrl Pts',(-2.86361230043232,7.60414901323426,
29.0314017193647));
#178957=CARTESIAN_POINT('Ctrl Pts',(-2.92023294230354,7.58258517603043,
29.0337739333906));
#178958=CARTESIAN_POINT('Ctrl Pts',(-2.9766083084613,7.56038957597419,29.0361461474165));
#178959=CARTESIAN_POINT('Ctrl Pts',(-3.16043399909156,7.48801538512858,
29.0438813323272));
#178960=CARTESIAN_POINT('Ctrl Pts',(-3.34173196659764,7.40888809131464,
29.0516165172379));
#178961=CARTESIAN_POINT('Ctrl Pts',(-3.51996838710042,7.32321719712816,
29.0593517021486));
#178962=CARTESIAN_POINT('Ctrl Pts',(-3.69814969249814,7.23757279449892,
29.067084495149));
#178963=CARTESIAN_POINT('Ctrl Pts',(-3.87327101813675,7.14538897388429,
29.0748172881494));
#178964=CARTESIAN_POINT('Ctrl Pts',(-4.04481941675133,7.04692297732645,
29.0825500811498));
#178965=CARTESIAN_POINT('Ctrl Pts',(-4.21634524754578,6.94846993433108,
29.090281856873));
#178966=CARTESIAN_POINT('Ctrl Pts',(-4.3842987816045,6.84373653803983,29.0980136325962));
#178967=CARTESIAN_POINT('Ctrl Pts',(-4.54819242409716,6.73302556328767,
29.1057454083193));
#178968=CARTESIAN_POINT('Ctrl Pts',(-4.71214471220984,6.62227497312603,
29.1134799506829));
#178969=CARTESIAN_POINT('Ctrl Pts',(-4.87203391087088,6.50554272554384,
29.1212144930466));
#178970=CARTESIAN_POINT('Ctrl Pts',(-5.02740159129819,6.38317482153767,
29.1289490354102));
#178971=CARTESIAN_POINT('Ctrl Pts',(-5.18279551159434,6.26078625095693,
29.1366848840517));
#178972=CARTESIAN_POINT('Ctrl Pts',(-5.33366611915968,6.13276035210405,
29.1444207326933));
#178973=CARTESIAN_POINT('Ctrl Pts',(-5.47958864309167,5.9994829664731,29.1521565813349));
#178974=CARTESIAN_POINT('Ctrl Pts',(-5.62563056744023,5.8660965272503,29.1598987597981));
#178975=CARTESIAN_POINT('Ctrl Pts',(-5.76671606303793,5.72745026007294,
29.1676409382614));
#178976=CARTESIAN_POINT('Ctrl Pts',(-5.90245710552311,5.58396701995631,
29.1753831167246));
#178977=CARTESIAN_POINT('Ctrl Pts',(-6.01601324878065,5.46393402867057,
29.1818599487173));
#178978=CARTESIAN_POINT('Ctrl Pts',(-6.12582973275853,5.34051664665965,
29.1883367807101));
#178979=CARTESIAN_POINT('Ctrl Pts',(-6.23170143661774,5.21397974366572,
29.1948136127028));
#178980=CARTESIAN_POINT('Ctrl Pts',(-6.3853236532053,5.03037185969414,29.2042116411742));
#178981=CARTESIAN_POINT('Ctrl Pts',(-6.53072766535562,4.8400916997463,29.2136096696457));
#178982=CARTESIAN_POINT('Ctrl Pts',(-6.66742265689711,4.64383060380061,
29.2230076981171));
#178983=CARTESIAN_POINT('Ctrl Pts',(-6.8043121539704,4.44729024474212,29.2324190991965));
#178984=CARTESIAN_POINT('Ctrl Pts',(-6.93246782083146,4.24475195686816,
29.2418305002759));
#178985=CARTESIAN_POINT('Ctrl Pts',(-7.05144140319556,4.03693716817582,
29.2512419013552));
#178986=CARTESIAN_POINT('Ctrl Pts',(-7.17023585075172,3.82943527972167,
29.2606391319819));
#178987=CARTESIAN_POINT('Ctrl Pts',(-7.27987583040652,3.61667280239571,
29.2700363626085));
#178988=CARTESIAN_POINT('Ctrl Pts',(-7.37995972155779,3.39939436821982,
29.2794335932351));
#178989=CARTESIAN_POINT('Ctrl Pts',(-7.47979116380052,3.18266399130795,
29.2888071205406));
#178990=CARTESIAN_POINT('Ctrl Pts',(-7.57011462987414,2.96144043637393,
29.2981806478461));
#178991=CARTESIAN_POINT('Ctrl Pts',(-7.65057629621841,2.73648860736546,
29.3075541751515));
#178992=CARTESIAN_POINT('Ctrl Pts',(-7.73051544922783,2.51299760232069,
29.3168668313213));
#178993=CARTESIAN_POINT('Ctrl Pts',(-7.80072043542531,2.28582662313103,
29.3261794874911));
#178994=CARTESIAN_POINT('Ctrl Pts',(-7.86088899879242,2.05575088742881,
29.3354921436608));
#178995=CARTESIAN_POINT('Ctrl Pts',(-7.89963083983558,1.90760778608734,
29.3414884551037));
#178996=CARTESIAN_POINT('Ctrl Pts',(-7.93421255934564,1.75826090109098,
29.3474847665466));
#178997=CARTESIAN_POINT('Ctrl Pts',(-7.9645635351637,1.60792265263002,29.3534810779894));
#178998=CARTESIAN_POINT('Ctrl Pts',(-8.00286805180554,1.41818793126225,
29.3610487362034));
#178999=CARTESIAN_POINT('Ctrl Pts',(-8.03441562384965,1.22694884437615,
29.3686163944174));
#179000=CARTESIAN_POINT('Ctrl Pts',(-8.05909331398302,1.03474756294192,
29.3761840526314));
#179001=CARTESIAN_POINT('Ctrl Pts',(-8.08376417130756,0.842599498587761,
29.3837496154969));
#179002=CARTESIAN_POINT('Ctrl Pts',(-8.10156888475985,0.649490134078745,
29.3913151783624));
#179003=CARTESIAN_POINT('Ctrl Pts',(-8.11244591473116,0.455970221683052,
29.3988807412279));
#179004=CARTESIAN_POINT('Ctrl Pts',(-8.12332199177175,0.262467263462304,
29.4064456412785));
#179005=CARTESIAN_POINT('Ctrl Pts',(-8.12727157357842,0.0685541960751146,
29.4140105413291));
#179006=CARTESIAN_POINT('Ctrl Pts',(-8.12428512635025,-0.12521480848541,
29.4215754413797));
#179007=CARTESIAN_POINT('Ctrl Pts',(-8.12129721339224,-0.3190789136761,
29.4291440542365));
#179008=CARTESIAN_POINT('Ctrl Pts',(-8.11136647299121,-0.51279844657361,
29.4367126670933));
#179009=CARTESIAN_POINT('Ctrl Pts',(-8.09453551293872,-0.705820368276455,
29.4442812799501));
#179010=CARTESIAN_POINT('Ctrl Pts',(-8.07770080997662,-0.898885214661145,
29.4518515759333));
#179011=CARTESIAN_POINT('Ctrl Pts',(-8.05396287399185,-1.09125177555957,
29.4594218719166));
#179012=CARTESIAN_POINT('Ctrl Pts',(-8.02341599667671,-1.28237409002689,
29.4669921678998));
#179013=CARTESIAN_POINT('Ctrl Pts',(-7.99283816666645,-1.47369006588444,
29.474570134751));
#179014=CARTESIAN_POINT('Ctrl Pts',(-7.95543768024925,-1.66375891510597,
29.4821481016022));
#179015=CARTESIAN_POINT('Ctrl Pts',(-7.91135977901552,-1.85204589831771,
29.4897260684535));
#179016=CARTESIAN_POINT('Ctrl Pts',(-7.8678856893714,-2.03775358760998,
29.4972002267276));
#179017=CARTESIAN_POINT('Ctrl Pts',(-7.81791611631227,-2.22172761022478,
29.5046743850016));
#179018=CARTESIAN_POINT('Ctrl Pts',(-7.76163701836414,-2.40347214622084,
29.5121485432757));
#179019=CARTESIAN_POINT('Ctrl Pts',(-7.70083495496687,-2.59982289103774,
29.5202233749946));
#179020=CARTESIAN_POINT('Ctrl Pts',(-7.63253904220119,-2.79399077746816,
29.5282982067135));
#179021=CARTESIAN_POINT('Ctrl Pts',(-7.55692786463111,-2.98538587309277,
29.5363730384324));
#179022=CARTESIAN_POINT('Ctrl Pts',(-7.48136671129449,-3.17665434202997,
29.5444425278556));
#179023=CARTESIAN_POINT('Ctrl Pts',(-7.39850006015966,-3.3651533845707,
29.5525120172788));
#179024=CARTESIAN_POINT('Ctrl Pts',(-7.30855578831577,-3.55030982473024,
29.5605815067021));
#179025=CARTESIAN_POINT('Ctrl Pts',(-7.21865877025028,-3.73536898975248,
29.5686467566795));
#179026=CARTESIAN_POINT('Ctrl Pts',(-7.12169168501351,-3.91708877020396,
29.5767120066569));
#179027=CARTESIAN_POINT('Ctrl Pts',(-7.01793009246643,-4.09491694418265,
29.5847772566343));
#179028=CARTESIAN_POINT('Ctrl Pts',(-6.91420889215014,-4.27267589335023,
29.5928393669776));
#179029=CARTESIAN_POINT('Ctrl Pts',(-6.80369861926473,-4.44654598430514,
29.6009014773209));
#179030=CARTESIAN_POINT('Ctrl Pts',(-6.6867205455098,-4.61599999011667,
29.6089635876641));
#179031=CARTESIAN_POINT('Ctrl Pts',(-6.56977210215631,-4.78541107343805,
29.6170236558848));
#179032=CARTESIAN_POINT('Ctrl Pts',(-6.44635930570642,-4.95040804246024,
29.6250837241055));
#179033=CARTESIAN_POINT('Ctrl Pts',(-6.31684682282501,-5.11049251828682,
29.6331437923262));
#179034=CARTESIAN_POINT('Ctrl Pts',(-6.18539404979508,-5.27297529831132,
29.6413246123897));
#179035=CARTESIAN_POINT('Ctrl Pts',(-6.04765755625816,-5.43039694305914,
29.6495054324531));
#179036=CARTESIAN_POINT('Ctrl Pts',(-5.90406171228676,-5.58227040369862,
29.6576862525165));
#179037=CARTESIAN_POINT('Ctrl Pts',(-5.76257165986339,-5.73191668393412,
29.6657471032182));
#179038=CARTESIAN_POINT('Ctrl Pts',(-5.61539316654647,-5.87617616748634,
29.67380795392));
#179039=CARTESIAN_POINT('Ctrl Pts',(-5.46297025584037,-6.01461915222431,
29.6818688046217));
#179040=CARTESIAN_POINT('Ctrl Pts',(-5.31052206718053,-6.1530850964724,
29.6899309921422));
#179041=CARTESIAN_POINT('Ctrl Pts',(-5.15282796097336,-6.28573240484384,
29.6979931796627));
#179042=CARTESIAN_POINT('Ctrl Pts',(-4.99036650953078,-6.41217043309467,
29.7060553671832));
#179043=CARTESIAN_POINT('Ctrl Pts',(-4.82785798925588,-6.53864509336066,
29.7141198905055));
#179044=CARTESIAN_POINT('Ctrl Pts',(-4.66057961893391,-6.65890669085907,
29.7221844138278));
#179045=CARTESIAN_POINT('Ctrl Pts',(-4.48904099831805,-6.77260647593817,
29.7302489371502));
#179046=CARTESIAN_POINT('Ctrl Pts',(-4.31314141460697,-6.88919680872534,
29.738518481875));
#179047=CARTESIAN_POINT('Ctrl Pts',(-4.13276239494973,-6.99888707914173,
29.7467880265999));
#179048=CARTESIAN_POINT('Ctrl Pts',(-3.94848241085994,-7.1013501683574,
29.7550575713248));
#179049=CARTESIAN_POINT('Ctrl Pts',(-3.76852833855681,-7.20140797038181,
29.7631329912174));
#179050=CARTESIAN_POINT('Ctrl Pts',(-3.58485469236599,-7.29457397854348,
29.77120841111));
#179051=CARTESIAN_POINT('Ctrl Pts',(-3.39802282682166,-7.38059133341624,
29.7792838310027));
#179052=CARTESIAN_POINT('Ctrl Pts',(-3.20445409092812,-7.46971034209882,
29.7876504381436));
#179053=CARTESIAN_POINT('Ctrl Pts',(-3.00749549223416,-7.55115543137243,
29.7960170452846));
#179054=CARTESIAN_POINT('Ctrl Pts',(-2.80779156485647,-7.62469632777731,
29.8043836524256));
#179055=CARTESIAN_POINT('Ctrl Pts',(-2.60808763747882,-7.69823722418218,
29.8127502595666));
#179056=CARTESIAN_POINT('Ctrl Pts',(-2.4056387498038,-7.7638738474689,29.8211168667075));
#179057=CARTESIAN_POINT('Ctrl Pts',(-2.20110462445034,-7.82143375569488,
29.8294834738485));
#179058=CARTESIAN_POINT('Ctrl Pts',(-2.00362718461449,-7.87700777442652,
29.8375614224816));
#179059=CARTESIAN_POINT('Ctrl Pts',(-1.80382204229118,-7.92516113503516,
29.8456393711146));
#179060=CARTESIAN_POINT('Ctrl Pts',(-1.60227339677148,-7.96570194800799,
29.8537173197477));
#179061=CARTESIAN_POINT('Ctrl Pts',(-1.40097140586131,-8.0061931472592,
29.8617853826122));
#179062=CARTESIAN_POINT('Ctrl Pts',(-1.19793047197389,-8.03909030748399,
29.8698534454767));
#179063=CARTESIAN_POINT('Ctrl Pts',(-0.993749792458142,-8.0642512927419,
29.8779215083412));
#179064=CARTESIAN_POINT('Ctrl Pts',(-0.789793851398478,-8.08938458369987,
29.885980690816));
#179065=CARTESIAN_POINT('Ctrl Pts',(-0.584700977059645,-8.10679863641572,
29.8940398732909));
#179066=CARTESIAN_POINT('Ctrl Pts',(-0.379081006085367,-8.11640222964124,
29.9020990557657));
#179067=CARTESIAN_POINT('Ctrl Pts',(-0.173725146775017,-8.12599348738702,
29.9101478865024));
#179068=CARTESIAN_POINT('Ctrl Pts',(0.0321561446039651,-8.12779428496848,
29.9181967172391));
#179069=CARTESIAN_POINT('Ctrl Pts',(0.237947405400235,-8.12176511570996,
29.9262455479758));
#179070=CARTESIAN_POINT('Ctrl Pts',(0.443583006615233,-8.11574050688788,
29.9342882906133));
#179071=CARTESIAN_POINT('Ctrl Pts',(0.649128398758211,-8.10189774556756,
29.9423310332508));
#179072=CARTESIAN_POINT('Ctrl Pts',(0.853966240181079,-8.08024932926769,
29.9503737758882));
#179073=CARTESIAN_POINT('Ctrl Pts',(1.05863723347137,-8.05861854641782,
29.9584099674091));
#179074=CARTESIAN_POINT('Ctrl Pts',(1.26260151263647,-8.02919482440692,
29.9664461589299));
#179075=CARTESIAN_POINT('Ctrl Pts',(1.46524469802764,-7.9920426386126,29.9744823504507));
#179076=CARTESIAN_POINT('Ctrl Pts',(1.58013520487318,-7.97097884883803,
29.9790385466788));
#179077=CARTESIAN_POINT('Ctrl Pts',(1.69460110762108,-7.94743174291968,
29.983594742907));
#179078=CARTESIAN_POINT('Ctrl Pts',(1.80853123421068,-7.92142047472449,
29.9881509391351));
#179079=CARTESIAN_POINT('Ctrl Pts',(2.00948858316323,-7.8755401122965,29.9961874536438));
#179080=CARTESIAN_POINT('Ctrl Pts',(2.20861949664047,-7.82202660687131,
30.0042239681525));
#179081=CARTESIAN_POINT('Ctrl Pts',(2.40533228911578,-7.76106076135454,
30.0122604826611));
#179082=CARTESIAN_POINT('Ctrl Pts',(2.60216391569675,-7.70005808639909,
30.0203018520245));
#179083=CARTESIAN_POINT('Ctrl Pts',(2.79657420525973,-7.63159418320123,
30.0283432213878));
#179084=CARTESIAN_POINT('Ctrl Pts',(2.98798925228111,-7.55589887377753,
30.0363845907511));
#179085=CARTESIAN_POINT('Ctrl Pts',(3.17954333713474,-7.48014858167667,
30.0444318011107));
#179086=CARTESIAN_POINT('Ctrl Pts',(3.36809754543241,-7.39715651978964,
30.0524790114702));
#179087=CARTESIAN_POINT('Ctrl Pts',(3.55309991214548,-7.30719977671418,
30.0605262218297));
#179088=CARTESIAN_POINT('Ctrl Pts',(3.7383749591358,-7.21711044382337,30.0685852932027));
#179089=CARTESIAN_POINT('Ctrl Pts',(3.92008741688246,-7.12003605088192,
30.0766443645756));
#179090=CARTESIAN_POINT('Ctrl Pts',(4.09771027214318,-7.0162994582666,30.0847034359486));
#179091=CARTESIAN_POINT('Ctrl Pts',(4.27547688629555,-6.91247890653715,
30.0927690299234));
#179092=CARTESIAN_POINT('Ctrl Pts',(4.44914702680273,-6.80198556403027,
30.1008346238982));
#179093=CARTESIAN_POINT('Ctrl Pts',(4.61822371020947,-6.6851849132959,30.108900217873));
#179094=CARTESIAN_POINT('Ctrl Pts',(4.78756588263793,-6.56820085885455,
30.1169784766731));
#179095=CARTESIAN_POINT('Ctrl Pts',(4.95229992811656,-6.44488988889585,
30.1250567354732));
#179096=CARTESIAN_POINT('Ctrl Pts',(5.11196154100573,-6.31565806276577,
30.1331349942733));
#179097=CARTESIAN_POINT('Ctrl Pts',(5.20210948782359,-6.24269134535427,
30.1376961309893));
#179098=CARTESIAN_POINT('Ctrl Pts',(5.29064102548129,-6.16783777771843,
30.1422572677054));
#179099=CARTESIAN_POINT('Ctrl Pts',(5.37747790963913,-6.09117549360082,
30.1468184044214));
#179100=CARTESIAN_POINT('Ctrl Pts',(5.52883585597059,-5.95755202244966,
30.1547685317547));
#179101=CARTESIAN_POINT('Ctrl Pts',(5.6753673482983,-5.81814516238551,30.1627186590879));
#179102=CARTESIAN_POINT('Ctrl Pts',(5.81661134720278,-5.6733341165572,30.1706687864212));
#179103=CARTESIAN_POINT('Ctrl Pts',(5.95772227539224,-5.52865950207861,
30.1786114236725));
#179104=CARTESIAN_POINT('Ctrl Pts',(6.09355540705588,-5.37859108581603,
30.1865540609238));
#179105=CARTESIAN_POINT('Ctrl Pts',(6.22368390162456,-5.2235472865821,30.194496698175));
#179106=CARTESIAN_POINT('Ctrl Pts',(6.35371169464857,-5.06862346990947,
30.2024331889183));
#179107=CARTESIAN_POINT('Ctrl Pts',(6.4780434366407,-4.90873219855639,30.2103696796615));
#179108=CARTESIAN_POINT('Ctrl Pts',(6.59628989787571,-4.7443278918813,30.2183061704047));
#179109=CARTESIAN_POINT('Ctrl Pts',(6.71945343540229,-4.57308711407514,
30.226572686504));
#179110=CARTESIAN_POINT('Ctrl Pts',(6.83601451609805,-4.39695019710985,
30.2348392026033));
#179111=CARTESIAN_POINT('Ctrl Pts',(6.94557959981183,-4.21646908979275,
30.2431057187026));
#179112=CARTESIAN_POINT('Ctrl Pts',(7.05066059802903,-4.04337439325814,
30.2510339174868));
#179113=CARTESIAN_POINT('Ctrl Pts',(7.1493066296484,-3.86628431438256,30.258962116271));
#179114=CARTESIAN_POINT('Ctrl Pts',(7.2412145404669,-3.68571560777968,30.2668903150552));
#179115=CARTESIAN_POINT('Ctrl Pts',(7.33310268708142,-3.50518573131358,
30.2748168089314));
#179116=CARTESIAN_POINT('Ctrl Pts',(7.41825544997759,-3.32117901450807,
30.2827433028075));
#179117=CARTESIAN_POINT('Ctrl Pts',(7.49641562669018,-3.13423679935248,
30.2906697966837));
#179118=CARTESIAN_POINT('Ctrl Pts',(7.57457091042752,-2.94730628713398,
30.2985957943463));
#179119=CARTESIAN_POINT('Ctrl Pts',(7.64573435264783,-2.75744095010262,
30.3065217920089));
#179120=CARTESIAN_POINT('Ctrl Pts',(7.70969674304275,-2.56520246624238,
30.3144477896715));
#179121=CARTESIAN_POINT('Ctrl Pts',(7.773664879282,-2.37294671329017,30.3223744993392));
#179122=CARTESIAN_POINT('Ctrl Pts',(7.8304305701621,-2.17831770466007,30.3303012090069));
#179123=CARTESIAN_POINT('Ctrl Pts',(7.87983423502881,-1.98189303217099,
30.3382279186747));
#179124=CARTESIAN_POINT('Ctrl Pts',(7.92926493333466,-1.7853608770803,30.3461589657984));
#179125=CARTESIAN_POINT('Ctrl Pts',(7.97132547621662,-1.5870314181205,30.3540900129221));
#179126=CARTESIAN_POINT('Ctrl Pts',(8.0059070414091,-1.38749414658807,30.3620210600459));
#179127=CARTESIAN_POINT('Ctrl Pts',(8.04049966217458,-1.18789308387503,
30.3699546426902));
#179128=CARTESIAN_POINT('Ctrl Pts',(8.06760848826027,-0.987083767686729,
30.3778882253345));
#179129=CARTESIAN_POINT('Ctrl Pts',(8.08717641414289,-0.785662274155305,
30.3858218079788));
#179130=CARTESIAN_POINT('Ctrl Pts',(8.10675980185596,-0.584081625024089,
30.3937616594382));
#179131=CARTESIAN_POINT('Ctrl Pts',(8.1187903637721,-0.381888164136896,
30.4017015108977));
#179132=CARTESIAN_POINT('Ctrl Pts',(8.12326304575953,-0.17968041601016,
30.4096413623571));
#179133=CARTESIAN_POINT('Ctrl Pts',(8.12458895121676,-0.119736883809696,
30.4119950938339));
#179134=CARTESIAN_POINT('Ctrl Pts',(8.12525101991889,-0.0597920845778729,
30.4143488253108));
#179135=CARTESIAN_POINT('Ctrl Pts',(8.12524999882064,0.000138438281265886,
30.4167025567876));
#179136=CARTESIAN_POINT('',(8.12479782686936,-0.00219746833155191,26.4167025567876));
#179137=CARTESIAN_POINT('Ctrl Pts',(8.12525,8.95881079881578E-13,26.4167025567876));
#179138=CARTESIAN_POINT('Ctrl Pts',(8.12524999999975,2.24624642433496,26.5047001499288));
#179139=CARTESIAN_POINT('Ctrl Pts',(7.14398562317555,4.4753524975352,26.59269774307));
#179140=CARTESIAN_POINT('Ctrl Pts',(3.83078204044869,7.50935546634392,26.7686929293524));
#179141=CARTESIAN_POINT('Ctrl Pts',(1.52412477697682,8.29110090552147,26.8566905224936));
#179142=CARTESIAN_POINT('Ctrl Pts',(-2.95101623932607,7.89663306204406,
27.032685708776));
#179143=CARTESIAN_POINT('Ctrl Pts',(-5.08535169588768,6.7234298308576,27.1206833019172));
#179144=CARTESIAN_POINT('Ctrl Pts',(-7.81671694684414,3.15661951052912,
27.2966784881996));
#179145=CARTESIAN_POINT('Ctrl Pts',(-8.39290461146703,0.790229551553876,
27.3846760813408));
#179146=CARTESIAN_POINT('Ctrl Pts',(-7.60701611462477,-3.63299000730427,
27.5606712676232));
#179147=CARTESIAN_POINT('Ctrl Pts',(-6.25093680401351,-5.65606750610023,
27.6486688607644));
#179148=CARTESIAN_POINT('Ctrl Pts',(-2.45807268688558,-8.06369575488316,
27.8246640470468));
#179149=CARTESIAN_POINT('Ctrl Pts',(-0.050229951045439,-8.42987470330085,
27.912661640188));
#179150=CARTESIAN_POINT('Ctrl Pts',(4.2868996088098,-7.2586363943457,28.0886568264704));
#179151=CARTESIAN_POINT('Ctrl Pts',(6.18309125557144,-5.73015646266396,
28.1766544196116));
#179152=CARTESIAN_POINT('Ctrl Pts',(7.8105055920291,-2.5864071380026,28.3153355274311));
#179153=CARTESIAN_POINT('Ctrl Pts',(8.12525000000015,-1.29375883538096,
28.3660190421094));
#179154=CARTESIAN_POINT('Ctrl Pts',(8.12525,9.51624341237972E-13,28.4167025567876));
#179155=CARTESIAN_POINT('',(8.12465437257904,0.000424865304964707,24.4167025657623));
#179156=CARTESIAN_POINT('Ctrl Pts',(8.12465437257904,0.000424865304964707,
24.4167025657623));
#179157=CARTESIAN_POINT('Ctrl Pts',(8.12471506055511,0.154179418475467,
24.4227315952114));
#179158=CARTESIAN_POINT('Ctrl Pts',(8.08253234226184,1.65664906305814,24.4816497797562));
#179159=CARTESIAN_POINT('Ctrl Pts',(7.20239531903253,4.46233054468966,24.5934571193965));
#179160=CARTESIAN_POINT('Ctrl Pts',(4.17773714921789,7.36911953511172,24.7521245846828));
#179161=CARTESIAN_POINT('Ctrl Pts',(0.172450800896666,8.45505245510799,
24.9107920499693));
#179162=CARTESIAN_POINT('Ctrl Pts',(-5.30273476857889,7.22585834388332,
25.1223486703512));
#179163=CARTESIAN_POINT('Ctrl Pts',(-8.68429813962363,2.18133867002514,
25.3339052907331));
#179164=CARTESIAN_POINT('Ctrl Pts',(-7.77043274392747,-3.32666936346071,
25.545461911115));
#179165=CARTESIAN_POINT('Ctrl Pts',(-4.41553899415244,-7.78962694628804,
25.757018531497));
#179166=CARTESIAN_POINT('Ctrl Pts',(1.56871213603083,-8.82446412344869,
25.9685751518788));
#179167=CARTESIAN_POINT('Ctrl Pts',(6.23719048967391,-5.71096367462437,
26.1801317722608));
#179168=CARTESIAN_POINT('Ctrl Pts',(7.88015377287066,-2.68210296929991,
26.3118778555319));
#179169=CARTESIAN_POINT('Ctrl Pts',(8.12460569558809,-0.666438545426924,
26.3907347837075));
#179170=CARTESIAN_POINT('Ctrl Pts',(8.12479782686936,-0.00219746833155191,
26.4167025567876));
#179171=CARTESIAN_POINT('',(8.12525,8.99861782310829E-13,22.4167025567876));
#179172=CARTESIAN_POINT('Ctrl Pts',(8.12524999843797,0.000159322666138746,
22.4167025567876));
#179173=CARTESIAN_POINT('Ctrl Pts',(8.12524613254614,0.19731480844615,22.4244104961116));
#179174=CARTESIAN_POINT('Ctrl Pts',(8.11806209000327,0.39450754566343,22.4321184354356));
#179175=CARTESIAN_POINT('Ctrl Pts',(8.10371576501125,0.591166949691999,
22.4398263747596));
#179176=CARTESIAN_POINT('Ctrl Pts',(8.08936474420554,0.787890723928413,
22.4475368370327));
#179177=CARTESIAN_POINT('Ctrl Pts',(8.06784677763421,0.984080460747862,
22.4552472993057));
#179178=CARTESIAN_POINT('Ctrl Pts',(8.03923178276477,1.17916915897796,22.4629577615788));
#179179=CARTESIAN_POINT('Ctrl Pts',(8.01061268339087,1.37428584052358,22.4706693298323));
#179180=CARTESIAN_POINT('Ctrl Pts',(7.97489458651551,1.56830081786643,22.4783808980859));
#179181=CARTESIAN_POINT('Ctrl Pts',(7.93219875068048,1.76065628167539,22.4860924663395));
#179182=CARTESIAN_POINT('Ctrl Pts',(7.88946783566493,1.95316978600304,22.4938103704684));
#179183=CARTESIAN_POINT('Ctrl Pts',(7.83974781083228,2.14402070647978,22.5015282745973));
#179184=CARTESIAN_POINT('Ctrl Pts',(7.78321038226485,2.33266450821901,22.5092461787263));
#179185=CARTESIAN_POINT('Ctrl Pts',(7.73062827977641,2.50811089777367,22.5164241427085));
#179186=CARTESIAN_POINT('Ctrl Pts',(7.67214987165433,2.68164812048831,22.5236021066907));
#179187=CARTESIAN_POINT('Ctrl Pts',(7.60795081508275,2.85285330113233,22.5307800706729));
#179188=CARTESIAN_POINT('Ctrl Pts',(7.52389570377249,3.07701034150697,22.5401780991444));
#179189=CARTESIAN_POINT('Ctrl Pts',(7.42998474518825,3.29730468523387,22.549576127616));
#179190=CARTESIAN_POINT('Ctrl Pts',(7.32657761269766,3.51296855203934,22.5589741560875));
#179191=CARTESIAN_POINT('Ctrl Pts',(7.2230233405123,3.72893929047707,22.568385557167));
#179192=CARTESIAN_POINT('Ctrl Pts',(7.10994588178427,3.94026633875174,22.5777969582464));
#179193=CARTESIAN_POINT('Ctrl Pts',(6.98775206573189,4.14620412309376,22.5872083593259));
#179194=CARTESIAN_POINT('Ctrl Pts',(6.86574223309334,4.35183183334347,22.5966055899526));
#179195=CARTESIAN_POINT('Ctrl Pts',(6.73464349860567,4.55208646802926,22.6060028205793));
#179196=CARTESIAN_POINT('Ctrl Pts',(6.59490586401416,4.74625159544789,22.615400051206));
#179197=CARTESIAN_POINT('Ctrl Pts',(6.45552069986431,4.93992696598452,22.6247735785116));
#179198=CARTESIAN_POINT('Ctrl Pts',(6.30754016686787,5.12754346748758,22.6341471058171));
#179199=CARTESIAN_POINT('Ctrl Pts',(6.15145546131005,5.30841626759043,22.6435206331227));
#179200=CARTESIAN_POINT('Ctrl Pts',(5.99638436066216,5.48811449035336,22.6528332892925));
#179201=CARTESIAN_POINT('Ctrl Pts',(5.83331401469013,5.66115626605527,22.6621459454623));
#179202=CARTESIAN_POINT('Ctrl Pts',(5.66277000741065,5.82689655010885,22.6714586016321));
#179203=CARTESIAN_POINT('Ctrl Pts',(5.55295869647669,5.93361479929755,22.6774549130745));
#179204=CARTESIAN_POINT('Ctrl Pts',(5.44004974799199,6.03730644182918,22.6834512245169));
#179205=CARTESIAN_POINT('Ctrl Pts',(5.32419319158091,6.1378053424024,22.6894475359593));
#179206=CARTESIAN_POINT('Ctrl Pts',(5.17797616646616,6.2646402037544,22.6970151941733));
#179207=CARTESIAN_POINT('Ctrl Pts',(5.02712019411757,6.3863370125112,22.7045828523873));
#179208=CARTESIAN_POINT('Ctrl Pts',(4.87204137709522,6.50253030614792,22.7121505106013));
#179209=CARTESIAN_POINT('Ctrl Pts',(4.71700549860974,6.61869142795021,22.7197160734668));
#179210=CARTESIAN_POINT('Ctrl Pts',(4.55774939586706,6.72935184644465,22.7272816363322));
#179211=CARTESIAN_POINT('Ctrl Pts',(4.39472196805478,6.83418659285775,22.7348471991977));
#179212=CARTESIAN_POINT('Ctrl Pts',(4.23170882298712,6.93901215475553,22.7424120992483));
#179213=CARTESIAN_POINT('Ctrl Pts',(4.06492532018506,7.03801286229386,22.7499769992989));
#179214=CARTESIAN_POINT('Ctrl Pts',(3.89484896389969,7.13090731330239,22.7575418993495));
#179215=CARTESIAN_POINT('Ctrl Pts',(3.7246891351898,7.22384735633334,22.7651105122063));
#179216=CARTESIAN_POINT('Ctrl Pts',(3.55123354591468,7.31067497624838,22.7726791250631));
#179217=CARTESIAN_POINT('Ctrl Pts',(3.37498441075564,7.39115469934545,22.7802477379199));
#179218=CARTESIAN_POINT('Ctrl Pts',(3.19869608088749,7.47165231971807,22.7878180339031));
#179219=CARTESIAN_POINT('Ctrl Pts',(3.01961330681129,7.54579908893877,22.7953883298864));
#179220=CARTESIAN_POINT('Ctrl Pts',(2.83825761526305,7.61340799326434,22.8029586258696));
#179221=CARTESIAN_POINT('Ctrl Pts',(2.656718158698,7.68108540468407,22.8105365927208));
#179222=CARTESIAN_POINT('Ctrl Pts',(2.47290153176808,7.74221159786422,22.818114559572));
#179223=CARTESIAN_POINT('Ctrl Pts',(2.28734460604277,7.79664942239338,22.8256925264233));
#179224=CARTESIAN_POINT('Ctrl Pts',(2.1043295758947,7.85034151746586,22.8331666846974));
#179225=CARTESIAN_POINT('Ctrl Pts',(1.91962196643571,7.89752730173872,22.8406408429716));
#179226=CARTESIAN_POINT('Ctrl Pts',(1.73374485027924,7.93812423413934,22.8481150012457));
#179227=CARTESIAN_POINT('Ctrl Pts',(1.53292940346886,7.98198380807579,22.8561898329646));
#179228=CARTESIAN_POINT('Ctrl Pts',(1.33032021960521,8.01824699099574,22.8642646646835));
#179229=CARTESIAN_POINT('Ctrl Pts',(1.12651862753549,8.04677844508692,22.8723394964024));
#179230=CARTESIAN_POINT('Ctrl Pts',(0.922851870271271,8.07529102281397,
22.8804089858256));
#179231=CARTESIAN_POINT('Ctrl Pts',(0.717994590687884,8.09608202834019,
22.8884784752488));
#179232=CARTESIAN_POINT('Ctrl Pts',(0.512557829620091,8.10906727273828,
22.8965479646721));
#179233=CARTESIAN_POINT('Ctrl Pts',(0.307228998306923,8.12204569511371,
22.9046132146495));
#179234=CARTESIAN_POINT('Ctrl Pts',(0.101321608117274,8.12722651473287,
22.9126784646269));
#179235=CARTESIAN_POINT('Ctrl Pts',(-0.104548033950805,8.12457735953674,
22.9207437146043));
#179236=CARTESIAN_POINT('Ctrl Pts',(-0.310337535247146,8.12192923560166,
22.9288058249476));
#179237=CARTESIAN_POINT('Ctrl Pts',(-0.516089001426615,8.11145722018747,
22.9368679352909));
#179238=CARTESIAN_POINT('Ctrl Pts',(-0.721185346747057,8.0931810345585,
22.9449300456341));
#179239=CARTESIAN_POINT('Ctrl Pts',(-0.926229741416818,8.07490947826475,
22.9529901138548));
#179240=CARTESIAN_POINT('Ctrl Pts',(-1.1306190309936,8.04883772304286,22.9610501820755));
#179241=CARTESIAN_POINT('Ctrl Pts',(-1.33373984546315,8.01503746635809,
22.9691102502962));
#179242=CARTESIAN_POINT('Ctrl Pts',(-1.53990371266804,7.98073083141845,
22.9772910703597));
#179243=CARTESIAN_POINT('Ctrl Pts',(-1.74476046205535,7.93846230746238,
22.9854718904231));
#179244=CARTESIAN_POINT('Ctrl Pts',(-1.9476771592851,7.88836112546194,22.9936527104865));
#179245=CARTESIAN_POINT('Ctrl Pts',(-2.14761814179938,7.83899466281469,
23.0017135611882));
#179246=CARTESIAN_POINT('Ctrl Pts',(-2.34567527301639,7.78202379074947,
23.00977441189));
#179247=CARTESIAN_POINT('Ctrl Pts',(-2.54125583220034,7.71762310286061,
23.0178352625917));
#179248=CARTESIAN_POINT('Ctrl Pts',(-2.73686882664154,7.65321173470327,
23.0258974501122));
#179249=CARTESIAN_POINT('Ctrl Pts',(-2.93000412883017,7.58136819220191,
23.0339596376327));
#179250=CARTESIAN_POINT('Ctrl Pts',(-3.12008597723112,7.50231637943814,
23.0420218251532));
#179251=CARTESIAN_POINT('Ctrl Pts',(-3.31022289673115,7.42324166353947,
23.0500863484755));
#179252=CARTESIAN_POINT('Ctrl Pts',(-3.49730430546083,7.33695463370158,
23.0581508717979));
#179253=CARTESIAN_POINT('Ctrl Pts',(-3.68077560478952,7.24372683842277,
23.0662153951202));
#179254=CARTESIAN_POINT('Ctrl Pts',(-3.86891122730385,7.14812894728343,
23.0744849398451));
#179255=CARTESIAN_POINT('Ctrl Pts',(-4.05325043723003,7.04523287427622,
23.0827544845699));
#179256=CARTESIAN_POINT('Ctrl Pts',(-4.23322351628943,6.93538075549094,
23.0910240292948));
#179257=CARTESIAN_POINT('Ctrl Pts',(-4.40897178673598,6.82810737892651,
23.0990994491874));
#179258=CARTESIAN_POINT('Ctrl Pts',(-4.58055636480016,6.71420107553466,
23.1071748690801));
#179259=CARTESIAN_POINT('Ctrl Pts',(-4.74747710272014,6.5940237125482,23.1152502889727));
#179260=CARTESIAN_POINT('Ctrl Pts',(-4.9204167462837,6.46951293828328,23.1236168961137));
#179261=CARTESIAN_POINT('Ctrl Pts',(-5.08834965723348,6.33827068294546,
23.1319835032547));
#179262=CARTESIAN_POINT('Ctrl Pts',(-5.25075782862163,6.20074429304004,
23.1403501103956));
#179263=CARTESIAN_POINT('Ctrl Pts',(-5.41316600000977,6.06321790313462,
23.1487167175366));
#179264=CARTESIAN_POINT('Ctrl Pts',(-5.57004918046089,5.91940765965785,
23.1570833246776));
#179265=CARTESIAN_POINT('Ctrl Pts',(-5.72093219888789,5.76980262558675,
23.1654499318186));
#179266=CARTESIAN_POINT('Ctrl Pts',(-5.86660956271246,5.62535915404454,
23.1735278804516));
#179267=CARTESIAN_POINT('Ctrl Pts',(-6.0069771118089,5.47523323290718,23.1816058290847));
#179268=CARTESIAN_POINT('Ctrl Pts',(-6.14157997247383,5.31983862576755,
23.1896837777177));
#179269=CARTESIAN_POINT('Ctrl Pts',(-6.27601810657397,5.16463419006776,
23.1977518405822));
#179270=CARTESIAN_POINT('Ctrl Pts',(-6.40470540980992,5.00417415775252,
23.2058199034467));
#179271=CARTESIAN_POINT('Ctrl Pts',(-6.52722290931678,4.83890986220969,
23.2138879663112));
#179272=CARTESIAN_POINT('Ctrl Pts',(-6.6496055557427,4.67382747047254,23.221947148786));
#179273=CARTESIAN_POINT('Ctrl Pts',(-6.76583174964362,4.50395160936267,
23.2300063312609));
#179274=CARTESIAN_POINT('Ctrl Pts',(-6.87552157740191,4.32976796158649,
23.2380655137357));
#179275=CARTESIAN_POINT('Ctrl Pts',(-6.98507051241126,4.1558080466163,23.2461143444724));
#179276=CARTESIAN_POINT('Ctrl Pts',(-7.0880996629979,3.97755164942091,23.2541631752091));
#179277=CARTESIAN_POINT('Ctrl Pts',(-7.18427134143612,3.79551483400074,
23.2622120059459));
#179278=CARTESIAN_POINT('Ctrl Pts',(-7.28037027605087,3.61361571040607,
23.2702547485833));
#179279=CARTESIAN_POINT('Ctrl Pts',(-7.36962193058903,3.42794214622832,
23.2782974912208));
#179280=CARTESIAN_POINT('Ctrl Pts',(-7.45173294182424,3.23903746909964,
23.2863402338582));
#179281=CARTESIAN_POINT('Ctrl Pts',(-7.53377707054975,3.05028666194177,
23.2943764253791));
#179282=CARTESIAN_POINT('Ctrl Pts',(-7.60869203270067,2.85831028048253,
23.3024126168999));
#179283=CARTESIAN_POINT('Ctrl Pts',(-7.67623115236972,2.66367469070243,
23.3104488084207));
#179284=CARTESIAN_POINT('Ctrl Pts',(-7.71452310714555,2.55332416735911,
23.3150050046488));
#179285=CARTESIAN_POINT('Ctrl Pts',(-7.75044499652292,2.44211928009065,
23.3195612008769));
#179286=CARTESIAN_POINT('Ctrl Pts',(-7.78395869918349,2.33016620263571,
23.324117397105));
#179287=CARTESIAN_POINT('Ctrl Pts',(-7.84307234227238,2.13269610121472,
23.3321539116137));
#179288=CARTESIAN_POINT('Ctrl Pts',(-7.89464404251992,1.93305348126937,
23.3401904261224));
#179289=CARTESIAN_POINT('Ctrl Pts',(-7.93853952839887,1.73184229032226,
23.348226940631));
#179290=CARTESIAN_POINT('Ctrl Pts',(-7.9824615315202,1.5305095477893,23.3562683099943));
#179291=CARTESIAN_POINT('Ctrl Pts',(-8.01869800149608,1.32760665236261,
23.3643096793576));
#179292=CARTESIAN_POINT('Ctrl Pts',(-8.04716608221183,1.1237462381692,23.3723510487209));
#179293=CARTESIAN_POINT('Ctrl Pts',(-8.07565484124043,0.919737746222929,
23.3803982590804));
#179294=CARTESIAN_POINT('Ctrl Pts',(-8.09636390961471,0.714770660353516,
23.38844546944));
#179295=CARTESIAN_POINT('Ctrl Pts',(-8.10926237207028,0.509461817435902,
23.3964926797995));
#179296=CARTESIAN_POINT('Ctrl Pts',(-8.12217984593844,0.303850363944689,
23.4045517511724));
#179297=CARTESIAN_POINT('Ctrl Pts',(-8.12726368494022,0.0978964621942852,
23.4126108225453));
#179298=CARTESIAN_POINT('Ctrl Pts',(-8.12453509800826,-0.107782205079918,
23.4206698939183));
#179299=CARTESIAN_POINT('Ctrl Pts',(-8.12180430269702,-0.313627338190728,
23.4287354878931));
#179300=CARTESIAN_POINT('Ctrl Pts',(-8.11124847955766,-0.5191964775084,
23.4368010818679));
#179301=CARTESIAN_POINT('Ctrl Pts',(-8.09294072368294,-0.723877065152807,
23.4448666758427));
#179302=CARTESIAN_POINT('Ctrl Pts',(-8.07460422044872,-0.928879048083216,
23.4529449346428));
#179303=CARTESIAN_POINT('Ctrl Pts',(-8.04849149397113,-1.13298937748313,
23.4610231934428));
#179304=CARTESIAN_POINT('Ctrl Pts',(-8.01472705075418,-1.33560393246244,
23.4691014522429));
#179305=CARTESIAN_POINT('Ctrl Pts',(-7.99566301165002,-1.45000391751123,
23.4736625889591));
#179306=CARTESIAN_POINT('Ctrl Pts',(-7.97416056690779,-1.56392728920816,
23.4782237256753));
#179307=CARTESIAN_POINT('Ctrl Pts',(-7.95024914288382,-1.67726745886728,
23.4827848623915));
#179308=CARTESIAN_POINT('Ctrl Pts',(-7.90785786651976,-1.87820214390952,
23.4908710561237));
#179309=CARTESIAN_POINT('Ctrl Pts',(-7.85780988190975,-2.07769396799896,
23.4989572498559));
#179310=CARTESIAN_POINT('Ctrl Pts',(-7.80022011101215,-2.27513818970665,
23.507043443588));
#179311=CARTESIAN_POINT('Ctrl Pts',(-7.74268170745739,-2.47240630053786,
23.5151224248191));
#179312=CARTESIAN_POINT('Ctrl Pts',(-7.67761501873223,-2.66763014792167,
23.5232014060502));
#179313=CARTESIAN_POINT('Ctrl Pts',(-7.60518575397833,-2.86021628727358,
23.5312803872813));
#179314=CARTESIAN_POINT('Ctrl Pts',(-7.53281120208989,-3.05265694759065,
23.5393532656724));
#179315=CARTESIAN_POINT('Ctrl Pts',(-7.45308527572228,-3.242463577664,23.5474261440635));
#179316=CARTESIAN_POINT('Ctrl Pts',(-7.3662233330471,-3.42905837952235,
23.5554990224546));
#179317=CARTESIAN_POINT('Ctrl Pts',(-7.27941516179569,-3.61553767086075,
23.5635669033732));
#179318=CARTESIAN_POINT('Ctrl Pts',(-7.18547991732006,-3.79880881266836,
23.5716347842919));
#179319=CARTESIAN_POINT('Ctrl Pts',(-7.08468109217274,-3.97831388715244,
23.5797026652105));
#179320=CARTESIAN_POINT('Ctrl Pts',(-6.98393093876615,-4.15773228578064,
23.5877666504706));
#179321=CARTESIAN_POINT('Ctrl Pts',(-6.87632396956717,-4.33338796830507,
23.5958306357307));
#179322=CARTESIAN_POINT('Ctrl Pts',(-6.76216993216977,-4.50474698190244,
23.6038946209907));
#179323=CARTESIAN_POINT('Ctrl Pts',(-6.64642951920311,-4.67848733705319,
23.612070669823));
#179324=CARTESIAN_POINT('Ctrl Pts',(-6.52395887079913,-4.84781042206556,
23.6202467186552));
#179325=CARTESIAN_POINT('Ctrl Pts',(-6.39512741719872,-5.01218843224127,
23.6284227674874));
#179326=CARTESIAN_POINT('Ctrl Pts',(-6.26812197128787,-5.17423661144646,
23.6364829321344));
#179327=CARTESIAN_POINT('Ctrl Pts',(-6.13493504605435,-5.33147871664951,
23.6445430967814));
#179328=CARTESIAN_POINT('Ctrl Pts',(-5.9959625525229,-5.48344058336033,
23.6526032614283));
#179329=CARTESIAN_POINT('Ctrl Pts',(-5.85699677344482,-5.63539510803646,
23.6606630366486));
#179330=CARTESIAN_POINT('Ctrl Pts',(-5.7122461974415,-5.78206966938098,
23.6687228118688));
#179331=CARTESIAN_POINT('Ctrl Pts',(-5.56214532607138,-5.92302515055966,
23.6767825870891));
#179332=CARTESIAN_POINT('Ctrl Pts',(-5.41203312189491,-6.06399127405612,
23.6848429708326));
#179333=CARTESIAN_POINT('Ctrl Pts',(-5.25657004797934,-6.19923723975241,
23.6929033545761));
#179334=CARTESIAN_POINT('Ctrl Pts',(-5.09622601367504,-6.32836218780514,
23.7009637383197));
#179335=CARTESIAN_POINT('Ctrl Pts',(-4.93185127324367,-6.46073306091851,
23.7092267428734));
#179336=CARTESIAN_POINT('Ctrl Pts',(-4.7623472301346,-6.58667091871485,
23.7174897474271));
#179337=CARTESIAN_POINT('Ctrl Pts',(-4.58825462489004,-6.70578907062213,
23.7257527519808));
#179338=CARTESIAN_POINT('Ctrl Pts',(-4.41829137045866,-6.82208182602993,
23.7338197640366));
#179339=CARTESIAN_POINT('Ctrl Pts',(-4.24395504270791,-6.93187456709233,
23.7418867760924));
#179340=CARTESIAN_POINT('Ctrl Pts',(-4.06577688249518,-7.03485223045003,
23.7499537881482));
#179341=CARTESIAN_POINT('Ctrl Pts',(-3.88110531757662,-7.14158274232207,
23.7583147889509));
#179342=CARTESIAN_POINT('Ctrl Pts',(-3.69230696823037,-7.2409919342672,
23.7666757897536));
#179343=CARTESIAN_POINT('Ctrl Pts',(-3.49999990501188,-7.3327817523377,
23.7750367905563));
#179344=CARTESIAN_POINT('Ctrl Pts',(-3.30769284179336,-7.42457157040823,
23.783397791359));
#179345=CARTESIAN_POINT('Ctrl Pts',(-3.11187742065025,-7.50874188779212,
23.7917587921616));
#179346=CARTESIAN_POINT('Ctrl Pts',(-2.91319360868107,-7.5850504652797,
23.8001197929643));
#179347=CARTESIAN_POINT('Ctrl Pts',(-2.73311055328088,-7.65421504215694,
23.8076980377938));
#179348=CARTESIAN_POINT('Ctrl Pts',(-2.55031007436823,-7.71705940980132,
23.8152762826232));
#179349=CARTESIAN_POINT('Ctrl Pts',(-2.36529515513901,-7.77335618581677,
23.8228545274527));
#179350=CARTESIAN_POINT('Ctrl Pts',(-2.18041791037555,-7.82961106992106,
23.8304271331109));
#179351=CARTESIAN_POINT('Ctrl Pts',(-1.99332985263676,-7.87932794874501,
23.8379997387692));
#179352=CARTESIAN_POINT('Ctrl Pts',(-1.80455404516674,-7.92232745224359,
23.8455723444274));
#179353=CARTESIAN_POINT('Ctrl Pts',(-1.61588286271852,-7.96530312417152,
23.8531407531282));
#179354=CARTESIAN_POINT('Ctrl Pts',(-1.42552614896208,-8.00156874760897,
23.8607091618289));
#179355=CARTESIAN_POINT('Ctrl Pts',(-1.23402217667708,-8.03099475967761,
23.8682775705297));
#179356=CARTESIAN_POINT('Ctrl Pts',(-1.04256447328066,-8.0604136621868,
23.8758441506425));
#179357=CARTESIAN_POINT('Ctrl Pts',(-0.84996042466078,-8.08299617879292,
23.8834107307554));
#179358=CARTESIAN_POINT('Ctrl Pts',(-0.656758684149105,-8.09866381530279,
23.8909773108682));
#179359=CARTESIAN_POINT('Ctrl Pts',(-0.463591216752003,-8.11432867244483,
23.8985425487039));
#179360=CARTESIAN_POINT('Ctrl Pts',(-0.269826635269474,-8.12308106450025,
23.9061077865396));
#179361=CARTESIAN_POINT('Ctrl Pts',(-0.0760186299643247,-8.12489438272267,
23.9136730243754));
#179362=CARTESIAN_POINT('Ctrl Pts',(0.117856771684291,-8.12670833152284,
23.9212408930073));
#179363=CARTESIAN_POINT('Ctrl Pts',(0.311775259201533,-8.12157837899451,
23.9288087616393));
#179364=CARTESIAN_POINT('Ctrl Pts',(0.505182741367443,-8.10953007025219,
23.9363766302713));
#179365=CARTESIAN_POINT('Ctrl Pts',(0.696094403204386,-8.09763723850358,
23.9438468395978));
#179366=CARTESIAN_POINT('Ctrl Pts',(0.88650782579579,-8.07900360419725,
23.9513170489243));
#179367=CARTESIAN_POINT('Ctrl Pts',(1.07589550392165,-8.0537032740933,23.9587872582508));
#179368=CARTESIAN_POINT('Ctrl Pts',(1.31182084776506,-8.02218596980935,
23.968093099694));
#179369=CARTESIAN_POINT('Ctrl Pts',(1.5460388441147,-7.98034070549909,23.9773989411372));
#179370=CARTESIAN_POINT('Ctrl Pts',(1.77774361147715,-7.9283866715967,23.9867047825804));
#179371=CARTESIAN_POINT('Ctrl Pts',(2.01069235499054,-7.8761537069677,23.9960605852089));
#179372=CARTESIAN_POINT('Ctrl Pts',(2.24110077828056,-7.81370319993051,
24.0054163878374));
#179373=CARTESIAN_POINT('Ctrl Pts',(2.46817220066963,-7.74130567477745,
24.0147721904659));
#179374=CARTESIAN_POINT('Ctrl Pts',(2.69634593110011,-7.66855669908379,
24.0241734104189));
#179375=CARTESIAN_POINT('Ctrl Pts',(2.92115015044056,-7.58576393175628,
24.0335746303719));
#179376=CARTESIAN_POINT('Ctrl Pts',(3.14179941299455,-7.49324922920672,
24.0429758503249));
#179377=CARTESIAN_POINT('Ctrl Pts',(3.36268748352705,-7.40063439829578,
24.0523872451877));
#179378=CARTESIAN_POINT('Ctrl Pts',(3.57941157252882,-7.29827661029634,
24.0617986400504));
#179379=CARTESIAN_POINT('Ctrl Pts',(3.79120698546053,-7.186545564866,24.0712100349132));
#179380=CARTESIAN_POINT('Ctrl Pts',(4.00275395882051,-7.07494558182599,
24.0806103900519));
#179381=CARTESIAN_POINT('Ctrl Pts',(4.2093837819533,-6.95399433920389,24.0900107451906));
#179382=CARTESIAN_POINT('Ctrl Pts',(4.4103580886906,-6.82410646839727,24.0994111003293));
#179383=CARTESIAN_POINT('Ctrl Pts',(4.53894559457774,-6.74100153014341,
24.1054256413986));
#179384=CARTESIAN_POINT('Ctrl Pts',(4.6652183752779,-6.65423912874416,24.1114401824679));
#179385=CARTESIAN_POINT('Ctrl Pts',(4.7889882302884,-6.56393778860367,24.1174547235371));
#179386=CARTESIAN_POINT('Ctrl Pts',(4.94831263328778,-6.44769617947591,
24.1251970220564));
#179387=CARTESIAN_POINT('Ctrl Pts',(5.10356257850886,-6.32553324874517,
24.1329393205757));
#179388=CARTESIAN_POINT('Ctrl Pts',(5.25426566110439,-6.1977721743413,24.140681619095));
#179389=CARTESIAN_POINT('Ctrl Pts',(5.40487486932615,-6.07009068351757,
24.1484190948633));
#179390=CARTESIAN_POINT('Ctrl Pts',(5.55094258597142,-5.93681821978935,
24.1561565706317));
#179391=CARTESIAN_POINT('Ctrl Pts',(5.69202712464408,-5.79831999589674,
24.1638940464001));
#179392=CARTESIAN_POINT('Ctrl Pts',(5.83304885520387,-5.6598834287396,24.1716280775937));
#179393=CARTESIAN_POINT('Ctrl Pts',(5.96909157444715,-5.51622598168545,
24.1793621087872));
#179394=CARTESIAN_POINT('Ctrl Pts',(6.09974821376229,-5.36775179113228,
24.1870961399808));
#179395=CARTESIAN_POINT('Ctrl Pts',(6.23038813314207,-5.21929660059993,
24.1948291814619));
#179396=CARTESIAN_POINT('Ctrl Pts',(6.3556431064549,-5.06602615429118,24.202562222943));
#179397=CARTESIAN_POINT('Ctrl Pts',(6.47514410617666,-4.90838021823347,
24.2102952644241));
#179398=CARTESIAN_POINT('Ctrl Pts',(6.5946331678376,-4.75075003088729,24.2180275333802));
#179399=CARTESIAN_POINT('Ctrl Pts',(6.70836919027415,-4.58874550826861,
24.2257598023362));
#179400=CARTESIAN_POINT('Ctrl Pts',(6.816024587135,-4.42283804700909,24.2334920712922));
#179401=CARTESIAN_POINT('Ctrl Pts',(6.92372139413071,-4.2568667686949,24.2412273145005));
#179402=CARTESIAN_POINT('Ctrl Pts',(7.0253327099813,-4.0869898489721,24.2489625577087));
#179403=CARTESIAN_POINT('Ctrl Pts',(7.12057495808006,-3.91370666106481,
24.2566978009169));
#179404=CARTESIAN_POINT('Ctrl Pts',(7.20029761287676,-3.76865973023976,
24.2631725968858));
#179405=CARTESIAN_POINT('Ctrl Pts',(7.27555848415153,-3.62122675606321,
24.2696473928547));
#179406=CARTESIAN_POINT('Ctrl Pts',(7.34621646707183,-3.47171300389629,
24.2761221888236));
#179407=CARTESIAN_POINT('Ctrl Pts',(7.43804233416082,-3.27740757134609,
24.2845367193479));
#179408=CARTESIAN_POINT('Ctrl Pts',(7.5221378580496,-3.07949401598327,24.2929512498722));
#179409=CARTESIAN_POINT('Ctrl Pts',(7.59824883961314,-2.87859377714494,
24.3013657803965));
#179410=CARTESIAN_POINT('Ctrl Pts',(7.67438162949918,-2.67763597371988,
24.309782721963));
#179411=CARTESIAN_POINT('Ctrl Pts',(7.74252521601516,-2.47369002499559,
24.3181996635296));
#179412=CARTESIAN_POINT('Ctrl Pts',(7.80247441353559,-2.26739511083146,
24.3266166050962));
#179413=CARTESIAN_POINT('Ctrl Pts',(7.86245134216148,-2.06100476943464,
24.3350374401443));
#179414=CARTESIAN_POINT('Ctrl Pts',(7.91422623132519,-1.85226354414678,
24.3434582751925));
#179415=CARTESIAN_POINT('Ctrl Pts',(7.95764402696705,-1.64182493055002,
24.3518791102406));
#179416=CARTESIAN_POINT('Ctrl Pts',(8.00106769685982,-1.43135784546596,
24.3603010845934));
#179417=CARTESIAN_POINT('Ctrl Pts',(8.03613196578301,-1.21919317265353,
24.3687230589462));
#179418=CARTESIAN_POINT('Ctrl Pts',(8.06273298342256,-1.00599423483932,
24.3771450332991));
#179419=CARTESIAN_POINT('Ctrl Pts',(8.08934101921505,-0.792739048697539,
24.3855692296234));
#179420=CARTESIAN_POINT('Ctrl Pts',(8.10748130955641,-0.578449314158817,
24.3939934259478));
#179421=CARTESIAN_POINT('Ctrl Pts',(8.11710176759307,-0.363794525848674,
24.4024176222721));
#179422=CARTESIAN_POINT('Ctrl Pts',(8.12253958060108,-0.242464273624073,
24.4071792671106));
#179423=CARTESIAN_POINT('Ctrl Pts',(8.12525633609621,-0.121017470923162,
24.4119409119492));
#179424=CARTESIAN_POINT('Ctrl Pts',(8.12524998890234,0.000424667562427413,
24.4167025567877));
#179425=CARTESIAN_POINT('',(8.12179382505447,-0.00475747993537114,20.4167025567876));
#179426=CARTESIAN_POINT('Ctrl Pts',(8.12525,8.44118043087094E-13,20.4167025567876));
#179427=CARTESIAN_POINT('Ctrl Pts',(8.12524999999977,2.24624642433502,20.5047001499288));
#179428=CARTESIAN_POINT('Ctrl Pts',(7.14398562317547,4.47535249753539,20.5926977430701));
#179429=CARTESIAN_POINT('Ctrl Pts',(3.83078204044833,7.50935546634414,20.7686929293525));
#179430=CARTESIAN_POINT('Ctrl Pts',(1.52412477697628,8.2911009055216,20.8566905224937));
#179431=CARTESIAN_POINT('Ctrl Pts',(-2.95101623932681,7.89663306204382,
21.0326857087761));
#179432=CARTESIAN_POINT('Ctrl Pts',(-5.08535169588843,6.72342983085707,
21.1206833019173));
#179433=CARTESIAN_POINT('Ctrl Pts',(-7.8167169468446,3.15661951052808,21.2966784881997));
#179434=CARTESIAN_POINT('Ctrl Pts',(-8.39290461146718,0.790229551552612,
21.3846760813409));
#179435=CARTESIAN_POINT('Ctrl Pts',(-7.60701611462415,-3.63299000730563,
21.5606712676233));
#179436=CARTESIAN_POINT('Ctrl Pts',(-6.25093680401244,-5.65606750610146,
21.6486688607645));
#179437=CARTESIAN_POINT('Ctrl Pts',(-2.45807268688382,-8.06369575488373,
21.8246640470469));
#179438=CARTESIAN_POINT('Ctrl Pts',(-0.0502299510434481,-8.42987470330089,
21.9126616401881));
#179439=CARTESIAN_POINT('Ctrl Pts',(4.28689960881172,-7.2586363943446,22.0886568264705));
#179440=CARTESIAN_POINT('Ctrl Pts',(6.18309125557306,-5.73015646266226,
22.1766544196117));
#179441=CARTESIAN_POINT('Ctrl Pts',(7.81050559202949,-2.58640713800104,
22.3153355274312));
#179442=CARTESIAN_POINT('Ctrl Pts',(8.12525000000014,-1.2937588353802,22.3660190421094));
#179443=CARTESIAN_POINT('Ctrl Pts',(8.12525,8.99861304443488E-13,22.4167025567876));
#179444=CARTESIAN_POINT('',(8.13495457859621,0.00273215638295254,18.4167025567877));
#179445=CARTESIAN_POINT('Ctrl Pts',(8.13495457859621,0.00273215638295254,
18.4167025567877));
#179446=CARTESIAN_POINT('Ctrl Pts',(8.12219365949143,2.60157214278194,18.5187220057913));
#179447=CARTESIAN_POINT('Ctrl Pts',(6.08468278693466,6.5155798553575,18.6736306098904));
#179448=CARTESIAN_POINT('Ctrl Pts',(0.934776268559737,8.40074683640842,
18.881428369085));
#179449=CARTESIAN_POINT('Ctrl Pts',(-4.60194067302227,7.68097745167893,
19.0929849894669));
#179450=CARTESIAN_POINT('Ctrl Pts',(-8.4515383039797,2.98387753236073,19.3045416098488));
#179451=CARTESIAN_POINT('Ctrl Pts',(-8.04309746149275,-2.61270635975162,
19.5160982302307));
#179452=CARTESIAN_POINT('Ctrl Pts',(-5.84417858547815,-6.13212745071067,
19.6747656955172));
#179453=CARTESIAN_POINT('Ctrl Pts',(-2.18625041274964,-8.18579265278837,
19.8334331608036));
#179454=CARTESIAN_POINT('Ctrl Pts',(1.98642421298176,-8.22870475927635,
19.99210062609));
#179455=CARTESIAN_POINT('Ctrl Pts',(5.67997759279721,-6.28687098380536,
20.1507680913764));
#179456=CARTESIAN_POINT('Ctrl Pts',(7.7478105945485,-3.16811172828057,20.2923020682757));
#179457=CARTESIAN_POINT('Ctrl Pts',(8.12198112487852,-0.915751868132923,
20.3809468900794));
#179458=CARTESIAN_POINT('Ctrl Pts',(8.12170811034813,-0.00487546759574239,
20.4167025567876));
#179459=CARTESIAN_POINT('',(8.11704416097361,0.0053549714669613,16.4167025567876));
#179460=CARTESIAN_POINT('Ctrl Pts',(8.11704416097361,0.0053549714669613,
16.4167025567876));
#179461=CARTESIAN_POINT('Ctrl Pts',(8.12312230185039,0.724943922503215,
16.4449405011213));
#179462=CARTESIAN_POINT('Ctrl Pts',(7.87111371571117,2.78990206214897,16.5260676005504));
#179463=CARTESIAN_POINT('Ctrl Pts',(6.09986490165294,5.85132482975188,16.660083855075));
#179464=CARTESIAN_POINT('Ctrl Pts',(1.38755966192534,8.84590022303072,16.8716404754569));
#179465=CARTESIAN_POINT('Ctrl Pts',(-4.5775196263014,7.70573415727464,17.0831970958388));
#179466=CARTESIAN_POINT('Ctrl Pts',(-7.84949254946182,3.14692199034251,
17.2947537162207));
#179467=CARTESIAN_POINT('Ctrl Pts',(-8.41592959045643,-0.964126308737623,
17.4534211815072));
#179468=CARTESIAN_POINT('Ctrl Pts',(-6.9230488953515,-4.88449446864917,
17.6120886467936));
#179469=CARTESIAN_POINT('Ctrl Pts',(-3.74670372206902,-7.5907624378775,
17.77075611208));
#179470=CARTESIAN_POINT('Ctrl Pts',(0.333338327069147,-8.46615484038642,
17.9294235773664));
#179471=CARTESIAN_POINT('Ctrl Pts',(4.35323706612459,-7.26682444103609,
18.0880910426529));
#179472=CARTESIAN_POINT('Ctrl Pts',(7.27202321558427,-4.31686572056175,
18.2467585079393));
#179473=CARTESIAN_POINT('Ctrl Pts',(8.11531900160381,-1.53650348273241,
18.3562956793176));
#179474=CARTESIAN_POINT('Ctrl Pts',(8.13542474898045,-0.0930209461116091,
18.4129436956003));
#179475=CARTESIAN_POINT('Ctrl Pts',(8.13495457859621,0.00273215638295254,
18.4167025567877));
#179476=CARTESIAN_POINT('',(8.12115743020385,-0.00265292485854291,14.4167025567876));
#179477=CARTESIAN_POINT('Ctrl Pts',(8.12115743020385,-0.00265292485854291,
14.4167025567876));
#179478=CARTESIAN_POINT('Ctrl Pts',(8.1208903862547,0.185607932901776,14.4240481515468));
#179479=CARTESIAN_POINT('Ctrl Pts',(8.06645284195536,1.72963063830796,14.4842829014014));
#179480=CARTESIAN_POINT('Ctrl Pts',(6.7327160091308,5.90303377185082,14.6502959614469));
#179481=CARTESIAN_POINT('Ctrl Pts',(1.4221714321135,8.84926286475003,14.8618525818288));
#179482=CARTESIAN_POINT('Ctrl Pts',(-4.01080233417677,7.44520758162725,
15.0734092022108));
#179483=CARTESIAN_POINT('Ctrl Pts',(-7.07955773652492,4.65158818748291,
15.2320766674971));
#179484=CARTESIAN_POINT('Ctrl Pts',(-8.44497665565605,0.685026647011867,
15.3907441327836));
#179485=CARTESIAN_POINT('Ctrl Pts',(-7.73996699874801,-3.42788185729165,
15.54941159807));
#179486=CARTESIAN_POINT('Ctrl Pts',(-5.16809395608709,-6.71399263350416,
15.7080790633565));
#179487=CARTESIAN_POINT('Ctrl Pts',(-1.31318116064738,-8.36857010785243,
15.8667465286429));
#179488=CARTESIAN_POINT('Ctrl Pts',(2.81786210763198,-7.97353776185511,
16.0254139939293));
#179489=CARTESIAN_POINT('Ctrl Pts',(6.88263605041008,-5.30498188964788,
16.2087326699775));
#179490=CARTESIAN_POINT('Ctrl Pts',(8.10035380767631,-1.97061005881078,
16.3391621909303));
#179491=CARTESIAN_POINT('Ctrl Pts',(8.11704416097361,0.0053549714669613,
16.4167025567876));
#179492=CARTESIAN_POINT('',(8.12771990326935,-0.00255226564017053,12.4167025567876));
#179493=CARTESIAN_POINT('Ctrl Pts',(8.12771990326935,-0.00255226564017053,
12.4167025567876));
#179494=CARTESIAN_POINT('Ctrl Pts',(8.10769023119547,2.34268520044713,12.5089341121632));
#179495=CARTESIAN_POINT('Ctrl Pts',(6.43672742380787,6.03729498712112,12.6540548226342));
#179496=CARTESIAN_POINT('Ctrl Pts',(1.69039256538473,8.28614652732196,12.8520646882007));
#179497=CARTESIAN_POINT('Ctrl Pts',(-2.45563682176706,8.10723493000556,
13.0107321534872));
#179498=CARTESIAN_POINT('Ctrl Pts',(-6.04529291051789,5.93644050317478,
13.1693996187736));
#179499=CARTESIAN_POINT('Ctrl Pts',(-8.13900558166093,2.32681140425045,
13.32806708406));
#179500=CARTESIAN_POINT('Ctrl Pts',(-8.26960761947707,-1.84403959870139,
13.4867345493464));
#179501=CARTESIAN_POINT('Ctrl Pts',(-6.36979470017056,-5.58418533793423,
13.6454020146329));
#179502=CARTESIAN_POINT('Ctrl Pts',(-2.94483553187357,-7.92752136468722,
13.8040694799193));
#179503=CARTESIAN_POINT('Ctrl Pts',(2.62992883968321,-8.56828449165679,
14.0156261003012));
#179504=CARTESIAN_POINT('Ctrl Pts',(7.31450585013114,-5.04406336557082,
14.219837125924));
#179505=CARTESIAN_POINT('Ctrl Pts',(8.12281313441969,-1.16989261279938,
14.3711589964513));
#179506=CARTESIAN_POINT('Ctrl Pts',(8.12115743020385,-0.00265292485854291,
14.4167025567876));
#179507=CARTESIAN_POINT('',(8.12607929659709,0.000602397285608403,10.4167025567876));
#179508=CARTESIAN_POINT('Ctrl Pts',(8.12607929659709,0.000602397285608403,
10.4167025567876));
#179509=CARTESIAN_POINT('Ctrl Pts',(8.13073112681322,0.470635535523587,
10.4351526074932));
#179510=CARTESIAN_POINT('Ctrl Pts',(7.98907354300784,2.28814380995213,10.5064918132942));
#179511=CARTESIAN_POINT('Ctrl Pts',(6.60661632725948,5.27923024708584,10.6307201741907));
#179512=CARTESIAN_POINT('Ctrl Pts',(3.30861330952928,7.79810799993987,10.7893876394771));
#179513=CARTESIAN_POINT('Ctrl Pts',(-0.838343829035709,8.43113704348409,
10.9480551047636));
#179514=CARTESIAN_POINT('Ctrl Pts',(-4.75851708790317,7.00099837833084,
11.10672257005));
#179515=CARTESIAN_POINT('Ctrl Pts',(-7.53094626422831,3.88223396860591,
11.2653900353364));
#179516=CARTESIAN_POINT('Ctrl Pts',(-8.46845332731798,-0.206660721371117,
11.4240575006229));
#179517=CARTESIAN_POINT('Ctrl Pts',(-7.3400337247469,-4.20018525983505,
11.5827249659093));
#179518=CARTESIAN_POINT('Ctrl Pts',(-3.47017141527117,-8.26377245453908,
11.7942815862912));
#179519=CARTESIAN_POINT('Ctrl Pts',(2.5951842104773,-8.56973112092244,12.0058382066731));
#179520=CARTESIAN_POINT('Ctrl Pts',(6.84908166713351,-4.95342653106151,
12.217394827055));
#179521=CARTESIAN_POINT('Ctrl Pts',(8.03485269117871,-2.03602439612437,
12.3367198920614));
#179522=CARTESIAN_POINT('Ctrl Pts',(8.13066181458715,-0.347015251302779,
12.4031558019722));
#179523=CARTESIAN_POINT('Ctrl Pts',(8.12771990326935,-0.00255226564017053,
12.4167025567876));
#179524=CARTESIAN_POINT('',(8.12524838875447,0.00511698572321418,8.41670255678763));
#179525=CARTESIAN_POINT('Ctrl Pts',(8.12524838875447,0.00511698572321418,
8.41670255678763));
#179526=CARTESIAN_POINT('Ctrl Pts',(8.125098058661,0.2438257521285,8.42604123424159));
#179527=CARTESIAN_POINT('Ctrl Pts',(8.11442430814408,0.48221832798838,8.43537991169555));
#179528=CARTESIAN_POINT('Ctrl Pts',(8.09333451737573,0.719460876180585,
8.4447185891495));
#179529=CARTESIAN_POINT('Ctrl Pts',(8.072136057386,0.957925862436575,8.45410538594323));
#179530=CARTESIAN_POINT('Ctrl Pts',(8.04041399138175,1.19522890544064,8.46349218273696));
#179531=CARTESIAN_POINT('Ctrl Pts',(7.99832782015985,1.43053823568509,8.47287897953069));
#179532=CARTESIAN_POINT('Ctrl Pts',(7.95606163645599,1.66685403944175,8.48230592586855));
#179533=CARTESIAN_POINT('Ctrl Pts',(7.90334252502713,1.90115900887101,8.4917328722064));
#179534=CARTESIAN_POINT('Ctrl Pts',(7.84038219011455,2.13262623903827,8.50115981854426));
#179535=CARTESIAN_POINT('Ctrl Pts',(7.77737494260372,2.36426593857363,8.5105937890275));
#179536=CARTESIAN_POINT('Ctrl Pts',(7.70411122610931,2.5930636433074,8.52002775951075));
#179537=CARTESIAN_POINT('Ctrl Pts',(7.62085292578376,2.8182065655436,8.529461729994));
#179538=CARTESIAN_POINT('Ctrl Pts',(7.5377264010515,3.04299314682599,8.53888076902834));
#179539=CARTESIAN_POINT('Ctrl Pts',(7.44463691312889,3.26413647656692,8.54829980806267));
#179540=CARTESIAN_POINT('Ctrl Pts',(7.34189438505438,3.48084392083399,8.55771884709701));
#179541=CARTESIAN_POINT('Ctrl Pts',(7.30435543667455,3.56002213180782,8.56116027322039));
#179542=CARTESIAN_POINT('Ctrl Pts',(7.26552833483325,3.6386083356071,8.56460169934378));
#179543=CARTESIAN_POINT('Ctrl Pts',(7.22542984209052,3.7165644296215,8.56804312546716));
#179544=CARTESIAN_POINT('Ctrl Pts',(7.13521883948435,3.89194502174051,8.57578542398638));
#179545=CARTESIAN_POINT('Ctrl Pts',(7.03852776872942,4.06421563435813,8.58352772250561));
#179546=CARTESIAN_POINT('Ctrl Pts',(6.93560288403208,4.23285957687069,8.59127002102483));
#179547=CARTESIAN_POINT('Ctrl Pts',(6.83274211221766,4.40139846947843,8.59900749679318));
#179548=CARTESIAN_POINT('Ctrl Pts',(6.72365544141641,4.5663148897864,8.60674497256152));
#179549=CARTESIAN_POINT('Ctrl Pts',(6.60863540454276,4.72711599734172,8.61448244832986));
#179550=CARTESIAN_POINT('Ctrl Pts',(6.49366657236876,4.88784551934864,8.62221647952338));
#179551=CARTESIAN_POINT('Ctrl Pts',(6.37276983990874,5.04446309062786,8.6299505107169));
#179552=CARTESIAN_POINT('Ctrl Pts',(6.24628154791172,5.19650405433476,8.63768454191043));
#179553=CARTESIAN_POINT('Ctrl Pts',(6.11980944243305,5.34852556158596,8.6454175833915));
#179554=CARTESIAN_POINT('Ctrl Pts',(5.9877474225559,5.49597135147781,8.65315062487257));
#179555=CARTESIAN_POINT('Ctrl Pts',(5.85047291171498,5.63840884219912,8.66088366635364));
#179556=CARTESIAN_POINT('Ctrl Pts',(5.71321211449538,5.78083210352127,8.66861593530963));
#179557=CARTESIAN_POINT('Ctrl Pts',(5.57074011136782,5.91824781031278,8.67634820426562));
#179558=CARTESIAN_POINT('Ctrl Pts',(5.42347198319433,6.05025943328104,8.68408047322161));
#179559=CARTESIAN_POINT('Ctrl Pts',(5.27614720766975,6.1823218351167,8.6918157164298));
#179560=CARTESIAN_POINT('Ctrl Pts',(5.12402288457192,6.30897576393484,8.69955095963798));
#179561=CARTESIAN_POINT('Ctrl Pts',(4.96754853923773,6.42986384558935,8.70728620284617));
#179562=CARTESIAN_POINT('Ctrl Pts',(4.83657147320705,6.53105338064936,8.7137609988153));
#179563=CARTESIAN_POINT('Ctrl Pts',(4.70254722464643,6.62820368388824,8.72023579478444));
#179564=CARTESIAN_POINT('Ctrl Pts',(4.56575557235517,6.72112815054197,8.72671059075357));
#179565=CARTESIAN_POINT('Ctrl Pts',(4.38799319042858,6.84188460208664,8.73512466525799));
#179566=CARTESIAN_POINT('Ctrl Pts',(4.2054713374984,6.95556232257409,8.74353873976241));
#179567=CARTESIAN_POINT('Ctrl Pts',(4.01876463813715,7.06181409736608,8.75195281426683));
#179568=CARTESIAN_POINT('Ctrl Pts',(3.83200579673226,7.16809554535512,8.76036923859074));
#179569=CARTESIAN_POINT('Ctrl Pts',(3.64106000524196,7.26694677693808,8.76878566291464));
#179570=CARTESIAN_POINT('Ctrl Pts',(3.4465269865376,7.3580662740674,8.77720208723855));
#179571=CARTESIAN_POINT('Ctrl Pts',(3.25194572499939,7.44920836819741,8.78562059877707));
#179572=CARTESIAN_POINT('Ctrl Pts',(3.05377569925666,7.53261478798179,8.7940391103156));
#179573=CARTESIAN_POINT('Ctrl Pts',(2.85263812737841,7.60803149814241,8.80245762185412));
#179574=CARTESIAN_POINT('Ctrl Pts',(2.65142329939928,7.68347717554625,8.81087936690775));
#179575=CARTESIAN_POINT('Ctrl Pts',(2.44723889432485,7.75092691688914,8.81930111196138));
#179576=CARTESIAN_POINT('Ctrl Pts',(2.24072421999721,7.81017557628623,8.827722857015));
#179577=CARTESIAN_POINT('Ctrl Pts',(2.03418716004291,7.86943065807617,8.83614551496279));
#179578=CARTESIAN_POINT('Ctrl Pts',(1.82531958104599,7.92048281310389,8.84456817291058));
#179579=CARTESIAN_POINT('Ctrl Pts',(1.61477458531803,7.96317716750739,8.85299083085837));
#179580=CARTESIAN_POINT('Ctrl Pts',(1.40418954999055,8.00587964114851,8.86141509055333));
#179581=CARTESIAN_POINT('Ctrl Pts',(1.19192671933118,8.04022108650938,8.86983935024829));
#179582=CARTESIAN_POINT('Ctrl Pts',(0.978649295929383,8.06609776273986,
8.87826360994325));
#179583=CARTESIAN_POINT('Ctrl Pts',(0.918610361257806,8.07338220967727,
8.8806350919755));
#179584=CARTESIAN_POINT('Ctrl Pts',(0.858491070339641,8.0799961730106,8.88300657400776));
#179585=CARTESIAN_POINT('Ctrl Pts',(0.7983063132151,8.08593807747629,8.88537805604001));
#179586=CARTESIAN_POINT('Ctrl Pts',(0.584509219070929,8.10704577931211,
8.89380238126012));
#179587=CARTESIAN_POINT('Ctrl Pts',(0.369863588301559,8.11967085437079,
8.90222670648022));
#179588=CARTESIAN_POINT('Ctrl Pts',(0.15503927395233,8.123770699991,8.91065103170033));
#179589=CARTESIAN_POINT('Ctrl Pts',(-0.0597479161277014,8.12786983710775,
8.919073901094));
#179590=CARTESIAN_POINT('Ctrl Pts',(-0.274713464367256,8.12344668231059,
8.92749677048766));
#179591=CARTESIAN_POINT('Ctrl Pts',(-0.489186275147421,8.11051073303694,
8.93591963988132));
#179592=CARTESIAN_POINT('Ctrl Pts',(-0.703615258049017,8.09757742724622,
8.9443407880475));
#179593=CARTESIAN_POINT('Ctrl Pts',(-0.917551441270378,8.07613481673323,
8.95276193621368));
#179594=CARTESIAN_POINT('Ctrl Pts',(-1.13032650600636,8.04624443776843,
8.96118308437986));
#179595=CARTESIAN_POINT('Ctrl Pts',(-1.34304187323866,8.01636244503541,
8.96960186985601));
#179596=CARTESIAN_POINT('Ctrl Pts',(-1.5545965114634,7.97803745437985,8.97802065533217));
#179597=CARTESIAN_POINT('Ctrl Pts',(-1.76432897031372,7.93138265670064,
8.98643944080832));
#179598=CARTESIAN_POINT('Ctrl Pts',(-1.97400284180562,7.88474089172686,
8.99485587455311));
#179599=CARTESIAN_POINT('Ctrl Pts',(-2.18185529279267,7.82977402285051,
9.00327230829789));
#179600=CARTESIAN_POINT('Ctrl Pts',(-2.38723563783614,7.76664622420418,
9.01168874204267));
#179601=CARTESIAN_POINT('Ctrl Pts',(-2.59254144175425,7.70354133727879,
9.0201021211113));
#179602=CARTESIAN_POINT('Ctrl Pts',(-2.79537667941255,7.63228151299868,
9.02851550017993));
#179603=CARTESIAN_POINT('Ctrl Pts',(-2.99510542884134,7.55308089673513,
9.03692887924856));
#179604=CARTESIAN_POINT('Ctrl Pts',(-3.05142041678122,7.53074970123889,
9.03930109327452));
#179605=CARTESIAN_POINT('Ctrl Pts',(-3.10748853771055,7.50778751544481,
9.04167330730049));
#179606=CARTESIAN_POINT('Ctrl Pts',(-3.16329578184452,7.48419984761662,
9.04404552132645));
#179607=CARTESIAN_POINT('Ctrl Pts',(-3.34526897145014,7.40728647881186,
9.05178070623714));
#179608=CARTESIAN_POINT('Ctrl Pts',(-3.52454764430374,7.32368480952295,
9.05951589114782));
#179609=CARTESIAN_POINT('Ctrl Pts',(-3.70060333951096,7.23361752417837,
9.0672510760585));
#179610=CARTESIAN_POINT('Ctrl Pts',(-3.87660459394719,7.14357808986381,
9.07498386905889));
#179611=CARTESIAN_POINT('Ctrl Pts',(-4.0493845412807,7.04707718170321,9.08271666205927));
#179612=CARTESIAN_POINT('Ctrl Pts',(-4.2184367754129,6.94438469083792,9.09044945505966));
#179613=CARTESIAN_POINT('Ctrl Pts',(-4.38746677010459,6.84170570954588,
9.09818123078281));
#179614=CARTESIAN_POINT('Ctrl Pts',(-4.55276972691651,6.73283695199524,
9.10591300650596));
#179615=CARTESIAN_POINT('Ctrl Pts',(-4.71386571423205,6.61809319900283,
9.11364478222911));
#179616=CARTESIAN_POINT('Ctrl Pts',(-4.87501934609027,6.50330838756275,
9.12137932459271));
#179617=CARTESIAN_POINT('Ctrl Pts',(-5.03196271033564,6.38264458232978,
9.12911386695631));
#179618=CARTESIAN_POINT('Ctrl Pts',(-5.184246105036,6.25645905324402,9.13684840931992));
#179619=CARTESIAN_POINT('Ctrl Pts',(-5.33655521870373,6.1302522128294,9.14458425796148));
#179620=CARTESIAN_POINT('Ctrl Pts',(-5.48420252739657,5.99852202175738,
9.15232010660305));
#179621=CARTESIAN_POINT('Ctrl Pts',(-5.62677296530292,5.86166474300912,
9.16005595524462));
#179622=CARTESIAN_POINT('Ctrl Pts',(-5.76946006079732,5.72469548143833,
9.16779813370783));
#179623=CARTESIAN_POINT('Ctrl Pts',(-5.90706173597879,5.5825910006595,9.17554031217104));
#179624=CARTESIAN_POINT('Ctrl Pts',(-6.03920057871778,5.43578365394677,
9.18328249063426));
#179625=CARTESIAN_POINT('Ctrl Pts',(-6.14974324939096,5.31296983294089,
9.18975932262712));
#179626=CARTESIAN_POINT('Ctrl Pts',(-6.25646343178564,5.18686545947815,
9.19623615461998));
#179627=CARTESIAN_POINT('Ctrl Pts',(-6.35916264071861,5.0577404116254,9.20271298661285));
#179628=CARTESIAN_POINT('Ctrl Pts',(-6.50818149601939,4.87037707142447,
9.21211101508435));
#179629=CARTESIAN_POINT('Ctrl Pts',(-6.6488191110939,4.6765474368328,9.22150904355584));
#179630=CARTESIAN_POINT('Ctrl Pts',(-6.78060197585802,4.47695481409968,
9.23090707202734));
#179631=CARTESIAN_POINT('Ctrl Pts',(-6.91257235660879,4.27707818776984,
9.24031847310676));
#179632=CARTESIAN_POINT('Ctrl Pts',(-7.0356627634241,4.07142220134046,9.24972987418617));
#179633=CARTESIAN_POINT('Ctrl Pts',(-7.14944298160735,3.86071918368138,
9.25914127526559));
#179634=CARTESIAN_POINT('Ctrl Pts',(-7.26305188446895,3.65033341497663,
9.26853850589229));
#179635=CARTESIAN_POINT('Ctrl Pts',(-7.3673786016306,3.43491583680912,9.27793573651898));
#179636=CARTESIAN_POINT('Ctrl Pts',(-7.46204011350519,3.21522081775722,
9.28733296714567));
#179637=CARTESIAN_POINT('Ctrl Pts',(-7.55646285373454,2.99607995149786,
9.2967064944512));
#179638=CARTESIAN_POINT('Ctrl Pts',(-7.64126905143205,2.77268322230516,
9.30608002175674));
#179639=CARTESIAN_POINT('Ctrl Pts',(-7.71612397236401,2.54580407840224,
9.31545354906227));
#179640=CARTESIAN_POINT('Ctrl Pts',(-7.79049278983644,2.32039827433284,
9.32476620523208));
#179641=CARTESIAN_POINT('Ctrl Pts',(-7.8550391226782,2.09155517351854,9.3340788614019));
#179642=CARTESIAN_POINT('Ctrl Pts',(-7.90948004424336,1.86005725509084,
9.34339151757171));
#179643=CARTESIAN_POINT('Ctrl Pts',(-7.94453392306917,1.710998426774,9.34938782901424));
#179644=CARTESIAN_POINT('Ctrl Pts',(-7.97539909056265,1.56083941500507,
9.35538414045678));
#179645=CARTESIAN_POINT('Ctrl Pts',(-8.00201021731963,1.40979432698968,
9.36138045189931));
#179646=CARTESIAN_POINT('Ctrl Pts',(-8.03559484912476,1.2191675371774,9.36894811011331));
#179647=CARTESIAN_POINT('Ctrl Pts',(-8.06238728747812,1.02720451234722,
9.37651576832731));
#179648=CARTESIAN_POINT('Ctrl Pts',(-8.08228808330916,0.834450058960203,
9.38408342654131));
#179649=CARTESIAN_POINT('Ctrl Pts',(-8.10218336896755,0.641748975816641,
9.39164898940678));
#179650=CARTESIAN_POINT('Ctrl Pts',(-8.11519077118466,0.448257265478159,
9.39921455227225));
#179651=CARTESIAN_POINT('Ctrl Pts',(-8.12126243570495,0.254527037675314,
9.40678011513772));
#179652=CARTESIAN_POINT('Ctrl Pts',(-8.12733356828999,0.060813782473072,
9.41434501518831));
#179653=CARTESIAN_POINT('Ctrl Pts',(-8.12647016194583,-0.13313758109363,
9.4219099152389));
#179654=CARTESIAN_POINT('Ctrl Pts',(-8.1186764370686,-0.326772815097942,
9.4294748152895));
#179655=CARTESIAN_POINT('Ctrl Pts',(-8.11087888707936,-0.520503084078696,
9.43704342814629));
#179656=CARTESIAN_POINT('Ctrl Pts',(-8.09614423488416,-0.713916545491256,
9.44461204100309));
#179657=CARTESIAN_POINT('Ctrl Pts',(-8.07452879829972,-0.906461387996509,
9.45218065385988));
#179658=CARTESIAN_POINT('Ctrl Pts',(-8.0529085548222,-1.0990490490896,9.45975094984312));
#179659=CARTESIAN_POINT('Ctrl Pts',(-8.02440453124403,-1.29076734241741,
9.46732124582635));
#179660=CARTESIAN_POINT('Ctrl Pts',(-7.98912453773546,-1.48107281490588,
9.47489154180958));
#179661=CARTESIAN_POINT('Ctrl Pts',(-7.95380879553575,-1.67157112109072,
9.4824695086608));
#179662=CARTESIAN_POINT('Ctrl Pts',(-7.91170344402178,-1.86065338679133,
9.49004747551202));
#179663=CARTESIAN_POINT('Ctrl Pts',(-7.8629669491208,-2.04778864132361,
9.49762544236324));
#179664=CARTESIAN_POINT('Ctrl Pts',(-7.81489808265974,-2.23236037916696,
9.5050996006374));
#179665=CARTESIAN_POINT('Ctrl Pts',(-7.76037875217189,-2.41503780479106,
9.51257375891156));
#179666=CARTESIAN_POINT('Ctrl Pts',(-7.69960716223324,-2.59532986531318,
9.52004791718572));
#179667=CARTESIAN_POINT('Ctrl Pts',(-7.6339515600846,-2.79011140399185,
9.52812274890461));
#179668=CARTESIAN_POINT('Ctrl Pts',(-7.56085858164267,-2.98252480353528,
9.5361975806235));
#179669=CARTESIAN_POINT('Ctrl Pts',(-7.48052139510541,-3.17198474458347,
9.54427241234239));
#179670=CARTESIAN_POINT('Ctrl Pts',(-7.40023735952158,-3.36131933923931,
9.55234190176561));
#179671=CARTESIAN_POINT('Ctrl Pts',(-7.31271879635653,-3.54770408113246,
9.56041139118882));
#179672=CARTESIAN_POINT('Ctrl Pts',(-7.2182077353601,-3.73057162532603,
9.56848088061203));
#179673=CARTESIAN_POINT('Ctrl Pts',(-7.12374632738373,-3.91334309689331,
9.57654613058944));
#179674=CARTESIAN_POINT('Ctrl Pts',(-7.02229989294093,-4.09260077501462,
9.58461138056686));
#179675=CARTESIAN_POINT('Ctrl Pts',(-6.91415760991501,-4.2677994455872,
9.59267663054428));
#179676=CARTESIAN_POINT('Ctrl Pts',(-6.80605742443153,-4.4429299149598,
9.60073874088756));
#179677=CARTESIAN_POINT('Ctrl Pts',(-6.69126675523716,-4.61400425905557,
9.60880085123083));
#179678=CARTESIAN_POINT('Ctrl Pts',(-6.57011985775149,-4.78050338534338,
9.61686296157411));
#179679=CARTESIAN_POINT('Ctrl Pts',(-6.4490036466253,-4.94696033760817,
9.6249230297948));
#179680=CARTESIAN_POINT('Ctrl Pts',(-6.32153460501466,-5.10884412785562,
9.63298309801549));
#179681=CARTESIAN_POINT('Ctrl Pts',(-6.18808965410538,-5.26566557951167,
9.64104316623618));
#179682=CARTESIAN_POINT('Ctrl Pts',(-6.05264549881148,-5.42483645039727,
9.64922398629962));
#179683=CARTESIAN_POINT('Ctrl Pts',(-5.91104514522524,-5.5787918197457,
9.65740480636305));
#179684=CARTESIAN_POINT('Ctrl Pts',(-5.76372491841141,-5.7270553190434,
9.66558562642648));
#179685=CARTESIAN_POINT('Ctrl Pts',(-5.61856510014355,-5.8731445769768,
9.67364647712821));
#179686=CARTESIAN_POINT('Ctrl Pts',(-5.46785226088467,-6.01370754355162,
9.68170732782993));
#179687=CARTESIAN_POINT('Ctrl Pts',(-5.31204095007485,-6.14832566697861,
9.68976817853165));
#179688=CARTESIAN_POINT('Ctrl Pts',(-5.15620379937592,-6.28296611559727,
9.69783036605216));
#179689=CARTESIAN_POINT('Ctrl Pts',(-4.99526673045904,-6.4116595474387,
9.70589255357267));
#179690=CARTESIAN_POINT('Ctrl Pts',(-4.82971786174866,-6.53402731387052,
9.71395474109319));
#179691=CARTESIAN_POINT('Ctrl Pts',(-4.66412102970979,-6.65643053306877,
9.72201926441551));
#179692=CARTESIAN_POINT('Ctrl Pts',(-4.49390998769988,-6.77250424322061,
9.73008378773784));
#179693=CARTESIAN_POINT('Ctrl Pts',(-4.31960283245551,-6.88191244730288,
9.73814831106017));
#179694=CARTESIAN_POINT('Ctrl Pts',(-4.14086433068113,-6.994102095812,9.74641785578504));
#179695=CARTESIAN_POINT('Ctrl Pts',(-3.95781899086813,-7.09928265356517,
9.75468740050991));
#179696=CARTESIAN_POINT('Ctrl Pts',(-3.77105322355808,-7.19714145668905,
9.76295694523478));
#179697=CARTESIAN_POINT('Ctrl Pts',(-3.58867172097493,-7.29270305671768,
9.77103236512742));
#179698=CARTESIAN_POINT('Ctrl Pts',(-3.40274280326232,-7.38128268722101,
9.77910778502006));
#179699=CARTESIAN_POINT('Ctrl Pts',(-3.21383402583139,-7.46263749735363,
9.7871832049127));
#179700=CARTESIAN_POINT('Ctrl Pts',(-3.01811348779624,-7.546925837088,9.79554981205368));
#179701=CARTESIAN_POINT('Ctrl Pts',(-2.81919455191184,-7.62345850405344,
9.80391641919466));
#179702=CARTESIAN_POINT('Ctrl Pts',(-2.6177272678535,-7.69202128920847,
9.81228302633563));
#179703=CARTESIAN_POINT('Ctrl Pts',(-2.41625998379515,-7.76058407436349,
9.82064963347661));
#179704=CARTESIAN_POINT('Ctrl Pts',(-2.21224472182711,-7.82117690662455,
9.82901624061759));
#179705=CARTESIAN_POINT('Ctrl Pts',(-2.00634528041495,-7.87364376754858,
9.83738284775857));
#179706=CARTESIAN_POINT('Ctrl Pts',(-1.80754962964786,-7.9243004555394,
9.84546079639163));
#179707=CARTESIAN_POINT('Ctrl Pts',(-1.60661112984514,-7.96748101058202,
9.8535387450247));
#179708=CARTESIAN_POINT('Ctrl Pts',(-1.40411856197274,-8.0030080986104,
9.86161669365776));
#179709=CARTESIAN_POINT('Ctrl Pts',(-1.20187380387928,-8.03849170869821,
9.86968475652224));
#179710=CARTESIAN_POINT('Ctrl Pts',(-0.998079077257228,-8.06634046783967,
9.87775281938672));
#179711=CARTESIAN_POINT('Ctrl Pts',(-0.793336921923672,-8.08642715238397,
9.88582088225121));
#179712=CARTESIAN_POINT('Ctrl Pts',(-0.588820123053253,-8.1064917278312,
9.89388006472607));
#179713=CARTESIAN_POINT('Ctrl Pts',(-0.383358286685486,-8.11881122997671,
9.90193924720093));
#179714=CARTESIAN_POINT('Ctrl Pts',(-0.177563325255657,-8.12330959818867,
9.90999842967579));
#179715=CARTESIAN_POINT('Ctrl Pts',(0.0279672997404689,-8.12780218840391,
9.9180472604125));
#179716=CARTESIAN_POINT('Ctrl Pts',(0.233829882009029,-8.1244936791582,
9.92609609114921));
#179717=CARTESIAN_POINT('Ctrl Pts',(0.439408168088388,-8.11335984807264,
9.93414492188592));
#179718=CARTESIAN_POINT('Ctrl Pts',(0.64483095568013,-8.10223443856664,
9.94218766452339));
#179719=CARTESIAN_POINT('Ctrl Pts',(0.849969561810193,-8.0832955223537,
9.95023040716086));
#179720=CARTESIAN_POINT('Ctrl Pts',(1.05420714503438,-8.05657091186185,
9.95827314979833));
#179721=CARTESIAN_POINT('Ctrl Pts',(1.25827836905849,-8.02986806957129,
9.96630934131915));
#179722=CARTESIAN_POINT('Ctrl Pts',(1.46144972204523,-7.99539222414565,
9.97434553283997));
#179723=CARTESIAN_POINT('Ctrl Pts',(1.6631086134198,-7.95322307636777,9.98238172436079));
#179724=CARTESIAN_POINT('Ctrl Pts',(1.77744106528548,-7.92931487164808,
9.98693792058886));
#179725=CARTESIAN_POINT('Ctrl Pts',(1.89128742262083,-7.90293465159328,
9.99149411681694));
#179726=CARTESIAN_POINT('Ctrl Pts',(2.00453702288224,-7.87410432280361,
9.99605031304501));
#179727=CARTESIAN_POINT('Ctrl Pts',(2.20429401534752,-7.82325151840061,
10.0040868275537));
#179728=CARTESIAN_POINT('Ctrl Pts',(2.40203572539872,-7.76481324266406,
10.0121233420623));
#179729=CARTESIAN_POINT('Ctrl Pts',(2.59717513615446,-7.69898492495219,
10.020159856571));
#179730=CARTESIAN_POINT('Ctrl Pts',(2.79243243053666,-7.63311684038448,
10.0282012259343));
#179731=CARTESIAN_POINT('Ctrl Pts',(2.98508399004642,-7.55984990822988,
10.0362425952976));
#179732=CARTESIAN_POINT('Ctrl Pts',(3.17456178869415,-7.47942812066959,
10.0442839646609));
#179733=CARTESIAN_POINT('Ctrl Pts',(3.36417721801751,-7.3989479172683,10.0523311750204));
#179734=CARTESIAN_POINT('Ctrl Pts',(3.55061399672931,-7.3113026130809,10.0603783853799));
#179735=CARTESIAN_POINT('Ctrl Pts',(3.73332720545528,-7.21678290788267,
10.0684255957394));
#179736=CARTESIAN_POINT('Ctrl Pts',(3.91630972040398,-7.12212388738831,
10.0764846671123));
#179737=CARTESIAN_POINT('Ctrl Pts',(4.09555741533467,-7.02057035998896,
10.0845437384853));
#179738=CARTESIAN_POINT('Ctrl Pts',(4.27055145076036,-6.91245816398975,
10.0926028098582));
#179739=CARTESIAN_POINT('Ctrl Pts',(4.44568711744493,-6.80425846748584,
10.100668403833));
#179740=CARTESIAN_POINT('Ctrl Pts',(4.61656199277263,-6.68948968504108,
10.1087339978078));
#179741=CARTESIAN_POINT('Ctrl Pts',(4.78268831542635,-6.56852951884851,
10.1167995917826));
#179742=CARTESIAN_POINT('Ctrl Pts',(4.94907549436119,-6.44737941755949,
10.1248778505827));
#179743=CARTESIAN_POINT('Ctrl Pts',(5.11069896875312,-6.32001869528888,
10.1329561093828));
#179744=CARTESIAN_POINT('Ctrl Pts',(5.26710465191401,-6.18686480766194,
10.1410343681829));
#179745=CARTESIAN_POINT('Ctrl Pts',(5.35541423962851,-6.11168362062782,
10.1455955048991));
#179746=CARTESIAN_POINT('Ctrl Pts',(5.44206109547213,-6.03465627404792,
10.1501566416153));
#179747=CARTESIAN_POINT('Ctrl Pts',(5.52696893801387,-5.95586281916649,
10.1547177783315));
#179748=CARTESIAN_POINT('Ctrl Pts',(5.67489187501032,-5.81859211585745,
10.1626640023657));
#179749=CARTESIAN_POINT('Ctrl Pts',(5.81785214234309,-5.67566425775407,
10.1706102264));
#179750=CARTESIAN_POINT('Ctrl Pts',(5.95539848735943,-5.52746925991063,
10.1785564504342));
#179751=CARTESIAN_POINT('Ctrl Pts',(6.09281483459454,-5.37941432410161,
10.1864951643344));
#179752=CARTESIAN_POINT('Ctrl Pts',(6.22482723158983,-5.22610241249131,
10.1944338782345));
#179753=CARTESIAN_POINT('Ctrl Pts',(6.35101957562125,-5.06796190914806,
10.2023725921347));
#179754=CARTESIAN_POINT('Ctrl Pts',(6.47711398298939,-4.90994413712695,
10.2103051448755));
#179755=CARTESIAN_POINT('Ctrl Pts',(6.59739713336566,-4.74710550222358,
10.2182376976162));
#179756=CARTESIAN_POINT('Ctrl Pts',(6.71149140988143,-4.57990945517352,
10.2261702503569));
#179757=CARTESIAN_POINT('Ctrl Pts',(6.82567620409571,-4.4125807616679,10.2341090964582));
#179758=CARTESIAN_POINT('Ctrl Pts',(6.93366208037581,-4.24088799197895,
10.2420479425595));
#179759=CARTESIAN_POINT('Ctrl Pts',(7.03511154143971,-4.06532817396108,
10.2499867886608));
#179760=CARTESIAN_POINT('Ctrl Pts',(7.13637486580226,-3.89009046830412,
10.257911068784));
#179761=CARTESIAN_POINT('Ctrl Pts',(7.23112556563233,-3.7110001773017,10.2658353489072));
#179762=CARTESIAN_POINT('Ctrl Pts',(7.31907177064689,-3.52857988128649,
10.2737596290304));
#179763=CARTESIAN_POINT('Ctrl Pts',(7.40699841233518,-3.34620016402927,
10.2816821464251));
#179764=CARTESIAN_POINT('Ctrl Pts',(7.48812343151978,-3.16049221822206,
10.2896046638199));
#179765=CARTESIAN_POINT('Ctrl Pts',(7.5622014199931,-2.97200222845715,10.2975271812146));
#179766=CARTESIAN_POINT('Ctrl Pts',(7.63627427329671,-2.78352530503093,
10.3054491494115));
#179767=CARTESIAN_POINT('Ctrl Pts',(7.70330094841308,-2.59226703245282,
10.3133711176084));
#179768=CARTESIAN_POINT('Ctrl Pts',(7.76308445035316,-2.39879290043657,
10.3212930858053));
#179769=CARTESIAN_POINT('Ctrl Pts',(7.82308545170148,-2.20461488678313,
10.3292438750539));
#179770=CARTESIAN_POINT('Ctrl Pts',(7.87579035692534,-2.00820517647219,
10.3371946643024));
#179771=CARTESIAN_POINT('Ctrl Pts',(7.9210506457439,-1.81015033355248,10.3451454535509));
#179772=CARTESIAN_POINT('Ctrl Pts',(7.96617330192918,-1.6126977583221,10.3530720651353));
#179773=CARTESIAN_POINT('Ctrl Pts',(8.00389651687895,-1.41361037583155,
10.3609986767197));
#179774=CARTESIAN_POINT('Ctrl Pts',(8.03412444581144,-1.21347927535452,
10.3689252883041));
#179775=CARTESIAN_POINT('Ctrl Pts',(8.06449067609217,-1.01243251833082,
10.3768881663847));
#179776=CARTESIAN_POINT('Ctrl Pts',(8.08729281276306,-0.810332804847844,
10.3848510444653));
#179777=CARTESIAN_POINT('Ctrl Pts',(8.10248639470418,-0.607784325343876,
10.3928139225459));
#179778=CARTESIAN_POINT('Ctrl Pts',(8.1176799766453,-0.405235845839927,
10.4007768006264));
#179779=CARTESIAN_POINT('Ctrl Pts',(8.12526501457307,-0.202238940266611,
10.408739678707));
#179780=CARTESIAN_POINT('Ctrl Pts',(8.12524997767401,0.00060233580707081,
10.4167025567876));
#179781=CARTESIAN_POINT('',(8.12456022843635,0.000454668290610622,4.4166972245402));
#179782=CARTESIAN_POINT('Ctrl Pts',(8.12524944607656,0.00300025542302204,
8.41865443786164));
#179783=CARTESIAN_POINT('Ctrl Pts',(8.12534260691395,-0.249296611252544,
8.40866000239997));
#179784=CARTESIAN_POINT('Ctrl Pts',(8.11368452319427,-0.501462439799894,
8.39863635441595));
#179785=CARTESIAN_POINT('Ctrl Pts',(8.0377516071859,-1.31764703565447,8.36566170274765));
#179786=CARTESIAN_POINT('Ctrl Pts',(7.92615719088016,-1.87552917470942,
8.34208384265915));
#179787=CARTESIAN_POINT('Ctrl Pts',(7.64656162715796,-2.77282008568974,
8.30231745151355));
#179788=CARTESIAN_POINT('Ctrl Pts',(7.51142444228261,-3.12040800446353,
8.28647102020751));
#179789=CARTESIAN_POINT('Ctrl Pts',(7.30041202776761,-3.5691590430266,8.26611919427734));
#179790=CARTESIAN_POINT('Ctrl Pts',(7.24536934550857,-3.67961094765436,
8.2611223662416));
#179791=CARTESIAN_POINT('Ctrl Pts',(7.17966997329027,-3.80425195867326,
8.25553074496127));
#179792=CARTESIAN_POINT('Ctrl Pts',(7.17145871633034,-3.81970859833049,
8.25483817907225));
#179793=CARTESIAN_POINT('Ctrl Pts',(7.15898032954345,-3.84301548696492,
8.25379528236128));
#179794=CARTESIAN_POINT('Ctrl Pts',(7.15475011581351,-3.85088537519616,
8.25344337872774));
#179795=CARTESIAN_POINT('Ctrl Pts',(7.14713155394543,-3.86500305670066,
8.25281256485714));
#179796=CARTESIAN_POINT('Ctrl Pts',(7.1437479759943,-3.87125340601894,8.25253344602394));
#179797=CARTESIAN_POINT('Ctrl Pts',(7.13697882924859,-3.88371868709492,
8.25197712692639));
#179798=CARTESIAN_POINT('Ctrl Pts',(7.13359333311571,-3.88993365081527,
8.25169992380246));
#179799=CARTESIAN_POINT('Ctrl Pts',(7.12415972589869,-3.90719777146968,
8.25093038305258));
#179800=CARTESIAN_POINT('Ctrl Pts',(7.11809401932202,-3.91823732817893,
8.25043885005597));
#179801=CARTESIAN_POINT('Ctrl Pts',(7.09387332162766,-3.96207701920554,
8.24848922888969));
#179802=CARTESIAN_POINT('Ctrl Pts',(7.07551689672411,-3.99476579024089,
8.24704069771003));
#179803=CARTESIAN_POINT('Ctrl Pts',(6.76188044598456,-4.54433926815202,
8.22279112250198));
#179804=CARTESIAN_POINT('Ctrl Pts',(6.4108794613095,-5.02740199910961,8.20309811404289));
#179805=CARTESIAN_POINT('Ctrl Pts',(5.88158080035,-5.60921083806592,8.17687225117711));
#179806=CARTESIAN_POINT('Ctrl Pts',(5.74797533568672,-5.74604363652688,
8.17049518475249));
#179807=CARTESIAN_POINT('Ctrl Pts',(5.5653126300551,-5.92036674148974,8.1619582002572));
#179808=CARTESIAN_POINT('Ctrl Pts',(5.52047853553056,-5.96219453576103,
8.15987661446729));
#179809=CARTESIAN_POINT('Ctrl Pts',(5.11529906270398,-6.33171644982272,
8.14116181751614));
#179810=CARTESIAN_POINT('Ctrl Pts',(4.7266803899364,-6.62686534366664,8.12381544392025));
#179811=CARTESIAN_POINT('Ctrl Pts',(4.2902568765596,-6.90030203766106,8.103975392903));
#179812=CARTESIAN_POINT('Ctrl Pts',(4.26644192529054,-6.91505210083696,
8.10289194788854));
#179813=CARTESIAN_POINT('Ctrl Pts',(4.23157834451104,-6.93639660154787,
8.10130457156946));
#179814=CARTESIAN_POINT('Ctrl Pts',(4.22058946460535,-6.94308848201863,
8.10080405154524));
#179815=CARTESIAN_POINT('Ctrl Pts',(4.20127629922086,-6.95478679598479,
8.0999240430966));
#179816=CARTESIAN_POINT('Ctrl Pts',(4.19295883117123,-6.95980446271971,
8.09954494727588));
#179817=CARTESIAN_POINT('Ctrl Pts',(4.1767916233789,-6.96951813026772,8.09880785797876));
#179818=CARTESIAN_POINT('Ctrl Pts',(4.16894290974978,-6.97421581598019,
8.09844992386518));
#179819=CARTESIAN_POINT('Ctrl Pts',(4.148031421311,-6.98668404236181,8.0974960051728));
#179820=CARTESIAN_POINT('Ctrl Pts',(4.13495477586364,-6.99443118334179,
8.09689921099505));
#179821=CARTESIAN_POINT('Ctrl Pts',(4.08820580666027,-7.02195027038946,
8.09476465377508));
#179822=CARTESIAN_POINT('Ctrl Pts',(4.05441303839648,-7.04151597170442,
8.09321979085663));
#179823=CARTESIAN_POINT('Ctrl Pts',(3.44455844645803,-7.38877064412927,
8.06530385254013));
#179824=CARTESIAN_POINT('Ctrl Pts',(2.83076068569412,-7.64496356562687,
8.03635968125928));
#179825=CARTESIAN_POINT('Ctrl Pts',(1.76624123764915,-7.94331856062741,
7.98676579225785));
#179826=CARTESIAN_POINT('Ctrl Pts',(1.33062448440572,-8.02778799728385,
7.96670764408717));
#179827=CARTESIAN_POINT('Ctrl Pts',(0.775496644500221,-8.08898196579719,
7.94277600558132));
#179828=CARTESIAN_POINT('Ctrl Pts',(0.660446611907645,-8.09918738663522,
7.93790535856544));
#179829=CARTESIAN_POINT('Ctrl Pts',(0.455676824548966,-8.11295873628207,
7.92943506002988));
#179830=CARTESIAN_POINT('Ctrl Pts',(0.36605036596667,-8.11749644997351,
7.92579858182746));
#179831=CARTESIAN_POINT('Ctrl Pts',(0.259815004791978,-8.1211118533455,
7.92156732655496));
#179832=CARTESIAN_POINT('Ctrl Pts',(0.243269607749017,-8.12162431257731,
7.92091051794962));
#179833=CARTESIAN_POINT('Ctrl Pts',(0.217750631279871,-8.12233665797232,
7.91990070580214));
#179834=CARTESIAN_POINT('Ctrl Pts',(0.208778151374865,-8.12257224081205,
7.91954627008097));
#179835=CARTESIAN_POINT('Ctrl Pts',(0.192395847720523,-8.12297521436143,
7.91890022384888));
#179836=CARTESIAN_POINT('Ctrl Pts',(0.184986157592064,-8.12314733445795,
7.91860842759105));
#179837=CARTESIAN_POINT('Ctrl Pts',(0.168805544615237,-8.12350104402242,
7.91797210607642));
#179838=CARTESIAN_POINT('Ctrl Pts',(0.160034536221588,-8.12367856774821,
7.91762773846986));
#179839=CARTESIAN_POINT('Ctrl Pts',(0.136054314233893,-8.12412507151278,
7.91668772858946));
#179840=CARTESIAN_POINT('Ctrl Pts',(0.120844564410304,-8.12436554747737,
7.91609316786816));
#179841=CARTESIAN_POINT('Ctrl Pts',(0.0466763598827749,-8.12532986964952,
7.91320160250645));
#179842=CARTESIAN_POINT('Ctrl Pts',(-0.0122889087893892,-8.12545465525289,
7.91092654445423));
#179843=CARTESIAN_POINT('Ctrl Pts',(-0.221388313676638,-8.12362097148719,
7.90292955103741));
#179844=CARTESIAN_POINT('Ctrl Pts',(-0.37146443918913,-8.11814307850608,
7.89731873305295));
#179845=CARTESIAN_POINT('Ctrl Pts',(-1.34457009813896,-8.05558092027543,
7.86138567143121));
#179846=CARTESIAN_POINT('Ctrl Pts',(-2.15498582732562,-7.87758984720788,
7.83291006186798));
#179847=CARTESIAN_POINT('Ctrl Pts',(-3.00975943467444,-7.54780382010189,
7.79821889491473));
#179848=CARTESIAN_POINT('Ctrl Pts',(-3.09423291042571,-7.51356884163044,
7.79474483606738));
#179849=CARTESIAN_POINT('Ctrl Pts',(-3.22114261913608,-7.45963228960563,
7.78945382780329));
#179850=CARTESIAN_POINT('Ctrl Pts',(-3.26401458009064,-7.44097321912761,
7.78765390572753));
#179851=CARTESIAN_POINT('Ctrl Pts',(-3.33336314464183,-7.41007613233208,
7.78472186493577));
#179852=CARTESIAN_POINT('Ctrl Pts',(-3.35993921279015,-7.39806370731183,
7.78359329768125));
#179853=CARTESIAN_POINT('Ctrl Pts',(-3.41107049969226,-7.37461993674546,
7.78141244117141));
#179854=CARTESIAN_POINT('Ctrl Pts',(-3.43563438110046,-7.36320837386806,
7.78036046433375));
#179855=CARTESIAN_POINT('Ctrl Pts',(-3.47949209787296,-7.3425662908357,
7.77847456083947));
#179856=CARTESIAN_POINT('Ctrl Pts',(-3.49880745423363,-7.33338198842546,
7.77764132398668));
#179857=CARTESIAN_POINT('Ctrl Pts',(-3.53658784984703,-7.31523446189932,
7.77600629816258));
#179858=CARTESIAN_POINT('Ctrl Pts',(-3.55505567025594,-7.30627730313551,
7.77520459026061));
#179859=CARTESIAN_POINT('Ctrl Pts',(-3.60303835966907,-7.28278001013083,
7.77311500387701));
#179860=CARTESIAN_POINT('Ctrl Pts',(-3.63249913769739,-7.26813044032397,
7.77182548892977));
#179861=CARTESIAN_POINT('Ctrl Pts',(-3.73370930349587,-7.21703392552023,
7.76737209568682));
#179862=CARTESIAN_POINT('Ctrl Pts',(-3.80500512558346,-7.17970052405029,
7.76419423100621));
#179863=CARTESIAN_POINT('Ctrl Pts',(-4.53486090853337,-6.78359321615267,
7.73121007958053));
#179864=CARTESIAN_POINT('Ctrl Pts',(-5.14125102299569,-6.33635816074945,
7.69947678387429));
#179865=CARTESIAN_POINT('Ctrl Pts',(-5.82529055125906,-5.66818198326413,
7.65900168320172));
#179866=CARTESIAN_POINT('Ctrl Pts',(-5.96740705251279,-5.51836510735763,
7.6503131271698));
#179867=CARTESIAN_POINT('Ctrl Pts',(-6.19879604448457,-5.25503430559901,
7.63583922995285));
#179868=CARTESIAN_POINT('Ctrl Pts',(-6.29103179474673,-5.14425693088022,
7.62997231297557));
#179869=CARTESIAN_POINT('Ctrl Pts',(-6.39189037085557,-5.01635096240967,
7.62348980335229));
#179870=CARTESIAN_POINT('Ctrl Pts',(-6.40345525169489,-5.00157978417776,
7.62274545896565));
#179871=CARTESIAN_POINT('Ctrl Pts',(-6.4207619423157,-4.97931649282912,
7.6216301462768));
#179872=CARTESIAN_POINT('Ctrl Pts',(-6.42654198222926,-4.97185426246654,
7.62125741857805));
#179873=CARTESIAN_POINT('Ctrl Pts',(-6.43646502730784,-4.95899705427772,
7.62061713785193));
#179874=CARTESIAN_POINT('Ctrl Pts',(-6.44061427861283,-4.9536069228976,
7.62034929099859));
#179875=CARTESIAN_POINT('Ctrl Pts',(-6.44915072201265,-4.94248870362179,
7.61979800370699));
#179876=CARTESIAN_POINT('Ctrl Pts',(-6.45353706358665,-4.93675996884284,
7.61951460398038));
#179877=CARTESIAN_POINT('Ctrl Pts',(-6.46408547284372,-4.92294524812819,
7.61883278074699));
#179878=CARTESIAN_POINT('Ctrl Pts',(-6.47024001582722,-4.91485351308372,
7.61843472280437));
#179879=CARTESIAN_POINT('Ctrl Pts',(-6.49275756970491,-4.88513277842739,
7.61697751651493));
#179880=CARTESIAN_POINT('Ctrl Pts',(-6.50902756029763,-4.86343328981747,
7.61592298916242));
#179881=CARTESIAN_POINT('Ctrl Pts',(-6.77406394104908,-4.50623863859396,
7.59872303054515));
#179882=CARTESIAN_POINT('Ctrl Pts',(-6.99670818662388,-4.15213277211256,
7.5841195827693));
#179883=CARTESIAN_POINT('Ctrl Pts',(-7.41618764208672,-3.35463143982238,
7.55346737421054));
#179884=CARTESIAN_POINT('Ctrl Pts',(-7.60259977251472,-2.90755416900889,
7.53755568600385));
#179885=CARTESIAN_POINT('Ctrl Pts',(-7.86953076971025,-2.06219278068322,
7.50676350167311));
#179886=CARTESIAN_POINT('Ctrl Pts',(-7.96211877441408,-1.66936444718148,
7.49220103349142));
#179887=CARTESIAN_POINT('Ctrl Pts',(-8.03021801509914,-1.23948548241302,
7.47546118782563));
#179888=CARTESIAN_POINT('Ctrl Pts',(-8.03506977776106,-1.20763374810521,
7.47421639424351));
#179889=CARTESIAN_POINT('Ctrl Pts',(-8.04170330318605,-1.16227412645094,
7.47243717475473));
#179890=CARTESIAN_POINT('Ctrl Pts',(-8.043640759158,-1.14878914381878,7.47190741067092));
#179891=CARTESIAN_POINT('Ctrl Pts',(-8.04691974277996,-1.1255519183334,
7.47099309931554));
#179892=CARTESIAN_POINT('Ctrl Pts',(-8.04827748155222,-1.11580197468481,
7.47060903788999));
#179893=CARTESIAN_POINT('Ctrl Pts',(-8.0508375941445,-1.09716996491519,
7.4698742706666));
#179894=CARTESIAN_POINT('Ctrl Pts',(-8.05204299659385,-1.08828832558782,
7.46952365605336));
#179895=CARTESIAN_POINT('Ctrl Pts',(-8.05482410754143,-1.06753898490405,
7.46870370087325));
#179896=CARTESIAN_POINT('Ctrl Pts',(-8.05638828600611,-1.05566977381634,
7.46823401631452));
#179897=CARTESIAN_POINT('Ctrl Pts',(-8.06167364626418,-1.0148677445927,
7.46661717166501));
#179898=CARTESIAN_POINT('Ctrl Pts',(-8.06526522551564,-0.985918525290401,
7.46546614354029));
#179899=CARTESIAN_POINT('Ctrl Pts',(-8.10168630555391,-0.67882770478392,
7.45321446269102));
#179900=CARTESIAN_POINT('Ctrl Pts',(-8.12026749782283,-0.399205255910186,
7.44168764108077));
#179901=CARTESIAN_POINT('Ctrl Pts',(-8.12566580845965,-0.0312605098491741,
7.42603884627491));
#179902=CARTESIAN_POINT('Ctrl Pts',(-8.12552815692169,0.0566895633651244,
7.4222630430183));
#179903=CARTESIAN_POINT('Ctrl Pts',(-8.11591258082036,0.596845258737921,
7.39887079871206));
#179904=CARTESIAN_POINT('Ctrl Pts',(-8.07011624145231,1.04758863163167,
7.37842566821632));
#179905=CARTESIAN_POINT('Ctrl Pts',(-7.92731785978853,1.8119497849267,7.34337567173789));
#179906=CARTESIAN_POINT('Ctrl Pts',(-7.84841626461965,2.1278886018736,7.3287895323074));
#179907=CARTESIAN_POINT('Ctrl Pts',(-7.70980537876419,2.56850799508236,
7.30892515066826));
#179908=CARTESIAN_POINT('Ctrl Pts',(-7.66555168973068,2.69771246994982,
7.30316198463242));
#179909=CARTESIAN_POINT('Ctrl Pts',(-7.59614441358077,2.88483085741031,
7.29496020799337));
#179910=CARTESIAN_POINT('Ctrl Pts',(-7.57354118326881,2.94365989215785,
7.29240365041295));
#179911=CARTESIAN_POINT('Ctrl Pts',(-7.53987257898884,3.02833262489012,
7.28875750915561));
#179912=CARTESIAN_POINT('Ctrl Pts',(-7.5293555430975,3.05438735736778,7.28763990774156));
#179913=CARTESIAN_POINT('Ctrl Pts',(-7.5145965565082,3.09041154358981,7.28610004706287));
#179914=CARTESIAN_POINT('Ctrl Pts',(-7.51046957890354,3.10042765143268,
7.28567248450194));
#179915=CARTESIAN_POINT('Ctrl Pts',(-7.50345776048527,3.11734906667848,
7.28495108287856));
#179916=CARTESIAN_POINT('Ctrl Pts',(-7.50058339563923,3.12425867886637,
7.28465677213816));
#179917=CARTESIAN_POINT('Ctrl Pts',(-7.49486730198034,3.13794609607371,
7.28407426865178));
#179918=CARTESIAN_POINT('Ctrl Pts',(-7.4920259153668,3.14472403560261,7.28378606113987));
#179919=CARTESIAN_POINT('Ctrl Pts',(-7.48572913914173,3.15968760508366,
7.28315031236115));
#179920=CARTESIAN_POINT('Ctrl Pts',(-7.48226950847464,3.16787144778167,
7.2828029564108));
#179921=CARTESIAN_POINT('Ctrl Pts',(-7.47007070796946,3.19659654872677,
7.2815849097379));
#179922=CARTESIAN_POINT('Ctrl Pts',(-7.46126027198687,3.2171075585464,7.28071726426838));
#179923=CARTESIAN_POINT('Ctrl Pts',(-7.33987764428502,3.49650979661669,
7.26892356072496));
#179924=CARTESIAN_POINT('Ctrl Pts',(-7.21396527920489,3.74941410588792,
7.2585382690809));
#179925=CARTESIAN_POINT('Ctrl Pts',(-6.86103050427722,4.37442016803562,
7.2325510889286));
#179926=CARTESIAN_POINT('Ctrl Pts',(-6.61679079851957,4.7357555489666,7.21717627980339));
#179927=CARTESIAN_POINT('Ctrl Pts',(-5.97215748615665,5.54155253418819,
7.17968465351304));
#179928=CARTESIAN_POINT('Ctrl Pts',(-5.549408455108,5.96485191978368,7.15719195527464));
#179929=CARTESIAN_POINT('Ctrl Pts',(-4.99597346967715,6.40880054611747,
7.12977449297168));
#179930=CARTESIAN_POINT('Ctrl Pts',(-4.9062968159236,6.47770998082798,7.12538876577189));
#179931=CARTESIAN_POINT('Ctrl Pts',(-4.77498594283834,6.57432056041182,
7.11903810587708));
#179932=CARTESIAN_POINT('Ctrl Pts',(-4.73448824508579,6.60354470062865,
7.11708899843027));
#179933=CARTESIAN_POINT('Ctrl Pts',(-4.66281366740475,6.65426857140178,
7.11365513904391));
#179934=CARTESIAN_POINT('Ctrl Pts',(-4.63175103283471,6.6759271920774,7.1121720778364));
#179935=CARTESIAN_POINT('Ctrl Pts',(-4.56655066807166,6.7207144542792,7.10906938499359));
#179936=CARTESIAN_POINT('Ctrl Pts',(-4.53238599631842,6.7438019649925,7.10744937750362));
#179937=CARTESIAN_POINT('Ctrl Pts',(-4.44206404910055,6.8038425577854,7.10318109711383));
#179938=CARTESIAN_POINT('Ctrl Pts',(-4.38562150698715,6.84036040635741,
7.10052847164612));
#179939=CARTESIAN_POINT('Ctrl Pts',(-4.13030844277705,7.00108671385293,
7.08859114512913));
#179940=CARTESIAN_POINT('Ctrl Pts',(-3.92657334985303,7.11735075261285,
7.0792288084521));
#179941=CARTESIAN_POINT('Ctrl Pts',(-3.69550106896186,7.23627012680759,
7.06876990993719));
#179942=CARTESIAN_POINT('Ctrl Pts',(-3.67284842843474,7.24779400351911,
7.06774627856101));
#179943=CARTESIAN_POINT('Ctrl Pts',(-3.20770173738158,7.4816832564008,7.04676157098265));
#179944=CARTESIAN_POINT('Ctrl Pts',(-2.74585191758023,7.66323864455631,
7.02651657541934));
#179945=CARTESIAN_POINT('Ctrl Pts',(-2.16117722389955,7.83338563846384,
7.00195916229492));
#179946=CARTESIAN_POINT('Ctrl Pts',(-2.05134039133282,7.86286338396046,
6.99739262479145));
#179947=CARTESIAN_POINT('Ctrl Pts',(-1.90679551975368,7.89842094187259,
6.99145350898929));
#179948=CARTESIAN_POINT('Ctrl Pts',(-1.87261656037477,7.90659406850063,
6.99005426983802));
#179949=CARTESIAN_POINT('Ctrl Pts',(-1.79235027644293,7.92523826995822,
6.98678081330815));
#179950=CARTESIAN_POINT('Ctrl Pts',(-1.74622235047893,7.93552951596186,
6.98490925483222));
#179951=CARTESIAN_POINT('Ctrl Pts',(-1.67824647164587,7.95007368156257,
6.98216629364125));
#179952=CARTESIAN_POINT('Ctrl Pts',(-1.65646679806028,7.95464018776109,
6.98128970645587));
#179953=CARTESIAN_POINT('Ctrl Pts',(-1.61652387749098,7.96284379054159,
6.97968633436949));
#179954=CARTESIAN_POINT('Ctrl Pts',(-1.59836647930091,7.96650834932912,
6.97895905787417));
#179955=CARTESIAN_POINT('Ctrl Pts',(-1.55735235247661,7.97464002883764,
6.97731964527661));
#179956=CARTESIAN_POINT('Ctrl Pts',(-1.53448860954826,7.97907103940914,
6.97640809438307));
#179957=CARTESIAN_POINT('Ctrl Pts',(-1.47505548828391,7.99032431816325,
6.97404418834783));
#179958=CARTESIAN_POINT('Ctrl Pts',(-1.43845767320748,7.99699386923838,
6.9725940568141));
#179959=CARTESIAN_POINT('Ctrl Pts',(-1.1850270053247,8.04138280916626,6.96258521506639));
#179960=CARTESIAN_POINT('Ctrl Pts',(-0.96678317271843,8.07053026927719,
6.95412927206227));
#179961=CARTESIAN_POINT('Ctrl Pts',(-0.573608558143245,8.10686133038639,
6.9389515139325));
#179962=CARTESIAN_POINT('Ctrl Pts',(-0.399120584786872,8.11732282281341,
6.93223603027996));
#179963=CARTESIAN_POINT('Ctrl Pts',(-0.113961355100009,8.1252023604628,
6.92121873631451));
#179964=CARTESIAN_POINT('Ctrl Pts',(-0.00344080132436661,8.12600076934443,
6.91693867788918));
#179965=CARTESIAN_POINT('Ctrl Pts',(0.153896966162853,8.12392745351893,
6.91081993913141));
#179966=CARTESIAN_POINT('Ctrl Pts',(0.200726542749659,8.12290529175856,
6.90899557764855));
#179967=CARTESIAN_POINT('Ctrl Pts',(0.282921203010633,8.12039997945412,
6.90578708406969));
#179968=CARTESIAN_POINT('Ctrl Pts',(0.318290368681357,8.11909055649516,
6.90440435854074));
#179969=CARTESIAN_POINT('Ctrl Pts',(0.392340890805987,8.11586446605905,
6.9015047369219));
#179970=CARTESIAN_POINT('Ctrl Pts',(0.431019368450027,8.11390224840457,
6.89998751152092));
#179971=CARTESIAN_POINT('Ctrl Pts',(0.534042672797172,8.10793698406128,
6.89593868383245));
#179972=CARTESIAN_POINT('Ctrl Pts',(0.59835621223947,8.10344454513105,6.89340325719327));
#179973=CARTESIAN_POINT('Ctrl Pts',(1.00324152840568,8.07031605083843,6.87738872789994));
#179974=CARTESIAN_POINT('Ctrl Pts',(1.34177188564481,8.02098101831701,6.86374158095071));
#179975=CARTESIAN_POINT('Ctrl Pts',(1.85459408217703,7.91286383608297,6.84280958408104));
#179976=CARTESIAN_POINT('Ctrl Pts',(2.03169094336306,7.86925448640611,6.83553700447935));
#179977=CARTESIAN_POINT('Ctrl Pts',(2.24912107997073,7.80788331740689,6.82660761787461));
#179978=CARTESIAN_POINT('Ctrl Pts',(2.29097489695784,7.79570532939139,6.82488883832693));
#179979=CARTESIAN_POINT('Ctrl Pts',(2.35373497259993,7.77689527612172,6.82231276765226));
#179980=CARTESIAN_POINT('Ctrl Pts',(2.37471550717156,7.77051444384044,6.82145183272699));
#179981=CARTESIAN_POINT('Ctrl Pts',(2.41469682568755,7.7581778329147,6.81981165584626));
#179982=CARTESIAN_POINT('Ctrl Pts',(2.43370197224416,7.75223701653842,6.81903216819185));
#179983=CARTESIAN_POINT('Ctrl Pts',(2.47748460362841,7.73837413629093,6.81723662437312));
#179984=CARTESIAN_POINT('Ctrl Pts',(2.50224629014142,7.73040281902605,6.81622127160013));
#179985=CARTESIAN_POINT('Ctrl Pts',(2.56936410481981,7.70843988313111,6.81346891702132));
#179986=CARTESIAN_POINT('Ctrl Pts',(2.61164407699267,7.69421812652251,6.81173490079762));
#179987=CARTESIAN_POINT('Ctrl Pts',(2.84790229169533,7.61257595434493,6.8020385380735));
#179988=CARTESIAN_POINT('Ctrl Pts',(3.03938889924414,7.5381679986173,6.79415245964485));
#179989=CARTESIAN_POINT('Ctrl Pts',(3.23201800181182,7.45478153987207,6.78610264548836));
#179990=CARTESIAN_POINT('Ctrl Pts',(3.23618258423733,7.45297460432817,6.78592855508331));
#179991=CARTESIAN_POINT('Ctrl Pts',(3.31091498706415,7.42047514374496,6.78280352748804));
#179992=CARTESIAN_POINT('Ctrl Pts',(3.38104480385011,7.38878511343108,6.7798546212425));
#179993=CARTESIAN_POINT('Ctrl Pts',(3.66554315654899,7.25532826509284,6.76780905966538));
#179994=CARTESIAN_POINT('Ctrl Pts',(3.87585341173315,7.14519097639767,6.75870773653853));
#179995=CARTESIAN_POINT('Ctrl Pts',(4.14474530550063,6.98900575353771,6.74669834615255));
#179996=CARTESIAN_POINT('Ctrl Pts',(4.20794370920409,6.95113837776932,6.74384794559773));
#179997=CARTESIAN_POINT('Ctrl Pts',(4.36176045991743,6.85610756234524,6.73683765943862));
#179998=CARTESIAN_POINT('Ctrl Pts',(4.45177966673619,6.79800138311449,6.73267166060439));
#179999=CARTESIAN_POINT('Ctrl Pts',(4.59084941709583,6.70428649628685,6.72612996389287));
#180000=CARTESIAN_POINT('Ctrl Pts',(4.64069558631785,6.66988007635293,6.72376342215126));
#180001=CARTESIAN_POINT('Ctrl Pts',(4.73543647177023,6.60290877862507,6.71922262612382));
#180002=CARTESIAN_POINT('Ctrl Pts',(4.78039165042046,6.5704351879868,6.71704911487873));
#180003=CARTESIAN_POINT('Ctrl Pts',(4.88912097587145,6.49018741059794,6.71174561180416));
#180004=CARTESIAN_POINT('Ctrl Pts',(4.95253152735596,6.44193045193084,6.70861281418788));
#180005=CARTESIAN_POINT('Ctrl Pts',(5.17186400146934,6.2698603368207,6.69763640265128));
#180006=CARTESIAN_POINT('Ctrl Pts',(5.32393619346197,6.14125629959123,6.68977121629631));
#180007=CARTESIAN_POINT('Ctrl Pts',(5.55119565259601,5.93427689029336,6.6776403218635));
#180008=CARTESIAN_POINT('Ctrl Pts',(5.62979524603987,5.85976287954128,6.67337050000588));
#180009=CARTESIAN_POINT('Ctrl Pts',(5.73758103940436,5.75340867349887,6.6674173026549));
#180010=CARTESIAN_POINT('Ctrl Pts',(5.76803843152039,5.72287342338029,6.66572379276338));
#180011=CARTESIAN_POINT('Ctrl Pts',(5.8257065919205,5.66412978541909,6.6624963737859));
#180012=CARTESIAN_POINT('Ctrl Pts',(5.85295918608722,5.63596418538932,6.66096199776645));
#180013=CARTESIAN_POINT('Ctrl Pts',(5.94161647773084,5.54300012504445,6.65593806446214));
#180014=CARTESIAN_POINT('Ctrl Pts',(6.00215730512554,5.47738665123967,6.65245576057196));
#180015=CARTESIAN_POINT('Ctrl Pts',(6.17649973924291,5.28207410494277,6.64225332444279));
#180016=CARTESIAN_POINT('Ctrl Pts',(6.28726577251524,5.14973251800901,6.63554457889934));
#180017=CARTESIAN_POINT('Ctrl Pts',(6.44104691979512,4.95363306853353,6.62583134624681));
#180018=CARTESIAN_POINT('Ctrl Pts',(6.48750297118287,4.89263437812307,6.62284042754036));
#180019=CARTESIAN_POINT('Ctrl Pts',(6.57266211790494,4.7774711202026,6.61724465829791));
#180020=CARTESIAN_POINT('Ctrl Pts',(6.61157640712332,4.72347065147373,6.61464113603285));
#180021=CARTESIAN_POINT('Ctrl Pts',(6.68119531416642,4.6243158944227,6.60989444328971));
#180022=CARTESIAN_POINT('Ctrl Pts',(6.71211666789849,4.57931852238201,6.60775275845275));
#180023=CARTESIAN_POINT('Ctrl Pts',(6.7806606895358,4.47738593186195,6.60292728369555));
#180024=CARTESIAN_POINT('Ctrl Pts',(6.81802428594229,4.42028154687014,6.60024195024954));
#180025=CARTESIAN_POINT('Ctrl Pts',(6.93068741383284,4.24326605037025,6.59196911941288));
#180026=CARTESIAN_POINT('Ctrl Pts',(7.00357515034894,4.12185267120524,6.5863657564496));
#180027=CARTESIAN_POINT('Ctrl Pts',(7.13877674625197,3.88269005900418,6.57545219426951));
#180028=CARTESIAN_POINT('Ctrl Pts',(7.20144151866026,3.76518993752006,6.5701461306324));
#180029=CARTESIAN_POINT('Ctrl Pts',(7.39781159943072,3.37413100157306,6.55266714804397));
#180030=CARTESIAN_POINT('Ctrl Pts',(7.51903306928777,3.09459498170755,6.54044844891182));
#180031=CARTESIAN_POINT('Ctrl Pts',(7.64656428269432,2.74843534593787,6.52574662935895));
#180032=CARTESIAN_POINT('Ctrl Pts',(7.66812658004269,2.68768989865309,6.52318263928415));
#180033=CARTESIAN_POINT('Ctrl Pts',(7.71296085907612,2.55644920807708,6.51768042639647));
#180034=CARTESIAN_POINT('Ctrl Pts',(7.73599424129968,2.48587831419442,6.51474465795376));
#180035=CARTESIAN_POINT('Ctrl Pts',(7.76661079117959,2.38752435064765,6.51068827575413));
#180036=CARTESIAN_POINT('Ctrl Pts',(7.77501807843115,2.36000203302036,6.50955697749339));
#180037=CARTESIAN_POINT('Ctrl Pts',(7.78910994264862,2.31297783533513,6.50763080211099));
#180038=CARTESIAN_POINT('Ctrl Pts',(7.79486791673719,2.29349827328752,6.5068348590345));
#180039=CARTESIAN_POINT('Ctrl Pts',(7.80568970057907,2.2563760230479,6.50532188057857));
#180040=CARTESIAN_POINT('Ctrl Pts',(7.81076689172109,2.23873737331282,6.50460464626402));
#180041=CARTESIAN_POINT('Ctrl Pts',(7.82503322855306,2.18853543035179,6.50256806908899));
#180042=CARTESIAN_POINT('Ctrl Pts',(7.8340788150833,2.15593169951779,6.50125103362099));
#180043=CARTESIAN_POINT('Ctrl Pts',(7.8886509379055,1.95435377673246,6.49313938982417));
#180044=CARTESIAN_POINT('Ctrl Pts',(7.92891277239194,1.78399997108743,6.48641778450668));
#180045=CARTESIAN_POINT('Ctrl Pts',(8.01352897698686,1.36610069993303,6.47008156455319));
#180046=CARTESIAN_POINT('Ctrl Pts',(8.05195484632911,1.11754224131128,6.4604901689047));
#180047=CARTESIAN_POINT('Ctrl Pts',(8.08901348025839,0.772466144738703,
6.44714064034087));
#180048=CARTESIAN_POINT('Ctrl Pts',(8.09754913961777,0.677156404271413,
6.44345074189368));
#180049=CARTESIAN_POINT('Ctrl Pts',(8.10975373398638,0.507124178290068,
6.43685352159689));
#180050=CARTESIAN_POINT('Ctrl Pts',(8.11407783103944,0.432459727183408,
6.43395163544928));
#180051=CARTESIAN_POINT('Ctrl Pts',(8.11916750736217,0.31697352879727,6.42945271224466));
#180052=CARTESIAN_POINT('Ctrl Pts',(8.12065721446378,0.276187652715635,
6.42786183699706));
#180053=CARTESIAN_POINT('Ctrl Pts',(8.12285490345266,0.200359892209235,
6.42489998955969));
#180054=CARTESIAN_POINT('Ctrl Pts',(8.12364356278413,0.165321273295582,
6.42352973111424));
#180055=CARTESIAN_POINT('Ctrl Pts',(8.1249006836545,0.0869269813255745,
6.42046003758502));
#180056=CARTESIAN_POINT('Ctrl Pts',(8.12524885851972,0.0435704858206847,
6.41875963865154));
#180057=CARTESIAN_POINT('Ctrl Pts',(8.12525232991186,-0.0886077110125687,
6.4135671185659));
#180058=CARTESIAN_POINT('Ctrl Pts',(8.12379824240537,-0.177422407388084,
6.41006615265063));
#180059=CARTESIAN_POINT('Ctrl Pts',(8.11682034707346,-0.390299132962066,
6.40164541196985));
#180060=CARTESIAN_POINT('Ctrl Pts',(8.10990803241573,-0.514293045013356,
6.39671642998146));
#180061=CARTESIAN_POINT('Ctrl Pts',(8.08878601781311,-0.782428510927059,
6.38601217876998));
#180062=CARTESIAN_POINT('Ctrl Pts',(8.07355855089664,-0.926447934362717,
6.38023404808976));
#180063=CARTESIAN_POINT('Ctrl Pts',(8.03214735229637,-1.23817823809826,
6.36769357498648));
#180064=CARTESIAN_POINT('Ctrl Pts',(8.00454069269799,-1.40563347901672,
6.36093538142092));
#180065=CARTESIAN_POINT('Ctrl Pts',(7.96508484775443,-1.60570354945919,
6.35287829542204));
#180066=CARTESIAN_POINT('Ctrl Pts',(7.95824592922307,-1.63926271979714,
6.35152746725958));
#180067=CARTESIAN_POINT('Ctrl Pts',(7.94737705343012,-1.69092562092554,
6.34944949725413));
#180068=CARTESIAN_POINT('Ctrl Pts',(7.94349696303247,-1.70906041019681,
6.34872038492125));
#180069=CARTESIAN_POINT('Ctrl Pts',(7.93600915400054,-1.74348056829766,
6.34733720531024));
#180070=CARTESIAN_POINT('Ctrl Pts',(7.93241330782144,-1.75976842238526,
6.34668296887366));
#180071=CARTESIAN_POINT('Ctrl Pts',(7.92353739585709,-1.79939300175523,
6.34509219263836));
#180072=CARTESIAN_POINT('Ctrl Pts',(7.91820434942849,-1.82271773045062,
6.34415649319395));
#180073=CARTESIAN_POINT('Ctrl Pts',(7.89986991021914,-1.90130641229966,
6.34100571826802));
#180074=CARTESIAN_POINT('Ctrl Pts',(7.88639230614848,-1.95645780314268,
6.33879776999435));
#180075=CARTESIAN_POINT('Ctrl Pts',(7.85210127511134,-2.09066384317768,
6.33342832649012));
#180076=CARTESIAN_POINT('Ctrl Pts',(7.83067064544867,-2.16955459697653,
6.33027487996843));
#180077=CARTESIAN_POINT('Ctrl Pts',(7.69761994025812,-2.63166163046686,
6.31178984219167));
#180078=CARTESIAN_POINT('Ctrl Pts',(7.55907402456714,-3.00655981756993,
6.29672429453929));
#180079=CARTESIAN_POINT('Ctrl Pts',(7.22927055340681,-3.73017709404831,
6.26648240530952));
#180080=CARTESIAN_POINT('Ctrl Pts',(7.0388702101042,-4.0780964977272,6.25134483720988));
#180081=CARTESIAN_POINT('Ctrl Pts',(6.78407955916589,-4.47228386014423,
6.23311409154311));
#180082=CARTESIAN_POINT('Ctrl Pts',(6.74346606891664,-4.53329060259494,
6.23026059779853));
#180083=CARTESIAN_POINT('Ctrl Pts',(6.67775340821961,-4.62916204609271,
6.22572361506056));
#180084=CARTESIAN_POINT('Ctrl Pts',(6.65319340791715,-4.66439163137536,
6.22404490304277));
#180085=CARTESIAN_POINT('Ctrl Pts',(6.60665046153806,-4.73003864165022,
6.22089478824505));
#180086=CARTESIAN_POINT('Ctrl Pts',(6.58473380664365,-4.76050171281416,
6.21942398551053));
#180087=CARTESIAN_POINT('Ctrl Pts',(6.53496280221221,-4.82867962352841,
6.21611169725738));
#180088=CARTESIAN_POINT('Ctrl Pts',(6.50699148376161,-4.86630738279328,
6.21426928946835));
#180089=CARTESIAN_POINT('Ctrl Pts',(6.42101029709143,-4.97990467058126,
6.20866289566927));
#180090=CARTESIAN_POINT('Ctrl Pts',(6.36198435342906,-5.05509433177263,
6.20489113107061));
#180091=CARTESIAN_POINT('Ctrl Pts',(6.05011725604874,-5.4382469709654,6.18534947580899));
#180092=CARTESIAN_POINT('Ctrl Pts',(5.77620356263925,-5.72834277345652,
6.16952276348681));
#180093=CARTESIAN_POINT('Ctrl Pts',(5.0645170486095,-6.37890855708647,6.13027338027674));
#180094=CARTESIAN_POINT('Ctrl Pts',(4.60819705605136,-6.71597053437957,
6.10639126153788));
#180095=CARTESIAN_POINT('Ctrl Pts',(3.84816781490912,-7.16318486787771,
6.06909059857595));
#180096=CARTESIAN_POINT('Ctrl Pts',(3.5665918704455,-7.30746514284052,6.05577989717409));
#180097=CARTESIAN_POINT('Ctrl Pts',(3.21325917657124,-7.4632134002591,6.04014392924312));
#180098=CARTESIAN_POINT('Ctrl Pts',(3.14883451750185,-7.49062282482243,
6.03733543806319));
#180099=CARTESIAN_POINT('Ctrl Pts',(3.07082393472642,-7.52262804402004,
6.03399211057144));
#180100=CARTESIAN_POINT('Ctrl Pts',(3.05757083009318,-7.52802450506658,
6.03342609993361));
#180101=CARTESIAN_POINT('Ctrl Pts',(3.03586744692814,-7.53679502147722,
6.03250251552035));
#180102=CARTESIAN_POINT('Ctrl Pts',(3.0274256636631,-7.54018993148782,6.03214409601736));
#180103=CARTESIAN_POINT('Ctrl Pts',(3.01230382465039,-7.54624177404082,
6.03150354448433));
#180104=CARTESIAN_POINT('Ctrl Pts',(3.00562591907132,-7.54890403166635,
6.03122119132868));
#180105=CARTESIAN_POINT('Ctrl Pts',(2.99148086956729,-7.55452144482498,
6.03062422551331));
#180106=CARTESIAN_POINT('Ctrl Pts',(2.98401285609766,-7.55747440144834,
6.03030970612527));
#180107=CARTESIAN_POINT('Ctrl Pts',(2.96413606855629,-7.56529990471083,
6.02947434770399));
#180108=CARTESIAN_POINT('Ctrl Pts',(2.95171962795997,-7.57015300518029,
6.02895434948083));
#180109=CARTESIAN_POINT('Ctrl Pts',(2.89394677691967,-7.59257040239105,
6.02654349991929));
#180110=CARTESIAN_POINT('Ctrl Pts',(2.84844414513394,-7.60975817291452,
6.02466949191959));
#180111=CARTESIAN_POINT('Ctrl Pts',(2.44874655658326,-7.75664894937057,
6.00844180996087));
#180112=CARTESIAN_POINT('Ctrl Pts',(2.08604493589621,-7.86196049688276,
5.99529705772231));
#180113=CARTESIAN_POINT('Ctrl Pts',(1.03945584850741,-8.08827540521311,
5.95902652866962));
#180114=CARTESIAN_POINT('Ctrl Pts',(0.345643442502322,-8.14746666044795,
5.93670786753447));
#180115=CARTESIAN_POINT('Ctrl Pts',(-0.597646219634858,-8.10711503305624,
5.90278417019366));
#180116=CARTESIAN_POINT('Ctrl Pts',(-0.847387615950354,-8.08482637934851,
5.89348793007021));
#180117=CARTESIAN_POINT('Ctrl Pts',(-1.12417482889773,-8.04715756974659,
5.88273011742332));
#180118=CARTESIAN_POINT('Ctrl Pts',(-1.15263909094815,-8.0431298077382,
5.88161847649228));
#180119=CARTESIAN_POINT('Ctrl Pts',(-1.19380699916249,-8.03708142628259,
5.88000287080551));
#180120=CARTESIAN_POINT('Ctrl Pts',(-1.20652829804827,-8.03518154543719,
5.87950254765853));
#180121=CARTESIAN_POINT('Ctrl Pts',(-1.22888439551128,-8.03178845360035,
5.87862137284333));
#180122=CARTESIAN_POINT('Ctrl Pts',(-1.23852113231481,-8.03030809028723,
5.87824090939046));
#180123=CARTESIAN_POINT('Ctrl Pts',(-1.25835564662612,-8.02722462583741,
5.87745653449831));
#180124=CARTESIAN_POINT('Ctrl Pts',(-1.26855307788293,-8.02561942872277,
5.87705256042104));
#180125=CARTESIAN_POINT('Ctrl Pts',(-1.29448170544511,-8.0214873017863,
5.87602358451191));
#180126=CARTESIAN_POINT('Ctrl Pts',(-1.31020854664372,-8.01893353129054,
5.87539777364794));
#180127=CARTESIAN_POINT('Ctrl Pts',(-1.3730919341761,-8.00853241381991,
5.87288867097006));
#180128=CARTESIAN_POINT('Ctrl Pts',(-1.4201858728081,-8.00031529844626,
5.87099423424373));
#180129=CARTESIAN_POINT('Ctrl Pts',(-1.72303468425219,-7.94471486958922,
5.85871123342657));
#180130=CARTESIAN_POINT('Ctrl Pts',(-1.97644567524322,-7.88549239591398,
5.84796478218518));
#180131=CARTESIAN_POINT('Ctrl Pts',(-2.59163390453521,-7.71020201346001,
5.82074546388056));
#180132=CARTESIAN_POINT('Ctrl Pts',(-2.9489396503776,-7.58073237732512,
5.80392948868379));
#180133=CARTESIAN_POINT('Ctrl Pts',(-3.68546763559995,-7.25387480309033,
5.76780109843996));
#180134=CARTESIAN_POINT('Ctrl Pts',(-4.06086922836336,-7.0505836638282,
5.74849142393269));
#180135=CARTESIAN_POINT('Ctrl Pts',(-4.60862968298228,-6.69563276166751,
5.72031328829264));
#180136=CARTESIAN_POINT('Ctrl Pts',(-4.7934564059013,-6.56458450353027,
5.71082429191021));
#180137=CARTESIAN_POINT('Ctrl Pts',(-4.98768420393661,-6.41428545528504,
5.70101965103718));
#180138=CARTESIAN_POINT('Ctrl Pts',(-5.00273301871611,-6.40255526895245,
5.70026075932994));
#180139=CARTESIAN_POINT('Ctrl Pts',(-5.02534892617591,-6.38479829813846,
5.69912123422882));
#180140=CARTESIAN_POINT('Ctrl Pts',(-5.03294673870893,-6.37881088166991,
5.6987385759128));
#180141=CARTESIAN_POINT('Ctrl Pts',(-5.04609027587779,-6.36841508369905,
5.6980768670434));
#180142=CARTESIAN_POINT('Ctrl Pts',(-5.05164095092335,-6.3640129991996,
5.69779749869067));
#180143=CARTESIAN_POINT('Ctrl Pts',(-5.06315734618847,-6.35485510907926,
5.69721802314798));
#180144=CARTESIAN_POINT('Ctrl Pts',(-5.06912214064605,-6.35009814832334,
5.69691797413697));
#180145=CARTESIAN_POINT('Ctrl Pts',(-5.08311297686504,-6.33890809433681,
5.69621436626992));
#180146=CARTESIAN_POINT('Ctrl Pts',(-5.09113353112616,-6.33246813915875,
5.69581114534354));
#180147=CARTESIAN_POINT('Ctrl Pts',(-5.11716616851667,-6.311484288515,5.69450277521781));
#180148=CARTESIAN_POINT('Ctrl Pts',(-5.13512841444604,-6.29687856803288,
5.69360060702961));
#180149=CARTESIAN_POINT('Ctrl Pts',(-5.17727803395046,-6.26230496239157,
5.6914844527172));
#180150=CARTESIAN_POINT('Ctrl Pts',(-5.20141277987012,-6.24227333638913,
5.69027340893791));
#180151=CARTESIAN_POINT('Ctrl Pts',(-5.48949761964464,-6.00033461408997,
5.67581873829444));
#180152=CARTESIAN_POINT('Ctrl Pts',(-5.7391931963483,-5.76196887449449,
5.66328538900836));
#180153=CARTESIAN_POINT('Ctrl Pts',(-6.15587418725555,-5.31014766605553,
5.64114682175235));
#180154=CARTESIAN_POINT('Ctrl Pts',(-6.32876330481973,-5.1028629732481,
5.63151489822027));
#180155=CARTESIAN_POINT('Ctrl Pts',(-6.78351995582515,-4.49889000133021,
5.60419711140439));
#180156=CARTESIAN_POINT('Ctrl Pts',(-7.04053775527606,-4.08496589091026,
5.58624595265662));
#180157=CARTESIAN_POINT('Ctrl Pts',(-7.2834664003618,-3.60191204589582,
5.56543942619082));
#180158=CARTESIAN_POINT('Ctrl Pts',(-7.30744357641358,-3.55301583217703,
5.56333594000879));
#180159=CARTESIAN_POINT('Ctrl Pts',(-7.34289665984757,-3.47883983662502,
5.56014883509978));
#180160=CARTESIAN_POINT('Ctrl Pts',(-7.3547376163541,-3.45373602818275,
5.55907087582187));
#180161=CARTESIAN_POINT('Ctrl Pts',(-7.37571027162546,-3.40867528428791,
5.55713718840274));
#180162=CARTESIAN_POINT('Ctrl Pts',(-7.38489020297537,-3.3887410479115,
5.55628218241575));
#180163=CARTESIAN_POINT('Ctrl Pts',(-7.40367061626517,-3.34752060961314,
5.5545150699663));
#180164=CARTESIAN_POINT('Ctrl Pts',(-7.41326033961299,-3.32622969113096,
5.55360280443975));
#180165=CARTESIAN_POINT('Ctrl Pts',(-7.43718893031105,-3.27248638254035,
5.55130099919129));
#180166=CARTESIAN_POINT('Ctrl Pts',(-7.45140723759167,-3.23998093676556,
5.54990968780126));
#180167=CARTESIAN_POINT('Ctrl Pts',(-7.5072290452423,-3.11005172897094,
5.54435080000825));
#180168=CARTESIAN_POINT('Ctrl Pts',(-7.54713794642953,-3.01191268001567,
5.54015719238398));
#180169=CARTESIAN_POINT('Ctrl Pts',(-7.87903707971608,-2.14769227750029,
5.50322087029232));
#180170=CARTESIAN_POINT('Ctrl Pts',(-8.05541768030784,-1.34230376443491,
5.4680569872185));
#180171=CARTESIAN_POINT('Ctrl Pts',(-8.12089080699165,-0.32985724350419,
5.4254761944709));
#180172=CARTESIAN_POINT('Ctrl Pts',(-8.12646672181003,-0.134968312819105,
5.41739007952805));
#180173=CARTESIAN_POINT('Ctrl Pts',(-8.12458564705031,0.12002795536611,
5.40707588049529));
#180174=CARTESIAN_POINT('Ctrl Pts',(-8.12347574967377,0.180112734732693,
5.40466501000413));
#180175=CARTESIAN_POINT('Ctrl Pts',(-8.12128124929383,0.254319730730189,
5.40171538954389));
#180176=CARTESIAN_POINT('Ctrl Pts',(-8.1208261899965,0.268457911773179,
5.40115466960329));
#180177=CARTESIAN_POINT('Ctrl Pts',(-8.12001203901789,0.291852454346871,
5.40022898440858));
#180178=CARTESIAN_POINT('Ctrl Pts',(-8.11967403561938,0.301109490127723,
5.39986325316387));
#180179=CARTESIAN_POINT('Ctrl Pts',(-8.11903385230963,0.317856988594379,
5.39920261111447));
#180180=CARTESIAN_POINT('Ctrl Pts',(-8.11873713531192,0.325347642247356,
5.39890749711187));
#180181=CARTESIAN_POINT('Ctrl Pts',(-8.1180791467036,0.341397000374113,
5.39827599979355));
#180182=CARTESIAN_POINT('Ctrl Pts',(-8.11771470568656,0.349955571162441,
5.39793973723901));
#180183=CARTESIAN_POINT('Ctrl Pts',(-8.11668863042323,0.373187602312117,
5.39702832568894));
#180184=CARTESIAN_POINT('Ctrl Pts',(-8.11600073939201,0.387859912290294,
5.39645419731952));
#180185=CARTESIAN_POINT('Ctrl Pts',(-8.11441020355196,0.419926147981283,
5.39520278108484));
#180186=CARTESIAN_POINT('Ctrl Pts',(-8.11349140746026,0.437319229577799,
5.39452614623912));
#180187=CARTESIAN_POINT('Ctrl Pts',(-8.08954533061119,0.864543708153112,
5.37796079832828));
#180188=CARTESIAN_POINT('Ctrl Pts',(-8.03555058516449,1.27204805710462,
5.36356684083488));
#180189=CARTESIAN_POINT('Ctrl Pts',(-7.87146529600756,2.05153295490933,
5.33643141259876));
#180190=CARTESIAN_POINT('Ctrl Pts',(-7.76510698738187,2.42319439503791,
5.32365072200401));
#180191=CARTESIAN_POINT('Ctrl Pts',(-7.45808207833201,3.26437629369158,
5.29309941169533));
#180192=CARTESIAN_POINT('Ctrl Pts',(-7.23885078118004,3.72533384370265,
5.27505788615528));
#180193=CARTESIAN_POINT('Ctrl Pts',(-6.96138661896661,4.1904446429482,5.25423394023942));
#180194=CARTESIAN_POINT('Ctrl Pts',(-6.94468076830957,4.21807289675835,
5.25298690382023));
#180195=CARTESIAN_POINT('Ctrl Pts',(-6.92121703811957,4.25636012545102,
5.25124453064633));
#180196=CARTESIAN_POINT('Ctrl Pts',(-6.91459823148122,4.26710418220342,
5.25075402213369));
#180197=CARTESIAN_POINT('Ctrl Pts',(-6.90314850834073,4.28559348986726,
5.24990719318394));
#180198=CARTESIAN_POINT('Ctrl Pts',(-6.89832951125912,4.29334611253515,
5.24955128842167));
#180199=CARTESIAN_POINT('Ctrl Pts',(-6.88835007369052,4.309340481012,5.24881530979452));
#180200=CARTESIAN_POINT('Ctrl Pts',(-6.8831878828718,4.31758111531482,5.24843517505561));
#180201=CARTESIAN_POINT('Ctrl Pts',(-6.8711264303219,4.33675873880178,5.24754831809148));
#180202=CARTESIAN_POINT('Ctrl Pts',(-6.86421583651924,4.34768855000711,
5.24704119918948));
#180203=CARTESIAN_POINT('Ctrl Pts',(-6.84206604716215,4.38253625971744,
5.2454189604195));
#180204=CARTESIAN_POINT('Ctrl Pts',(-6.82672778400444,4.4063907685154,5.24430035863782));
#180205=CARTESIAN_POINT('Ctrl Pts',(-6.49992156421237,4.90884702246101,
5.22056537378684));
#180206=CARTESIAN_POINT('Ctrl Pts',(-6.1390299566808,5.35330865290066,5.19607918780533));
#180207=CARTESIAN_POINT('Ctrl Pts',(-5.4704259057323,6.0193995109578,5.1539656341846));
#180208=CARTESIAN_POINT('Ctrl Pts',(-5.18846286744886,6.26407037739234,
5.13699553120796));
#180209=CARTESIAN_POINT('Ctrl Pts',(-4.56780363947828,6.73189070104351,
5.10226249786165));
#180210=CARTESIAN_POINT('Ctrl Pts',(-4.22713812340037,6.95086991935527,
5.08461539831018));
#180211=CARTESIAN_POINT('Ctrl Pts',(-3.84785604988537,7.15642482874979,
5.0673592963047));
#180212=CARTESIAN_POINT('Ctrl Pts',(-3.82412029836396,7.1691363830802,5.06628841617375));
#180213=CARTESIAN_POINT('Ctrl Pts',(-3.79159301836404,7.18634868814052,
5.06483260021745));
#180214=CARTESIAN_POINT('Ctrl Pts',(-3.78285600005353,7.19095164553996,
5.0644427089687));
#180215=CARTESIAN_POINT('Ctrl Pts',(-3.76796439187685,7.19876239864356,
5.06378008768861));
#180216=CARTESIAN_POINT('Ctrl Pts',(-3.76181405757817,7.20197825095378,
5.06350697697769));
#180217=CARTESIAN_POINT('Ctrl Pts',(-3.74990588199596,7.20818531521317,
5.06297924628006));
#180218=CARTESIAN_POINT('Ctrl Pts',(-3.74414856567166,7.21117751693691,
5.06272458046948));
#180219=CARTESIAN_POINT('Ctrl Pts',(-3.73046953443604,7.21826600701172,
5.06212063346116));
#180220=CARTESIAN_POINT('Ctrl Pts',(-3.72254463770475,7.22235616100697,
5.06177163217249));
#180221=CARTESIAN_POINT('Ctrl Pts',(-3.69911827548553,7.23439804480659,
5.06074255917797));
#180222=CARTESIAN_POINT('Ctrl Pts',(-3.68359789515752,7.24231300341309,
5.06006412501378));
#180223=CARTESIAN_POINT('Ctrl Pts',(-3.5601255894997,7.3047808282414,5.05469247676947));
#180224=CARTESIAN_POINT('Ctrl Pts',(-3.45099010739142,7.35696853685853,
5.05009958089078));
#180225=CARTESIAN_POINT('Ctrl Pts',(-3.02101973879993,7.55090288573556,
5.03246266239784));
#180226=CARTESIAN_POINT('Ctrl Pts',(-2.69229794003966,7.67425863066218,
5.01993542762059));
#180227=CARTESIAN_POINT('Ctrl Pts',(-1.61270406842232,8.00144487814768,
4.97954131372518));
#180228=CARTESIAN_POINT('Ctrl Pts',(-0.84031410007732,8.11897324172928,
4.95118425324574));
#180229=CARTESIAN_POINT('Ctrl Pts',(0.10236826241514,8.12628913446624,4.91491667432805));
#180230=CARTESIAN_POINT('Ctrl Pts',(0.267791726187582,8.12252061476756,
4.90852397459318));
#180231=CARTESIAN_POINT('Ctrl Pts',(0.491608188638076,8.11057677420916,
4.89980637060434));
#180232=CARTESIAN_POINT('Ctrl Pts',(0.550197193736433,8.1068130126858,4.89751802596582));
#180233=CARTESIAN_POINT('Ctrl Pts',(0.644141471555606,8.09975491367764,
4.89383735157487));
#180234=CARTESIAN_POINT('Ctrl Pts',(0.679525000258183,8.09686319881122,
4.89244844177727));
#180235=CARTESIAN_POINT('Ctrl Pts',(0.75038111184046,8.09060475567301,4.88966157928532));
#180236=CARTESIAN_POINT('Ctrl Pts',(0.785852776565953,8.08723639619641,
4.88826364236603));
#180237=CARTESIAN_POINT('Ctrl Pts',(0.868243654216268,8.07886544471657,
4.88500978743938));
#180238=CARTESIAN_POINT('Ctrl Pts',(0.915143674549388,8.07368725835118,
4.88315240841811));
#180239=CARTESIAN_POINT('Ctrl Pts',(1.05558306582045,8.05694204098354,4.87757419875539));
#180240=CARTESIAN_POINT('Ctrl Pts',(1.14896853074906,8.04415575231379,4.87384306263687));
#180241=CARTESIAN_POINT('Ctrl Pts',(1.37076988736651,8.00984562814346,4.86492447764506));
#180242=CARTESIAN_POINT('Ctrl Pts',(1.49893199230972,7.98685416410106,4.85972544058036));
#180243=CARTESIAN_POINT('Ctrl Pts',(1.97290890052978,7.89001501689279,4.84031823128928));
#180244=CARTESIAN_POINT('Ctrl Pts',(2.31433922519872,7.7967002249336,4.82596878109188));
#180245=CARTESIAN_POINT('Ctrl Pts',(2.98289097917001,7.56618044286883,4.79722650145095));
#180246=CARTESIAN_POINT('Ctrl Pts',(3.30930773043352,7.42921361795735,4.78286617568901));
#180247=CARTESIAN_POINT('Ctrl Pts',(3.67411639125232,7.24730814750974,4.76664647285415));
#180248=CARTESIAN_POINT('Ctrl Pts',(3.72222598233871,7.22271697120772,4.76450413228667));
#180249=CARTESIAN_POINT('Ctrl Pts',(3.78957621870951,7.18743929959827,4.76150149796102));
#180250=CARTESIAN_POINT('Ctrl Pts',(3.8090239551273,7.17715181093442,4.76063405742896));
#180251=CARTESIAN_POINT('Ctrl Pts',(3.84482723829831,7.15802603207816,4.7590364468075));
#180252=CARTESIAN_POINT('Ctrl Pts',(3.86119465249933,7.1492103777332,4.75830586496622));
#180253=CARTESIAN_POINT('Ctrl Pts',(3.89306109876846,7.13190543436495,4.75688282963261));
#180254=CARTESIAN_POINT('Ctrl Pts',(3.90856298256548,7.12342159760816,4.75619027692029));
#180255=CARTESIAN_POINT('Ctrl Pts',(3.94650682583049,7.10249462525842,4.75449418663749));
#180256=CARTESIAN_POINT('Ctrl Pts',(3.96891778323162,7.08999560401707,4.75349161142473));
#180257=CARTESIAN_POINT('Ctrl Pts',(4.0211739101204,7.06052594744116,4.75115141356499));
#180258=CARTESIAN_POINT('Ctrl Pts',(4.0509715119971,7.0434718777822,4.74981508304263));
#180259=CARTESIAN_POINT('Ctrl Pts',(4.13928601414858,6.99218099983484,4.74584706432741));
#180260=CARTESIAN_POINT('Ctrl Pts',(4.1974836481589,6.95740001342429,4.74322247336926));
#180261=CARTESIAN_POINT('Ctrl Pts',(4.44449831574806,6.80554757911282,4.73202276886598));
#180262=CARTESIAN_POINT('Ctrl Pts',(4.62890654610473,6.68148697339444,4.7235068423513));
#180263=CARTESIAN_POINT('Ctrl Pts',(4.95638727298149,6.44110207872386,4.70787586103235));
#180264=CARTESIAN_POINT('Ctrl Pts',(5.10102979365904,6.3271687958893,4.70077625663744));
#180265=CARTESIAN_POINT('Ctrl Pts',(5.28315293130661,6.17340498692566,4.69152043902881));
#180266=CARTESIAN_POINT('Ctrl Pts',(5.32427670190291,6.13797292236906,4.68940874404883));
#180267=CARTESIAN_POINT('Ctrl Pts',(5.39231515997852,6.07815297300311,4.68587719103964));
#180268=CARTESIAN_POINT('Ctrl Pts',(5.41942697564301,6.05399187253007,4.68445972415975));
#180269=CARTESIAN_POINT('Ctrl Pts',(5.4707946460436,6.00759321835222,4.681754163444));
#180270=CARTESIAN_POINT('Ctrl Pts',(5.49507918200014,5.98538846790477,4.68046644303451));
#180271=CARTESIAN_POINT('Ctrl Pts',(5.54504320464867,5.93914309908232,4.67779882725267));
#180272=CARTESIAN_POINT('Ctrl Pts',(5.5707028042295,5.91508200701462,4.67641873018814));
#180273=CARTESIAN_POINT('Ctrl Pts',(5.66201748323369,5.82833472129175,4.67147058462562));
#180274=CARTESIAN_POINT('Ctrl Pts',(5.72677697876963,5.76471620053082,4.66789244235388));
#180275=CARTESIAN_POINT('Ctrl Pts',(5.83823466527357,5.6514902503089,4.66160992866191));
#180276=CARTESIAN_POINT('Ctrl Pts',(5.88540043062122,5.6023555550965,4.65891076108105));
#180277=CARTESIAN_POINT('Ctrl Pts',(6.14874366581022,5.32102294302209,4.64360852361233));
#180278=CARTESIAN_POINT('Ctrl Pts',(6.35179329391646,5.07691375995268,4.63089333341676));
#180279=CARTESIAN_POINT('Ctrl Pts',(6.60865141920152,4.72850714447214,4.6136562108051));
#180280=CARTESIAN_POINT('Ctrl Pts',(6.67526202607647,4.63399726782813,4.60906702635525));
#180281=CARTESIAN_POINT('Ctrl Pts',(6.75737873598373,4.51204022588916,4.60326967860078));
#180282=CARTESIAN_POINT('Ctrl Pts',(6.77477263137045,4.48588120519447,4.60203333108536));
#180283=CARTESIAN_POINT('Ctrl Pts',(6.80192954443494,4.44452116390416,4.6000902187715));
#180284=CARTESIAN_POINT('Ctrl Pts',(6.81179426605689,4.4293874048048,4.59938168554052));
#180285=CARTESIAN_POINT('Ctrl Pts',(6.8318076396895,4.39845931960947,4.59793856714897));
#180286=CARTESIAN_POINT('Ctrl Pts',(6.84195219379009,4.38266245477478,4.5972040513849));
#180287=CARTESIAN_POINT('Ctrl Pts',(6.86312212308146,4.34944448544432,4.59566472019088));
#180288=CARTESIAN_POINT('Ctrl Pts',(6.87413612886836,4.33201628497644,4.59486008754088));
#180289=CARTESIAN_POINT('Ctrl Pts',(6.90026625551849,4.29031824866774,4.59294184532809));
#180290=CARTESIAN_POINT('Ctrl Pts',(6.91532085340261,4.26601014698498,4.59182913438244));
#180291=CARTESIAN_POINT('Ctrl Pts',(6.95585665404035,4.19978004988552,4.58881170286466));
#180292=CARTESIAN_POINT('Ctrl Pts',(6.98108705254511,4.15770584059715,4.58691022677691));
#180293=CARTESIAN_POINT('Ctrl Pts',(7.06230916243994,4.01943591635763,4.58070721442079));
#180294=CARTESIAN_POINT('Ctrl Pts',(7.1167057915507,3.92231751934114,4.57642206672313));
#180295=CARTESIAN_POINT('Ctrl Pts',(7.2915260128715,3.59458078179143,4.56215110718107));
#180296=CARTESIAN_POINT('Ctrl Pts',(7.40286786778409,3.35930204235497,4.55220930235642));
#180297=CARTESIAN_POINT('Ctrl Pts',(7.59796583798547,2.89000862147893,4.53268231613359));
#180298=CARTESIAN_POINT('Ctrl Pts',(7.68265787026303,2.65668978895327,4.52311229968511));
#180299=CARTESIAN_POINT('Ctrl Pts',(7.78026824986612,2.34381319174337,4.51036639596665));
#180300=CARTESIAN_POINT('Ctrl Pts',(7.80287468792881,2.26741721694004,4.50726132353649));
#180301=CARTESIAN_POINT('Ctrl Pts',(7.83924221422636,2.13752621834267,4.50199211535184));
#180302=CARTESIAN_POINT('Ctrl Pts',(7.85358797868169,2.08420072479798,4.49983177053173));
#180303=CARTESIAN_POINT('Ctrl Pts',(7.87962932393522,1.98331234279912,4.49574956977132));
#180304=CARTESIAN_POINT('Ctrl Pts',(7.89144061056077,1.93578180702159,4.49382845729737));
#180305=CARTESIAN_POINT('Ctrl Pts',(7.92462991764106,1.79686831131078,4.48821972597953));
#180306=CARTESIAN_POINT('Ctrl Pts',(7.94485526131314,1.70521841400727,4.48452669359542));
#180307=CARTESIAN_POINT('Ctrl Pts',(7.99103232689364,1.47727294633488,4.47536113521955));
#180308=CARTESIAN_POINT('Ctrl Pts',(8.01508953984548,1.3406239431761,4.46988345684139));
#180309=CARTESIAN_POINT('Ctrl Pts',(8.05473324783536,1.07591111125145,4.45931645733786));
#180310=CARTESIAN_POINT('Ctrl Pts',(8.07079218089952,0.947958941933727,
4.4542285512639));
#180311=CARTESIAN_POINT('Ctrl Pts',(8.08859149756639,0.772419289995171,
4.44728749952557));
#180312=CARTESIAN_POINT('Ctrl Pts',(8.09296897744624,0.725118696483148,
4.44542108391337));
#180313=CARTESIAN_POINT('Ctrl Pts',(8.09998902213617,0.641255755700322,
4.44211989343702));
#180314=CARTESIAN_POINT('Ctrl Pts',(8.10279940678399,0.604708923499361,
4.44068400515952));
#180315=CARTESIAN_POINT('Ctrl Pts',(8.1089410853851,0.517089391751259,4.43724695953343));
#180316=CARTESIAN_POINT('Ctrl Pts',(8.11203731028862,0.46600178376016,4.43524734198575));
#180317=CARTESIAN_POINT('Ctrl Pts',(8.12170829110583,0.276850531843856,
4.42785506884705));
#180318=CARTESIAN_POINT('Ctrl Pts',(8.12524251661006,0.138655883878553,
4.42247614954586));
#180319=CARTESIAN_POINT('Ctrl Pts',(8.12524998812855,0.000439223138430957,
4.41709488796514));
#180320=CARTESIAN_POINT('',(8.12571492871015,-5.96162441064372E-5,2.41670257632164));
#180321=CARTESIAN_POINT('Ctrl Pts',(8.12571492871015,-5.96162441064372E-5,
2.41670257632164));
#180322=CARTESIAN_POINT('Ctrl Pts',(8.12424960426803,1.03977077379999,2.45736153240871));
#180323=CARTESIAN_POINT('Ctrl Pts',(7.66272101425109,3.43456748704045,2.55090964359126));
#180324=CARTESIAN_POINT('Ctrl Pts',(5.3892250497751,6.51729066085763,2.69734690986928));
#180325=CARTESIAN_POINT('Ctrl Pts',(0.335793904015849,8.95641601104349,
2.90890353025119));
#180326=CARTESIAN_POINT('Ctrl Pts',(-5.44841867805424,7.1057006866787,3.12046015063309));
#180327=CARTESIAN_POINT('Ctrl Pts',(-8.15520229705821,2.22234120788701,
3.332016771015));
#180328=CARTESIAN_POINT('Ctrl Pts',(-8.30012585283045,-3.35904394789357,
3.5435733913969));
#180329=CARTESIAN_POINT('Ctrl Pts',(-4.25467436631767,-7.88859242601576,
3.75513001177881));
#180330=CARTESIAN_POINT('Ctrl Pts',(1.33775837807641,-8.35032807926611,
3.96668663216071));
#180331=CARTESIAN_POINT('Ctrl Pts',(5.15483525499161,-6.72198816743905,
4.12535409744715));
#180332=CARTESIAN_POINT('Ctrl Pts',(7.60768009450967,-3.60555357023,4.2753576282403));
#180333=CARTESIAN_POINT('Ctrl Pts',(8.1240908003074,-1.12746725914049,4.37247200393799));
#180334=CARTESIAN_POINT('Ctrl Pts',(8.12456022843635,0.000454668290610622,
4.4166972245402));
#180335=CARTESIAN_POINT('Ctrl Pts',(8.12525,4.45452207025868E-13,0.416702556787629));
#180336=CARTESIAN_POINT('Ctrl Pts',(8.12524999999988,2.24624642433457,0.50470014992883));
#180337=CARTESIAN_POINT('Ctrl Pts',(7.14398562317574,4.47535249753493,0.59269774307003));
#180338=CARTESIAN_POINT('Ctrl Pts',(3.83078204044889,7.50935546634383,0.768692929352432));
#180339=CARTESIAN_POINT('Ctrl Pts',(1.52412477697697,8.29110090552146,0.856690522493633));
#180340=CARTESIAN_POINT('Ctrl Pts',(-2.95101623932604,7.89663306204409,
1.03268570877603));
#180341=CARTESIAN_POINT('Ctrl Pts',(-5.08535169588772,6.72342983085759,
1.12068330191723));
#180342=CARTESIAN_POINT('Ctrl Pts',(-7.81671694684421,3.15661951052899,
1.29667848819964));
#180343=CARTESIAN_POINT('Ctrl Pts',(-8.39290461146706,0.790229551553667,
1.38467608134084));
#180344=CARTESIAN_POINT('Ctrl Pts',(-7.60701611462464,-3.63299000730456,
1.56067126762324));
#180345=CARTESIAN_POINT('Ctrl Pts',(-6.25093680401326,-5.65606750610053,
1.64866886076444));
#180346=CARTESIAN_POINT('Ctrl Pts',(-2.45807268688511,-8.06369575488332,
1.82466404704684));
#180347=CARTESIAN_POINT('Ctrl Pts',(-0.0502299510448689,-8.42987470330086,
1.91266164018804));
#180348=CARTESIAN_POINT('Ctrl Pts',(4.28689960881039,-7.25863639434537,
2.08865682647044));
#180349=CARTESIAN_POINT('Ctrl Pts',(6.18309125557196,-5.73015646266342,
2.17665441961164));
#180350=CARTESIAN_POINT('Ctrl Pts',(7.8104963945153,-2.5864249052526,2.31533474365933));
#180351=CARTESIAN_POINT('Ctrl Pts',(8.1252402654945,-1.29379881447011,2.36601747456583));
#180352=CARTESIAN_POINT('Ctrl Pts',(8.1252499997742,-6.00202038690051E-5,
2.41670020547233));
#180353=CARTESIAN_POINT('Origin',(7.,0.,120.));
#180354=CARTESIAN_POINT('',(-7.,-8.57252759403147E-16,120.));
#180355=CARTESIAN_POINT('Origin',(0.,0.,120.));
#180356=CARTESIAN_POINT('',(-4.,-4.89858719658941E-16,120.));
#180357=CARTESIAN_POINT('Origin',(0.,0.,120.));
#180358=CARTESIAN_POINT('Origin',(0.,0.,140.));
#180359=CARTESIAN_POINT('',(-10.,-1.22464679914735E-15,160.));
#180360=CARTESIAN_POINT('',(-8.5,-1.04094977927525E-15,140.));
#180361=CARTESIAN_POINT('Origin',(0.,0.,160.));
#180362=CARTESIAN_POINT('Origin',(4.,16.,160.));
#180363=CARTESIAN_POINT('',(4.,16.,160.));
#180364=CARTESIAN_POINT('',(-4.,16.,160.));
#180365=CARTESIAN_POINT('',(2.,16.,160.));
#180366=CARTESIAN_POINT('',(4.,16.,0.));
#180367=CARTESIAN_POINT('',(4.,16.,160.));
#180368=CARTESIAN_POINT('',(-4.,16.,0.));
#180369=CARTESIAN_POINT('',(2.,16.,0.));
#180370=CARTESIAN_POINT('',(-4.,16.,160.));
#180371=CARTESIAN_POINT('Origin',(4.,24.,160.));
#180372=CARTESIAN_POINT('',(4.,19.5959179422654,0.));
#180373=CARTESIAN_POINT('',(4.,19.5959179422654,160.));
#180374=CARTESIAN_POINT('',(4.,19.5959179422654,0.));
#180375=CARTESIAN_POINT('',(4.,12.,0.));
#180376=CARTESIAN_POINT('',(4.,12.,160.));
#180377=CARTESIAN_POINT('Origin',(-4.,16.,160.));
#180378=CARTESIAN_POINT('',(-4.,19.5959179422654,160.));
#180379=CARTESIAN_POINT('',(-4.,19.5959179422654,0.));
#180380=CARTESIAN_POINT('',(-4.,19.5959179422654,0.));
#180381=CARTESIAN_POINT('',(-4.,8.,160.));
#180382=CARTESIAN_POINT('',(-4.,8.,0.));
#180383=CARTESIAN_POINT('Origin',(0.,0.,160.));
#180384=CARTESIAN_POINT('Origin',(0.,0.,160.));
#180385=CARTESIAN_POINT('Origin',(1.01053986535715E-15,-4.14056453134834E-16,
99.));
#180386=CARTESIAN_POINT('Ctrl Pts',(-5.31037376991249,-4.5779424402591,
99.));
#180387=CARTESIAN_POINT('Ctrl Pts',(-5.4441239624656,-4.44540070235016,
99.));
#180388=CARTESIAN_POINT('Ctrl Pts',(-5.5722612323594,-4.307542198691,98.9999999999999));
#180389=CARTESIAN_POINT('Ctrl Pts',(-5.69462771650504,-4.16482393050322,
99.));
#180390=CARTESIAN_POINT('Ctrl Pts',(-5.81894587851274,-4.01982938473437,
99.));
#180391=CARTESIAN_POINT('Ctrl Pts',(-5.93730819124591,-3.86981839507266,
99.));
#180392=CARTESIAN_POINT('Ctrl Pts',(-6.04951933541627,-3.71522500998853,
99.));
#180393=CARTESIAN_POINT('Ctrl Pts',(-6.14969329868596,-3.57721525887465,
99.));
#180394=CARTESIAN_POINT('Ctrl Pts',(-6.24496481579415,-3.43555263050148,
99.));
#180395=CARTESIAN_POINT('Ctrl Pts',(-6.33517059446557,-3.29052067230091,
99.));
#180396=CARTESIAN_POINT('Ctrl Pts',(-6.35035764256056,-3.26610308667676,
99.));
#180397=CARTESIAN_POINT('Ctrl Pts',(-6.36539986619513,-3.24159175654722,
99.));
#180398=CARTESIAN_POINT('Ctrl Pts',(-6.380290705594,-3.21699782006883,99.));
#180399=CARTESIAN_POINT('Ctrl Pts',(-6.48066943276825,-3.05121078995038,
99.));
#180400=CARTESIAN_POINT('Ctrl Pts',(-6.57424835379599,-2.88155110031512,
99.));
#180401=CARTESIAN_POINT('Ctrl Pts',(-6.66083506361849,-2.70846730956609,
99.));
#180402=CARTESIAN_POINT('Ctrl Pts',(-6.74771904956312,-2.53478927429357,
99.));
#180403=CARTESIAN_POINT('Ctrl Pts',(-6.82756318108919,-2.35766302336224,
99.));
#180404=CARTESIAN_POINT('Ctrl Pts',(-6.90013458560465,-2.17750647052253,
99.));
#180405=CARTESIAN_POINT('Ctrl Pts',(-6.94218771559863,-2.07311071042365,
99.));
#180406=CARTESIAN_POINT('Ctrl Pts',(-6.98179799933791,-1.96769679885147,
99.0000000000001));
#180407=CARTESIAN_POINT('Ctrl Pts',(-7.01891332167098,-1.86134180381851,
99.0000000000001));
#180408=CARTESIAN_POINT('Ctrl Pts',(-7.0309690691284,-1.82679572202925,
99.0000000000001));
#180409=CARTESIAN_POINT('Ctrl Pts',(-7.04276153851497,-1.79215032813677,
99.));
#180410=CARTESIAN_POINT('Ctrl Pts',(-7.05428882037421,-1.75740820588289,
99.));
#180411=CARTESIAN_POINT('Ctrl Pts',(-7.0624020809098,-1.73295561655203,
99.));
#180412=CARTESIAN_POINT('Ctrl Pts',(-7.07038375930567,-1.70845559507833,
99.));
#180413=CARTESIAN_POINT('Ctrl Pts',(-7.07822921067514,-1.68392195839963,
99.));
#180414=CARTESIAN_POINT('Ctrl Pts',(-7.09344804866636,-1.63633088627839,
99.));
#180415=CARTESIAN_POINT('Ctrl Pts',(-7.1081584504933,-1.58860089826392,
99.0000000000001));
#180416=CARTESIAN_POINT('Ctrl Pts',(-7.12235757386568,-1.54073952803008,
99.0000000000001));
#180417=CARTESIAN_POINT('Ctrl Pts',(-7.17672926898223,-1.35746738073137,
99.0000000000001));
#180418=CARTESIAN_POINT('Ctrl Pts',(-7.2236074452293,-1.17227121702206,
98.9999999999999));
#180419=CARTESIAN_POINT('Ctrl Pts',(-7.26310819089592,-0.985637740964515,
98.9999999999999));
#180420=CARTESIAN_POINT('Ctrl Pts',(-7.30356248337767,-0.794498938395065,
98.9999999999999));
#180421=CARTESIAN_POINT('Ctrl Pts',(-7.33627911130937,-0.601852048356352,
98.9999999999999));
#180422=CARTESIAN_POINT('Ctrl Pts',(-7.36133604383713,-0.40819153426746,
99.));
#180423=CARTESIAN_POINT('Ctrl Pts',(-7.38658963276242,-0.213011098336481,
99.));
#180424=CARTESIAN_POINT('Ctrl Pts',(-7.40406296219896,-0.0168003880434584,
99.));
#180425=CARTESIAN_POINT('Ctrl Pts',(-7.41378618299848,0.179953433725718,
98.9999999999999));
#180426=CARTESIAN_POINT('Ctrl Pts',(-7.42351220200831,0.376763878561074,
98.9999999999999));
#180427=CARTESIAN_POINT('Ctrl Pts',(-7.42548374008242,0.574118468878499,
98.9999999999999));
#180428=CARTESIAN_POINT('Ctrl Pts',(-7.41967984053872,0.771538034948267,
99.));
#180429=CARTESIAN_POINT('Ctrl Pts',(-7.41706251960698,0.860566171758501,
99.));
#180430=CARTESIAN_POINT('Ctrl Pts',(-7.41286325582366,0.949607569888835,
99.));
#180431=CARTESIAN_POINT('Ctrl Pts',(-7.4070766488981,1.0386182379253,99.));
#180432=CARTESIAN_POINT('Ctrl Pts',(-7.4048233678607,1.07327862750993,99.));
#180433=CARTESIAN_POINT('Ctrl Pts',(-7.40232878885474,1.1079408443067,99.));
#180434=CARTESIAN_POINT('Ctrl Pts',(-7.39959553385162,1.14256672634978,
99.));
#180435=CARTESIAN_POINT('Ctrl Pts',(-7.38373855400664,1.34344879298543,
99.));
#180436=CARTESIAN_POINT('Ctrl Pts',(-7.35984388220669,1.54328450280515,
99.0000000000001));
#180437=CARTESIAN_POINT('Ctrl Pts',(-7.32799719857053,1.74156168524455,
99.0000000000001));
#180438=CARTESIAN_POINT('Ctrl Pts',(-7.30708081276114,1.8717869260415,99.));
#180439=CARTESIAN_POINT('Ctrl Pts',(-7.28273319238425,2.00134031869882,
99.));
#180440=CARTESIAN_POINT('Ctrl Pts',(-7.25496680053308,2.13007981682335,
99.));
#180441=CARTESIAN_POINT('Ctrl Pts',(-7.21294541865853,2.32491289567739,
99.));
#180442=CARTESIAN_POINT('Ctrl Pts',(-7.16309648166436,2.51788222848557,
99.));
#180443=CARTESIAN_POINT('Ctrl Pts',(-7.10569000657273,2.70861680076425,
99.));
#180444=CARTESIAN_POINT('Ctrl Pts',(-7.04776212324125,2.90108376607787,
99.));
#180445=CARTESIAN_POINT('Ctrl Pts',(-6.98213864267679,3.09127581520037,
99.0000000000001));
#180446=CARTESIAN_POINT('Ctrl Pts',(-6.90904422969321,3.27880510883622,
99.0000000000001));
#180447=CARTESIAN_POINT('Ctrl Pts',(-6.83602882644324,3.46613169697206,
99.0000000000001));
#180448=CARTESIAN_POINT('Ctrl Pts',(-6.75555839763656,3.65080191536816,
99.0000000000001));
#180449=CARTESIAN_POINT('Ctrl Pts',(-6.66780748293597,3.8324131713319,99.0000000000001));
#180450=CARTESIAN_POINT('Ctrl Pts',(-6.65631659233788,3.85619497555336,
99.0000000000001));
#180451=CARTESIAN_POINT('Ctrl Pts',(-6.64470079214548,3.8799242953817,99.0000000000001));
#180452=CARTESIAN_POINT('Ctrl Pts',(-6.63296041476652,3.9036001974702,99.0000000000001));
#180453=CARTESIAN_POINT('Ctrl Pts',(-6.62357084759944,3.92253540421238,
99.0000000000001));
#180454=CARTESIAN_POINT('Ctrl Pts',(-6.61410251488555,3.94143453716387,
99.0000000000001));
#180455=CARTESIAN_POINT('Ctrl Pts',(-6.60455977814979,3.96028910061425,
99.0000000000001));
#180456=CARTESIAN_POINT('Ctrl Pts',(-6.5121376073237,4.14289706018757,99.0000000000001));
#180457=CARTESIAN_POINT('Ctrl Pts',(-6.4126341111438,4.32154027408393,99.0000000000001));
#180458=CARTESIAN_POINT('Ctrl Pts',(-6.30635263066292,4.4958407175706,99.0000000000001));
#180459=CARTESIAN_POINT('Ctrl Pts',(-6.19486933451546,4.67867208077645,
99.0000000000001));
#180460=CARTESIAN_POINT('Ctrl Pts',(-6.07592850174037,4.85672597420854,
99.));
#180461=CARTESIAN_POINT('Ctrl Pts',(-5.94982020079738,5.0295555387748,99.));
#180462=CARTESIAN_POINT('Ctrl Pts',(-5.8237118998544,5.20238510334106,99.));
#180463=CARTESIAN_POINT('Ctrl Pts',(-5.69043581377082,5.36999112631312,
99.));
#180464=CARTESIAN_POINT('Ctrl Pts',(-5.55022529123391,5.53190436285328,
99.));
#180465=CARTESIAN_POINT('Ctrl Pts',(-5.41582967601333,5.68710262218101,
99.));
#180466=CARTESIAN_POINT('Ctrl Pts',(-5.27506221971937,5.83707093675673,
99.));
#180467=CARTESIAN_POINT('Ctrl Pts',(-5.12835296435508,5.9815326016203,99.));
#180468=CARTESIAN_POINT('Ctrl Pts',(-5.02818687131797,6.08016414689722,
99.));
#180469=CARTESIAN_POINT('Ctrl Pts',(-4.92525007450858,6.17622815003104,
99.));
#180470=CARTESIAN_POINT('Ctrl Pts',(-4.81966940361318,6.26962688161364,
99.));
#180471=CARTESIAN_POINT('Ctrl Pts',(-4.79262515876311,6.29355075086131,
98.9999999999999));
#180472=CARTESIAN_POINT('Ctrl Pts',(-4.76540395473991,6.31730253980657,
99.));
#180473=CARTESIAN_POINT('Ctrl Pts',(-4.73803536116702,6.34085724026832,
99.));
#180474=CARTESIAN_POINT('Ctrl Pts',(-4.58135254906828,6.47570584681658,
99.));
#180475=CARTESIAN_POINT('Ctrl Pts',(-4.41966754978226,6.60425479419713,
99.));
#180476=CARTESIAN_POINT('Ctrl Pts',(-4.2534808509546,6.72628759081721,99.));
#180477=CARTESIAN_POINT('Ctrl Pts',(-4.08406266016045,6.85069330900507,
98.9999999999999));
#180478=CARTESIAN_POINT('Ctrl Pts',(-3.90996557742534,6.96832754417173,
98.9999999999999));
#180479=CARTESIAN_POINT('Ctrl Pts',(-3.73167391547189,7.07893251890552,
98.9999999999999));
#180480=CARTESIAN_POINT('Ctrl Pts',(-3.55289453959222,7.18984005173932,
99.));
#180481=CARTESIAN_POINT('Ctrl Pts',(-3.36989703671833,7.29368031139852,
98.9999999999999));
#180482=CARTESIAN_POINT('Ctrl Pts',(-3.18313162493484,7.39015734245661,
98.9999999999999));
#180483=CARTESIAN_POINT('Ctrl Pts',(-2.99809644729706,7.48574058996121,
98.9999999999999));
#180484=CARTESIAN_POINT('Ctrl Pts',(-2.80936223503177,7.57409682111926,
99.));
#180485=CARTESIAN_POINT('Ctrl Pts',(-2.61733841546728,7.65489620503951,
99.));
#180486=CARTESIAN_POINT('Ctrl Pts',(-2.51411760901224,7.69832924156714,
99.));
#180487=CARTESIAN_POINT('Ctrl Pts',(-2.40994583401986,7.73957796042281,
99.));
#180488=CARTESIAN_POINT('Ctrl Pts',(-2.30488418583278,7.77858539180664,
99.));
#180489=CARTESIAN_POINT('Ctrl Pts',(-2.23787782486739,7.80346360448216,
99.));
#180490=CARTESIAN_POINT('Ctrl Pts',(-2.17050946251637,7.82743005065559,
99.));
#180491=CARTESIAN_POINT('Ctrl Pts',(-2.10279483963357,7.85048474619616,
98.9999999999999));
#180492=CARTESIAN_POINT('Ctrl Pts',(2.10208451021631,7.8486258844723,99.));
#180493=CARTESIAN_POINT('Ctrl Pts',(2.30190062853963,7.78030966332679,99.));
#180494=CARTESIAN_POINT('Ctrl Pts',(2.49875490991879,7.70414622796948,99.));
#180495=CARTESIAN_POINT('Ctrl Pts',(2.69224761706191,7.62041821762084,99.));
#180496=CARTESIAN_POINT('Ctrl Pts',(2.88624622343728,7.53647129495876,99.));
#180497=CARTESIAN_POINT('Ctrl Pts',(3.07686623436583,7.44491978320085,99.));
#180498=CARTESIAN_POINT('Ctrl Pts',(3.2636773692486,7.34600421877401,99.));
#180499=CARTESIAN_POINT('Ctrl Pts',(3.36420325946888,7.29277626115312,99.));
#180500=CARTESIAN_POINT('Ctrl Pts',(3.46362570021794,7.23741518831547,99.));
#180501=CARTESIAN_POINT('Ctrl Pts',(3.56187347705617,7.1799538143239,99.));
#180502=CARTESIAN_POINT('Ctrl Pts',(3.60872217996291,7.1525537964774,99.));
#180503=CARTESIAN_POINT('Ctrl Pts',(3.65530374284034,7.12467617000491,99.));
#180504=CARTESIAN_POINT('Ctrl Pts',(3.70161017699924,7.09632425594086,99.));
#180505=CARTESIAN_POINT('Ctrl Pts',(3.73919757890556,7.07331071995833,99.));
#180506=CARTESIAN_POINT('Ctrl Pts',(3.7766037026839,7.04998468560165,99.));
#180507=CARTESIAN_POINT('Ctrl Pts',(3.81382418637943,7.02634785912935,99.));
#180508=CARTESIAN_POINT('Ctrl Pts',(3.83950955773068,7.01003639282833,99.));
#180509=CARTESIAN_POINT('Ctrl Pts',(3.86509847400006,6.99358202542449,99.));
#180510=CARTESIAN_POINT('Ctrl Pts',(3.89058870562973,6.97698620639156,99.));
#180511=CARTESIAN_POINT('Ctrl Pts',(4.06559275533802,6.86304704800397,99.));
#180512=CARTESIAN_POINT('Ctrl Pts',(4.23596366333074,6.74243376712933,99.0000000000001));
#180513=CARTESIAN_POINT('Ctrl Pts',(4.40128720552182,6.61538533541099,99.));
#180514=CARTESIAN_POINT('Ctrl Pts',(4.56468155565826,6.48981945615782,99.));
#180515=CARTESIAN_POINT('Ctrl Pts',(4.72314610040225,6.35796726953965,99.));
#180516=CARTESIAN_POINT('Ctrl Pts',(4.87624397923126,6.2200250828707,99.));
#180517=CARTESIAN_POINT('Ctrl Pts',(4.9694927706806,6.13600731400844,99.));
#180518=CARTESIAN_POINT('Ctrl Pts',(5.06074989929111,6.04972965074367,99.));
#180519=CARTESIAN_POINT('Ctrl Pts',(5.14990873179672,5.96123116898666,99.));
#180520=CARTESIAN_POINT('Ctrl Pts',(5.18053035147137,5.93083634691477,98.9999999999999));
#180521=CARTESIAN_POINT('Ctrl Pts',(5.21090440419704,5.90017952976678,98.9999999999999));
#180522=CARTESIAN_POINT('Ctrl Pts',(5.24102638922979,5.86926220478056,99.));
#180523=CARTESIAN_POINT('Ctrl Pts',(5.26128721225004,5.84846641562109,99.));
#180524=CARTESIAN_POINT('Ctrl Pts',(5.28143496446116,5.82755166573488,99.));
#180525=CARTESIAN_POINT('Ctrl Pts',(5.30145552672904,5.80653198951449,99.));
#180526=CARTESIAN_POINT('Ctrl Pts',(5.33795501899862,5.76821101233864,99.));
#180527=CARTESIAN_POINT('Ctrl Pts',(5.37404154619558,5.72953138765668,98.9999999999999));
#180528=CARTESIAN_POINT('Ctrl Pts',(5.40970872589704,5.6904972373425,98.9999999999999));
#180529=CARTESIAN_POINT('Ctrl Pts',(5.54691998828725,5.54033327468093,98.9999999999999));
#180530=CARTESIAN_POINT('Ctrl Pts',(5.6779283030564,5.38492524438802,99.));
#180531=CARTESIAN_POINT('Ctrl Pts',(5.80255536908089,5.22473368313874,98.9999999999999));
#180532=CARTESIAN_POINT('Ctrl Pts',(5.92854010608881,5.06279701593907,98.9999999999999));
#180533=CARTESIAN_POINT('Ctrl Pts',(6.04800416329334,4.89597139565613,98.9999999999999));
#180534=CARTESIAN_POINT('Ctrl Pts',(6.1607195382386,4.72470292325923,98.9999999999999));
#180535=CARTESIAN_POINT('Ctrl Pts',(6.27313238497297,4.55389413566188,98.9999999999999));
#180536=CARTESIAN_POINT('Ctrl Pts',(6.37883299157331,4.37866563188071,98.9999999999999));
#180537=CARTESIAN_POINT('Ctrl Pts',(6.47754731264676,4.19944056913079,98.9999999999999));
#180538=CARTESIAN_POINT('Ctrl Pts',(6.57481450704896,4.02284289991042,98.9999999999999));
#180539=CARTESIAN_POINT('Ctrl Pts',(6.66529890074785,3.84236434123862,98.9999999999999));
#180540=CARTESIAN_POINT('Ctrl Pts',(6.7486888561583,3.65840077965049,98.9999999999999));
#180541=CARTESIAN_POINT('Ctrl Pts',(6.78704586559754,3.57378276980052,98.9999999999999));
#180542=CARTESIAN_POINT('Ctrl Pts',(6.82390116975331,3.48842735837073,98.9999999999999));
#180543=CARTESIAN_POINT('Ctrl Pts',(6.85922070921012,3.40237299082903,98.9999999999999));
#180544=CARTESIAN_POINT('Ctrl Pts',(6.86883102667818,3.37895791225478,98.9999999999999));
#180545=CARTESIAN_POINT('Ctrl Pts',(6.87832762775247,3.35549108616156,98.9999999999999));
#180546=CARTESIAN_POINT('Ctrl Pts',(6.88770979494492,3.33197328910791,98.9999999999999));
#180547=CARTESIAN_POINT('Ctrl Pts',(6.89678219080322,3.30923197996156,98.9999999999999));
#180548=CARTESIAN_POINT('Ctrl Pts',(6.9057443663046,3.28645104029557,98.9999999999999));
#180549=CARTESIAN_POINT('Ctrl Pts',(6.91459439792578,3.26363522828114,98.9999999999999));
#180550=CARTESIAN_POINT('Ctrl Pts',(6.98724898062089,3.07632817993211,98.9999999999999));
#180551=CARTESIAN_POINT('Ctrl Pts',(7.05238393900141,2.88658602815681,98.9999999999999));
#180552=CARTESIAN_POINT('Ctrl Pts',(7.10978797891896,2.69482691931312,98.9999999999999));
#180553=CARTESIAN_POINT('Ctrl Pts',(7.14635429773413,2.57267654941297,98.9999999999999));
#180554=CARTESIAN_POINT('Ctrl Pts',(7.17978269938958,2.44970735410828,99.));
#180555=CARTESIAN_POINT('Ctrl Pts',(7.21000787802527,2.32602464360164,99.));
#180556=CARTESIAN_POINT('Ctrl Pts',(7.25759404308455,2.13130004170314,99.));
#180557=CARTESIAN_POINT('Ctrl Pts',(7.29724296889094,1.93480668573839,98.9999999999999));
#180558=CARTESIAN_POINT('Ctrl Pts',(7.3289508054908,1.73700590882653,98.9999999999999));
#180559=CARTESIAN_POINT('Ctrl Pts',(7.36047806932643,1.54033158634623,99.));
#180560=CARTESIAN_POINT('Ctrl Pts',(7.38415432922803,1.34236400852322,99.));
#180561=CARTESIAN_POINT('Ctrl Pts',(7.39992496655846,1.14356149378338,99.));
#180562=CARTESIAN_POINT('Ctrl Pts',(7.41563864782707,0.945476959432181,
99.0000000000001));
#180563=CARTESIAN_POINT('Ctrl Pts',(7.42350362986571,0.746562848109662,
99.0000000000001));
#180564=CARTESIAN_POINT('Ctrl Pts',(7.42341659129658,0.547287345855029,
99.0000000000001));
#180565=CARTESIAN_POINT('Ctrl Pts',(7.42340550747857,0.521910855612056,
99.0000000000001));
#180566=CARTESIAN_POINT('Ctrl Pts',(7.42326540537986,0.496528532433158,
99.0000000000001));
#180567=CARTESIAN_POINT('Ctrl Pts',(7.42299601492983,0.471141368953221,
99.0000000000001));
#180568=CARTESIAN_POINT('Ctrl Pts',(7.42274491984217,0.44747834734576,99.0000000000001));
#180569=CARTESIAN_POINT('Ctrl Pts',(7.42238158447833,0.423819981672156,
99.0000000000001));
#180570=CARTESIAN_POINT('Ctrl Pts',(7.42190613018156,0.400170373528206,
99.0000000000001));
#180571=CARTESIAN_POINT('Ctrl Pts',(7.41795192148876,0.203483779803561,
99.0000000000001));
#180572=CARTESIAN_POINT('Ctrl Pts',(7.4062462526585,0.00732774803814901,
99.0000000000001));
#180573=CARTESIAN_POINT('Ctrl Pts',(7.38680961699137,-0.187863192996554,
99.0000000000001));
#180574=CARTESIAN_POINT('Ctrl Pts',(7.36725247120289,-0.384264347794748,
99.0000000000001));
#180575=CARTESIAN_POINT('Ctrl Pts',(7.3398681641559,-0.579689108817622,
99.0000000000001));
#180576=CARTESIAN_POINT('Ctrl Pts',(7.30462493342045,-0.77368649553837,
99.0000000000001));
#180577=CARTESIAN_POINT('Ctrl Pts',(7.2693817026849,-0.967683882260041,
99.0000000000001));
#180578=CARTESIAN_POINT('Ctrl Pts',(7.22627947325658,-1.16025458134264,
99.0000000000001));
#180579=CARTESIAN_POINT('Ctrl Pts',(7.17523488235393,-1.35092889850015,
99.0000000000001));
#180580=CARTESIAN_POINT('Ctrl Pts',(7.1298757765253,-1.52036539270661,99.0000000000001));
#180581=CARTESIAN_POINT('Ctrl Pts',(7.07824390585094,-1.68830450180102,
99.0000000000001));
#180582=CARTESIAN_POINT('Ctrl Pts',(7.02047627612835,-1.85438726839183,
99.));
#180583=CARTESIAN_POINT('Ctrl Pts',(6.99159246126706,-1.93742865168724,
99.));
#180584=CARTESIAN_POINT('Ctrl Pts',(6.96117429436383,-2.02000562832631,
99.));
#180585=CARTESIAN_POINT('Ctrl Pts',(6.92923657396901,-2.10207115808548,
99.));
#180586=CARTESIAN_POINT('Ctrl Pts',(6.9132677137716,-2.14310392296506,99.));
#180587=CARTESIAN_POINT('Ctrl Pts',(6.8969189421459,-2.18400880153455,99.));
#180588=CARTESIAN_POINT('Ctrl Pts',(6.88019197511766,-2.22477975857366,
99.));
#180589=CARTESIAN_POINT('Ctrl Pts',(6.86909426420502,-2.25182974881326,
99.));
#180590=CARTESIAN_POINT('Ctrl Pts',(6.85782907052836,-2.27882315355165,
99.));
#180591=CARTESIAN_POINT('Ctrl Pts',(6.84640004100657,-2.30575073479,99.));
#180592=CARTESIAN_POINT('Ctrl Pts',(6.84060272525045,-2.31940961026055,
99.));
#180593=CARTESIAN_POINT('Ctrl Pts',(6.83476365407463,-2.33305061289471,
99.));
#180594=CARTESIAN_POINT('Ctrl Pts',(6.82888422386179,-2.34667057652511,
99.));
#180595=CARTESIAN_POINT('Ctrl Pts',(6.75258519374973,-2.52342069984376,
99.));
#180596=CARTESIAN_POINT('Ctrl Pts',(6.66941539803663,-2.69681260533179,
99.));
#180597=CARTESIAN_POINT('Ctrl Pts',(6.57963636685594,-2.86641735240571,
99.));
#180598=CARTESIAN_POINT('Ctrl Pts',(6.48992260889698,-3.03589878952498,
98.9999999999999));
#180599=CARTESIAN_POINT('Ctrl Pts',(6.39360879097073,-3.20159920820404,
99.));
#180600=CARTESIAN_POINT('Ctrl Pts',(6.29091200366129,-3.36306354964613,
99.));
#180601=CARTESIAN_POINT('Ctrl Pts',(6.18918516724972,-3.52300289223437,
98.9999999999999));
#180602=CARTESIAN_POINT('Ctrl Pts',(6.08119490995241,-3.67878634959697,
98.9999999999999));
#180603=CARTESIAN_POINT('Ctrl Pts',(5.96711584560785,-3.82993631724309,
98.9999999999999));
#180604=CARTESIAN_POINT('Ctrl Pts',(5.85555853856988,-3.97774506240029,
98.9999999999998));
#180605=CARTESIAN_POINT('Ctrl Pts',(5.73817818216436,-4.12112330181221,
98.9999999999999));
#180606=CARTESIAN_POINT('Ctrl Pts',(5.61510989546301,-4.25958363995518,
98.9999999999999));
#180607=CARTESIAN_POINT('Ctrl Pts',(5.55868785672443,-4.32306233761039,
98.9999999999999));
#180608=CARTESIAN_POINT('Ctrl Pts',(5.50106993712163,-4.38550675014418,
98.9999999999999));
#180609=CARTESIAN_POINT('Ctrl Pts',(5.44226749982611,-4.44686660289124,
98.9999999999999));
#180610=CARTESIAN_POINT('Ctrl Pts',(5.39901359961217,-4.49200168691037,
98.9999999999999));
#180611=CARTESIAN_POINT('Ctrl Pts',(5.35511875420783,-4.5365498853096,98.9999999999999));
#180612=CARTESIAN_POINT('Ctrl Pts',(5.3105951928988,-4.58050191706119,98.9999999999999));
#180613=CARTESIAN_POINT('Ctrl Pts',(-5.30378086654373,4.57361536730093,
0.00446747043563128));
#180614=CARTESIAN_POINT('Ctrl Pts',(-6.0639413951417,3.69210156778049,0.057372191261254));
#180615=CARTESIAN_POINT('Ctrl Pts',(-7.13636830945187,1.54513735705448,
0.163166067182353));
#180616=CARTESIAN_POINT('Ctrl Pts',(-7.00278762888421,-2.05811838864947,
0.321849098198928));
#180617=CARTESIAN_POINT('Ctrl Pts',(-5.17287422036016,-5.15049374409531,
0.480516563485356));
#180618=CARTESIAN_POINT('Ctrl Pts',(-2.06992536476629,-7.00586681229451,
0.639184028771785));
#180619=CARTESIAN_POINT('Ctrl Pts',(1.51099084548779,-7.1268219767527,0.797851494058213));
#180620=CARTESIAN_POINT('Ctrl Pts',(5.8549714641742,-5.04026049610657,1.00940811444012));
#180621=CARTESIAN_POINT('Ctrl Pts',(8.19966432523108,1.11131240077932,1.2738538899175));
#180622=CARTESIAN_POINT('Ctrl Pts',(4.30252989486095,6.41644447484682,1.53829966539488));
#180623=CARTESIAN_POINT('Ctrl Pts',(-0.440438479635278,7.27223127969325,
1.74985628577678));
#180624=CARTESIAN_POINT('Ctrl Pts',(-3.85933553388024,6.20169133701892,
1.90852375106322));
#180625=CARTESIAN_POINT('Ctrl Pts',(-6.35800508006661,3.58921836875176,
2.06719121634964));
#180626=CARTESIAN_POINT('Ctrl Pts',(-7.2961685757795,0.117923577904027,
2.22585868163607));
#180627=CARTESIAN_POINT('Ctrl Pts',(-6.47127337767897,-3.38407271816467,
2.3845261469225));
#180628=CARTESIAN_POINT('Ctrl Pts',(-4.05427435445179,-6.07236054551186,
2.54319361220892));
#180629=CARTESIAN_POINT('Ctrl Pts',(-0.679028220406368,-7.25757857856526,
2.70186107749536));
#180630=CARTESIAN_POINT('Ctrl Pts',(4.10468304959755,-6.54456291005896,
2.91341769787726));
#180631=CARTESIAN_POINT('Ctrl Pts',(7.32848383063627,-2.42047858723412,
3.12497431825917));
#180632=CARTESIAN_POINT('Ctrl Pts',(6.88866860112692,2.3718685787921,3.33653093864107));
#180633=CARTESIAN_POINT('Ctrl Pts',(4.28490662509515,6.4190526417461,3.54808755902298));
#180634=CARTESIAN_POINT('Ctrl Pts',(-0.794465437437627,7.68440215608013,
3.75964417940489));
#180635=CARTESIAN_POINT('Ctrl Pts',(-5.00317805612076,5.30101957579333,
3.97120079978678));
#180636=CARTESIAN_POINT('Ctrl Pts',(-6.93319317044858,2.28946327644455,
4.12986826507322));
#180637=CARTESIAN_POINT('Ctrl Pts',(-7.18305822535648,-1.31770430691025,
4.28853573035964));
#180638=CARTESIAN_POINT('Ctrl Pts',(-5.67670789282273,-4.58383194552348,
4.44720319564608));
#180639=CARTESIAN_POINT('Ctrl Pts',(-2.80114571582052,-6.74435065760599,
4.6058706609325));
#180640=CARTESIAN_POINT('Ctrl Pts',(0.777722768978429,-7.25988463091362,
4.76453812621893));
#180641=CARTESIAN_POINT('Ctrl Pts',(4.12824572376459,-6.00751555059738,
4.92320559150536));
#180642=CARTESIAN_POINT('Ctrl Pts',(7.34465462839528,-2.39523911495696,
5.13476221188726));
#180643=CARTESIAN_POINT('Ctrl Pts',(7.17759831039412,2.83667934145036,5.34631883226917));
#180644=CARTESIAN_POINT('Ctrl Pts',(3.76964374075252,6.23453863249777,5.55787545265107));
#180645=CARTESIAN_POINT('Ctrl Pts',(-0.822518600318629,7.67386017329656,
5.76943207303298));
#180646=CARTESIAN_POINT('Ctrl Pts',(-5.53318091736508,5.39119949546253,
5.98098869341488));
#180647=CARTESIAN_POINT('Ctrl Pts',(-7.23773325362757,0.86479597768524,
6.1925453137968));
#180648=CARTESIAN_POINT('Ctrl Pts',(-6.79019730453254,-2.6840267763159,
6.35121277908321));
#180649=CARTESIAN_POINT('Ctrl Pts',(-4.6710360787768,-5.61374242815181,
6.50988024436965));
#180650=CARTESIAN_POINT('Ctrl Pts',(-1.42191810959925,-7.15644284387903,
6.66854770965607));
#180651=CARTESIAN_POINT('Ctrl Pts',(2.17016344940662,-6.97302464538298,
6.8272151749425));
#180652=CARTESIAN_POINT('Ctrl Pts',(5.24835772874372,-5.07597481362461,
6.98588264022893));
#180653=CARTESIAN_POINT('Ctrl Pts',(7.01857685474314,-1.96779920245025,
7.14455010551536));
#180654=CARTESIAN_POINT('Ctrl Pts',(7.17389309592126,2.86642300166595,7.35610672589728));
#180655=CARTESIAN_POINT('Ctrl Pts',(3.6936765813652,6.77653452959824,7.56766334627916));
#180656=CARTESIAN_POINT('Ctrl Pts',(-1.09991472711457,7.20207424796267,
7.77921996666108));
#180657=CARTESIAN_POINT('Ctrl Pts',(-5.54797533933759,5.36513155035279,
7.99077658704298));
#180658=CARTESIAN_POINT('Ctrl Pts',(-7.70244879166337,0.594479258170977,
8.20233320742488));
#180659=CARTESIAN_POINT('Ctrl Pts',(-6.1112839041896,-3.97301696557823,
8.4138898278068));
#180660=CARTESIAN_POINT('Ctrl Pts',(-3.4940250724007,-6.41112844610217,
8.57255729309321));
#180661=CARTESIAN_POINT('Ctrl Pts',(0.0100858356750476,-7.30291588173751,
8.73122475837966));
#180662=CARTESIAN_POINT('Ctrl Pts',(3.49317025910466,-6.40580102964345,
8.88989222366607));
#180663=CARTESIAN_POINT('Ctrl Pts',(6.13370953241007,-3.96362075277578,
9.04855968895252));
#180664=CARTESIAN_POINT('Ctrl Pts',(7.28180167568219,-0.534923840390513,
9.20722715423893));
#180665=CARTESIAN_POINT('Ctrl Pts',(6.6496768096039,2.985708139488,9.36589461952537));
#180666=CARTESIAN_POINT('Ctrl Pts',(3.67177574156317,6.79699829926491,9.57745123990726));
#180667=CARTESIAN_POINT('Ctrl Pts',(-1.50548545536504,7.56955616019083,
9.78900786028918));
#180668=CARTESIAN_POINT('Ctrl Pts',(-5.45870349896653,4.82516756086003,
10.0005644806711));
#180669=CARTESIAN_POINT('Ctrl Pts',(-7.69710713562264,0.564985540828748,
10.212121101053));
#180670=CARTESIAN_POINT('Ctrl Pts',(-6.29491438534592,-4.47830055464201,
10.4236777214349));
#180671=CARTESIAN_POINT('Ctrl Pts',(-2.14692484031353,-6.96587169681106,
10.6352343418168));
#180672=CARTESIAN_POINT('Ctrl Pts',(1.42467490292068,-7.16108096448956,
10.7939018071032));
#180673=CARTESIAN_POINT('Ctrl Pts',(4.68652417010474,-5.60081898500879,
10.9525692723897));
#180674=CARTESIAN_POINT('Ctrl Pts',(6.78612783456425,-2.68048396813529,
11.1112367376761));
#180675=CARTESIAN_POINT('Ctrl Pts',(7.24893206726443,0.88637801416566,11.2699042029625));
#180676=CARTESIAN_POINT('Ctrl Pts',(5.93378011989064,4.25453083756337,11.428571668249));
#180677=CARTESIAN_POINT('Ctrl Pts',(3.19285241050036,6.55273593632083,11.5872391335354));
#180678=CARTESIAN_POINT('Ctrl Pts',(-1.53541180788721,7.57123725402545,
11.7987957539173));
#180679=CARTESIAN_POINT('Ctrl Pts',(-6.00554205653118,4.8474871351901,12.0103523742992));
#180680=CARTESIAN_POINT('Ctrl Pts',(-7.28262268868039,0.207587702725835,
12.2219089946811));
#180681=CARTESIAN_POINT('Ctrl Pts',(-6.27191716258512,-4.49752398818159,
12.433465615063));
#180682=CARTESIAN_POINT('Ctrl Pts',(-1.96419739535735,-7.47148255492932,
12.6450222354449));
#180683=CARTESIAN_POINT('Ctrl Pts',(2.81440621039056,-6.72396999170161,
12.8565788558268));
#180684=CARTESIAN_POINT('Ctrl Pts',(5.68179560826575,-4.58562730985399,
13.0152463211133));
#180685=CARTESIAN_POINT('Ctrl Pts',(7.18667145538097,-1.29785804008884,
13.1739137863997));
#180686=CARTESIAN_POINT('Ctrl Pts',(6.92779700763258,2.28957505042202,13.3325812516861));
#180687=CARTESIAN_POINT('Ctrl Pts',(4.9979528284151,5.32476756532605,13.4912487169725));
#180688=CARTESIAN_POINT('Ctrl Pts',(1.83027665600578,7.06830011540733,13.649916182259));
#180689=CARTESIAN_POINT('Ctrl Pts',(-1.74664355286525,7.07685601560628,
13.8085836475454));
#180690=CARTESIAN_POINT('Ctrl Pts',(-6.02959695876137,4.82960490013808,
14.0201402679273));
#180691=CARTESIAN_POINT('Ctrl Pts',(-7.7167925087142,-0.125619648347784,
14.2316968883092));
#180692=CARTESIAN_POINT('Ctrl Pts',(-5.72469512022718,-4.50639009190866,
14.4432535086911));
#180693=CARTESIAN_POINT('Ctrl Pts',(-1.93422387439583,-7.47150887855429,
14.654810129073));
#180694=CARTESIAN_POINT('Ctrl Pts',(3.27863805495107,-6.99511654521699,
14.8663667494549));
#180695=CARTESIAN_POINT('Ctrl Pts',(6.46880555178497,-3.35964425193866,
15.0779233698368));
#180696=CARTESIAN_POINT('Ctrl Pts',(7.30044898119669,0.119263707518536,
15.2365908351232));
#180697=CARTESIAN_POINT('Ctrl Pts',(6.34952905775644,3.60779196247754,15.3952583004097));
#180698=CARTESIAN_POINT('Ctrl Pts',(3.85239056755433,6.19641930517106,15.5539257656961));
#180699=CARTESIAN_POINT('Ctrl Pts',(0.426063761775362,7.29048364449936,
15.7125932309825));
#180700=CARTESIAN_POINT('Ctrl Pts',(-3.12315621384476,6.59974805753294,
15.871260696269));
#180701=CARTESIAN_POINT('Ctrl Pts',(-5.87504698961792,4.31468163786968,
16.0299281615554));
#180702=CARTESIAN_POINT('Ctrl Pts',(-7.72380553529842,-0.154761201324391,
16.2414847819373));
#180703=CARTESIAN_POINT('Ctrl Pts',(-5.84457985362868,-5.04039217255527,
16.4530414023192));
#180704=CARTESIAN_POINT('Ctrl Pts',(-1.50837888309736,-7.12772607673944,
16.6645980227011));
#180705=CARTESIAN_POINT('Ctrl Pts',(3.30166900737697,-6.97593353497041,
16.876154643083));
#180706=CARTESIAN_POINT('Ctrl Pts',(6.99896548152602,-3.2704136076266,17.0877112634649));
#180707=CARTESIAN_POINT('Ctrl Pts',(7.11927210416913,1.56480652899573,17.2992678838468));
#180708=CARTESIAN_POINT('Ctrl Pts',(5.52897756315104,4.76877198712199,17.4579353491332));
#180709=CARTESIAN_POINT('Ctrl Pts',(2.5638425465892,6.83808405155348,17.6166028144197));
#180710=CARTESIAN_POINT('Ctrl Pts',(-1.01195855279308,7.22581934301619,
17.7752702797061));
#180711=CARTESIAN_POINT('Ctrl Pts',(-4.34367742670664,5.87070255697988,
17.9339377449926));
#180712=CARTESIAN_POINT('Ctrl Pts',(-6.62628248831759,3.06645716487327,
18.092605210279));
#180713=CARTESIAN_POINT('Ctrl Pts',(-7.27524254505321,-0.451110493156939,
18.2512726755654));
#180714=CARTESIAN_POINT('Ctrl Pts',(-5.83129435071667,-5.06726051943665,
18.4628292959473));
#180715=CARTESIAN_POINT('Ctrl Pts',(-1.25830740500688,-7.61454722180532,
18.6743859163292));
#180716=CARTESIAN_POINT('Ctrl Pts',(3.40838641667838,-6.43914496766518,
18.8859425367111));
#180717=CARTESIAN_POINT('Ctrl Pts',(7.0043589337785,-3.24092931817342,19.097499157093));
#180718=CARTESIAN_POINT('Ctrl Pts',(7.46916864160391,1.97297814985943,19.3090557774749));
#180719=CARTESIAN_POINT('Ctrl Pts',(4.46374735160538,5.76260482311814,19.5206123978568));
#180720=CARTESIAN_POINT('Ctrl Pts',(1.1900032485206,7.20379562643869,19.6792798631432));
#180721=CARTESIAN_POINT('Ctrl Pts',(-2.41242090028973,6.89296072088447,
19.8379473284297));
#180722=CARTESIAN_POINT('Ctrl Pts',(-5.40638235949189,4.89975051134777,
19.9966147937161));
#180723=CARTESIAN_POINT('Ctrl Pts',(-7.09633602667786,1.7247310214306,20.1552822590025));
#180724=CARTESIAN_POINT('Ctrl Pts',(-7.05234807878063,-1.89081086698428,
20.313949724289));
#180725=CARTESIAN_POINT('Ctrl Pts',(-5.29701847508217,-5.00741949920584,
20.4726171895754));
#180726=CARTESIAN_POINT('Ctrl Pts',(-1.23089278942476,-7.62666545204941,
20.6841738099573));
#180727=CARTESIAN_POINT('Ctrl Pts',(3.91228788997283,-6.65271902191656,
20.8957304303392));
#180728=CARTESIAN_POINT('Ctrl Pts',(6.7423921741068,-2.76040461718001,21.1072870507211));
#180729=CARTESIAN_POINT('Ctrl Pts',(7.45442002495894,1.99907203724366,21.318843671103));
#180730=CARTESIAN_POINT('Ctrl Pts',(4.47089830846171,6.30017390965807,21.5304002914849));
#180731=CARTESIAN_POINT('Ctrl Pts',(-0.264617112092554,7.28441024039534,
21.7419569118668));
#180732=CARTESIAN_POINT('Ctrl Pts',(-3.70157536819359,6.29357759565806,
21.9006243771533));
#180733=CARTESIAN_POINT('Ctrl Pts',(-6.26842339864247,3.74693877654311,
22.0592918424397));
#180734=CARTESIAN_POINT('Ctrl Pts',(-7.29023306121876,0.298374267641664,
22.2179593077261));
#180735=CARTESIAN_POINT('Ctrl Pts',(-6.55365419606674,-3.22215747259312,
22.3766267730125));
#180736=CARTESIAN_POINT('Ctrl Pts',(-4.2035000142001,-5.97003909447894,
22.535294238299));
#180737=CARTESIAN_POINT('Ctrl Pts',(-0.859006836306873,-7.23842261971257,
22.6939617035854));
#180738=CARTESIAN_POINT('Ctrl Pts',(3.94110103574177,-6.64445976755199,
22.9055183239673));
#180739=CARTESIAN_POINT('Ctrl Pts',(7.26612585956124,-2.60155374951473,
23.1170749443492));
#180740=CARTESIAN_POINT('Ctrl Pts',(6.94541914943577,2.20019060961913,23.3286315647311));
#180741=CARTESIAN_POINT('Ctrl Pts',(4.44285646893537,6.31076012181081,23.540188185113));
#180742=CARTESIAN_POINT('Ctrl Pts',(-0.603532440634358,7.70174470945665,
23.7517448054949));
#180743=CARTESIAN_POINT('Ctrl Pts',(-4.87010077296144,5.42353881036995,
23.9633014258768));
#180744=CARTESIAN_POINT('Ctrl Pts',(-6.87424567478842,2.46079774903175,
24.1219688911633));
#180745=CARTESIAN_POINT('Ctrl Pts',(-7.21354498832649,-1.13905697890876,
24.2806363564497));
#180746=CARTESIAN_POINT('Ctrl Pts',(-5.78870296013593,-4.44155865995165,
24.4393038217361));
#180747=CARTESIAN_POINT('Ctrl Pts',(-2.96763823370584,-6.67276594926407,
24.5979712870226));
#180748=CARTESIAN_POINT('Ctrl Pts',(0.597336160113703,-7.27694775787263,
24.7566387523089));
#180749=CARTESIAN_POINT('Ctrl Pts',(3.97790360703269,-6.10810426069701,
24.9153062175955));
#180750=CARTESIAN_POINT('Ctrl Pts',(7.28295751464038,-2.57675237779755,
25.1268628379772));
#180751=CARTESIAN_POINT('Ctrl Pts',(7.24577773808857,2.65770048892243,25.3384194583593));
#180752=CARTESIAN_POINT('Ctrl Pts',(3.92318728070308,6.13907871268442,25.549976078741));
#180753=CARTESIAN_POINT('Ctrl Pts',(-0.631845655261499,7.69190730485788,
25.7615326991231));
#180754=CARTESIAN_POINT('Ctrl Pts',(-5.39769956561323,5.52684018005954,
25.9730893195048));
#180755=CARTESIAN_POINT('Ctrl Pts',(-7.21404553293603,1.0441272983282,26.1846459398869));
#180756=CARTESIAN_POINT('Ctrl Pts',(-6.85470811288257,-2.51470790474136,
26.3433134051732));
#180757=CARTESIAN_POINT('Ctrl Pts',(-4.80889757630427,-5.49610645825077,
26.5019808704597));
#180758=CARTESIAN_POINT('Ctrl Pts',(-1.59906073563414,-7.11895568564879,
26.6606483357461));
#180759=CARTESIAN_POINT('Ctrl Pts',(1.99646611371862,-7.02472811976266,
26.8193158010326));
#180760=CARTESIAN_POINT('Ctrl Pts',(5.1207860900796,-5.20464494260984,26.977983266319));
#180761=CARTESIAN_POINT('Ctrl Pts',(6.96758661695681,-2.14135272703788,
27.1366507316054));
#180762=CARTESIAN_POINT('Ctrl Pts',(7.24281175153932,2.68752691303849,27.3482073519873));
#180763=CARTESIAN_POINT('Ctrl Pts',(3.8606926253612,6.68279278229395,27.5597639723692));
#180764=CARTESIAN_POINT('Ctrl Pts',(-0.92086328633324,7.22714996993207,
27.7713205927511));
#180765=CARTESIAN_POINT('Ctrl Pts',(-5.41313628853642,5.50114737489633,
27.9828772131331));
#180766=CARTESIAN_POINT('Ctrl Pts',(-7.68532563280776,0.785425295142589,
28.1944338335149));
#180767=CARTESIAN_POINT('Ctrl Pts',(-6.20798885225515,-3.82014779513366,
28.4059904538969));
#180768=CARTESIAN_POINT('Ctrl Pts',(-3.65203538103778,-6.32245337939593,
28.5646579191832));
#180769=CARTESIAN_POINT('Ctrl Pts',(-0.171132320066336,-7.3009174648697,
28.7233253844697));
#180770=CARTESIAN_POINT('Ctrl Pts',(3.33314067339357,-6.49050834232939,
28.8819928497561));
#180771=CARTESIAN_POINT('Ctrl Pts',(6.03346730846092,-4.11460257346248,
29.0406603150426));
#180772=CARTESIAN_POINT('Ctrl Pts',(7.26628585314741,-0.715450249379295,
29.199327780329));
#180773=CARTESIAN_POINT('Ctrl Pts',(6.72171682947609,2.81978325953014,29.3579952456154));
#180774=CARTESIAN_POINT('Ctrl Pts',(3.83930631857236,6.70379369974286,29.5695518659973));
#180775=CARTESIAN_POINT('Ctrl Pts',(-1.31719041161547,7.60458258802853,
29.7811084863792));
#180776=CARTESIAN_POINT('Ctrl Pts',(-5.33729063949059,4.95913445165702,
29.9926651067611));
#180777=CARTESIAN_POINT('Ctrl Pts',(-7.6807174806566,0.755808111186173,
30.2042217271431));
#180778=CARTESIAN_POINT('Ctrl Pts',(-6.40410093183508,-4.32071917988325,
30.4157783475249));
#180779=CARTESIAN_POINT('Ctrl Pts',(-2.31911537984777,-6.91045285211773,
30.6273349679068));
#180780=CARTESIAN_POINT('Ctrl Pts',(1.2465406732832,-7.19422793000318,30.7860024331933));
#180781=CARTESIAN_POINT('Ctrl Pts',(4.54610201023657,-5.71538612976707,
30.9446698984797));
#180782=CARTESIAN_POINT('Ctrl Pts',(6.71752456355529,-2.84805003967788,
31.1033373637662));
#180783=CARTESIAN_POINT('Ctrl Pts',(7.26869464646612,0.70622959173733,31.2620048290525));
#180784=CARTESIAN_POINT('Ctrl Pts',(6.03752522859731,4.1059795753313,31.420672294339));
#180785=CARTESIAN_POINT('Ctrl Pts',(3.35446931300588,6.47149058521222,31.5793397596254));
#180786=CARTESIAN_POINT('Ctrl Pts',(-1.34706583454684,7.60700575876862,
31.7908963800074));
#180787=CARTESIAN_POINT('Ctrl Pts',(-5.88340697707029,4.99501644249136,
32.0024530003892));
#180788=CARTESIAN_POINT('Ctrl Pts',(-7.27522915446992,0.388235276547886,
32.2140096207711));
#180789=CARTESIAN_POINT('Ctrl Pts',(-6.38158780188008,-4.34050734885841,
32.425566241153));
#180790=CARTESIAN_POINT('Ctrl Pts',(-2.14899046180226,-7.42044223558306,
32.6371228615349));
#180791=CARTESIAN_POINT('Ctrl Pts',(2.64669056104301,-6.79173643779515,
32.8486794819169));
#180792=CARTESIAN_POINT('Ctrl Pts',(5.5662580231132,-4.72520378175531,33.0073469472032));
#180793=CARTESIAN_POINT('Ctrl Pts',(7.15225342400828,-1.47578896139418,
33.1660144124897));
#180794=CARTESIAN_POINT('Ctrl Pts',(6.98247749603769,2.11696322778769,33.3246818777761));
#180795=CARTESIAN_POINT('Ctrl Pts',(5.12854302045249,5.19910844156755,33.4833493430626));
#180796=CARTESIAN_POINT('Ctrl Pts',(2.00510636243318,7.0207070608534,33.642016808349));
#180797=CARTESIAN_POINT('Ctrl Pts',(-1.57050014739987,7.11801826728517,
33.8006842736354));
#180798=CARTESIAN_POINT('Ctrl Pts',(-5.90789820339567,4.97773661364845,
34.0122408940173));
#180799=CARTESIAN_POINT('Ctrl Pts',(-7.71753351631667,0.0659040448482104,
34.2237975143992));
#180800=CARTESIAN_POINT('Ctrl Pts',(-5.83475426225609,-4.36294952745157,
34.4353541347811));
#180801=CARTESIAN_POINT('Ctrl Pts',(-2.11902682337525,-7.42121231608519,
34.646910755163));
#180802=CARTESIAN_POINT('Ctrl Pts',(3.10405121203628,-7.07431898132942,
34.8584673755449));
#180803=CARTESIAN_POINT('Ctrl Pts',(6.38344726014795,-3.51912714224682,
35.0700239959268));
#180804=CARTESIAN_POINT('Ctrl Pts',(7.30116047104728,-0.0619268520409932,
35.2286914612133));
#180805=CARTESIAN_POINT('Ctrl Pts',(6.43709792822838,3.44912341939353,35.3873589264997));
#180806=CARTESIAN_POINT('Ctrl Pts',(4.00496272239371,6.09891784521768,35.5460263917862));
#180807=CARTESIAN_POINT('Ctrl Pts',(0.606839125529545,7.27766641002028,
35.7046938570725));
#180808=CARTESIAN_POINT('Ctrl Pts',(-2.95842794681358,6.67521409712822,
35.8633613223591));
#180809=CARTESIAN_POINT('Ctrl Pts',(-5.76617316348475,4.45913689127132,
36.0220287876453));
#180810=CARTESIAN_POINT('Ctrl Pts',(-7.72526750394771,0.0369454867507112,
36.2335854080274));
#180811=CARTESIAN_POINT('Ctrl Pts',(-5.96785284504142,-4.89381235219836,
36.4451420284092));
#180812=CARTESIAN_POINT('Ctrl Pts',(-1.68478230696053,-7.08810231713384,
36.6566986487911));
#180813=CARTESIAN_POINT('Ctrl Pts',(3.12755108137221,-7.05571336946209,
36.868255269173));
#180814=CARTESIAN_POINT('Ctrl Pts',(6.9156581202202,-3.44307939797708,37.0798118895549));
#180815=CARTESIAN_POINT('Ctrl Pts',(7.15590917899246,1.38766659843061,37.2913685099369));
#180816=CARTESIAN_POINT('Ctrl Pts',(5.64560773197196,4.63010717971896,37.4500359752233));
#180817=CARTESIAN_POINT('Ctrl Pts',(2.73273377903033,6.77235913052149,37.6087034405097));
#180818=CARTESIAN_POINT('Ctrl Pts',(-0.83234498276647,7.24870520300981,
37.7673709057962));
#180819=CARTESIAN_POINT('Ctrl Pts',(-4.19666392570441,5.97667917781288,
37.9260383710825));
#180820=CARTESIAN_POINT('Ctrl Pts',(-6.54815087122052,3.22993797567709,
38.084705836369));
#180821=CARTESIAN_POINT('Ctrl Pts',(-7.28419626503113,-0.270443226750539,
38.2433733016553));
#180822=CARTESIAN_POINT('Ctrl Pts',(-5.9552381459358,-4.92100209324613,
38.4549299220374));
#180823=CARTESIAN_POINT('Ctrl Pts',(-1.44686784289757,-7.58097885261444,
38.6664865424192));
#180824=CARTESIAN_POINT('Ctrl Pts',(3.2475555385614,-6.52173818118793,38.8780431628012));
#180825=CARTESIAN_POINT('Ctrl Pts',(6.9217815368992,-3.41373802070984,39.089599783183));
#180826=CARTESIAN_POINT('Ctrl Pts',(7.51582637584137,1.78703018014509,39.3011564035649));
#180827=CARTESIAN_POINT('Ctrl Pts',(4.60536655768288,5.65006669303687,39.5127130239469));
#180828=CARTESIAN_POINT('Ctrl Pts',(1.36839230042613,7.17204863836835,39.6713804892333));
#180829=CARTESIAN_POINT('Ctrl Pts',(-2.24063568138784,6.9507002412061,39.8300479545197));
#180830=CARTESIAN_POINT('Ctrl Pts',(-5.2831349041589,5.03239613652743,39.9887154198062));
#180831=CARTESIAN_POINT('Ctrl Pts',(-7.05135335594436,1.9002889120929,40.1473828850925));
#180832=CARTESIAN_POINT('Ctrl Pts',(-7.09709525436831,-1.71523121164749,
40.306050350379));
#180833=CARTESIAN_POINT('Ctrl Pts',(-5.41964188346313,-4.87443705687134,
40.4647178156654));
#180834=CARTESIAN_POINT('Ctrl Pts',(-1.41976237131237,-7.59377361958779,
40.6762744360474));
#180835=CARTESIAN_POINT('Ctrl Pts',(3.7460022112624,-6.74775031783296,40.8878310564292));
#180836=CARTESIAN_POINT('Ctrl Pts',(6.67181921361694,-2.92686082019938,
41.0993876768112));
#180837=CARTESIAN_POINT('Ctrl Pts',(7.50172979602892,1.81348200596779,41.310944297193));
#180838=CARTESIAN_POINT('Ctrl Pts',(4.62585458842672,6.18729280891685,41.5225009175749));
#180839=CARTESIAN_POINT('Ctrl Pts',(-0.0837797822404395,7.28873347807959,
41.7340575379569));
#180840=CARTESIAN_POINT('Ctrl Pts',(-3.54426633103808,6.38349084229388,
41.8927250032432));
#180841=CARTESIAN_POINT('Ctrl Pts',(-6.17351645534622,3.90133011617787,
42.0513924685297));
#180842=CARTESIAN_POINT('Ctrl Pts',(-7.28058439966683,0.479182731092116,
42.2100599338161));
#180843=CARTESIAN_POINT('Ctrl Pts',(-6.63159105267217,-3.05854249765599,
42.3687273991026));
#180844=CARTESIAN_POINT('Ctrl Pts',(-4.35034664277355,-5.86389488707565,
42.5273948643889));
#180845=CARTESIAN_POINT('Ctrl Pts',(-1.03835704400452,-7.21487833684687,
42.6860623296755));
#180846=CARTESIAN_POINT('Ctrl Pts',(3.77501143071734,-6.74020857799426,
42.8976189500573));
#180847=CARTESIAN_POINT('Ctrl Pts',(7.1993333690414,-2.78105482849902,43.1091755704392));
#180848=CARTESIAN_POINT('Ctrl Pts',(6.99787622017836,2.02716903286916,43.3207321908211));
#180849=CARTESIAN_POINT('Ctrl Pts',(4.59808407027556,6.19857159357774,43.532288811203));
#180850=CARTESIAN_POINT('Ctrl Pts',(-0.412234987062465,7.71434931083846,
43.743845431585));
#180851=CARTESIAN_POINT('Ctrl Pts',(-4.73402112950856,5.54271582504479,
43.9554020519668));
#180852=CARTESIAN_POINT('Ctrl Pts',(-6.81106657879855,2.63061802727325,
44.1140695172533));
#180853=CARTESIAN_POINT('Ctrl Pts',(-7.23958845831873,-0.959708849175259,
44.2727369825396));
#180854=CARTESIAN_POINT('Ctrl Pts',(-5.89713365859142,-4.29654976458308,
44.4314044478262));
#180855=CARTESIAN_POINT('Ctrl Pts',(-3.13230292181754,-6.59707211633677,
44.5900719131126));
#180856=CARTESIAN_POINT('Ctrl Pts',(0.416581565586644,-7.28952941102346,
44.748739378399));
#180857=CARTESIAN_POINT('Ctrl Pts',(3.82511181316626,-6.20493143702771,
44.9074068436854));
#180858=CARTESIAN_POINT('Ctrl Pts',(7.21677530648096,-2.75667877403707,
45.1189634640673));
#180859=CARTESIAN_POINT('Ctrl Pts',(7.30949492399773,2.47708495470907,45.3305200844492));
#180860=CARTESIAN_POINT('Ctrl Pts',(4.07431487762509,6.03983811237955,45.5420767048312));
#180861=CARTESIAN_POINT('Ctrl Pts',(-0.440783824531858,7.70521760537255,
45.7536333252129));
#180862=CARTESIAN_POINT('Ctrl Pts',(-5.25889366826367,5.65907705053069,
45.9651899455951));
#180863=CARTESIAN_POINT('Ctrl Pts',(-7.18591574462435,1.22281586655384,
46.1767465659768));
#180864=CARTESIAN_POINT('Ctrl Pts',(-6.9149963450596,-2.34384093444894,
46.3354140312633));
#180865=CARTESIAN_POINT('Ctrl Pts',(-4.94379997775315,-5.37508475202271,
46.4940814965496));
#180866=CARTESIAN_POINT('Ctrl Pts',(-1.77521407621494,-7.07708644730382,
46.6527489618362));
#180867=CARTESIAN_POINT('Ctrl Pts',(1.82153073585822,-7.07210174974048,
46.8114164271225));
#180868=CARTESIAN_POINT('Ctrl Pts',(4.99007686623289,-5.33011694781774,
46.9700838924091));
#180869=CARTESIAN_POINT('Ctrl Pts',(6.91227697700186,-2.31357490358806,
47.1287513576954));
#180870=CARTESIAN_POINT('Ctrl Pts',(7.30733455477124,2.50694719739402,47.3403079780773));
#180871=CARTESIAN_POINT('Ctrl Pts',(4.02520767790373,6.58499020741276,47.5518645984592));
#180872=CARTESIAN_POINT('Ctrl Pts',(-0.741099433620822,7.24771064107016,
47.7634212188411));
#180873=CARTESIAN_POINT('Ctrl Pts',(-5.27532288542961,5.63393445682585,
47.9749778392231));
#180874=CARTESIAN_POINT('Ctrl Pts',(-7.66274994821465,0.975569028180616,
48.1865344596049));
#180875=CARTESIAN_POINT('Ctrl Pts',(-6.30175893983736,-3.66453279862005,
48.3980910799869));
#180876=CARTESIAN_POINT('Ctrl Pts',(-3.80592445995426,-6.23071373925649,
48.5567585452732));
#180877=CARTESIAN_POINT('Ctrl Pts',(-0.355881681196406,-7.29281176210305,
48.7154260105597));
#180878=CARTESIAN_POINT('Ctrl Pts',(3.17791768866892,-6.5742646074729,48.8740934758461));
#180879=CARTESIAN_POINT('Ctrl Pts',(5.91706485393949,-4.25746597045867,
49.0327609411326));
#180880=CARTESIAN_POINT('Ctrl Pts',(7.71518712742009,0.212958204582113,
49.2443175615145));
#180881=CARTESIAN_POINT('Ctrl Pts',(5.3332736079391,6.33388915228324,49.5087633369919));
#180882=CARTESIAN_POINT('Ctrl Pts',(-2.45101487628526,7.91115770243905,
49.8260982675646));
#180883=CARTESIAN_POINT('Ctrl Pts',(-7.02573858895822,3.19290517876247,
50.0905440430422));
#180884=CARTESIAN_POINT('Ctrl Pts',(-7.10655132029403,-1.61882067803289,
50.3021006634239));
#180885=CARTESIAN_POINT('Ctrl Pts',(-5.48414662636755,-4.82881078130398,
50.4607681287105));
#180886=CARTESIAN_POINT('Ctrl Pts',(-2.50656909549661,-6.84409312782312,
50.6194355939968));
#180887=CARTESIAN_POINT('Ctrl Pts',(2.27895306528776,-7.37372428966872,
50.8309922143788));
#180888=CARTESIAN_POINT('Ctrl Pts',(7.53371292847594,-3.43308380079491,
51.0954379898561));
#180889=CARTESIAN_POINT('Ctrl Pts',(6.96415171352099,4.48792878509655,51.412772920429));
#180890=CARTESIAN_POINT('Ctrl Pts',(1.17864575368756,7.62636082207304,51.6772186959064));
#180891=CARTESIAN_POINT('Ctrl Pts',(-3.46063736178883,6.40824902510984,
51.8887753162883));
#180892=CARTESIAN_POINT('Ctrl Pts',(-7.03711701014562,3.17872162429317,
52.1003319366701));
#180893=CARTESIAN_POINT('Ctrl Pts',(-7.44912142538699,-2.03950264176283,
52.3118885570521));
#180894=CARTESIAN_POINT('Ctrl Pts',(-4.4132576416278,-5.8020426150045,52.523445177434));
#180895=CARTESIAN_POINT('Ctrl Pts',(-1.12530437433415,-7.2141332047132,
52.6821126427204));
#180896=CARTESIAN_POINT('Ctrl Pts',(2.47337717630653,-6.87120137135288,
52.8407801080068));
#180897=CARTESIAN_POINT('Ctrl Pts',(5.44992684100399,-4.85145260601411,
52.9994475732933));
#180898=CARTESIAN_POINT('Ctrl Pts',(7.11132296817816,-1.6615052764948,53.1581150385797));
#180899=CARTESIAN_POINT('Ctrl Pts',(7.03528347837356,1.95349460782157,53.3167825038662));
#180900=CARTESIAN_POINT('Ctrl Pts',(5.2522263462681,5.05436226548548,53.4754499691526));
#180901=CARTESIAN_POINT('Ctrl Pts',(1.16298787833305,7.63731658881341,53.6870065895345));
#180902=CARTESIAN_POINT('Ctrl Pts',(-3.9713456319968,6.61763934552863,53.8985632099163));
#180903=CARTESIAN_POINT('Ctrl Pts',(-6.76668767926396,2.70029239264587,
54.1101198302983));
#180904=CARTESIAN_POINT('Ctrl Pts',(-7.43633718779138,-2.06533199412456,
54.3216764506802));
#180905=CARTESIAN_POINT('Ctrl Pts',(-4.41465255275869,-6.3397124742808,
54.5332330710621));
#180906=CARTESIAN_POINT('Ctrl Pts',(0.329432312156239,-7.2817668285877,
54.7447896914439));
#180907=CARTESIAN_POINT('Ctrl Pts',(3.75743771505433,-6.26038688161627,
54.9034571567305));
#180908=CARTESIAN_POINT('Ctrl Pts',(6.30152019550041,-3.69100566880029,
55.0621246220168));
#180909=CARTESIAN_POINT('Ctrl Pts',(7.29259979915511,-0.233484326409,55.2207920873034));
#180910=CARTESIAN_POINT('Ctrl Pts',(6.52471960310607,3.2803529583477,55.3794595525896));
#180911=CARTESIAN_POINT('Ctrl Pts',(4.15020428334716,6.00721098109562,55.5381270178762));
#180912=CARTESIAN_POINT('Ctrl Pts',(0.794555753034778,7.24578055922568,
55.6967944831625));
#180913=CARTESIAN_POINT('Ctrl Pts',(-4.00007614591683,6.60912352067989,
55.9083511035445));
#180914=CARTESIAN_POINT('Ctrl Pts',(-7.28899019261408,2.53678713496527,
56.1199077239264));
#180915=CARTESIAN_POINT('Ctrl Pts',(-6.92556390568595,-2.26191300443743,
56.3314643443083));
#180916=CARTESIAN_POINT('Ctrl Pts',(-4.38651904809834,-6.35004862765727,
56.5430209646902));
#180917=CARTESIAN_POINT('Ctrl Pts',(0.672048848250074,-7.69606869279577,
56.7545775850721));
#180918=CARTESIAN_POINT('Ctrl Pts',(4.91817373622454,-5.37998344443186,
56.966134205454));
#180919=CARTESIAN_POINT('Ctrl Pts',(6.89587288824271,-2.39952417604946,
57.1248016707404));
#180920=CARTESIAN_POINT('Ctrl Pts',(7.20312249874772,1.20320753242157,57.2834691360269));
#180921=CARTESIAN_POINT('Ctrl Pts',(5.7489468681493,4.49289830715034,57.4421366013132));
#180922=CARTESIAN_POINT('Ctrl Pts',(2.90813762287981,6.6989116777301,57.6008040665998));
#180923=CARTESIAN_POINT('Ctrl Pts',(-0.662072407274711,7.27134370570345,
57.7594715318861));
#180924=CARTESIAN_POINT('Ctrl Pts',(-4.03210406990081,6.07246173606323,
57.9181389971726));
#180925=CARTESIAN_POINT('Ctrl Pts',(-7.30560046055249,2.51183695474357,
58.1296956175544));
#180926=CARTESIAN_POINT('Ctrl Pts',(-7.22183907457384,-2.72207775414384,
58.3412522379364));
#180927=CARTESIAN_POINT('Ctrl Pts',(-3.86839828499165,-6.1737493137209,
58.5528088583183));
#180928=CARTESIAN_POINT('Ctrl Pts',(0.700273394512465,-7.68597970928456,
58.7643654787002));
#180929=CARTESIAN_POINT('Ctrl Pts',(5.44667094866594,-5.47858545187604,
58.9759220990821));
#180930=CARTESIAN_POINT('Ctrl Pts',(7.22305188360823,-0.979885836762679,
59.187478719464));
#180931=CARTESIAN_POINT('Ctrl Pts',(6.83205747267965,2.57561057790011,59.3461461847504));
#180932=CARTESIAN_POINT('Ctrl Pts',(4.75979552384035,5.53868474197977,59.5048136500368));
#180933=CARTESIAN_POINT('Ctrl Pts',(1.5356435340166,7.13290433322296,59.6634811153233));
#180934=CARTESIAN_POINT('Ctrl Pts',(-2.0589023719168,7.00668274740098,59.8221485806097));
#180935=CARTESIAN_POINT('Ctrl Pts',(-5.16690111965939,5.1588673154724,59.9808160458961));
#180936=CARTESIAN_POINT('Ctrl Pts',(-6.98636728977782,2.07926113288135,
60.1394835111826));
#180937=CARTESIAN_POINT('Ctrl Pts',(-7.2186077705201,-2.7518766018717,60.3510401315645));
#180938=CARTESIAN_POINT('Ctrl Pts',(-3.80106741782251,-6.71688569232549,
60.5625967519464));
#180939=CARTESIAN_POINT('Ctrl Pts',(0.985143555366984,-7.21866871766008,
60.7741533723283));
#180940=CARTESIAN_POINT('Ctrl Pts',(5.46187841175089,-5.45275628777296,
60.9857099927101));
#180941=CARTESIAN_POINT('Ctrl Pts',(7.692011048468,-0.717000004733705,61.1972666130922));
#180942=CARTESIAN_POINT('Ctrl Pts',(6.17374629198927,3.8752434102308,61.408823233474));
#180943=CARTESIAN_POINT('Ctrl Pts',(3.59562521266291,6.35470365076531,61.5674906987604));
#180944=CARTESIAN_POINT('Ctrl Pts',(0.106152327585856,7.30215131198737,
61.7261581640469));
#180945=CARTESIAN_POINT('Ctrl Pts',(-3.39076980577516,6.46058862757269,
61.8848256293334));
#180946=CARTESIAN_POINT('Ctrl Pts',(-6.06984555801569,4.06074586765145,
62.0434930946197));
#180947=CARTESIAN_POINT('Ctrl Pts',(-7.27236513221156,0.650756899909928,
62.2021605599062));
#180948=CARTESIAN_POINT('Ctrl Pts',(-6.6963564918669,-2.8794903195219,62.3608280251925));
#180949=CARTESIAN_POINT('Ctrl Pts',(-3.77949506399865,-6.73769545451199,
62.5723846455745));
#180950=CARTESIAN_POINT('Ctrl Pts',(1.38481388060952,-7.5925593467993,62.7839412659564));
#180951=CARTESIAN_POINT('Ctrl Pts',(5.38121221862196,-4.91143980296606,
62.9954978863382));
#180952=CARTESIAN_POINT('Ctrl Pts',(7.68713950594068,-0.687425003040209,
63.2070545067203));
#180953=CARTESIAN_POINT('Ctrl Pts',(6.36539585962448,4.37754023703006,63.418611127102));
#180954=CARTESIAN_POINT('Ctrl Pts',(2.25752519810707,6.93081775451498,63.6301677474841));
#180955=CARTESIAN_POINT('Ctrl Pts',(-1.31051506173819,7.18284967348925,
63.7888352127705));
#180956=CARTESIAN_POINT('Ctrl Pts',(-4.59678504746447,5.67470257610194,
63.9475026780568));
#180957=CARTESIAN_POINT('Ctrl Pts',(-6.74260426573885,2.78815584322654,
64.1061701433434));
#180958=CARTESIAN_POINT('Ctrl Pts',(-7.26212184340347,-0.770888079667159,
64.2648376086296));
#180959=CARTESIAN_POINT('Ctrl Pts',(-6.00074570958805,-4.15954686087889,
64.4235050739162));
#180960=CARTESIAN_POINT('Ctrl Pts',(-3.29674459808297,-6.50108681847883,
64.5821725392026));
#180961=CARTESIAN_POINT('Ctrl Pts',(1.41470968505832,-7.5947165505728,64.7937291595845));
#180962=CARTESIAN_POINT('Ctrl Pts',(5.92762625552272,-4.94246030772492,
65.0052857799664));
#180963=CARTESIAN_POINT('Ctrl Pts',(7.27839608796312,-0.323475295391354,
65.2168424003483));
#180964=CARTESIAN_POINT('Ctrl Pts',(6.3427075198956,4.39712727080518,65.4283990207302));
#180965=CARTESIAN_POINT('Ctrl Pts',(2.08286845720701,7.43927294609588,65.6399556411121));
#180966=CARTESIAN_POINT('Ctrl Pts',(-2.70702760250574,6.767913735093,65.8515122614941));
#180967=CARTESIAN_POINT('Ctrl Pts',(-5.60808871082759,4.67548074217773,
66.0101797267804));
#180968=CARTESIAN_POINT('Ctrl Pts',(-7.16510371778334,1.41208031401127,
66.1688471920669));
#180969=CARTESIAN_POINT('Ctrl Pts',(-6.96336145416755,-2.17901871242343,
66.3275146573532));
#180970=CARTESIAN_POINT('Ctrl Pts',(-5.08207139110363,-5.24454311408888,
66.4861821226398));
#180971=CARTESIAN_POINT('Ctrl Pts',(-1.9425474276618,-7.03827312984311,
66.6448495879261));
#180972=CARTESIAN_POINT('Ctrl Pts',(1.63378349280974,-7.10376000896784,
66.8035170532126));
#180973=CARTESIAN_POINT('Ctrl Pts',(5.95196273324006,-4.92496320784874,
67.0150736735945));
#180974=CARTESIAN_POINT('Ctrl Pts',(7.71781440523415,0.00277938102636093,
67.2266302939764));
#180975=CARTESIAN_POINT('Ctrl Pts',(5.79569591456879,4.41470211292405,67.4381869143583));
#180976=CARTESIAN_POINT('Ctrl Pts',(2.05289915213827,7.43977634003525,67.6497435347402));
#180977=CARTESIAN_POINT('Ctrl Pts',(-3.16688493518823,7.04641488870896,
67.8613001551221));
#180978=CARTESIAN_POINT('Ctrl Pts',(-6.41451232295659,3.46217943281784,
68.072856775504));
#180979=CARTESIAN_POINT('Ctrl Pts',(-7.30142245391383,-0.0030509785204721,
68.2315242407905));
#180980=CARTESIAN_POINT('Ctrl Pts',(-6.40614816070338,-3.50627264241207,
68.3901917060768));
#180981=CARTESIAN_POINT('Ctrl Pts',(-3.95052789288941,-6.13431778260475,
68.5488591713634));
#180982=CARTESIAN_POINT('Ctrl Pts',(-0.542048797793145,-7.28277867304929,
68.7075266366497));
#180983=CARTESIAN_POINT('Ctrl Pts',(3.01771567371951,-6.64862175729487,
68.8661941019362));
#180984=CARTESIAN_POINT('Ctrl Pts',(5.80562811966774,-4.40764527866205,
69.0248615672226));
#180985=CARTESIAN_POINT('Ctrl Pts',(7.72529037506696,0.0318056196186821,
69.2364181876045));
#180986=CARTESIAN_POINT('Ctrl Pts',(5.92406490744874,4.9467284027863,69.4479748079864));
#180987=CARTESIAN_POINT('Ctrl Pts',(1.62163628485237,7.10281505036246,69.6595314283683));
#180988=CARTESIAN_POINT('Ctrl Pts',(-3.19021829660345,7.02760088071422,
69.8710880487503));
#180989=CARTESIAN_POINT('Ctrl Pts',(-6.94602533424518,3.38139838418462,
70.082644669132));
#180990=CARTESIAN_POINT('Ctrl Pts',(-7.14327651483587,-1.45129438742892,
70.2942012895141));
#180991=CARTESIAN_POINT('Ctrl Pts',(-5.60417935245795,-4.68016590993002,
70.4528687548005));
#180992=CARTESIAN_POINT('Ctrl Pts',(-2.67235615860385,-6.79641042473032,
70.6115362200868));
#180993=CARTESIAN_POINT('Ctrl Pts',(0.896820584063685,-7.24101085004557,
70.7702036853734));
#180994=CARTESIAN_POINT('Ctrl Pts',(4.24968613157379,-5.93909503905437,
70.9288711506597));
#180995=CARTESIAN_POINT('Ctrl Pts',(6.57663582428436,-3.17153596759146,
71.0875386159461));
#180996=CARTESIAN_POINT('Ctrl Pts',(7.28150105130947,0.335256925607207,
71.2462060812327));
#180997=CARTESIAN_POINT('Ctrl Pts',(5.91120873762049,4.97380480485727,71.4577627016144));
#180998=CARTESIAN_POINT('Ctrl Pts',(1.37934497512927,7.59355479062239,71.6693193219963));
#180999=CARTESIAN_POINT('Ctrl Pts',(-3.30546598448607,6.49257887941386,
71.8808759423784));
#181000=CARTESIAN_POINT('Ctrl Pts',(-6.95188739007309,3.35200367457157,
72.0924325627602));
#181001=CARTESIAN_POINT('Ctrl Pts',(-7.49962539393021,-1.85384517348655,
72.3039891831422));
#181002=CARTESIAN_POINT('Ctrl Pts',(-4.55490242328635,-5.69082759189985,
72.515545803524));
#181003=CARTESIAN_POINT('Ctrl Pts',(-1.30451174193676,-7.18394239078625,
72.6742132688105));
#181004=CARTESIAN_POINT('Ctrl Pts',(2.30240347260119,-6.93048485671565,
72.8328807340969));
#181005=CARTESIAN_POINT('Ctrl Pts',(5.32771060717041,-4.98518053602091,
72.9915481993833));
#181006=CARTESIAN_POINT('Ctrl Pts',(7.06798540710278,-1.83746139681714,
73.1502156646698));
#181007=CARTESIAN_POINT('Ctrl Pts',(7.08154981624765,1.77832262511333,73.3088831299561));
#181008=CARTESIAN_POINT('Ctrl Pts',(5.37604808188036,4.92247516882501,73.4675505952426));
#181009=CARTESIAN_POINT('Ctrl Pts',(1.35212671216226,7.60610783060554,73.6791072156245));
#181010=CARTESIAN_POINT('Ctrl Pts',(-3.80590427361156,6.71414622857621,
73.8906638360064));
#181011=CARTESIAN_POINT('Ctrl Pts',(-6.69760208823675,2.8673702494886,74.1022204563883));
#181012=CARTESIAN_POINT('Ctrl Pts',(-7.48529396902241,-1.88017050182019,
74.3137770767701));
#181013=CARTESIAN_POINT('Ctrl Pts',(-4.57060869449738,-6.22821476334324,
74.5253336971522));
#181014=CARTESIAN_POINT('Ctrl Pts',(0.14864125104275,-7.28769926279049,
74.736890317534));
#181015=CARTESIAN_POINT('Ctrl Pts',(3.60093471970022,-6.35169649018624,
74.8955577828204));
#181016=CARTESIAN_POINT('Ctrl Pts',(6.20799117870964,-3.84623551344357,
75.054225248107));
#181017=CARTESIAN_POINT('Ctrl Pts',(7.28456049178201,-0.414371490388394,
75.2128927133932));
#181018=CARTESIAN_POINT('Ctrl Pts',(6.60410948866829,3.11743804453148,75.3715601786798));
#181019=CARTESIAN_POINT('Ctrl Pts',(4.29798968114953,5.90237781404404,75.5302276439661));
#181020=CARTESIAN_POINT('Ctrl Pts',(0.974108399537163,7.22383330319435,
75.6888951092526));
#181021=CARTESIAN_POINT('Ctrl Pts',(-3.83484522790941,6.70634662499054,
75.9004517296344));
#181022=CARTESIAN_POINT('Ctrl Pts',(-7.22379777981015,2.71687551334403,
76.1120083500165));
#181023=CARTESIAN_POINT('Ctrl Pts',(-6.97955867591795,-2.08936511156467,
76.3235649703983));
#181024=CARTESIAN_POINT('Ctrl Pts',(-4.54273890266891,-6.23924596251639,
76.5351215907802));
#181025=CARTESIAN_POINT('Ctrl Pts',(0.480871141788821,-7.71037521275954,
76.7466782111622));
#181026=CARTESIAN_POINT('Ctrl Pts',(4.78316007615798,-5.50036675615697,
76.958234831544));
#181027=CARTESIAN_POINT('Ctrl Pts',(6.83420758004432,-2.56989998090428,
77.1169022968304));
#181028=CARTESIAN_POINT('Ctrl Pts',(7.23076101275103,1.02409827472298,77.2755697621169));
#181029=CARTESIAN_POINT('Ctrl Pts',(5.85866375653961,4.34886011252226,77.4342372274033));
#181030=CARTESIAN_POINT('Ctrl Pts',(3.07346940853301,6.62468624876852,77.5929046926898));
#181031=CARTESIAN_POINT('Ctrl Pts',(-0.481436928319852,7.2855334494488,
77.7515721579762));
#181032=CARTESIAN_POINT('Ctrl Pts',(-3.88018004147505,6.17064482952365,
77.9102396232625));
#181033=CARTESIAN_POINT('Ctrl Pts',(-7.2410220538478,2.69234518444999,78.1217962436445));
#181034=CARTESIAN_POINT('Ctrl Pts',(-7.28716117403719,-2.54203637704176,
78.3333528640264));
#181035=CARTESIAN_POINT('Ctrl Pts',(-4.02040297608787,-6.07585761764288,
78.5449094844083));
#181036=CARTESIAN_POINT('Ctrl Pts',(0.509337346907534,-7.70098970169701,
78.7564661047903));
#181037=CARTESIAN_POINT('Ctrl Pts',(5.30904783833082,-5.61205256807673,
78.968022725172));
#181038=CARTESIAN_POINT('Ctrl Pts',(7.19651283393159,-1.15881741333442,
79.1795793455541));
#181039=CARTESIAN_POINT('Ctrl Pts',(6.89386514584086,2.40528636755536,79.3382468108404));
#181040=CARTESIAN_POINT('Ctrl Pts',(4.89576720374896,5.41886940113037,79.4969142761268));
#181041=CARTESIAN_POINT('Ctrl Pts',(1.71216705625423,7.09260243224975,79.6555817414134));
#181042=CARTESIAN_POINT('Ctrl Pts',(-1.88440410108198,7.05561501809986,
79.8142492066997));
#181043=CARTESIAN_POINT('Ctrl Pts',(-5.03729766256781,5.2854906506091,79.9729166719862));
#181044=CARTESIAN_POINT('Ctrl Pts',(-6.93262114598237,2.25198108621416,
80.1315841372726));
#181045=CARTESIAN_POINT('Ctrl Pts',(-7.28467029558747,-2.57190623101369,
80.3431407576545));
#181046=CARTESIAN_POINT('Ctrl Pts',(-3.96657026414199,-6.62049750836168,
80.5546973780365));
#181047=CARTESIAN_POINT('Ctrl Pts',(0.805715678220276,-7.2408913902831,
80.7662539984183));
#181048=CARTESIAN_POINT('Ctrl Pts',(5.32489154541992,-5.5866087162172,80.9778106188002));
#181049=CARTESIAN_POINT('Ctrl Pts',(7.67185086545011,-0.907649312693826,
81.1893672391822));
#181050=CARTESIAN_POINT('Ctrl Pts',(6.26800584722486,3.72085439993874,81.400923859564));
#181051=CARTESIAN_POINT('Ctrl Pts',(3.7522041082529,6.26352484540433,81.5595913248505));
#181052=CARTESIAN_POINT('Ctrl Pts',(0.287315719605677,7.29726878887425,
81.7182587901368));
#181053=CARTESIAN_POINT('Ctrl Pts',(-3.22941224766972,6.54273809846297,
81.8769262554235));
#181054=CARTESIAN_POINT('Ctrl Pts',(-5.96721292964122,4.21011305693017,
82.0355937207096));
#181055=CARTESIAN_POINT('Ctrl Pts',(-7.25397792594564,0.831013482971333,
82.1942611859963));
#181056=CARTESIAN_POINT('Ctrl Pts',(-6.76574644210904,-2.71243983296907,
82.3529286512825));
#181057=CARTESIAN_POINT('Ctrl Pts',(-3.94552092764993,-6.64183616073285,
82.5644852716646));
#181058=CARTESIAN_POINT('Ctrl Pts',(1.19598519098252,-7.62458433893602,
82.7760418920463));
#181059=CARTESIAN_POINT('Ctrl Pts',(5.25768245471263,-5.04345725523793,
82.9875985124284));
#181060=CARTESIAN_POINT('Ctrl Pts',(7.6677146990491,-0.877962534841406,
83.1991551328101));
#181061=CARTESIAN_POINT('Ctrl Pts',(6.47206043035542,4.21824095594002,83.4107117531922));
#181062=CARTESIAN_POINT('Ctrl Pts',(2.42881185107603,6.87266525872325,83.622268373574));
#181063=CARTESIAN_POINT('Ctrl Pts',(-1.13187581356494,7.21315716601639,
83.7809358388604));
#181064=CARTESIAN_POINT('Ctrl Pts',(-4.45455716730101,5.78702017821416,
83.9396033041469));
#181065=CARTESIAN_POINT('Ctrl Pts',(-6.67134261913675,2.95460876404444,
84.0982707694333));
#181066=CARTESIAN_POINT('Ctrl Pts',(-7.27901458618699,-0.59044792648265,
84.2569382347199));
#181067=CARTESIAN_POINT('Ctrl Pts',(-6.10211325965054,-4.0093631570841,
84.415605700006));
#181068=CARTESIAN_POINT('Ctrl Pts',(-3.45704788576693,-6.41727938318902,
84.5742731652928));
#181069=CARTESIAN_POINT('Ctrl Pts',(1.22581826102235,-7.62748271499098,
84.7858297856743));
#181070=CARTESIAN_POINT('Ctrl Pts',(5.80315849686724,-5.08802696325753,
84.9973864060566));
#181071=CARTESIAN_POINT('Ctrl Pts',(7.26812821260561,-0.503982306367513,
85.2089430264381));
#181072=CARTESIAN_POINT('Ctrl Pts',(6.44986511072318,4.23838494854769,85.4204996468203));
#181073=CARTESIAN_POINT('Ctrl Pts',(2.26682573146811,7.38529783283633,85.6320562672021));
#181074=CARTESIAN_POINT('Ctrl Pts',(-2.53825459376176,6.83300215012667,
85.843612887584));
#181075=CARTESIAN_POINT('Ctrl Pts',(-5.49034419207115,4.8132005787809,86.0022803528705));
#181076=CARTESIAN_POINT('Ctrl Pts',(-7.12785800821615,1.58944088110241,
86.1609478181568));
#181077=CARTESIAN_POINT('Ctrl Pts',(-7.01528763922505,-2.00555843330848,
86.3196152834433));
#181078=CARTESIAN_POINT('Ctrl Pts',(-5.21064498668112,-5.11682136903231,
86.4782827487299));
#181079=CARTESIAN_POINT('Ctrl Pts',(-2.11659747242173,-6.98790342654534,
86.636950214016));
#181080=CARTESIAN_POINT('Ctrl Pts',(1.45700724128982,-7.14211345927923,
86.7956176793028));
#181081=CARTESIAN_POINT('Ctrl Pts',(5.82792165520774,-5.07113913803433,
87.0071742996843));
#181082=CARTESIAN_POINT('Ctrl Pts',(7.71550693145075,-0.188731845047518,
87.2187309200666));
#181083=CARTESIAN_POINT('Ctrl Pts',(5.90345804255837,4.26952796217078,87.4302875404482));
#181084=CARTESIAN_POINT('Ctrl Pts',(2.23687814569083,7.38654473214158,87.6418441608304));
#181085=CARTESIAN_POINT('Ctrl Pts',(-2.99105958231513,7.12282847972511,
87.853400781212));
#181086=CARTESIAN_POINT('Ctrl Pts',(-6.32662643415989,3.62028351499959,
88.0649574015941));
#181087=CARTESIAN_POINT('Ctrl Pts',(-7.29924993347449,0.178127953053212,
88.2236248668804));
#181088=CARTESIAN_POINT('Ctrl Pts',(-6.4911804899301,-3.34623040852862,
88.3822923321669));
#181089=CARTESIAN_POINT('Ctrl Pts',(-4.10152883824385,-6.03440025847909,
88.5409597974534));
#181090=CARTESIAN_POINT('Ctrl Pts',(-0.722597256169509,-7.2670857505046,
88.6996272627396));
#181091=CARTESIAN_POINT('Ctrl Pts',(2.85180711825703,-6.72145633916083,
88.8582947280263));
#181092=CARTESIAN_POINT('Ctrl Pts',(5.69446886265268,-4.55034934248657,
89.0169621933125));
#181093=CARTESIAN_POINT('Ctrl Pts',(7.72370085836359,-0.159900053332423,
89.2285188136947));
#181094=CARTESIAN_POINT('Ctrl Pts',(6.04498924497306,4.79820507552133,89.4400754340764));
#181095=CARTESIAN_POINT('Ctrl Pts',(1.79738669100653,7.06038858441927,89.6516320544583));
#181096=CARTESIAN_POINT('Ctrl Pts',(-3.0148526110767,7.10459926048484,89.8631886748402));
#181097=CARTESIAN_POINT('Ctrl Pts',(-6.85998029030325,3.55271634009713,
90.0747452952221));
#181098=CARTESIAN_POINT('Ctrl Pts',(-7.17708950032582,-1.27359376203776,
90.286301915604));
#181099=CARTESIAN_POINT('Ctrl Pts',(-5.71858768820459,-4.53966232348847,
90.4449693808904));
#181100=CARTESIAN_POINT('Ctrl Pts',(-2.84017988572216,-6.72800567156068,
90.603636846177));
#181101=CARTESIAN_POINT('Ctrl Pts',(0.716865503818649,-7.2610349909575,
90.7623043114633));
#181102=CARTESIAN_POINT('Ctrl Pts',(4.10100447634138,-6.04271829434759,
90.9209717767497));
#181103=CARTESIAN_POINT('Ctrl Pts',(6.49591206166963,-3.3337524872193,91.0796392420362));
#181104=CARTESIAN_POINT('Ctrl Pts',(7.28757804590501,0.154470033412751,
91.2383067073226));
#181105=CARTESIAN_POINT('Ctrl Pts',(6.03280890944947,4.82559215419812,91.4498633277045));
#181106=CARTESIAN_POINT('Ctrl Pts',(1.5673472359543,7.55698945086174,91.6614199480865));
#181107=CARTESIAN_POINT('Ctrl Pts',(-3.14334088454258,6.57260176518045,
91.8729765684682));
#181108=CARTESIAN_POINT('Ctrl Pts',(-6.86656994343417,3.52347614302835,
92.0845331888503));
#181109=CARTESIAN_POINT('Ctrl Pts',(-7.54331757626141,-1.6671781308104,
92.2960898092321));
#181110=CARTESIAN_POINT('Ctrl Pts',(-4.69471247615664,-5.57604963511976,
92.5076464296141));
#181111=CARTESIAN_POINT('Ctrl Pts',(-1.48237289522515,-7.14936009422644,
92.6663138949004));
#181112=CARTESIAN_POINT('Ctrl Pts',(2.12972100334073,-6.98548284302441,
92.8249813601869));
#181113=CARTESIAN_POINT('Ctrl Pts',(5.20236750987503,-5.11584768931891,
92.9836488254733));
#181114=CARTESIAN_POINT('Ctrl Pts',(7.02021416653538,-2.01228108246395,
93.1423162907598));
#181115=CARTESIAN_POINT('Ctrl Pts',(7.1234967097829,1.60205299418413,93.3009837560462));
#181116=CARTESIAN_POINT('Ctrl Pts',(5.4965393404678,4.78755783384145,93.4596512213326));
#181117=CARTESIAN_POINT('Ctrl Pts',(1.54044884797169,7.57021402675984,93.6712078417144));
#181118=CARTESIAN_POINT('Ctrl Pts',(-3.63812709720397,6.8065187894964,93.8827644620965));
#181119=CARTESIAN_POINT('Ctrl Pts',(-6.62438866228044,3.03268210390607,
94.0943210824783));
#181120=CARTESIAN_POINT('Ctrl Pts',(-7.52964381413117,-1.6938510040437,
94.3058777028602));
#181121=CARTESIAN_POINT('Ctrl Pts',(-4.72374865002601,-6.11288153979815,
94.5174343232423));
#181122=CARTESIAN_POINT('Ctrl Pts',(-0.0322420101528263,-7.2891437288087,
94.7289909436239));
#181123=CARTESIAN_POINT('Ctrl Pts',(3.44221456469878,-6.43909438121071,
94.8876584089105));
#181124=CARTESIAN_POINT('Ctrl Pts',(6.11063877182138,-3.99909701236707,
95.0463258741969));
#181125=CARTESIAN_POINT('Ctrl Pts',(7.27203543413222,-0.59500289912095,
95.2049933394833));
#181126=CARTESIAN_POINT('Ctrl Pts',(6.67943187871136,2.95260222294936,95.3636608047698));
#181127=CARTESIAN_POINT('Ctrl Pts',(4.44312903876971,5.79391180272748,95.522328270056));
#181128=CARTESIAN_POINT('Ctrl Pts',(1.15305975893871,7.1974337368613,95.6809957353428));
#181129=CARTESIAN_POINT('Ctrl Pts',(-3.66724954191073,6.79944796472536,
95.8925523557242));
#181130=CARTESIAN_POINT('Ctrl Pts',(-7.15416271867079,2.89527501251126,
96.1041089761066));
#181131=CARTESIAN_POINT('Ctrl Pts',(-7.02924814289869,-1.9155119933763,
96.3156655964883));
#181132=CARTESIAN_POINT('Ctrl Pts',(-4.69617864516543,-6.12464676367938,
96.5272222168702));
#181133=CARTESIAN_POINT('Ctrl Pts',(0.289432265469185,-7.71984168134798,
96.7387788372523));
#181134=CARTESIAN_POINT('Ctrl Pts',(4.64515762980606,-5.61747601173444,
96.950335457634));
#181135=CARTESIAN_POINT('Ctrl Pts',(6.76842455697748,-2.73845433636555,
97.1090029229205));
#181136=CARTESIAN_POINT('Ctrl Pts',(7.25376943663278,0.843893506703,97.2676703882068));
#181137=CARTESIAN_POINT('Ctrl Pts',(5.96510980865853,4.20302829244156,97.4263378534934));
#181138=CARTESIAN_POINT('Ctrl Pts',(3.23627226523146,6.54471228718507,97.5850053187797));
#181139=CARTESIAN_POINT('Ctrl Pts',(-0.299318307035372,7.29834602864233,
97.7436727840662));
#181140=CARTESIAN_POINT('Ctrl Pts',(-3.72798211249406,6.25951141932153,
97.9023402493526));
#181141=CARTESIAN_POINT('Ctrl Pts',(-7.16726359359828,2.88320234719056,
98.1138968697345));
#181142=CARTESIAN_POINT('Ctrl Pts',(-7.40368502527283,-3.69526160713197,
98.3783426452119));
#181143=CARTESIAN_POINT('Ctrl Pts',(-2.00393381935232,-7.46117725044532,
98.6427884206892));
#181144=CARTESIAN_POINT('Ctrl Pts',(2.76117551751445,-6.74170561393421,
98.8543450410712));
#181145=CARTESIAN_POINT('Ctrl Pts',(5.65332152640388,-4.62673929743301,
99.0130125063575));
#181146=CARTESIAN_POINT('Ctrl Pts',(7.17439520364235,-1.34694727795331,
99.1716799716442));
#181147=CARTESIAN_POINT('Ctrl Pts',(6.94703914831595,2.23909199201735,99.3303474369303));
#181148=CARTESIAN_POINT('Ctrl Pts',(5.03003528944799,5.29274464953559,99.4890207192591));
#181149=CARTESIAN_POINT('Ctrl Pts',(2.93567476420474,6.46407674877753,99.5948048464922));
#181150=CARTESIAN_POINT('Ctrl Pts',(1.81148773798651,6.7650987574823,99.6476998186297));
#181151=CARTESIAN_POINT('Ctrl Pts',(-5.59319257183209,4.82318409121508,
-0.216170757716313));
#181152=CARTESIAN_POINT('Ctrl Pts',(-6.39483282223799,3.89356867920839,
-0.16326603689069));
#181153=CARTESIAN_POINT('Ctrl Pts',(-7.52577891557862,1.62945095308381,
-0.057472160969592));
#181154=CARTESIAN_POINT('Ctrl Pts',(-7.38490913059102,-2.17042384913742,
0.101210870046983));
#181155=CARTESIAN_POINT('Ctrl Pts',(-5.45514273541142,-5.43154102245448,
0.259878335333412));
#181156=CARTESIAN_POINT('Ctrl Pts',(-2.18287509717614,-7.38815633597361,
0.41854580061984));
#181157=CARTESIAN_POINT('Ctrl Pts',(1.59344116692286,-7.51571166761254,
0.577213265906269));
#181158=CARTESIAN_POINT('Ctrl Pts',(6.17446001743441,-5.31529267069683,
0.788769886288175));
#181159=CARTESIAN_POINT('Ctrl Pts',(8.64709586414073,1.1719534463109,1.05321566176556));
#181160=CARTESIAN_POINT('Ctrl Pts',(4.53730628273561,6.7665709570828,1.31766143724294));
#181161=CARTESIAN_POINT('Ctrl Pts',(-0.464471910629743,7.66905552806737,
1.52921805762484));
#181162=CARTESIAN_POINT('Ctrl Pts',(-4.0699281104299,6.54009937284872,1.68788552291128));
#181163=CARTESIAN_POINT('Ctrl Pts',(-6.70494269659998,3.7850714469408,1.8465529881977));
#181164=CARTESIAN_POINT('Ctrl Pts',(-7.69429901191945,0.124358320332814,
2.00522045348413));
#181165=CARTESIAN_POINT('Ctrl Pts',(-6.82439171170274,-3.5687316022377,
2.16388791877056));
#181166=CARTESIAN_POINT('Ctrl Pts',(-4.27550416845679,-6.40371138085426,
2.32255538405699));
#181167=CARTESIAN_POINT('Ctrl Pts',(-0.716080791044483,-7.65360327218264,
2.48122284934342));
#181168=CARTESIAN_POINT('Ctrl Pts',(4.32866351767188,-6.90168043806902,
2.69277946972532));
#181169=CARTESIAN_POINT('Ctrl Pts',(7.72837761508381,-2.55255697681545,
2.90433609010723));
#181170=CARTESIAN_POINT('Ctrl Pts',(7.26456296350423,2.50129446334141,3.11589271048913));
#181171=CARTESIAN_POINT('Ctrl Pts',(4.51872136302912,6.76932144397021,3.32744933087104));
#181172=CARTESIAN_POINT('Ctrl Pts',(-0.837817077112605,8.10371735557139,
3.53900595125293));
#181173=CARTESIAN_POINT('Ctrl Pts',(-5.27618675114756,5.59028060557585,
3.75056257163485));
#181174=CARTESIAN_POINT('Ctrl Pts',(-7.3115171074744,2.41439254628121,3.90923003692127));
#181175=CARTESIAN_POINT('Ctrl Pts',(-7.57501656271908,-1.38960755105337,
4.0678975022077));
#181176=CARTESIAN_POINT('Ctrl Pts',(-5.98646912787849,-4.83395815802925,
4.22656496749413));
#181177=CARTESIAN_POINT('Ctrl Pts',(-2.953995989762,-7.11237001473912,4.38523243278056));
#181178=CARTESIAN_POINT('Ctrl Pts',(0.820160810533175,-7.65603515901766,
4.54389989806699));
#181179=CARTESIAN_POINT('Ctrl Pts',(4.35351193758964,-6.33532798549869,
4.70256736335343));
#181180=CARTESIAN_POINT('Ctrl Pts',(7.74543080566278,-2.52594026085192,
4.91412398373532));
#181181=CARTESIAN_POINT('Ctrl Pts',(7.56925871627352,2.99146858071628,5.12568060411723));
#181182=CARTESIAN_POINT('Ctrl Pts',(3.9753421002422,6.57473904852535,5.33723722449913));
#181183=CARTESIAN_POINT('Ctrl Pts',(-0.867401018491525,8.09260012782741,
5.54879384488104));
#181184=CARTESIAN_POINT('Ctrl Pts',(-5.83511030797489,5.68538137793315,
5.76035046526294));
#181185=CARTESIAN_POINT('Ctrl Pts',(-7.63267504629624,0.911985347858353,
5.97190708564485));
#181186=CARTESIAN_POINT('Ctrl Pts',(-7.1607183781963,-2.83048621457686,
6.13057455093128));
#181187=CARTESIAN_POINT('Ctrl Pts',(-4.92592076406795,-5.92006782319774,
6.28924201621771));
#181188=CARTESIAN_POINT('Ctrl Pts',(-1.49950799410512,-7.54694885824143,
6.44790948150413));
#181189=CARTESIAN_POINT('Ctrl Pts',(2.28858287895152,-7.3535220687151,6.60657694679056));
#181190=CARTESIAN_POINT('Ctrl Pts',(5.53474515659174,-5.35295581336359,
6.765244412077));
#181191=CARTESIAN_POINT('Ctrl Pts',(7.40155992801486,-2.07517621088562,
6.92391187736342));
#181192=CARTESIAN_POINT('Ctrl Pts',(7.56535131915662,3.02283526489178,7.13546849774533));
#181193=CARTESIAN_POINT('Ctrl Pts',(3.89522963664692,7.14631006586288,7.34702511812723));
#181194=CARTESIAN_POINT('Ctrl Pts',(-1.1599338351539,7.59507023368757,7.55858173850914));
#181195=CARTESIAN_POINT('Ctrl Pts',(-5.85071201799335,5.65789098181395,
7.77013835889103));
#181196=CARTESIAN_POINT('Ctrl Pts',(-8.12274874292138,0.626918240888216,
7.98169497927295));
#181197=CARTESIAN_POINT('Ctrl Pts',(-6.44475867260803,-4.1898128031289,
8.19325159965485));
#181198=CARTESIAN_POINT('Ctrl Pts',(-3.68468373269764,-6.76096484830223,
8.35191906494128));
#181199=CARTESIAN_POINT('Ctrl Pts',(0.0106361900308246,-7.70141449849661,
8.51058653022771));
#181200=CARTESIAN_POINT('Ctrl Pts',(3.68378227475696,-6.75534673041355,
8.66925399551413));
#181201=CARTESIAN_POINT('Ctrl Pts',(6.46840800132986,-4.17990386666028,
8.82792146080057));
#181202=CARTESIAN_POINT('Ctrl Pts',(7.6791481523861,-0.564113059316087,
8.98658892608699));
#181203=CARTESIAN_POINT('Ctrl Pts',(7.01253009361185,3.14862944145831,9.14525639137342));
#181204=CARTESIAN_POINT('Ctrl Pts',(3.87213373250231,7.16789048318619,9.35681301175533));
#181205=CARTESIAN_POINT('Ctrl Pts',(-1.58763536387134,7.98260455184212,
9.56836963213724));
#181206=CARTESIAN_POINT('Ctrl Pts',(-5.75656887614772,5.08846274729946,
9.77992625251913));
#181207=CARTESIAN_POINT('Ctrl Pts',(-8.11711560843863,0.595815138232739,
9.99148287290104));
#181208=CARTESIAN_POINT('Ctrl Pts',(-6.63840932843439,-4.72266822987694,
10.2030394932829));
#181209=CARTESIAN_POINT('Ctrl Pts',(-2.26407620738462,-7.34597880480092,
10.4145961136648));
#181210=CARTESIAN_POINT('Ctrl Pts',(1.5024152175209,-7.5518400674371,10.5732635789513));
#181211=CARTESIAN_POINT('Ctrl Pts',(4.94225399493611,-5.90643918581452,
10.7319310442377));
#181212=CARTESIAN_POINT('Ctrl Pts',(7.15642684923409,-2.82675008578538,
10.8905985095241));
#181213=CARTESIAN_POINT('Ctrl Pts',(7.64448494621918,0.934745052522767,
11.0492659748105));
#181214=CARTESIAN_POINT('Ctrl Pts',(6.25756902944692,4.48668805821105,11.207933440097));
#181215=CARTESIAN_POINT('Ctrl Pts',(3.36707696541851,6.91029944230909,11.3666009053834));
#181216=CARTESIAN_POINT('Ctrl Pts',(-1.61919470933465,7.98437737801743,
11.5781575257653));
#181217=CARTESIAN_POINT('Ctrl Pts',(-6.33324680367213,5.11200023508237,
11.7897141461472));
#181218=CARTESIAN_POINT('Ctrl Pts',(-7.68001396564619,0.218915152436606,
12.0012707665291));
#181219=CARTESIAN_POINT('Ctrl Pts',(-6.61415721494119,-4.74294062958273,
12.212827386911));
#181220=CARTESIAN_POINT('Ctrl Pts',(-2.0713778637849,-7.87917935871215,
12.4243840072929));
#181221=CARTESIAN_POINT('Ctrl Pts',(2.96798007047616,-7.0908772359057,12.6359406276748));
#181222=CARTESIAN_POINT('Ctrl Pts',(5.99183446497284,-4.83585149010497,
12.7946080929613));
#181223=CARTESIAN_POINT('Ctrl Pts',(7.57882695606709,-1.3686783318874,12.9532755582477));
#181224=CARTESIAN_POINT('Ctrl Pts',(7.30582649194216,2.4145104194355,13.1119430235341));
#181225=CARTESIAN_POINT('Ctrl Pts',(5.27067639815129,5.61532445297314,13.2706104888206));
#181226=CARTESIAN_POINT('Ctrl Pts',(1.93014946400685,7.45399644060694,13.429277954107));
#181227=CARTESIAN_POINT('Ctrl Pts',(-1.84195274867956,7.46301921108751,
13.5879454193934));
#181228=CARTESIAN_POINT('Ctrl Pts',(-6.35861431108908,5.09314221911649,
13.7995020397753));
#181229=CARTESIAN_POINT('Ctrl Pts',(-8.13787515437763,-0.132474342680147,
14.0110586601572));
#181230=CARTESIAN_POINT('Ctrl Pts',(-6.03707487698749,-4.75229053048462,
14.2226152805391));
#181231=CARTESIAN_POINT('Ctrl Pts',(-2.03976877603939,-7.87920711873978,
14.434171900921));
#181232=CARTESIAN_POINT('Ctrl Pts',(3.45754367989726,-7.37681945847504,
14.6457285213029));
#181233=CARTESIAN_POINT('Ctrl Pts',(6.82178922381607,-3.54297014653757,
14.8572851416848));
#181234=CARTESIAN_POINT('Ctrl Pts',(7.69881298645689,0.125771576874462,
15.0159526069713));
#181235=CARTESIAN_POINT('Ctrl Pts',(6.69600416270939,3.8046585469876,15.1746200722577));
#181236=CARTESIAN_POINT('Ctrl Pts',(4.06260417774054,6.53453966174601,15.3332875375441));
#181237=CARTESIAN_POINT('Ctrl Pts',(0.449312806741529,7.6883038706782,15.4919550028306));
#181238=CARTESIAN_POINT('Ctrl Pts',(-3.29357765252681,6.95987687655195,
15.650622468117));
#181239=CARTESIAN_POINT('Ctrl Pts',(-6.19563100519067,4.55012111058039,
15.8092899334034));
#181240=CARTESIAN_POINT('Ctrl Pts',(-8.14527086117322,-0.163206064397509,
16.0208465537853));
#181241=CARTESIAN_POINT('Ctrl Pts',(-6.16350136729878,-5.31543153234161,
16.2324031741672));
#181242=CARTESIAN_POINT('Ctrl Pts',(-1.59068667743553,-7.5166651016735,
16.4439597945491));
#181243=CARTESIAN_POINT('Ctrl Pts',(3.48183136358408,-7.35658968784228,
16.655516414931));
#181244=CARTESIAN_POINT('Ctrl Pts',(7.38087841990553,-3.44887044869859,
16.867073035313));
#181245=CARTESIAN_POINT('Ctrl Pts',(7.50774982071213,1.65019341382345,17.0786296556948));
#181246=CARTESIAN_POINT('Ctrl Pts',(5.83067758909786,5.02898983315523,17.2372971209813));
#181247=CARTESIAN_POINT('Ctrl Pts',(2.70374388530774,7.21121816400311,17.3959645862677));
#181248=CARTESIAN_POINT('Ctrl Pts',(-1.06717815138028,7.62011102866245,
17.5546320515542));
#181249=CARTESIAN_POINT('Ctrl Pts',(-4.58069911423817,6.19104950965544,
17.7132995168405));
#181250=CARTESIAN_POINT('Ctrl Pts',(-6.98785921309585,3.23378470339919,
17.871966982127));
#181251=CARTESIAN_POINT('Ctrl Pts',(-7.67223110931155,-0.475726264506312,
18.0306344474134));
#181252=CARTESIAN_POINT('Ctrl Pts',(-6.1494909136111,-5.34376600580041,
18.2421910677953));
#181253=CARTESIAN_POINT('Ctrl Pts',(-1.326969535103,-8.03005064321598,18.4537476881773));
#181254=CARTESIAN_POINT('Ctrl Pts',(3.59437202768935,-6.7905101489543,18.6653043085591));
#181255=CARTESIAN_POINT('Ctrl Pts',(7.38656617696681,-3.4177772883843,18.8768609289411));
#181256=CARTESIAN_POINT('Ctrl Pts',(7.87673918194969,2.08063775820587,19.0884175493229));
#181257=CARTESIAN_POINT('Ctrl Pts',(4.70732090140145,6.07705320074283,19.2999741697049));
#181258=CARTESIAN_POINT('Ctrl Pts',(1.25493822191392,7.59688554271855,19.4586416349913));
#181259=CARTESIAN_POINT('Ctrl Pts',(-2.54405960561978,7.26908929159913,
19.6173091002777));
#181260=CARTESIAN_POINT('Ctrl Pts',(-5.70139272614777,5.16711546979122,
19.7759765655641));
#181261=CARTESIAN_POINT('Ctrl Pts',(-7.48356218900576,1.81884451492439,
19.9346440308506));
#181262=CARTESIAN_POINT('Ctrl Pts',(-7.43717394831114,-1.99398684863986,
20.093311496137));
#181263=CARTESIAN_POINT('Ctrl Pts',(-5.58606117657983,-5.28065963729316,
20.2519789614235));
#181264=CARTESIAN_POINT('Ctrl Pts',(-1.29805898466894,-8.04283012960326,
20.4635355818053));
#181265=CARTESIAN_POINT('Ctrl Pts',(4.12576992068009,-7.01573831049282,
20.6750922021873));
#181266=CARTESIAN_POINT('Ctrl Pts',(7.11030466256198,-2.91103176932789,
20.8866488225691));
#181267=CARTESIAN_POINT('Ctrl Pts',(7.86118577672066,2.10815551219311,21.098205442951));
#181268=CARTESIAN_POINT('Ctrl Pts',(4.71486206491794,6.64395584950197,21.3097620633329));
#181269=CARTESIAN_POINT('Ctrl Pts',(-0.279056488753504,7.68189905879491,
21.5213186837149));
#181270=CARTESIAN_POINT('Ctrl Pts',(-3.90355943701511,6.63699959406936,
21.6799861490013));
#181271=CARTESIAN_POINT('Ctrl Pts',(-6.61047280658732,3.951398192989,21.8386536142877));
#181272=CARTESIAN_POINT('Ctrl Pts',(-7.68803961380581,0.314655672885429,
21.9973210795742));
#181273=CARTESIAN_POINT('Ctrl Pts',(-6.9112678087856,-3.39798111846303,
22.1559885448605));
#181274=CARTESIAN_POINT('Ctrl Pts',(-4.4328726330734,-6.29580654951658,
22.314656010147));
#181275=CARTESIAN_POINT('Ctrl Pts',(-0.905880310080676,-7.63340202905871,
22.4733234754334));
#181276=CARTESIAN_POINT('Ctrl Pts',(4.15615531497542,-7.00702837293636,
22.6848800958154));
#181277=CARTESIAN_POINT('Ctrl Pts',(7.66261695313574,-2.743512877539,22.8964367161972));
#181278=CARTESIAN_POINT('Ctrl Pts',(7.32441022213643,2.32024853288402,23.1079933365791));
#181279=CARTESIAN_POINT('Ctrl Pts',(4.68529006477581,6.65511972008154,23.319549956961));
#181280=CARTESIAN_POINT('Ctrl Pts',(-0.63646542886217,8.12200624102177,
23.5311065773429));
#181281=CARTESIAN_POINT('Ctrl Pts',(-5.13584783248266,5.71948535403429,
23.7426631977248));
#181282=CARTESIAN_POINT('Ctrl Pts',(-7.24935302054271,2.59507623655552,
23.9013306630113));
#181283=CARTESIAN_POINT('Ctrl Pts',(-7.60716689857828,-1.20121196437697,
24.0599981282977));
#181284=CARTESIAN_POINT('Ctrl Pts',(-6.1045754362536,-4.68392143817716,
24.2186655935842));
#181285=CARTESIAN_POINT('Ctrl Pts',(-3.12957351412315,-7.03687913963897,
24.3773330588706));
#181286=CARTESIAN_POINT('Ctrl Pts',(0.629931035558008,-7.67402937057367,
24.536000524157));
#181287=CARTESIAN_POINT('Ctrl Pts',(4.19496609421918,-6.44140552533228,
24.6946679894434));
#181288=CARTESIAN_POINT('Ctrl Pts',(7.68036706207295,-2.71735816799305,
24.9062246098253));
#181289=CARTESIAN_POINT('Ctrl Pts',(7.6411584945879,2.80272337919616,25.1177812302072));
#181290=CARTESIAN_POINT('Ctrl Pts',(4.13726405907001,6.47407016196261,25.3293378505891));
#181291=CARTESIAN_POINT('Ctrl Pts',(-0.666323612245312,8.11163203821956,
25.540894470971));
#181292=CARTESIAN_POINT('Ctrl Pts',(-5.69223613777299,5.82842357530445,
25.7524510913529));
#181293=CARTESIAN_POINT('Ctrl Pts',(-7.60769475643336,1.10110225064071,
25.9640077117349));
#181294=CARTESIAN_POINT('Ctrl Pts',(-7.22874935141058,-2.65192811072765,
26.1226751770213));
#181295=CARTESIAN_POINT('Ctrl Pts',(-5.0713049575923,-5.7960128047898,26.2813426423077));
#181296=CARTESIAN_POINT('Ctrl Pts',(-1.68631677165908,-7.50741613616482,
26.4400101075941));
#181297=CARTESIAN_POINT('Ctrl Pts',(2.10540739109427,-7.40804684945452,
26.5986775728806));
#181298=CARTESIAN_POINT('Ctrl Pts',(5.40021230923117,-5.48864709242768,
26.757345038167));
#181299=CARTESIAN_POINT('Ctrl Pts',(7.3477873030896,-2.2582000402942,26.9160125034534));
#181300=CARTESIAN_POINT('Ctrl Pts',(7.63803066288575,2.83417734345448,27.1275691238354));
#181301=CARTESIAN_POINT('Ctrl Pts',(4.07135925439712,7.04745310742402,27.3391257442172));
#181302=CARTESIAN_POINT('Ctrl Pts',(-0.971112084453145,7.62151426397118,
27.5506823645992));
#181303=CARTESIAN_POINT('Ctrl Pts',(-5.70851519721377,5.80132878941409,
27.7622389849811));
#181304=CARTESIAN_POINT('Ctrl Pts',(-8.10469122370494,0.828283640870579,
27.9737956053629));
#181305=CARTESIAN_POINT('Ctrl Pts',(-6.54674052494879,-4.02860201216538,
28.1853522257449));
#181306=CARTESIAN_POINT('Ctrl Pts',(-3.85131619862713,-6.66745104430312,
28.3440196910312));
#181307=CARTESIAN_POINT('Ctrl Pts',(-0.180470506885619,-7.69930703390452,
28.5026871563177));
#181308=CARTESIAN_POINT('Ctrl Pts',(3.51502034574916,-6.84467627173819,
28.6613546216041));
#181309=CARTESIAN_POINT('Ctrl Pts',(6.36269585437578,-4.33912432074682,
28.8200220868905));
#181310=CARTESIAN_POINT('Ctrl Pts',(7.66278567710082,-0.754490262896438,
28.978689552177));
#181311=CARTESIAN_POINT('Ctrl Pts',(7.08850112525183,2.97365052935496,29.1373570174634));
#181312=CARTESIAN_POINT('Ctrl Pts',(4.04880595981722,7.06959998310242,29.3489136378453));
#181313=CARTESIAN_POINT('Ctrl Pts',(-1.38906561400548,8.01954226871414,
29.5604702582273));
#181314=CARTESIAN_POINT('Ctrl Pts',(-5.62853087442155,5.22973981687144,
29.7720268786091));
#181315=CARTESIAN_POINT('Ctrl Pts',(-8.09983161825924,0.797050334391309,
29.9835834989911));
#181316=CARTESIAN_POINT('Ctrl Pts',(-6.75355386327359,-4.55648810348452,
30.1951401193729));
#181317=CARTESIAN_POINT('Ctrl Pts',(-2.44566267765865,-7.28753591692948,
30.4066967397549));
#181318=CARTESIAN_POINT('Ctrl Pts',(1.31456072747546,-7.58679576525994,
30.5653642050413));
#181319=CARTESIAN_POINT('Ctrl Pts',(4.79416941126681,-6.02725792232762,
30.7240316703277));
#181320=CARTESIAN_POINT('Ctrl Pts',(7.08408009972356,-3.00345974446586,
30.8826991356141));
#181321=CARTESIAN_POINT('Ctrl Pts',(7.66532591117842,0.744766461116509,
31.0413666009006));
#181322=CARTESIAN_POINT('Ctrl Pts',(6.36697520326575,4.33003079099741,31.200034066187));
#181323=CARTESIAN_POINT('Ctrl Pts',(3.53751282642449,6.82462077161154,31.3587015314734));
#181324=CARTESIAN_POINT('Ctrl Pts',(-1.42057125080021,8.02209766474667,
31.5702581518554));
#181325=CARTESIAN_POINT('Ctrl Pts',(-6.20444717254293,5.26757978229367,
31.7818147722372));
#181326=CARTESIAN_POINT('Ctrl Pts',(-7.6722169880436,0.409420132458434,
31.9933713926192));
#181327=CARTESIAN_POINT('Ctrl Pts',(-6.72981225810521,-4.57735605457585,
32.204928013001));
#181328=CARTESIAN_POINT('Ctrl Pts',(-2.26625454375591,-7.82535391942366,
32.416484633383));
#181329=CARTESIAN_POINT('Ctrl Pts',(2.7911126719703,-7.16234149742921,32.6280412537649));
#181330=CARTESIAN_POINT('Ctrl Pts',(5.86999233399055,-4.98304423910511,
32.7867087190513));
#181331=CARTESIAN_POINT('Ctrl Pts',(7.54253083406379,-1.55631841966368,
32.9453761843377));
#181332=CARTESIAN_POINT('Ctrl Pts',(7.3634907335968,2.23247967788305,33.1040436496241));
#181333=CARTESIAN_POINT('Ctrl Pts',(5.4083925124548,5.48280848082534,33.2627111149106));
#181334=CARTESIAN_POINT('Ctrl Pts',(2.11451911274058,7.4038063732003,33.421378580197));
#181335=CARTESIAN_POINT('Ctrl Pts',(-1.65619771621946,7.50642756564124,
33.5800460454834));
#181336=CARTESIAN_POINT('Ctrl Pts',(-6.23027481297625,5.24935704407002,
33.7916026658653));
#181337=CARTESIAN_POINT('Ctrl Pts',(-8.13865659658314,0.0695002345258844,
34.0031592862473));
#181338=CARTESIAN_POINT('Ctrl Pts',(-6.15313962233573,-4.60102283677544,
34.2147159066291));
#181339=CARTESIAN_POINT('Ctrl Pts',(-2.23465587780572,-7.82616602095135,
34.4262725270111));
#181340=CARTESIAN_POINT('Ctrl Pts',(3.27343014702295,-7.46034373832027,
34.6378291473929));
#181341=CARTESIAN_POINT('Ctrl Pts',(6.73177318153571,-3.71115554858403,
34.8493857677749));
#181342=CARTESIAN_POINT('Ctrl Pts',(7.6995633002137,-0.0653060180177375,
35.0080532330613));
#181343=CARTESIAN_POINT('Ctrl Pts',(6.78835140860278,3.63733192869553,35.1667206983477));
#181344=CARTESIAN_POINT('Ctrl Pts',(4.22350174583183,6.43171783420898,35.3253881636342));
#181345=CARTESIAN_POINT('Ctrl Pts',(0.639952549815799,7.67478723745301,
35.4840556289205));
#181346=CARTESIAN_POINT('Ctrl Pts',(-3.1198606489942,7.03946087572367,35.6427230942071));
#181347=CARTESIAN_POINT('Ctrl Pts',(-6.08081625493652,4.70245886182211,
35.8013905594934));
#181348=CARTESIAN_POINT('Ctrl Pts',(-8.14681260514703,0.0389614931793878,
36.0129471798754));
#181349=CARTESIAN_POINT('Ctrl Pts',(-6.29350100288451,-5.16085328278152,
36.2245038002573));
#181350=CARTESIAN_POINT('Ctrl Pts',(-1.77671591673179,-7.47487919017552,
36.4360604206391));
#181351=CARTESIAN_POINT('Ctrl Pts',(3.29821233503487,-7.44072287299623,
36.6476170410211));
#181352=CARTESIAN_POINT('Ctrl Pts',(7.29302522118576,-3.63095810282656,
36.859173661403));
#181353=CARTESIAN_POINT('Ctrl Pts',(7.54638607283336,1.46338747882308,37.0707302817849));
#181354=CARTESIAN_POINT('Ctrl Pts',(5.95367192282226,4.88275849550071,37.2293977470713));
#181355=CARTESIAN_POINT('Ctrl Pts',(2.88185101501516,7.14190682755269,37.3880652123578));
#181356=CARTESIAN_POINT('Ctrl Pts',(-0.877763597696466,7.64424570265017,
37.5467326776441));
#181357=CARTESIAN_POINT('Ctrl Pts',(-4.42566351935687,6.30280896264681,
37.7054001429306));
#181358=CARTESIAN_POINT('Ctrl Pts',(-6.90546418370667,3.40618618069116,
37.864067608217));
#181359=CARTESIAN_POINT('Ctrl Pts',(-7.68167340742512,-0.285200517333806,
38.0227350735034));
#181360=CARTESIAN_POINT('Ctrl Pts',(-6.28019795679177,-5.18952668794002,
38.2342916938854));
#181361=CARTESIAN_POINT('Ctrl Pts',(-1.52581916088684,-7.994650546958,38.4458483142672));
#181362=CARTESIAN_POINT('Ctrl Pts',(3.42476508210843,-6.87761023094924,
38.6574049346492));
#181363=CARTESIAN_POINT('Ctrl Pts',(7.29948277468298,-3.60001565299542,
38.8689615550311));
#181364=CARTESIAN_POINT('Ctrl Pts',(7.92594289136418,1.88454315529457,39.0805181754129));
#181365=CARTESIAN_POINT('Ctrl Pts',(4.85666785056708,5.95837419626339,39.2920747957949));
#181366=CARTESIAN_POINT('Ctrl Pts',(1.44306143912829,7.56340621498592,39.4507422610813));
#181367=CARTESIAN_POINT('Ctrl Pts',(-2.36290057313157,7.32997948753485,
39.6094097263677));
#181368=CARTESIAN_POINT('Ctrl Pts',(-5.57142002007046,5.30699917617148,
39.7680771916542));
#181369=CARTESIAN_POINT('Ctrl Pts',(-7.43612494637858,2.00398208276263,
39.9267446569406));
#181370=CARTESIAN_POINT('Ctrl Pts',(-7.48436284551581,-1.80882632849291,
40.085412122227));
#181371=CARTESIAN_POINT('Ctrl Pts',(-5.71537578330039,-5.14042073463766,
40.2440795875134));
#181372=CARTESIAN_POINT('Ctrl Pts',(-1.49723462352733,-8.00814348669179,
40.4556362078954));
#181373=CARTESIAN_POINT('Ctrl Pts',(3.95041052209858,-7.11595518441463,
40.6671928282772));
#181374=CARTESIAN_POINT('Ctrl Pts',(7.03588074341516,-3.08657099722778,
40.8787494486592));
#181375=CARTESIAN_POINT('Ctrl Pts',(7.91107710269774,1.91243837936691,41.090306069041));
#181376=CARTESIAN_POINT('Ctrl Pts',(4.87827385282309,6.52491515946354,41.301862689423));
#181377=CARTESIAN_POINT('Ctrl Pts',(-0.0883513982737931,7.68645820283012,
41.5134193098049));
#181378=CARTESIAN_POINT('Ctrl Pts',(-3.7376665088871,6.73181914183104,41.6720867750913));
#181379=CARTESIAN_POINT('Ctrl Pts',(-6.51038707084204,4.11421421343349,
41.8307542403778));
#181380=CARTESIAN_POINT('Ctrl Pts',(-7.67786445320275,0.505330321808945,
41.9894217056641));
#181381=CARTESIAN_POINT('Ctrl Pts',(-6.99345745017656,-3.22543815609603,
42.1480891709506));
#181382=CARTESIAN_POINT('Ctrl Pts',(-4.58773224978883,-6.18387036524922,
42.306756636237));
#181383=CARTESIAN_POINT('Ctrl Pts',(-1.09501713052869,-7.60857300400148,
42.4654241015234));
#181384=CARTESIAN_POINT('Ctrl Pts',(3.98100268924364,-7.108001914039,42.6769807219053));
#181385=CARTESIAN_POINT('Ctrl Pts',(7.59217979307386,-2.93280880187554,
42.8885373422872));
#181386=CARTESIAN_POINT('Ctrl Pts',(7.37972972077339,2.13778567814032,43.1000939626691));
#181387=CARTESIAN_POINT('Ctrl Pts',(4.8489879792647,6.53680939419379,43.311650583051));
#181388=CARTESIAN_POINT('Ctrl Pts',(-0.43472943651037,8.13529863838765,
43.523207203433));
#181389=CARTESIAN_POINT('Ctrl Pts',(-4.99234272356322,5.84516550749184,
43.7347638238148));
#181390=CARTESIAN_POINT('Ctrl Pts',(-7.18272642731095,2.77416310735713,
43.8934312891013));
#181391=CARTESIAN_POINT('Ctrl Pts',(-7.63463148404488,-1.0120773352815,
44.0520987543877));
#181392=CARTESIAN_POINT('Ctrl Pts',(-6.21892287865747,-4.53099983435654,
44.2107662196742));
#181393=CARTESIAN_POINT('Ctrl Pts',(-3.30322346942185,-6.95705491712383,
44.3694336849606));
#181394=CARTESIAN_POINT('Ctrl Pts',(0.439313195026434,-7.6872975674912,
44.528101150247));
#181395=CARTESIAN_POINT('Ctrl Pts',(4.03383690204582,-6.54351627557473,
44.6867686155335));
#181396=CARTESIAN_POINT('Ctrl Pts',(7.61057348568299,-2.90710261789513,
44.8983252359153));
#181397=CARTESIAN_POINT('Ctrl Pts',(7.70835253972146,2.61225218709017,45.1098818562973));
#181398=CARTESIAN_POINT('Ctrl Pts',(4.29663824397178,6.36941429430586,45.3214384766791));
#181399=CARTESIAN_POINT('Ctrl Pts',(-0.464836099980491,8.12566864264212,
45.532995097061));
#181400=CARTESIAN_POINT('Ctrl Pts',(-5.54585601130899,5.96787622243531,
45.744551717443));
#181401=CARTESIAN_POINT('Ctrl Pts',(-7.57803000839963,1.28954132789886,
45.9561083378248));
#181402=CARTESIAN_POINT('Ctrl Pts',(-7.29232733490318,-2.4717374329718,
46.1147758031113));
#181403=CARTESIAN_POINT('Ctrl Pts',(-5.21356858587787,-5.66838730039252,
46.2734432683977));
#181404=CARTESIAN_POINT('Ctrl Pts',(-1.87208228136461,-7.4632622167643,
46.4321107336842));
#181405=CARTESIAN_POINT('Ctrl Pts',(1.92092630474857,-7.458005518932,46.5907781989705));
#181406=CARTESIAN_POINT('Ctrl Pts',(5.262370667903,-5.62096573551653,46.7494456642571));
#181407=CARTESIAN_POINT('Ctrl Pts',(7.28945957893753,-2.43981987392297,
46.9081131295434));
#181408=CARTESIAN_POINT('Ctrl Pts',(7.70607428550732,2.64374392443121,47.1196697499254));
#181409=CARTESIAN_POINT('Ctrl Pts',(4.24485140895422,6.94431373400415,47.3312263703072));
#181410=CARTESIAN_POINT('Ctrl Pts',(-0.781539047599859,7.64319687039387,
47.5427829906891));
#181411=CARTESIAN_POINT('Ctrl Pts',(-5.56318172248103,5.94136167142255,
47.754339611071));
#181412=CARTESIAN_POINT('Ctrl Pts',(-8.08088365047604,1.02880295755603,
47.965896231453));
#181413=CARTESIAN_POINT('Ctrl Pts',(-6.64562737011112,-3.86449556348911,
48.1774528518348));
#181414=CARTESIAN_POINT('Ctrl Pts',(-4.01360255146483,-6.57070544212201,
48.3361203171214));
#181415=CARTESIAN_POINT('Ctrl Pts',(-0.375301096671435,-7.69075902680454,
48.4947877824077));
#181416=CARTESIAN_POINT('Ctrl Pts',(3.35132729979093,-6.93300286965634,
48.6534552476943));
#181417=CARTESIAN_POINT('Ctrl Pts',(6.23994166064972,-4.48978335266614,
48.8121227129805));
#181418=CARTESIAN_POINT('Ctrl Pts',(8.13618217215324,0.224578706766124,
49.0236793333626));
#181419=CARTESIAN_POINT('Ctrl Pts',(5.62429464528615,6.67951083364511,49.2881251088398));
#181420=CARTESIAN_POINT('Ctrl Pts',(-2.5847595412482,8.34284628442979,49.6054600394127));
#181421=CARTESIAN_POINT('Ctrl Pts',(-7.40911245697885,3.36713261308933,
49.8699058148902));
#181422=CARTESIAN_POINT('Ctrl Pts',(-7.49433490111638,-1.70715495593281,
50.0814624352719));
#181423=CARTESIAN_POINT('Ctrl Pts',(-5.78340036009558,-5.09230476755583,
50.2401299005585));
#181424=CARTESIAN_POINT('Ctrl Pts',(-2.64334519062654,-7.2175551378715,
50.3987973658448));
#181425=CARTESIAN_POINT('Ctrl Pts',(2.40330882384813,-7.7760867127584,50.6103539862269));
#181426=CARTESIAN_POINT('Ctrl Pts',(7.94480546051037,-3.62041707533747,
50.8747997617041));
#181427=CARTESIAN_POINT('Ctrl Pts',(7.34416496708709,4.73282184451775,51.1921346922771));
#181428=CARTESIAN_POINT('Ctrl Pts',(1.24296098202915,8.04250887686602,51.4565804677543));
#181429=CARTESIAN_POINT('Ctrl Pts',(-3.64947415302537,6.75792830578459,
51.6681370881364));
#181430=CARTESIAN_POINT('Ctrl Pts',(-7.42111176510748,3.35217510381507,
51.8796937085182));
#181431=CARTESIAN_POINT('Ctrl Pts',(-7.8555980481714,-2.1507922957559,52.0912503289001));
#181432=CARTESIAN_POINT('Ctrl Pts',(-4.65407611661369,-6.1186429968107,
52.302806949282));
#181433=CARTESIAN_POINT('Ctrl Pts',(-1.18670892066426,-7.60778721220126,
52.4614744145685));
#181434=CARTESIAN_POINT('Ctrl Pts',(2.60834208613747,-7.24614259843243,
52.6201418798549));
#181435=CARTESIAN_POINT('Ctrl Pts',(5.74731330180241,-5.1161820899732,52.7788093451413));
#181436=CARTESIAN_POINT('Ctrl Pts',(7.49936692377579,-1.75216872725107,
52.9374768104277));
#181437=CARTESIAN_POINT('Ctrl Pts',(7.41917818290533,2.0600910566469,53.0961442757142));
#181438=CARTESIAN_POINT('Ctrl Pts',(5.53882487318358,5.33016393210911,53.2548117410006));
#181439=CARTESIAN_POINT('Ctrl Pts',(1.22644870252003,8.05406246753895,53.4663683613825));
#181440=CARTESIAN_POINT('Ctrl Pts',(-4.18805026979504,6.97874443945398,
53.6779249817644));
#181441=CARTESIAN_POINT('Ctrl Pts',(-7.13592590189922,2.84763939769702,
53.8894816021462));
#181442=CARTESIAN_POINT('Ctrl Pts',(-7.84211621237246,-2.17803107982334,
54.1010382225283));
#181443=CARTESIAN_POINT('Ctrl Pts',(-4.65554714393779,-6.68565191717772,
54.31259484291));
#181444=CARTESIAN_POINT('Ctrl Pts',(0.347408463441009,-7.67911140378827,
54.5241514632921));
#181445=CARTESIAN_POINT('Ctrl Pts',(3.96247002766141,-6.60199776048994,
54.6828189285784));
#181446=CARTESIAN_POINT('Ctrl Pts',(6.64537559819868,-3.89241298024765,
54.841486393865));
#181447=CARTESIAN_POINT('Ctrl Pts',(7.69053549766263,-0.246224878623426,
55.0001538591513));
#181448=CARTESIAN_POINT('Ctrl Pts',(6.88075434028287,3.45935216052283,55.1588213244378));
#181449=CARTESIAN_POINT('Ctrl Pts',(4.37666871111325,6.33500679653603,55.3174887897242));
#181450=CARTESIAN_POINT('Ctrl Pts',(0.837912320965971,7.64116146966611,
55.4761562550106));
#181451=CARTESIAN_POINT('Ctrl Pts',(-4.21834852326479,6.96976393111749,
55.6877128753925));
#181452=CARTESIAN_POINT('Ctrl Pts',(-7.6867289255209,2.67521213953418,55.8992694957745));
#181453=CARTESIAN_POINT('Ctrl Pts',(-7.3034715361975,-2.38533893705042,
56.1108261161562));
#181454=CARTESIAN_POINT('Ctrl Pts',(-4.62587847676516,-6.69655208400989,
56.3223827365383));
#181455=CARTESIAN_POINT('Ctrl Pts',(0.708720575099877,-8.1160205008443,
56.53393935692));
#181456=CARTESIAN_POINT('Ctrl Pts',(5.18654399580368,-5.67355330002261,
56.7454959773021));
#181457=CARTESIAN_POINT('Ctrl Pts',(7.27216036735544,-2.53045914511118,
56.9041634425884));
#181458=CARTESIAN_POINT('Ctrl Pts',(7.59617568443146,1.26886302470831,57.0628309078749));
#181459=CARTESIAN_POINT('Ctrl Pts',(6.06264997138618,4.73806253875762,57.2214983731613));
#181460=CARTESIAN_POINT('Ctrl Pts',(3.06682613015959,7.06445156352318,57.3801658384477));
#181461=CARTESIAN_POINT('Ctrl Pts',(-0.698199749115411,7.66811952177836,
57.5388333037342));
#181462=CARTESIAN_POINT('Ctrl Pts',(-4.25212411675666,6.40381809307606,
57.6975007690206));
#181463=CARTESIAN_POINT('Ctrl Pts',(-7.704245566873,2.64890050144179,57.9090573894025));
#181464=CARTESIAN_POINT('Ctrl Pts',(-7.6159135686908,-2.87061352222651,
58.1206140097845));
#181465=CARTESIAN_POINT('Ctrl Pts',(-4.07948538918484,-6.51063263561258,
58.3321706301662));
#181466=CARTESIAN_POINT('Ctrl Pts',(0.738485251746679,-8.10538099120919,
58.5437272505483));
#181467=CARTESIAN_POINT('Ctrl Pts',(5.74387974500619,-5.77753572868652,
58.7552838709301));
#181468=CARTESIAN_POINT('Ctrl Pts',(7.61719255714318,-1.03335532167188,
58.9668404913121));
#181469=CARTESIAN_POINT('Ctrl Pts',(7.20486273246497,2.71615406343716,59.1255079565984));
#181470=CARTESIAN_POINT('Ctrl Pts',(5.01952355070286,5.8409144600932,59.2841754218849));
#181471=CARTESIAN_POINT('Ctrl Pts',(1.61943908007662,7.52212592036633,59.4428428871712));
#181472=CARTESIAN_POINT('Ctrl Pts',(-2.17125061206326,7.38901679425637,
59.6015103524578));
#181473=CARTESIAN_POINT('Ctrl Pts',(-5.44884370019278,5.44037151496626,
59.7601778177441));
#181474=CARTESIAN_POINT('Ctrl Pts',(-7.3675927819281,2.19272029066876,59.9188452830306));
#181475=CARTESIAN_POINT('Ctrl Pts',(-7.61250594188919,-2.90203840533433,
60.1304019034125));
#181476=CARTESIAN_POINT('Ctrl Pts',(-4.00848047484515,-7.08340636717186,
60.3419585237944));
#181477=CARTESIAN_POINT('Ctrl Pts',(1.03889993849945,-7.61257021473515,
60.5535151441763));
#181478=CARTESIAN_POINT('Ctrl Pts',(5.75991703457443,-5.75029714315045,
60.7650717645582));
#181479=CARTESIAN_POINT('Ctrl Pts',(8.111741442813,-0.756124583837398,60.9766283849402));
#181480=CARTESIAN_POINT('Ctrl Pts',(6.51062944899396,4.08670403275333,61.188185005322));
#181481=CARTESIAN_POINT('Ctrl Pts',(3.79182789345968,6.70146111802254,61.3468524706085));
#181482=CARTESIAN_POINT('Ctrl Pts',(0.111944747544373,7.70060820842643,
61.5055199358949));
#181483=CARTESIAN_POINT('Ctrl Pts',(-3.57579413020001,6.81312392624366,
61.6641874011813));
#181484=CARTESIAN_POINT('Ctrl Pts',(-6.40105915789561,4.28232881307684,
61.8228548664678));
#181485=CARTESIAN_POINT('Ctrl Pts',(-7.66919668452351,0.686266787831419,
61.9815223317541));
#181486=CARTESIAN_POINT('Ctrl Pts',(-7.06175694869098,-3.03661562780735,
62.1401897970406));
#181487=CARTESIAN_POINT('Ctrl Pts',(-3.98573098119137,-7.10535165680803,
62.3517464174224));
#181488=CARTESIAN_POINT('Ctrl Pts',(1.46037909659013,-8.00686295461261,
62.5633030378044));
#181489=CARTESIAN_POINT('Ctrl Pts',(5.67484912480221,-5.17944261163483,
62.7748596581863));
#181490=CARTESIAN_POINT('Ctrl Pts',(8.1066040745539,-0.72493576138295,62.9864162785683));
#181491=CARTESIAN_POINT('Ctrl Pts',(6.71273676923672,4.61640971841437,63.1979728989501));
#181492=CARTESIAN_POINT('Ctrl Pts',(2.38071170104819,7.30901207208755,63.409529519332));
#181493=CARTESIAN_POINT('Ctrl Pts',(-1.38202600994047,7.5747966307905,63.5681969846185));
#181494=CARTESIAN_POINT('Ctrl Pts',(-4.8476180726037,5.98435438692876,63.7268644499048));
#181495=CARTESIAN_POINT('Ctrl Pts',(-7.11052832740991,2.9402972980683,63.8855319151914));
#181496=CARTESIAN_POINT('Ctrl Pts',(-7.65839444960578,-0.812953172350435,
64.0441993804778));
#181497=CARTESIAN_POINT('Ctrl Pts',(-6.32818873419878,-4.38652108559234,
64.2028668457641));
#181498=CARTESIAN_POINT('Ctrl Pts',(-3.47663824377446,-6.85583198418356,
64.3615343110507));
#181499=CARTESIAN_POINT('Ctrl Pts',(1.49190622706167,-8.00913787064428,
64.5730909314324));
#181500=CARTESIAN_POINT('Ctrl Pts',(6.25107936682005,-5.21215581400079,
64.7846475518145));
#181501=CARTESIAN_POINT('Ctrl Pts',(7.67555673177271,-0.341126389811259,
64.9962041721963));
#181502=CARTESIAN_POINT('Ctrl Pts',(6.68881039361302,4.63706555894997,65.2077607925782));
#181503=CARTESIAN_POINT('Ctrl Pts',(2.19652445606137,7.84521216636351,65.4193174129601));
#181504=CARTESIAN_POINT('Ctrl Pts',(-2.85474212812762,7.13721885998481,
65.630874033342));
#181505=CARTESIAN_POINT('Ctrl Pts',(-5.91410559916608,4.93060795966368,
65.7895414986284));
#181506=CARTESIAN_POINT('Ctrl Pts',(-7.55608233053341,1.48913337897857,
65.9482089639149));
#181507=CARTESIAN_POINT('Ctrl Pts',(-7.34333158560759,-2.29792134759746,
66.1068764292013));
#181508=CARTESIAN_POINT('Ctrl Pts',(-5.35938506312473,-5.53072238964705,
66.2655438944878));
#181509=CARTESIAN_POINT('Ctrl Pts',(-2.04854652109898,-7.42233097085277,
66.4242113597741));
#181510=CARTESIAN_POINT('Ctrl Pts',(1.72293424745511,-7.49139127614996,
66.5828788250607));
#181511=CARTESIAN_POINT('Ctrl Pts',(6.27674381446943,-5.19370394890329,
66.7944354454424));
#181512=CARTESIAN_POINT('Ctrl Pts',(8.1389528127818,0.00293104366527835,
67.0059920658245));
#181513=CARTESIAN_POINT('Ctrl Pts',(6.1119499756196,4.65559940845542,67.2175486862063));
#181514=CARTESIAN_POINT('Ctrl Pts',(2.16491981425747,7.84574302902793,67.4291053065882));
#181515=CARTESIAN_POINT('Ctrl Pts',(-3.33969252143794,7.43091700152713,
67.6406619269702));
#181516=CARTESIAN_POINT('Ctrl Pts',(-6.764533373353,3.65110037032991,67.852218547352));
#181517=CARTESIAN_POINT('Ctrl Pts',(-7.69983957871388,-0.00321746143493831,
68.0108860126386));
#181518=CARTESIAN_POINT('Ctrl Pts',(-6.75571280339331,-3.69759961654247,
68.1695534779248));
#181519=CARTESIAN_POINT('Ctrl Pts',(-4.16609656796089,-6.46904944194669,
68.3282209432115));
#181520=CARTESIAN_POINT('Ctrl Pts',(-0.571626804665265,-7.68017846162284,
68.4868884084976));
#181521=CARTESIAN_POINT('Ctrl Pts',(3.18238353258899,-7.01141747020483,
68.6455558737843));
#181522=CARTESIAN_POINT('Ctrl Pts',(6.12242415190615,-4.64815750352609,
68.8042233390705));
#181523=CARTESIAN_POINT('Ctrl Pts',(8.14683672427592,0.0335411586319285,
69.0157799594527));
#181524=CARTESIAN_POINT('Ctrl Pts',(6.24732368646782,5.21665680644255,69.2273365798343));
#181525=CARTESIAN_POINT('Ctrl Pts',(1.71012420212608,7.49039475393584,69.4388932002164));
#181526=CARTESIAN_POINT('Ctrl Pts',(-3.3642991156822,7.41107636851257,69.6504498205982));
#181527=CARTESIAN_POINT('Ctrl Pts',(-7.32504948466601,3.56591133772674,
69.8620064409801));
#181528=CARTESIAN_POINT('Ctrl Pts',(-7.53306408138971,-1.53048724891962,
70.073563061362));
#181529=CARTESIAN_POINT('Ctrl Pts',(-5.90998291862105,-4.93554878322507,
70.2322305266485));
#181530=CARTESIAN_POINT('Ctrl Pts',(-2.81817876561956,-7.16727053006921,
70.3908979919348));
#181531=CARTESIAN_POINT('Ctrl Pts',(0.945757442712733,-7.63613149150012,
70.5495654572214));
#181532=CARTESIAN_POINT('Ctrl Pts',(4.48157899088049,-6.26317396810003,
70.7082329225078));
#181533=CARTESIAN_POINT('Ctrl Pts',(6.93550347678732,-3.34459734698479,
70.8669003877941));
#181534=CARTESIAN_POINT('Ctrl Pts',(7.67883112382652,0.353550908897835,
71.0255678530808));
#181535=CARTESIAN_POINT('Ctrl Pts',(6.2337659933061,5.24521068805003,71.2371244734623));
#181536=CARTESIAN_POINT('Ctrl Pts',(1.45461176904061,8.00791271687411,71.4486810938446));
#181537=CARTESIAN_POINT('Ctrl Pts',(-3.48583553055409,6.84685979193482,
71.6602377142262));
#181538=CARTESIAN_POINT('Ctrl Pts',(-7.33123141562007,3.53491264536072,
71.8717943346083));
#181539=CARTESIAN_POINT('Ctrl Pts',(-7.90885786957273,-1.95500404609076,
72.0833509549901));
#181540=CARTESIAN_POINT('Ctrl Pts',(-4.80345003694453,-6.00135929735981,
72.2949075753721));
#181541=CARTESIAN_POINT('Ctrl Pts',(-1.37569510665384,-7.57594897445298,
72.4535750406583));
#181542=CARTESIAN_POINT('Ctrl Pts',(2.42803885084062,-7.30866100903549,
72.6122425059449));
#181543=CARTESIAN_POINT('Ctrl Pts',(5.61842808794537,-5.25720715936825,
72.7709099712313));
#181544=CARTESIAN_POINT('Ctrl Pts',(7.45366455959685,-1.93772625496934,
72.9295774365178));
#181545=CARTESIAN_POINT('Ctrl Pts',(7.46796913860933,1.8753604546235,73.0882449018041));
#181546=CARTESIAN_POINT('Ctrl Pts',(5.66940319632406,5.19108014491588,73.2469123670907));
#181547=CARTESIAN_POINT('Ctrl Pts',(1.42590828560569,8.02115073928762,73.4584689874725));
#181548=CARTESIAN_POINT('Ctrl Pts',(-4.01358126361283,7.08051741895192,
73.6700256078544));
#181549=CARTESIAN_POINT('Ctrl Pts',(-7.06307051358718,3.023834201239,73.8815822282364));
#181550=CARTESIAN_POINT('Ctrl Pts',(-7.89374442100557,-1.98276587007854,
74.0931388486181));
#181551=CARTESIAN_POINT('Ctrl Pts',(-4.82001335312958,-6.56807010445122,
74.3046954690001));
#181552=CARTESIAN_POINT('Ctrl Pts',(0.156752166448748,-7.68536755345788,
74.516252089382));
#181553=CARTESIAN_POINT('Ctrl Pts',(3.79742712466257,-6.69828986554504,
74.6749195546685));
#181554=CARTESIAN_POINT('Ctrl Pts',(6.54674297835105,-4.05611326045006,
74.8335870199548));
#181555=CARTESIAN_POINT('Ctrl Pts',(7.68205750895736,-0.436982522532017,
74.9922544852414));
#181556=CARTESIAN_POINT('Ctrl Pts',(6.96447629814245,3.28754745955083,75.1509219505277));
#181557=CARTESIAN_POINT('Ctrl Pts',(4.53251832293027,6.2244531922321,75.3095894158142));
#181558=CARTESIAN_POINT('Ctrl Pts',(1.02726262670822,7.61801661649528,75.4682568811006));
#181559=CARTESIAN_POINT('Ctrl Pts',(-4.04410144057219,7.07229221396395,
75.6798135014825));
#181560=CARTESIAN_POINT('Ctrl Pts',(-7.61797915470459,2.86512741046386,
75.8913701218644));
#181561=CARTESIAN_POINT('Ctrl Pts',(-7.36041264205738,-2.20337561371838,
76.1029267422464));
#181562=CARTESIAN_POINT('Ctrl Pts',(-4.7906227888216,-6.5797032436827,76.3144833626282));
#181563=CARTESIAN_POINT('Ctrl Pts',(0.507110864105959,-8.13110768547802,
76.5260399830101));
#181564=CARTESIAN_POINT('Ctrl Pts',(5.04416303784523,-5.8005055746086,76.7375966033921));
#181565=CARTESIAN_POINT('Ctrl Pts',(7.2071301648577,-2.71013185597771,76.8962640686785));
#181566=CARTESIAN_POINT('Ctrl Pts',(7.62532235076434,1.07998030219135,77.0549315339649));
#181567=CARTESIAN_POINT('Ctrl Pts',(6.17835378732253,4.58616460395872,77.2135989992513));
#181568=CARTESIAN_POINT('Ctrl Pts',(3.24117958454841,6.98617587145457,77.3722664645377));
#181569=CARTESIAN_POINT('Ctrl Pts',(-0.507707523942078,7.68308355805921,
77.5309339298242));
#181570=CARTESIAN_POINT('Ctrl Pts',(-4.09191004142901,6.50735874885361,
77.6896013951107));
#181571=CARTESIAN_POINT('Ctrl Pts',(-7.63614330666086,2.83925853374987,
77.9011580154925));
#181572=CARTESIAN_POINT('Ctrl Pts',(-7.68480010278568,-2.68074781729478,
78.1127146358744));
#181573=CARTESIAN_POINT('Ctrl Pts',(-4.23978452870737,-6.4073992779146,
78.3242712562563));
#181574=CARTESIAN_POINT('Ctrl Pts',(0.537130386221318,-8.12121003471172,
78.5358278766383));
#181575=CARTESIAN_POINT('Ctrl Pts',(5.59874694676139,-5.91828575243403,
78.74738449702));
#181576=CARTESIAN_POINT('Ctrl Pts',(7.58920534966798,-1.22205066752606,
78.9589411174022));
#181577=CARTESIAN_POINT('Ctrl Pts',(7.27004306836239,2.53653576244122,79.1176085826884));
#181578=CARTESIAN_POINT('Ctrl Pts',(5.1629148048253,5.71456114888126,79.2762760479749));
#181579=CARTESIAN_POINT('Ctrl Pts',(1.80559497116204,7.47962486332303,79.4349435132613));
#181580=CARTESIAN_POINT('Ctrl Pts',(-1.98723048438653,7.44061915488974,
79.5936109785478));
#181581=CARTESIAN_POINT('Ctrl Pts',(-5.3121681640557,5.57390431266812,79.7522784438342));
#181582=CARTESIAN_POINT('Ctrl Pts',(-7.31091386931737,2.37486506329353,
79.9109459091206));
#181583=CARTESIAN_POINT('Ctrl Pts',(-7.68217330443316,-2.71224758124834,
80.1225025295025));
#181584=CARTESIAN_POINT('Ctrl Pts',(-4.18301432417714,-6.98175856381715,
80.3340591498844));
#181585=CARTESIAN_POINT('Ctrl Pts',(0.849681210409256,-7.63600551317016,
80.5456157702664));
#181586=CARTESIAN_POINT('Ctrl Pts',(5.61545519829567,-5.8914535044961,80.7571723906482));
#181587=CARTESIAN_POINT('Ctrl Pts',(8.09048117796806,-0.957177063179817,
80.9687290110302));
#181588=CARTESIAN_POINT('Ctrl Pts',(6.61003247061829,3.92389046875689,81.1802856314119));
#181589=CARTESIAN_POINT('Ctrl Pts',(3.95695083834681,6.60530695372241,81.3389530966986));
#181590=CARTESIAN_POINT('Ctrl Pts',(0.302993692444209,7.69545926040326,
81.4976205619847));
#181591=CARTESIAN_POINT('Ctrl Pts',(-3.40563176525438,6.89975605187724,
81.6562880272715));
#181592=CARTESIAN_POINT('Ctrl Pts',(-6.2928261691851,4.43984653007363,81.8149554925576));
#181593=CARTESIAN_POINT('Ctrl Pts',(-7.64980614255145,0.876359441878015,
81.9736229578442));
#181594=CARTESIAN_POINT('Ctrl Pts',(-7.13493330420416,-2.86044968807139,
82.1322904231306));
#181595=CARTESIAN_POINT('Ctrl Pts',(-4.16081638737094,-7.00426160361813,
82.3438470435126));
#181596=CARTESIAN_POINT('Ctrl Pts',(1.26124658136258,-8.04063545627494,
82.5554036638944));
#181597=CARTESIAN_POINT('Ctrl Pts',(5.54457870540081,-5.31866386756137,
82.7669602842763));
#181598=CARTESIAN_POINT('Ctrl Pts',(8.08611931314516,-0.925870365270548,
82.9785169046583));
#181599=CARTESIAN_POINT('Ctrl Pts',(6.82522171152634,4.44841794460044,83.1900735250401));
#181600=CARTESIAN_POINT('Ctrl Pts',(2.56134496232852,7.24768636582629,83.4016301454221));
#181601=CARTESIAN_POINT('Ctrl Pts',(-1.19363894398475,7.60675791394662,
83.5602976107085));
#181602=CARTESIAN_POINT('Ctrl Pts',(-4.69762923579942,6.1028008298772,83.7189650759949));
#181603=CARTESIAN_POINT('Ctrl Pts',(-7.03537814257748,3.11583306466665,
83.8776325412813));
#181604=CARTESIAN_POINT('Ctrl Pts',(-7.67620897962355,-0.622666931299617,
84.0363000065679));
#181605=CARTESIAN_POINT('Ctrl Pts',(-6.43508761299876,-4.22814229928651,
84.194967471854));
#181606=CARTESIAN_POINT('Ctrl Pts',(-3.64568880986591,-6.76745142391492,
84.3536349371408));
#181607=CARTESIAN_POINT('Ctrl Pts',(1.29270755419318,-8.04369198817716,
84.5651915575224));
#181608=CARTESIAN_POINT('Ctrl Pts',(6.11981976906105,-5.36566561331532,
84.7767481779045));
#181609=CARTESIAN_POINT('Ctrl Pts',(7.66472856868996,-0.531483136886555,
84.9883047982863));
#181610=CARTESIAN_POINT('Ctrl Pts',(6.80181525865428,4.46966113557217,85.1998614186682));
#181611=CARTESIAN_POINT('Ctrl Pts',(2.39051973713001,7.7882917900992,85.4114180390501));
#181612=CARTESIAN_POINT('Ctrl Pts',(-2.67675967323638,7.20585895817874,
85.6229746594321));
#181613=CARTESIAN_POINT('Ctrl Pts',(-5.78993610871133,5.0758427622442,85.7816421247185));
#181614=CARTESIAN_POINT('Ctrl Pts',(-7.51680423226243,1.67617198999052,
85.9403095900049));
#181615=CARTESIAN_POINT('Ctrl Pts',(-7.39809122969079,-2.11499585179245,
86.0989770552914));
#181616=CARTESIAN_POINT('Ctrl Pts',(-5.49497454123724,-5.39603124503018,
86.2576445205777));
#181617=CARTESIAN_POINT('Ctrl Pts',(-2.23209396432371,-7.36921274115597,
86.4163119858643));
#181618=CARTESIAN_POINT('Ctrl Pts',(1.53651183639463,-7.53183756131588,
86.5749794511506));
#181619=CARTESIAN_POINT('Ctrl Pts',(6.14593418003887,-5.34785626919466,
86.7865360715324));
#181620=CARTESIAN_POINT('Ctrl Pts',(8.13651942694822,-0.199030386124499,
86.9980926919146));
#181621=CARTESIAN_POINT('Ctrl Pts',(6.22559236563579,4.50250353175033,87.2096493122962));
#181622=CARTESIAN_POINT('Ctrl Pts',(2.35893799977536,7.78960672902815,87.4212059326784));
#181623=CARTESIAN_POINT('Ctrl Pts',(-3.15427289676359,7.5115002572107,87.63276255306));
#181624=CARTESIAN_POINT('Ctrl Pts',(-6.67185181037829,3.8178317267503,87.8443191734422));
#181625=CARTESIAN_POINT('Ctrl Pts',(-7.697548510231,0.187847870966458,88.0029866387283));
#181626=CARTESIAN_POINT('Ctrl Pts',(-6.84538509645438,-3.52882434918875,
88.161654104015));
#181627=CARTESIAN_POINT('Ctrl Pts',(-4.32533719029197,-6.36367971272943,
88.3203215693013));
#181628=CARTESIAN_POINT('Ctrl Pts',(-0.762027260803349,-7.66362922250155,
88.4789890345877));
#181629=CARTESIAN_POINT('Ctrl Pts',(3.00742183576063,-7.08822642074706,
88.6376564998743));
#181630=CARTESIAN_POINT('Ctrl Pts',(6.00519926153617,-4.79864850793173,
88.7963239651606));
#181631=CARTESIAN_POINT('Ctrl Pts',(8.14516047232624,-0.168625328428629,
89.0078805855426));
#181632=CARTESIAN_POINT('Ctrl Pts',(6.37484650903789,5.06002899852491,89.2194372059244));
#181633=CARTESIAN_POINT('Ctrl Pts',(1.89546479045971,7.4456532006678,89.4309938263063));
#181634=CARTESIAN_POINT('Ctrl Pts',(-3.1793642410478,7.49227632315112,89.6425504466883));
#181635=CARTESIAN_POINT('Ctrl Pts',(-7.23430921602959,3.74657761006007,
89.8541070670701));
#181636=CARTESIAN_POINT('Ctrl Pts',(-7.56872214193795,-1.34309002362748,
90.0656636874521));
#181637=CARTESIAN_POINT('Ctrl Pts',(-6.03063418038231,-4.78737832977405,
90.2243311527385));
#181638=CARTESIAN_POINT('Ctrl Pts',(-2.99516013938188,-7.09513313093194,
90.3829986180249));
#181639=CARTESIAN_POINT('Ctrl Pts',(0.755982743603434,-7.65724829082198,
90.5416660833114));
#181640=CARTESIAN_POINT('Ctrl Pts',(4.32478421550443,-6.37245163932341,
90.7003335485977));
#181641=CARTESIAN_POINT('Ctrl Pts',(6.85037485613197,-3.51566554445393,
90.8590010138843));
#181642=CARTESIAN_POINT('Ctrl Pts',(7.68523972212387,0.162899008310248,
91.0176684791705));
#181643=CARTESIAN_POINT('Ctrl Pts',(6.36200152846888,5.08891050944583,91.2292250995527));
#181644=CARTESIAN_POINT('Ctrl Pts',(1.65287275967981,7.9693521141867,91.4407817199344));
#181645=CARTESIAN_POINT('Ctrl Pts',(-3.31486374127232,6.9312492909561,91.6523383403164));
#181646=CARTESIAN_POINT('Ctrl Pts',(-7.24125844712909,3.71574186153288,
91.8638949606982));
#181647=CARTESIAN_POINT('Ctrl Pts',(-7.95493420564528,-1.75815113252337,
92.0754515810801));
#181648=CARTESIAN_POINT('Ctrl Pts',(-4.95088911273936,-5.88031824543361,
92.2870082014621));
#181649=CARTESIAN_POINT('Ctrl Pts',(-1.56326161937788,-7.53947962379497,
92.4456756667484));
#181650=CARTESIAN_POINT('Ctrl Pts',(2.24593360768367,-7.36666007351953,
92.604343132035));
#181651=CARTESIAN_POINT('Ctrl Pts',(5.48624538689425,-5.39500443448174,
92.7630105973214));
#181652=CARTESIAN_POINT('Ctrl Pts',(7.40328658309064,-2.122085336118,92.9216780626076));
#181653=CARTESIAN_POINT('Ctrl Pts',(7.5122049506152,1.68947230894764,93.0803455278944));
#181654=CARTESIAN_POINT('Ctrl Pts',(5.79646930811482,5.0488007682166,93.2390129931805));
#181655=CARTESIAN_POINT('Ctrl Pts',(1.62450660586534,7.98329831625276,93.4505696135627));
#181656=CARTESIAN_POINT('Ctrl Pts',(-3.83664898069644,7.17793047853722,
93.6621262339443));
#181657=CARTESIAN_POINT('Ctrl Pts',(-6.98586204654806,3.19816663680324,
93.8736828543265));
#181658=CARTESIAN_POINT('Ctrl Pts',(-7.94051430657702,-1.78627946591266,
94.0852394747081));
#181659=CARTESIAN_POINT('Ctrl Pts',(-4.98150970512187,-6.44644348648762,
94.2967960950903));
#181660=CARTESIAN_POINT('Ctrl Pts',(-0.0340013617126023,-7.68689083973357,
94.5083527154719));
#181661=CARTESIAN_POINT('Ctrl Pts',(3.63004607814272,-6.79045680214596,
94.6670201807586));
#181662=CARTESIAN_POINT('Ctrl Pts',(6.44407833726602,-4.21731596128019,
94.8256876460449));
#181663=CARTESIAN_POINT('Ctrl Pts',(7.66884899579075,-0.627470455383009,
94.9843551113314));
#181664=CARTESIAN_POINT('Ctrl Pts',(7.04390880922885,3.11371703253214,95.1430225766178));
#181665=CARTESIAN_POINT('Ctrl Pts',(4.68557750794345,6.11006851004831,95.3016900419042));
#181666=CARTESIAN_POINT('Ctrl Pts',(1.21597883488297,7.59017650355904,95.4603575071907));
#181667=CARTESIAN_POINT('Ctrl Pts',(-3.86736055146191,7.17047381967795,
95.6719141275726));
#181668=CARTESIAN_POINT('Ctrl Pts',(-7.54454431331429,3.05326164501626,
95.8834707479544));
#181669=CARTESIAN_POINT('Ctrl Pts',(-7.41281351694419,-2.02003584276841,
96.0950273683364));
#181670=CARTESIAN_POINT('Ctrl Pts',(-4.95243528627397,-6.45885070399418,
96.3065839887182));
#181671=CARTESIAN_POINT('Ctrl Pts',(0.305225731983484,-8.14109071138399,
96.5181406091002));
#181672=CARTESIAN_POINT('Ctrl Pts',(4.8986302043341,-5.92400513744318,96.729697229482));
#181673=CARTESIAN_POINT('Ctrl Pts',(7.13775755591544,-2.8878837263204,96.8883646947684));
#181674=CARTESIAN_POINT('Ctrl Pts',(7.64958627659066,0.889942290580429,
97.047032160055));
#181675=CARTESIAN_POINT('Ctrl Pts',(6.29060828708289,4.43237517084745,97.2056996253414));
#181676=CARTESIAN_POINT('Ctrl Pts',(3.41286611377566,6.90183796626506,97.3643670906277));
#181677=CARTESIAN_POINT('Ctrl Pts',(-0.315651225729196,7.69659528197362,
97.5230345559143));
#181678=CARTESIAN_POINT('Ctrl Pts',(-3.93140711959932,6.60107452679552,
97.6817020212007));
#181679=CARTESIAN_POINT('Ctrl Pts',(-7.55836006441197,3.04053020989608,
97.8932586415825));
#181680=CARTESIAN_POINT('Ctrl Pts',(-7.80768231748721,-3.89690115260277,
98.1577044170599));
#181681=CARTESIAN_POINT('Ctrl Pts',(-2.11328258743627,-7.86831172410565,
98.4221501925374));
#181682=CARTESIAN_POINT('Ctrl Pts',(2.9118447354237,-7.10958063882229,98.6337068129191));
#181683=CARTESIAN_POINT('Ctrl Pts',(5.96180663630364,-4.87920683779491,
98.7923742782056));
#181684=CARTESIAN_POINT('Ctrl Pts',(7.56588082541761,-1.42044622492244,
98.9510417434921));
#181685=CARTESIAN_POINT('Ctrl Pts',(7.32611861958554,2.3612726491774,99.1097092087785));
#181686=CARTESIAN_POINT('Ctrl Pts',(5.30450950461827,5.58155414095716,99.268382491107));
#181687=CARTESIAN_POINT('Ctrl Pts',(3.0958658922055,6.81680238395213,99.3741666183402));
#181688=CARTESIAN_POINT('Ctrl Pts',(1.91033529005388,7.1342502773344,99.4270615904777));
#181689=CARTESIAN_POINT('Ctrl Pts',(-5.88260427712044,5.07275281512923,
-0.436808985868258));
#181690=CARTESIAN_POINT('Ctrl Pts',(-6.72572424933426,4.0950357906363,-0.383904265042635));
#181691=CARTESIAN_POINT('Ctrl Pts',(-7.91518952170536,1.71376454911315,
-0.278110389121537));
#181692=CARTESIAN_POINT('Ctrl Pts',(-7.76703063229785,-2.28272930962537,
-0.119427358104962));
#181693=CARTESIAN_POINT('Ctrl Pts',(-5.73741125046268,-5.71258830081366,
0.0392401071814675));
#181694=CARTESIAN_POINT('Ctrl Pts',(-2.295824829586,-7.77044585965269,0.197907572467895));
#181695=CARTESIAN_POINT('Ctrl Pts',(1.67589148835794,-7.90460135847237,
0.356575037754326));
#181696=CARTESIAN_POINT('Ctrl Pts',(6.49394857069463,-5.59032484528709,
0.568131658136229));
#181697=CARTESIAN_POINT('Ctrl Pts',(9.09452740305039,1.23259449184249,0.832577433613612));
#181698=CARTESIAN_POINT('Ctrl Pts',(4.77208267061024,7.11669743931879,1.09702320909099));
#181699=CARTESIAN_POINT('Ctrl Pts',(-0.488505341624206,8.0658797764415,
1.30857982947289));
#181700=CARTESIAN_POINT('Ctrl Pts',(-4.28052068697957,6.87850740867851,
1.46724729475932));
#181701=CARTESIAN_POINT('Ctrl Pts',(-7.05188031313337,3.98092452512984,
1.62591476004575));
#181702=CARTESIAN_POINT('Ctrl Pts',(-8.09242944805938,0.130793062761592,
1.78458222533218));
#181703=CARTESIAN_POINT('Ctrl Pts',(-7.17751004572653,-3.75339048631073,
1.94324969061861));
#181704=CARTESIAN_POINT('Ctrl Pts',(-4.49673398246179,-6.73506221619666,
2.10191715590504));
#181705=CARTESIAN_POINT('Ctrl Pts',(-0.753133361682607,-8.04962796580004,
2.26058462119146));
#181706=CARTESIAN_POINT('Ctrl Pts',(4.55264398574624,-7.25879796607905,
2.47214124157337));
#181707=CARTESIAN_POINT('Ctrl Pts',(8.12827139953132,-2.68463536639679,
2.68369786195528));
#181708=CARTESIAN_POINT('Ctrl Pts',(7.64045732588155,2.63072034789073,2.89525448233718));
#181709=CARTESIAN_POINT('Ctrl Pts',(4.75253610096309,7.11959024619432,3.1068111027191));
#181710=CARTESIAN_POINT('Ctrl Pts',(-0.881168716787595,8.52303255506265,
3.31836772310098));
#181711=CARTESIAN_POINT('Ctrl Pts',(-5.54919544617434,5.87954163535837,
3.52992434348291));
#181712=CARTESIAN_POINT('Ctrl Pts',(-7.68984104450024,2.53932181611785,
3.68859180876932));
#181713=CARTESIAN_POINT('Ctrl Pts',(-7.96697490008165,-1.46151079519648,
3.84725927405576));
#181714=CARTESIAN_POINT('Ctrl Pts',(-6.29623036293426,-5.08408437053503,
4.00592673934218));
#181715=CARTESIAN_POINT('Ctrl Pts',(-3.10684626370346,-7.48038937187224,
4.16459420462861));
#181716=CARTESIAN_POINT('Ctrl Pts',(0.862598852087911,-8.05218568712171,
4.32326166991504));
#181717=CARTESIAN_POINT('Ctrl Pts',(4.5787781514147,-6.6631404204,4.48192913520147));
#181718=CARTESIAN_POINT('Ctrl Pts',(8.14620698293027,-2.6566414067469,4.69348575558337));
#181719=CARTESIAN_POINT('Ctrl Pts',(7.96091912215295,3.14625781998219,4.90504237596528));
#181720=CARTESIAN_POINT('Ctrl Pts',(4.18104045973186,6.91493946455292,5.11659899634718));
#181721=CARTESIAN_POINT('Ctrl Pts',(-0.912283436664409,8.51134008235826,
5.32815561672909));
#181722=CARTESIAN_POINT('Ctrl Pts',(-6.13703969858474,5.97956326040377,
5.539712237111));
#181723=CARTESIAN_POINT('Ctrl Pts',(-8.02761683896492,0.959174718031465,
5.7512688574929));
#181724=CARTESIAN_POINT('Ctrl Pts',(-7.53123945186008,-2.97694565283782,
5.90993632277932));
#181725=CARTESIAN_POINT('Ctrl Pts',(-5.18080544935911,-6.22639321824364,
6.06860378806576));
#181726=CARTESIAN_POINT('Ctrl Pts',(-1.57709787861097,-7.93745487260388,
6.22727125335218));
#181727=CARTESIAN_POINT('Ctrl Pts',(2.40700230849641,-7.73401949204719,
6.38593871863862));
#181728=CARTESIAN_POINT('Ctrl Pts',(5.82113258443977,-5.6299368131026,6.54460618392504));
#181729=CARTESIAN_POINT('Ctrl Pts',(7.78454300128656,-2.18255321932097,
6.70327364921147));
#181730=CARTESIAN_POINT('Ctrl Pts',(7.95680954239199,3.17924752811758,6.91483026959338));
#181731=CARTESIAN_POINT('Ctrl Pts',(4.09678269192862,7.51608560212756,7.12638688997527));
#181732=CARTESIAN_POINT('Ctrl Pts',(-1.21995294319321,7.98806621941246,
7.33794351035719));
#181733=CARTESIAN_POINT('Ctrl Pts',(-6.15344869664912,5.95065041327512,
7.54950013073908));
#181734=CARTESIAN_POINT('Ctrl Pts',(-8.54304869417939,0.659357223605445,
7.76105675112099));
#181735=CARTESIAN_POINT('Ctrl Pts',(-6.77823344102648,-4.40660864067956,
7.9726133715029));
#181736=CARTESIAN_POINT('Ctrl Pts',(-3.87534239299458,-7.11080125050227,
8.13128083678932));
#181737=CARTESIAN_POINT('Ctrl Pts',(0.0111865443866004,-8.0999131152557,
8.28994830207576));
#181738=CARTESIAN_POINT('Ctrl Pts',(3.87439429040926,-7.10489243118364,
8.44861576736218));
#181739=CARTESIAN_POINT('Ctrl Pts',(6.80310647024964,-4.39618698054479,
8.60728323264862));
#181740=CARTESIAN_POINT('Ctrl Pts',(8.07649462909002,-0.593302278241658,
8.76595069793504));
#181741=CARTESIAN_POINT('Ctrl Pts',(7.37538337761979,3.31155074342861,8.92461816322147));
#181742=CARTESIAN_POINT('Ctrl Pts',(4.07249172344147,7.53878266710748,9.13617478360338));
#181743=CARTESIAN_POINT('Ctrl Pts',(-1.66978527237763,8.3956529434934,9.34773140398528));
#181744=CARTESIAN_POINT('Ctrl Pts',(-6.0544342533289,5.35175793373891,9.55928802436719));
#181745=CARTESIAN_POINT('Ctrl Pts',(-8.53712408125462,0.626644735636713,
9.77084464474909));
#181746=CARTESIAN_POINT('Ctrl Pts',(-6.98190427152286,-4.96703590511184,
9.98240126513099));
#181747=CARTESIAN_POINT('Ctrl Pts',(-2.3812275744557,-7.72608591279081,
10.1939578855129));
#181748=CARTESIAN_POINT('Ctrl Pts',(1.58015553212113,-7.94259917038461,
10.3526253507993));
#181749=CARTESIAN_POINT('Ctrl Pts',(5.19798381976746,-6.21205938662028,
10.5112928160857));
#181750=CARTESIAN_POINT('Ctrl Pts',(7.52672586390396,-2.97301620343546,
10.6699602813721));
#181751=CARTESIAN_POINT('Ctrl Pts',(8.04003782517391,0.983112090879871,
10.8286277466587));
#181752=CARTESIAN_POINT('Ctrl Pts',(6.5813579390032,4.7188452788587,10.987295211945));
#181753=CARTESIAN_POINT('Ctrl Pts',(3.54130152033665,7.26786294829738,11.1459626772314));
#181754=CARTESIAN_POINT('Ctrl Pts',(-1.70297761078211,8.3975175020094,11.3575192976133));
#181755=CARTESIAN_POINT('Ctrl Pts',(-6.66095155081305,5.37651333497463,
11.5690759179952));
#181756=CARTESIAN_POINT('Ctrl Pts',(-8.07740524261201,0.230242602147388,
11.7806325383771));
#181757=CARTESIAN_POINT('Ctrl Pts',(-6.95639726729727,-4.9883572709839,
11.9921891587591));
#181758=CARTESIAN_POINT('Ctrl Pts',(-2.17855833221247,-8.28687616249494,
12.2037457791409));
#181759=CARTESIAN_POINT('Ctrl Pts',(3.12155393056176,-7.45778448010983,
12.4153023995229));
#181760=CARTESIAN_POINT('Ctrl Pts',(6.30187332167991,-5.08607567035594,
12.5739698648093));
#181761=CARTESIAN_POINT('Ctrl Pts',(7.97098245675322,-1.43949862368597,
12.7326373300957));
#181762=CARTESIAN_POINT('Ctrl Pts',(7.68385597625173,2.53944578844899,12.8913047953821));
#181763=CARTESIAN_POINT('Ctrl Pts',(5.5433999678875,5.90588134062023,13.0499722606686));
#181764=CARTESIAN_POINT('Ctrl Pts',(2.03002227200793,7.83969276580654,13.208639725955));
#181765=CARTESIAN_POINT('Ctrl Pts',(-1.93726194449388,7.84918240656874,
13.3673071912414));
#181766=CARTESIAN_POINT('Ctrl Pts',(-6.68763166341679,5.3566795380949,13.5788638116233));
#181767=CARTESIAN_POINT('Ctrl Pts',(-8.55895780004107,-0.139329037012525,
13.7904204320052));
#181768=CARTESIAN_POINT('Ctrl Pts',(-6.34945463374779,-4.99819096906056,
14.0019770523871));
#181769=CARTESIAN_POINT('Ctrl Pts',(-2.14531367768294,-8.2869053589253,
14.2135336727691));
#181770=CARTESIAN_POINT('Ctrl Pts',(3.63644930484346,-7.75852237173309,
14.425090293151));
#181771=CARTESIAN_POINT('Ctrl Pts',(7.17477289584716,-3.7262960411365,14.6366469135329));
#181772=CARTESIAN_POINT('Ctrl Pts',(8.0971769917171,0.132279446230392,14.7953143788193));
#181773=CARTESIAN_POINT('Ctrl Pts',(7.04247926766235,4.00152513149765,14.9539818441057));
#181774=CARTESIAN_POINT('Ctrl Pts',(4.27281778792673,6.87266001832097,15.1126493093922));
#181775=CARTESIAN_POINT('Ctrl Pts',(0.4725618517077,8.08612409685704,15.2713167746785));
#181776=CARTESIAN_POINT('Ctrl Pts',(-3.46399909120887,7.32000569557098,
15.429984239965));
#181777=CARTESIAN_POINT('Ctrl Pts',(-6.51621502076343,4.78556058329111,
15.5886517052514));
#181778=CARTESIAN_POINT('Ctrl Pts',(-8.56673618704802,-0.171650927470619,
15.8002083256334));
#181779=CARTESIAN_POINT('Ctrl Pts',(-6.48242288096887,-5.59047089212797,
16.0117649460152));
#181780=CARTESIAN_POINT('Ctrl Pts',(-1.67299447177369,-7.90560412660755,
16.2233215663972));
#181781=CARTESIAN_POINT('Ctrl Pts',(3.66199371979118,-7.73724584071417,
16.4348781867791));
#181782=CARTESIAN_POINT('Ctrl Pts',(7.76279135828505,-3.62732728977057,
16.646434807161));
#181783=CARTESIAN_POINT('Ctrl Pts',(7.89622753725514,1.73558029865116,16.8579914275429));
#181784=CARTESIAN_POINT('Ctrl Pts',(6.1323776150447,5.28920767918846,17.0166588928293));
#181785=CARTESIAN_POINT('Ctrl Pts',(2.84364522402627,7.58435227645275,17.1753263581157));
#181786=CARTESIAN_POINT('Ctrl Pts',(-1.12239774996747,8.0144027143087,17.3339938234021));
#181787=CARTESIAN_POINT('Ctrl Pts',(-4.81772080176973,6.511396462331,17.4926612886886));
#181788=CARTESIAN_POINT('Ctrl Pts',(-7.34943593787407,3.40111224192512,
17.651328753975));
#181789=CARTESIAN_POINT('Ctrl Pts',(-8.06921967356995,-0.500342035855678,
17.8099962192614));
#181790=CARTESIAN_POINT('Ctrl Pts',(-6.46768747650548,-5.6202714921642,
18.0215528396434));
#181791=CARTESIAN_POINT('Ctrl Pts',(-1.39563166519913,-8.44555406462666,
18.2331094600252));
#181792=CARTESIAN_POINT('Ctrl Pts',(3.78035763870035,-7.14187533024342,
18.4446660804073));
#181793=CARTESIAN_POINT('Ctrl Pts',(7.76877342015511,-3.59462525859519,
18.6562227007891));
#181794=CARTESIAN_POINT('Ctrl Pts',(8.28430972229547,2.18829736655231,18.867779321171));
#181795=CARTESIAN_POINT('Ctrl Pts',(4.95089445119752,6.39150157836752,19.0793359415529));
#181796=CARTESIAN_POINT('Ctrl Pts',(1.31987319530725,7.98997545899841,19.2380034068393));
#181797=CARTESIAN_POINT('Ctrl Pts',(-2.67569831094984,7.64521786231378,
19.3966708721258));
#181798=CARTESIAN_POINT('Ctrl Pts',(-5.99640309280362,5.43448042823468,
19.5553383374121));
#181799=CARTESIAN_POINT('Ctrl Pts',(-7.87078835133371,1.91295800841818,
19.7140058026986));
#181800=CARTESIAN_POINT('Ctrl Pts',(-7.82199981784164,-2.09716283029542,
19.872673267985));
#181801=CARTESIAN_POINT('Ctrl Pts',(-5.8751038780775,-5.55389977538047,
20.0313407332714));
#181802=CARTESIAN_POINT('Ctrl Pts',(-1.3652251799131,-8.4589948071571,20.2428973536535));
#181803=CARTESIAN_POINT('Ctrl Pts',(4.33925195138733,-7.3787575990691,20.4544539740352));
#181804=CARTESIAN_POINT('Ctrl Pts',(7.47821715101717,-3.06165892147577,
20.6660105944172));
#181805=CARTESIAN_POINT('Ctrl Pts',(8.26795152848235,2.21723898714254,20.877567214799));
#181806=CARTESIAN_POINT('Ctrl Pts',(4.95882582137418,6.98773778934587,21.089123835181));
#181807=CARTESIAN_POINT('Ctrl Pts',(-0.293495865414464,8.0793878771945,
21.3006804555629));
#181808=CARTESIAN_POINT('Ctrl Pts',(-4.10554350583665,6.98042159248063,
21.4593479208493));
#181809=CARTESIAN_POINT('Ctrl Pts',(-6.95252221453218,4.15585760943489,
21.6180153861357));
#181810=CARTESIAN_POINT('Ctrl Pts',(-8.08584616639284,0.330937078129198,
21.7766828514222));
#181811=CARTESIAN_POINT('Ctrl Pts',(-7.26888142150446,-3.57380476433294,
21.9353503167086));
#181812=CARTESIAN_POINT('Ctrl Pts',(-4.66224525194671,-6.62157400455422,
22.094017781995));
#181813=CARTESIAN_POINT('Ctrl Pts',(-0.952753783854475,-8.02838143840485,
22.2526852472814));
#181814=CARTESIAN_POINT('Ctrl Pts',(4.37120959420905,-7.36959697832074,
22.4642418676634));
#181815=CARTESIAN_POINT('Ctrl Pts',(8.05910804671024,-2.88547200556326,
22.6757984880452));
#181816=CARTESIAN_POINT('Ctrl Pts',(7.70340129483707,2.44030645614891,22.8873551084271));
#181817=CARTESIAN_POINT('Ctrl Pts',(4.92772366061626,6.99947931835228,23.0989117288091));
#181818=CARTESIAN_POINT('Ctrl Pts',(-0.669398417089992,8.54226777258687,
23.3104683491909));
#181819=CARTESIAN_POINT('Ctrl Pts',(-5.40159489200389,6.01543189769863,
23.5220249695729));
#181820=CARTESIAN_POINT('Ctrl Pts',(-7.62446036629699,2.7293547240793,23.6806924348593));
#181821=CARTESIAN_POINT('Ctrl Pts',(-8.00078880883006,-1.26336694984519,
23.8393599001457));
#181822=CARTESIAN_POINT('Ctrl Pts',(-6.42044791237127,-4.92628421640267,
23.9980273654321));
#181823=CARTESIAN_POINT('Ctrl Pts',(-3.29150879454047,-7.40099233001387,
24.1566948307186));
#181824=CARTESIAN_POINT('Ctrl Pts',(0.662525911002324,-8.07111098327473,
24.315362296005));
#181825=CARTESIAN_POINT('Ctrl Pts',(4.41202858140564,-6.77470678996754,
24.4740297612914));
#181826=CARTESIAN_POINT('Ctrl Pts',(8.07777660950554,-2.85796395818857,
24.6855863816734));
#181827=CARTESIAN_POINT('Ctrl Pts',(8.03653925108718,2.9477462694699,24.8971430020552));
#181828=CARTESIAN_POINT('Ctrl Pts',(4.35134083743695,6.80906161124081,25.1086996224372));
#181829=CARTESIAN_POINT('Ctrl Pts',(-0.700801569229135,8.53135677158124,
25.320256242819));
#181830=CARTESIAN_POINT('Ctrl Pts',(-5.98677270993274,6.13000697054935,
25.531812863201));
#181831=CARTESIAN_POINT('Ctrl Pts',(-8.00134397993067,1.15807720295321,
25.7433694835829));
#181832=CARTESIAN_POINT('Ctrl Pts',(-7.60279058993861,-2.78914831671395,
25.9020369488693));
#181833=CARTESIAN_POINT('Ctrl Pts',(-5.33371233888031,-6.09591915132881,
26.0607044141557));
#181834=CARTESIAN_POINT('Ctrl Pts',(-1.77357280768402,-7.89587658668085,
26.2193718794422));
#181835=CARTESIAN_POINT('Ctrl Pts',(2.21434866846989,-7.79136557914638,
26.3780393447286));
#181836=CARTESIAN_POINT('Ctrl Pts',(5.67963852838276,-5.77264924224552,
26.536706810015));
#181837=CARTESIAN_POINT('Ctrl Pts',(7.72798798922236,-2.37504735355052,
26.6953742753014));
#181838=CARTESIAN_POINT('Ctrl Pts',(8.03324957423221,2.98082777387049,26.9069308956833));
#181839=CARTESIAN_POINT('Ctrl Pts',(4.28202588343303,7.41211343255407,27.1184875160653));
#181840=CARTESIAN_POINT('Ctrl Pts',(-1.02136088257305,8.0158785580103,27.3300441364471));
#181841=CARTESIAN_POINT('Ctrl Pts',(-6.00389410589115,6.10151020393185,
27.5416007568292));
#181842=CARTESIAN_POINT('Ctrl Pts',(-8.5240568146021,0.871141986598558,
27.7531573772109));
#181843=CARTESIAN_POINT('Ctrl Pts',(-6.88549219764244,-4.23705622919709,
27.9647139975929));
#181844=CARTESIAN_POINT('Ctrl Pts',(-4.05059701621648,-7.01244870921033,
28.1233814628793));
#181845=CARTESIAN_POINT('Ctrl Pts',(-0.189808693704911,-8.09769660293935,
28.2820489281657));
#181846=CARTESIAN_POINT('Ctrl Pts',(3.69690001810475,-7.19884420114699,
28.4407163934522));
#181847=CARTESIAN_POINT('Ctrl Pts',(6.69192440029062,-4.56364606803117,
28.5993838587386));
#181848=CARTESIAN_POINT('Ctrl Pts',(8.05928550105423,-0.793530276413581,
28.758051324025));
#181849=CARTESIAN_POINT('Ctrl Pts',(7.45528542102758,3.12751779917977,28.9167187893114));
#181850=CARTESIAN_POINT('Ctrl Pts',(4.25830560106211,7.43540626646198,29.1282754096933));
#181851=CARTESIAN_POINT('Ctrl Pts',(-1.4609408163955,8.43450194939975,29.3398320300753));
#181852=CARTESIAN_POINT('Ctrl Pts',(-5.91977110935251,5.50034518208584,
29.5513886504571));
#181853=CARTESIAN_POINT('Ctrl Pts',(-8.5189457558619,0.838292557596449,
29.7629452708391));
#181854=CARTESIAN_POINT('Ctrl Pts',(-7.10300679471207,-4.79225702708581,
29.9745018912209));
#181855=CARTESIAN_POINT('Ctrl Pts',(-2.57220997546955,-7.66461898174121,
30.1860585116029));
#181856=CARTESIAN_POINT('Ctrl Pts',(1.38258078166772,-7.9793636005167,30.3447259768893));
#181857=CARTESIAN_POINT('Ctrl Pts',(5.04223681229703,-6.33912971488816,
30.5033934421758));
#181858=CARTESIAN_POINT('Ctrl Pts',(7.45063563589183,-3.15886944925386,
30.6620609074621));
#181859=CARTESIAN_POINT('Ctrl Pts',(8.0619571758907,0.783303330495699,30.8207283727486));
#181860=CARTESIAN_POINT('Ctrl Pts',(6.6964251779342,4.5540820066635,30.979395838035));
#181861=CARTESIAN_POINT('Ctrl Pts',(3.72055633984306,7.17775095801089,31.1380633033215));
#181862=CARTESIAN_POINT('Ctrl Pts',(-1.49407666705354,8.4371895707247,31.3496199237034));
#181863=CARTESIAN_POINT('Ctrl Pts',(-6.5254873680156,5.540143122096,31.5611765440852));
#181864=CARTESIAN_POINT('Ctrl Pts',(-8.06920482161725,0.430604988368971,
31.7727331644672));
#181865=CARTESIAN_POINT('Ctrl Pts',(-7.07803671433036,-4.81420476029328,
31.984289784849));
#181866=CARTESIAN_POINT('Ctrl Pts',(-2.38351862570955,-8.23026560326427,
32.195846405231));
#181867=CARTESIAN_POINT('Ctrl Pts',(2.93553478289759,-7.53294655706325,
32.4074030256128));
#181868=CARTESIAN_POINT('Ctrl Pts',(6.17372664486792,-5.24088469645491,
32.5660704908993));
#181869=CARTESIAN_POINT('Ctrl Pts',(7.93280824411931,-1.63684787793316,
32.7247379561857));
#181870=CARTESIAN_POINT('Ctrl Pts',(7.74450397115589,2.3479961279784,32.8834054214723));
#181871=CARTESIAN_POINT('Ctrl Pts',(5.68824200445711,5.76650852008312,33.0420728867586));
#181872=CARTESIAN_POINT('Ctrl Pts',(2.223931863048,7.7869056855472,33.2007403520451));
#181873=CARTESIAN_POINT('Ctrl Pts',(-1.74189528503904,7.89483686399733,
33.3594078173314));
#181874=CARTESIAN_POINT('Ctrl Pts',(-6.55265142255683,5.52097747449158,
33.5709644377134));
#181875=CARTESIAN_POINT('Ctrl Pts',(-8.5597796768496,0.0730964242035642,
33.7825210580952));
#181876=CARTESIAN_POINT('Ctrl Pts',(-6.47152498241538,-4.83909614609933,
33.9940776784773));
#181877=CARTESIAN_POINT('Ctrl Pts',(-2.35028493223617,-8.23111972581751,
34.2056342988591));
#181878=CARTESIAN_POINT('Ctrl Pts',(3.4428090820096,-7.84636849531113,34.4171909192411));
#181879=CARTESIAN_POINT('Ctrl Pts',(7.08009910292349,-3.90318395492124,
34.6287475396229));
#181880=CARTESIAN_POINT('Ctrl Pts',(8.09796612938011,-0.0686851839944798,
34.7874150049093));
#181881=CARTESIAN_POINT('Ctrl Pts',(7.1396048889772,3.82554043799754,34.9460824701958));
#181882=CARTESIAN_POINT('Ctrl Pts',(4.44204076926994,6.76451782320029,35.1047499354821));
#181883=CARTESIAN_POINT('Ctrl Pts',(0.673065974102065,8.07190806488574,
35.2634174007686));
#181884=CARTESIAN_POINT('Ctrl Pts',(-3.28129335117483,7.40370765431913,
35.422084866055));
#181885=CARTESIAN_POINT('Ctrl Pts',(-6.39545934638827,4.94578083237291,
35.5807523313416));
#181886=CARTESIAN_POINT('Ctrl Pts',(-8.56835770634636,0.0409774996080618,
35.7923089517233));
#181887=CARTESIAN_POINT('Ctrl Pts',(-6.61914916072759,-5.42789421336466,
36.0038655721053));
#181888=CARTESIAN_POINT('Ctrl Pts',(-1.86864952650306,-7.8616560632172,
36.2154221924872));
#181889=CARTESIAN_POINT('Ctrl Pts',(3.46887358869753,-7.82573237653036,
36.4269788128691));
#181890=CARTESIAN_POINT('Ctrl Pts',(7.67039232215131,-3.81883680767606,
36.6385354332509));
#181891=CARTESIAN_POINT('Ctrl Pts',(7.93686296667427,1.53910835921557,36.8500920536329));
#181892=CARTESIAN_POINT('Ctrl Pts',(6.26173611367256,5.13540981128245,37.0087595189193));
#181893=CARTESIAN_POINT('Ctrl Pts',(3.030968251,7.51145452458389,37.1674269842058));
#181894=CARTESIAN_POINT('Ctrl Pts',(-0.923182212626471,8.03978620229051,
37.3260944494921));
#181895=CARTESIAN_POINT('Ctrl Pts',(-4.65466311300933,6.62893874748074,
37.4847619147786));
#181896=CARTESIAN_POINT('Ctrl Pts',(-7.26277749619282,3.58243438570523,
37.643429380065));
#181897=CARTESIAN_POINT('Ctrl Pts',(-8.07915054981909,-0.299957807917071,
37.8020968453515));
#181898=CARTESIAN_POINT('Ctrl Pts',(-6.60515776764774,-5.45805128263392,
38.0136534657333));
#181899=CARTESIAN_POINT('Ctrl Pts',(-1.60477047887609,-8.40832224130156,
38.2252100861153));
#181900=CARTESIAN_POINT('Ctrl Pts',(3.60197462565547,-7.23348228071057,
38.4367667064971));
#181901=CARTESIAN_POINT('Ctrl Pts',(7.67718401246675,-3.78629328528101,
38.6483233268791));
#181902=CARTESIAN_POINT('Ctrl Pts',(8.33605940688698,1.98205613044405,38.859879947261));
#181903=CARTESIAN_POINT('Ctrl Pts',(5.10796914345129,6.26668169948992,39.0714365676429));
#181904=CARTESIAN_POINT('Ctrl Pts',(1.51773057783043,7.9547637916035,39.2301040329293));
#181905=CARTESIAN_POINT('Ctrl Pts',(-2.48516546487529,7.70925873386361,
39.3887714982157));
#181906=CARTESIAN_POINT('Ctrl Pts',(-5.85970513598202,5.58160221581555,
39.5474389635022));
#181907=CARTESIAN_POINT('Ctrl Pts',(-7.82089653681279,2.10767525343236,
39.7061064287886));
#181908=CARTESIAN_POINT('Ctrl Pts',(-7.87163043666332,-1.90242144533834,
39.864773894075));
#181909=CARTESIAN_POINT('Ctrl Pts',(-6.01110968313766,-5.40640441240397,
40.0234413593615));
#181910=CARTESIAN_POINT('Ctrl Pts',(-1.57470687574229,-8.42251335379584,
40.2349979797433));
#181911=CARTESIAN_POINT('Ctrl Pts',(4.15481883293474,-7.48416005099628,
40.4465546001254));
#181912=CARTESIAN_POINT('Ctrl Pts',(7.39994227321339,-3.24628117425619,
40.6581112205073));
#181913=CARTESIAN_POINT('Ctrl Pts',(8.32042440936654,2.01139475276605,40.8696678408892));
#181914=CARTESIAN_POINT('Ctrl Pts',(5.13069311721947,6.86253751001021,41.081224461271));
#181915=CARTESIAN_POINT('Ctrl Pts',(-0.0929230143071497,8.08418292758069,
41.292781081653));
#181916=CARTESIAN_POINT('Ctrl Pts',(-3.93106668673612,7.08014744136818,
41.4514485469393));
#181917=CARTESIAN_POINT('Ctrl Pts',(-6.84725768633784,4.32709831068912,
41.6101160122258));
#181918=CARTESIAN_POINT('Ctrl Pts',(-8.07514450673869,0.531477912525767,
41.7687834775121));
#181919=CARTESIAN_POINT('Ctrl Pts',(-7.35532384768093,-3.39233381453608,
41.9274509427987));
#181920=CARTESIAN_POINT('Ctrl Pts',(-4.82511785680412,-6.5038458434228,
42.086118408085));
#181921=CARTESIAN_POINT('Ctrl Pts',(-1.15167721705284,-8.00226767115608,
42.2447858733715));
#181922=CARTESIAN_POINT('Ctrl Pts',(4.18699394776991,-7.47579525008377,
42.4563424937533));
#181923=CARTESIAN_POINT('Ctrl Pts',(7.98502621710635,-3.08456277525204,
42.6678991141353));
#181924=CARTESIAN_POINT('Ctrl Pts',(7.76158322136841,2.24840232341148,42.8794557345171));
#181925=CARTESIAN_POINT('Ctrl Pts',(5.09989188825386,6.87504719480985,43.0910123548991));
#181926=CARTESIAN_POINT('Ctrl Pts',(-0.457223885958288,8.55624796593684,
43.302568975281));
#181927=CARTESIAN_POINT('Ctrl Pts',(-5.25066431761787,6.1476151899389,43.5141255956629));
#181928=CARTESIAN_POINT('Ctrl Pts',(-7.55438627582335,2.91770818744103,
43.6727930609493));
#181929=CARTESIAN_POINT('Ctrl Pts',(-8.02967450977103,-1.06444582138774,
43.8314605262359));
#181930=CARTESIAN_POINT('Ctrl Pts',(-6.5407120987235,-4.76544990412998,
43.9901279915221));
#181931=CARTESIAN_POINT('Ctrl Pts',(-3.47414401702616,-7.31703771791091,
44.1487954568087));
#181932=CARTESIAN_POINT('Ctrl Pts',(0.462044824466225,-8.08506572395892,
44.3074629220949));
#181933=CARTESIAN_POINT('Ctrl Pts',(4.24256199092539,-6.88210111412175,
44.4661303873815));
#181934=CARTESIAN_POINT('Ctrl Pts',(8.00437166488504,-3.05752646175317,
44.6776870077635));
#181935=CARTESIAN_POINT('Ctrl Pts',(8.10721015544517,2.74741941947125,44.8892436281453));
#181936=CARTESIAN_POINT('Ctrl Pts',(4.51896161031848,6.69899047623219,45.1008002485272));
#181937=CARTESIAN_POINT('Ctrl Pts',(-0.488888375429131,8.54611967991167,
45.3123568689091));
#181938=CARTESIAN_POINT('Ctrl Pts',(-5.83281835435429,6.27667539433993,
45.523913489291));
#181939=CARTESIAN_POINT('Ctrl Pts',(-7.97014427217491,1.35626678924387,
45.7354701096728));
#181940=CARTESIAN_POINT('Ctrl Pts',(-7.66965832474677,-2.59963393149468,
45.8941375749593));
#181941=CARTESIAN_POINT('Ctrl Pts',(-5.4833371940026,-5.96168984876232,
46.0528050402458));
#181942=CARTESIAN_POINT('Ctrl Pts',(-1.96895048651429,-7.84943798622479,
46.2114725055322));
#181943=CARTESIAN_POINT('Ctrl Pts',(2.02032187363893,-7.84390928812353,
46.3701399708186));
#181944=CARTESIAN_POINT('Ctrl Pts',(5.53466446957311,-5.91181452321533,
46.5288074361051));
#181945=CARTESIAN_POINT('Ctrl Pts',(7.66664218087319,-2.56606484425791,
46.6874749013914));
#181946=CARTESIAN_POINT('Ctrl Pts',(8.10481401624341,2.78054065146841,46.8990315217734));
#181947=CARTESIAN_POINT('Ctrl Pts',(4.46449514000472,7.30363726059554,47.1105881421552));
#181948=CARTESIAN_POINT('Ctrl Pts',(-0.821978661578898,8.03868309971759,
47.3221447625372));
#181949=CARTESIAN_POINT('Ctrl Pts',(-5.85104055953245,6.24878888601925,
47.533701382919));
#181950=CARTESIAN_POINT('Ctrl Pts',(-8.49901735273743,1.08203688693143,
47.745258003301));
#181951=CARTESIAN_POINT('Ctrl Pts',(-6.9894958003849,-4.06445832835817,
47.9568146236829));
#181952=CARTESIAN_POINT('Ctrl Pts',(-4.22128064297539,-6.91069714498755,
48.1154820889693));
#181953=CARTESIAN_POINT('Ctrl Pts',(-0.394720512146466,-8.08870629150604,
48.2741495542558));
#181954=CARTESIAN_POINT('Ctrl Pts',(3.52473691091294,-7.29174113183975,
48.4328170195422));
#181955=CARTESIAN_POINT('Ctrl Pts',(6.56281846735994,-4.72210073487363,
48.5914844848286));
#181956=CARTESIAN_POINT('Ctrl Pts',(8.55717721688639,0.236199208950159,
48.8030411052105));
#181957=CARTESIAN_POINT('Ctrl Pts',(5.9153156826332,7.02513251500696,49.0674868806879));
#181958=CARTESIAN_POINT('Ctrl Pts',(-2.71850420621116,8.77453486642056,
49.3848218112606));
#181959=CARTESIAN_POINT('Ctrl Pts',(-7.79248632499947,3.54136004741615,
49.6492675867384));
#181960=CARTESIAN_POINT('Ctrl Pts',(-7.88211848193875,-1.79548923383272,
49.8608242071199));
#181961=CARTESIAN_POINT('Ctrl Pts',(-6.08265409382359,-5.3557987538077,
50.0194916724066));
#181962=CARTESIAN_POINT('Ctrl Pts',(-2.78012128575648,-7.59101714791989,
50.1781591376928));
#181963=CARTESIAN_POINT('Ctrl Pts',(2.52766458240851,-8.17844913584806,
50.3897157580749));
#181964=CARTESIAN_POINT('Ctrl Pts',(8.35589799254476,-3.80775034988006,
50.6541615335521));
#181965=CARTESIAN_POINT('Ctrl Pts',(7.72417822065321,4.97771490393895,50.9714964641252));
#181966=CARTESIAN_POINT('Ctrl Pts',(1.30727621037075,8.45865693165901,51.2359422396023));
#181967=CARTESIAN_POINT('Ctrl Pts',(-3.8383109442619,7.10760758645932,51.4474988599843));
#181968=CARTESIAN_POINT('Ctrl Pts',(-7.80510652006937,3.52562858333696,
51.6590554803662));
#181969=CARTESIAN_POINT('Ctrl Pts',(-8.2620746709558,-2.26208194974895,
51.8706121007481));
#181970=CARTESIAN_POINT('Ctrl Pts',(-4.89489459159957,-6.43524337861689,
52.08216872113));
#181971=CARTESIAN_POINT('Ctrl Pts',(-1.24811346699438,-8.00144121968931,
52.2408361864165));
#181972=CARTESIAN_POINT('Ctrl Pts',(2.74330699596842,-7.62108382551198,
52.3995036517029));
#181973=CARTESIAN_POINT('Ctrl Pts',(6.04469976260079,-5.38091157393227,
52.5581711169893));
#181974=CARTESIAN_POINT('Ctrl Pts',(7.88741087937344,-1.84283217800734,
52.7168385822757));
#181975=CARTESIAN_POINT('Ctrl Pts',(7.80307288743708,2.16668750547222,52.8755060475622));
#181976=CARTESIAN_POINT('Ctrl Pts',(5.82542340009905,5.60596559873273,53.0341735128486));
#181977=CARTESIAN_POINT('Ctrl Pts',(1.28990952670701,8.4708083462645,53.2457301332307));
#181978=CARTESIAN_POINT('Ctrl Pts',(-4.40475490759329,7.33984953337933,
53.4572867536124));
#181979=CARTESIAN_POINT('Ctrl Pts',(-7.50516412453447,2.99498640274816,
53.6688433739943));
#181980=CARTESIAN_POINT('Ctrl Pts',(-8.24789523695355,-2.29073016552212,
53.8803999943762));
#181981=CARTESIAN_POINT('Ctrl Pts',(-4.89644173511686,-7.03159136007465,
54.0919566147581));
#181982=CARTESIAN_POINT('Ctrl Pts',(0.365384614725759,-8.07645597898883,
54.30351323514));
#181983=CARTESIAN_POINT('Ctrl Pts',(4.1675023402685,-6.94360863936363,54.4621807004266));
#181984=CARTESIAN_POINT('Ctrl Pts',(6.98923100089694,-4.09382029169499,
54.6208481657129));
#181985=CARTESIAN_POINT('Ctrl Pts',(8.08847119617018,-0.25896543083787,
54.7795156309993));
#181986=CARTESIAN_POINT('Ctrl Pts',(7.23678907745967,3.63835136269798,54.9381830962858));
#181987=CARTESIAN_POINT('Ctrl Pts',(4.60313313887934,6.66280261197641,55.0968505615722));
#181988=CARTESIAN_POINT('Ctrl Pts',(0.88126888889716,8.03654238010657,55.2555180268586));
#181989=CARTESIAN_POINT('Ctrl Pts',(-4.43662090061271,7.33040434155508,
55.4670746472405));
#181990=CARTESIAN_POINT('Ctrl Pts',(-8.08446765842773,2.81363714410309,
55.6786312676224));
#181991=CARTESIAN_POINT('Ctrl Pts',(-7.68137916670904,-2.50876486966342,
55.8901878880043));
#181992=CARTESIAN_POINT('Ctrl Pts',(-4.865237905432,-7.04305554036251,56.1017445083862));
#181993=CARTESIAN_POINT('Ctrl Pts',(0.745392301949692,-8.53597230889284,
56.3133011287681));
#181994=CARTESIAN_POINT('Ctrl Pts',(5.4549142553828,-5.96712315561334,56.5248577491501));
#181995=CARTESIAN_POINT('Ctrl Pts',(7.64844784646817,-2.66139411417292,
56.6835252144364));
#181996=CARTESIAN_POINT('Ctrl Pts',(7.9892288701152,1.33451851699505,56.8421926797231));
#181997=CARTESIAN_POINT('Ctrl Pts',(6.37635307462309,4.98322677036489,57.0008601450092));
#181998=CARTESIAN_POINT('Ctrl Pts',(3.22551463743937,7.42999144931627,57.1595276102958));
#181999=CARTESIAN_POINT('Ctrl Pts',(-0.734327090956097,8.06489533785327,
57.3181950755822));
#182000=CARTESIAN_POINT('Ctrl Pts',(-4.47214416361251,6.73517445008891,
57.4768625408686));
#182001=CARTESIAN_POINT('Ctrl Pts',(-8.10289067319347,2.78596404814002,
57.6884191612504));
#182002=CARTESIAN_POINT('Ctrl Pts',(-8.00998806280779,-3.01914929030919,
57.8999757816326));
#182003=CARTESIAN_POINT('Ctrl Pts',(-4.29057249337804,-6.84751595750426,
58.1115324020142));
#182004=CARTESIAN_POINT('Ctrl Pts',(0.776697108980894,-8.52478227313381,
58.3230890223963));
#182005=CARTESIAN_POINT('Ctrl Pts',(6.04108854134644,-6.07648600549702,
58.5346456427781));
#182006=CARTESIAN_POINT('Ctrl Pts',(8.01133323067813,-1.08682480658109,
58.74620226316));
#182007=CARTESIAN_POINT('Ctrl Pts',(7.57766799225029,2.85669754897422,58.9048697284464));
#182008=CARTESIAN_POINT('Ctrl Pts',(5.27925157756536,6.14314417820664,59.0635371937329));
#182009=CARTESIAN_POINT('Ctrl Pts',(1.70323462613665,7.91134750750969,59.2222046590193));
#182010=CARTESIAN_POINT('Ctrl Pts',(-2.28359885220972,7.77135084111175,
59.3808721243058));
#182011=CARTESIAN_POINT('Ctrl Pts',(-5.73078628072618,5.72187571446011,
59.5395395895922));
#182012=CARTESIAN_POINT('Ctrl Pts',(-7.74881827407838,2.30617944845616,
59.6982070548786));
#182013=CARTESIAN_POINT('Ctrl Pts',(-8.0064041132583,-3.05220020879696,
59.9097636752605));
#182014=CARTESIAN_POINT('Ctrl Pts',(-4.21589353186778,-7.44992704201823,
60.1213202956424));
#182015=CARTESIAN_POINT('Ctrl Pts',(1.09265632163192,-8.00647171181022,
60.3328769160243));
#182016=CARTESIAN_POINT('Ctrl Pts',(6.05795565739796,-6.04783799852794,
60.5444335364063));
#182017=CARTESIAN_POINT('Ctrl Pts',(8.53147183715803,-0.795249162941086,
60.7559901567881));
#182018=CARTESIAN_POINT('Ctrl Pts',(6.84751260599863,4.29816465527584,60.9675467771701));
#182019=CARTESIAN_POINT('Ctrl Pts',(3.98803057425647,7.04821858527979,61.1262142424565));
#182020=CARTESIAN_POINT('Ctrl Pts',(0.117737167502885,8.09906510486547,
61.284881707743));
#182021=CARTESIAN_POINT('Ctrl Pts',(-3.76081845462485,7.16565922491463,
61.4435491730294));
#182022=CARTESIAN_POINT('Ctrl Pts',(-6.73227275777555,4.50391175850224,
61.6022166383157));
#182023=CARTESIAN_POINT('Ctrl Pts',(-8.06602823683544,0.72177667575291,
61.7608841036022));
#182024=CARTESIAN_POINT('Ctrl Pts',(-7.42715740551509,-3.1937409360928,
61.9195515688887));
#182025=CARTESIAN_POINT('Ctrl Pts',(-4.19196689838406,-7.47300785910407,
62.1311081892706));
#182026=CARTESIAN_POINT('Ctrl Pts',(1.53594431257073,-8.4211665624259,62.3426648096525));
#182027=CARTESIAN_POINT('Ctrl Pts',(5.96848603098247,-5.44744542030362,
62.5542214300343));
#182028=CARTESIAN_POINT('Ctrl Pts',(8.5260686431671,-0.762446519725676,
62.7657780504163));
#182029=CARTESIAN_POINT('Ctrl Pts',(7.06007767884898,4.85527919979866,62.9773346707981));
#182030=CARTESIAN_POINT('Ctrl Pts',(2.50389820398932,7.68720638966013,63.1888912911801));
#182031=CARTESIAN_POINT('Ctrl Pts',(-1.45353695814277,7.96674358809175,
63.3475587564665));
#182032=CARTESIAN_POINT('Ctrl Pts',(-5.09845109774291,6.29400619775557,
63.5062262217529));
#182033=CARTESIAN_POINT('Ctrl Pts',(-7.47845238908096,3.09243875291006,
63.6648936870394));
#182034=CARTESIAN_POINT('Ctrl Pts',(-8.05466705580809,-0.855018265033708,
63.8235611523257));
#182035=CARTESIAN_POINT('Ctrl Pts',(-6.65563175880953,-4.61349531030578,
63.9822286176123));
#182036=CARTESIAN_POINT('Ctrl Pts',(-3.65653188946597,-7.21057714988829,
64.1408960828986));
#182037=CARTESIAN_POINT('Ctrl Pts',(1.56910276906502,-8.42355919071576,
64.3524527032806));
#182038=CARTESIAN_POINT('Ctrl Pts',(6.57453247811738,-5.48185132027664,
64.5640093236623));
#182039=CARTESIAN_POINT('Ctrl Pts',(8.07271737558231,-0.35877748423116,
64.7755659440445));
#182040=CARTESIAN_POINT('Ctrl Pts',(7.03491326733044,4.87700384709477,64.9871225644261));
#182041=CARTESIAN_POINT('Ctrl Pts',(2.31018045491571,8.25115138663115,65.1986791848083));
#182042=CARTESIAN_POINT('Ctrl Pts',(-3.00245665374948,7.50652398487662,
65.41023580519));
#182043=CARTESIAN_POINT('Ctrl Pts',(-6.22012248750458,5.18573517714964,
65.5689032704766));
#182044=CARTESIAN_POINT('Ctrl Pts',(-7.94706094328348,1.56618644394587,
65.7275707357629));
#182045=CARTESIAN_POINT('Ctrl Pts',(-7.72330171704765,-2.4168239827715,
65.8862382010493));
#182046=CARTESIAN_POINT('Ctrl Pts',(-5.63669873514582,-5.81690166520522,
66.0449056663359));
#182047=CARTESIAN_POINT('Ctrl Pts',(-2.15454561453617,-7.80638881186242,
66.2035731316222));
#182048=CARTESIAN_POINT('Ctrl Pts',(1.81208500210048,-7.87902254333207,
66.3622405969087));
#182049=CARTESIAN_POINT('Ctrl Pts',(6.60152489569881,-5.46244468995782,
66.5737972172905));
#182050=CARTESIAN_POINT('Ctrl Pts',(8.56009122032943,0.00308270630419909,
66.7853538376725));
#182051=CARTESIAN_POINT('Ctrl Pts',(6.42820403667042,4.8964967039868,66.9969104580544));
#182052=CARTESIAN_POINT('Ctrl Pts',(2.27694047637668,8.25170971802063,67.2084670784361));
#182053=CARTESIAN_POINT('Ctrl Pts',(-3.51250010768767,7.81541911434526,
67.4200236988182));
#182054=CARTESIAN_POINT('Ctrl Pts',(-7.11455442374939,3.84002130784199,
67.6315803192001));
#182055=CARTESIAN_POINT('Ctrl Pts',(-8.09825670351394,-0.00338394434941844,
67.7902477844866));
#182056=CARTESIAN_POINT('Ctrl Pts',(-7.10527744608323,-3.88892659067283,
67.9489152497728));
#182057=CARTESIAN_POINT('Ctrl Pts',(-4.38166524303238,-6.80378110128866,
68.1075827150595));
#182058=CARTESIAN_POINT('Ctrl Pts',(-0.601204811537375,-8.07757825019637,
68.2662501803458));
#182059=CARTESIAN_POINT('Ctrl Pts',(3.34705139145844,-7.37421318311479,
68.4249176456322));
#182060=CARTESIAN_POINT('Ctrl Pts',(6.43922018414456,-4.88866972839014,
68.5835851109187));
#182061=CARTESIAN_POINT('Ctrl Pts',(8.56838307348488,0.0352766976451838,
68.7951417313005));
#182062=CARTESIAN_POINT('Ctrl Pts',(6.57058246548689,5.48658521009879,69.0066983516824));
#182063=CARTESIAN_POINT('Ctrl Pts',(1.79861211939978,7.87797445750923,69.2182549720644));
#182064=CARTESIAN_POINT('Ctrl Pts',(-3.53837993476094,7.79455185631092,
69.4298115924462));
#182065=CARTESIAN_POINT('Ctrl Pts',(-7.70407363508685,3.75042429126886,
69.6413682128281));
#182066=CARTESIAN_POINT('Ctrl Pts',(-7.92285164794354,-1.60968011041032,
69.8529248332102));
#182067=CARTESIAN_POINT('Ctrl Pts',(-6.21578648478412,-5.19093165652013,
70.0115922984965));
#182068=CARTESIAN_POINT('Ctrl Pts',(-2.96400137263525,-7.53813063540808,
70.1702597637831));
#182069=CARTESIAN_POINT('Ctrl Pts',(0.994694301361778,-8.03125213295468,
70.3289272290693));
#182070=CARTESIAN_POINT('Ctrl Pts',(4.7134718501872,-6.58725289714569,70.4875946943558));
#182071=CARTESIAN_POINT('Ctrl Pts',(7.29437112929025,-3.51765872637811,
70.6462621596422));
#182072=CARTESIAN_POINT('Ctrl Pts',(8.07616119634359,0.371844892188463,
70.8049296249286));
#182073=CARTESIAN_POINT('Ctrl Pts',(6.55632324899169,5.51661657124278,71.0164862453105));
#182074=CARTESIAN_POINT('Ctrl Pts',(1.52987856295196,8.42227064312582,71.2280428656924));
#182075=CARTESIAN_POINT('Ctrl Pts',(-3.66620507662212,7.20114070445578,
71.4395994860744));
#182076=CARTESIAN_POINT('Ctrl Pts',(-7.71057544116701,3.71782161614985,
71.6511561064562));
#182077=CARTESIAN_POINT('Ctrl Pts',(-8.31809034521527,-2.05616291869497,
71.8627127268381));
#182078=CARTESIAN_POINT('Ctrl Pts',(-5.05199765060271,-6.31189100281976,
72.0742693472201));
#182079=CARTESIAN_POINT('Ctrl Pts',(-1.44687847137091,-7.96795555811971,
72.2329368125064));
#182080=CARTESIAN_POINT('Ctrl Pts',(2.55367422908007,-7.68683716135536,
72.391604277793));
#182081=CARTESIAN_POINT('Ctrl Pts',(5.90914556872033,-5.52923378271561,
72.5502717430793));
#182082=CARTESIAN_POINT('Ctrl Pts',(7.8393437120909,-2.03799111312154,72.7089392083658));
#182083=CARTESIAN_POINT('Ctrl Pts',(7.85438846097099,1.97239828413365,72.8676066736522));
#182084=CARTESIAN_POINT('Ctrl Pts',(5.96275831076774,5.45968512100677,73.0262741389386));
#182085=CARTESIAN_POINT('Ctrl Pts',(1.49968985904912,8.43619364796968,73.2378307593206));
#182086=CARTESIAN_POINT('Ctrl Pts',(-4.2212582536141,7.44688860932765,73.4493873797026));
#182087=CARTESIAN_POINT('Ctrl Pts',(-7.42853893893759,3.18029815298939,
73.6609440000843));
#182088=CARTESIAN_POINT('Ctrl Pts',(-8.30219487298872,-2.08536123833689,
73.8725006204664));
#182089=CARTESIAN_POINT('Ctrl Pts',(-5.06941801176177,-6.90792544555923,
74.0840572408481));
#182090=CARTESIAN_POINT('Ctrl Pts',(0.164863081854742,-8.08303584412526,
74.2956138612302));
#182091=CARTESIAN_POINT('Ctrl Pts',(3.99391952962493,-7.04488324090387,
74.4542813265165));
#182092=CARTESIAN_POINT('Ctrl Pts',(6.88549477799248,-4.26599100745655,
74.6129487918029));
#182093=CARTESIAN_POINT('Ctrl Pts',(8.07955452613269,-0.459593554675651,
74.7716162570894));
#182094=CARTESIAN_POINT('Ctrl Pts',(7.32484310761663,3.45765687457021,74.9302837223757));
#182095=CARTESIAN_POINT('Ctrl Pts',(4.76704696471102,6.54652857042015,75.0889511876623));
#182096=CARTESIAN_POINT('Ctrl Pts',(1.08041685387929,8.01219992979621,75.2476186529485));
#182097=CARTESIAN_POINT('Ctrl Pts',(-4.25335765323495,7.43823780293737,
75.4591752733308));
#182098=CARTESIAN_POINT('Ctrl Pts',(-8.01216052959904,3.01337930758371,
75.6707318937123));
#182099=CARTESIAN_POINT('Ctrl Pts',(-7.74126660819681,-2.31738611587211,
75.8822885140946));
#182100=CARTESIAN_POINT('Ctrl Pts',(-5.03850667497429,-6.92016052484901,
76.0938451344761));
#182101=CARTESIAN_POINT('Ctrl Pts',(0.533350586423094,-8.55184015819647,
76.3054017548582));
#182102=CARTESIAN_POINT('Ctrl Pts',(5.30516599953248,-6.10064439306021,
76.51695837524));
#182103=CARTESIAN_POINT('Ctrl Pts',(7.58005274967108,-2.85036373105114,
76.6756258405266));
#182104=CARTESIAN_POINT('Ctrl Pts',(8.01988368877764,1.13586232965973,76.8342933058129));
#182105=CARTESIAN_POINT('Ctrl Pts',(6.49804381810543,4.82346909539517,76.9929607710994));
#182106=CARTESIAN_POINT('Ctrl Pts',(3.4088897605638,7.34766549414064,77.1516282363858));
#182107=CARTESIAN_POINT('Ctrl Pts',(-0.533978119564296,8.08063366666963,
77.3102957016723));
#182108=CARTESIAN_POINT('Ctrl Pts',(-4.30364004138297,6.84407266818358,
77.4689631669586));
#182109=CARTESIAN_POINT('Ctrl Pts',(-8.03126455947391,2.98617188304975,
77.6805197873407));
#182110=CARTESIAN_POINT('Ctrl Pts',(-8.08243903153417,-2.81945925754779,
77.8920764077226));
#182111=CARTESIAN_POINT('Ctrl Pts',(-4.45916608132687,-6.73894093818632,
78.1036330281042));
#182112=CARTESIAN_POINT('Ctrl Pts',(0.564923425535108,-8.54143036772646,
78.3151896484865));
#182113=CARTESIAN_POINT('Ctrl Pts',(5.88844605519194,-6.22451893679133,
78.526746268868));
#182114=CARTESIAN_POINT('Ctrl Pts',(7.98189786540439,-1.28528392171771,
78.7383028892501));
#182115=CARTESIAN_POINT('Ctrl Pts',(7.64622099088389,2.66778515732707,78.8969703545365));
#182116=CARTESIAN_POINT('Ctrl Pts',(5.43006240590164,6.01025289663214,79.0556378198229));
#182117=CARTESIAN_POINT('Ctrl Pts',(1.89902288606984,7.86664729439632,79.2143052851094));
#182118=CARTESIAN_POINT('Ctrl Pts',(-2.09005686769106,7.82562329167963,
79.3729727503958));
#182119=CARTESIAN_POINT('Ctrl Pts',(-5.5870386655436,5.86231797472716,79.5316402156822));
#182120=CARTESIAN_POINT('Ctrl Pts',(-7.68920659265237,2.49774904037289,
79.6903076809687));
#182121=CARTESIAN_POINT('Ctrl Pts',(-8.07967631327886,-2.85258893148296,
79.9018643013505));
#182122=CARTESIAN_POINT('Ctrl Pts',(-4.39945838421227,-7.34301961927268,
80.1134209217327));
#182123=CARTESIAN_POINT('Ctrl Pts',(0.893646742598228,-8.03111963605721,
80.3249775421143));
#182124=CARTESIAN_POINT('Ctrl Pts',(5.90601885117144,-6.19629829277502,
80.5365341624965));
#182125=CARTESIAN_POINT('Ctrl Pts',(8.50911149048599,-1.00670481366578,
80.7480907828781));
#182126=CARTESIAN_POINT('Ctrl Pts',(6.95205909401174,4.12692653757503,80.9596474032601));
#182127=CARTESIAN_POINT('Ctrl Pts',(4.16169756844071,6.94708906204051,81.1183148685464));
#182128=CARTESIAN_POINT('Ctrl Pts',(0.318671665282749,8.09364973193226,
81.276982333833));
#182129=CARTESIAN_POINT('Ctrl Pts',(-3.58185128283906,7.25677400529152,
81.4356497991193));
#182130=CARTESIAN_POINT('Ctrl Pts',(-6.618439408729,4.6695800032171,81.5943172644059));
#182131=CARTESIAN_POINT('Ctrl Pts',(-8.04563435915725,0.921705400784701,
81.7529847296922));
#182132=CARTESIAN_POINT('Ctrl Pts',(-7.50412016629928,-3.00845954317373,
81.9116521949786));
#182133=CARTESIAN_POINT('Ctrl Pts',(-4.37611184709195,-7.36668704650339,
82.1232088153607));
#182134=CARTESIAN_POINT('Ctrl Pts',(1.32650797174266,-8.45668657361387,
82.3347654357425));
#182135=CARTESIAN_POINT('Ctrl Pts',(5.83147495608897,-5.5938704798848,82.5463220561243));
#182136=CARTESIAN_POINT('Ctrl Pts',(8.50452392724124,-0.973778195699686,
82.7578786765063));
#182137=CARTESIAN_POINT('Ctrl Pts',(7.17838299269727,4.67859493326084,82.9694352968883));
#182138=CARTESIAN_POINT('Ctrl Pts',(2.69387807358101,7.62270747292933,83.18099191727));
#182139=CARTESIAN_POINT('Ctrl Pts',(-1.25540207440457,8.00035866187685,
83.3396593825567));
#182140=CARTESIAN_POINT('Ctrl Pts',(-4.94070130429781,6.41858148154023,
83.4983268478428));
#182141=CARTESIAN_POINT('Ctrl Pts',(-7.39941366601822,3.27705736528888,
83.6569943131295));
#182142=CARTESIAN_POINT('Ctrl Pts',(-8.07340337306009,-0.654885936116582,
83.8156617784157));
#182143=CARTESIAN_POINT('Ctrl Pts',(-6.76806196634699,-4.44692144148893,
83.9743292437024));
#182144=CARTESIAN_POINT('Ctrl Pts',(-3.8343297339649,-7.11762346464079,
84.1329967089886));
#182145=CARTESIAN_POINT('Ctrl Pts',(1.35959684736402,-8.45990126136336,
84.3445533293706));
#182146=CARTESIAN_POINT('Ctrl Pts',(6.43648104125485,-5.64330426337308,
84.5561099497524));
#182147=CARTESIAN_POINT('Ctrl Pts',(8.06132892477432,-0.558983967405612,
84.7676665701346));
#182148=CARTESIAN_POINT('Ctrl Pts',(7.15376540658539,4.70093732259667,84.9792231905161));
#182149=CARTESIAN_POINT('Ctrl Pts',(2.51421374279191,8.19128574736206,85.1907798108983));
#182150=CARTESIAN_POINT('Ctrl Pts',(-2.815264752711,7.57871576623082,85.40233643128));
#182151=CARTESIAN_POINT('Ctrl Pts',(-6.0895280253515,5.33848494570748,85.5610038965666));
#182152=CARTESIAN_POINT('Ctrl Pts',(-7.90575045630871,1.76290309887863,
85.7196713618529));
#182153=CARTESIAN_POINT('Ctrl Pts',(-7.78089482015652,-2.22443327027643,
85.8783388271395));
#182154=CARTESIAN_POINT('Ctrl Pts',(-5.77930409579335,-5.67524112102804,
86.0370062924257));
#182155=CARTESIAN_POINT('Ctrl Pts',(-2.34759045622567,-7.75052205576662,
86.1956737577123));
#182156=CARTESIAN_POINT('Ctrl Pts',(1.61601643149944,-7.92156166335252,
86.3543412229986));
#182157=CARTESIAN_POINT('Ctrl Pts',(6.46394670487,-5.624573400355,86.5658978433806));
#182158=CARTESIAN_POINT('Ctrl Pts',(8.55753192244567,-0.209328927201481,
86.7774544637624));
#182159=CARTESIAN_POINT('Ctrl Pts',(6.54772668871323,4.73547910132988,86.9890110841444));
#182160=CARTESIAN_POINT('Ctrl Pts',(2.48099785385986,8.1926687259147,87.2005677045262));
#182161=CARTESIAN_POINT('Ctrl Pts',(-3.31748621121201,7.9001720346963,87.4121243249083));
#182162=CARTESIAN_POINT('Ctrl Pts',(-7.01707718659673,4.01537993850101,
87.6236809452901));
#182163=CARTESIAN_POINT('Ctrl Pts',(-8.09584708698749,0.197567788879703,
87.7823484105764));
#182164=CARTESIAN_POINT('Ctrl Pts',(-7.19958970297868,-3.71141828984888,
87.941015875863));
#182165=CARTESIAN_POINT('Ctrl Pts',(-4.54914554234009,-6.69295916697977,
88.0996833411494));
#182166=CARTESIAN_POINT('Ctrl Pts',(-0.801457265437198,-8.0601726944985,
88.2583508064357));
#182167=CARTESIAN_POINT('Ctrl Pts',(3.16303655326425,-7.45499650233329,
88.4170182717223));
#182168=CARTESIAN_POINT('Ctrl Pts',(6.31592966041965,-5.04694767337688,
88.5756857370086));
#182169=CARTESIAN_POINT('Ctrl Pts',(8.56662008628893,-0.177350603524844,
88.7872423573906));
#182170=CARTESIAN_POINT('Ctrl Pts',(6.70470377310268,5.3218529215285,88.9987989777724));
#182171=CARTESIAN_POINT('Ctrl Pts',(1.99354288991289,7.83091781691632,89.2103555981544));
#182172=CARTESIAN_POINT('Ctrl Pts',(-3.34387587101894,7.87995338581739,
89.4219122185362));
#182173=CARTESIAN_POINT('Ctrl Pts',(-7.60863814175591,3.94043888002301,
89.6334688389183));
#182174=CARTESIAN_POINT('Ctrl Pts',(-7.96035478355009,-1.41258628521722,
89.8450254593));
#182175=CARTESIAN_POINT('Ctrl Pts',(-6.34268067256004,-5.03509433605964,
90.0036929245866));
#182176=CARTESIAN_POINT('Ctrl Pts',(-3.15014039304159,-7.46226059030319,
90.1623603898729));
#182177=CARTESIAN_POINT('Ctrl Pts',(0.795099983388211,-8.05346159068648,
90.3210278551594));
#182178=CARTESIAN_POINT('Ctrl Pts',(4.54856395466749,-6.70218498429923,
90.4796953204458));
#182179=CARTESIAN_POINT('Ctrl Pts',(7.20483765059431,-3.69757860168855,
90.6383627857322));
#182180=CARTESIAN_POINT('Ctrl Pts',(8.08290139834275,0.171327983207752,
90.7970302510186));
#182181=CARTESIAN_POINT('Ctrl Pts',(6.69119414748828,5.35222886469354,91.0085868714007));
#182182=CARTESIAN_POINT('Ctrl Pts',(1.73839828340533,8.38171477751168,91.2201434917824));
#182183=CARTESIAN_POINT('Ctrl Pts',(-3.48638659800205,7.28989681673174,
91.4317001121644));
#182184=CARTESIAN_POINT('Ctrl Pts',(-7.61594695082403,3.90800758003743,
91.6432567325462));
#182185=CARTESIAN_POINT('Ctrl Pts',(-8.36655083502915,-1.84912413423635,
91.8548133529282));
#182186=CARTESIAN_POINT('Ctrl Pts',(-5.20706574932211,-6.18458685574747,
92.0663699733101));
#182187=CARTESIAN_POINT('Ctrl Pts',(-1.64415034353059,-7.9295991533635,
92.2250374385965));
#182188=CARTESIAN_POINT('Ctrl Pts',(2.3621462120266,-7.74783730401467,92.383704903883));
#182189=CARTESIAN_POINT('Ctrl Pts',(5.7701232639135,-5.67416117964458,92.5423723691693));
#182190=CARTESIAN_POINT('Ctrl Pts',(7.78635899964589,-2.23188958977203,
92.7010398344559));
#182191=CARTESIAN_POINT('Ctrl Pts',(7.90091319144752,1.77689162371117,92.8597072997422));
#182192=CARTESIAN_POINT('Ctrl Pts',(6.09639927576183,5.31004370259175,93.0183747650287));
#182193=CARTESIAN_POINT('Ctrl Pts',(1.70856436375901,8.39638260574568,93.2299313854105));
#182194=CARTESIAN_POINT('Ctrl Pts',(-4.03517086418892,7.54934216757803,
93.4414880057924));
#182195=CARTESIAN_POINT('Ctrl Pts',(-7.34733543081567,3.36365116970041,
93.6530446261744));
#182196=CARTESIAN_POINT('Ctrl Pts',(-8.35138479902285,-1.87870792778163,
93.8646012465563));
#182197=CARTESIAN_POINT('Ctrl Pts',(-5.23927076021774,-6.78000543317708,
94.0761578669382));
#182198=CARTESIAN_POINT('Ctrl Pts',(-0.03576071327238,-8.08463795065846,
94.2877144873201));
#182199=CARTESIAN_POINT('Ctrl Pts',(3.81787759158665,-7.14181922308119,
94.4463819526065));
#182200=CARTESIAN_POINT('Ctrl Pts',(6.77751790271065,-4.43553491019332,
94.605049417893));
#182201=CARTESIAN_POINT('Ctrl Pts',(8.06566255744928,-0.659938011645058,
94.7637168831795));
#182202=CARTESIAN_POINT('Ctrl Pts',(7.40838573974634,3.27483184211492,94.9223843484658));
#182203=CARTESIAN_POINT('Ctrl Pts',(4.9280259771172,6.42622521736914,95.0810518137522));
#182204=CARTESIAN_POINT('Ctrl Pts',(1.27889791082725,7.98291927025678,95.2397192790387));
#182205=CARTESIAN_POINT('Ctrl Pts',(-4.0674715610131,7.54149967463055,95.4512758994206));
#182206=CARTESIAN_POINT('Ctrl Pts',(-7.93492590795773,3.21124827752124,
95.6628325198024));
#182207=CARTESIAN_POINT('Ctrl Pts',(-7.79637889098973,-2.1245596921605,
95.8743891401844));
#182208=CARTESIAN_POINT('Ctrl Pts',(-5.20869192738245,-6.79305464430902,
96.0859457605662));
#182209=CARTESIAN_POINT('Ctrl Pts',(0.32101919849777,-8.56233974141997,
96.2975023809482));
#182210=CARTESIAN_POINT('Ctrl Pts',(5.15210277886213,-6.23053426315196,
96.5090590013301));
#182211=CARTESIAN_POINT('Ctrl Pts',(7.50709055485341,-3.03731311627524,
96.6677264666165));
#182212=CARTESIAN_POINT('Ctrl Pts',(8.04540311654855,0.935991074457848,
96.826393931903));
#182213=CARTESIAN_POINT('Ctrl Pts',(6.61610676550725,4.66172204925334,96.9850613971894));
#182214=CARTESIAN_POINT('Ctrl Pts',(3.58945996231984,7.25896364534505,97.1437288624758));
#182215=CARTESIAN_POINT('Ctrl Pts',(-0.331984144423014,8.09484453530492,
97.3023963277622));
#182216=CARTESIAN_POINT('Ctrl Pts',(-4.13483212670458,6.9426376342695,97.4610637930487));
#182217=CARTESIAN_POINT('Ctrl Pts',(-7.94945653522564,3.19785807260161,
97.6726204134305));
#182218=CARTESIAN_POINT('Ctrl Pts',(-8.21167960970159,-4.09854069807359,
97.937066188908));
#182219=CARTESIAN_POINT('Ctrl Pts',(-2.22263135552021,-8.275446197766,98.2015119643853));
#182220=CARTESIAN_POINT('Ctrl Pts',(3.06251395333299,-7.47745566371039,
98.4130685847673));
#182221=CARTESIAN_POINT('Ctrl Pts',(6.27029174620337,-5.13167437815679,
98.5717360500536));
#182222=CARTESIAN_POINT('Ctrl Pts',(7.95736644719291,-1.49394517189156,
98.7304035153404));
#182223=CARTESIAN_POINT('Ctrl Pts',(7.7051980908551,2.48345330633745,98.8890709806263));
#182224=CARTESIAN_POINT('Ctrl Pts',(5.57898371978856,5.87036363237872,99.0477442629553));
#182225=CARTESIAN_POINT('Ctrl Pts',(3.25605702020626,7.16952801912672,99.1535283901882));
#182226=CARTESIAN_POINT('Ctrl Pts',(2.00918284212126,7.50340179718649,99.2064233623258));
#182227=CARTESIAN_POINT('Ctrl Pts',(-6.17201598240879,5.32232153904337,
-0.657447214020203));
#182228=CARTESIAN_POINT('Ctrl Pts',(-7.05661567643055,4.2965029020642,-0.60454249319458));
#182229=CARTESIAN_POINT('Ctrl Pts',(-8.30460012783212,1.79807814514246,
-0.498748617273481));
#182230=CARTESIAN_POINT('Ctrl Pts',(-8.14915213400464,-2.39503477011331,
-0.340065586256907));
#182231=CARTESIAN_POINT('Ctrl Pts',(-6.01967976551396,-5.99363557917286,
-0.181398120970476));
#182232=CARTESIAN_POINT('Ctrl Pts',(-2.40877456199585,-8.15273538333176,
-0.0227306556840495));
#182233=CARTESIAN_POINT('Ctrl Pts',(1.75834180979301,-8.29349104933222,
0.135936809602381));
#182234=CARTESIAN_POINT('Ctrl Pts',(6.81343712395487,-5.86535701987734,
0.347493429984283));
#182235=CARTESIAN_POINT('Ctrl Pts',(9.54195894196003,1.29323553737407,0.611939205461667));
#182236=CARTESIAN_POINT('Ctrl Pts',(5.0068590584849,7.46682392155477,0.876384980939047));
#182237=CARTESIAN_POINT('Ctrl Pts',(-0.512538772618678,8.46270402481564,
1.08794160132095));
#182238=CARTESIAN_POINT('Ctrl Pts',(-4.49111326352922,7.21691544450829,
1.24660906660738));
#182239=CARTESIAN_POINT('Ctrl Pts',(-7.39881792966678,4.17677760331887,
1.40527653189381));
#182240=CARTESIAN_POINT('Ctrl Pts',(-8.49055988419928,0.137227805190378,
1.56394399718024));
#182241=CARTESIAN_POINT('Ctrl Pts',(-7.53062837975034,-3.93804937038376,
1.72261146246667));
#182242=CARTESIAN_POINT('Ctrl Pts',(-4.71796379646677,-7.06641305153905,
1.88127892775309));
#182243=CARTESIAN_POINT('Ctrl Pts',(-0.79018593232073,-8.44565265941745,
2.03994639303953));
#182244=CARTESIAN_POINT('Ctrl Pts',(4.77662445382059,-7.61591549408909,
2.25150301342142));
#182245=CARTESIAN_POINT('Ctrl Pts',(8.52816518397885,-2.81671375597811,
2.46305963380334));
#182246=CARTESIAN_POINT('Ctrl Pts',(8.01635168825888,2.76014623244002,2.67461625418524));
#182247=CARTESIAN_POINT('Ctrl Pts',(4.98635083889706,7.46985904841845,2.88617287456715));
#182248=CARTESIAN_POINT('Ctrl Pts',(-0.924520356462571,8.94234775455389,
3.09772949494905));
#182249=CARTESIAN_POINT('Ctrl Pts',(-5.82220414120115,6.16880266514092,
3.30928611533096));
#182250=CARTESIAN_POINT('Ctrl Pts',(-8.06816498152606,2.66425108595449,
3.46795358061738));
#182251=CARTESIAN_POINT('Ctrl Pts',(-8.35893323744424,-1.5334140393396,
3.62662104590382));
#182252=CARTESIAN_POINT('Ctrl Pts',(-6.60599159799001,-5.33421058304081,
3.78528851119024));
#182253=CARTESIAN_POINT('Ctrl Pts',(-3.25969653764494,-7.84840872900535,
3.94395597647667));
#182254=CARTESIAN_POINT('Ctrl Pts',(0.905036893642654,-8.44833621522575,
4.1026234417631));
#182255=CARTESIAN_POINT('Ctrl Pts',(4.80404436523976,-6.99095285530132,
4.26129090704952));
#182256=CARTESIAN_POINT('Ctrl Pts',(8.54698316019777,-2.78734255264185,
4.47284752743144));
#182257=CARTESIAN_POINT('Ctrl Pts',(8.35257952803235,3.3010470592481,4.68440414781333));
#182258=CARTESIAN_POINT('Ctrl Pts',(4.38673881922155,7.2551398805805,4.89596076819524));
#182259=CARTESIAN_POINT('Ctrl Pts',(-0.957165854837313,8.93008003688911,
5.10751738857714));
#182260=CARTESIAN_POINT('Ctrl Pts',(-6.43896908919455,6.2737451428744,5.31907400895906));
#182261=CARTESIAN_POINT('Ctrl Pts',(-8.4225586316336,1.00636408820458,5.53063062934095));
#182262=CARTESIAN_POINT('Ctrl Pts',(-7.90176052552384,-3.12340509109876,
5.68929809462739));
#182263=CARTESIAN_POINT('Ctrl Pts',(-5.43569013465026,-6.53271861328957,
5.84796555991382));
#182264=CARTESIAN_POINT('Ctrl Pts',(-1.65468776311683,-8.32796088696628,
6.00663302520024));
#182265=CARTESIAN_POINT('Ctrl Pts',(2.52542173804131,-8.11451691537931,
6.16530049048667));
#182266=CARTESIAN_POINT('Ctrl Pts',(6.10752001228779,-5.90691781284157,
6.32396795577311));
#182267=CARTESIAN_POINT('Ctrl Pts',(8.16752607455826,-2.28993022775634,
6.48263542105952));
#182268=CARTESIAN_POINT('Ctrl Pts',(8.34826776562736,3.33565979134341,6.69419204144145));
#182269=CARTESIAN_POINT('Ctrl Pts',(4.29833574721033,7.88586113839222,6.90574866182333));
#182270=CARTESIAN_POINT('Ctrl Pts',(-1.27997205123254,8.38106220513736,
7.11730528220525));
#182271=CARTESIAN_POINT('Ctrl Pts',(-6.45618537530488,6.24340984473629,
7.32886190258714));
#182272=CARTESIAN_POINT('Ctrl Pts',(-8.9633486454374,0.691796206322683,
7.54041852296907));
#182273=CARTESIAN_POINT('Ctrl Pts',(-7.11170820944491,-4.62340447823024,
7.75197514335095));
#182274=CARTESIAN_POINT('Ctrl Pts',(-4.06600105329151,-7.46063765270232,
7.91064260863739));
#182275=CARTESIAN_POINT('Ctrl Pts',(0.0117368987423702,-8.4984117320148,
8.06931007392382));
#182276=CARTESIAN_POINT('Ctrl Pts',(4.06500630606157,-7.45443813195372,
8.22797753921025));
#182277=CARTESIAN_POINT('Ctrl Pts',(7.13780493916943,-4.61247009442929,
8.38664500449667));
#182278=CARTESIAN_POINT('Ctrl Pts',(8.47384110579392,-0.622491497167233,
8.5453124697831));
#182279=CARTESIAN_POINT('Ctrl Pts',(7.73823666162773,3.47447204539893,8.70397993506954));
#182280=CARTESIAN_POINT('Ctrl Pts',(4.27284971438061,7.90967485102876,8.91553655545142));
#182281=CARTESIAN_POINT('Ctrl Pts',(-1.75193518088393,8.80870133514469,
9.12709317583335));
#182282=CARTESIAN_POINT('Ctrl Pts',(-6.3522996305101,5.61505312017836,9.33864979621524));
#182283=CARTESIAN_POINT('Ctrl Pts',(-8.95713255407061,0.657474333040693,
9.55020641659717));
#182284=CARTESIAN_POINT('Ctrl Pts',(-7.32539921461132,-5.21140358034675,
9.76176303697903));
#182285=CARTESIAN_POINT('Ctrl Pts',(-2.49837894152679,-8.10619302078068,
9.97331965736098));
#182286=CARTESIAN_POINT('Ctrl Pts',(1.65789584672137,-8.33335827333214,
10.1319871226474));
#182287=CARTESIAN_POINT('Ctrl Pts',(5.45371364459879,-6.51767958742603,
10.2906545879339));
#182288=CARTESIAN_POINT('Ctrl Pts',(7.89702487857384,-3.11928232108554,
10.4493220532203));
#182289=CARTESIAN_POINT('Ctrl Pts',(8.43559070412863,1.03147912923697,10.6079895185067));
#182290=CARTESIAN_POINT('Ctrl Pts',(6.90514684855951,4.95100249950638,10.7666569837931));
#182291=CARTESIAN_POINT('Ctrl Pts',(3.71552607525479,7.62542645428566,10.9253244490795));
#182292=CARTESIAN_POINT('Ctrl Pts',(-1.78676051222955,8.8106576260014,11.1368810694615));
#182293=CARTESIAN_POINT('Ctrl Pts',(-6.98865629795398,5.64102643486689,
11.3484376898434));
#182294=CARTESIAN_POINT('Ctrl Pts',(-8.47479651957782,0.241570051858162,
11.5599943102253));
#182295=CARTESIAN_POINT('Ctrl Pts',(-7.29863731965333,-5.23377391238505,
11.7715509306072));
#182296=CARTESIAN_POINT('Ctrl Pts',(-2.28573880064005,-8.69457296627776,
11.9831075509891));
#182297=CARTESIAN_POINT('Ctrl Pts',(3.27512779064737,-7.82469172431395,
12.194664171371));
#182298=CARTESIAN_POINT('Ctrl Pts',(6.61191217838697,-5.33629985060691,
12.3533316366574));
#182299=CARTESIAN_POINT('Ctrl Pts',(8.36313795743936,-1.51031891548454,
12.5119991019438));
#182300=CARTESIAN_POINT('Ctrl Pts',(8.06188546056129,2.66438115746247,12.6706665672303));
#182301=CARTESIAN_POINT('Ctrl Pts',(5.8161235376237,6.19643822826732,12.8293340325167));
#182302=CARTESIAN_POINT('Ctrl Pts',(2.129895080009,8.22538909100614,12.9880014978031));
#182303=CARTESIAN_POINT('Ctrl Pts',(-2.03257114030819,8.23534560204998,
13.1466689630895));
#182304=CARTESIAN_POINT('Ctrl Pts',(-7.01664901574451,5.62021685707332,
13.3582255834715));
#182305=CARTESIAN_POINT('Ctrl Pts',(-8.98004044570451,-0.146183731344905,
13.5697822038533));
#182306=CARTESIAN_POINT('Ctrl Pts',(-6.66183439050809,-5.24409140763651,
13.7813388242353));
#182307=CARTESIAN_POINT('Ctrl Pts',(-2.25085857932651,-8.69460359911083,
13.9928954446172));
#182308=CARTESIAN_POINT('Ctrl Pts',(3.81535492978966,-8.14022528499111,
14.2044520649991));
#182309=CARTESIAN_POINT('Ctrl Pts',(7.52775656787826,-3.90962193573543,
14.416008685381));
#182310=CARTESIAN_POINT('Ctrl Pts',(8.49554099697729,0.138787315586332,
14.5746761506674));
#182311=CARTESIAN_POINT('Ctrl Pts',(7.38895437261531,4.19839171600769,14.7333436159538));
#182312=CARTESIAN_POINT('Ctrl Pts',(4.48303139811294,7.21078037489595,14.8920110812403));
#182313=CARTESIAN_POINT('Ctrl Pts',(0.495810896673869,8.48394432303586,
15.0506785465267));
#182314=CARTESIAN_POINT('Ctrl Pts',(-3.63442052989092,7.68013451459002,
15.2093460118131));
#182315=CARTESIAN_POINT('Ctrl Pts',(-6.83679903633618,5.02100005600181,
15.3680134770995));
#182316=CARTESIAN_POINT('Ctrl Pts',(-8.9882015129228,-0.180095790543731,
15.5795700974815));
#182317=CARTESIAN_POINT('Ctrl Pts',(-6.80134439463898,-5.86551025191433,
15.7911267178633));
#182318=CARTESIAN_POINT('Ctrl Pts',(-1.75530226611185,-8.2945431515416,
16.0026833382453));
#182319=CARTESIAN_POINT('Ctrl Pts',(3.84215607599829,-8.11790199358606,
16.2142399586272));
#182320=CARTESIAN_POINT('Ctrl Pts',(8.14470429666455,-3.80578413084255,
16.4257965790091));
#182321=CARTESIAN_POINT('Ctrl Pts',(8.28470525379816,1.82096718347887,16.637353199391));
#182322=CARTESIAN_POINT('Ctrl Pts',(6.43407764099153,5.5494255252217,16.7960206646774));
#182323=CARTESIAN_POINT('Ctrl Pts',(2.98354656274481,7.95748638890239,16.9546881299639));
#182324=CARTESIAN_POINT('Ctrl Pts',(-1.17761734855467,8.40869439995495,
17.1133555952503));
#182325=CARTESIAN_POINT('Ctrl Pts',(-5.05474248930127,6.83174341500656,
17.2720230605367));
#182326=CARTESIAN_POINT('Ctrl Pts',(-7.7110126626523,3.56843978045104,17.4306905258231));
#182327=CARTESIAN_POINT('Ctrl Pts',(-8.46620823782832,-0.524957807205056,
17.5893579911096));
#182328=CARTESIAN_POINT('Ctrl Pts',(-6.78588403939986,-5.89677697852795,
17.8009146114915));
#182329=CARTESIAN_POINT('Ctrl Pts',(-1.46429379529528,-8.86105748603732,
18.0124712318734));
#182330=CARTESIAN_POINT('Ctrl Pts',(3.96634324971134,-7.49324051153254,
18.2240278522553));
#182331=CARTESIAN_POINT('Ctrl Pts',(8.15098066334341,-3.77147322880607,
18.4355844726372));
#182332=CARTESIAN_POINT('Ctrl Pts',(8.69188026264128,2.29595697489877,18.6471410930191));
#182333=CARTESIAN_POINT('Ctrl Pts',(5.19446800099358,6.70594995599219,18.858697713401));
#182334=CARTESIAN_POINT('Ctrl Pts',(1.38480816870057,8.38306537527828,19.0173651786874));
#182335=CARTESIAN_POINT('Ctrl Pts',(-2.80733701627989,8.02134643302842,
19.1760326439739));
#182336=CARTESIAN_POINT('Ctrl Pts',(-6.29141345945949,5.70184538667814,
19.3347001092603));
#182337=CARTESIAN_POINT('Ctrl Pts',(-8.25801451366162,2.00707150191196,
19.4933675745467));
#182338=CARTESIAN_POINT('Ctrl Pts',(-8.20682568737216,-2.20033881195099,
19.6520350398332));
#182339=CARTESIAN_POINT('Ctrl Pts',(-6.16414657957517,-5.8271399134678,
19.8107025051195));
#182340=CARTESIAN_POINT('Ctrl Pts',(-1.43239137515728,-8.87515948471095,
20.0222591255015));
#182341=CARTESIAN_POINT('Ctrl Pts',(4.5527339820946,-7.74177688764536,20.2338157458833));
#182342=CARTESIAN_POINT('Ctrl Pts',(7.84612963947235,-3.21228607362366,
20.4453723662653));
#182343=CARTESIAN_POINT('Ctrl Pts',(8.67471728024408,2.32632246209199,20.6569289866471));
#182344=CARTESIAN_POINT('Ctrl Pts',(5.20278957783041,7.33151972918976,20.8684856070291));
#182345=CARTESIAN_POINT('Ctrl Pts',(-0.307935242075415,8.47687669559407,
21.080042227411));
#182346=CARTESIAN_POINT('Ctrl Pts',(-4.30752757465816,7.32384359089192,
21.2387096926974));
#182347=CARTESIAN_POINT('Ctrl Pts',(-7.29457162247705,4.36031702588079,
21.3973771579839));
#182348=CARTESIAN_POINT('Ctrl Pts',(-8.48365271897988,0.347218483372963,
21.5560446232702));
#182349=CARTESIAN_POINT('Ctrl Pts',(-7.62649503422331,-3.74962841020285,
21.7147120885567));
#182350=CARTESIAN_POINT('Ctrl Pts',(-4.89161787082002,-6.94734145959187,
21.8733795538431));
#182351=CARTESIAN_POINT('Ctrl Pts',(-0.999627257628274,-8.42336084775099,
22.0320470191296));
#182352=CARTESIAN_POINT('Ctrl Pts',(4.58626387344269,-7.73216558370512,
22.2436036395115));
#182353=CARTESIAN_POINT('Ctrl Pts',(8.45559914028475,-3.02743113358754,
22.4551602598934));
#182354=CARTESIAN_POINT('Ctrl Pts',(8.08239236753771,2.56036437941381,22.6667168802753));
#182355=CARTESIAN_POINT('Ctrl Pts',(5.17015725645673,7.343838916623,22.8782735006572));
#182356=CARTESIAN_POINT('Ctrl Pts',(-0.702331405317825,8.96252930415199,
23.0898301210391));
#182357=CARTESIAN_POINT('Ctrl Pts',(-5.66734195152509,6.31137844136298,
23.301386741421));
#182358=CARTESIAN_POINT('Ctrl Pts',(-7.99956771205129,2.86363321160307,
23.4600542067074));
#182359=CARTESIAN_POINT('Ctrl Pts',(-8.39441071908186,-1.32552193531339,
23.6187216719939));
#182360=CARTESIAN_POINT('Ctrl Pts',(-6.73632038848893,-5.16864699462819,
23.7773891372803));
#182361=CARTESIAN_POINT('Ctrl Pts',(-3.45344407495777,-7.76510552038876,
23.9360566025667));
#182362=CARTESIAN_POINT('Ctrl Pts',(0.695120786446635,-8.46819259597579,
24.0947240678531));
#182363=CARTESIAN_POINT('Ctrl Pts',(4.62909106859212,-7.10800805460281,
24.2533915331396));
#182364=CARTESIAN_POINT('Ctrl Pts',(8.47518615693812,-2.99856974838409,
24.4649481535214));
#182365=CARTESIAN_POINT('Ctrl Pts',(8.43192000758649,3.09276915974365,24.6765047739034));
#182366=CARTESIAN_POINT('Ctrl Pts',(4.56541761580388,7.144053060519,24.8880613942853));
#182367=CARTESIAN_POINT('Ctrl Pts',(-0.735279526212941,8.95108150494292,
25.0996180146672));
#182368=CARTESIAN_POINT('Ctrl Pts',(-6.28130928209251,6.43159036579426,
25.311174635049));
#182369=CARTESIAN_POINT('Ctrl Pts',(-8.39499320342797,1.2150521552657,25.522731255431));
#182370=CARTESIAN_POINT('Ctrl Pts',(-7.97683182846663,-2.92636852270024,
25.6813987207174));
#182371=CARTESIAN_POINT('Ctrl Pts',(-5.59611972016833,-6.39582549786784,
25.8400661860039));
#182372=CARTESIAN_POINT('Ctrl Pts',(-1.86082884370897,-8.28433703719686,
25.9987336512902));
#182373=CARTESIAN_POINT('Ctrl Pts',(2.32328994584553,-8.17468430883825,
26.1574011165767));
#182374=CARTESIAN_POINT('Ctrl Pts',(5.95906474753433,-6.05665139206334,
26.3160685818631));
#182375=CARTESIAN_POINT('Ctrl Pts',(8.10818867535513,-2.49189466680684,
26.4747360471496));
#182376=CARTESIAN_POINT('Ctrl Pts',(8.42846848557864,3.1274782042865,26.6862926675315));
#182377=CARTESIAN_POINT('Ctrl Pts',(4.49269251246894,7.77677375768411,26.8978492879134));
#182378=CARTESIAN_POINT('Ctrl Pts',(-1.07160968069293,8.41024285204944,
27.1094059082953));
#182379=CARTESIAN_POINT('Ctrl Pts',(-6.29927301456852,6.40169161844959,
27.3209625286772));
#182380=CARTESIAN_POINT('Ctrl Pts',(-8.94342240549927,0.91400033232656,
27.5325191490591));
#182381=CARTESIAN_POINT('Ctrl Pts',(-7.22424387033608,-4.44551044622881,
27.744075769441));
#182382=CARTESIAN_POINT('Ctrl Pts',(-4.24987783380582,-7.35744637411753,
27.9027432347274));
#182383=CARTESIAN_POINT('Ctrl Pts',(-0.199146880524199,-8.49608617197416,
28.0614107000139));
#182384=CARTESIAN_POINT('Ctrl Pts',(3.87877969046034,-7.55301213055581,
28.2200781653003));
#182385=CARTESIAN_POINT('Ctrl Pts',(7.02115294620548,-4.78816781531549,
28.3787456305867));
#182386=CARTESIAN_POINT('Ctrl Pts',(8.45578532500763,-0.832570289930731,
28.5374130958732));
#182387=CARTESIAN_POINT('Ctrl Pts',(7.82206971680332,3.28138506900459,28.6960805611595));
#182388=CARTESIAN_POINT('Ctrl Pts',(4.46780524230699,7.80121254982153,28.9076371815415));
#182389=CARTESIAN_POINT('Ctrl Pts',(-1.53281601878551,8.84946163008538,
29.1191938019234));
#182390=CARTESIAN_POINT('Ctrl Pts',(-6.21101134428347,5.77095054730025,
29.3307504223052));
#182391=CARTESIAN_POINT('Ctrl Pts',(-8.93805989346455,0.879534780801609,
29.5423070426872));
#182392=CARTESIAN_POINT('Ctrl Pts',(-7.45245972615058,-5.02802595068711,
29.7538636630691));
#182393=CARTESIAN_POINT('Ctrl Pts',(-2.69875727328044,-8.04170204655293,
29.965420283451));
#182394=CARTESIAN_POINT('Ctrl Pts',(1.45060083585998,-8.37193143577347,
30.1240877487374));
#182395=CARTESIAN_POINT('Ctrl Pts',(5.29030421332727,-6.6510015074487,30.2827552140239));
#182396=CARTESIAN_POINT('Ctrl Pts',(7.81719117206012,-3.31427915404184,
30.4414226793103));
#182397=CARTESIAN_POINT('Ctrl Pts',(8.45858844060299,0.821840199874878,
30.6000901445967));
#182398=CARTESIAN_POINT('Ctrl Pts',(7.02587515260265,4.77813322232961,30.7587576098831));
#182399=CARTESIAN_POINT('Ctrl Pts',(3.90359985326166,7.53088114441021,30.9174250751696));
#182400=CARTESIAN_POINT('Ctrl Pts',(-1.5675820833069,8.85228147670276,31.1289816955514));
#182401=CARTESIAN_POINT('Ctrl Pts',(-6.84652756348825,5.81270646189832,
31.3405383159334));
#182402=CARTESIAN_POINT('Ctrl Pts',(-8.46619265519094,0.451789844279516,
31.5520949363152));
#182403=CARTESIAN_POINT('Ctrl Pts',(-7.42626117055549,-5.05105346601071,
31.7636515566973));
#182404=CARTESIAN_POINT('Ctrl Pts',(-2.50078270766321,-8.63517728710487,
31.9752081770791));
#182405=CARTESIAN_POINT('Ctrl Pts',(3.07995689382489,-7.9035516166973,32.186764797461));
#182406=CARTESIAN_POINT('Ctrl Pts',(6.47746095574527,-5.49872515380471,
32.3454322627474));
#182407=CARTESIAN_POINT('Ctrl Pts',(8.32308565417483,-1.71737733620265,
32.5040997280339));
#182408=CARTESIAN_POINT('Ctrl Pts',(8.12551720871498,2.46351257807376,32.6627671933203));
#182409=CARTESIAN_POINT('Ctrl Pts',(5.96809149645942,6.05020855934091,32.8214346586068));
#182410=CARTESIAN_POINT('Ctrl Pts',(2.33334461335539,8.17000499789411,32.9801021238931));
#182411=CARTESIAN_POINT('Ctrl Pts',(-1.82759285385863,8.28324616235341,
33.1387695891796));
#182412=CARTESIAN_POINT('Ctrl Pts',(-6.87502803213741,5.79259790491315,
33.3503262095615));
#182413=CARTESIAN_POINT('Ctrl Pts',(-8.98090275711608,0.0766926138812347,
33.5618828299434));
#182414=CARTESIAN_POINT('Ctrl Pts',(-6.78991034249501,-5.07716945542322,
33.7734394503253));
#182415=CARTESIAN_POINT('Ctrl Pts',(-2.46591398666662,-8.63607343068368,
33.9849960707071));
#182416=CARTESIAN_POINT('Ctrl Pts',(3.61218801699627,-8.23239325230199,
34.1965526910891));
#182417=CARTESIAN_POINT('Ctrl Pts',(7.42842502431126,-4.09521236125845,
34.408109311471));
#182418=CARTESIAN_POINT('Ctrl Pts',(8.49636895854652,-0.072064349971219,
34.5667767767574));
#182419=CARTESIAN_POINT('Ctrl Pts',(7.49085836935161,4.01374894729953,34.7254442420439));
#182420=CARTESIAN_POINT('Ctrl Pts',(4.66057979270806,7.09731781219159,34.8841117073303));
#182421=CARTESIAN_POINT('Ctrl Pts',(0.706179398388318,8.46902889231848,
35.0427791726167));
#182422=CARTESIAN_POINT('Ctrl Pts',(-3.44272605335546,7.76795443291458,
35.2014466379032));
#182423=CARTESIAN_POINT('Ctrl Pts',(-6.71010243784006,5.18910280292371,
35.3601141031895));
#182424=CARTESIAN_POINT('Ctrl Pts',(-8.98990280754567,0.0429935060367458,
35.5716707235715));
#182425=CARTESIAN_POINT('Ctrl Pts',(-6.94479731857069,-5.69493514394782,
35.7832273439534));
#182426=CARTESIAN_POINT('Ctrl Pts',(-1.96058313627431,-8.24843293625886,
35.9947839643353));
#182427=CARTESIAN_POINT('Ctrl Pts',(3.63953484236017,-8.21074188006452,
36.2063405847172));
#182428=CARTESIAN_POINT('Ctrl Pts',(8.04775942311691,-4.00671551252553,
36.4178972050991));
#182429=CARTESIAN_POINT('Ctrl Pts',(8.32733986051514,1.61482923960804,36.629453825481));
#182430=CARTESIAN_POINT('Ctrl Pts',(6.56980030452289,5.3880611270642,36.7881212907674));
#182431=CARTESIAN_POINT('Ctrl Pts',(3.18008548698482,7.88100222161509,36.9467887560539));
#182432=CARTESIAN_POINT('Ctrl Pts',(-0.968600827556462,8.43532670193088,
37.1054562213403));
#182433=CARTESIAN_POINT('Ctrl Pts',(-4.8836627066618,6.95506853231466,37.2641236866267));
#182434=CARTESIAN_POINT('Ctrl Pts',(-7.62009080867894,3.75868259071931,
37.4227911519132));
#182435=CARTESIAN_POINT('Ctrl Pts',(-8.47662769221309,-0.314715098500337,
37.5814586171996));
#182436=CARTESIAN_POINT('Ctrl Pts',(-6.9301175785037,-5.72657587732783,
37.7930152375815));
#182437=CARTESIAN_POINT('Ctrl Pts',(-1.68372179686536,-8.82199393564511,
38.0045718579634));
#182438=CARTESIAN_POINT('Ctrl Pts',(3.7791841692025,-7.58935433047188,38.2161284783453));
#182439=CARTESIAN_POINT('Ctrl Pts',(8.05488525025052,-3.97257091756658,
38.4276850987272));
#182440=CARTESIAN_POINT('Ctrl Pts',(8.74617592240978,2.07956910559353,38.6392417191091));
#182441=CARTESIAN_POINT('Ctrl Pts',(5.3592704363355,6.57498920271645,38.850798339491));
#182442=CARTESIAN_POINT('Ctrl Pts',(1.59239971653258,8.34612136822109,39.0094658047774));
#182443=CARTESIAN_POINT('Ctrl Pts',(-2.60743035661901,8.08853798019237,
39.1681332700639));
#182444=CARTESIAN_POINT('Ctrl Pts',(-6.14799025189356,5.85620525545962,
39.3268007353503));
#182445=CARTESIAN_POINT('Ctrl Pts',(-8.20566812724701,2.21136842410207,
39.4854682006367));
#182446=CARTESIAN_POINT('Ctrl Pts',(-8.25889802781082,-1.99601656218376,
39.6441356659231));
#182447=CARTESIAN_POINT('Ctrl Pts',(-6.30684358297493,-5.67238809017028,
39.8028031312096));
#182448=CARTESIAN_POINT('Ctrl Pts',(-1.65217912795724,-8.83688322089987,
40.0143597515915));
#182449=CARTESIAN_POINT('Ctrl Pts',(4.35922714377091,-7.85236491757794,
40.2259163719734));
#182450=CARTESIAN_POINT('Ctrl Pts',(7.76400380301161,-3.4059913512846,40.4374729923552));
#182451=CARTESIAN_POINT('Ctrl Pts',(8.72977171603534,2.11035112616518,40.6490296127373));
#182452=CARTESIAN_POINT('Ctrl Pts',(5.38311238161584,7.2001598605569,40.8605862331191));
#182453=CARTESIAN_POINT('Ctrl Pts',(-0.097494630340501,8.48190765233122,
41.072142853501));
#182454=CARTESIAN_POINT('Ctrl Pts',(-4.12446686458516,7.42847574090534,
41.2308103187874));
#182455=CARTESIAN_POINT('Ctrl Pts',(-7.18412830183364,4.53998240794474,
41.3894777840739));
#182456=CARTESIAN_POINT('Ctrl Pts',(-8.47242456027463,0.557625503242588,
41.5481452493602));
#182457=CARTESIAN_POINT('Ctrl Pts',(-7.71719024518532,-3.55922947297612,
41.7068127146468));
#182458=CARTESIAN_POINT('Ctrl Pts',(-5.06250346381941,-6.82382132159638,
41.8654801799331));
#182459=CARTESIAN_POINT('Ctrl Pts',(-1.208337303577,-8.39596233831067,42.0241476452196));
#182460=CARTESIAN_POINT('Ctrl Pts',(4.39298520629619,-7.84358858612854,
42.2357042656015));
#182461=CARTESIAN_POINT('Ctrl Pts',(8.37787264113882,-3.23631674862855,
42.4472608859834));
#182462=CARTESIAN_POINT('Ctrl Pts',(8.14343672196345,2.35901896868263,42.6588175063653));
#182463=CARTESIAN_POINT('Ctrl Pts',(5.35079579724299,7.2132849954259,42.8703741267472));
#182464=CARTESIAN_POINT('Ctrl Pts',(-0.479718335406196,8.97719729348602,
43.0819307471292));
#182465=CARTESIAN_POINT('Ctrl Pts',(-5.50898591167253,6.45006487238597,
43.293487367511));
#182466=CARTESIAN_POINT('Ctrl Pts',(-7.92604612433575,3.06125326752493,
43.4521548327974));
#182467=CARTESIAN_POINT('Ctrl Pts',(-8.4247175354972,-1.11681430749398,
43.6108222980838));
#182468=CARTESIAN_POINT('Ctrl Pts',(-6.86250131878953,-4.99989997390344,
43.7694897633703));
#182469=CARTESIAN_POINT('Ctrl Pts',(-3.64506456463047,-7.67702051869797,
43.9281572286567));
#182470=CARTESIAN_POINT('Ctrl Pts',(0.484776453906018,-8.48283388042666,
44.0868246939431));
#182471=CARTESIAN_POINT('Ctrl Pts',(4.45128707980494,-7.22068595266879,
44.2454921592296));
#182472=CARTESIAN_POINT('Ctrl Pts',(8.39816984408708,-3.20795030561121,
44.4570487796115));
#182473=CARTESIAN_POINT('Ctrl Pts',(8.50606777116889,2.88258665185232,44.6686053999934));
#182474=CARTESIAN_POINT('Ctrl Pts',(4.74128497666517,7.02856665815852,44.8801620203753));
#182475=CARTESIAN_POINT('Ctrl Pts',(-0.51294065087776,8.96657071718121,
45.0917186407571));
#182476=CARTESIAN_POINT('Ctrl Pts',(-6.11978069739963,6.58547456624455,
45.3032752611392));
#182477=CARTESIAN_POINT('Ctrl Pts',(-8.36225853595016,1.4229922505889,45.5148318815209));
#182478=CARTESIAN_POINT('Ctrl Pts',(-8.04698931459037,-2.72753043001754,
45.6734993468075));
#182479=CARTESIAN_POINT('Ctrl Pts',(-5.75310580212732,-6.25499239713214,
45.8321668120938));
#182480=CARTESIAN_POINT('Ctrl Pts',(-2.06581869166397,-8.23561375568526,
45.9908342773804));
#182481=CARTESIAN_POINT('Ctrl Pts',(2.11971744252928,-8.22981305731506,
46.1495017426667));
#182482=CARTESIAN_POINT('Ctrl Pts',(5.80695827124323,-6.20266331091412,
46.3081692079531));
#182483=CARTESIAN_POINT('Ctrl Pts',(8.04382478280886,-2.69230981459282,
46.4668366732396));
#182484=CARTESIAN_POINT('Ctrl Pts',(8.50355374697948,2.9173373785056,46.6783932936214));
#182485=CARTESIAN_POINT('Ctrl Pts',(4.68413887105522,7.66296078718693,46.8899499140035));
#182486=CARTESIAN_POINT('Ctrl Pts',(-0.862418275557941,8.43416932904131,
47.1015065343852));
#182487=CARTESIAN_POINT('Ctrl Pts',(-6.13889939658387,6.55621610061593,
47.3130631547673));
#182488=CARTESIAN_POINT('Ctrl Pts',(-8.91715105499881,1.13527081630686,
47.524619775149));
#182489=CARTESIAN_POINT('Ctrl Pts',(-7.33336423065867,-4.26442109322725,
47.7361763955311));
#182490=CARTESIAN_POINT('Ctrl Pts',(-4.42895873448593,-7.25068884785307,
47.8948438608174));
#182491=CARTESIAN_POINT('Ctrl Pts',(-0.414139927621501,-8.48665355620754,
48.0535113261039));
#182492=CARTESIAN_POINT('Ctrl Pts',(3.69814652203495,-7.65047939402318,
48.2121787913904));
#182493=CARTESIAN_POINT('Ctrl Pts',(6.88569527407017,-4.95441811708111,
48.3708462566766));
#182494=CARTESIAN_POINT('Ctrl Pts',(8.97817226161953,0.247819711134177,
48.5824028770587));
#182495=CARTESIAN_POINT('Ctrl Pts',(6.20633671998026,7.37075419636882,48.8468486525359));
#182496=CARTESIAN_POINT('Ctrl Pts',(-2.85224887117413,9.20622344841131,
49.1641835831089));
#182497=CARTESIAN_POINT('Ctrl Pts',(-8.17586019302007,3.71558748174298,
49.4286293585863));
#182498=CARTESIAN_POINT('Ctrl Pts',(-8.26990206276113,-1.88382351173266,
49.6401859789681));
#182499=CARTESIAN_POINT('Ctrl Pts',(-6.38190782755159,-5.61929274005956,
49.7988534442546));
#182500=CARTESIAN_POINT('Ctrl Pts',(-2.91689738088643,-7.96447915796828,
49.957520909541));
#182501=CARTESIAN_POINT('Ctrl Pts',(2.65202034096889,-8.58081155893773,
50.1690775299229));
#182502=CARTESIAN_POINT('Ctrl Pts',(8.76699052457919,-3.99508362442263,
50.4335233054003));
#182503=CARTESIAN_POINT('Ctrl Pts',(8.10419147421929,5.22260796336014,50.7508582359731));
#182504=CARTESIAN_POINT('Ctrl Pts',(1.37159143871236,8.874804986452,51.0153040114506));
#182505=CARTESIAN_POINT('Ctrl Pts',(-4.02714773549846,7.45728686713406,
51.2268606318324));
#182506=CARTESIAN_POINT('Ctrl Pts',(-8.18910127503122,3.69908206285886,
51.4384172522143));
#182507=CARTESIAN_POINT('Ctrl Pts',(-8.66855129374023,-2.37337160374202,
51.6499738725964));
#182508=CARTESIAN_POINT('Ctrl Pts',(-5.13571306658545,-6.75184376042308,
51.8615304929781));
#182509=CARTESIAN_POINT('Ctrl Pts',(-1.3095180133245,-8.39509522717736,
52.0201979582646));
#182510=CARTESIAN_POINT('Ctrl Pts',(2.87827190579938,-7.99602505259151,
52.178865423551));
#182511=CARTESIAN_POINT('Ctrl Pts',(6.34208622339921,-5.64564105789136,
52.3375328888374));
#182512=CARTESIAN_POINT('Ctrl Pts',(8.27545483497107,-1.93349562876361,
52.4962003541239));
#182513=CARTESIAN_POINT('Ctrl Pts',(8.18696759196887,2.27328395429753,52.6548678194103));
#182514=CARTESIAN_POINT('Ctrl Pts',(6.11202192701451,5.88176726535637,52.8135352846966));
#182515=CARTESIAN_POINT('Ctrl Pts',(1.35337035089401,8.88755422499004,53.0250919050788));
#182516=CARTESIAN_POINT('Ctrl Pts',(-4.62145954539154,7.7009546273047,53.2366485254604));
#182517=CARTESIAN_POINT('Ctrl Pts',(-7.87440234716974,3.14233340779931,
53.4482051458425));
#182518=CARTESIAN_POINT('Ctrl Pts',(-8.6536742615346,-2.40342925122091,
53.6597617662243));
#182519=CARTESIAN_POINT('Ctrl Pts',(-5.13733632629595,-7.37753080297155,
53.8713183866063));
#182520=CARTESIAN_POINT('Ctrl Pts',(0.383360766010533,-8.4738005541894,
54.0828750069881));
#182521=CARTESIAN_POINT('Ctrl Pts',(4.37253465287558,-7.28521951823731,
54.2415424722746));
#182522=CARTESIAN_POINT('Ctrl Pts',(7.33308640359521,-4.29522760314234,
54.400209937561));
#182523=CARTESIAN_POINT('Ctrl Pts',(8.48640689467772,-0.271705983052308,
54.5588774028474));
#182524=CARTESIAN_POINT('Ctrl Pts',(7.59282381463648,3.81735056487313,54.7175448681339));
#182525=CARTESIAN_POINT('Ctrl Pts',(4.82959756664542,6.99059842741678,54.8762123334202));
#182526=CARTESIAN_POINT('Ctrl Pts',(0.924625456828362,8.43192329054703,
55.0348797987068));
#182527=CARTESIAN_POINT('Ctrl Pts',(-4.65489327796069,7.69104475199265,
55.2464364190885));
#182528=CARTESIAN_POINT('Ctrl Pts',(-8.48220639133452,2.95206214867202,
55.4579930394708));
#182529=CARTESIAN_POINT('Ctrl Pts',(-8.0592867972206,-2.63219080227642,
55.6695496598523));
#182530=CARTESIAN_POINT('Ctrl Pts',(-5.10459733409883,-7.38955899671512,
55.8811062802345));
#182531=CARTESIAN_POINT('Ctrl Pts',(0.782064028799498,-8.95592411694139,
56.0926629006161));
#182532=CARTESIAN_POINT('Ctrl Pts',(5.72328451496193,-6.26069301120408,
56.3042195209983));
#182533=CARTESIAN_POINT('Ctrl Pts',(8.0247353255809,-2.79232908323465,56.4628869862845));
#182534=CARTESIAN_POINT('Ctrl Pts',(8.38228205579894,1.40017400928179,56.6215544515712));
#182535=CARTESIAN_POINT('Ctrl Pts',(6.69005617785998,5.22839100197216,56.7802219168573));
#182536=CARTESIAN_POINT('Ctrl Pts',(3.38420314471914,7.79553133510935,56.9388893821439));
#182537=CARTESIAN_POINT('Ctrl Pts',(-0.770454432796781,8.46167115392818,
57.0975568474303));
#182538=CARTESIAN_POINT('Ctrl Pts',(-4.69216421046836,7.06653080710174,
57.2562243127168));
#182539=CARTESIAN_POINT('Ctrl Pts',(-8.50153577951395,2.92302759483824,
57.4677809330986));
#182540=CARTESIAN_POINT('Ctrl Pts',(-8.40406255692474,-3.16768505839187,
57.6793375534805));
#182541=CARTESIAN_POINT('Ctrl Pts',(-4.50165959757123,-7.18439927939594,
57.8908941738625));
#182542=CARTESIAN_POINT('Ctrl Pts',(0.814908966215111,-8.94418355505842,
58.1024507942443));
#182543=CARTESIAN_POINT('Ctrl Pts',(6.33829733768668,-6.37543628230751,
58.3140074146263));
#182544=CARTESIAN_POINT('Ctrl Pts',(8.40547390421308,-1.14029429149029,
58.5255640350081));
#182545=CARTESIAN_POINT('Ctrl Pts',(7.95047325203561,2.99724103451126,58.6842315002946));
#182546=CARTESIAN_POINT('Ctrl Pts',(5.53897960442787,6.44537389632009,58.8428989655811));
#182547=CARTESIAN_POINT('Ctrl Pts',(1.78703017219667,8.30056909465304,59.0015664308674));
#182548=CARTESIAN_POINT('Ctrl Pts',(-2.39594709235619,8.15368488796713,
59.1602338961539));
#182549=CARTESIAN_POINT('Ctrl Pts',(-6.01272886125954,6.00337991395397,
59.3189013614403));
#182550=CARTESIAN_POINT('Ctrl Pts',(-8.13004376622867,2.41963860624355,
59.4775688267267));
#182551=CARTESIAN_POINT('Ctrl Pts',(-8.40030228462738,-3.20236201225959,
59.6891254471087));
#182552=CARTESIAN_POINT('Ctrl Pts',(-4.42330658889043,-7.81644771686461,
59.9006820674905));
#182553=CARTESIAN_POINT('Ctrl Pts',(1.14641270476439,-8.40037320888529,
60.1122386878725));
#182554=CARTESIAN_POINT('Ctrl Pts',(6.35599428022148,-6.34537885390543,
60.3237953082543));
#182555=CARTESIAN_POINT('Ctrl Pts',(8.95120223150307,-0.834373742044771,
60.5353519286364));
#182556=CARTESIAN_POINT('Ctrl Pts',(7.1843957630033,4.50962527779835,60.7469085490181));
#182557=CARTESIAN_POINT('Ctrl Pts',(4.18423325505326,7.39497605253704,60.9055760143047));
#182558=CARTESIAN_POINT('Ctrl Pts',(0.123529587461397,8.49752200130453,
61.0642434795908));
#182559=CARTESIAN_POINT('Ctrl Pts',(-3.9458427790497,7.5181945235856,61.2229109448775));
#182560=CARTESIAN_POINT('Ctrl Pts',(-7.06348635765548,4.72549470392764,
61.3815784101638));
#182561=CARTESIAN_POINT('Ctrl Pts',(-8.46285978914737,0.757286563674393,
61.5402458754504));
#182562=CARTESIAN_POINT('Ctrl Pts',(-7.79255786233917,-3.35086624437824,
61.6989133407367));
#182563=CARTESIAN_POINT('Ctrl Pts',(-4.39820281557677,-7.84066406140013,
61.9104699611186));
#182564=CARTESIAN_POINT('Ctrl Pts',(1.61150952855133,-8.8354701702392,62.1220265815006));
#182565=CARTESIAN_POINT('Ctrl Pts',(6.26212293716273,-5.71544822897241,
62.3335832018824));
#182566=CARTESIAN_POINT('Ctrl Pts',(8.94553321178029,-0.799957278068402,
62.5451398222644));
#182567=CARTESIAN_POINT('Ctrl Pts',(7.40741858846125,5.09414868118294,62.7566964426463));
#182568=CARTESIAN_POINT('Ctrl Pts',(2.62708470693044,8.06540070723271,62.9682530630282));
#182569=CARTESIAN_POINT('Ctrl Pts',(-1.52504790634506,8.35869054539299,
63.1269205283146));
#182570=CARTESIAN_POINT('Ctrl Pts',(-5.34928412288214,6.6036580085824,63.285587993601));
#182571=CARTESIAN_POINT('Ctrl Pts',(-7.84637645075201,3.24458020775182,
63.4442554588875));
#182572=CARTESIAN_POINT('Ctrl Pts',(-8.45093966201039,-0.897083357716978,
63.6029229241739));
#182573=CARTESIAN_POINT('Ctrl Pts',(-6.98307478342027,-4.84046953501923,
63.7615903894603));
#182574=CARTESIAN_POINT('Ctrl Pts',(-3.83642553515746,-7.565322315593,63.9202578547468));
#182575=CARTESIAN_POINT('Ctrl Pts',(1.64629931106835,-8.83798051078726,
64.1318144751286));
#182576=CARTESIAN_POINT('Ctrl Pts',(6.89798558941472,-5.75154682655248,
64.3433710955106));
#182577=CARTESIAN_POINT('Ctrl Pts',(8.46987801939189,-0.376428578651072,
64.5549277158925));
#182578=CARTESIAN_POINT('Ctrl Pts',(7.38101614104786,5.11694213523958,64.7664843362744));
#182579=CARTESIAN_POINT('Ctrl Pts',(2.42383645377006,8.65709060689877,64.9780409566562));
#182580=CARTESIAN_POINT('Ctrl Pts',(-3.15017117937135,7.87582910976843,
65.1895975770382));
#182581=CARTESIAN_POINT('Ctrl Pts',(-6.52613937584308,5.44086239463559,
65.3482650423246));
#182582=CARTESIAN_POINT('Ctrl Pts',(-8.33803955603354,1.64323950891316,
65.506932507611));
#182583=CARTESIAN_POINT('Ctrl Pts',(-8.10327184848769,-2.53572661794554,
65.6655999728974));
#182584=CARTESIAN_POINT('Ctrl Pts',(-5.91401240716692,-6.10308094076339,
65.824267438184));
#182585=CARTESIAN_POINT('Ctrl Pts',(-2.26054470797334,-8.19044665287207,
65.9829349034703));
#182586=CARTESIAN_POINT('Ctrl Pts',(1.90123575674584,-8.26665381051419,
66.1416023687568));
#182587=CARTESIAN_POINT('Ctrl Pts',(6.92630597692818,-5.73118543101237,
66.3531589891386));
#182588=CARTESIAN_POINT('Ctrl Pts',(8.98122962787707,0.00323436894311558,
66.5647156095205));
#182589=CARTESIAN_POINT('Ctrl Pts',(6.74445809772123,5.13739399951818,66.7762722299025));
#182590=CARTESIAN_POINT('Ctrl Pts',(2.38896113849587,8.65767640701331,66.9878288502843));
#182591=CARTESIAN_POINT('Ctrl Pts',(-3.68530769393738,8.19992122716341,
67.1993854706664));
#182592=CARTESIAN_POINT('Ctrl Pts',(-7.46457547414581,4.02894224535407,
67.4109420910481));
#182593=CARTESIAN_POINT('Ctrl Pts',(-8.496673828314,-0.00355042726389536,
67.5696095563346));
#182594=CARTESIAN_POINT('Ctrl Pts',(-7.45484208877315,-4.0802535648032,
67.728277021621));
#182595=CARTESIAN_POINT('Ctrl Pts',(-4.59723391810387,-7.13851276063061,
67.8869444869076));
#182596=CARTESIAN_POINT('Ctrl Pts',(-0.630782818409487,-8.4749780387699,
68.0456119521938));
#182597=CARTESIAN_POINT('Ctrl Pts',(3.5117192503279,-7.73700889602476,68.2042794174804));
#182598=CARTESIAN_POINT('Ctrl Pts',(6.75601621638297,-5.12918195325416,
68.3629468827666));
#182599=CARTESIAN_POINT('Ctrl Pts',(8.98992942269384,0.0370122366584145,
68.5745035031487));
#182600=CARTESIAN_POINT('Ctrl Pts',(6.89384124450594,5.75651361375506,68.7860601235305));
#182601=CARTESIAN_POINT('Ctrl Pts',(1.8871000366735,8.26555416108259,68.9976167439125));
#182602=CARTESIAN_POINT('Ctrl Pts',(-3.7124607538397,8.1780273441093,69.2091733642944));
#182603=CARTESIAN_POINT('Ctrl Pts',(-8.08309778550766,3.93493724481097,
69.4207299846762));
#182604=CARTESIAN_POINT('Ctrl Pts',(-8.3126392144974,-1.68887297190101,
69.6322866050581));
#182605=CARTESIAN_POINT('Ctrl Pts',(-6.52159005094721,-5.4463145298152,
69.7909540703446));
#182606=CARTESIAN_POINT('Ctrl Pts',(-3.10982397965096,-7.90899074074696,
69.949621535631));
#182607=CARTESIAN_POINT('Ctrl Pts',(1.04363116001082,-8.42637277440925,
70.1082890009175));
#182608=CARTESIAN_POINT('Ctrl Pts',(4.94536470949391,-6.91133182619133,
70.2669564662039));
#182609=CARTESIAN_POINT('Ctrl Pts',(7.65323878179321,-3.69072010577144,
70.4256239314902));
#182610=CARTESIAN_POINT('Ctrl Pts',(8.47349126886064,0.390138875479095,
70.5842913967768));
#182611=CARTESIAN_POINT('Ctrl Pts',(6.87888050467731,5.78802245443554,70.7958480171586));
#182612=CARTESIAN_POINT('Ctrl Pts',(1.60514535686331,8.83662856937753,71.0074046375406));
#182613=CARTESIAN_POINT('Ctrl Pts',(-3.84657462269014,7.55542161697674,
71.2189612579225));
#182614=CARTESIAN_POINT('Ctrl Pts',(-8.08991946671398,3.90073058693897,
71.4305178783043));
#182615=CARTESIAN_POINT('Ctrl Pts',(-8.72732282085781,-2.15732179129917,
71.6420744986863));
#182616=CARTESIAN_POINT('Ctrl Pts',(-5.30054526426088,-6.62242270827973,
71.8536311190682));
#182617=CARTESIAN_POINT('Ctrl Pts',(-1.51806183608798,-8.35996214178644,
72.0122985843546));
#182618=CARTESIAN_POINT('Ctrl Pts',(2.67930960731952,-8.06501331367521,
72.1709660496411));
#182619=CARTESIAN_POINT('Ctrl Pts',(6.19986304949528,-5.80126040606293,
72.3296335149275));
#182620=CARTESIAN_POINT('Ctrl Pts',(8.22502286458498,-2.13825597127375,
72.4883009802139));
#182621=CARTESIAN_POINT('Ctrl Pts',(8.24080778333267,2.06943611364381,72.6469684455002));
#182622=CARTESIAN_POINT('Ctrl Pts',(6.25611342521144,5.72829009709764,72.8056359107867));
#182623=CARTESIAN_POINT('Ctrl Pts',(1.57347143249256,8.85123655665177,73.0171925311688));
#182624=CARTESIAN_POINT('Ctrl Pts',(-4.42893524361537,7.81325979970337,
73.2287491515504));
#182625=CARTESIAN_POINT('Ctrl Pts',(-7.79400736428803,3.3367621047398,73.4403057719326));
#182626=CARTESIAN_POINT('Ctrl Pts',(-8.71064532497189,-2.18795660659524,
73.6518623923142));
#182627=CARTESIAN_POINT('Ctrl Pts',(-5.31882267039395,-7.2477807866672,
73.8634190126964));
#182628=CARTESIAN_POINT('Ctrl Pts',(0.172973997260735,-8.48070413479266,
74.0749756330781));
#182629=CARTESIAN_POINT('Ctrl Pts',(4.19041193458728,-7.39147661626266,
74.2336430983647));
#182630=CARTESIAN_POINT('Ctrl Pts',(7.2242465776339,-4.47586875446305,74.392310563651));
#182631=CARTESIAN_POINT('Ctrl Pts',(8.47705154330805,-0.482204586819274,
74.5509780289375));
#182632=CARTESIAN_POINT('Ctrl Pts',(7.68520991709078,3.62776628958957,74.7096454942239));
#182633=CARTESIAN_POINT('Ctrl Pts',(5.00157560649177,6.86860394860821,74.8683129595104));
#182634=CARTESIAN_POINT('Ctrl Pts',(1.13357108105033,8.40638324309714,75.0269804247967));
#182635=CARTESIAN_POINT('Ctrl Pts',(-4.4626138658977,7.80418339191081,75.2385370451786));
#182636=CARTESIAN_POINT('Ctrl Pts',(-8.40634190449351,3.16163120470357,
75.4500936655605));
#182637=CARTESIAN_POINT('Ctrl Pts',(-8.1221205743362,-2.43139661802582,
75.6616502859425));
#182638=CARTESIAN_POINT('Ctrl Pts',(-5.286390561127,-7.26061780601531,75.8732069063243));
#182639=CARTESIAN_POINT('Ctrl Pts',(0.559590308740241,-8.97257263091493,
76.0847635267063));
#182640=CARTESIAN_POINT('Ctrl Pts',(5.56616896121972,-6.40078321151184,
76.2963201470882));
#182641=CARTESIAN_POINT('Ctrl Pts',(7.95297533448445,-2.99059560612457,
76.4549876123746));
#182642=CARTESIAN_POINT('Ctrl Pts',(8.41444502679094,1.19174435712809,76.6136550776611));
#182643=CARTESIAN_POINT('Ctrl Pts',(6.81773384888835,5.06077358683163,76.7723225429474));
#182644=CARTESIAN_POINT('Ctrl Pts',(3.57659993657919,7.70915511682669,76.9309900082339));
#182645=CARTESIAN_POINT('Ctrl Pts',(-0.560248715186514,8.47818377528005,
77.0896574735203));
#182646=CARTESIAN_POINT('Ctrl Pts',(-4.51537004133694,7.18078658751354,
77.2483249388068));
#182647=CARTESIAN_POINT('Ctrl Pts',(-8.42638581228697,3.13308523234964,
77.4598815591886));
#182648=CARTESIAN_POINT('Ctrl Pts',(-8.48007796028266,-2.95817069780082,
77.6714381795706));
#182649=CARTESIAN_POINT('Ctrl Pts',(-4.67854763394638,-7.07048259845802,
77.8829947999524));
#182650=CARTESIAN_POINT('Ctrl Pts',(0.592716464848895,-8.9616507007412,
78.0945514203345));
#182651=CARTESIAN_POINT('Ctrl Pts',(6.1781451636225,-6.53075212114861,78.3061080407161));
#182652=CARTESIAN_POINT('Ctrl Pts',(8.37459038114081,-1.34851717590935,
78.5176646610983));
#182653=CARTESIAN_POINT('Ctrl Pts',(8.02239891340539,2.79903455221292,78.6763321263845));
#182654=CARTESIAN_POINT('Ctrl Pts',(5.69721000697799,6.30594464438302,78.834999591671));
#182655=CARTESIAN_POINT('Ctrl Pts',(1.99245080097765,8.25366972546961,78.9936670569575));
#182656=CARTESIAN_POINT('Ctrl Pts',(-2.1928832509956,8.21062742846951,79.1523345222438));
#182657=CARTESIAN_POINT('Ctrl Pts',(-5.8619091670315,6.15073163678617,79.3110019875304));
#182658=CARTESIAN_POINT('Ctrl Pts',(-8.06749931598736,2.62063301745226,
79.4696694528166));
#182659=CARTESIAN_POINT('Ctrl Pts',(-8.47717932212457,-2.99293028171761,
79.6812260731989));
#182660=CARTESIAN_POINT('Ctrl Pts',(-4.6159024442474,-7.70428067472816,
79.8927826935804));
#182661=CARTESIAN_POINT('Ctrl Pts',(0.9376122747872,-8.42623375894427,80.1043393139626));
#182662=CARTESIAN_POINT('Ctrl Pts',(6.1965825040472,-6.50114308105391,80.3158959343442));
#182663=CARTESIAN_POINT('Ctrl Pts',(8.92774180300392,-1.05623256415178,
80.5274525547263));
#182664=CARTESIAN_POINT('Ctrl Pts',(7.29408571740519,4.32996260639319,80.7390091751082));
#182665=CARTESIAN_POINT('Ctrl Pts',(4.36644429853462,7.28887117035859,80.8976766403946));
#182666=CARTESIAN_POINT('Ctrl Pts',(0.334349638121285,8.49184020346127,
81.0563441056809));
#182667=CARTESIAN_POINT('Ctrl Pts',(-3.75807080042374,7.61379195870581,
81.2150115709676));
#182668=CARTESIAN_POINT('Ctrl Pts',(-6.94405264827288,4.89931347636055,
81.3736790362538));
#182669=CARTESIAN_POINT('Ctrl Pts',(-8.44146257576306,0.967051359691387,
81.5323465015405));
#182670=CARTESIAN_POINT('Ctrl Pts',(-7.87330702839439,-3.15646939827605,
81.6910139668267));
#182671=CARTESIAN_POINT('Ctrl Pts',(-4.59140730681298,-7.72911248938867,
81.9025705872088));
#182672=CARTESIAN_POINT('Ctrl Pts',(1.39176936212274,-8.87273769095279,
82.1141272075905));
#182673=CARTESIAN_POINT('Ctrl Pts',(6.11837120677715,-5.86907709220823,
82.3256838279725));
#182674=CARTESIAN_POINT('Ctrl Pts',(8.92292854133732,-1.02168602612884,
82.5372404483544));
#182675=CARTESIAN_POINT('Ctrl Pts',(7.5315442738682,4.90877192192126,82.7487970687363));
#182676=CARTESIAN_POINT('Ctrl Pts',(2.82641118483351,7.99772858003235,82.9603536891183));
#182677=CARTESIAN_POINT('Ctrl Pts',(-1.31716520482439,8.39395940980711,
83.1190211544045));
#182678=CARTESIAN_POINT('Ctrl Pts',(-5.18377337279622,6.73436213320326,
83.2776886196911));
#182679=CARTESIAN_POINT('Ctrl Pts',(-7.76344918945897,3.43828166591109,
83.4363560849775));
#182680=CARTESIAN_POINT('Ctrl Pts',(-8.47059776649664,-0.687104940933551,
83.595023550264));
#182681=CARTESIAN_POINT('Ctrl Pts',(-7.10103631969523,-4.66570058369135,
83.7536910155502));
#182682=CARTESIAN_POINT('Ctrl Pts',(-4.02297065806388,-7.46779550536667,
83.9123584808369));
#182683=CARTESIAN_POINT('Ctrl Pts',(1.42648614053484,-8.87611053454955,
84.1239151012184));
#182684=CARTESIAN_POINT('Ctrl Pts',(6.75314231344867,-5.92094291343086,
84.3354717216008));
#182685=CARTESIAN_POINT('Ctrl Pts',(8.45792928085866,-0.586484797924657,
84.5470283419822));
#182686=CARTESIAN_POINT('Ctrl Pts',(7.50571555451649,4.93221350962116,84.7585849623646));
#182687=CARTESIAN_POINT('Ctrl Pts',(2.63790774845381,8.59427970462494,84.9701415827459));
#182688=CARTESIAN_POINT('Ctrl Pts',(-2.95376983218562,7.95157257428289,
85.1816982031284));
#182689=CARTESIAN_POINT('Ctrl Pts',(-6.38911994199167,5.60112712917077,
85.3403656684144));
#182690=CARTESIAN_POINT('Ctrl Pts',(-8.29469668035499,1.84963420776674,
85.4990331337012));
#182691=CARTESIAN_POINT('Ctrl Pts',(-8.16369841062226,-2.3338706887604,
85.6577005989873));
#182692=CARTESIAN_POINT('Ctrl Pts',(-6.06363365034946,-5.95445099702591,
85.816368064274));
#182693=CARTESIAN_POINT('Ctrl Pts',(-2.46308694812765,-8.13183137037725,
85.9750355295601));
#182694=CARTESIAN_POINT('Ctrl Pts',(1.69552102660424,-8.31128576538918,
86.1337029948468));
#182695=CARTESIAN_POINT('Ctrl Pts',(6.78195922970113,-5.90129053151531,
86.3452596152285));
#182696=CARTESIAN_POINT('Ctrl Pts',(8.97854441794314,-0.219627468278469,
86.5568162356106));
#182697=CARTESIAN_POINT('Ctrl Pts',(6.86986101179065,4.96845467090943,86.7683728559925));
#182698=CARTESIAN_POINT('Ctrl Pts',(2.6030577079444,8.59573072280125,86.9799294763743));
#182699=CARTESIAN_POINT('Ctrl Pts',(-3.48069952566048,8.28884381218191,
87.1914860967563));
#182700=CARTESIAN_POINT('Ctrl Pts',(-7.36230256281513,4.21292815025172,
87.4030427171382));
#182701=CARTESIAN_POINT('Ctrl Pts',(-8.494145663744,0.207287706792954,87.5617101824246));
#182702=CARTESIAN_POINT('Ctrl Pts',(-7.55379430950297,-3.89401223050901,
87.720377647711));
#182703=CARTESIAN_POINT('Ctrl Pts',(-4.77295389438821,-7.0222386212301,
87.8790451129976));
#182704=CARTESIAN_POINT('Ctrl Pts',(-0.840887270071041,-8.45671616649546,
88.0377125782838));
#182705=CARTESIAN_POINT('Ctrl Pts',(3.31865127076786,-7.82176658391953,
88.1963800435704));
#182706=CARTESIAN_POINT('Ctrl Pts',(6.62666005930314,-5.29524683882204,
88.3550475088568));
#182707=CARTESIAN_POINT('Ctrl Pts',(8.9880797002516,-0.186075878621066,
88.5666041292387));
#182708=CARTESIAN_POINT('Ctrl Pts',(7.03456103716749,5.5836768445321,88.7781607496206));
#182709=CARTESIAN_POINT('Ctrl Pts',(2.09162098936609,8.21618243316483,88.9897173700025));
#182710=CARTESIAN_POINT('Ctrl Pts',(-3.50838750099007,8.26763044848369,
89.2012739903845));
#182711=CARTESIAN_POINT('Ctrl Pts',(-7.9829670674822,4.13430014998594,89.4128306107662));
#182712=CARTESIAN_POINT('Ctrl Pts',(-8.35198742516224,-1.48208254680695,
89.6243872311483));
#182713=CARTESIAN_POINT('Ctrl Pts',(-6.65472716473773,-5.28281034234522,
89.7830546964346));
#182714=CARTESIAN_POINT('Ctrl Pts',(-3.30512064670134,-7.82938804967445,
89.9417221617211));
#182715=CARTESIAN_POINT('Ctrl Pts',(0.834217223173009,-8.44967489055097,
90.1003896270074));
#182716=CARTESIAN_POINT('Ctrl Pts',(4.77234369383054,-7.03191832927506,
90.259057092294));
#182717=CARTESIAN_POINT('Ctrl Pts',(7.55930044505665,-3.87949165892316,
90.4177245575803));
#182718=CARTESIAN_POINT('Ctrl Pts',(8.48056307456161,0.179756958105245,
90.5763920228666));
#182719=CARTESIAN_POINT('Ctrl Pts',(7.02038676650769,5.61554721994126,90.7879486432487));
#182720=CARTESIAN_POINT('Ctrl Pts',(1.82392380713085,8.79407744083663,90.9995052636305));
#182721=CARTESIAN_POINT('Ctrl Pts',(-3.65790945473178,7.6485443425074,91.2110618840126));
#182722=CARTESIAN_POINT('Ctrl Pts',(-7.99063545451894,4.10027329854195,
91.4226185043941));
#182723=CARTESIAN_POINT('Ctrl Pts',(-8.77816746441304,-1.9400971359493,
91.6341751247764));
#182724=CARTESIAN_POINT('Ctrl Pts',(-5.46324238590482,-6.48885546606135,
91.8457317451582));
#182725=CARTESIAN_POINT('Ctrl Pts',(-1.72503906768333,-8.31971868293201,
92.0043992104447));
#182726=CARTESIAN_POINT('Ctrl Pts',(2.47835881636955,-8.12901453450982,
92.163066675731));
#182727=CARTESIAN_POINT('Ctrl Pts',(6.05400114093271,-5.95331792480741,
92.3217341410176));
#182728=CARTESIAN_POINT('Ctrl Pts',(8.16943141620118,-2.34169384342607,
92.4804016063039));
#182729=CARTESIAN_POINT('Ctrl Pts',(8.28962143227979,1.86431093847469,92.6390690715904));
#182730=CARTESIAN_POINT('Ctrl Pts',(6.39632924340885,5.57128663696691,92.7977365368768));
#182731=CARTESIAN_POINT('Ctrl Pts',(1.79262212165266,8.80946689523861,93.0092931572587));
#182732=CARTESIAN_POINT('Ctrl Pts',(-4.23369274768137,7.92075385661886,
93.2208497776406));
#182733=CARTESIAN_POINT('Ctrl Pts',(-7.7088088150833,3.52913570259757,93.4324063980225));
#182734=CARTESIAN_POINT('Ctrl Pts',(-8.76225529146867,-1.97113638965059,
93.6439630184044));
#182735=CARTESIAN_POINT('Ctrl Pts',(-5.49703181531362,-7.11356737986656,
93.8555196387864));
#182736=CARTESIAN_POINT('Ctrl Pts',(-0.0375200648321471,-8.48238506158333,
94.0670762591681));
#182737=CARTESIAN_POINT('Ctrl Pts',(4.00570910503058,-7.49318164401645,
94.2257437244544));
#182738=CARTESIAN_POINT('Ctrl Pts',(7.11095746815531,-4.65375385910643,
94.3844111897412));
#182739=CARTESIAN_POINT('Ctrl Pts',(8.46247611910779,-0.692405567907114,
94.5430786550272));
#182740=CARTESIAN_POINT('Ctrl Pts',(7.77286267026383,3.43594665169769,94.7017461203141));
#182741=CARTESIAN_POINT('Ctrl Pts',(5.17047444629095,6.74238192468996,94.8604135856003));
#182742=CARTESIAN_POINT('Ctrl Pts',(1.34181698677152,8.37566203695453,95.0190810508868));
#182743=CARTESIAN_POINT('Ctrl Pts',(-4.26758257056428,7.91252552958314,
95.2306376712688));
#182744=CARTESIAN_POINT('Ctrl Pts',(-8.32530750260123,3.36923491002623,
95.4421942916505));
#182745=CARTESIAN_POINT('Ctrl Pts',(-8.17994426503522,-2.22908354155261,
95.6537509120326));
#182746=CARTESIAN_POINT('Ctrl Pts',(-5.46494856849098,-7.12725858462383,
95.8653075324143));
#182747=CARTESIAN_POINT('Ctrl Pts',(0.336812665012069,-8.98358877145597,
96.0768641527964));
#182748=CARTESIAN_POINT('Ctrl Pts',(5.40557535339018,-6.5370633888607,96.2884207731781));
#182749=CARTESIAN_POINT('Ctrl Pts',(7.87642355379138,-3.1867425062301,96.4470882384646));
#182750=CARTESIAN_POINT('Ctrl Pts',(8.44121995650644,0.982039858335275,
96.605755703751));
#182751=CARTESIAN_POINT('Ctrl Pts',(6.94160524393157,4.89106892765923,96.7644231690373));
#182752=CARTESIAN_POINT('Ctrl Pts',(3.76605381086406,7.61608932442504,96.9230906343239));
#182753=CARTESIAN_POINT('Ctrl Pts',(-0.348317063116852,8.49309378863622,
97.0817580996103));
#182754=CARTESIAN_POINT('Ctrl Pts',(-4.33825713380984,7.2842007417435,97.2404255648969));
#182755=CARTESIAN_POINT('Ctrl Pts',(-8.34055300603935,3.35518593530714,
97.4519821852785));
#182756=CARTESIAN_POINT('Ctrl Pts',(-8.61567690191595,-4.30018024354439,
97.7164279607563));
#182757=CARTESIAN_POINT('Ctrl Pts',(-2.33198012360416,-8.68258067142632,
97.9808737362333));
#182758=CARTESIAN_POINT('Ctrl Pts',(3.21318317124227,-7.84533068859849,
98.1924303566154));
#182759=CARTESIAN_POINT('Ctrl Pts',(6.57877685610312,-5.38414191851868,
98.3510978219017));
#182760=CARTESIAN_POINT('Ctrl Pts',(8.34885206896818,-1.56744411886069,
98.5097652871882));
#182761=CARTESIAN_POINT('Ctrl Pts',(8.08427756212467,2.60563396349751,98.6684327524747));
#182762=CARTESIAN_POINT('Ctrl Pts',(5.85345793495883,6.15917312380028,98.8271060348031));
#182763=CARTESIAN_POINT('Ctrl Pts',(3.41624814820702,7.52225365430131,98.9328901620362));
#182764=CARTESIAN_POINT('Ctrl Pts',(2.10803039418863,7.87255331703859,98.9857851341739));
#182765=CARTESIAN_POINT('Ctrl Pts',(-5.31037376991254,4.57794244025904,
-5.5424415057459E-16));
#182766=CARTESIAN_POINT('Ctrl Pts',(-5.44331700421711,4.4462003696002,-1.29451042284116E-17));
#182767=CARTESIAN_POINT('Ctrl Pts',(-5.57062214561908,4.30929729963032,
-5.26815061343554E-17));
#182768=CARTESIAN_POINT('Ctrl Pts',(-5.69215510135391,4.1677062093632,-6.00214322687975E-16));
#182769=CARTESIAN_POINT('Ctrl Pts',(-5.81562375753537,4.02385994530381,
-2.0711506702255E-16));
#182770=CARTESIAN_POINT('Ctrl Pts',(-5.93313534079326,3.87517474031655,
-2.03905455560608E-15));
#182771=CARTESIAN_POINT('Ctrl Pts',(-6.0445238637167,3.72209865847224,-2.23432383705813E-15));
#182772=CARTESIAN_POINT('Ctrl Pts',(-6.15706744801159,3.56743522934661,
-2.43588381465624E-15));
#182773=CARTESIAN_POINT('Ctrl Pts',(-6.26336079465251,3.40828890743599,
-2.83121763992797E-15));
#182774=CARTESIAN_POINT('Ctrl Pts',(-6.36320004341494,3.24508007515358,
-8.46545056276682E-16));
#182775=CARTESIAN_POINT('Ctrl Pts',(-6.46313479819719,3.08171511763823,
3.73578344344788E-16));
#182776=CARTESIAN_POINT('Ctrl Pts',(-6.55660354150345,2.91427931386131,
-4.62227720763348E-16));
#182777=CARTESIAN_POINT('Ctrl Pts',(-6.6433625023191,2.74316055617857,-2.4980018054066E-16));
#182778=CARTESIAN_POINT('Ctrl Pts',(-6.69216088121534,2.64691323030984,
-1.28918032690918E-15));
#182779=CARTESIAN_POINT('Ctrl Pts',(-6.73883580575461,2.54950020323732,
-4.43215479361793E-15));
#182780=CARTESIAN_POINT('Ctrl Pts',(-6.78333763054534,2.45098684037426,
-3.88578058618805E-15));
#182781=CARTESIAN_POINT('Ctrl Pts',(-6.80155036661689,2.41066944022755,
-4.0530119472609E-15));
#182782=CARTESIAN_POINT('Ctrl Pts',(-6.81939896718112,2.37016796639514,
-4.21525031975438E-15));
#182783=CARTESIAN_POINT('Ctrl Pts',(-6.83688040508793,2.32948533314358,
-3.38618022510673E-15));
#182784=CARTESIAN_POINT('Ctrl Pts',(-6.84857336763547,2.30227358377367,
-2.8316328464711E-15));
#182785=CARTESIAN_POINT('Ctrl Pts',(-6.86010074485217,2.27498362189078,
-2.63071505109977E-15));
#182786=CARTESIAN_POINT('Ctrl Pts',(-6.87145407498761,2.24763530599042,
-2.83106871279415E-15));
#182787=CARTESIAN_POINT('Ctrl Pts',(-6.9466808909752,2.06642620669855,-4.158605907689E-15));
#182788=CARTESIAN_POINT('Ctrl Pts',(-7.01434821512689,1.88247767504642,
-3.52510701043973E-15));
#182789=CARTESIAN_POINT('Ctrl Pts',(-7.07427559886283,1.69624669194298,
-3.24740234702858E-15));
#182790=CARTESIAN_POINT('Ctrl Pts',(-7.09090024774233,1.64458375404096,
-3.17036340033011E-15));
#182791=CARTESIAN_POINT('Ctrl Pts',(-7.10692902931713,1.59274494156417,
-3.35064743386125E-15));
#182792=CARTESIAN_POINT('Ctrl Pts',(-7.12235757386584,1.54073952802914,
-3.30291349825984E-15));
#182793=CARTESIAN_POINT('Ctrl Pts',(-7.17736258705981,1.35533263831109,
-3.29727963165626E-15));
#182794=CARTESIAN_POINT('Ctrl Pts',(-7.22474203445627,1.1678103027789,-7.24618974341882E-15));
#182795=CARTESIAN_POINT('Ctrl Pts',(-7.2645811339778,0.978661458527771,
-5.93969318174459E-15));
#182796=CARTESIAN_POINT('Ctrl Pts',(-7.30481065710714,0.787658953549531,
-4.6203929395823E-15));
#182797=CARTESIAN_POINT('Ctrl Pts',(-7.33735147280739,0.594997259193497,
-3.65400968452058E-15));
#182798=CARTESIAN_POINT('Ctrl Pts',(-7.36224272937163,0.401157436213471,
-4.46864767411626E-15));
#182799=CARTESIAN_POINT('Ctrl Pts',(-7.38723762758615,0.206510507369071,
-5.28667763492113E-15));
#182800=CARTESIAN_POINT('Ctrl Pts',(-7.40451925616537,0.0106749153794845,
6.33680537375195E-16));
#182801=CARTESIAN_POINT('Ctrl Pts',(-7.41407644285483,-0.185874504306108,
-2.47024622979097E-15));
#182802=CARTESIAN_POINT('Ctrl Pts',(-7.41856230265033,-0.278128968746951,
-3.92713733649873E-15));
#182803=CARTESIAN_POINT('Ctrl Pts',(-7.42134566510405,-0.370540804922235,
-2.36763060747942E-15));
#182804=CARTESIAN_POINT('Ctrl Pts',(-7.42242141675543,-0.463061154024065,
-1.27675647831893E-15));
#182805=CARTESIAN_POINT('Ctrl Pts',(-7.42269559403654,-0.486641854765678,
-1.53461354303058E-15));
#182806=CARTESIAN_POINT('Ctrl Pts',(-7.42285872142643,-0.51022086257157,
5.6084351793085E-16));
#182807=CARTESIAN_POINT('Ctrl Pts',(-7.42291095902123,-0.533793942563365,
6.10622663543836E-16));
#182808=CARTESIAN_POINT('Ctrl Pts',(-7.42335282790941,-0.733194598119087,
1.18421068391936E-15));
#182809=CARTESIAN_POINT('Ctrl Pts',(-7.41586523167998,-0.932247529804568,
7.72423861470331E-16));
#182810=CARTESIAN_POINT('Ctrl Pts',(-7.40054244195954,-1.13044606574323,
2.22044604925031E-16));
#182811=CARTESIAN_POINT('Ctrl Pts',(-7.38505711727589,-1.33074697287766,
2.03079395727939E-16));
#182812=CARTESIAN_POINT('Ctrl Pts',(-7.36156964218886,-1.53017596445833,
1.52734294973599E-15));
#182813=CARTESIAN_POINT('Ctrl Pts',(-7.33012671706286,-1.72822631265957,
4.55191440096314E-15));
#182814=CARTESIAN_POINT('Ctrl Pts',(-7.30875088127035,-1.86286683051321,
7.77125758281482E-15));
#182815=CARTESIAN_POINT('Ctrl Pts',(-7.28369723421018,-1.99687051716647,
3.11416431501379E-15));
#182816=CARTESIAN_POINT('Ctrl Pts',(-7.25496680053326,-2.13007981682257,
3.77475828372553E-15));
#182817=CARTESIAN_POINT('Ctrl Pts',(-7.21283996301465,-2.32540184313392,
5.39452731674499E-15));
#182818=CARTESIAN_POINT('Ctrl Pts',(-7.1628105078922,-2.5190165641108,7.91946181298321E-15));
#182819=CARTESIAN_POINT('Ctrl Pts',(-7.10510958622245,-2.71054433168845,
7.43849426498855E-15));
#182820=CARTESIAN_POINT('Ctrl Pts',(-7.04813384283894,-2.89966500117753,
6.96357145964442E-15));
#182821=CARTESIAN_POINT('Ctrl Pts',(-6.98367793666496,-3.08675141819751,
4.05359569947312E-15));
#182822=CARTESIAN_POINT('Ctrl Pts',(-6.9119160153231,-3.27142605479363,
7.21644966006352E-15));
#182823=CARTESIAN_POINT('Ctrl Pts',(-6.90344888187215,-3.29321567195866,
7.50934034666217E-15));
#182824=CARTESIAN_POINT('Ctrl Pts',(-6.89487915416516,-3.31497377116827,
4.18261731543151E-15));
#182825=CARTESIAN_POINT('Ctrl Pts',(-6.88620977404331,-3.33669297006139,
4.6074255521944E-15));
#182826=CARTESIAN_POINT('Ctrl Pts',(-6.81144348703153,-3.52400323161249,
7.94999150818934E-15));
#182827=CARTESIAN_POINT('Ctrl Pts',(-6.72942390076641,-3.70803833235806,
5.973420582007E-15));
#182828=CARTESIAN_POINT('Ctrl Pts',(-6.64046121208781,-3.88843228962424,
5.32907051820075E-15));
#182829=CARTESIAN_POINT('Ctrl Pts',(-6.55004708816424,-4.07176939251072,
4.94538641220604E-15));
#182830=CARTESIAN_POINT('Ctrl Pts',(-6.45246134861859,-4.25134619449774,
4.35779931711698E-15));
#182831=CARTESIAN_POINT('Ctrl Pts',(-6.34797624592836,-4.42677407068446,
5.10702591327572E-15));
#182832=CARTESIAN_POINT('Ctrl Pts',(-6.24321137245675,-4.60267167502124,
4.46111568676177E-15));
#182833=CARTESIAN_POINT('Ctrl Pts',(-6.13150990586085,-4.77439874985371,
3.81014534070484E-15));
#182834=CARTESIAN_POINT('Ctrl Pts',(-6.01309583774504,-4.9415495441527,
3.21964677141295E-15));
#182835=CARTESIAN_POINT('Ctrl Pts',(-5.89542306846566,-5.10765393669139,
1.39687856458722E-15));
#182836=CARTESIAN_POINT('Ctrl Pts',(-5.77112118527314,-5.26923978164349,
3.32033915991433E-15));
#182837=CARTESIAN_POINT('Ctrl Pts',(-5.64036429125108,-5.42588572441345,
7.21644966006352E-16));
#182838=CARTESIAN_POINT('Ctrl Pts',(-5.61065088558373,-5.46148219891278,
6.16089719191022E-17));
#182839=CARTESIAN_POINT('Ctrl Pts',(-5.58060397387421,-5.49682346636191,
-5.43804932423255E-16));
#182840=CARTESIAN_POINT('Ctrl Pts',(-5.55022529123342,-5.53190436285383,
-3.88578058618805E-16));
#182841=CARTESIAN_POINT('Ctrl Pts',(-5.49592838736925,-5.59460570138167,
-1.3145331549245E-15));
#182842=CARTESIAN_POINT('Ctrl Pts',(-5.4405716751327,-5.65647532218303,
-2.98346659311989E-15));
#182843=CARTESIAN_POINT('Ctrl Pts',(-5.38418198249291,-5.71749394780626,
-1.0547118733939E-15));
#182844=CARTESIAN_POINT('Ctrl Pts',(-5.3532841852219,-5.75092809216853,
-2.12288582659533E-15));
#182845=CARTESIAN_POINT('Ctrl Pts',(-5.32207678287485,-5.78410615876794,
-9.2856319916077E-16));
#182846=CARTESIAN_POINT('Ctrl Pts',(-5.29056207773922,-5.81702691076677,
-9.43689570931383E-16));
#182847=CARTESIAN_POINT('Ctrl Pts',(-5.26481480858875,-5.84392290927611,
-9.56047699099551E-16));
#182848=CARTESIAN_POINT('Ctrl Pts',(-5.2388654098733,-5.87064385109954,
-1.61816256334409E-15));
#182849=CARTESIAN_POINT('Ctrl Pts',(-5.21273330931233,-5.89717117551002,
-1.55431223447522E-15));
#182850=CARTESIAN_POINT('Ctrl Pts',(-5.06794396085344,-6.04415032893814,
-1.2005386258731E-15));
#182851=CARTESIAN_POINT('Ctrl Pts',(-4.91743267615075,-6.18531130546595,
-6.78621530379578E-15));
#182852=CARTESIAN_POINT('Ctrl Pts',(-4.7616898899603,-6.32041813742794,
-7.21644966006352E-15));
#182853=CARTESIAN_POINT('Ctrl Pts',(-4.60415030900679,-6.45708368844242,
-7.65164760313445E-15));
#182854=CARTESIAN_POINT('Ctrl Pts',(-4.44125734847368,-6.5875551138735,
-5.31908651156807E-15));
#182855=CARTESIAN_POINT('Ctrl Pts',(-4.27347429869626,-6.71155865210133,
-5.55111512312578E-15));
#182856=CARTESIAN_POINT('Ctrl Pts',(-4.18666791907056,-6.775714704984,-5.67116040639858E-15));
#182857=CARTESIAN_POINT('Ctrl Pts',(-4.09855191061382,-6.83813894088107,
-6.05852963778292E-15));
#182858=CARTESIAN_POINT('Ctrl Pts',(-4.0091865085521,-6.89878969045305,
-6.99440505513849E-15));
#182859=CARTESIAN_POINT('Ctrl Pts',(-3.96288609764166,-6.9302129768975,
-7.47928416254308E-15));
#182860=CARTESIAN_POINT('Ctrl Pts',(-3.91625027173235,-6.96116016182333,
-5.96833885139656E-15));
#182861=CARTESIAN_POINT('Ctrl Pts',(-3.86928716320199,-6.99162514744697,
-6.43929354282591E-15));
#182862=CARTESIAN_POINT('Ctrl Pts',(-3.82791623921479,-7.01846248091889,
-6.85416877894764E-15));
#182863=CARTESIAN_POINT('Ctrl Pts',(-3.78628685685069,-7.04492822151511,
-6.98377421794483E-15));
#182864=CARTESIAN_POINT('Ctrl Pts',(-3.74443893455879,-7.07099713057179,
-6.99440505513849E-15));
#182865=CARTESIAN_POINT('Ctrl Pts',(-3.56475677190967,-7.18292904261593,
-7.04005061441867E-15));
#182866=CARTESIAN_POINT('Ctrl Pts',(-3.38092705064562,-7.28762890985193,
-5.99451951854587E-15));
#182867=CARTESIAN_POINT('Ctrl Pts',(-3.19343322407553,-7.3848264137291,
-4.88498130835069E-15));
#182868=CARTESIAN_POINT('Ctrl Pts',(-3.00594251740804,-7.48202230023705,
-3.77546156090279E-15));
#182869=CARTESIAN_POINT('Ctrl Pts',(-2.81478723729241,-7.57171655436551,
-2.84648883508677E-17));
#182870=CARTESIAN_POINT('Ctrl Pts',(-2.6204162358938,-7.65360035997005,
-1.33226762955019E-15));
#182871=CARTESIAN_POINT('Ctrl Pts',(-2.51614285898561,-7.6975282137293,
-2.03171309038931E-15));
#182872=CARTESIAN_POINT('Ctrl Pts',(-2.41094347454657,-7.73920755509353,
-2.1150680020794E-15));
#182873=CARTESIAN_POINT('Ctrl Pts',(-2.30488418583266,-7.77858539180668,
-2.22044604925031E-16));
#182874=CARTESIAN_POINT('Ctrl Pts',(-2.23785903866026,-7.80347057945064,
9.04037669818684E-16));
#182875=CARTESIAN_POINT('Ctrl Pts',(-2.17049042810051,-7.82743653127443,
2.51112873167852E-15));
#182876=CARTESIAN_POINT('Ctrl Pts',(-2.10279483963403,-7.85048474619609,
1.88737914186277E-15));
#182877=CARTESIAN_POINT('Ctrl Pts',(2.10803039481951,-7.87255331939627,
0.0142148672352196));
#182878=CARTESIAN_POINT('Ctrl Pts',(3.4162481492297,-7.52225365655416,0.0671098393728272));
#182879=CARTESIAN_POINT('Ctrl Pts',(5.85345793671154,-6.159173125645,0.172893966605912));
#182880=CARTESIAN_POINT('Ctrl Pts',(8.08427756454558,-2.60563396427805,
0.331567248934471));
#182881=CARTESIAN_POINT('Ctrl Pts',(8.34885207146841,1.56744411932978,0.490234714220902));
#182882=CARTESIAN_POINT('Ctrl Pts',(6.57877685807347,5.38414192013079,0.648902179507327));
#182883=CARTESIAN_POINT('Ctrl Pts',(3.21318317220485,7.84533069094777,0.807569644793758));
#182884=CARTESIAN_POINT('Ctrl Pts',(-2.33198012430219,8.68258067402656,
1.01912626517566));
#182885=CARTESIAN_POINT('Ctrl Pts',(-8.61567690449593,4.3001802448325,1.28357204065304));
#182886=CARTESIAN_POINT('Ctrl Pts',(-8.34055300853718,-3.3551859363116,
1.54801781613043));
#182887=CARTESIAN_POINT('Ctrl Pts',(-4.33825713510923,-7.28420074392475,
1.75957443651233));
#182888=CARTESIAN_POINT('Ctrl Pts',(-0.348317063221276,-8.49309379117966,
1.91824190179876));
#182889=CARTESIAN_POINT('Ctrl Pts',(3.76605381199188,-7.61608932670582,
2.07690936708519));
#182890=CARTESIAN_POINT('Ctrl Pts',(6.94160524601032,-4.89106892912396,
2.23557683237162));
#182891=CARTESIAN_POINT('Ctrl Pts',(8.44121995903425,-0.98203985862958,
2.39424429765805));
#182892=CARTESIAN_POINT('Ctrl Pts',(7.87642355615024,3.18674250718402,2.55291176294447));
#182893=CARTESIAN_POINT('Ctrl Pts',(5.40557535500932,6.53706339081806,2.7115792282309));
#182894=CARTESIAN_POINT('Ctrl Pts',(0.336812665113362,8.98358877414629,
2.92313584861281));
#182895=CARTESIAN_POINT('Ctrl Pts',(-5.46494857012726,7.12725858675843,
3.13469246899471));
#182896=CARTESIAN_POINT('Ctrl Pts',(-8.17994426748479,2.22908354222041,
3.34624908937662));
#182897=CARTESIAN_POINT('Ctrl Pts',(-8.32530750509452,-3.36923491103502,
3.55780570975852));
#182898=CARTESIAN_POINT('Ctrl Pts',(-4.2675825718424,-7.9125255319526,3.76936233014043));
#182899=CARTESIAN_POINT('Ctrl Pts',(1.34181698717311,-8.37566203946278,
3.98091895052233));
#182900=CARTESIAN_POINT('Ctrl Pts',(5.17047444783897,-6.74238192670933,
4.13958641580877));
#182901=CARTESIAN_POINT('Ctrl Pts',(7.77286267259136,-3.43594665272709,
4.29825388109519));
#182902=CARTESIAN_POINT('Ctrl Pts',(8.46247612164212,0.692405568114126,
4.45692134638163));
#182903=CARTESIAN_POINT('Ctrl Pts',(7.11095747028491,4.65375386049991,4.61558881166805));
#182904=CARTESIAN_POINT('Ctrl Pts',(4.00570910623038,7.49318164626026,4.77425627695448));
#182905=CARTESIAN_POINT('Ctrl Pts',(-0.0375200648430894,8.48238506412354,
4.93292374224091));
#182906=CARTESIAN_POINT('Ctrl Pts',(-5.49703181695961,7.11356738199704,
5.14448036262281));
#182907=CARTESIAN_POINT('Ctrl Pts',(-8.76225529409264,1.97113639024106,
5.35603698300472));
#182908=CARTESIAN_POINT('Ctrl Pts',(-7.7088088173919,-3.52913570365432,
5.56759360338662));
#182909=CARTESIAN_POINT('Ctrl Pts',(-4.23369274894941,-7.92075385899074,
5.77915022376853));
#182910=CARTESIAN_POINT('Ctrl Pts',(1.79262212218929,-8.80946689787677,
5.99070684415043));
#182911=CARTESIAN_POINT('Ctrl Pts',(6.39632924532418,-5.57128663863554,
6.20226346453234));
#182912=CARTESIAN_POINT('Ctrl Pts',(8.28962143476218,-1.86431093903326,
6.36093092981877));
#182913=CARTESIAN_POINT('Ctrl Pts',(8.16943141864774,2.34169384412702,6.51959839510519));
#182914=CARTESIAN_POINT('Ctrl Pts',(6.05400114274586,5.95331792659014,6.67826586039163));
#182915=CARTESIAN_POINT('Ctrl Pts',(2.47835881711179,8.12901453694417,6.83693332567804));
#182916=CARTESIAN_POINT('Ctrl Pts',(-1.7250390681998,8.31971868542347,6.99560079096449));
#182917=CARTESIAN_POINT('Ctrl Pts',(-5.46324238754078,6.48885546800465,
7.1542682562509));
#182918=CARTESIAN_POINT('Ctrl Pts',(-8.77816746704173,1.94009713653053,
7.36582487663282));
#182919=CARTESIAN_POINT('Ctrl Pts',(-7.99063545691195,-4.10027329976967,
7.57738149701471));
#182920=CARTESIAN_POINT('Ctrl Pts',(-3.65790945582747,-7.64854434479778,
7.78893811739663));
#182921=CARTESIAN_POINT('Ctrl Pts',(1.82392380767687,-8.79407744347022,
8.00049473777853));
#182922=CARTESIAN_POINT('Ctrl Pts',(7.02038676861,-5.61554722162305,8.21205135816044));
#182923=CARTESIAN_POINT('Ctrl Pts',(8.48056307710129,-0.179756958159142,
8.42360797854234));
#182924=CARTESIAN_POINT('Ctrl Pts',(7.55930044732043,3.87949166008483,8.58227544382877));
#182925=CARTESIAN_POINT('Ctrl Pts',(4.77234369525983,7.03191833138082,8.7409429091152));
#182926=CARTESIAN_POINT('Ctrl Pts',(0.834217223423008,8.44967489308136,
8.89961037440162));
#182927=CARTESIAN_POINT('Ctrl Pts',(-3.30512064769089,7.82938805201916,
9.05827783968807));
#182928=CARTESIAN_POINT('Ctrl Pts',(-6.65472716673046,5.28281034392745,
9.21694530497447));
#182929=CARTESIAN_POINT('Ctrl Pts',(-8.35198742766335,1.48208254725105,
9.37561277026092));
#182930=CARTESIAN_POINT('Ctrl Pts',(-7.98296706987295,-4.13430015122383,
9.58716939064281));
#182931=CARTESIAN_POINT('Ctrl Pts',(-3.50838750204087,-8.26763045095955,
9.79872601102473));
#182932=CARTESIAN_POINT('Ctrl Pts',(2.09162098999237,-8.21618243562534,
10.0102826314066));
#182933=CARTESIAN_POINT('Ctrl Pts',(7.03456103927407,-5.58367684620427,
10.2218392517885));
#182934=CARTESIAN_POINT('Ctrl Pts',(8.98807970294324,0.186075878676646,
10.4333958721704));
#182935=CARTESIAN_POINT('Ctrl Pts',(6.62666006128773,5.29524684040758,10.6449524925523));
#182936=CARTESIAN_POINT('Ctrl Pts',(3.31865127176191,7.82176658626181,10.8036199578387));
#182937=CARTESIAN_POINT('Ctrl Pts',(-0.840887270322603,8.45671616902799,
10.9622874231252));
#182938=CARTESIAN_POINT('Ctrl Pts',(-4.77295389581727,7.02223862333318,
11.1209548884116));
#182939=CARTESIAN_POINT('Ctrl Pts',(-7.5537943117649,3.89401223167548,11.279622353698));
#182940=CARTESIAN_POINT('Ctrl Pts',(-8.49414566628779,-0.207287706854769,
11.4382898189845));
#182941=CARTESIAN_POINT('Ctrl Pts',(-7.36230256501997,-4.21292815151322,
11.5969572842709));
#182942=CARTESIAN_POINT('Ctrl Pts',(-3.48069952670291,-8.28884381466413,
11.8085139046528));
#182943=CARTESIAN_POINT('Ctrl Pts',(2.60305770872397,-8.59573072537543,
12.0200705250347));
#182944=CARTESIAN_POINT('Ctrl Pts',(6.86986101384801,-4.96845467239725,
12.2316271454166));
#182945=CARTESIAN_POINT('Ctrl Pts',(8.97854442063184,0.219627468344228,
12.4431837657985));
#182946=CARTESIAN_POINT('Ctrl Pts',(6.78195923173225,5.90129053328225,12.6547403861804));
#182947=CARTESIAN_POINT('Ctrl Pts',(1.69552102711242,8.31128576787805,12.8662970065623));
#182948=CARTESIAN_POINT('Ctrl Pts',(-2.46308694886501,8.13183137281261,
13.0249644718488));
#182949=CARTESIAN_POINT('Ctrl Pts',(-6.06363365216522,5.95445099880917,
13.1836319371352));
#182950=CARTESIAN_POINT('Ctrl Pts',(-8.16369841306695,2.33387068945947,
13.3422994024216));
#182951=CARTESIAN_POINT('Ctrl Pts',(-8.29469668283903,-1.84963420832045,
13.500966867708));
#182952=CARTESIAN_POINT('Ctrl Pts',(-6.38911994390509,-5.60112713084813,
13.6596343329945));
#182953=CARTESIAN_POINT('Ctrl Pts',(-2.95376983307013,-7.95157257666414,
13.8183017982809));
#182954=CARTESIAN_POINT('Ctrl Pts',(2.63790774924367,-8.5942797071986,14.0298584186628));
#182955=CARTESIAN_POINT('Ctrl Pts',(7.50571555676396,-4.93221351109846,
14.2414150390447));
#182956=CARTESIAN_POINT('Ctrl Pts',(8.45792928339156,0.586484798099847,
14.4529716594266));
#182957=CARTESIAN_POINT('Ctrl Pts',(6.7531423154713,5.92094291520376,14.6645282798085));
#182958=CARTESIAN_POINT('Ctrl Pts',(1.4264861409623,8.87611053720761,14.8760849001904));
#182959=CARTESIAN_POINT('Ctrl Pts',(-4.02297065926845,7.46779550760314,
15.0876415205724));
#182960=CARTESIAN_POINT('Ctrl Pts',(-7.10103632182176,4.66570058508865,
15.2463089858587));
#182961=CARTESIAN_POINT('Ctrl Pts',(-8.47059776903331,0.687104941139273,
15.4049764511452));
#182962=CARTESIAN_POINT('Ctrl Pts',(-7.76344919178384,-3.4382816669407,
15.5636439164316));
#182963=CARTESIAN_POINT('Ctrl Pts',(-5.18377337434866,-6.73436213521994,
15.7223113817181));
#182964=CARTESIAN_POINT('Ctrl Pts',(-1.31716520521893,-8.39395941232081,
15.8809788470045));
#182965=CARTESIAN_POINT('Ctrl Pts',(2.82641118567979,-7.99772858242742,
16.0396463122909));
#182966=CARTESIAN_POINT('Ctrl Pts',(7.53154427612354,-4.90877192339148,
16.2512029326728));
#182967=CARTESIAN_POINT('Ctrl Pts',(8.92292854400946,1.02168602643451,16.4627595530547));
#182968=CARTESIAN_POINT('Ctrl Pts',(6.11837120860958,5.86907709396564,16.6743161734366));
#182969=CARTESIAN_POINT('Ctrl Pts',(1.39176936253974,8.87273769360992,16.8858727938185));
#182970=CARTESIAN_POINT('Ctrl Pts',(-4.59140730818783,7.72911249170335,
17.0974294142004));
#182971=CARTESIAN_POINT('Ctrl Pts',(-7.87330703075219,3.15646939922137,
17.3089860345823));
#182972=CARTESIAN_POINT('Ctrl Pts',(-8.441462578291,-0.967051359980911,
17.4676534998688));
#182973=CARTESIAN_POINT('Ctrl Pts',(-6.94405265035244,-4.89931347782761,
17.6263209651552));
#182974=CARTESIAN_POINT('Ctrl Pts',(-3.75807080154932,-7.61379196098583,
17.7849884304416));
#182975=CARTESIAN_POINT('Ctrl Pts',(0.334349638221215,-8.49184020600429,
17.943655895728));
#182976=CARTESIAN_POINT('Ctrl Pts',(4.36644429984199,-7.28887117254147,
18.1023233610145));
#182977=CARTESIAN_POINT('Ctrl Pts',(7.29408571958939,-4.32996260769013,
18.2609908263009));
#182978=CARTESIAN_POINT('Ctrl Pts',(8.92774180567757,1.05623256446788,18.4725474466828));
#182979=CARTESIAN_POINT('Ctrl Pts',(6.19658250590297,6.50114308300071,18.6841040670647));
#182980=CARTESIAN_POINT('Ctrl Pts',(0.937612275068185,8.4262337614676,18.8956606874466));
#182981=CARTESIAN_POINT('Ctrl Pts',(-4.61590244562942,7.70428067703549,
19.1072173078285));
#182982=CARTESIAN_POINT('Ctrl Pts',(-8.4771793246631,2.99293028261425,19.3187739282104));
#182983=CARTESIAN_POINT('Ctrl Pts',(-8.06749931840342,-2.6206330182368,
19.5303305485923));
#182984=CARTESIAN_POINT('Ctrl Pts',(-5.86190916878713,-6.1507316386279,
19.6889980138788));
#182985=CARTESIAN_POINT('Ctrl Pts',(-2.19288325165259,-8.21062743092827,
19.8476654791652));
#182986=CARTESIAN_POINT('Ctrl Pts',(1.99245080157417,-8.25366972794139,
20.0063329444516));
#182987=CARTESIAN_POINT('Ctrl Pts',(5.6972100086841,-6.30594464627148,20.165000409738));
#182988=CARTESIAN_POINT('Ctrl Pts',(8.02239891580781,-2.79903455305117,
20.3236678750245));
#182989=CARTESIAN_POINT('Ctrl Pts',(8.37459038364871,1.34851717631298,20.4823353403109));
#182990=CARTESIAN_POINT('Ctrl Pts',(6.17814516547287,6.53075212310415,20.6938919606928));
#182991=CARTESIAN_POINT('Ctrl Pts',(0.592716465026654,8.96165070342495,
20.9054485810747));
#182992=CARTESIAN_POINT('Ctrl Pts',(-4.67854763534728,7.07048260057551,
21.1170052014566));
#182993=CARTESIAN_POINT('Ctrl Pts',(-8.48007796282208,2.95817069868685,
21.3285618218385));
#182994=CARTESIAN_POINT('Ctrl Pts',(-8.4263858148105,-3.13308523328778,
21.5401184422205));
#182995=CARTESIAN_POINT('Ctrl Pts',(-4.51537004268918,-7.18078658966394,
21.7516750626023));
#182996=CARTESIAN_POINT('Ctrl Pts',(-0.560248715354337,-8.47818377781896,
21.9103425278888));
#182997=CARTESIAN_POINT('Ctrl Pts',(3.57659993765015,-7.70915511913537,
22.0690099931752));
#182998=CARTESIAN_POINT('Ctrl Pts',(6.81773385092994,-5.0607735883473,22.2276774584616));
#182999=CARTESIAN_POINT('Ctrl Pts',(8.41444502931074,-1.19174435748521,
22.386344923748));
#183000=CARTESIAN_POINT('Ctrl Pts',(7.95297533686621,2.99059560701983,22.5450123890345));
#183001=CARTESIAN_POINT('Ctrl Pts',(5.56616896288688,6.40078321342844,22.7036798543209));
#183002=CARTESIAN_POINT('Ctrl Pts',(0.559590308908195,8.97257263360188,
22.9152364747028));
#183003=CARTESIAN_POINT('Ctrl Pts',(-5.28639056270976,7.26061780818986,
23.1267930950847));
#183004=CARTESIAN_POINT('Ctrl Pts',(-8.12212057676843,2.4313966187543,23.3383497154666));
#183005=CARTESIAN_POINT('Ctrl Pts',(-8.40634190701105,-3.16163120565004,
23.5499063358486));
#183006=CARTESIAN_POINT('Ctrl Pts',(-4.46261386723436,-7.80418339424779,
23.7614629562304));
#183007=CARTESIAN_POINT('Ctrl Pts',(1.13357108138952,-8.4063832456146,23.9730195766124));
#183008=CARTESIAN_POINT('Ctrl Pts',(5.0015756079893,-6.8686039506653,24.1316870418987));
#183009=CARTESIAN_POINT('Ctrl Pts',(7.6852099193921,-3.6277662906763,24.2903545071852));
#183010=CARTESIAN_POINT('Ctrl Pts',(8.47705154584668,0.482204586963322,
24.4490219724716));
#183011=CARTESIAN_POINT('Ctrl Pts',(7.22424657979749,4.4758687558031,24.6076894377581));
#183012=CARTESIAN_POINT('Ctrl Pts',(4.19041193584253,7.39147661847597,24.7663569030444));
#183013=CARTESIAN_POINT('Ctrl Pts',(0.172973997312942,8.48070413733235,
24.9250243683309));
#183014=CARTESIAN_POINT('Ctrl Pts',(-5.31882267198645,7.24778078883794,
25.1365809887128));
#183015=CARTESIAN_POINT('Ctrl Pts',(-8.71064532758041,2.18795660725075,
25.3481376090947));
#183016=CARTESIAN_POINT('Ctrl Pts',(-7.79400736662216,-3.33676210573878,
25.5596942294766));
#183017=CARTESIAN_POINT('Ctrl Pts',(-4.42893524494197,-7.81325980204303,
25.7712508498586));
#183018=CARTESIAN_POINT('Ctrl Pts',(1.57347143296348,-8.85123655930249,
25.9828074702404));
#183019=CARTESIAN_POINT('Ctrl Pts',(6.25611342708481,-5.72829009881323,
26.1943640906224));
#183020=CARTESIAN_POINT('Ctrl Pts',(8.24080778580045,-2.06943611426375,
26.3530315559088));
#183021=CARTESIAN_POINT('Ctrl Pts',(8.22502286704817,2.13825597191375,26.5116990211952));
#183022=CARTESIAN_POINT('Ctrl Pts',(6.19986305135223,5.80126040779994,26.6703664864817));
#183023=CARTESIAN_POINT('Ctrl Pts',(2.67930960812223,8.06501331609031,26.829033951768));
#183024=CARTESIAN_POINT('Ctrl Pts',(-1.51806183654231,8.35996214429004,
26.9877014170545));
#183025=CARTESIAN_POINT('Ctrl Pts',(-5.30054526584808,6.62242271026307,
27.1463688823409));
#183026=CARTESIAN_POINT('Ctrl Pts',(-8.72732282347127,2.15732179194542,
27.3579255027229));
#183027=CARTESIAN_POINT('Ctrl Pts',(-8.08991946913675,-3.90073058810687,
27.5694821231047));
#183028=CARTESIAN_POINT('Ctrl Pts',(-3.84657462384231,-7.5554216192392,
27.7810387434866));
#183029=CARTESIAN_POINT('Ctrl Pts',(1.60514535734365,-8.83662857202387,
27.9925953638685));
#183030=CARTESIAN_POINT('Ctrl Pts',(6.87888050673705,-5.78802245616915,
28.2041519842505));
#183031=CARTESIAN_POINT('Ctrl Pts',(8.47349127139817,-0.390138875596302,
28.4157086046323));
#183032=CARTESIAN_POINT('Ctrl Pts',(7.65323878408526,3.69072010687644,28.5743760699188));
#183033=CARTESIAN_POINT('Ctrl Pts',(4.94536471097505,6.91133182826096,28.7330435352052));
#183034=CARTESIAN_POINT('Ctrl Pts',(1.04363116032353,8.42637277693261,28.8917110004916));
#183035=CARTESIAN_POINT('Ctrl Pts',(-3.10982398058202,7.90899074311553,
29.050378465778));
#183036=CARTESIAN_POINT('Ctrl Pts',(-6.52159005289998,5.44631453144641,
29.2090459310645));
#183037=CARTESIAN_POINT('Ctrl Pts',(-8.31263921698669,1.68887297240714,
29.3677133963509));
#183038=CARTESIAN_POINT('Ctrl Pts',(-8.08309778792846,-3.93493724598903,
29.5792700167329));
#183039=CARTESIAN_POINT('Ctrl Pts',(-3.71246075495181,-8.17802734655816,
29.7908266371147));
#183040=CARTESIAN_POINT('Ctrl Pts',(1.88710003723826,-8.26555416355795,
30.0023832574966));
#183041=CARTESIAN_POINT('Ctrl Pts',(6.89384124657026,-5.75651361547919,
30.2139398778785));
#183042=CARTESIAN_POINT('Ctrl Pts',(8.98992942538604,-0.0370122366697308,
30.4254964982604));
#183043=CARTESIAN_POINT('Ctrl Pts',(6.75601621840632,5.12918195478999,30.6370531186424));
#183044=CARTESIAN_POINT('Ctrl Pts',(3.51171925137983,7.73700889834157,30.7957205839287));
#183045=CARTESIAN_POINT('Ctrl Pts',(-0.63078281859802,8.47497804130793,
30.9543880492152));
#183046=CARTESIAN_POINT('Ctrl Pts',(-4.59723391948035,7.13851276276853,
31.1130555145016));
#183047=CARTESIAN_POINT('Ctrl Pts',(-7.45484209100556,4.0802535660253,31.2717229797881));
#183048=CARTESIAN_POINT('Ctrl Pts',(-8.49667383085844,0.00355042726519961,
31.4303904450745));
#183049=CARTESIAN_POINT('Ctrl Pts',(-7.46457547638134,-4.02894224656035,
31.5890579103609));
#183050=CARTESIAN_POINT('Ctrl Pts',(-3.68530769504133,-8.19992122961889,
31.8006145307429));
#183051=CARTESIAN_POINT('Ctrl Pts',(2.38896113921104,-8.6576764096061,32.0121711511247));
#183052=CARTESIAN_POINT('Ctrl Pts',(6.74445809974086,-5.13739400105683,
32.2237277715067));
#183053=CARTESIAN_POINT('Ctrl Pts',(8.98122963056665,-0.0032343689442986,
32.4352843918885));
#183054=CARTESIAN_POINT('Ctrl Pts',(6.92630597900252,5.73118543272851,32.6468410122704));
#183055=CARTESIAN_POINT('Ctrl Pts',(1.90123575731541,8.26665381298975,32.8583976326524));
#183056=CARTESIAN_POINT('Ctrl Pts',(-2.26054470865007,8.19044665532488,
33.0170650979387));
#183057=CARTESIAN_POINT('Ctrl Pts',(-5.91401240893771,6.10308094259127,
33.1757325632252));
#183058=CARTESIAN_POINT('Ctrl Pts',(-8.10327185091423,2.53572661870529,
33.3344000285116));
#183059=CARTESIAN_POINT('Ctrl Pts',(-8.33803955853058,-1.64323950940491,
33.4930674937981));
#183060=CARTESIAN_POINT('Ctrl Pts',(-6.52613937779765,-5.44086239626474,
33.6517349590845));
#183061=CARTESIAN_POINT('Ctrl Pts',(-3.1501711803149,-7.87582911212693,
33.810402424371));
#183062=CARTESIAN_POINT('Ctrl Pts',(2.4238364544957,-8.65709060949134,34.0219590447528));
#183063=CARTESIAN_POINT('Ctrl Pts',(7.38101614325807,-5.11694213677213,
34.2335156651348));
#183064=CARTESIAN_POINT('Ctrl Pts',(8.46987802192835,0.376428578763512,
34.4450722855166));
#183065=CARTESIAN_POINT('Ctrl Pts',(6.89798559148066,5.7515468282746,34.6566289058985));
#183066=CARTESIAN_POINT('Ctrl Pts',(1.64629931156174,8.83798051343387,34.8681855262805));
#183067=CARTESIAN_POINT('Ctrl Pts',(-3.83642553630601,7.56532231785874,
35.0797421466623));
#183068=CARTESIAN_POINT('Ctrl Pts',(-6.98307478551133,4.84046953646904,
35.2384096119488));
#183069=CARTESIAN_POINT('Ctrl Pts',(-8.45093966454115,0.897083357985828,
35.3970770772352));
#183070=CARTESIAN_POINT('Ctrl Pts',(-7.84637645310182,-3.24458020872331,
35.5557445425216));
#183071=CARTESIAN_POINT('Ctrl Pts',(-5.34928412448423,-6.60365801055984,
35.7144120078081));
#183072=CARTESIAN_POINT('Ctrl Pts',(-1.52504790680204,-8.35869054789607,
35.8730794730945));
#183073=CARTESIAN_POINT('Ctrl Pts',(2.62708470771682,-8.06540070964814,
36.0317469383809));
#183074=CARTESIAN_POINT('Ctrl Pts',(7.40741859067934,-5.09414868270878,
36.2433035587628));
#183075=CARTESIAN_POINT('Ctrl Pts',(8.94553321445923,0.799957278307623,
36.4548601791447));
#183076=CARTESIAN_POINT('Ctrl Pts',(6.26212293903824,5.71544823068376,36.6664167995266));
#183077=CARTESIAN_POINT('Ctrl Pts',(1.61150952903428,8.83547017288509,36.8779734199086));
#183078=CARTESIAN_POINT('Ctrl Pts',(-4.39820281689368,7.84066406374832,
37.0895300402904));
#183079=CARTESIAN_POINT('Ctrl Pts',(-7.79255786467272,3.35086624538187,
37.3010866606724));
#183080=CARTESIAN_POINT('Ctrl Pts',(-8.46285979168174,-0.757286563901003,
37.4597541259587));
#183081=CARTESIAN_POINT('Ctrl Pts',(-7.06348635977089,-4.72549470534256,
37.6184215912452));
#183082=CARTESIAN_POINT('Ctrl Pts',(-3.94584278023162,-7.51819452583688,
37.7770890565316));
#183083=CARTESIAN_POINT('Ctrl Pts',(0.123529587498059,-8.4975220038493,
37.9357565218181));
#183084=CARTESIAN_POINT('Ctrl Pts',(4.18423325630602,-7.39497605475173,
38.0944239871045));
#183085=CARTESIAN_POINT('Ctrl Pts',(7.18439576515461,-4.50962527914911,
38.2530914523909));
#183086=CARTESIAN_POINT('Ctrl Pts',(8.95120223418368,0.834373742294213,
38.4646480727728));
#183087=CARTESIAN_POINT('Ctrl Pts',(6.35599428212517,6.34537885580543,38.6762046931547));
#183088=CARTESIAN_POINT('Ctrl Pts',(1.14641270510795,8.40037321140093,38.8877613135367));
#183089=CARTESIAN_POINT('Ctrl Pts',(-4.42330659021481,7.81644771920545,
39.0993179339185));
#183090=CARTESIAN_POINT('Ctrl Pts',(-8.40030228714286,3.20236201321892,
39.3108745543005));
#183091=CARTESIAN_POINT('Ctrl Pts',(-8.13004376866344,-2.41963860696786,
39.5224311746824));
#183092=CARTESIAN_POINT('Ctrl Pts',(-6.01272886306041,-6.00337991575155,
39.6810986399688));
#183093=CARTESIAN_POINT('Ctrl Pts',(-2.39594709307398,-8.15368489040877,
39.8397661052552));
#183094=CARTESIAN_POINT('Ctrl Pts',(1.7870301727314,-8.3005690971389,39.9984335705416));
#183095=CARTESIAN_POINT('Ctrl Pts',(5.53897960608638,-6.44537389825049,
40.1571010358281));
#183096=CARTESIAN_POINT('Ctrl Pts',(7.95047325441626,-2.99724103540918,
40.3157685011145));
#183097=CARTESIAN_POINT('Ctrl Pts',(8.40547390673061,1.14029429183156,40.4744359664009));
#183098=CARTESIAN_POINT('Ctrl Pts',(6.33829733958424,6.3754362842165,40.6859925867828));
#183099=CARTESIAN_POINT('Ctrl Pts',(0.814908966460877,8.94418355773692,
40.8975492071648));
#183100=CARTESIAN_POINT('Ctrl Pts',(-4.50165959892069,7.18439928154756,
41.1091058275466));
#183101=CARTESIAN_POINT('Ctrl Pts',(-8.4040625594374,3.16768505934088,41.3206624479286));
#183102=CARTESIAN_POINT('Ctrl Pts',(-8.50153578206802,-2.92302759571368,
41.5322190683104));
#183103=CARTESIAN_POINT('Ctrl Pts',(-4.69216421186369,-7.06653080921752,
41.7437756886924));
#183104=CARTESIAN_POINT('Ctrl Pts',(-0.770454433048681,-8.46167115646284,
41.9024431539787));
#183105=CARTESIAN_POINT('Ctrl Pts',(3.38420314577333,-7.7955313374426,42.0611106192652));
#183106=CARTESIAN_POINT('Ctrl Pts',(6.69005617978553,-5.22839100354053,
42.2197780845516));
#183107=CARTESIAN_POINT('Ctrl Pts',(8.38228205845596,-1.40017400969653,
42.3784455498381));
#183108=CARTESIAN_POINT('Ctrl Pts',(8.02473532771008,2.79232908406186,42.5371130151245));
#183109=CARTESIAN_POINT('Ctrl Pts',(5.7232845171658,6.26069301309463,42.6957804804109));
#183110=CARTESIAN_POINT('Ctrl Pts',(0.782064027926499,8.95592411958767,
42.9073371007928));
#183111=CARTESIAN_POINT('Ctrl Pts',(-5.10459733350807,7.38955899899651,
43.1188937211747));
#183112=CARTESIAN_POINT('Ctrl Pts',(-8.05928680212849,2.63219080298456,
43.3304503415566));
#183113=CARTESIAN_POINT('Ctrl Pts',(-8.48220638770805,-2.95206214935692,
43.5420069619386));
#183114=CARTESIAN_POINT('Ctrl Pts',(-4.65489329170895,-7.69104475469404,
43.7535635823204));
#183115=CARTESIAN_POINT('Ctrl Pts',(0.92462547235416,-8.43192329258054,
43.9651202027024));
#183116=CARTESIAN_POINT('Ctrl Pts',(4.82959753593432,-6.99059843054699,
44.1237876679887));
#183117=CARTESIAN_POINT('Ctrl Pts',(7.59282387950186,-3.81735056399868,
44.2824551332753));
#183118=CARTESIAN_POINT('Ctrl Pts',(8.48640677810244,0.271705979293537,
44.4411225985615));
#183119=CARTESIAN_POINT('Ctrl Pts',(7.33308663060707,4.29522761167587,44.5997900638482));
#183120=CARTESIAN_POINT('Ctrl Pts',(4.37253423460613,7.28521950689286,44.7584575291344));
#183121=CARTESIAN_POINT('Ctrl Pts',(0.383361516135644,8.47380058090509,
44.917124994421));
#183122=CARTESIAN_POINT('Ctrl Pts',(-5.13733802342598,7.37753075052028,
45.1286816148028));
#183123=CARTESIAN_POINT('Ctrl Pts',(-8.65367101925888,2.40342935654577,
45.3402382351847));
#183124=CARTESIAN_POINT('Ctrl Pts',(-7.87440616908082,-3.1423335318712,
45.5517948555667));
#183125=CARTESIAN_POINT('Ctrl Pts',(-4.62145010432963,-7.70095432521442,
45.7633514759484));
#183126=CARTESIAN_POINT('Ctrl Pts',(1.35335143495645,-8.88755483745821,
45.9749080963306));
#183127=CARTESIAN_POINT('Ctrl Pts',(6.11204527800326,-5.88176651441044,
46.1864647167123));
#183128=CARTESIAN_POINT('Ctrl Pts',(8.18691835566083,-2.27328554229023,
46.3451321819989));
#183129=CARTESIAN_POINT('Ctrl Pts',(8.2755506768925,1.93349871892714,46.5037996472851));
#183130=CARTESIAN_POINT('Ctrl Pts',(6.34190383553277,5.64563517982648,46.6624671125717));
#183131=CARTESIAN_POINT('Ctrl Pts',(2.87861614074041,7.99603615249718,46.821134577858));
#183132=CARTESIAN_POINT('Ctrl Pts',(-1.31016046092372,8.39507451559495,
46.9798020431445));
#183133=CARTESIAN_POINT('Ctrl Pts',(-5.13456471748913,6.75188081050702,
47.1384695084309));
#183134=CARTESIAN_POINT('Ctrl Pts',(-8.67114696343998,2.37328761312805,
47.3500261288128));
#183135=CARTESIAN_POINT('Ctrl Pts',(-8.18413847504018,-3.69891909332623,
47.5615827491948));
#183136=CARTESIAN_POINT('Ctrl Pts',(-4.0329686081033,-7.45748897431712,
47.7731393695766));
#183137=CARTESIAN_POINT('Ctrl Pts',(1.38561984066132,-8.87412604512891,
47.9846959899586));
#183138=CARTESIAN_POINT('Ctrl Pts',(6.73265434236434,-5.95615549819381,
48.1962526103404));
#183139=CARTESIAN_POINT('Ctrl Pts',(8.46179816320036,-0.601240457908621,
48.4078092307224));
#183140=CARTESIAN_POINT('Ctrl Pts',(7.74120582594587,3.50169910810985,48.5664766960087));
#183141=CARTESIAN_POINT('Ctrl Pts',(5.1177835704526,6.78255791217336,48.7251441612953));
#183142=CARTESIAN_POINT('Ctrl Pts',(1.24779844848575,8.40530319096317,48.8838116265816));
#183143=CARTESIAN_POINT('Ctrl Pts',(-2.90429742469008,7.97020167864347,
49.0424790918682));
#183144=CARTESIAN_POINT('Ctrl Pts',(-7.56136164456266,4.84714368437679,
49.2540357122499));
#183145=CARTESIAN_POINT('Ctrl Pts',(-9.27805728479038,-2.6008240964781,
49.5184814877275));
#183146=CARTESIAN_POINT('Ctrl Pts',(-2.82248521115999,-9.21539207487178,
49.8358164183001));
#183147=CARTESIAN_POINT('Ctrl Pts',(4.66791625045747,-7.67208173557313,
50.1002621937777));
#183148=CARTESIAN_POINT('Ctrl Pts',(7.89643897624826,-3.09617872360307,
50.3118188141594));
#183149=CARTESIAN_POINT('Ctrl Pts',(8.43764997470094,1.05416382293544,50.470486279446));
#183150=CARTESIAN_POINT('Ctrl Pts',(6.8928911275569,4.94259754937307,50.6291537447324));
#183151=CARTESIAN_POINT('Ctrl Pts',(2.63608800317644,8.58571947985341,50.8407103651143));
#183152=CARTESIAN_POINT('Ctrl Pts',(-4.99930908329347,8.23575890671189,
51.1051561405917));
#183153=CARTESIAN_POINT('Ctrl Pts',(-9.63818235852632,0.24288735913145,
51.4224910711645));
#183154=CARTESIAN_POINT('Ctrl Pts',(-6.12768469299847,-6.5646711245724,
51.6869368466419));
#183155=CARTESIAN_POINT('Ctrl Pts',(-0.867116444760915,-8.43072686169507,
51.8984934670238));
#183156=CARTESIAN_POINT('Ctrl Pts',(4.68814972923802,-7.66588807412999,
52.1100500874056));
#183157=CARTESIAN_POINT('Ctrl Pts',(8.50145527199978,-2.91580736816088,
52.3216067077878));
#183158=CARTESIAN_POINT('Ctrl Pts',(8.0447532361429,2.69163301364258,52.5331633281694));
#183159=CARTESIAN_POINT('Ctrl Pts',(5.80643884209009,6.20304194060494,52.691830793456));
#183160=CARTESIAN_POINT('Ctrl Pts',(2.11999576383795,8.22961018578338,52.8504982587423));
#183161=CARTESIAN_POINT('Ctrl Pts',(-2.06596615843867,8.23572124922552,
53.0091657240289));
#183162=CARTESIAN_POINT('Ctrl Pts',(-5.75302831553045,6.25493591622287,
53.1678331893151));
#183163=CARTESIAN_POINT('Ctrl Pts',(-8.047029127633,2.72755944959616,53.3265006546018));
#183164=CARTESIAN_POINT('Ctrl Pts',(-8.36223966014006,-1.42300601179314,
53.485168119888));
#183165=CARTESIAN_POINT('Ctrl Pts',(-6.11979599351654,-6.58546341990916,
53.6967247402701));
#183166=CARTESIAN_POINT('Ctrl Pts',(-0.512933016603738,-8.96657628475243,
53.9082813606519));
#183167=CARTESIAN_POINT('Ctrl Pts',(4.74128188989137,-7.02856440921785,
54.1198379810338));
#183168=CARTESIAN_POINT('Ctrl Pts',(8.50607039726349,-2.8825885650715,54.3313946014157));
#183169=CARTESIAN_POINT('Ctrl Pts',(8.39816847567835,3.20795130586528,54.5429512217976));
#183170=CARTESIAN_POINT('Ctrl Pts',(4.45128768753787,7.22068551281421,54.7545078421795));
#183171=CARTESIAN_POINT('Ctrl Pts',(0.484776114812333,8.48283413024505,
54.913175307466));
#183172=CARTESIAN_POINT('Ctrl Pts',(-3.64506438395335,7.67702038850236,
55.0718427727524));
#183173=CARTESIAN_POINT('Ctrl Pts',(-6.86250141715301,4.99990004560204,
55.2305102380388));
#183174=CARTESIAN_POINT('Ctrl Pts',(-8.42471748741338,1.11681427094036,
55.3891777033253));
#183175=CARTESIAN_POINT('Ctrl Pts',(-7.92604615270924,-3.06125324948971,
55.5478451686116));
#183176=CARTESIAN_POINT('Ctrl Pts',(-5.50898590099322,-6.45006488330444,
55.7065126338981));
#183177=CARTESIAN_POINT('Ctrl Pts',(-0.479718345538541,-8.97719728889355,
55.91806925428));
#183178=CARTESIAN_POINT('Ctrl Pts',(5.35079580383119,-7.2132850012205,56.1296258746619));
#183179=CARTESIAN_POINT('Ctrl Pts',(8.14343672238523,-2.35901896791911,
56.3411824950438));
#183180=CARTESIAN_POINT('Ctrl Pts',(8.3778726453612,3.23631674834871,56.5527391154256));
#183181=CARTESIAN_POINT('Ctrl Pts',(4.39298520671649,7.84358858913003,56.7642957358077));
#183182=CARTESIAN_POINT('Ctrl Pts',(-1.20833730354274,8.39596234053631,
56.9758523561894));
#183183=CARTESIAN_POINT('Ctrl Pts',(-5.06250346555688,6.82382132380148,
57.134519821476));
#183184=CARTESIAN_POINT('Ctrl Pts',(-7.71719024737759,3.55922947395562,
57.2931872867624));
#183185=CARTESIAN_POINT('Ctrl Pts',(-8.47242456287475,-0.557625503363572,
57.4518547520488));
#183186=CARTESIAN_POINT('Ctrl Pts',(-7.18412830395208,-4.53998240932834,
57.6105222173352));
#183187=CARTESIAN_POINT('Ctrl Pts',(-4.12446686583729,-7.42847574311758,
57.7691896826217));
#183188=CARTESIAN_POINT('Ctrl Pts',(-0.0974946303616515,-8.48190765487712,
57.927857147908));
#183189=CARTESIAN_POINT('Ctrl Pts',(5.38311238322129,-7.20015986270839,
58.13941376829));
#183190=CARTESIAN_POINT('Ctrl Pts',(8.72977171865282,-2.1103511267997,58.3509703886718));
#183191=CARTESIAN_POINT('Ctrl Pts',(7.76400380533544,3.40599135230539,58.5625270090538));
#183192=CARTESIAN_POINT('Ctrl Pts',(4.35922714507761,7.85236491992856,58.7740836294357));
#183193=CARTESIAN_POINT('Ctrl Pts',(-1.65217912845243,8.83688322354667,
58.9856402498176));
#183194=CARTESIAN_POINT('Ctrl Pts',(-6.30684358486332,5.67238809186887,
59.1971968701995));
#183195=CARTESIAN_POINT('Ctrl Pts',(-8.25889803028424,1.99601656278161,
59.355864335486));
#183196=CARTESIAN_POINT('Ctrl Pts',(-8.20566812970426,-2.21136842476436,
59.5145318007724));
#183197=CARTESIAN_POINT('Ctrl Pts',(-6.14799025373477,-5.85620525721325,
59.6731992660588));
#183198=CARTESIAN_POINT('Ctrl Pts',(-2.60743035739999,-8.08853798261459,
59.8318667313452));
#183199=CARTESIAN_POINT('Ctrl Pts',(1.59239971700936,-8.34612137072049,
59.9905341966317));
#183200=CARTESIAN_POINT('Ctrl Pts',(5.35927043794044,-6.57498920468546,
60.149201661918));
#183201=CARTESIAN_POINT('Ctrl Pts',(8.74617592502894,-2.07956910621628,
60.3607582823));
#183202=CARTESIAN_POINT('Ctrl Pts',(8.05488525266272,3.97257091875613,60.5723149026819));
#183203=CARTESIAN_POINT('Ctrl Pts',(3.77918417033432,7.58935433274461,60.7838715230638));
#183204=CARTESIAN_POINT('Ctrl Pts',(-1.68372179736957,8.82199393828704,
60.9954281434456));
#183205=CARTESIAN_POINT('Ctrl Pts',(-6.9301175805791,5.72657587904268,61.2069847638278));
#183206=CARTESIAN_POINT('Ctrl Pts',(-8.47662769475153,0.314715098594593,
61.4185413842094));
#183207=CARTESIAN_POINT('Ctrl Pts',(-7.62009081096093,-3.7586825918449,
61.577208849496));
#183208=CARTESIAN_POINT('Ctrl Pts',(-4.88366270812431,-6.95506853439749,
61.7358763147823));
#183209=CARTESIAN_POINT('Ctrl Pts',(-0.968600827846532,-8.43532670445697,
61.8945437800688));
#183210=CARTESIAN_POINT('Ctrl Pts',(3.18008548793708,-7.8810022239752,62.0532112453553));
#183211=CARTESIAN_POINT('Ctrl Pts',(6.56980030649021,-5.38806112867788,
62.2118787106416));
#183212=CARTESIAN_POINT('Ctrl Pts',(8.32733986300889,-1.6148292400918,62.3705461759281));
#183213=CARTESIAN_POINT('Ctrl Pts',(8.04775942552698,4.00671551372531,62.5821027963099));
#183214=CARTESIAN_POINT('Ctrl Pts',(3.63953484345023,8.21074188252331,62.7936594166919));
#183215=CARTESIAN_POINT('Ctrl Pts',(-1.96058313686132,8.24843293872902,
63.0052160370739));
#183216=CARTESIAN_POINT('Ctrl Pts',(-6.94479732065039,5.69493514565335,
63.2167726574556));
#183217=CARTESIAN_POINT('Ctrl Pts',(-8.9899028102379,-0.0429935060496113,
63.4283292778377));
#183218=CARTESIAN_POINT('Ctrl Pts',(-6.71010243984948,-5.1891028044777,
63.6398858982195));
#183219=CARTESIAN_POINT('Ctrl Pts',(-3.44272605438647,-7.76795443524078,
63.798553363506));
#183220=CARTESIAN_POINT('Ctrl Pts',(0.706179398599664,-8.46902889485467,
63.9572208287924));
#183221=CARTESIAN_POINT('Ctrl Pts',(4.66057979410362,-7.09731781431708,
64.1158882940788));
#183222=CARTESIAN_POINT('Ctrl Pts',(7.49085837159483,-4.01374894850164,
64.2745557593653));
#183223=CARTESIAN_POINT('Ctrl Pts',(8.49636896109091,0.0720643499926889,
64.4332232246516));
#183224=CARTESIAN_POINT('Ctrl Pts',(7.42842502653588,4.0952123624847,64.5918906899381));
#183225=CARTESIAN_POINT('Ctrl Pts',(3.61218801807817,8.23239325476728,64.8034473103199));
#183226=CARTESIAN_POINT('Ctrl Pts',(-2.465913987405,8.63607343326995,65.0150039307019));
#183227=CARTESIAN_POINT('Ctrl Pts',(-6.78991034452835,5.07716945694371,
65.2265605510838));
#183228=CARTESIAN_POINT('Ctrl Pts',(-8.98090275980552,-0.076692613904169,
65.4381171714657));
#183229=CARTESIAN_POINT('Ctrl Pts',(-6.87502803419633,-5.79259790664771,
65.6496737918476));
#183230=CARTESIAN_POINT('Ctrl Pts',(-1.82759285440602,-8.28324616483398,
65.8612304122296));
#183231=CARTESIAN_POINT('Ctrl Pts',(2.33334461405416,-8.17000500034077,
66.0198978775159));
#183232=CARTESIAN_POINT('Ctrl Pts',(5.96809149824668,-6.05020856115271,
66.1785653428025));
#183233=CARTESIAN_POINT('Ctrl Pts',(8.1255172111483,-2.46351257881153,66.3372328080887));
#183234=CARTESIAN_POINT('Ctrl Pts',(8.32308565666732,1.71737733671682,66.4959002733753));
#183235=CARTESIAN_POINT('Ctrl Pts',(6.47746095768515,5.49872515545137,66.6545677386617));
#183236=CARTESIAN_POINT('Ctrl Pts',(3.07995689474727,7.90355161906414,66.8132352039482));
#183237=CARTESIAN_POINT('Ctrl Pts',(-2.50078270841206,8.63517728969084,
67.0247918243299));
#183238=CARTESIAN_POINT('Ctrl Pts',(-7.42626117277933,5.05105346752343,
67.2363484447121));
#183239=CARTESIAN_POINT('Ctrl Pts',(-8.46619265772629,-0.451789844414717,
67.4479050650937));
#183240=CARTESIAN_POINT('Ctrl Pts',(-6.84652756553861,-5.81270646363901,
67.6594616854758));
#183241=CARTESIAN_POINT('Ctrl Pts',(-1.56758208377637,-8.85228147935368,
67.8710183058576));
#183242=CARTESIAN_POINT('Ctrl Pts',(3.90359985443053,-7.53088114666553,
68.0825749262395));
#183243=CARTESIAN_POINT('Ctrl Pts',(7.02587515470665,-4.7781332237606,68.241242391526));
#183244=CARTESIAN_POINT('Ctrl Pts',(8.45858844313609,-0.821840200121001,
68.3999098568124));
#183245=CARTESIAN_POINT('Ctrl Pts',(7.81719117440107,3.31427915503444,68.5585773220988));
#183246=CARTESIAN_POINT('Ctrl Pts',(5.29030421491151,6.65100150944047,68.7172447873853));
#183247=CARTESIAN_POINT('Ctrl Pts',(1.45060083629443,8.37193143828057,68.8759122526716));
#183248=CARTESIAN_POINT('Ctrl Pts',(-2.69875727408849,8.04170204896118,
69.0345797179581));
#183249=CARTESIAN_POINT('Ctrl Pts',(-7.45245972838229,5.02802595219296,
69.24613633834));
#183250=CARTESIAN_POINT('Ctrl Pts',(-8.93805989614121,-0.879534781064867,
69.4576929587219));
#183251=CARTESIAN_POINT('Ctrl Pts',(-6.21101134614356,-5.77095054902837,
69.6692495791038));
#183252=CARTESIAN_POINT('Ctrl Pts',(-1.53281601924463,-8.84946163273552,
69.8808061994857));
#183253=CARTESIAN_POINT('Ctrl Pts',(4.46780524364497,-7.80121255215777,
70.0923628198677));
#183254=CARTESIAN_POINT('Ctrl Pts',(7.82206971914578,-3.28138506998721,
70.3039194402494));
#183255=CARTESIAN_POINT('Ctrl Pts',(8.45578532753984,0.832570290180003,
70.4625869055361));
#183256=CARTESIAN_POINT('Ctrl Pts',(7.02115294830815,4.78816781674929,70.6212543708223));
#183257=CARTESIAN_POINT('Ctrl Pts',(3.87877969162206,7.55301213281761,70.7799218361088));
#183258=CARTESIAN_POINT('Ctrl Pts',(-0.199146880583746,8.4960861745185,
70.9385893013953));
#183259=CARTESIAN_POINT('Ctrl Pts',(-4.24987783507853,7.35744637632085,
71.0972567666816));
#183260=CARTESIAN_POINT('Ctrl Pts',(-7.22424387249952,4.44551044756007,
71.2559242319681));
#183261=CARTESIAN_POINT('Ctrl Pts',(-8.94342240817753,-0.914000332600309,
71.4674808523501));
#183262=CARTESIAN_POINT('Ctrl Pts',(-6.29927301645491,-6.40169162036673,
71.6790374727318));
#183263=CARTESIAN_POINT('Ctrl Pts',(-1.07160968101382,-8.41024285456801,
71.8905940931139));
#183264=CARTESIAN_POINT('Ctrl Pts',(4.4926925138143,-7.776773760013,72.1021507134955));
#183265=CARTESIAN_POINT('Ctrl Pts',(8.42846848810263,-3.12747820522319,
72.3137073338779));
#183266=CARTESIAN_POINT('Ctrl Pts',(8.10818867778331,2.49189466755299,72.5252639542594));
#183267=CARTESIAN_POINT('Ctrl Pts',(5.9590647493189,6.05665139387714,72.6839314195461));
#183268=CARTESIAN_POINT('Ctrl Pts',(2.32328994654124,8.17468431128629,72.8425988848323));
#183269=CARTESIAN_POINT('Ctrl Pts',(-1.86082884426617,8.28433703967775,
73.0012663501188));
#183270=CARTESIAN_POINT('Ctrl Pts',(-5.59611972184407,6.39582549978325,
73.1599338154052));
#183271=CARTESIAN_POINT('Ctrl Pts',(-7.97683183085544,2.9263685235767,73.3186012806917));
#183272=CARTESIAN_POINT('Ctrl Pts',(-8.39499320594201,-1.21505215562958,
73.4772687459781));
#183273=CARTESIAN_POINT('Ctrl Pts',(-6.28130928397353,-6.43159036772032,
73.68882536636));
#183274=CARTESIAN_POINT('Ctrl Pts',(-0.735279526433169,-8.95108150762345,
73.900381986742));
#183275=CARTESIAN_POINT('Ctrl Pts',(4.56541761717103,-7.14405306265844,
74.1119386071238));
#183276=CARTESIAN_POINT('Ctrl Pts',(8.43192001011159,-3.09276916066988,
74.3234952275058));
#183277=CARTESIAN_POINT('Ctrl Pts',(8.47518615947612,2.998569749282,74.5350518478876));
#183278=CARTESIAN_POINT('Ctrl Pts',(4.62909106997849,7.10800805673135,74.7466084682696));
#183279=CARTESIAN_POINT('Ctrl Pts',(0.695120786654891,8.46819259851175,
74.9052759335559));
#183280=CARTESIAN_POINT('Ctrl Pts',(-3.45344407599199,7.76510552271418,
75.0639433988424));
#183281=CARTESIAN_POINT('Ctrl Pts',(-6.73632039050628,5.16864699617596,
75.2226108641288));
#183282=CARTESIAN_POINT('Ctrl Pts',(-8.39441072159572,1.3255219357103,75.3812783294153));
#183283=CARTESIAN_POINT('Ctrl Pts',(-7.99956771444687,-2.86363321246058,
75.5399457947017));
#183284=CARTESIAN_POINT('Ctrl Pts',(-5.66734195322239,-6.31137844325295,
75.6986132599881));
#183285=CARTESIAN_POINT('Ctrl Pts',(-0.702331405528227,-8.96252930683599,
75.91016988037));
#183286=CARTESIAN_POINT('Ctrl Pts',(5.17015725800501,-7.34383891882227,
76.1217265007519));
#183287=CARTESIAN_POINT('Ctrl Pts',(8.08239236995815,-2.56036438018052,
76.3332831211339));
#183288=CARTESIAN_POINT('Ctrl Pts',(8.4555991428169,3.0274311344942,76.5448397415157));
#183289=CARTESIAN_POINT('Ctrl Pts',(4.58626387481611,7.73216558602067,76.7563963618976));
#183290=CARTESIAN_POINT('Ctrl Pts',(-0.999627257927594,8.42336085027349,
76.9679529822796));
#183291=CARTESIAN_POINT('Ctrl Pts',(-4.89161787228477,6.94734146167241,
77.1266204475658));
#183292=CARTESIAN_POINT('Ctrl Pts',(-7.62649503650707,3.749628411326,77.2852879128524));
#183293=CARTESIAN_POINT('Ctrl Pts',(-8.48365272152047,-0.347218483476703,
77.4439553781389));
#183294=CARTESIAN_POINT('Ctrl Pts',(-7.29457162466165,-4.36031702718641,
77.6026228434252));
#183295=CARTESIAN_POINT('Ctrl Pts',(-4.30752757594821,-7.32384359308516,
77.7612903087117));
#183296=CARTESIAN_POINT('Ctrl Pts',(-0.307935242167678,-8.47687669813258,
77.919957773998));
#183297=CARTESIAN_POINT('Ctrl Pts',(5.20278957938838,-7.33151973138541,
78.1315143943802));
#183298=CARTESIAN_POINT('Ctrl Pts',(8.67471728284177,-2.32632246278883,
78.3430710147618));
#183299=CARTESIAN_POINT('Ctrl Pts',(7.84612964182211,3.21228607458539,78.5546276351438));
#183300=CARTESIAN_POINT('Ctrl Pts',(4.55273398345825,7.74177688996364,78.7661842555257));
#183301=CARTESIAN_POINT('Ctrl Pts',(-1.43239137558603,8.87515948736878,
78.9777408759076));
#183302=CARTESIAN_POINT('Ctrl Pts',(-6.16414658142105,5.82713991521296,
79.1892974962896));
#183303=CARTESIAN_POINT('Ctrl Pts',(-8.20682568982982,2.20033881260999,
79.3479649615759));
#183304=CARTESIAN_POINT('Ctrl Pts',(-8.25801451613462,-2.00707150251296,
79.5066324268624));
#183305=CARTESIAN_POINT('Ctrl Pts',(-6.29141346134359,-5.70184538838567,
79.6652998921488));
#183306=CARTESIAN_POINT('Ctrl Pts',(-2.80733701712054,-8.02134643543056,
79.8239673574353));
#183307=CARTESIAN_POINT('Ctrl Pts',(1.38480816911518,-8.38306537778871,
79.9826348227216));
#183308=CARTESIAN_POINT('Ctrl Pts',(5.19446800254897,-6.70594995800052,
80.1413022880081));
#183309=CARTESIAN_POINT('Ctrl Pts',(8.69188026524415,-2.29595697558664,
80.35285890839));
#183310=CARTESIAN_POINT('Ctrl Pts',(8.15098066578445,3.77147322993531,80.5644155287719));
#183311=CARTESIAN_POINT('Ctrl Pts',(3.96634325089928,7.49324051377649,80.7759721491538));
#183312=CARTESIAN_POINT('Ctrl Pts',(-1.4642937957338,8.86105748869096,80.9875287695356));
#183313=CARTESIAN_POINT('Ctrl Pts',(-6.78588404143214,5.89677698029374,
81.1990853899178));
#183314=CARTESIAN_POINT('Ctrl Pts',(-8.46620824036368,0.524957807362146,
81.4106420102994));
#183315=CARTESIAN_POINT('Ctrl Pts',(-7.71101266496146,-3.56843978151961,
81.5693094755861));
#183316=CARTESIAN_POINT('Ctrl Pts',(-5.05474249081517,-6.83174341705231,
81.7279769408722));
#183317=CARTESIAN_POINT('Ctrl Pts',(-1.1776173489075,-8.40869440247311,
81.886644406159));
#183318=CARTESIAN_POINT('Ctrl Pts',(2.98354656363832,-7.95748639128541,
82.0453118714451));
#183319=CARTESIAN_POINT('Ctrl Pts',(6.43407764291852,-5.54942552688341,
82.2039793367317));
#183320=CARTESIAN_POINT('Ctrl Pts',(8.2847052562792,-1.82096718402392,82.3626468020181));
#183321=CARTESIAN_POINT('Ctrl Pts',(8.14470429910349,3.80578413198247,82.5742034224));
#183322=CARTESIAN_POINT('Ctrl Pts',(3.84215607714871,8.1179019960172,82.785760042782));
#183323=CARTESIAN_POINT('Ctrl Pts',(-1.75530226663762,8.29454315402551,
82.9973166631638));
#183324=CARTESIAN_POINT('Ctrl Pts',(-6.80134439667575,5.8655102536708,83.2088732835457));
#183325=CARTESIAN_POINT('Ctrl Pts',(-8.98820151561447,0.180095790597725,
83.4204299039276));
#183326=CARTESIAN_POINT('Ctrl Pts',(-6.83679903838358,-5.02100005750552,
83.6319865243096));
#183327=CARTESIAN_POINT('Ctrl Pts',(-3.63442053097905,-7.68013451689011,
83.790653989596));
#183328=CARTESIAN_POINT('Ctrl Pts',(0.495810896822684,-8.48394432557652,
83.9493214548824));
#183329=CARTESIAN_POINT('Ctrl Pts',(4.48303139945561,-7.21078037705518,
84.1079889201689));
#183330=CARTESIAN_POINT('Ctrl Pts',(7.38895437482808,-4.19839171726494,
84.2666563854553));
#183331=CARTESIAN_POINT('Ctrl Pts',(8.49554099952146,-0.138787315627807,
84.4253238507417));
#183332=CARTESIAN_POINT('Ctrl Pts',(7.52775657013251,3.9096219369063,84.5839913160281));
#183333=CARTESIAN_POINT('Ctrl Pts',(3.81535493093217,8.14022528742885,84.7955479364101));
#183334=CARTESIAN_POINT('Ctrl Pts',(-2.25085858000059,8.69460360171458,
85.0071045567919));
#183335=CARTESIAN_POINT('Ctrl Pts',(-6.66183439250307,5.24409140920695,
85.2186611771738));
#183336=CARTESIAN_POINT('Ctrl Pts',(-8.98004044839375,0.146183731388637,
85.4302177975557));
#183337=CARTESIAN_POINT('Ctrl Pts',(-7.01664901784579,-5.62021685875639,
85.6417744179377));
#183338=CARTESIAN_POINT('Ctrl Pts',(-2.03257114091683,-8.2353456045162,
85.8533310383195));
#183339=CARTESIAN_POINT('Ctrl Pts',(2.12989508064693,-8.22538909346939,
86.0119985036061));
#183340=CARTESIAN_POINT('Ctrl Pts',(5.81612353936555,-6.19643823012284,
86.1706659688923));
#183341=CARTESIAN_POINT('Ctrl Pts',(8.06188546297556,-2.66438115826029,
86.3293334341789));
#183342=CARTESIAN_POINT('Ctrl Pts',(8.36313795994383,1.51031891593676,86.4880008994653));
#183343=CARTESIAN_POINT('Ctrl Pts',(6.6119121803671,5.33629985220495,86.6466683647516));
#183344=CARTESIAN_POINT('Ctrl Pts',(3.27512779162817,7.82469172665717,86.8053358300382));
#183345=CARTESIAN_POINT('Ctrl Pts',(-2.28573880132459,8.69457296888152,
87.0168924504199));
#183346=CARTESIAN_POINT('Ctrl Pts',(-7.29863732183906,5.2337739139524,87.2284490708019));
#183347=CARTESIAN_POINT('Ctrl Pts',(-8.47479652211573,-0.241570051930617,
87.440005691184));
#183348=CARTESIAN_POINT('Ctrl Pts',(-6.98865630004681,-5.64102643655628,
87.6515623115655));
#183349=CARTESIAN_POINT('Ctrl Pts',(-1.78676051276461,-8.81065762863984,
87.8631189319479));
#183350=CARTESIAN_POINT('Ctrl Pts',(3.71552607636741,-7.62542645656924,
88.0746755523293));
#183351=CARTESIAN_POINT('Ctrl Pts',(6.90514685062736,-4.9510025009891,88.2333430176163));
#183352=CARTESIAN_POINT('Ctrl Pts',(8.43559070665481,-1.03147912954588,
88.3920104829023));
#183353=CARTESIAN_POINT('Ctrl Pts',(7.89702488093872,3.11928232201967,88.5506779481889));
#183354=CARTESIAN_POINT('Ctrl Pts',(5.45371364623198,6.51767958937793,88.7093454134752));
#183355=CARTESIAN_POINT('Ctrl Pts',(1.6578958472177,8.33335827582775,88.8680128787618));
#183356=CARTESIAN_POINT('Ctrl Pts',(-2.49837894227512,8.10619302320815,
89.026680344048));
#183357=CARTESIAN_POINT('Ctrl Pts',(-7.32539921680512,5.21140358190732,
89.2382369644301));
#183358=CARTESIAN_POINT('Ctrl Pts',(-8.95713255675292,-0.657474333237619,
89.4497935848118));
#183359=CARTESIAN_POINT('Ctrl Pts',(-6.35229963241242,-5.61505312185985,
89.661350205194));
#183360=CARTESIAN_POINT('Ctrl Pts',(-1.75193518140865,-8.8087013377826,
89.8729068255757));
#183361=CARTESIAN_POINT('Ctrl Pts',(4.27284971566023,-7.90967485339745,
90.0844634459577));
#183362=CARTESIAN_POINT('Ctrl Pts',(7.73823666394516,-3.4744720464393,90.2960200663396));
#183363=CARTESIAN_POINT('Ctrl Pts',(8.47384110833154,0.622491497353808,
90.4546875316259));
#183364=CARTESIAN_POINT('Ctrl Pts',(7.13780494130685,4.61247009581071,90.6133549969124));
#183365=CARTESIAN_POINT('Ctrl Pts',(4.06500630727874,7.45443813418621,90.772022462199));
#183366=CARTESIAN_POINT('Ctrl Pts',(0.0117368987456195,8.4984117345598,
90.9306899274851));
#183367=CARTESIAN_POINT('Ctrl Pts',(-4.06600105450924,7.46063765493643,
91.0893573927718));
#183368=CARTESIAN_POINT('Ctrl Pts',(-7.11170821157464,4.62340447961477,
91.2480248580581));
#183369=CARTESIAN_POINT('Ctrl Pts',(-8.96334864812165,-0.691796206529803,
91.45958147844));
#183370=CARTESIAN_POINT('Ctrl Pts',(-6.45618537723826,-6.24340984660604,
91.671138098822));
#183371=CARTESIAN_POINT('Ctrl Pts',(-1.27997205161572,-8.38106220764725,
91.8826947192038));
#183372=CARTESIAN_POINT('Ctrl Pts',(4.29833574849777,-7.88586114075367,
92.0942513395859));
#183373=CARTESIAN_POINT('Ctrl Pts',(8.34826776812752,-3.335659792342,92.3058079599677));
#183374=CARTESIAN_POINT('Ctrl Pts',(8.1675260770041,2.28993022844238,92.5173645803496));
#183375=CARTESIAN_POINT('Ctrl Pts',(6.10752001411662,5.90691781461061,92.6760320456359));
#183376=CARTESIAN_POINT('Ctrl Pts',(2.52542173879755,8.11451691780934,92.8346995109225));
#183377=CARTESIAN_POINT('Ctrl Pts',(-1.65468776361244,8.32796088946025,
92.9933669762088));
#183378=CARTESIAN_POINT('Ctrl Pts',(-5.43569013627816,6.53271861524583,
93.1520344414954));
#183379=CARTESIAN_POINT('Ctrl Pts',(-7.9017605278901,3.12340509203412,93.3107019067816));
#183380=CARTESIAN_POINT('Ctrl Pts',(-8.4225586341559,-1.0063640885058,93.4693693720683));
#183381=CARTESIAN_POINT('Ctrl Pts',(-6.43896909112289,-6.27374514475321,
93.6809259924499));
#183382=CARTESIAN_POINT('Ctrl Pts',(-0.957165855123717,-8.93008003956348,
93.892482612832));
#183383=CARTESIAN_POINT('Ctrl Pts',(4.38673882053551,-7.255139882753,94.1040392332139));
#183384=CARTESIAN_POINT('Ctrl Pts',(8.35257953053373,-3.30104706023637,
94.3155958535957));
#183385=CARTESIAN_POINT('Ctrl Pts',(8.54698316275725,2.78734255347677,94.5271524739777));
#183386=CARTESIAN_POINT('Ctrl Pts',(4.80404436667829,6.99095285739496,94.7387090943597));
#183387=CARTESIAN_POINT('Ctrl Pts',(0.905036893913656,8.44833621775569,
94.8973765596459));
#183388=CARTESIAN_POINT('Ctrl Pts',(-3.259696538621,7.84840873135576,95.0560440249325));
#183389=CARTESIAN_POINT('Ctrl Pts',(-6.60599159996829,5.3342105846383,95.2147114902188));
#183390=CARTESIAN_POINT('Ctrl Pts',(-8.35893323994751,1.53341403979869,
95.3733789555053));
#183391=CARTESIAN_POINT('Ctrl Pts',(-8.06816498394215,-2.66425108675267,
95.5320464207917));
#183392=CARTESIAN_POINT('Ctrl Pts',(-5.82220414294444,-6.16880266698849,
95.6907138860781));
#183393=CARTESIAN_POINT('Ctrl Pts',(-0.924520356739141,-8.94234775723183,
95.9022705064601));
#183394=CARTESIAN_POINT('Ctrl Pts',(4.98635084039052,-7.46985905065529,
96.113827126842));
#183395=CARTESIAN_POINT('Ctrl Pts',(8.01635169065955,-2.76014623326642,
96.3253837472238));
#183396=CARTESIAN_POINT('Ctrl Pts',(8.52816518653268,2.81671375682173,96.5369403676058));
#183397=CARTESIAN_POINT('Ctrl Pts',(4.77662445525099,7.61591549636984,96.7484969879877));
#183398=CARTESIAN_POINT('Ctrl Pts',(-0.790185932557508,8.44565266194666,
96.9600536083696));
#183399=CARTESIAN_POINT('Ctrl Pts',(-4.71796379787996,7.06641305365506,
97.118721073656));
#183400=CARTESIAN_POINT('Ctrl Pts',(-7.5306283820057,3.93804937156272,97.2773885389424));
#183401=CARTESIAN_POINT('Ctrl Pts',(-8.49055988674188,-0.137227805231727,
97.4360560042289));
#183402=CARTESIAN_POINT('Ctrl Pts',(-7.39881793188242,-4.17677760456979,
97.5947234695152));
#183403=CARTESIAN_POINT('Ctrl Pts',(-4.49111326487404,-7.21691544666963,
97.7533909348017));
#183404=CARTESIAN_POINT('Ctrl Pts',(-0.512538772771953,-8.46270402734996,
97.9120584000882));
#183405=CARTESIAN_POINT('Ctrl Pts',(5.0068590599844,-7.4668239237907,98.12361502047));
#183406=CARTESIAN_POINT('Ctrl Pts',(9.54195894481759,-1.29323553776124,
98.3880607959474));
#183407=CARTESIAN_POINT('Ctrl Pts',(6.81343712599511,5.86535702163415,98.6525065714248));
#183408=CARTESIAN_POINT('Ctrl Pts',(1.75834181031916,8.29349105181592,98.8640631918067));
#183409=CARTESIAN_POINT('Ctrl Pts',(-2.40877456271746,8.15273538577312,
99.0227306570931));
#183410=CARTESIAN_POINT('Ctrl Pts',(-6.01967976731674,5.99363558096764,
99.1813981223796));
#183411=CARTESIAN_POINT('Ctrl Pts',(-8.14915213644516,2.39503477083037,
99.340065587666));
#183412=CARTESIAN_POINT('Ctrl Pts',(-8.304600130319,-1.79807814568109,99.4987486186825));
#183413=CARTESIAN_POINT('Ctrl Pts',(-7.05661567854373,-4.29650290335088,
99.6045424946037));
#183414=CARTESIAN_POINT('Ctrl Pts',(-6.1720159842572,-5.32232154063713,
99.6574472154292));
#183415=CARTESIAN_POINT('Ctrl Pts',(2.0091828425417,-7.50340179875822,-0.206423361386482));
#183416=CARTESIAN_POINT('Ctrl Pts',(3.2560570208879,-7.16952802062857,-0.153528389248873));
#183417=CARTESIAN_POINT('Ctrl Pts',(5.57898372095689,-5.87036363360852,
-0.0477442620157891));
#183418=CARTESIAN_POINT('Ctrl Pts',(7.70519809246894,-2.48345330685785,
0.110929020312771));
#183419=CARTESIAN_POINT('Ctrl Pts',(7.95736644885961,1.49394517220418,0.269596485599199));
#183420=CARTESIAN_POINT('Ctrl Pts',(6.27029174751694,5.13167437923139,0.428263950885628));
#183421=CARTESIAN_POINT('Ctrl Pts',(3.06251395397477,7.47745566527645,0.586931416172058));
#183422=CARTESIAN_POINT('Ctrl Pts',(-2.22263135598543,8.27544619949939,
0.79848803655396));
#183423=CARTESIAN_POINT('Ctrl Pts',(-8.21167961142144,4.09854069893237,
1.06293381203135));
#183424=CARTESIAN_POINT('Ctrl Pts',(-7.9494565368908,-3.19785807327113,
1.32737958750873));
#183425=CARTESIAN_POINT('Ctrl Pts',(-4.13483212757085,-6.94263763572355,
1.53893620789063));
#183426=CARTESIAN_POINT('Ctrl Pts',(-0.331984144492666,-8.09484453700046,
1.69760367317706));
#183427=CARTESIAN_POINT('Ctrl Pts',(3.58945996307169,-7.25896364686547,
1.85627113846349));
#183428=CARTESIAN_POINT('Ctrl Pts',(6.61610676689296,-4.66172205022977,
2.01493860374992));
#183429=CARTESIAN_POINT('Ctrl Pts',(8.04540311823364,-0.935991074654104,
2.17360606903635));
#183430=CARTESIAN_POINT('Ctrl Pts',(7.50709055642592,3.03731311691104,2.33227353432277));
#183431=CARTESIAN_POINT('Ctrl Pts',(5.15210277994162,6.23053426445669,2.49094099960921));
#183432=CARTESIAN_POINT('Ctrl Pts',(0.321019198565415,8.56233974321341,
2.70249761999111));
#183433=CARTESIAN_POINT('Ctrl Pts',(-5.20869192847317,6.79305464573205,
2.91405424037301));
#183434=CARTESIAN_POINT('Ctrl Pts',(-7.79637889262264,2.12455969260576,
3.12561086075492));
#183435=CARTESIAN_POINT('Ctrl Pts',(-7.93492590961988,-3.21124827819366,
3.33716748113683));
#183436=CARTESIAN_POINT('Ctrl Pts',(-4.06747156186517,-7.54149967621007,
3.54872410151873));
#183437=CARTESIAN_POINT('Ctrl Pts',(1.27889791109489,-7.98291927192884,
3.76028072190064));
#183438=CARTESIAN_POINT('Ctrl Pts',(4.92802597814904,-6.42622521871537,
3.91894818718706));
#183439=CARTESIAN_POINT('Ctrl Pts',(7.40838574129789,-3.27483184280127,
4.07761565247349));
#183440=CARTESIAN_POINT('Ctrl Pts',(8.06566255913872,0.659938011782959,
4.23628311775992));
#183441=CARTESIAN_POINT('Ctrl Pts',(6.77751790413037,4.4355349111222,4.39495058304635));
#183442=CARTESIAN_POINT('Ctrl Pts',(3.81787759238652,7.14181922457694,4.55361804833277));
#183443=CARTESIAN_POINT('Ctrl Pts',(-0.035760713279578,8.08463795235184,
4.71228551361921));
#183444=CARTESIAN_POINT('Ctrl Pts',(-5.23927076131497,6.78000543459735,
4.9238421340011));
#183445=CARTESIAN_POINT('Ctrl Pts',(-8.35138480077202,1.87870792817531,
5.13539875438302));
#183446=CARTESIAN_POINT('Ctrl Pts',(-7.34733543235467,-3.36365117040484,
5.34695537476492));
#183447=CARTESIAN_POINT('Ctrl Pts',(-4.03517086503427,-7.54934216915915,
5.55851199514683));
#183448=CARTESIAN_POINT('Ctrl Pts',(1.70856436411669,-8.39638260750436,
5.77006861552873));
#183449=CARTESIAN_POINT('Ctrl Pts',(6.09639927703859,-5.31004370370416,
5.98162523591064));
#183450=CARTESIAN_POINT('Ctrl Pts',(7.9009131931023,-1.77689162408361,6.14029270119706));
#183451=CARTESIAN_POINT('Ctrl Pts',(7.78635900127687,2.23188959023923,6.2989601664835));
#183452=CARTESIAN_POINT('Ctrl Pts',(5.77012326512224,5.67416118083297,6.45762763176992));
#183453=CARTESIAN_POINT('Ctrl Pts',(2.36214621252141,7.74783730563748,6.61629509705636));
#183454=CARTESIAN_POINT('Ctrl Pts',(-1.64415034387486,7.92959915502436,
6.77496256234278));
#183455=CARTESIAN_POINT('Ctrl Pts',(-5.20706575041264,6.18458685704297,
6.93363002762921));
#183456=CARTESIAN_POINT('Ctrl Pts',(-8.36655083678149,1.84912413462387,
7.14518664801111));
#183457=CARTESIAN_POINT('Ctrl Pts',(-7.61594695241928,-3.90800758085578,
7.35674326839301));
#183458=CARTESIAN_POINT('Ctrl Pts',(-3.48638659873253,-7.28989681825855,
7.56829988877493));
#183459=CARTESIAN_POINT('Ctrl Pts',(1.73839828376926,-8.3817147792673,7.77985650915683));
#183460=CARTESIAN_POINT('Ctrl Pts',(6.69119414888973,-5.35222886581472,
7.99141312953873));
#183461=CARTESIAN_POINT('Ctrl Pts',(8.08290140003575,-0.171327983243689,
8.20296974992065));
#183462=CARTESIAN_POINT('Ctrl Pts',(7.20483765210341,3.69757860246291,8.36163721520705));
#183463=CARTESIAN_POINT('Ctrl Pts',(4.54856395562032,6.70218498570296,8.52030468049351));
#183464=CARTESIAN_POINT('Ctrl Pts',(0.795099983554925,8.05346159237329,
8.67897214577991));
#183465=CARTESIAN_POINT('Ctrl Pts',(-3.1501403937012,7.46226059186625,8.83763961106636));
#183466=CARTESIAN_POINT('Ctrl Pts',(-6.34268067388839,5.03509433711445,
8.99630707635277));
#183467=CARTESIAN_POINT('Ctrl Pts',(-7.9603547852174,1.41258628551333,9.15497454163922));
#183468=CARTESIAN_POINT('Ctrl Pts',(-7.60863814334965,-3.94043888084814,
9.36653116202111));
#183469=CARTESIAN_POINT('Ctrl Pts',(-3.34387587171949,-7.87995338746789,
9.57808778240303));
#183470=CARTESIAN_POINT('Ctrl Pts',(1.99354289033037,-7.83091781855655,
9.7896444027849));
#183471=CARTESIAN_POINT('Ctrl Pts',(6.70470377450696,-5.32185292264324,
10.0012010231668));
#183472=CARTESIAN_POINT('Ctrl Pts',(8.56662008808325,0.177350603561869,
10.2127576435487));
#183473=CARTESIAN_POINT('Ctrl Pts',(6.31592966174266,5.04694767443379,10.4243142639306));
#183474=CARTESIAN_POINT('Ctrl Pts',(3.16303655392699,7.45499650389469,10.5829817292171));
#183475=CARTESIAN_POINT('Ctrl Pts',(-0.801457265604823,8.06017269618677,
10.7416491945035));
#183476=CARTESIAN_POINT('Ctrl Pts',(-4.54914554329267,6.69295916838177,
10.9003166597899));
#183477=CARTESIAN_POINT('Ctrl Pts',(-7.1995897044865,3.71141829062658,11.0589841250764));
#183478=CARTESIAN_POINT('Ctrl Pts',(-8.09584708868326,-0.19756778892084,
11.2176515903628));
#183479=CARTESIAN_POINT('Ctrl Pts',(-7.01707718806656,-4.01537993934193,
11.3763190556492));
#183480=CARTESIAN_POINT('Ctrl Pts',(-3.31748621190696,-7.90017203635101,
11.5878756760311));
#183481=CARTESIAN_POINT('Ctrl Pts',(2.48099785437956,-8.19266872763073,
11.799432296413));
#183482=CARTESIAN_POINT('Ctrl Pts',(6.54772669008474,-4.73547910232167,
12.0109889167949));
#183483=CARTESIAN_POINT('Ctrl Pts',(8.55753192423801,0.209328927245312,
12.2225455371769));
#183484=CARTESIAN_POINT('Ctrl Pts',(6.46394670622404,5.62457340153279,12.4341021575587));
#183485=CARTESIAN_POINT('Ctrl Pts',(1.61601643183833,7.92156166501164,12.6456587779407));
#183486=CARTESIAN_POINT('Ctrl Pts',(-2.34759045671714,7.75052205739014,
12.8043262432271));
#183487=CARTESIAN_POINT('Ctrl Pts',(-5.77930409700375,5.67524112221684,
12.9629937085135));
#183488=CARTESIAN_POINT('Ctrl Pts',(-7.78089482178619,2.2244332707425,13.1216611737999));
#183489=CARTESIAN_POINT('Ctrl Pts',(-7.90575045796466,-1.7629030992477,
13.2803286390864));
#183490=CARTESIAN_POINT('Ctrl Pts',(-6.08952802662705,-5.33848494682565,
13.4389961043728));
#183491=CARTESIAN_POINT('Ctrl Pts',(-2.81526475330063,-7.57871576781822,
13.5976635696592));
#183492=CARTESIAN_POINT('Ctrl Pts',(2.51421374331843,-8.19128574907772,
13.8092201900411));
#183493=CARTESIAN_POINT('Ctrl Pts',(7.15376540808352,-4.70093732358155,
14.020776810423));
#183494=CARTESIAN_POINT('Ctrl Pts',(8.06132892646283,0.558983967522269,
14.2323334308049));
#183495=CARTESIAN_POINT('Ctrl Pts',(6.43648104260328,5.64330426455488,14.4438900511868));
#183496=CARTESIAN_POINT('Ctrl Pts',(1.35959684764904,8.45990126313526,14.6554466715687));
#183497=CARTESIAN_POINT('Ctrl Pts',(-3.83432973476785,7.11762346613171,
14.8670032919507));
#183498=CARTESIAN_POINT('Ctrl Pts',(-6.76806196776461,4.44692144242042,
15.0256707572371));
#183499=CARTESIAN_POINT('Ctrl Pts',(-8.07340337475109,0.654885936253715,
15.1843382225235));
#183500=CARTESIAN_POINT('Ctrl Pts',(-7.39941366756805,-3.27705736597523,
15.3430056878099));
#183501=CARTESIAN_POINT('Ctrl Pts',(-4.94070130533272,-6.4185814828846,
15.5016731530964));
#183502=CARTESIAN_POINT('Ctrl Pts',(-1.25540207466762,-8.00035866355257,
15.6603406183828));
#183503=CARTESIAN_POINT('Ctrl Pts',(2.69387807414514,-7.62270747452594,
15.8190080836692));
#183504=CARTESIAN_POINT('Ctrl Pts',(7.17838299420069,-4.67859493424099,
16.0305647040511));
#183505=CARTESIAN_POINT('Ctrl Pts',(8.50452392902259,0.973778195903384,
16.2421213244331));
#183506=CARTESIAN_POINT('Ctrl Pts',(5.83147495731057,5.59387048105627,16.4536779448149));
#183507=CARTESIAN_POINT('Ctrl Pts',(1.32650797202072,8.45668657538519,16.6652345651969));
#183508=CARTESIAN_POINT('Ctrl Pts',(-4.37611184800845,7.36668704804644,
16.8767911855787));
#183509=CARTESIAN_POINT('Ctrl Pts',(-7.50412016787103,3.00845954380391,
17.0883478059607));
#183510=CARTESIAN_POINT('Ctrl Pts',(-8.04563436084246,-0.921705400977682,
17.247015271247));
#183511=CARTESIAN_POINT('Ctrl Pts',(-6.61843941011529,-4.66958000419504,
17.4056827365335));
#183512=CARTESIAN_POINT('Ctrl Pts',(-3.58185128358946,-7.25677400681142,
17.5643502018199));
#183513=CARTESIAN_POINT('Ctrl Pts',(0.31867166534931,-8.09364973362753,
17.7230176671064));
#183514=CARTESIAN_POINT('Ctrl Pts',(4.16169756931217,-6.94708906349569,
17.8816851323928));
#183515=CARTESIAN_POINT('Ctrl Pts',(6.95205909546775,-4.12692653843969,
18.0403525976792));
#183516=CARTESIAN_POINT('Ctrl Pts',(8.50911149226834,1.00670481387645,18.2519092180611));
#183517=CARTESIAN_POINT('Ctrl Pts',(5.90601885240856,6.19629829407277,18.4634658384431));
#183518=CARTESIAN_POINT('Ctrl Pts',(0.893646742785605,8.03111963773931,
18.6750224588249));
#183519=CARTESIAN_POINT('Ctrl Pts',(-4.39945838513347,7.34301962081084,
18.8865790792069));
#183520=CARTESIAN_POINT('Ctrl Pts',(-8.07967631497109,2.85258893208078,
19.0981356995887));
#183521=CARTESIAN_POINT('Ctrl Pts',(-7.68920659426301,-2.4977490408958,
19.3096923199707));
#183522=CARTESIAN_POINT('Ctrl Pts',(-5.58703866671401,-5.86231797595484,
19.4683597852571));
#183523=CARTESIAN_POINT('Ctrl Pts',(-2.09005686812911,-7.82562329331867,
19.6270272505435));
#183524=CARTESIAN_POINT('Ctrl Pts',(1.89902288646746,-7.8666472960441,19.7856947158299));
#183525=CARTESIAN_POINT('Ctrl Pts',(5.43006240703896,-6.01025289789105,
19.9443621811164));
#183526=CARTESIAN_POINT('Ctrl Pts',(7.6462209924854,-2.66778515788588,20.1030296464028));
#183527=CARTESIAN_POINT('Ctrl Pts',(7.98189786707622,1.28528392198672,20.2616971116892));
#183528=CARTESIAN_POINT('Ctrl Pts',(5.88844605642552,6.22451893809486,20.4732537320711));
#183529=CARTESIAN_POINT('Ctrl Pts',(0.564923425653677,8.54143036951552,
20.684810352453));
#183530=CARTESIAN_POINT('Ctrl Pts',(-4.4591660822607,6.73894093959792,20.8963669728349));
#183531=CARTESIAN_POINT('Ctrl Pts',(-8.082439033227,2.8194592581385,21.1079235932168));
#183532=CARTESIAN_POINT('Ctrl Pts',(-8.03126456115619,-2.98617188367512,
21.3194802135988));
#183533=CARTESIAN_POINT('Ctrl Pts',(-4.30364004228442,-6.84407266961708,
21.5310368339806));
#183534=CARTESIAN_POINT('Ctrl Pts',(-0.533978119676184,-8.08063366836214,
21.6897042992671));
#183535=CARTESIAN_POINT('Ctrl Pts',(3.4088897612777,-7.34766549567967,21.8483717645535));
#183536=CARTESIAN_POINT('Ctrl Pts',(6.49804381946639,-4.82346909640559,
22.00703922984));
#183537=CARTESIAN_POINT('Ctrl Pts',(8.01988369045738,-1.13586232989786,
22.1657066951263));
#183538=CARTESIAN_POINT('Ctrl Pts',(7.58005275125885,2.85036373164785,22.3243741604128));
#183539=CARTESIAN_POINT('Ctrl Pts',(5.30516600064393,6.1006443943378,22.4830416256992));
#183540=CARTESIAN_POINT('Ctrl Pts',(0.533350586535182,8.55184015998767,
22.6945982460811));
#183541=CARTESIAN_POINT('Ctrl Pts',(-5.03850667602932,6.92016052629867,
22.9061548664631));
#183542=CARTESIAN_POINT('Ctrl Pts',(-7.74126660981814,2.31738611635783,
23.1177114868449));
#183543=CARTESIAN_POINT('Ctrl Pts',(-8.01216053127736,-3.01337930821458,
23.3292681072269));
#183544=CARTESIAN_POINT('Ctrl Pts',(-4.25335765412606,-7.43823780449522,
23.5408247276087));
#183545=CARTESIAN_POINT('Ctrl Pts',(1.08041685410531,-8.01219993147444,
23.7523813479907));
#183546=CARTESIAN_POINT('Ctrl Pts',(4.76704696570923,-6.5465285717915,23.9110488132771));
#183547=CARTESIAN_POINT('Ctrl Pts',(7.3248431091507,-3.45765687529476,24.0697162785635));
#183548=CARTESIAN_POINT('Ctrl Pts',(8.07955452782502,0.459593554771575,
24.22838374385));
#183549=CARTESIAN_POINT('Ctrl Pts',(6.88549477943484,4.26599100834977,24.3870512091364));
#183550=CARTESIAN_POINT('Ctrl Pts',(3.99391953046181,7.04488324237925,24.5457186744228));
#183551=CARTESIAN_POINT('Ctrl Pts',(0.164863081889657,8.08303584581827,
24.7043861397092));
#183552=CARTESIAN_POINT('Ctrl Pts',(-5.06941801282327,6.90792544700635,
24.9159427600911));
#183553=CARTESIAN_POINT('Ctrl Pts',(-8.30219487472764,2.08536123877397,
25.127499380473));
#183554=CARTESIAN_POINT('Ctrl Pts',(-7.42853894049362,-3.18029815365528,
25.339056000855));
#183555=CARTESIAN_POINT('Ctrl Pts',(-4.22125825449852,-7.44688861088727,
25.5506126212369));
#183556=CARTESIAN_POINT('Ctrl Pts',(1.49968985936297,-8.43619364973677,
25.7621692416187));
#183557=CARTESIAN_POINT('Ctrl Pts',(5.96275831201656,-5.45968512215048,
25.9737258620007));
#183558=CARTESIAN_POINT('Ctrl Pts',(7.85438846261605,-1.97239828454699,
26.1323933272871));
#183559=CARTESIAN_POINT('Ctrl Pts',(7.83934371373296,2.03799111354809,26.2910607925735));
#183560=CARTESIAN_POINT('Ctrl Pts',(5.9091455699583,5.52923378387345,26.44972825786));
#183561=CARTESIAN_POINT('Ctrl Pts',(2.55367422961529,7.68683716296529,26.6083957231464));
#183562=CARTESIAN_POINT('Ctrl Pts',(-1.4468784716737,7.96795555978871,26.7670631884328));
#183563=CARTESIAN_POINT('Ctrl Pts',(-5.05199765166073,6.31189100414194,
26.9257306537192));
#183564=CARTESIAN_POINT('Ctrl Pts',(-8.31809034695746,2.05616291912584,
27.1372872741011));
#183565=CARTESIAN_POINT('Ctrl Pts',(-7.71057544278213,-3.71782161692833,
27.3488438944831));
#183566=CARTESIAN_POINT('Ctrl Pts',(-3.66620507739025,-7.20114070596396,
27.5604005148649));
#183567=CARTESIAN_POINT('Ctrl Pts',(1.52987856327207,-8.42227064488995,
27.7719571352469));
#183568=CARTESIAN_POINT('Ctrl Pts',(6.5563232503647,-5.51661657239854,27.9835137556287));
#183569=CARTESIAN_POINT('Ctrl Pts',(8.07616119803516,-0.371844892266704,
28.1950703760107));
#183570=CARTESIAN_POINT('Ctrl Pts',(7.29437113081824,3.51765872711467,28.353737841297));
#183571=CARTESIAN_POINT('Ctrl Pts',(4.71347185117461,6.58725289852531,28.5124053065836));
#183572=CARTESIAN_POINT('Ctrl Pts',(0.994694301570285,8.03125213463683,
28.6710727718699));
#183573=CARTESIAN_POINT('Ctrl Pts',(-2.96400137325586,7.53813063698705,
28.8297402371564));
#183574=CARTESIAN_POINT('Ctrl Pts',(-6.21578648608584,5.19093165760762,
28.9884077024428));
#183575=CARTESIAN_POINT('Ctrl Pts',(-7.92285164960296,1.60968011074781,
29.1470751677293));
#183576=CARTESIAN_POINT('Ctrl Pts',(-7.70407363670064,-3.75042429205407,
29.3586317881111));
#183577=CARTESIAN_POINT('Ctrl Pts',(-3.53837993550241,-7.79455185794337,
29.5701884084931));
#183578=CARTESIAN_POINT('Ctrl Pts',(1.79861211977617,-7.87797445915938,
29.7817450288749));
#183579=CARTESIAN_POINT('Ctrl Pts',(6.57058246686297,-5.48658521124823,
29.9933016492569));
#183580=CARTESIAN_POINT('Ctrl Pts',(8.56838307527957,-0.0352766976527707,
30.2048582696387));
#183581=CARTESIAN_POINT('Ctrl Pts',(6.43922018549342,4.88866972941389,30.4164148900207));
#183582=CARTESIAN_POINT('Ctrl Pts',(3.34705139215976,7.3742131846592,30.575082355307));
#183583=CARTESIAN_POINT('Ctrl Pts',(-0.601204811662946,8.07757825188831,
30.7337498205936));
#183584=CARTESIAN_POINT('Ctrl Pts',(-4.38166524394992,6.80378110271389,
30.8924172858799));
#183585=CARTESIAN_POINT('Ctrl Pts',(-7.10527744757138,3.88892659148757,
31.0510847511664));
#183586=CARTESIAN_POINT('Ctrl Pts',(-8.09825670521013,0.00338394435035205,
31.2097522164528));
#183587=CARTESIAN_POINT('Ctrl Pts',(-7.11455442523969,-3.84002130864605,
31.3684196817392));
#183588=CARTESIAN_POINT('Ctrl Pts',(-3.51250010842368,-7.81541911598213,
31.5799763021212));
#183589=CARTESIAN_POINT('Ctrl Pts',(2.27694047685335,-8.25170971974905,
31.791532922503));
#183590=CARTESIAN_POINT('Ctrl Pts',(6.42820403801672,-4.89649670501255,
32.003089542885));
#183591=CARTESIAN_POINT('Ctrl Pts',(8.56009122212236,-0.00308270630504298,
32.2146461632669));
#183592=CARTESIAN_POINT('Ctrl Pts',(6.60152489708165,5.46244469110179,32.4262027836487));
#183593=CARTESIAN_POINT('Ctrl Pts',(1.81208500248022,7.87902254498234,32.6377594040307));
#183594=CARTESIAN_POINT('Ctrl Pts',(-2.15454561498722,7.80638881349754,
32.796426869317));
#183595=CARTESIAN_POINT('Ctrl Pts',(-5.6366987363262,5.8169016664238,32.9550943346036));
#183596=CARTESIAN_POINT('Ctrl Pts',(-7.72330171866522,2.41682398327808,
33.1137617998899));
#183597=CARTESIAN_POINT('Ctrl Pts',(-7.94706094494807,-1.56618644427357,
33.2724292651764));
#183598=CARTESIAN_POINT('Ctrl Pts',(-6.22012248880763,-5.18573517823562,
33.4310967304628));
#183599=CARTESIAN_POINT('Ctrl Pts',(-3.00245665437853,-7.50652398644883,
33.5897641957493));
#183600=CARTESIAN_POINT('Ctrl Pts',(2.31018045539937,-8.25115138835942,
33.8013208161311));
#183601=CARTESIAN_POINT('Ctrl Pts',(7.03491326880379,-4.87700384811648,
34.0128774365131));
#183602=CARTESIAN_POINT('Ctrl Pts',(8.07271737727317,0.358777484306035,
34.2244340568949));
#183603=CARTESIAN_POINT('Ctrl Pts',(6.57453247949466,5.48185132142458,34.4359906772769));
#183604=CARTESIAN_POINT('Ctrl Pts',(1.56910276939402,8.42355919248004,34.6475472976587));
#183605=CARTESIAN_POINT('Ctrl Pts',(-3.65653189023152,7.21057715139873,
34.8591039180407));
#183606=CARTESIAN_POINT('Ctrl Pts',(-6.65563176020345,4.61349531127234,
35.0177713833271));
#183607=CARTESIAN_POINT('Ctrl Pts',(-8.05466705749516,0.855018265212991,
35.1764388486135));
#183608=CARTESIAN_POINT('Ctrl Pts',(-7.4784523906474,-3.09243875355764,
35.3351063139));
#183609=CARTESIAN_POINT('Ctrl Pts',(-5.09845109881096,-6.29400619907375,
35.4937737791864));
#183610=CARTESIAN_POINT('Ctrl Pts',(-1.45353695844748,-7.96674358976034,
35.6524412444728));
#183611=CARTESIAN_POINT('Ctrl Pts',(2.50389820451343,-7.68720639127034,
35.8111087097592));
#183612=CARTESIAN_POINT('Ctrl Pts',(7.06007768032758,-4.85527920081592,
36.0226653301412));
#183613=CARTESIAN_POINT('Ctrl Pts',(8.52606864495294,0.762446519885064,
36.234221950523));
#183614=CARTESIAN_POINT('Ctrl Pts',(5.96848603223279,5.44744542144437,36.445778570905));
#183615=CARTESIAN_POINT('Ctrl Pts',(1.53594431289278,8.42116656418975,36.6573351912868));
#183616=CARTESIAN_POINT('Ctrl Pts',(-4.19196689926189,7.47300786066947,
36.8688918116688));
#183617=CARTESIAN_POINT('Ctrl Pts',(-7.42715740707066,3.19374093676189,
37.0804484320506));
#183618=CARTESIAN_POINT('Ctrl Pts',(-8.06602823852491,-0.721776675903932,
37.2391158973371));
#183619=CARTESIAN_POINT('Ctrl Pts',(-6.73227275918578,-4.50391175944539,
37.3977833626235));
#183620=CARTESIAN_POINT('Ctrl Pts',(-3.76081845541284,-7.16565922641535,
37.5564508279099));
#183621=CARTESIAN_POINT('Ctrl Pts',(0.11773716752723,-8.09906510656189,
37.7151182931964));
#183622=CARTESIAN_POINT('Ctrl Pts',(3.98803057509151,-7.04821858675621,
37.8737857584828));
#183623=CARTESIAN_POINT('Ctrl Pts',(6.8475126074327,-4.29816465617636,38.0324532237692));
#183624=CARTESIAN_POINT('Ctrl Pts',(8.53147183894502,0.795249163107236,
38.2440098441512));
#183625=CARTESIAN_POINT('Ctrl Pts',(6.05795565866709,6.04783799979448,38.455566464533));
#183626=CARTESIAN_POINT('Ctrl Pts',(1.09265632186101,8.0064717134872,38.667123084915));
#183627=CARTESIAN_POINT('Ctrl Pts',(-4.21589353275059,7.44992704357874,
38.8786797052968));
#183628=CARTESIAN_POINT('Ctrl Pts',(-8.00640411493513,3.05220020943656,
39.0902363256788));
#183629=CARTESIAN_POINT('Ctrl Pts',(-7.7488182757015,-2.30617944893889,
39.3017929460607));
#183630=CARTESIAN_POINT('Ctrl Pts',(-5.73078628192673,-5.72187571565837,
39.4604604113471));
#183631=CARTESIAN_POINT('Ctrl Pts',(-2.28359885268831,-7.77135084273937,
39.6191278766335));
#183632=CARTESIAN_POINT('Ctrl Pts',(1.70323462649298,-7.91134750916685,
39.7777953419201));
#183633=CARTESIAN_POINT('Ctrl Pts',(5.27925157867091,-6.14314417949359,
39.9364628072063));
#183634=CARTESIAN_POINT('Ctrl Pts',(7.57766799383721,-2.85669754957289,
40.0951302724929));
#183635=CARTESIAN_POINT('Ctrl Pts',(8.01133323235648,1.08682480680852,40.2537977377792));
#183636=CARTESIAN_POINT('Ctrl Pts',(6.04108854261124,6.07648600676953,40.4653543581612));
#183637=CARTESIAN_POINT('Ctrl Pts',(0.776697109145226,8.52478227491935,
40.6769109785431));
#183638=CARTESIAN_POINT('Ctrl Pts',(-4.29057249427801,6.84751595893862,
40.8884675989249));
#183639=CARTESIAN_POINT('Ctrl Pts',(-8.0099880644816,3.01914929094193,41.1000242193069));
#183640=CARTESIAN_POINT('Ctrl Pts',(-8.1028906748984,-2.78596404872365,
41.3115808396888));
#183641=CARTESIAN_POINT('Ctrl Pts',(-4.47214416453986,-6.73517445149922,
41.5231374600707));
#183642=CARTESIAN_POINT('Ctrl Pts',(-0.734327091130077,-8.06489533954312,
41.681804925357));
#183643=CARTESIAN_POINT('Ctrl Pts',(3.22551463815378,-7.42999145087132,
41.8404723906437));
#183644=CARTESIAN_POINT('Ctrl Pts',(6.3763530758844,-4.98322677141116,41.9991398559298));
#183645=CARTESIAN_POINT('Ctrl Pts',(7.98922887192849,-1.33451851727022,
42.1578073212165));
#183646=CARTESIAN_POINT('Ctrl Pts',(7.64844784780906,2.66139411472179,42.3164747865027));
#183647=CARTESIAN_POINT('Ctrl Pts',(5.45491425699232,5.96712315687812,42.4751422517893));
#183648=CARTESIAN_POINT('Ctrl Pts',(0.745392301050544,8.53597231064671,
42.686698872171));
#183649=CARTESIAN_POINT('Ctrl Pts',(-4.86523790443101,7.04305554190294,
42.8982554925532));
#183650=CARTESIAN_POINT('Ctrl Pts',(-7.68137917069536,2.50876487011254,
43.1098121129349));
#183651=CARTESIAN_POINT('Ctrl Pts',(-8.0844676542436,-2.81363714450263,
43.3213687333169));
#183652=CARTESIAN_POINT('Ctrl Pts',(-4.43662091331696,-7.33040434346995,
43.5329253536988));
#183653=CARTESIAN_POINT('Ctrl Pts',(0.881268903615611,-8.03654238132135,
43.7444819740807));
#183654=CARTESIAN_POINT('Ctrl Pts',(4.60313310919397,-6.66280261436008,
43.9031494393671));
#183655=CARTESIAN_POINT('Ctrl Pts',(7.23678913863202,-3.63835136153705,
44.0618169046536));
#183656=CARTESIAN_POINT('Ctrl Pts',(8.08847108433317,0.25896542723205,44.2204843699399));
#183657=CARTESIAN_POINT('Ctrl Pts',(6.98923121663487,4.09382029945987,44.3791518352265));
#183658=CARTESIAN_POINT('Ctrl Pts',(4.16750194123697,6.94360862792613,44.5378193005128));
#183659=CARTESIAN_POINT('Ctrl Pts',(0.365385329643911,8.0764560037248,44.6964867657992));
#183660=CARTESIAN_POINT('Ctrl Pts',(-4.89644335222612,7.03159130944993,
44.9080433861812));
#183661=CARTESIAN_POINT('Ctrl Pts',(-8.24789214596878,2.29073026570201,
45.119600006563));
#183662=CARTESIAN_POINT('Ctrl Pts',(-7.50516776655695,-2.99498652073261,
45.331156626945));
#183663=CARTESIAN_POINT('Ctrl Pts',(-4.40474590883526,-7.33984924479369,
45.5427132473268));
#183664=CARTESIAN_POINT('Ctrl Pts',(1.28989149763967,-8.47080892925094,
45.7542698677089));
#183665=CARTESIAN_POINT('Ctrl Pts',(5.82544565561335,-5.60596488249478,
45.9658264880906));
#183666=CARTESIAN_POINT('Ctrl Pts',(7.80302595916402,-2.1666890188074,46.1244939533772));
#183667=CARTESIAN_POINT('Ctrl Pts',(7.88750222646596,1.84283512310428,46.2831614186634));
#183668=CARTESIAN_POINT('Ctrl Pts',(6.04452592653096,5.3809059710111,46.4418288839501));
#183669=CARTESIAN_POINT('Ctrl Pts',(2.7436350891584,7.62109440424651,46.6004963492363));
#183670=CARTESIAN_POINT('Ctrl Pts',(-1.24872578950165,8.00142147857247,
46.7591638145229));
#183671=CARTESIAN_POINT('Ctrl Pts',(-4.89380008924511,6.43527869080786,
46.9178312798092));
#183672=CARTESIAN_POINT('Ctrl Pts',(-8.2645486264883,2.26200189733122,47.1293879001912));
#183673=CARTESIAN_POINT('Ctrl Pts',(-7.80037642979242,-3.52547325528354,
47.3409445205731));
#183674=CARTESIAN_POINT('Ctrl Pts',(-3.84385887026274,-7.10780021600436,
47.5525011409549));
#183675=CARTESIAN_POINT('Ctrl Pts',(1.32064680707816,-8.4580098257796,47.7640577613369));
#183676=CARTESIAN_POINT('Ctrl Pts',(6.41695377006199,-5.67686569600247,
47.9756143817187));
#183677=CARTESIAN_POINT('Ctrl Pts',(8.06501639081381,-0.573047720393685,
48.1871710021008));
#183678=CARTESIAN_POINT('Ctrl Pts',(7.37821331433221,3.33750110294794,48.345838467387));
#183679=CARTESIAN_POINT('Ctrl Pts',(4.87780582617054,6.46451731396927,48.5045059326737));
#183680=CARTESIAN_POINT('Ctrl Pts',(1.18928799120203,8.01117052161392,48.6631733979599));
#183681=CARTESIAN_POINT('Ctrl Pts',(-2.7681121532524,7.5964713334689,48.8218408632464));
#183682=CARTESIAN_POINT('Ctrl Pts',(-7.20680219784448,4.6198565020302,49.0333974836283));
#183683=CARTESIAN_POINT('Ctrl Pts',(-8.84300034502869,-2.47886897833852,
49.2978432591057));
#183684=CARTESIAN_POINT('Ctrl Pts',(-2.6901361923085,-8.78327356646699,
49.6151781896785));
#183685=CARTESIAN_POINT('Ctrl Pts',(4.44903321313057,-7.31233051837037,
49.8796239651559));
#183686=CARTESIAN_POINT('Ctrl Pts',(7.52616743441877,-2.95099595536838,
50.0911805855378));
#183687=CARTESIAN_POINT('Ctrl Pts',(8.0420005338647,1.00473307760414,50.2498480508243));
#183688=CARTESIAN_POINT('Ctrl Pts',(6.56967689983475,4.71083444441478,50.4085155161107));
#183689=CARTESIAN_POINT('Ctrl Pts',(2.51247932687687,8.18312691894298,50.6200721364926));
#183690=CARTESIAN_POINT('Ctrl Pts',(-4.76488672051435,7.84957633027501,
50.8845179119699));
#183691=CARTESIAN_POINT('Ctrl Pts',(-9.18623881118053,0.231498139607691,
51.201852842543));
#183692=CARTESIAN_POINT('Ctrl Pts',(-5.84035172354906,-6.25684744528986,
51.4662986180201));
#183693=CARTESIAN_POINT('Ctrl Pts',(-0.82645652908081,-8.03540205221921,
51.6778552384022));
#183694=CARTESIAN_POINT('Ctrl Pts',(4.46831792482671,-7.30642728360933,
51.8894118587839));
#183695=CARTESIAN_POINT('Ctrl Pts',(8.10281394002393,-2.77908238451519,
52.100968479166));
#183696=CARTESIAN_POINT('Ctrl Pts',(7.66752709745631,2.56541977891761,52.3125250995478));
#183697=CARTESIAN_POINT('Ctrl Pts',(5.53416939644934,5.9121753980673,52.4711925648344));
#183698=CARTESIAN_POINT('Ctrl Pts',(2.02058714401458,7.84371592872507,52.6298600301206));
#183699=CARTESIAN_POINT('Ctrl Pts',(-1.9690910382543,7.84954043858405,52.7885274954072));
#183700=CARTESIAN_POINT('Ctrl Pts',(-5.48326334033245,5.96163601576004,
52.9471949606936));
#183701=CARTESIAN_POINT('Ctrl Pts',(-7.66969627022757,2.59966159008363,
53.10586242598));
#183702=CARTESIAN_POINT('Ctrl Pts',(-7.97012628075206,-1.35627990505007,
53.2645298912664));
#183703=CARTESIAN_POINT('Ctrl Pts',(-5.83283293269671,-6.27666477010184,
53.4760865116484));
#183704=CARTESIAN_POINT('Ctrl Pts',(-0.488881099089476,-8.5461249856449,
53.6876431320301));
#183705=CARTESIAN_POINT('Ctrl Pts',(4.51895866787966,-6.69898833214349,
53.8991997524122));
#183706=CARTESIAN_POINT('Ctrl Pts',(8.10721265766993,-2.74742124273045,
54.1107563727939));
#183707=CARTESIAN_POINT('Ctrl Pts',(8.00437035992183,3.05752741482916,54.322312993176));
#183708=CARTESIAN_POINT('Ctrl Pts',(4.24256256977924,6.8821006942729,54.5338696135578));
#183709=CARTESIAN_POINT('Ctrl Pts',(0.462044501231383,8.08506596133534,
54.6925370788443));
#183710=CARTESIAN_POINT('Ctrl Pts',(-3.47414384450845,7.31703759316164,
54.8512045441307));
#183711=CARTESIAN_POINT('Ctrl Pts',(-6.54071219188587,4.76544997203763,
55.0098720094171));
#183712=CARTESIAN_POINT('Ctrl Pts',(-8.02967446321915,1.06444578645232,
55.1685394747036));
#183713=CARTESIAN_POINT('Ctrl Pts',(-7.5543863021864,-2.91770816998886,
55.3272069399899));
#183714=CARTESIAN_POINT('Ctrl Pts',(-5.25066430696669,-6.14761519979205,
55.4858744052765));
#183715=CARTESIAN_POINT('Ctrl Pts',(-0.457223895574364,-8.55624796078953,
55.6974310256582));
#183716=CARTESIAN_POINT('Ctrl Pts',(5.09989189407407,-6.8750471997139,55.9089876460403));
#183717=CARTESIAN_POINT('Ctrl Pts',(7.76158322107178,-2.24840232248137,
56.1205442664221));
#183718=CARTESIAN_POINT('Ctrl Pts',(7.98502622041197,3.08456277470767,56.332100886804));
#183719=CARTESIAN_POINT('Ctrl Pts',(4.18699394779361,7.47579525227161,56.5436575071859));
#183720=CARTESIAN_POINT('Ctrl Pts',(-1.15167721691652,8.00226767255704,
56.7552141275679));
#183721=CARTESIAN_POINT('Ctrl Pts',(-4.8251178580258,6.50384584493907,56.9138815928542));
#183722=CARTESIAN_POINT('Ctrl Pts',(-7.35532384910833,3.39233381516429,
57.0725490581407));
#183723=CARTESIAN_POINT('Ctrl Pts',(-8.07514450849003,-0.531477912593235,
57.2312165234271));
#183724=CARTESIAN_POINT('Ctrl Pts',(-6.84725768774057,-4.32709831161835,
57.3898839887136));
#183725=CARTESIAN_POINT('Ctrl Pts',(-3.93106668757571,-7.08014744283938,
57.5485514539999));
#183726=CARTESIAN_POINT('Ctrl Pts',(-0.0929230143189289,-8.08418292927951,
57.7072189192864));
#183727=CARTESIAN_POINT('Ctrl Pts',(5.1306931182878,-6.86253751144311,57.9187755396683));
#183728=CARTESIAN_POINT('Ctrl Pts',(8.32042441111236,-2.01139475318977,
58.1303321600502));
#183729=CARTESIAN_POINT('Ctrl Pts',(7.39994227476214,3.24628117493691,58.3418887804322));
#183730=CARTESIAN_POINT('Ctrl Pts',(4.1548188338062,7.48416005256301,58.5534454008139));
#183731=CARTESIAN_POINT('Ctrl Pts',(-1.57470687607251,8.42251335556041,
58.765002021196));
#183732=CARTESIAN_POINT('Ctrl Pts',(-6.01110968439643,5.40640441353625,
58.9765586415778));
#183733=CARTESIAN_POINT('Ctrl Pts',(-7.87163043831221,1.90242144573692,
59.1352261068644));
#183734=CARTESIAN_POINT('Ctrl Pts',(-7.82089653845082,-2.10767525387386,
59.2938935721506));
#183735=CARTESIAN_POINT('Ctrl Pts',(-5.85970513720944,-5.58160221698454,
59.4525610374372));
#183736=CARTESIAN_POINT('Ctrl Pts',(-2.48516546539594,-7.70925873547831,
59.6112285027235));
#183737=CARTESIAN_POINT('Ctrl Pts',(1.51773057814824,-7.9547637932697,59.7698959680101));
#183738=CARTESIAN_POINT('Ctrl Pts',(5.10796914452118,-6.26668170080252,
59.9285634332964));
#183739=CARTESIAN_POINT('Ctrl Pts',(8.33605940863296,-1.98205613085918,
60.1401200536783));
#183740=CARTESIAN_POINT('Ctrl Pts',(7.67718401407479,3.78629328607396,60.3516766740603));
#183741=CARTESIAN_POINT('Ctrl Pts',(3.60197462640998,7.23348228222562,60.5632332944421));
#183742=CARTESIAN_POINT('Ctrl Pts',(-1.60477047921222,8.40832224306274,
60.7747899148241));
#183743=CARTESIAN_POINT('Ctrl Pts',(-6.60515776903126,5.45805128377708,
60.9863465352058));
#183744=CARTESIAN_POINT('Ctrl Pts',(-8.0791505515113,0.299957807979901,
61.1979031555879));
#183745=CARTESIAN_POINT('Ctrl Pts',(-7.26277749771403,-3.58243438645558,
61.3565706208743));
#183746=CARTESIAN_POINT('Ctrl Pts',(-4.65466311398428,-6.62893874886922,
61.5152380861607));
#183747=CARTESIAN_POINT('Ctrl Pts',(-0.923182212819831,-8.03978620397445,
61.6739055514471));
#183748=CARTESIAN_POINT('Ctrl Pts',(3.03096825163476,-7.51145452615722,
61.8325730167336));
#183749=CARTESIAN_POINT('Ctrl Pts',(6.26173611498402,-5.1354098123582,61.9912404820199));
#183750=CARTESIAN_POINT('Ctrl Pts',(7.93686296833665,-1.53910835953809,
62.1499079473065));
#183751=CARTESIAN_POINT('Ctrl Pts',(7.67039232375798,3.81883680847582,62.3614645676883));
#183752=CARTESIAN_POINT('Ctrl Pts',(3.46887358942421,7.82573237816946,62.5730211880701));
#183753=CARTESIAN_POINT('Ctrl Pts',(-1.86864952689433,7.86165606486387,
62.7845778084522));
#183754=CARTESIAN_POINT('Ctrl Pts',(-6.61914916211397,5.42789421450165,
62.996134428834));
#183755=CARTESIAN_POINT('Ctrl Pts',(-8.56835770814106,-0.0409774996166555,
63.207691049216));
#183756=CARTESIAN_POINT('Ctrl Pts',(-6.39545934772782,-4.94578083340884,
63.4192476695978));
#183757=CARTESIAN_POINT('Ctrl Pts',(-3.28129335186214,-7.40370765586983,
63.5779151348843));
#183758=CARTESIAN_POINT('Ctrl Pts',(0.673065974242905,-8.07190806657644,
63.7365826001707));
#183759=CARTESIAN_POINT('Ctrl Pts',(4.44204077020023,-6.76451782461722,
63.8952500654571));
#183760=CARTESIAN_POINT('Ctrl Pts',(7.13960489047256,-3.82554043879892,
64.0539175307436));
#183761=CARTESIAN_POINT('Ctrl Pts',(8.09796613107626,0.0686851840087504,
64.21258499603));
#183762=CARTESIAN_POINT('Ctrl Pts',(7.08009910440649,3.90318395573866,64.3712524613163));
#183763=CARTESIAN_POINT('Ctrl Pts',(3.44280908273089,7.84636849695452,64.5828090816984));
#183764=CARTESIAN_POINT('Ctrl Pts',(-2.35028493272838,8.23111972754161,
64.7943657020802));
#183765=CARTESIAN_POINT('Ctrl Pts',(-6.47152498377083,4.83909614711294,
65.0059223224622));
#183766=CARTESIAN_POINT('Ctrl Pts',(-8.55977967864248,-0.073096424218834,
65.2174789428439));
#183767=CARTESIAN_POINT('Ctrl Pts',(-6.55265142392936,-5.52097747564786,
65.429035563226));
#183768=CARTESIAN_POINT('Ctrl Pts',(-1.74189528540399,-7.89483686565093,
65.6405921836078));
#183769=CARTESIAN_POINT('Ctrl Pts',(2.22393186351381,-7.78690568717823,
65.7992596488943));
#183770=CARTESIAN_POINT('Ctrl Pts',(5.68824200564854,-5.76650852129091,
65.9579271141807));
#183771=CARTESIAN_POINT('Ctrl Pts',(7.74450397277799,-2.34799612847024,
66.1165945794671));
#183772=CARTESIAN_POINT('Ctrl Pts',(7.93280824578086,1.63684787827589,66.2752620447535));
#183773=CARTESIAN_POINT('Ctrl Pts',(6.17372664616111,5.24088469755259,66.4339295100401));
#183774=CARTESIAN_POINT('Ctrl Pts',(2.93553478351249,7.53294655864104,66.5925969753264));
#183775=CARTESIAN_POINT('Ctrl Pts',(-2.38351862620874,8.23026560498812,
66.8041535957083));
#183776=CARTESIAN_POINT('Ctrl Pts',(-7.0780367158128,4.81420476130172,67.0157102160903));
#183777=CARTESIAN_POINT('Ctrl Pts',(-8.06920482330742,-0.430604988459075,
67.2272668364721));
#183778=CARTESIAN_POINT('Ctrl Pts',(-6.52548736938242,-5.54014312325638,
67.4388234568541));
#183779=CARTESIAN_POINT('Ctrl Pts',(-1.49407666736653,-8.43718957249187,
67.6503800772358));
#183780=CARTESIAN_POINT('Ctrl Pts',(3.72055634062224,-7.17775095951435,
67.8619366976179));
#183781=CARTESIAN_POINT('Ctrl Pts',(6.69642517933677,-4.55408200761746,
68.0206041629042));
#183782=CARTESIAN_POINT('Ctrl Pts',(8.06195717757933,-0.783303330659765,
68.1792716281907));
#183783=CARTESIAN_POINT('Ctrl Pts',(7.45063563745237,3.15886944991555,68.3379390934771));
#183784=CARTESIAN_POINT('Ctrl Pts',(5.04223681335312,6.33912971621593,68.4966065587636));
#183785=CARTESIAN_POINT('Ctrl Pts',(1.38258078195735,7.97936360218798,68.6552740240499));
#183786=CARTESIAN_POINT('Ctrl Pts',(-2.57220997600818,7.66461898334663,
68.8139414893365));
#183787=CARTESIAN_POINT('Ctrl Pts',(-7.10300679619978,4.79225702808968,
69.0254981097182));
#183788=CARTESIAN_POINT('Ctrl Pts',(-8.51894575764623,-0.838292557771904,
69.2370547301004));
#183789=CARTESIAN_POINT('Ctrl Pts',(-5.91977111059251,-5.50034518323783,
69.4486113504821));
#183790=CARTESIAN_POINT('Ctrl Pts',(-1.4609408167016,-8.43450195116639,
69.6601679708642));
#183791=CARTESIAN_POINT('Ctrl Pts',(4.25830560195405,-7.4354062680194,69.8717245912458));
#183792=CARTESIAN_POINT('Ctrl Pts',(7.45528542258912,-3.1275177998348,70.0832812116279));
#183793=CARTESIAN_POINT('Ctrl Pts',(8.05928550274226,0.793530276579739,
70.2419486769142));
#183794=CARTESIAN_POINT('Ctrl Pts',(6.69192440169235,4.56364606898694,70.4006161422007));
#183795=CARTESIAN_POINT('Ctrl Pts',(3.69690001887922,7.19884420265474,70.5592836074872));
#183796=CARTESIAN_POINT('Ctrl Pts',(-0.189808693744583,8.09769660463547,
70.7179510727736));
#183797=CARTESIAN_POINT('Ctrl Pts',(-4.05059701706489,7.01244871067912,
70.87661853806));
#183798=CARTESIAN_POINT('Ctrl Pts',(-6.88549219908465,4.23705623008454,
71.0352860033464));
#183799=CARTESIAN_POINT('Ctrl Pts',(-8.52405681638749,-0.871141986781069,
71.2468426237284));
#183800=CARTESIAN_POINT('Ctrl Pts',(-6.00389410714868,-6.10151020520986,
71.4583992441102));
#183801=CARTESIAN_POINT('Ctrl Pts',(-1.02136088278692,-8.01587855968927,
71.6699558644921));
#183802=CARTESIAN_POINT('Ctrl Pts',(4.28202588432986,-7.41211343410654,
71.881512484874));
#183803=CARTESIAN_POINT('Ctrl Pts',(8.03324957591474,-2.98082777449497,
72.0930691052561));
#183804=CARTESIAN_POINT('Ctrl Pts',(7.72798799084106,2.37504735404791,72.3046257256377));
#183805=CARTESIAN_POINT('Ctrl Pts',(5.67963852957239,5.77264924345462,72.4632931909244));
#183806=CARTESIAN_POINT('Ctrl Pts',(2.21434866893366,7.79136558077833,72.6219606562107));
#183807=CARTESIAN_POINT('Ctrl Pts',(-1.77357280805547,7.89587658833466,
72.7806281214972));
#183808=CARTESIAN_POINT('Ctrl Pts',(-5.33371233999737,6.09591915260571,
72.9392955867835));
#183809=CARTESIAN_POINT('Ctrl Pts',(-7.60279059153105,2.78914831729824,
73.09796305207));
#183810=CARTESIAN_POINT('Ctrl Pts',(-8.00134398160658,-1.15807720319577,
73.2566305173565));
#183811=CARTESIAN_POINT('Ctrl Pts',(-5.98677271118669,-6.13000697183332,
73.4681871377381));
#183812=CARTESIAN_POINT('Ctrl Pts',(-0.700801569375949,-8.53135677336813,
73.6797437581205));
#183813=CARTESIAN_POINT('Ctrl Pts',(4.35134083834832,-6.80906161266702,
73.891300378502));
#183814=CARTESIAN_POINT('Ctrl Pts',(8.03653925277048,-2.94774627008737,
74.1028569988843));
#183815=CARTESIAN_POINT('Ctrl Pts',(8.07777661119743,2.85796395878713,74.3144136192658));
#183816=CARTESIAN_POINT('Ctrl Pts',(4.41202858232987,6.77470679138646,74.5259702396479));
#183817=CARTESIAN_POINT('Ctrl Pts',(0.662525911141174,8.07111098496528,
74.6846377049342));
#183818=CARTESIAN_POINT('Ctrl Pts',(-3.29150879522989,7.40099233156405,
74.8433051702208));
#183819=CARTESIAN_POINT('Ctrl Pts',(-6.42044791371609,4.92628421743445,
75.0019726355071));
#183820=CARTESIAN_POINT('Ctrl Pts',(-8.00078881050586,1.26336695010976,
75.1606401007937));
#183821=CARTESIAN_POINT('Ctrl Pts',(-7.62446036789397,-2.72935472465092,
75.3193075660799));
#183822=CARTESIAN_POINT('Ctrl Pts',(-5.40159489313535,-6.01543189895851,
75.4779750313666));
#183823=CARTESIAN_POINT('Ctrl Pts',(-0.669398417230296,-8.54226777437611,
75.6895316517482));
#183824=CARTESIAN_POINT('Ctrl Pts',(4.92772366164841,-6.99947931981837,
75.9010882721302));
#183825=CARTESIAN_POINT('Ctrl Pts',(7.70340129645059,-2.44030645666002,
76.1126448925122));
#183826=CARTESIAN_POINT('Ctrl Pts',(8.05910804839823,2.88547200616767,76.324201512894));
#183827=CARTESIAN_POINT('Ctrl Pts',(4.37120959512461,7.36959697986436,76.535758133276));
#183828=CARTESIAN_POINT('Ctrl Pts',(-0.952753784053995,8.02838144008641,
76.7473147536578));
#183829=CARTESIAN_POINT('Ctrl Pts',(-4.66224525292312,6.62157400594119,
76.9059822189443));
#183830=CARTESIAN_POINT('Ctrl Pts',(-7.26888142302682,3.57380476508172,
77.0646496842306));
#183831=CARTESIAN_POINT('Ctrl Pts',(-8.08584616808648,-0.330937078198273,
77.2233171495173));
#183832=CARTESIAN_POINT('Ctrl Pts',(-6.95252221598853,-4.15585761030523,
77.3819846148034));
#183833=CARTESIAN_POINT('Ctrl Pts',(-4.10554350669663,-6.98042159394269,
77.5406520800901));
#183834=CARTESIAN_POINT('Ctrl Pts',(-0.293495865475981,-8.07938787888673,
77.6993195453763));
#183835=CARTESIAN_POINT('Ctrl Pts',(4.95882582241272,-6.98773779080956,
77.9108761657584));
#183836=CARTESIAN_POINT('Ctrl Pts',(8.26795153021402,-2.21723898760715,
78.1224327861402));
#183837=CARTESIAN_POINT('Ctrl Pts',(7.47821715258361,3.06165892211683,78.3339894065222));
#183838=CARTESIAN_POINT('Ctrl Pts',(4.33925195229646,7.37875760061446,78.5455460269039));
#183839=CARTESIAN_POINT('Ctrl Pts',(-1.36522518019884,8.45899480892892,
78.757102647286));
#183840=CARTESIAN_POINT('Ctrl Pts',(-5.87510387930802,5.55389977654387,
78.9686592676679));
#183841=CARTESIAN_POINT('Ctrl Pts',(-7.82199981947996,2.09716283073475,
79.1273267329542));
#183842=CARTESIAN_POINT('Ctrl Pts',(-7.87078835298228,-1.9129580088188,
79.2859941982408));
#183843=CARTESIAN_POINT('Ctrl Pts',(-5.99640309405961,-5.43448042937297,
79.4446616635271));
#183844=CARTESIAN_POINT('Ctrl Pts',(-2.67569831151025,-7.64521786391511,
79.6033291288137));
#183845=CARTESIAN_POINT('Ctrl Pts',(1.31987319558362,-7.9899754606719,79.7619965940999));
#183846=CARTESIAN_POINT('Ctrl Pts',(4.95089445223432,-6.39150157970637,
79.9206640593866));
#183847=CARTESIAN_POINT('Ctrl Pts',(8.28430972403062,-2.18829736701093,
80.1322206797682));
#183848=CARTESIAN_POINT('Ctrl Pts',(7.76877342178239,3.59462525934789,80.3437773001502));
#183849=CARTESIAN_POINT('Ctrl Pts',(3.78035763949229,7.14187533173929,80.5553339205322));
#183850=CARTESIAN_POINT('Ctrl Pts',(-1.39563166549146,8.44555406639563,
80.766890540914));
#183851=CARTESIAN_POINT('Ctrl Pts',(-6.4676874778603,5.62027149334128,80.978447161296));
#183852=CARTESIAN_POINT('Ctrl Pts',(-8.06921967526007,0.500342035960366,
81.1900037816779));
#183853=CARTESIAN_POINT('Ctrl Pts',(-7.3494359394134,-3.40111224263743,
81.3486712469643));
#183854=CARTESIAN_POINT('Ctrl Pts',(-4.81772080277898,-6.51139646369471,
81.5073387122507));
#183855=CARTESIAN_POINT('Ctrl Pts',(-1.12239775020272,-8.01440271598737,
81.6660061775372));
#183856=CARTESIAN_POINT('Ctrl Pts',(2.84364522462193,-7.58435227804134,
81.8246736428235));
#183857=CARTESIAN_POINT('Ctrl Pts',(6.13237761632933,-5.28920768029616,
81.9833411081101));
#183858=CARTESIAN_POINT('Ctrl Pts',(7.8962275389091,-1.73558029901443,82.1420085733965));
#183859=CARTESIAN_POINT('Ctrl Pts',(7.76279135991085,3.62732729053053,82.3535651937783));
#183860=CARTESIAN_POINT('Ctrl Pts',(3.66199372055804,7.73724584233487,82.5651218141603));
#183861=CARTESIAN_POINT('Ctrl Pts',(-1.67299447212423,7.90560412826337,
82.7766784345421));
#183862=CARTESIAN_POINT('Ctrl Pts',(-6.48242288232662,5.59047089329887,
82.9882350549241));
#183863=CARTESIAN_POINT('Ctrl Pts',(-8.56673618884236,0.171650927506622,
83.199791675306));
#183864=CARTESIAN_POINT('Ctrl Pts',(-6.51621502212827,-4.78556058429354,
83.4113482956879));
#183865=CARTESIAN_POINT('Ctrl Pts',(-3.46399909193418,-7.32000569710434,
83.5700157609743));
#183866=CARTESIAN_POINT('Ctrl Pts',(0.47256185180701,-8.08612409855068,
83.7286832262607));
#183867=CARTESIAN_POINT('Ctrl Pts',(4.27281778882183,-6.87266001976035,
83.8873506915472));
#183868=CARTESIAN_POINT('Ctrl Pts',(7.04247926913745,-4.00152513233574,
84.0460181568335));
#183869=CARTESIAN_POINT('Ctrl Pts',(8.09717699341311,-0.132279446258024,
84.2046856221201));
#183870=CARTESIAN_POINT('Ctrl Pts',(7.17477289734989,3.72629604191705,84.3633530874064));
#183871=CARTESIAN_POINT('Ctrl Pts',(3.63644930560508,7.75852237335814,84.5749097077883));
#183872=CARTESIAN_POINT('Ctrl Pts',(-2.14531367813232,8.28690536066105,
84.7864663281702));
#183873=CARTESIAN_POINT('Ctrl Pts',(-6.34945463507768,4.99819097010746,
84.9980229485521));
#183874=CARTESIAN_POINT('Ctrl Pts',(-8.5589578018338,0.139329037041669,
85.209579568934));
#183875=CARTESIAN_POINT('Ctrl Pts',(-6.68763166481757,-5.35667953921688,
85.421136189316));
#183876=CARTESIAN_POINT('Ctrl Pts',(-1.93726194489959,-7.84918240821281,
85.6326928096978));
#183877=CARTESIAN_POINT('Ctrl Pts',(2.03002227243321,-7.83969276744859,
85.7913602749844));
#183878=CARTESIAN_POINT('Ctrl Pts',(5.54339996904871,-5.90588134185714,
85.9500277402706));
#183879=CARTESIAN_POINT('Ctrl Pts',(7.68385597786112,-2.53944578898081,
86.1086952055573));
#183880=CARTESIAN_POINT('Ctrl Pts',(7.97098245842279,1.43949862398741,86.2673626708435));
#183881=CARTESIAN_POINT('Ctrl Pts',(6.30187332299991,5.08607567142123,86.42603013613));
#183882=CARTESIAN_POINT('Ctrl Pts',(3.1215539312156,7.45778448167187,86.5846976014164));
#183883=CARTESIAN_POINT('Ctrl Pts',(-2.17855833266883,8.28687616423068,
86.7962542217983));
#183884=CARTESIAN_POINT('Ctrl Pts',(-6.95639726875433,4.98835727202873,
87.0078108421803));
#183885=CARTESIAN_POINT('Ctrl Pts',(-8.07740524430385,-0.230242602195722,
87.2193674625621));
#183886=CARTESIAN_POINT('Ctrl Pts',(-6.66095155220817,-5.37651333610082,
87.4309240829441));
#183887=CARTESIAN_POINT('Ctrl Pts',(-1.70297761113879,-8.39751750376825,
87.6424807033259));
#183888=CARTESIAN_POINT('Ctrl Pts',(3.54130152107833,-7.26786294981969,
87.8540373237079));
#183889=CARTESIAN_POINT('Ctrl Pts',(6.58135794038168,-4.71884527984714,
88.0127047889942));
#183890=CARTESIAN_POINT('Ctrl Pts',(8.04003782685793,-0.983112091085808,
88.1713722542807));
#183891=CARTESIAN_POINT('Ctrl Pts',(7.52672586548044,2.97301620405819,88.3300397195672));
#183892=CARTESIAN_POINT('Ctrl Pts',(5.19798382085618,6.21205938792148,88.4887071848536));
#183893=CARTESIAN_POINT('Ctrl Pts',(1.58015553245196,7.94259917204825,88.64737465014));
#183894=CARTESIAN_POINT('Ctrl Pts',(-2.3812275749546,7.726085914409,88.8060421154264));
#183895=CARTESIAN_POINT('Ctrl Pts',(-6.98190427298533,4.96703590615213,
89.0175987358083));
#183896=CARTESIAN_POINT('Ctrl Pts',(-8.5371240830427,-0.626644735768,89.2291553561904));
#183897=CARTESIAN_POINT('Ctrl Pts',(-6.05443425459705,-5.35175793485983,
89.440711976572));
#183898=CARTESIAN_POINT('Ctrl Pts',(-1.66978527272744,-8.3956529452519,
89.6522685969541));
#183899=CARTESIAN_POINT('Ctrl Pts',(4.0724917242945,-7.53878266868651,89.863825217336));
#183900=CARTESIAN_POINT('Ctrl Pts',(7.37538337916467,-3.31155074412213,
90.0753818377178));
#183901=CARTESIAN_POINT('Ctrl Pts',(8.07649463078164,0.593302278366084,
90.2340493030044));
#183902=CARTESIAN_POINT('Ctrl Pts',(6.80310647167449,4.39618698146572,90.3927167682906));
#183903=CARTESIAN_POINT('Ctrl Pts',(3.87439429122061,7.10489243267192,90.5513842335773));
#183904=CARTESIAN_POINT('Ctrl Pts',(0.0111865443886908,8.09991311695225,
90.7100516988636));
#183905=CARTESIAN_POINT('Ctrl Pts',(-3.87534239380638,7.11080125199156,
90.86871916415));
#183906=CARTESIAN_POINT('Ctrl Pts',(-6.7782334424462,4.40660864160255,91.0273866294365));
#183907=CARTESIAN_POINT('Ctrl Pts',(-8.54304869596879,-0.659357223743514,
91.2389432498183));
#183908=CARTESIAN_POINT('Ctrl Pts',(-6.15344869793795,-5.95065041452155,
91.4504998702001));
#183909=CARTESIAN_POINT('Ctrl Pts',(-1.21995294344862,-7.98806622108564,
91.6620564905823));
#183910=CARTESIAN_POINT('Ctrl Pts',(4.09678269278692,-7.51608560370173,
91.8736131109638));
#183911=CARTESIAN_POINT('Ctrl Pts',(7.95680954405873,-3.17924752878318,
92.0851697313462));
#183912=CARTESIAN_POINT('Ctrl Pts',(7.78454300291698,2.18255321977839,92.2967263517278));
#183913=CARTESIAN_POINT('Ctrl Pts',(5.82113258565889,5.6299368142819,92.4553938170143));
#183914=CARTESIAN_POINT('Ctrl Pts',(2.40700230900052,7.73401949366712,92.6140612823008));
#183915=CARTESIAN_POINT('Ctrl Pts',(-1.57709787894137,7.93745487426641,
92.772728747587));
#183916=CARTESIAN_POINT('Ctrl Pts',(-5.18080545044434,6.22639321954773,
92.9313962128737));
#183917=CARTESIAN_POINT('Ctrl Pts',(-7.53123945343747,2.97694565346133,
93.0900636781598));
#183918=CARTESIAN_POINT('Ctrl Pts',(-8.02761684064636,-0.959174718232218,
93.2487311434466));
#183919=CARTESIAN_POINT('Ctrl Pts',(-6.13703969987023,-5.97956326165626,
93.4602877638282));
#183920=CARTESIAN_POINT('Ctrl Pts',(-0.912283436855274,-8.51134008414109,
93.6718443842103));
#183921=CARTESIAN_POINT('Ctrl Pts',(4.18104046060788,-6.91493946600112,
93.8834010045922));
#183922=CARTESIAN_POINT('Ctrl Pts',(7.96091912382044,-3.14625782064091,
94.094957624974));
#183923=CARTESIAN_POINT('Ctrl Pts',(8.14620698463648,2.65664140730353,94.306514245356));
#183924=CARTESIAN_POINT('Ctrl Pts',(4.57877815237362,6.6631404217957,94.5180708657379));
#183925=CARTESIAN_POINT('Ctrl Pts',(0.86259885226857,8.05218568880823,94.6767383310243));
#183926=CARTESIAN_POINT('Ctrl Pts',(-3.1068462643541,7.48038937343908,94.8354057963108));
#183927=CARTESIAN_POINT('Ctrl Pts',(-6.29623036425301,5.08408437159998,
94.9940732615971));
#183928=CARTESIAN_POINT('Ctrl Pts',(-7.96697490175043,1.46151079550249,
95.1527407268836));
#183929=CARTESIAN_POINT('Ctrl Pts',(-7.68984104611083,-2.53932181665002,
95.31140819217));
#183930=CARTESIAN_POINT('Ctrl Pts',(-5.54919544733642,-5.87954163659009,
95.4700756574564));
#183931=CARTESIAN_POINT('Ctrl Pts',(-0.881168716971856,-8.52303255684783,
95.6816322778383));
#183932=CARTESIAN_POINT('Ctrl Pts',(4.75253610195871,-7.11959024768543,
95.8931888982204));
#183933=CARTESIAN_POINT('Ctrl Pts',(7.64045732748193,-2.63072034844158,
96.104745518602));
#183934=CARTESIAN_POINT('Ctrl Pts',(8.12827140123375,2.68463536695919,96.3163021389842));
#183935=CARTESIAN_POINT('Ctrl Pts',(4.55264398669978,7.25879796759945,96.5278587593658));
#183936=CARTESIAN_POINT('Ctrl Pts',(-0.753133361840499,8.0496279674861,
96.739415379748));
#183937=CARTESIAN_POINT('Ctrl Pts',(-4.49673398340393,6.73506221760718,
96.8980828450341));
#183938=CARTESIAN_POINT('Ctrl Pts',(-7.17751004723008,3.75339048709656,
97.0567503103208));
#183939=CARTESIAN_POINT('Ctrl Pts',(-8.0924294497543,-0.130793062789233,
97.2154177756071));
#183940=CARTESIAN_POINT('Ctrl Pts',(-7.05188031461038,-3.98092452596377,
97.3740852408936));
#183941=CARTESIAN_POINT('Ctrl Pts',(-4.28052068787601,-6.87850741011934,
97.5327527061801));
#183942=CARTESIAN_POINT('Ctrl Pts',(-0.488505341726331,-8.06587977813096,
97.6914201714664));
#183943=CARTESIAN_POINT('Ctrl Pts',(4.77208267160989,-7.11669744080927,
97.9029767918484));
#183944=CARTESIAN_POINT('Ctrl Pts',(9.09452740495533,-1.23259449210053,
98.1674225673258));
#183945=CARTESIAN_POINT('Ctrl Pts',(6.49394857205468,5.59032484645831,98.4318683428031));
#183946=CARTESIAN_POINT('Ctrl Pts',(1.67589148870856,7.90460136012811,98.6434249631851));
#183947=CARTESIAN_POINT('Ctrl Pts',(-2.29582483006711,7.77044586128011,
98.8020924284714));
#183948=CARTESIAN_POINT('Ctrl Pts',(-5.73741125166451,5.7125883020101,98.960759893758));
#183949=CARTESIAN_POINT('Ctrl Pts',(-7.76703063392476,2.28272931010332,
99.1194273590443));
#183950=CARTESIAN_POINT('Ctrl Pts',(-7.91518952336318,-1.71376454947224,
99.2781103900609));
#183951=CARTESIAN_POINT('Ctrl Pts',(-6.72572425074295,-4.09503579149403,
99.383904265982));
#183952=CARTESIAN_POINT('Ctrl Pts',(-5.88260427835266,-5.07275281619164,
99.4368089868075));
#183953=CARTESIAN_POINT('Ctrl Pts',(1.9103352902639,-7.13425027812016,-0.427061590008181));
#183954=CARTESIAN_POINT('Ctrl Pts',(3.0958658925461,-6.81680238470299,-0.374166617870574));
#183955=CARTESIAN_POINT('Ctrl Pts',(5.30450950520224,-5.58155414157205,
-0.26838249063749));
#183956=CARTESIAN_POINT('Ctrl Pts',(7.32611862039227,-2.36127264943766,
-0.10970920830893));
#183957=CARTESIAN_POINT('Ctrl Pts',(7.56588082625083,1.42044622507859,0.0489582569774992));
#183958=CARTESIAN_POINT('Ctrl Pts',(5.96180663696039,4.879206838332,0.207625722263927));
#183959=CARTESIAN_POINT('Ctrl Pts',(2.91184473574469,7.10958063960511,0.366293187550357));
#183960=CARTESIAN_POINT('Ctrl Pts',(-2.1132825876687,7.86831172497225,0.577849807932259));
#183961=CARTESIAN_POINT('Ctrl Pts',(-7.80768231834692,3.89690115303222,
0.842295583409641));
#183962=CARTESIAN_POINT('Ctrl Pts',(-7.55836006524443,-3.04053021023064,
1.10674135888703));
#183963=CARTESIAN_POINT('Ctrl Pts',(-3.93140712003248,-6.60107452752234,
1.31829797926893));
#183964=CARTESIAN_POINT('Ctrl Pts',(-0.315651225764061,-7.69659528282126,
1.47696544455536));
#183965=CARTESIAN_POINT('Ctrl Pts',(3.41286611415151,-6.90183796702513,
1.63563290984179));
#183966=CARTESIAN_POINT('Ctrl Pts',(6.29060828777561,-4.43237517133558,
1.79430037512822));
#183967=CARTESIAN_POINT('Ctrl Pts',(7.64958627743303,-0.889942290678628,
1.95296784041465));
#183968=CARTESIAN_POINT('Ctrl Pts',(7.13775755670161,2.88788372663806,2.11163530570107));
#183969=CARTESIAN_POINT('Ctrl Pts',(4.89863020487389,5.92400513809533,2.27030277098751));
#183970=CARTESIAN_POINT('Ctrl Pts',(0.305225732017479,8.14109071228054,
2.4818593913694));
#183971=CARTESIAN_POINT('Ctrl Pts',(-4.95243528681909,6.45885070470568,
2.69341601175132));
#183972=CARTESIAN_POINT('Ctrl Pts',(-7.41281351776048,2.02003584299111,
2.90497263213322));
#183973=CARTESIAN_POINT('Ctrl Pts',(-7.54454431414525,-3.05326164535232,
3.11652925251513));
#183974=CARTESIAN_POINT('Ctrl Pts',(-3.86736055188791,-7.17047382046754,
3.32808587289703));
#183975=CARTESIAN_POINT('Ctrl Pts',(1.21597883501667,-7.59017650439491,
3.53964249327894));
#183976=CARTESIAN_POINT('Ctrl Pts',(4.68557750845913,-6.1100685107214,3.69830995856536));
#183977=CARTESIAN_POINT('Ctrl Pts',(7.0439088100044,-3.11371703287544,3.85697742385179));
#183978=CARTESIAN_POINT('Ctrl Pts',(7.66884899663536,0.627470455451795,
4.01564488913822));
#183979=CARTESIAN_POINT('Ctrl Pts',(6.44407833797578,4.21731596174447,4.17431235442465));
#183980=CARTESIAN_POINT('Ctrl Pts',(3.63004607854268,6.79045680289362,4.33297981971107));
#183981=CARTESIAN_POINT('Ctrl Pts',(-0.0340013617160748,7.68689084058012,
4.49164728499751));
#183982=CARTESIAN_POINT('Ctrl Pts',(-4.98150970567032,6.4464434871977,4.70320390537941));
#183983=CARTESIAN_POINT('Ctrl Pts',(-7.94051430745141,1.78627946610955,
4.91476052576132));
#183984=CARTESIAN_POINT('Ctrl Pts',(-6.98586204731743,-3.19816663715534,
5.12631714614322));
#183985=CARTESIAN_POINT('Ctrl Pts',(-3.83664898111913,-7.17793047932758,
5.33787376652512));
#183986=CARTESIAN_POINT('Ctrl Pts',(1.62450660604406,-7.98329831713192,
5.54943038690703));
#183987=CARTESIAN_POINT('Ctrl Pts',(5.79646930875302,-5.0488007687728,5.76098700728893));
#183988=CARTESIAN_POINT('Ctrl Pts',(7.51220495144241,-1.68947230913394,
5.91965447257537));
#183989=CARTESIAN_POINT('Ctrl Pts',(7.40328658390602,2.12208533635141,6.07832193786179));
#183990=CARTESIAN_POINT('Ctrl Pts',(5.48624538749858,5.39500443507579,6.23698940314823));
#183991=CARTESIAN_POINT('Ctrl Pts',(2.24593360793106,7.36666007433078,6.39565686843465));
#183992=CARTESIAN_POINT('Ctrl Pts',(-1.56326161954992,7.53947962462525,
6.55432433372108));
#183993=CARTESIAN_POINT('Ctrl Pts',(-4.95088911328448,5.88031824608128,
6.7129917990075));
#183994=CARTESIAN_POINT('Ctrl Pts',(-7.95493420652126,1.7581511327172,6.92454841938941));
#183995=CARTESIAN_POINT('Ctrl Pts',(-7.2412584479266,-3.71574186194191,
7.13610503977132));
#183996=CARTESIAN_POINT('Ctrl Pts',(-3.31486374163761,-6.93124929171932,
7.34766166015322));
#183997=CARTESIAN_POINT('Ctrl Pts',(1.65287275986168,-7.96935211506437,
7.55921828053513));
#183998=CARTESIAN_POINT('Ctrl Pts',(6.36200152916944,-5.08891051000637,
7.77077490091703));
#183999=CARTESIAN_POINT('Ctrl Pts',(7.68523972297024,-0.162899008328246,
7.98233152129894));
#184000=CARTESIAN_POINT('Ctrl Pts',(6.85037485688638,3.515665544841,8.14099898658536));
#184001=CARTESIAN_POINT('Ctrl Pts',(4.32478421598083,6.3724516400251,8.2996664518718));
#184002=CARTESIAN_POINT('Ctrl Pts',(0.755982743686845,7.65724829166524,
8.45833391715822));
#184003=CARTESIAN_POINT('Ctrl Pts',(-2.99516013971152,7.09513313171334,
8.61700138244464));
#184004=CARTESIAN_POINT('Ctrl Pts',(-6.0306341810463,4.78737833030146,8.77566884773109));
#184005=CARTESIAN_POINT('Ctrl Pts',(-7.56872214277144,1.34309002377562,
8.93433631301751));
#184006=CARTESIAN_POINT('Ctrl Pts',(-7.23430921682634,-3.74657761047246,
9.14589293339943));
#184007=CARTESIAN_POINT('Ctrl Pts',(-3.17936424139809,-7.4922763239762,
9.3574495537813));
#184008=CARTESIAN_POINT('Ctrl Pts',(1.89546479066837,-7.44565320148777,
9.56900617416324));
#184009=CARTESIAN_POINT('Ctrl Pts',(6.37484650973986,-5.0600289990822,9.78056279454512));
#184010=CARTESIAN_POINT('Ctrl Pts',(8.14516047322325,0.168625328447077,
9.99211941492704));
#184011=CARTESIAN_POINT('Ctrl Pts',(6.00519926219761,4.79864850846001,10.203676035309));
#184012=CARTESIAN_POINT('Ctrl Pts',(3.00742183609204,7.08822642152758,10.3623435005954));
#184013=CARTESIAN_POINT('Ctrl Pts',(-0.762027260887039,7.66362922334555,
10.5210109658818));
#184014=CARTESIAN_POINT('Ctrl Pts',(-4.32533719076805,6.36367971343036,
10.6796784311683));
#184015=CARTESIAN_POINT('Ctrl Pts',(-6.84538509720808,3.52882434957768,
10.8383458964547));
#184016=CARTESIAN_POINT('Ctrl Pts',(-7.69754851107875,-0.187847870986907,
10.9970133617411));
#184017=CARTESIAN_POINT('Ctrl Pts',(-6.67185181111312,-3.81783172717063,
11.1556808270275));
#184018=CARTESIAN_POINT('Ctrl Pts',(-3.154272897111,-7.51150025803788,11.3672374474094));
#184019=CARTESIAN_POINT('Ctrl Pts',(2.35893800003516,-7.78960672988603,
11.5787940677913));
#184020=CARTESIAN_POINT('Ctrl Pts',(6.22559236632147,-4.5025035322461,11.7903506881733));
#184021=CARTESIAN_POINT('Ctrl Pts',(8.13651942784416,0.199030386146407,
12.0019073085552));
#184022=CARTESIAN_POINT('Ctrl Pts',(6.14593418071584,5.34785626978331,12.213463928937));
#184023=CARTESIAN_POINT('Ctrl Pts',(1.53651183656423,7.53183756214526,12.425020549319));
#184024=CARTESIAN_POINT('Ctrl Pts',(-2.23209396456929,7.36921274196765,
12.5836880146054));
#184025=CARTESIAN_POINT('Ctrl Pts',(-5.49497454184229,5.39603124562451,
12.7423554798918));
#184026=CARTESIAN_POINT('Ctrl Pts',(-7.39809123050544,2.11499585202551,
12.9010229451783));
#184027=CARTESIAN_POINT('Ctrl Pts',(-7.51680423309027,-1.67617199017493,
13.0596904104647));
#184028=CARTESIAN_POINT('Ctrl Pts',(-5.78993610934901,-5.07584276280316,
13.2183578757511));
#184029=CARTESIAN_POINT('Ctrl Pts',(-2.67675967353113,-7.2058589589723,
13.3770253410375));
#184030=CARTESIAN_POINT('Ctrl Pts',(2.39051973739319,-7.78829179095684,
13.5885819614195));
#184031=CARTESIAN_POINT('Ctrl Pts',(6.80181525940307,-4.46966113606466,
13.8001385818013));
#184032=CARTESIAN_POINT('Ctrl Pts',(7.66472856953409,0.531483136944698,
14.0116952021832));
#184033=CARTESIAN_POINT('Ctrl Pts',(6.11981976973525,5.36566561390598,14.2232518225652));
#184034=CARTESIAN_POINT('Ctrl Pts',(1.29270755433579,8.04369198906295,14.4348084429471));
#184035=CARTESIAN_POINT('Ctrl Pts',(-3.64568881026725,6.76745142466027,
14.646365063329));
#184036=CARTESIAN_POINT('Ctrl Pts',(-6.43508761370743,4.22814229975222,
14.8050325286154));
#184037=CARTESIAN_POINT('Ctrl Pts',(-7.67620898046891,0.62266693136815,
14.9636999939018));
#184038=CARTESIAN_POINT('Ctrl Pts',(-7.03537814335224,-3.11583306500975,
15.1223674591882));
#184039=CARTESIAN_POINT('Ctrl Pts',(-4.6976292363168,-6.10280083054923,
15.2810349244747));
#184040=CARTESIAN_POINT('Ctrl Pts',(-1.19363894411629,-7.60675791478432,
15.4397023897611));
#184041=CARTESIAN_POINT('Ctrl Pts',(2.56134496261047,-7.24768636662445,
15.5983698550475));
#184042=CARTESIAN_POINT('Ctrl Pts',(6.82522171227787,-4.4484179450905,15.8099264754294));
#184043=CARTESIAN_POINT('Ctrl Pts',(8.08611931403569,0.925870365372249,
16.0214830958114));
#184044=CARTESIAN_POINT('Ctrl Pts',(5.54457870601156,5.31866386814692,16.2330397161932));
#184045=CARTESIAN_POINT('Ctrl Pts',(1.26124658150169,8.04063545716044,16.4445963365752));
#184046=CARTESIAN_POINT('Ctrl Pts',(-4.16081638782906,7.00426160438954,
16.656152956957));
#184047=CARTESIAN_POINT('Ctrl Pts',(-7.13493330498989,2.86044968838645,
16.867709577339));
#184048=CARTESIAN_POINT('Ctrl Pts',(-7.6498061433939,-0.876359441974459,
17.0263770426254));
#184049=CARTESIAN_POINT('Ctrl Pts',(-6.29282616987816,-4.43984653056245,
17.1850445079118));
#184050=CARTESIAN_POINT('Ctrl Pts',(-3.40563176562958,-6.89975605263704,
17.3437119731982));
#184051=CARTESIAN_POINT('Ctrl Pts',(0.302993692477398,-7.69545926125072,
17.5023794384847));
#184052=CARTESIAN_POINT('Ctrl Pts',(3.95695083878236,-6.60530695444992,
17.6610469037711));
#184053=CARTESIAN_POINT('Ctrl Pts',(6.6100324713461,-3.92389046918924,17.8197143690576));
#184054=CARTESIAN_POINT('Ctrl Pts',(8.0904811788591,0.957177063285023,18.0312709894394));
#184055=CARTESIAN_POINT('Ctrl Pts',(5.61545519891417,5.89145350514484,18.2428276098214));
#184056=CARTESIAN_POINT('Ctrl Pts',(0.84968121050301,7.63600551401102,18.4543842302032));
#184057=CARTESIAN_POINT('Ctrl Pts',(-4.18301432463752,6.98175856458619,
18.6659408505852));
#184058=CARTESIAN_POINT('Ctrl Pts',(-7.68217330527907,2.71224758154732,
18.877497470967));
#184059=CARTESIAN_POINT('Ctrl Pts',(-7.31091387012258,-2.37486506355482,
19.089054091349));
#184060=CARTESIAN_POINT('Ctrl Pts',(-5.31216816464087,-5.57390431328177,
19.2477215566354));
#184061=CARTESIAN_POINT('Ctrl Pts',(-1.98723048460563,-7.44061915570909,
19.4063890219218));
#184062=CARTESIAN_POINT('Ctrl Pts',(1.80559497136075,-7.4796248641468,19.5650564872083));
#184063=CARTESIAN_POINT('Ctrl Pts',(5.16291480539385,-5.71456114951061,
19.7237239524947));
#184064=CARTESIAN_POINT('Ctrl Pts',(7.27004306916297,-2.53653576272058,
19.8823914177811));
#184065=CARTESIAN_POINT('Ctrl Pts',(7.58920535050375,1.22205066766044,20.0410588830675));
#184066=CARTESIAN_POINT('Ctrl Pts',(5.59874694737816,5.91828575308559,20.2526155034494));
#184067=CARTESIAN_POINT('Ctrl Pts',(0.537130386280701,8.1212100356061,20.4641721238314));
#184068=CARTESIAN_POINT('Ctrl Pts',(-4.23978452917413,6.40739927862032,
20.6757287442132));
#184069=CARTESIAN_POINT('Ctrl Pts',(-7.68480010363191,2.68074781759015,
20.8872853645952));
#184070=CARTESIAN_POINT('Ctrl Pts',(-7.63614330750188,-2.83925853406245,
21.0988419849771));
#184071=CARTESIAN_POINT('Ctrl Pts',(-4.09191004187968,-6.50735874957023,
21.310398605359));
#184072=CARTESIAN_POINT('Ctrl Pts',(-0.507707523998028,-7.68308355890531,
21.4690660706454));
#184073=CARTESIAN_POINT('Ctrl Pts',(3.24117958490524,-6.98617587222398,
21.6277335359318));
#184074=CARTESIAN_POINT('Ctrl Pts',(6.17835378800283,-4.58616460446389,
21.7864010012183));
#184075=CARTESIAN_POINT('Ctrl Pts',(7.62532235160403,-1.07998030231049,
21.9450684665047));
#184076=CARTESIAN_POINT('Ctrl Pts',(7.20713016565148,2.71013185627586,22.1037359317911));
#184077=CARTESIAN_POINT('Ctrl Pts',(5.04416303840098,5.80050557524718,22.2624033970775));
#184078=CARTESIAN_POINT('Ctrl Pts',(0.50711086416215,8.13110768637341,22.4739600174594));
#184079=CARTESIAN_POINT('Ctrl Pts',(-4.79062278934888,6.57970324440751,
22.6855166378414));
#184080=CARTESIAN_POINT('Ctrl Pts',(-7.36041264286785,2.20337561396134,
22.8970732582232));
#184081=CARTESIAN_POINT('Ctrl Pts',(-7.61797915554366,-2.86512741077909,
23.1086298786052));
#184082=CARTESIAN_POINT('Ctrl Pts',(-4.04410144101776,-7.07229221474271,
23.320186498987));
#184083=CARTESIAN_POINT('Ctrl Pts',(1.0272626268211,-7.61801661733424,23.531743119369));
#184084=CARTESIAN_POINT('Ctrl Pts',(4.53251832342916,-6.22445319291774,
23.6904105846554));
#184085=CARTESIAN_POINT('Ctrl Pts',(6.96447629890928,-3.28754745991319,
23.8490780499418));
#184086=CARTESIAN_POINT('Ctrl Pts',(7.68205750980338,0.436982522579811,
24.0077455152283));
#184087=CARTESIAN_POINT('Ctrl Pts',(6.54674297907218,4.05611326089645,24.1664129805147));
#184088=CARTESIAN_POINT('Ctrl Pts',(3.79742712508109,6.69828986628251,24.3250804458011));
#184089=CARTESIAN_POINT('Ctrl Pts',(0.156752166466377,7.68536755430423,
24.4837479110876));
#184090=CARTESIAN_POINT('Ctrl Pts',(-4.8200133536601,6.56807010517477,24.6953045314694));
#184091=CARTESIAN_POINT('Ctrl Pts',(-7.89374442187484,1.98276587029716,
24.9068611518514));
#184092=CARTESIAN_POINT('Ctrl Pts',(-7.06307051436508,-3.02383420157176,
25.1184177722332));
#184093=CARTESIAN_POINT('Ctrl Pts',(-4.01358126405507,-7.08051741973153,
25.3299743926152));
#184094=CARTESIAN_POINT('Ctrl Pts',(1.42590828576246,-8.02115074017103,
25.541531012997));
#184095=CARTESIAN_POINT('Ctrl Pts',(5.66940319694829,-5.19108014548771,
25.753087633379));
#184096=CARTESIAN_POINT('Ctrl Pts',(7.46796913943167,-1.87536045483022,
25.9117550986654));
#184097=CARTESIAN_POINT('Ctrl Pts',(7.45366456041774,1.93772625518244,26.0704225639519));
#184098=CARTESIAN_POINT('Ctrl Pts',(5.61842808856437,5.25720715994694,26.2290900292382));
#184099=CARTESIAN_POINT('Ctrl Pts',(2.42803885110833,7.30866100984028,26.3877574945247));
#184100=CARTESIAN_POINT('Ctrl Pts',(-1.37569510680508,7.57594897528736,
26.5464249598111));
#184101=CARTESIAN_POINT('Ctrl Pts',(-4.80345003747338,6.00135929802082,
26.7050924250976));
#184102=CARTESIAN_POINT('Ctrl Pts',(-7.90885787044363,1.95500404630625,
26.9166490454794));
#184103=CARTESIAN_POINT('Ctrl Pts',(-7.33123141642751,-3.53491264574978,
27.1282056658614));
#184104=CARTESIAN_POINT('Ctrl Pts',(-3.4858355309382,-6.84685979268871,
27.3397622862433));
#184105=CARTESIAN_POINT('Ctrl Pts',(1.45461176920048,-8.00791271775603,
27.5513189066251));
#184106=CARTESIAN_POINT('Ctrl Pts',(6.23376599399237,-5.24521068862792,
27.7628755270071));
#184107=CARTESIAN_POINT('Ctrl Pts',(7.67883112467215,-0.353550908937111,
27.974432147389));
#184108=CARTESIAN_POINT('Ctrl Pts',(6.93550347755123,3.34459734735289,28.1330996126754));
#184109=CARTESIAN_POINT('Ctrl Pts',(4.48157899137418,6.26317396878968,28.2917670779619));
#184110=CARTESIAN_POINT('Ctrl Pts',(0.94575744281704,7.63613149234103,28.4504345432483));
#184111=CARTESIAN_POINT('Ctrl Pts',(-2.8181787659297,7.16727053085858,28.6091020085347));
#184112=CARTESIAN_POINT('Ctrl Pts',(-5.90998291927167,4.93554878376881,
28.7677694738211));
#184113=CARTESIAN_POINT('Ctrl Pts',(-7.53306408221923,1.53048724908849,
28.9264369391076));
#184114=CARTESIAN_POINT('Ctrl Pts',(-7.32504948547284,-3.56591133811914,
29.1379935594895));
#184115=CARTESIAN_POINT('Ctrl Pts',(-3.36429911605302,-7.41107636932855,
29.3495501798714));
#184116=CARTESIAN_POINT('Ctrl Pts',(1.71012420231409,-7.49039475476082,
29.5611068002533));
#184117=CARTESIAN_POINT('Ctrl Pts',(6.24732368715564,-5.21665680701726,
29.7726634206352));
#184118=CARTESIAN_POINT('Ctrl Pts',(8.14683672517312,-0.0335411586358248,
29.984220041017));
#184119=CARTESIAN_POINT('Ctrl Pts',(6.1224241525805,4.64815750403779,30.195776661399));
#184120=CARTESIAN_POINT('Ctrl Pts',(3.18238353293971,7.01141747097681,30.3544441266854));
#184121=CARTESIAN_POINT('Ctrl Pts',(-0.571626804727882,7.68017846246866,
30.5131115919718));
#184122=CARTESIAN_POINT('Ctrl Pts',(-4.16609656841948,6.46904944265926,
30.6717790572583));
#184123=CARTESIAN_POINT('Ctrl Pts',(-6.7557128041372,3.69759961694983,30.8304465225447));
#184124=CARTESIAN_POINT('Ctrl Pts',(-7.69983957956182,0.00321746143552028,
30.9891139878311));
#184125=CARTESIAN_POINT('Ctrl Pts',(-6.76453337409805,-3.65110037073176,
31.1477814531175));
#184126=CARTESIAN_POINT('Ctrl Pts',(-3.33969252180603,-7.43091700234533,
31.3593380734995));
#184127=CARTESIAN_POINT('Ctrl Pts',(2.16491981449567,-7.84574302989205,
31.5708946938813));
#184128=CARTESIAN_POINT('Ctrl Pts',(6.11194997629257,-4.65559940896827,
31.7824513142633));
#184129=CARTESIAN_POINT('Ctrl Pts',(8.1389528136781,-0.00293104366579359,
31.9940079346452));
#184130=CARTESIAN_POINT('Ctrl Pts',(6.27674381516078,5.19370394947507,32.2055645550271));
#184131=CARTESIAN_POINT('Ctrl Pts',(1.72293424764504,7.49139127697494,32.417121175409));
#184132=CARTESIAN_POINT('Ctrl Pts',(-2.04854652132436,7.42233097167019,
32.5757886406954));
#184133=CARTESIAN_POINT('Ctrl Pts',(-5.3593850637147,5.53072239025633,32.7344561059818));
#184134=CARTESIAN_POINT('Ctrl Pts',(-7.34333158641618,2.29792134785086,
32.8931235712683));
#184135=CARTESIAN_POINT('Ctrl Pts',(-7.55608233136559,-1.48913337914222,
33.0517910365546));
#184136=CARTESIAN_POINT('Ctrl Pts',(-5.91410559981757,-4.93060796020649,
33.2104585018412));
#184137=CARTESIAN_POINT('Ctrl Pts',(-2.85474212844216,-7.13721886077074,
33.3691259671275));
#184138=CARTESIAN_POINT('Ctrl Pts',(2.19652445630305,-7.84521216722752,
33.5806825875095));
#184139=CARTESIAN_POINT('Ctrl Pts',(6.6888103943495,-4.63706555946082,33.7922392078914));
#184140=CARTESIAN_POINT('Ctrl Pts',(7.67555673261799,0.341126389848561,
34.0037958282733));
#184141=CARTESIAN_POINT('Ctrl Pts',(6.25107936750864,5.21215581457453,34.2153524486552));
#184142=CARTESIAN_POINT('Ctrl Pts',(1.49190622722631,8.00913787152622,34.4269090690371));
#184143=CARTESIAN_POINT('Ctrl Pts',(-3.47663824415704,6.85583198493872,
34.638465689419));
#184144=CARTESIAN_POINT('Ctrl Pts',(-6.32818873489555,4.38652108607564,
34.7971331547054));
#184145=CARTESIAN_POINT('Ctrl Pts',(-7.65839445044915,0.812953172440143,
34.9558006199919));
#184146=CARTESIAN_POINT('Ctrl Pts',(-7.11052832819302,-2.94029729839196,
35.1144680852783));
#184147=CARTESIAN_POINT('Ctrl Pts',(-4.84761807313768,-5.98435438758767,
35.2731355505647));
#184148=CARTESIAN_POINT('Ctrl Pts',(-1.38202601009292,-7.57479663162461,
35.4318030158511));
#184149=CARTESIAN_POINT('Ctrl Pts',(2.38071170131004,-7.30901207289255,
35.5904704811375));
#184150=CARTESIAN_POINT('Ctrl Pts',(6.71273676997582,-4.61640971892303,
35.8020271015195));
#184151=CARTESIAN_POINT('Ctrl Pts',(8.10660407544666,0.724935761462476,
36.0135837219014));
#184152=CARTESIAN_POINT('Ctrl Pts',(5.67484912542736,5.179442612205,36.2251403422833));
#184153=CARTESIAN_POINT('Ctrl Pts',(1.46037909675127,8.00686295549433,36.4366969626652));
#184154=CARTESIAN_POINT('Ctrl Pts',(-3.9857309816301,7.10535165759066,36.648253583047));
#184155=CARTESIAN_POINT('Ctrl Pts',(-7.06175694946863,3.03661562814189,
36.859810203429));
#184156=CARTESIAN_POINT('Ctrl Pts',(-7.66919668536809,-0.686266787906841,
37.0184776687154));
#184157=CARTESIAN_POINT('Ctrl Pts',(-6.40105915860065,-4.28232881354824,
37.1771451340019));
#184158=CARTESIAN_POINT('Ctrl Pts',(-3.57579413059405,-6.81312392699381,
37.3358125992882));
#184159=CARTESIAN_POINT('Ctrl Pts',(0.111944747556397,-7.70060820927449,
37.4944800645747));
#184160=CARTESIAN_POINT('Ctrl Pts',(3.79182789387702,-6.7014611187607,37.6531475298611));
#184161=CARTESIAN_POINT('Ctrl Pts',(6.51062944971077,-4.08670403320362,
37.8118149951476));
#184162=CARTESIAN_POINT('Ctrl Pts',(8.11174144370636,0.756124583920268,
38.0233716155295));
#184163=CARTESIAN_POINT('Ctrl Pts',(5.759917035209,5.75029714378351,38.2349282359114));
#184164=CARTESIAN_POINT('Ctrl Pts',(1.03889993861408,7.61257021557348,38.4464848562933));
#184165=CARTESIAN_POINT('Ctrl Pts',(-4.00848047528635,7.08340636795202,
38.6580414766752));
#184166=CARTESIAN_POINT('Ctrl Pts',(-7.61250594272741,2.90203840565421,
38.8695980970571));
#184167=CARTESIAN_POINT('Ctrl Pts',(-7.36759278273956,-2.19272029090994,
39.081154717439));
#184168=CARTESIAN_POINT('Ctrl Pts',(-5.44884370079305,-5.44037151556518,
39.2398221827254));
#184169=CARTESIAN_POINT('Ctrl Pts',(-2.17125061230263,-7.38901679506997,
39.3984896480118));
#184170=CARTESIAN_POINT('Ctrl Pts',(1.61943908025456,-7.5221259211948,39.5571571132983));
#184171=CARTESIAN_POINT('Ctrl Pts',(5.01952355125543,-5.84091446073667,
39.7158245785847));
#184172=CARTESIAN_POINT('Ctrl Pts',(7.20486273325817,-2.71615406373658,
39.8744920438711));
#184173=CARTESIAN_POINT('Ctrl Pts',(7.61719255798237,1.03335532178548,40.0331595091576));
#184174=CARTESIAN_POINT('Ctrl Pts',(5.74387974563822,5.77753572932256,40.2447161295394));
#184175=CARTESIAN_POINT('Ctrl Pts',(0.738485251829574,8.10538099210179,
40.4562727499214));
#184176=CARTESIAN_POINT('Ctrl Pts',(-4.07948538963533,6.51063263632969,
40.6678293703032));
#184177=CARTESIAN_POINT('Ctrl Pts',(-7.61591356952583,2.870613522543,40.8793859906852));
#184178=CARTESIAN_POINT('Ctrl Pts',(-7.70424556772878,-2.64890050173359,
41.0909426110671));
#184179=CARTESIAN_POINT('Ctrl Pts',(-4.25212411721605,-6.40381809378092,
41.302499231449));
#184180=CARTESIAN_POINT('Ctrl Pts',(-0.698199749211469,-7.66811952262341,
41.4611666967354));
#184181=CARTESIAN_POINT('Ctrl Pts',(3.06682613053423,-7.06445156430003,
41.6198341620219));
#184182=CARTESIAN_POINT('Ctrl Pts',(6.06264997198326,-4.7380625392818,41.7785016273082));
#184183=CARTESIAN_POINT('Ctrl Pts',(7.59617568540101,-1.2688630248439,41.9371690925948));
#184184=CARTESIAN_POINT('Ctrl Pts',(7.27216036790802,2.5304591453817,42.0958365578811));
#184185=CARTESIAN_POINT('Ctrl Pts',(5.18654399681884,5.67355330066163,42.2545040231676));
#184186=CARTESIAN_POINT('Ctrl Pts',(0.708720574174565,8.1160205017057,42.4660606435494));
#184187=CARTESIAN_POINT('Ctrl Pts',(-4.62587847535394,6.69655208480938,
42.6776172639315));
#184188=CARTESIAN_POINT('Ctrl Pts',(-7.30347153926227,2.38533893724051,
42.8891738843132));
#184189=CARTESIAN_POINT('Ctrl Pts',(-7.68672892077909,-2.67521213964834,
43.1007305046952));
#184190=CARTESIAN_POINT('Ctrl Pts',(-4.21834853492501,-6.96976393224585,
43.3122871250771));
#184191=CARTESIAN_POINT('Ctrl Pts',(0.837912334877082,-7.64116147006215,
43.523843745459));
#184192=CARTESIAN_POINT('Ctrl Pts',(4.37666868245361,-6.33500679817317,
43.6825112107454));
#184193=CARTESIAN_POINT('Ctrl Pts',(6.88075439776222,-3.45935215907542,
43.8411786760319));
#184194=CARTESIAN_POINT('Ctrl Pts',(7.69053539056388,0.246224875170558,
43.9998461413183));
#184195=CARTESIAN_POINT('Ctrl Pts',(6.64537580266269,3.89241298724387,44.1585136066047));
#184196=CARTESIAN_POINT('Ctrl Pts',(3.96246964786781,6.60199774895939,44.3171810718911));
#184197=CARTESIAN_POINT('Ctrl Pts',(0.347409143152186,7.67911142654452,
44.4758485371776));
#184198=CARTESIAN_POINT('Ctrl Pts',(-4.65554868102627,6.68565186837957,
44.6874051575595));
#184199=CARTESIAN_POINT('Ctrl Pts',(-7.84211327267865,2.17803117485824,
44.8989617779414));
#184200=CARTESIAN_POINT('Ctrl Pts',(-7.13592936403309,-2.84763950959403,
45.1105183983233));
#184201=CARTESIAN_POINT('Ctrl Pts',(-4.18804171334091,-6.97874416437295,
45.3220750187052));
#184202=CARTESIAN_POINT('Ctrl Pts',(1.22643156032289,-8.0540630210437,45.5336316390871));
#184203=CARTESIAN_POINT('Ctrl Pts',(5.53884603322342,-5.33016325057911,
45.745188259469));
#184204=CARTESIAN_POINT('Ctrl Pts',(7.41913356266724,-2.06009249532456,
45.9038557247554));
#184205=CARTESIAN_POINT('Ctrl Pts',(7.49945377603941,1.7521715272814,46.0625231900418));
#184206=CARTESIAN_POINT('Ctrl Pts',(5.74714801752916,5.11617676219574,46.2211906553283));
#184207=CARTESIAN_POINT('Ctrl Pts',(2.6086540375764,7.2461526559958,46.3798581206147));
#184208=CARTESIAN_POINT('Ctrl Pts',(-1.18729111807959,7.60776844155002,
46.5385255859012));
#184209=CARTESIAN_POINT('Ctrl Pts',(-4.6530354610011,6.11867657110869,46.6971930511876));
#184210=CARTESIAN_POINT('Ctrl Pts',(-7.85795028953664,2.1507161815344,46.9087496715695));
#184211=CARTESIAN_POINT('Ctrl Pts',(-7.41661438454468,-3.35202741724084,
47.1203062919514));
#184212=CARTESIAN_POINT('Ctrl Pts',(-3.65474913242218,-6.75811145769161,
47.3318629123333));
#184213=CARTESIAN_POINT('Ctrl Pts',(1.25567377349499,-8.04189360643028,
47.5434195327152));
#184214=CARTESIAN_POINT('Ctrl Pts',(6.10125319775964,-5.39757589381113,
47.754976153097));
#184215=CARTESIAN_POINT('Ctrl Pts',(7.66823461842726,-0.544854982878747,
47.9665327734791));
#184216=CARTESIAN_POINT('Ctrl Pts',(7.01522080271856,3.17330309778602,48.1252002387653));
#184217=CARTESIAN_POINT('Ctrl Pts',(4.63782808188847,6.14647671576517,48.283867704052));
#184218=CARTESIAN_POINT('Ctrl Pts',(1.13077753391832,7.61703785226467,48.4425351693382));
#184219=CARTESIAN_POINT('Ctrl Pts',(-2.63192688181473,7.22274098829433,
48.6012026346247));
#184220=CARTESIAN_POINT('Ctrl Pts',(-6.85224275112629,4.39256931968361,
48.8127592550066));
#184221=CARTESIAN_POINT('Ctrl Pts',(-8.40794340526699,-2.35691386019897,
49.077205030484));
#184222=CARTESIAN_POINT('Ctrl Pts',(-2.55778717345702,-8.35115505806219,
49.3945399610569));
#184223=CARTESIAN_POINT('Ctrl Pts',(4.23015017580366,-6.95257930116764,
49.6589857365342));
#184224=CARTESIAN_POINT('Ctrl Pts',(7.1558958925893,-2.80581318713367,49.8705423569161));
#184225=CARTESIAN_POINT('Ctrl Pts',(7.64635109302848,0.955302332272822,
50.0292098222026));
#184226=CARTESIAN_POINT('Ctrl Pts',(6.24646267211259,4.47907133945649,50.1878772874891));
#184227=CARTESIAN_POINT('Ctrl Pts',(2.3888706505773,7.78053435803256,50.3994339078708));
#184228=CARTESIAN_POINT('Ctrl Pts',(-4.53046435773524,7.46339375383813,
50.6638796833484));
#184229=CARTESIAN_POINT('Ctrl Pts',(-8.73429526383473,0.220108920083938,
50.9812146139211));
#184230=CARTESIAN_POINT('Ctrl Pts',(-5.55301875409966,-5.94902376600732,
51.2456603893986));
#184231=CARTESIAN_POINT('Ctrl Pts',(-0.785796613400711,-7.64007724274336,
51.4572170097804));
#184232=CARTESIAN_POINT('Ctrl Pts',(4.24848612041541,-6.94696649308868,
51.6687736301623));
#184233=CARTESIAN_POINT('Ctrl Pts',(7.70417260804807,-2.64235740086951,
51.8803302505443));
#184234=CARTESIAN_POINT('Ctrl Pts',(7.29030095876973,2.43920654419265,52.0918868709261));
#184235=CARTESIAN_POINT('Ctrl Pts',(5.26189995080857,5.62130885552968,52.2505543362126));
#184236=CARTESIAN_POINT('Ctrl Pts',(1.92117852419122,7.45782167166676,52.409221801499));
#184237=CARTESIAN_POINT('Ctrl Pts',(-1.87221591806992,7.46335962794256,
52.5678892667854));
#184238=CARTESIAN_POINT('Ctrl Pts',(-5.21349836513446,5.66833611529721,
52.7265567320719));
#184239=CARTESIAN_POINT('Ctrl Pts',(-7.29236341282212,2.47176373057108,
52.8852241973583));
#184240=CARTESIAN_POINT('Ctrl Pts',(-7.5780129013641,-1.28955379830699,
53.0438916626446));
#184241=CARTESIAN_POINT('Ctrl Pts',(-5.54586987187687,-5.96786612029453,
53.2554482830267));
#184242=CARTESIAN_POINT('Ctrl Pts',(-0.464829181575225,-8.12567368653735,
53.4670049034085));
#184243=CARTESIAN_POINT('Ctrl Pts',(4.29663544586798,-6.36941225506916,
53.6785615237905));
#184244=CARTESIAN_POINT('Ctrl Pts',(7.70835491807636,-2.61225392038938,
53.8901181441723));
#184245=CARTESIAN_POINT('Ctrl Pts',(7.61057224416527,2.90710352379302,54.1016747645543));
#184246=CARTESIAN_POINT('Ctrl Pts',(4.03383745202061,6.54351587573162,54.3132313849361));
#184247=CARTESIAN_POINT('Ctrl Pts',(0.439312887650428,7.68729779242562,
54.4718988502226));
#184248=CARTESIAN_POINT('Ctrl Pts',(-3.30322330506354,6.95705479782095,
54.630566315509));
#184249=CARTESIAN_POINT('Ctrl Pts',(-6.21892296661873,4.53099989847321,
54.7892337807954));
#184250=CARTESIAN_POINT('Ctrl Pts',(-7.63463143902492,1.0120773019643,54.9479012460819));
#184251=CARTESIAN_POINT('Ctrl Pts',(-7.18272645166355,-2.77416309048803,
55.1065687113683));
#184252=CARTESIAN_POINT('Ctrl Pts',(-4.99234271294018,-5.84516551627964,
55.2652361766548));
#184253=CARTESIAN_POINT('Ctrl Pts',(-0.434729445610179,-8.13529863268552,
55.4767927970366));
#184254=CARTESIAN_POINT('Ctrl Pts',(4.84898798431694,-6.53680939820729,
55.6883494174187));
#184255=CARTESIAN_POINT('Ctrl Pts',(7.37972971975833,-2.13778567704362,
55.8999060378003));
#184256=CARTESIAN_POINT('Ctrl Pts',(7.59217979546274,2.93280880106663,56.1114626581825));
#184257=CARTESIAN_POINT('Ctrl Pts',(3.98100268887075,7.10800191541319,56.3230192785642));
#184258=CARTESIAN_POINT('Ctrl Pts',(-1.0950171302903,7.60857300457776,56.5345758989462));
#184259=CARTESIAN_POINT('Ctrl Pts',(-4.58773225049471,6.18387036607666,
56.6932433642326));
#184260=CARTESIAN_POINT('Ctrl Pts',(-6.99345745083907,3.22543815637297,
56.851910829519));
#184261=CARTESIAN_POINT('Ctrl Pts',(-7.6778644541053,-0.505330321822897,
57.0105782948054));
#184262=CARTESIAN_POINT('Ctrl Pts',(-6.5103870715291,-4.11421421390834,
57.1692457600919));
#184263=CARTESIAN_POINT('Ctrl Pts',(-3.73766650931412,-6.73181914256119,
57.3279132253782));
#184264=CARTESIAN_POINT('Ctrl Pts',(-0.0883513982762259,-7.68645820368191,
57.4865806906648));
#184265=CARTESIAN_POINT('Ctrl Pts',(4.87827385335432,-6.52491516017783,
57.6981373110465));
#184266=CARTESIAN_POINT('Ctrl Pts',(7.91107710357185,-1.91243837957983,
57.9096939314286));
#184267=CARTESIAN_POINT('Ctrl Pts',(7.03588074418887,3.08657099756842,58.1212505518105));
#184268=CARTESIAN_POINT('Ctrl Pts',(3.95041052253477,7.11595518519746,58.3328071721923));
#184269=CARTESIAN_POINT('Ctrl Pts',(-1.49723462369259,8.00814348757412,
58.5443637925744));
#184270=CARTESIAN_POINT('Ctrl Pts',(-5.71537578392953,5.14042073520366,
58.7559204129561));
#184271=CARTESIAN_POINT('Ctrl Pts',(-7.48436284634017,1.80882632869221,
58.9145878782426));
#184272=CARTESIAN_POINT('Ctrl Pts',(-7.43612494719741,-2.00398208298336,
59.073255343529));
#184273=CARTESIAN_POINT('Ctrl Pts',(-5.5714200206841,-5.30699917675582,
59.2319228088155));
#184274=CARTESIAN_POINT('Ctrl Pts',(-2.36290057339191,-7.32997948834203,
59.3905902741018));
#184275=CARTESIAN_POINT('Ctrl Pts',(1.4430614392871,-7.56340621581888,59.5492577393884));
#184276=CARTESIAN_POINT('Ctrl Pts',(4.85666785110194,-5.95837419691958,
59.7079252046747));
#184277=CARTESIAN_POINT('Ctrl Pts',(7.92594289223697,-1.8845431555021,59.9194818250565));
#184278=CARTESIAN_POINT('Ctrl Pts',(7.29948277548688,3.60001565339179,60.1310384454387));
#184279=CARTESIAN_POINT('Ctrl Pts',(3.42476508248566,6.87761023170662,60.3425950658204));
#184280=CARTESIAN_POINT('Ctrl Pts',(-1.52581916105486,7.99465054783844,
60.5541516862024));
#184281=CARTESIAN_POINT('Ctrl Pts',(-6.28019795748342,5.18952668851147,
60.7657083065843));
#184282=CARTESIAN_POINT('Ctrl Pts',(-7.68167340827104,0.285200517365215,
60.9772649269661));
#184283=CARTESIAN_POINT('Ctrl Pts',(-6.90546418446714,-3.40618618106626,
61.1359323922526));
#184284=CARTESIAN_POINT('Ctrl Pts',(-4.42566351984426,-6.30280896334092,
61.294599857539));
#184285=CARTESIAN_POINT('Ctrl Pts',(-0.877763597793129,-7.64424570349199,
61.4532673228255));
#184286=CARTESIAN_POINT('Ctrl Pts',(2.88185101533245,-7.1419068283392,61.6119347881118));
#184287=CARTESIAN_POINT('Ctrl Pts',(5.95367192347783,-4.88275849603854,
61.7706022533983));
#184288=CARTESIAN_POINT('Ctrl Pts',(7.54638607366438,-1.46338747898439,
61.9292697186847));
#184289=CARTESIAN_POINT('Ctrl Pts',(7.29302522198898,3.63095810322632,62.1408263390666));
#184290=CARTESIAN_POINT('Ctrl Pts',(3.29821233539819,7.44072287381559,62.3523829594485));
#184291=CARTESIAN_POINT('Ctrl Pts',(-1.77671591692733,7.47487919099873,
62.5639395798305));
#184292=CARTESIAN_POINT('Ctrl Pts',(-6.29350100357757,5.16085328334994,
62.7754962002123));
#184293=CARTESIAN_POINT('Ctrl Pts',(-8.14681260604421,-0.0389614931836734,
62.9870528205943));
#184294=CARTESIAN_POINT('Ctrl Pts',(-6.08081625560616,-4.70245886234001,
63.1986094409762));
#184295=CARTESIAN_POINT('Ctrl Pts',(-3.1198606493378,-7.03946087649886,
63.3572769062625));
#184296=CARTESIAN_POINT('Ctrl Pts',(0.639952549886159,-7.67478723829821,
63.515944371549));
#184297=CARTESIAN_POINT('Ctrl Pts',(4.22350174629681,-6.43171783491736,
63.6746118368354));
#184298=CARTESIAN_POINT('Ctrl Pts',(6.78835140935033,-3.6373319290962,63.8332793021219));
#184299=CARTESIAN_POINT('Ctrl Pts',(7.69956330106161,0.0653060180248196,
63.9919467674083));
#184300=CARTESIAN_POINT('Ctrl Pts',(6.73177318227711,3.71115554899262,64.1506142326947));
#184301=CARTESIAN_POINT('Ctrl Pts',(3.27343014738359,7.46034373914179,64.3621708530767));
#184302=CARTESIAN_POINT('Ctrl Pts',(-2.23465587805173,7.82616602181326,
64.5737274734585));
#184303=CARTESIAN_POINT('Ctrl Pts',(-6.15313962301333,4.60102283728218,
64.7852840938405));
#184304=CARTESIAN_POINT('Ctrl Pts',(-8.13865659747939,-0.0695002345335011,
64.9968407142223));
#184305=CARTESIAN_POINT('Ctrl Pts',(-6.23027481366242,-5.24935704464801,
65.2083973346043));
#184306=CARTESIAN_POINT('Ctrl Pts',(-1.65619771640194,-7.50642756646789,
65.4199539549862));
#184307=CARTESIAN_POINT('Ctrl Pts',(2.11451911297346,-7.40380637401568,
65.5786214202726));
#184308=CARTESIAN_POINT('Ctrl Pts',(5.40839251305042,-5.48280848142911,
65.737288885559));
#184309=CARTESIAN_POINT('Ctrl Pts',(7.36349073440769,-2.23247967812894,
65.8959563508455));
#184310=CARTESIAN_POINT('Ctrl Pts',(7.54253083489441,1.55631841983495,66.0546238161318));
#184311=CARTESIAN_POINT('Ctrl Pts',(5.86999233463708,4.98304423965384,66.2132912814184));
#184312=CARTESIAN_POINT('Ctrl Pts',(2.79111267227769,7.16234149821795,66.3719587467047));
#184313=CARTESIAN_POINT('Ctrl Pts',(-2.26625454400543,7.82535392028544,
66.5835153670866));
#184314=CARTESIAN_POINT('Ctrl Pts',(-6.72981225884627,4.57735605508002,
66.7950719874686));
#184315=CARTESIAN_POINT('Ctrl Pts',(-7.67221698888851,-0.409420132503432,
67.0066286078505));
#184316=CARTESIAN_POINT('Ctrl Pts',(-6.20444717322626,-5.26757978287376,
67.2181852282322));
#184317=CARTESIAN_POINT('Ctrl Pts',(-1.42057125095667,-8.02209766563004,
67.4297418486144));
#184318=CARTESIAN_POINT('Ctrl Pts',(3.53751282681393,-6.82462077236317,
67.6412984689961));
#184319=CARTESIAN_POINT('Ctrl Pts',(6.36697520396691,-4.33003079147432,
67.7999659342826));
#184320=CARTESIAN_POINT('Ctrl Pts',(7.66532591202258,-0.744766461198532,
67.9586333995689));
#184321=CARTESIAN_POINT('Ctrl Pts',(7.08408010050368,3.00345974479668,68.1173008648555));
#184322=CARTESIAN_POINT('Ctrl Pts',(4.79416941179473,6.02725792299139,68.2759683301418));
#184323=CARTESIAN_POINT('Ctrl Pts',(1.31456072762026,7.5867957660954,68.4346357954283));
#184324=CARTESIAN_POINT('Ctrl Pts',(-2.44566267792787,7.28753591773205,
68.5933032607148));
#184325=CARTESIAN_POINT('Ctrl Pts',(-6.75355386401727,4.55648810398642,
68.8048598810967));
#184326=CARTESIAN_POINT('Ctrl Pts',(-8.09983161915125,-0.797050334478962,
69.0164165014784));
#184327=CARTESIAN_POINT('Ctrl Pts',(-5.62853087504148,-5.22973981744729,
69.2279731218606));
#184328=CARTESIAN_POINT('Ctrl Pts',(-1.38906561415854,-8.0195422695973,
69.4395297422423));
#184329=CARTESIAN_POINT('Ctrl Pts',(4.04880596026311,-7.06959998388101,
69.6510863626243));
#184330=CARTESIAN_POINT('Ctrl Pts',(7.08850112603248,-2.97365052968238,
69.8626429830061));
#184331=CARTESIAN_POINT('Ctrl Pts',(7.66278567794466,0.754490262979475,
70.0213104482926));
#184332=CARTESIAN_POINT('Ctrl Pts',(6.36269585507655,4.33912432122458,70.1799779135791));
#184333=CARTESIAN_POINT('Ctrl Pts',(3.51502034613637,6.84467627249188,70.3386453788654));
#184334=CARTESIAN_POINT('Ctrl Pts',(-0.180470506905408,7.69930703475246,
70.4973128441519));
#184335=CARTESIAN_POINT('Ctrl Pts',(-3.85131619905127,6.66745104503739,
70.6559803094382));
#184336=CARTESIAN_POINT('Ctrl Pts',(-6.54674052566976,4.02860201260901,
70.8146477747248));
#184337=CARTESIAN_POINT('Ctrl Pts',(-8.10469122459747,-0.828283640961824,
71.0262043951065));
#184338=CARTESIAN_POINT('Ctrl Pts',(-5.70851519784241,-5.80132879005301,
71.2377610154887));
#184339=CARTESIAN_POINT('Ctrl Pts',(-0.971112084560053,-7.6215142648105,
71.4493176358703));
#184340=CARTESIAN_POINT('Ctrl Pts',(4.07135925484543,-7.0474531082001,71.6608742562524));
#184341=CARTESIAN_POINT('Ctrl Pts',(7.63803066372684,-2.83417734376672,
71.8724308766342));
#184342=CARTESIAN_POINT('Ctrl Pts',(7.34778730389881,2.25820004054282,72.0839874970162));
#184343=CARTESIAN_POINT('Ctrl Pts',(5.40021230982589,5.48864709303213,72.2426549623026));
#184344=CARTESIAN_POINT('Ctrl Pts',(2.10540739132609,7.40804685027035,72.401322427589));
#184345=CARTESIAN_POINT('Ctrl Pts',(-1.68631677184475,7.50741613699158,
72.5599898928755));
#184346=CARTESIAN_POINT('Ctrl Pts',(-5.07130495815068,5.79601280542814,
72.7186573581618));
#184347=CARTESIAN_POINT('Ctrl Pts',(-7.22874935220666,2.6519281110198,72.8773248234484));
#184348=CARTESIAN_POINT('Ctrl Pts',(-7.60769475727116,-1.10110225076198,
73.0359922887348));
#184349=CARTESIAN_POINT('Ctrl Pts',(-5.69223613839982,-5.82842357594631,
73.2475489091166));
#184350=CARTESIAN_POINT('Ctrl Pts',(-0.666323612318729,-8.11163203911284,
73.4591055294986));
#184351=CARTESIAN_POINT('Ctrl Pts',(4.1372640595256,-6.47407016267561,73.6706621498805));
#184352=CARTESIAN_POINT('Ctrl Pts',(7.64115849542936,-2.80272337950486,
73.8822187702623));
#184353=CARTESIAN_POINT('Ctrl Pts',(7.68036706291875,2.71735816829225,74.0937753906443));
#184354=CARTESIAN_POINT('Ctrl Pts',(4.19496609468124,6.44140552604157,74.3053320110261));
#184355=CARTESIAN_POINT('Ctrl Pts',(0.629931035627467,7.67402937141879,
74.4639994763127));
#184356=CARTESIAN_POINT('Ctrl Pts',(-3.1295735144678,7.03687914041394,74.622666941599));
#184357=CARTESIAN_POINT('Ctrl Pts',(-6.10457543692591,4.68392143869292,
74.7813344068855));
#184358=CARTESIAN_POINT('Ctrl Pts',(-7.60716689941602,1.20121196450923,
74.9400018721718));
#184359=CARTESIAN_POINT('Ctrl Pts',(-7.24935302134104,-2.59507623684127,
75.0986693374583));
#184360=CARTESIAN_POINT('Ctrl Pts',(-5.13584783304834,-5.71948535466407,
75.2573368027448));
#184361=CARTESIAN_POINT('Ctrl Pts',(-0.636465428932352,-8.12200624191624,
75.4688934231266));
#184362=CARTESIAN_POINT('Ctrl Pts',(4.6852900652918,-6.65511972081445,75.6804500435086));
#184363=CARTESIAN_POINT('Ctrl Pts',(7.32441022294305,-2.32024853313952,
75.8920066638904));
#184364=CARTESIAN_POINT('Ctrl Pts',(7.66261695397957,2.74351287784116,76.1035632842725));
#184365=CARTESIAN_POINT('Ctrl Pts',(4.1561553154331,7.00702837370805,76.3151199046541));
#184366=CARTESIAN_POINT('Ctrl Pts',(-0.905880310180398,7.63340202989932,
76.5266765250363));
#184367=CARTESIAN_POINT('Ctrl Pts',(-4.43287263356147,6.29580655020996,
76.6853439903225));
#184368=CARTESIAN_POINT('Ctrl Pts',(-6.91126780954659,3.39798111883746,
76.844011455609));
#184369=CARTESIAN_POINT('Ctrl Pts',(-7.68803961465247,-0.314655672919856,
77.0026789208954));
#184370=CARTESIAN_POINT('Ctrl Pts',(-6.61047280731541,-3.95139819342403,
77.1613463861817));
#184371=CARTESIAN_POINT('Ctrl Pts',(-3.90355943744507,-6.63699959480023,
77.3200138514683));
#184372=CARTESIAN_POINT('Ctrl Pts',(-0.279056488784278,-7.68189905964088,
77.4786813167547));
#184373=CARTESIAN_POINT('Ctrl Pts',(4.71486206543706,-6.64395585023371,
77.6902379371367));
#184374=CARTESIAN_POINT('Ctrl Pts',(7.86118577758629,-2.10815551242545,
77.9017945575185));
#184375=CARTESIAN_POINT('Ctrl Pts',(7.1103046633451,2.91103176964826,78.1133511779004));
#184376=CARTESIAN_POINT('Ctrl Pts',(4.12576992113469,7.01573831126531,78.3249077982824));
#184377=CARTESIAN_POINT('Ctrl Pts',(-1.29805898481169,8.04283013048902,
78.5364644186642));
#184378=CARTESIAN_POINT('Ctrl Pts',(-5.58606117719495,5.28065963787479,
78.7480210390462));
#184379=CARTESIAN_POINT('Ctrl Pts',(-7.43717394913015,1.9939868488595,78.9066885043326));
#184380=CARTESIAN_POINT('Ctrl Pts',(-7.48356218982991,-1.81884451512464,
79.065355969619));
#184381=CARTESIAN_POINT('Ctrl Pts',(-5.70139272677566,-5.16711547036028,
79.2240234349055));
#184382=CARTESIAN_POINT('Ctrl Pts',(-2.54405960589992,-7.26908929239964,
79.3826909001919));
#184383=CARTESIAN_POINT('Ctrl Pts',(1.25493822205205,-7.59688554355514,
79.5413583654783));
#184384=CARTESIAN_POINT('Ctrl Pts',(4.70732090191969,-6.07705320141218,
79.7000258307647));
#184385=CARTESIAN_POINT('Ctrl Pts',(7.87673918281708,-2.08063775843527,
79.9115824511467));
#184386=CARTESIAN_POINT('Ctrl Pts',(7.38656617778034,3.41777728876049,80.1231390715286));
#184387=CARTESIAN_POINT('Ctrl Pts',(3.59437202808532,6.79051014970209,80.3346956919104));
#184388=CARTESIAN_POINT('Ctrl Pts',(-1.32696953524914,8.03005064410032,
80.5462523122924));
#184389=CARTESIAN_POINT('Ctrl Pts',(-6.14949091428842,5.34376600638882,
80.7578089326743));
#184390=CARTESIAN_POINT('Ctrl Pts',(-7.67223111015648,0.475726264558584,
80.969365553056));
#184391=CARTESIAN_POINT('Ctrl Pts',(-6.98785921386535,-3.23378470375526,
81.1280330183426));
#184392=CARTESIAN_POINT('Ctrl Pts',(-4.58069911474279,-6.19104951033711,
81.2867004836291));
#184393=CARTESIAN_POINT('Ctrl Pts',(-1.06717815149796,-7.62011102950162,
81.4453679489154));
#184394=CARTESIAN_POINT('Ctrl Pts',(2.70374388560553,-7.21121816479727,
81.6040354142019));
#184395=CARTESIAN_POINT('Ctrl Pts',(5.83067758974013,-5.0289898337089,81.7627028794884));
#184396=CARTESIAN_POINT('Ctrl Pts',(7.50774982153899,-1.65019341400493,
81.9213703447746));
#184397=CARTESIAN_POINT('Ctrl Pts',(7.38087842071822,3.44887044907858,82.1329269651568));
#184398=CARTESIAN_POINT('Ctrl Pts',(3.48183136396736,7.35658968865254,82.3444835855383));
#184399=CARTESIAN_POINT('Ctrl Pts',(-1.59068667761081,7.51666510250124,
82.5560402059206));
#184400=CARTESIAN_POINT('Ctrl Pts',(-6.16350136797752,5.31543153292694,
82.7675968263023));
#184401=CARTESIAN_POINT('Ctrl Pts',(-8.14527086207023,0.163206064415523,
82.9791534466843));
#184402=CARTESIAN_POINT('Ctrl Pts',(-6.19563100587296,-4.55012111108156,
83.1907100670662));
#184403=CARTESIAN_POINT('Ctrl Pts',(-3.29357765288929,-6.95987687731857,
83.3493775323525));
#184404=CARTESIAN_POINT('Ctrl Pts',(0.449312806791323,-7.68830387152485,
83.508044997639));
#184405=CARTESIAN_POINT('Ctrl Pts',(4.06260417818805,-6.5345396624655,83.6667124629256));
#184406=CARTESIAN_POINT('Ctrl Pts',(6.69600416344681,-3.80465854740654,
83.8253799282118));
#184407=CARTESIAN_POINT('Ctrl Pts',(7.69881298730476,-0.125771576888246,
83.9840473934985));
#184408=CARTESIAN_POINT('Ctrl Pts',(6.82178922456726,3.54297014692783,84.1427148587846));
#184409=CARTESIAN_POINT('Ctrl Pts',(3.45754368027798,7.3768194592874,84.3542714791668));
#184410=CARTESIAN_POINT('Ctrl Pts',(-2.03976877626405,7.87920711960751,
84.5658280995486));
#184411=CARTESIAN_POINT('Ctrl Pts',(-6.0370748776523,4.75229053100797,84.7773847199304));
#184412=CARTESIAN_POINT('Ctrl Pts',(-8.13787515527384,0.132474342694702,
84.9889413403124));
#184413=CARTESIAN_POINT('Ctrl Pts',(-6.35861431178935,-5.09314221967737,
85.2004979606943));
#184414=CARTESIAN_POINT('Ctrl Pts',(-1.84195274888236,-7.46301921190938,
85.4120545810761));
#184415=CARTESIAN_POINT('Ctrl Pts',(1.93014946421949,-7.45399644142782,
85.5707220463626));
#184416=CARTESIAN_POINT('Ctrl Pts',(5.27067639873185,-5.61532445359144,
85.7293895116489));
#184417=CARTESIAN_POINT('Ctrl Pts',(7.30582649274669,-2.41451041970134,
85.8880569769355));
#184418=CARTESIAN_POINT('Ctrl Pts',(7.57882695690173,1.36867833203807,86.046724442222));
#184419=CARTESIAN_POINT('Ctrl Pts',(5.99183446563274,4.8358514906375,86.2053919075083));
#184420=CARTESIAN_POINT('Ctrl Pts',(2.96798007080302,7.09087723668659,86.3640593727949));
#184421=CARTESIAN_POINT('Ctrl Pts',(-2.07137786401307,7.87917935957984,
86.5756159931766));
#184422=CARTESIAN_POINT('Ctrl Pts',(-6.6141572156696,4.74294063010507,86.7871726135587));
#184423=CARTESIAN_POINT('Ctrl Pts',(-7.68001396649197,-0.218915152460824,
86.9987292339403));
#184424=CARTESIAN_POINT('Ctrl Pts',(-6.33324680436952,-5.11200023564539,
87.2102858543225));
#184425=CARTESIAN_POINT('Ctrl Pts',(-1.61919470951296,-7.98437737889667,
87.4218424747043));
#184426=CARTESIAN_POINT('Ctrl Pts',(3.36707696578925,-6.91029944307013,
87.633399095086));
#184427=CARTESIAN_POINT('Ctrl Pts',(6.25756903013603,-4.4866880587052,87.7920665603727));
#184428=CARTESIAN_POINT('Ctrl Pts',(7.64448494706102,-0.934745052625723,
87.9507340256589));
#184429=CARTESIAN_POINT('Ctrl Pts',(7.1564268500222,2.82675008609669,88.1094014909455));
#184430=CARTESIAN_POINT('Ctrl Pts',(4.94225399548035,5.90643918646504,88.2680689562319));
#184431=CARTESIAN_POINT('Ctrl Pts',(1.50241521768622,7.55184006826877,88.4267364215184));
#184432=CARTESIAN_POINT('Ctrl Pts',(-2.26407620763408,7.34597880560986,
88.5854038868047));
#184433=CARTESIAN_POINT('Ctrl Pts',(-6.63840932916552,4.72266823039694,
88.7969605071868));
#184434=CARTESIAN_POINT('Ctrl Pts',(-8.11711560933248,-0.595815138298367,
89.0085171275685));
#184435=CARTESIAN_POINT('Ctrl Pts',(-5.75656887678168,-5.08846274785982,
89.2200737479506));
#184436=CARTESIAN_POINT('Ctrl Pts',(-1.58763536404624,-7.98260455272119,
89.4316303683323));
#184437=CARTESIAN_POINT('Ctrl Pts',(3.87213373292876,-7.16789048397557,
89.6431869887142));
#184438=CARTESIAN_POINT('Ctrl Pts',(7.01253009438418,-3.14862944180495,
89.8547436090961));
#184439=CARTESIAN_POINT('Ctrl Pts',(7.67914815323174,0.564113059378357,
90.0134110743827));
#184440=CARTESIAN_POINT('Ctrl Pts',(6.46840800204212,4.17990386712071,90.172078539669));
#184441=CARTESIAN_POINT('Ctrl Pts',(3.68378227516248,6.75534673115761,90.3307460049555));
#184442=CARTESIAN_POINT('Ctrl Pts',(0.0106361900317569,7.70141449934472,
90.489413470242));
#184443=CARTESIAN_POINT('Ctrl Pts',(-3.6846837331035,6.76096484904669,90.6480809355283));
#184444=CARTESIAN_POINT('Ctrl Pts',(-6.44475867331778,4.18981280359029,
90.8067484008148));
#184445=CARTESIAN_POINT('Ctrl Pts',(-8.12274874381592,-0.626918240957216,
91.0183050211967));
#184446=CARTESIAN_POINT('Ctrl Pts',(-5.85071201863764,-5.65789098243707,
91.2298616415786));
#184447=CARTESIAN_POINT('Ctrl Pts',(-1.1599338352815,-7.59507023452402,
91.4414182619603));
#184448=CARTESIAN_POINT('Ctrl Pts',(3.89522963707608,-7.14631006664979,
91.6529748823425));
#184449=CARTESIAN_POINT('Ctrl Pts',(7.56535131998991,-3.02283526522436,
91.8645315027241));
#184450=CARTESIAN_POINT('Ctrl Pts',(7.40155992882987,2.0751762111144,92.0760881231063));
#184451=CARTESIAN_POINT('Ctrl Pts',(5.53474515720112,5.35295581395318,92.2347555883925));
#184452=CARTESIAN_POINT('Ctrl Pts',(2.28858287920351,7.35352206952492,92.393423053679));
#184453=CARTESIAN_POINT('Ctrl Pts',(-1.49950799427032,7.54694885907257,
92.5520905189655));
#184454=CARTESIAN_POINT('Ctrl Pts',(-4.9259207646105,5.92006782384962,92.710757984252));
#184455=CARTESIAN_POINT('Ctrl Pts',(-7.16071837898484,2.83048621488856,
92.8694254495382));
#184456=CARTESIAN_POINT('Ctrl Pts',(-7.63267504713682,-0.911985347958647,
93.028092914825));
#184457=CARTESIAN_POINT('Ctrl Pts',(-5.83511030861758,-5.68538137855928,
93.2396495352064));
#184458=CARTESIAN_POINT('Ctrl Pts',(-0.867401018586824,-8.0926001287187,
93.4512061555888));
#184459=CARTESIAN_POINT('Ctrl Pts',(3.97534210068024,-6.57473904924924,
93.6627627759704));
#184460=CARTESIAN_POINT('Ctrl Pts',(7.56925871710715,-2.99146858104545,
93.8743193963525));
#184461=CARTESIAN_POINT('Ctrl Pts',(7.74543080651569,2.52594026113027,94.0858760167343));
#184462=CARTESIAN_POINT('Ctrl Pts',(4.35351193806897,6.33532798619646,94.2974326371162));
#184463=CARTESIAN_POINT('Ctrl Pts',(0.820160810623469,7.65603515986074,
94.4561001024026));
#184464=CARTESIAN_POINT('Ctrl Pts',(-2.95399599008719,7.11237001552241,
94.614767567689));
#184465=CARTESIAN_POINT('Ctrl Pts',(-5.98646912853775,4.83395815856167,
94.7734350329756));
#184466=CARTESIAN_POINT('Ctrl Pts',(-7.57501656355332,1.38960755120628,
94.9321024982618));
#184467=CARTESIAN_POINT('Ctrl Pts',(-7.31151710827953,-2.41439254654737,
95.0907699635484));
#184468=CARTESIAN_POINT('Ctrl Pts',(-5.27618675172836,-5.5902806061917,
95.2494374288348));
#184469=CARTESIAN_POINT('Ctrl Pts',(-0.837817077204601,-8.10371735646381,
95.4609940492167));
#184470=CARTESIAN_POINT('Ctrl Pts',(4.51872136352693,-6.76932144471558,
95.6725506695986));
#184471=CARTESIAN_POINT('Ctrl Pts',(7.2645629643043,-2.50129446361673,95.8841072899803));
#184472=CARTESIAN_POINT('Ctrl Pts',(7.72837761593481,2.55255697709665,96.0956639103624));
#184473=CARTESIAN_POINT('Ctrl Pts',(4.32866351814856,6.90168043882907,96.3072205307442));
#184474=CARTESIAN_POINT('Ctrl Pts',(-0.71608079112348,7.65360327302554,
96.5187771511263));
#184475=CARTESIAN_POINT('Ctrl Pts',(-4.27550416892791,6.40371138155931,
96.6774446164126));
#184476=CARTESIAN_POINT('Ctrl Pts',(-6.82439171245445,3.5687316026304,96.836112081699));
#184477=CARTESIAN_POINT('Ctrl Pts',(-7.69429901276673,-0.124358320346745,
96.9947795469856));
#184478=CARTESIAN_POINT('Ctrl Pts',(-6.70494269733832,-3.78507144735772,
97.1534470122718));
#184479=CARTESIAN_POINT('Ctrl Pts',(-4.069928110878,-6.54009937356905,97.3121144775584));
#184480=CARTESIAN_POINT('Ctrl Pts',(-0.464471910680699,-7.66905552891195,
97.4707819428448));
#184481=CARTESIAN_POINT('Ctrl Pts',(4.53730628323536,-6.76657095782785,
97.6823385632266));
#184482=CARTESIAN_POINT('Ctrl Pts',(8.64709586509307,-1.17195344643985,
97.9467843387042));
#184483=CARTESIAN_POINT('Ctrl Pts',(6.17446001811424,5.31529267128248,98.2112301141812));
#184484=CARTESIAN_POINT('Ctrl Pts',(1.59344116709797,7.51571166844028,98.4227867345635));
#184485=CARTESIAN_POINT('Ctrl Pts',(-2.18287509741676,7.38815633678711,
98.5814541998497));
#184486=CARTESIAN_POINT('Ctrl Pts',(-5.45514273601227,5.43154102305253,
98.7401216651363));
#184487=CARTESIAN_POINT('Ctrl Pts',(-7.38490913140437,2.17042384937628,
98.8987891304226));
#184488=CARTESIAN_POINT('Ctrl Pts',(-7.52577891640735,-1.62945095326339,
99.0574721614392));
#184489=CARTESIAN_POINT('Ctrl Pts',(-6.39483282294218,-3.89356867963719,
99.1632660373603));
#184490=CARTESIAN_POINT('Ctrl Pts',(-5.59319257244812,-4.82318409174615,
99.2161707581859));
#184491=CARTESIAN_POINT('Ctrl Pts',(1.81148773798609,-6.76509875748211,
-0.647699818629882));
#184492=CARTESIAN_POINT('Ctrl Pts',(2.9356747642043,-6.4640767487774,-0.594804846492275));
#184493=CARTESIAN_POINT('Ctrl Pts',(5.03003528944759,-5.29274464953558,
-0.48902071925919));
#184494=CARTESIAN_POINT('Ctrl Pts',(6.94703914831561,-2.23909199201746,
-0.330347436930631));
#184495=CARTESIAN_POINT('Ctrl Pts',(7.17439520364204,1.34694727795299,-0.171679971644201));
#184496=CARTESIAN_POINT('Ctrl Pts',(5.65332152640384,4.62673929743261,-0.0130125063577741));
#184497=CARTESIAN_POINT('Ctrl Pts',(2.76117551751462,6.7417056139338,0.145654958928656));
#184498=CARTESIAN_POINT('Ctrl Pts',(-2.00393381935195,7.46117725044506,
0.35721157931056));
#184499=CARTESIAN_POINT('Ctrl Pts',(-7.40368502527241,3.69526160713211,
0.621657354787942));
#184500=CARTESIAN_POINT('Ctrl Pts',(-7.16726359359808,-2.88320234719017,
0.886103130265323));
#184501=CARTESIAN_POINT('Ctrl Pts',(-3.72798211249409,-6.25951141932115,
1.09765975064723));
#184502=CARTESIAN_POINT('Ctrl Pts',(-0.299318307035459,-7.29834602864205,
1.25632721593366));
#184503=CARTESIAN_POINT('Ctrl Pts',(3.23627226523133,-6.5447122871848,1.41499468122009));
#184504=CARTESIAN_POINT('Ctrl Pts',(5.96510980865824,-4.20302829244138,
1.57366214650652));
#184505=CARTESIAN_POINT('Ctrl Pts',(7.25376943663242,-0.843893506703157,
1.73232961179295));
#184506=CARTESIAN_POINT('Ctrl Pts',(6.76842455697729,2.73845433636508,1.89099707707937));
#184507=CARTESIAN_POINT('Ctrl Pts',(4.64515762980617,5.61747601173395,2.0496645423658));
#184508=CARTESIAN_POINT('Ctrl Pts',(0.28943226546954,7.71984168134768,2.26122116274771));
#184509=CARTESIAN_POINT('Ctrl Pts',(-4.696178645165,6.1246467636793,2.47277778312961));
#184510=CARTESIAN_POINT('Ctrl Pts',(-7.02924814289832,1.91551199337645,
2.68433440351152));
#184511=CARTESIAN_POINT('Ctrl Pts',(-7.15416271867062,-2.89527501251096,
2.89589102389342));
#184512=CARTESIAN_POINT('Ctrl Pts',(-3.66724954191068,-6.79944796472502,
3.10744764427533));
#184513=CARTESIAN_POINT('Ctrl Pts',(1.15305975893845,-7.19743373686098,
3.31900426465724));
#184514=CARTESIAN_POINT('Ctrl Pts',(4.4431290387692,-5.79391180272745,3.47767172994366));
#184515=CARTESIAN_POINT('Ctrl Pts',(6.67943187871092,-2.95260222294961,
3.63633919523009));
#184516=CARTESIAN_POINT('Ctrl Pts',(7.27203543413197,0.595002899120626,
3.79500666051652));
#184517=CARTESIAN_POINT('Ctrl Pts',(6.11063877182122,3.99909701236675,3.95367412580295));
#184518=CARTESIAN_POINT('Ctrl Pts',(3.44221456469882,6.4390943812103,4.11234159108937));
#184519=CARTESIAN_POINT('Ctrl Pts',(-0.0322420101525694,7.2891437288084,
4.27100905637581));
#184520=CARTESIAN_POINT('Ctrl Pts',(-4.72374865002565,6.11288153979805,
4.4825656767577));
#184521=CARTESIAN_POINT('Ctrl Pts',(-7.52964381413083,1.69385100404379,
4.69412229713962));
#184522=CARTESIAN_POINT('Ctrl Pts',(-6.6243886622802,-3.03268210390586,
4.90567891752152));
#184523=CARTESIAN_POINT('Ctrl Pts',(-3.63812709720399,-6.806518789496,5.11723553790342));
#184524=CARTESIAN_POINT('Ctrl Pts',(1.54044884797145,-7.57021402675952,
5.32879215828533));
#184525=CARTESIAN_POINT('Ctrl Pts',(5.49653934046743,-4.78755783384142,
5.54034877866723));
#184526=CARTESIAN_POINT('Ctrl Pts',(7.12349670978252,-1.60205299418428,
5.69901624395365));
#184527=CARTESIAN_POINT('Ctrl Pts',(7.02021416653516,2.01228108246361,5.85768370924009));
#184528=CARTESIAN_POINT('Ctrl Pts',(5.20236750987495,5.11584768931862,6.01635117452652));
#184529=CARTESIAN_POINT('Ctrl Pts',(2.12972100334069,6.98548284302409,6.17501863981295));
#184530=CARTESIAN_POINT('Ctrl Pts',(-1.482372895225,7.14936009422613,6.33368610509938));
#184531=CARTESIAN_POINT('Ctrl Pts',(-4.69471247615635,5.5760496351196,6.4923535703858));
#184532=CARTESIAN_POINT('Ctrl Pts',(-7.54331757626103,1.66717813081053,
6.70391019076773));
#184533=CARTESIAN_POINT('Ctrl Pts',(-6.86656994343393,-3.52347614302802,
6.91546681114959));
#184534=CARTESIAN_POINT('Ctrl Pts',(-3.14334088454267,-6.57260176518009,
7.12702343153154));
#184535=CARTESIAN_POINT('Ctrl Pts',(1.56734723595408,-7.55698945086143,
7.33858005191341));
#184536=CARTESIAN_POINT('Ctrl Pts',(6.03280890944917,-4.82559215419803,
7.55013667229535));
#184537=CARTESIAN_POINT('Ctrl Pts',(7.28757804590471,-0.154470033412791,
7.76169329267723));
#184538=CARTESIAN_POINT('Ctrl Pts',(6.49591206166936,3.33375248721907,7.92036075796366));
#184539=CARTESIAN_POINT('Ctrl Pts',(4.10100447634132,6.04271829434726,8.0790282232501));
#184540=CARTESIAN_POINT('Ctrl Pts',(0.71686550381877,7.26103499095718,8.23769568853653));
#184541=CARTESIAN_POINT('Ctrl Pts',(-2.84017988572185,6.72800567156045,
8.39636315382295));
#184542=CARTESIAN_POINT('Ctrl Pts',(-5.71858768820421,4.53966232348845,
8.55503061910938));
#184543=CARTESIAN_POINT('Ctrl Pts',(-7.1770895003255,1.27359376203791,8.7136980843958));
#184544=CARTESIAN_POINT('Ctrl Pts',(-6.85998029030304,-3.55271634009679,
8.92525470477772));
#184545=CARTESIAN_POINT('Ctrl Pts',(-3.0148526110767,-7.10459926048452,
9.13681132515961));
#184546=CARTESIAN_POINT('Ctrl Pts',(1.79738669100636,-7.06038858441899,
9.34836794554153));
#184547=CARTESIAN_POINT('Ctrl Pts',(6.04498924497277,-4.79820507552116,
9.55992456592342));
#184548=CARTESIAN_POINT('Ctrl Pts',(7.72370085836326,0.15990005333229,9.77148118630533));
#184549=CARTESIAN_POINT('Ctrl Pts',(5.69446886265255,4.55034934248621,9.98303780668723));
#184550=CARTESIAN_POINT('Ctrl Pts',(2.85180711825711,6.72145633916047,10.1417052719737));
#184551=CARTESIAN_POINT('Ctrl Pts',(-0.722597256169256,7.26708575050433,
10.3003727372601));
#184552=CARTESIAN_POINT('Ctrl Pts',(-4.10152883824344,6.03440025847895,
10.4590402025466));
#184553=CARTESIAN_POINT('Ctrl Pts',(-6.49118048992967,3.34623040852877,
10.617707667833));
#184554=CARTESIAN_POINT('Ctrl Pts',(-7.29924993347423,-0.178127953052982,
10.7763751331194));
#184555=CARTESIAN_POINT('Ctrl Pts',(-6.32662643415969,-3.62028351499932,
10.9350425984058));
#184556=CARTESIAN_POINT('Ctrl Pts',(-2.99105958231506,-7.12282847972478,
11.1465992187878));
#184557=CARTESIAN_POINT('Ctrl Pts',(2.23687814569076,-7.38654473214131,
11.3581558391696));
#184558=CARTESIAN_POINT('Ctrl Pts',(5.90345804255817,-4.26952796217054,
11.5697124595516));
#184559=CARTESIAN_POINT('Ctrl Pts',(7.71550693145034,0.188731845047503,
11.7812690799335));
#184560=CARTESIAN_POINT('Ctrl Pts',(5.82792165520761,5.07113913803384,11.9928257003154));
#184561=CARTESIAN_POINT('Ctrl Pts',(1.45700724129014,7.14211345927886,12.2043823206973));
#184562=CARTESIAN_POINT('Ctrl Pts',(-2.11659747242143,6.98790342654516,
12.3630497859837));
#184563=CARTESIAN_POINT('Ctrl Pts',(-5.21064498668082,5.11682136903217,
12.5217172512701));
#184564=CARTESIAN_POINT('Ctrl Pts',(-7.01528763922469,2.00555843330852,
12.6803847165566));
#184565=CARTESIAN_POINT('Ctrl Pts',(-7.12785800821589,-1.58944088110218,
12.839052181843));
#184566=CARTESIAN_POINT('Ctrl Pts',(-5.49034419207099,-4.81320057878068,
12.9977196471294));
#184567=CARTESIAN_POINT('Ctrl Pts',(-2.53825459376162,-6.83300215012639,
13.1563871124158));
#184568=CARTESIAN_POINT('Ctrl Pts',(2.26682573146794,-7.38529783283597,
13.3679437327978));
#184569=CARTESIAN_POINT('Ctrl Pts',(6.44986511072266,-4.23838494854773,
13.5795003531797));
#184570=CARTESIAN_POINT('Ctrl Pts',(7.26812821260535,0.503982306367112,
13.7910569735616));
#184571=CARTESIAN_POINT('Ctrl Pts',(5.80315849686722,5.08802696325712,14.0026135939435));
#184572=CARTESIAN_POINT('Ctrl Pts',(1.22581826102254,7.62748271499059,14.2141702143254));
#184573=CARTESIAN_POINT('Ctrl Pts',(-3.45704788576664,6.41727938318885,
14.4257268347073));
#184574=CARTESIAN_POINT('Ctrl Pts',(-6.10211325965028,4.009363157084,14.5843942999937));
#184575=CARTESIAN_POINT('Ctrl Pts',(-7.27901458618669,0.590447926482588,
14.7430617652802));
#184576=CARTESIAN_POINT('Ctrl Pts',(-6.67134261913644,-2.95460876404428,
14.9017292305666));
#184577=CARTESIAN_POINT('Ctrl Pts',(-4.45455716730087,-5.78702017821389,
15.060396695853));
#184578=CARTESIAN_POINT('Ctrl Pts',(-1.13187581356497,-7.21315716601607,
15.2190641611394));
#184579=CARTESIAN_POINT('Ctrl Pts',(2.42881185107581,-6.87266525872296,
15.3777316264259));
#184580=CARTESIAN_POINT('Ctrl Pts',(6.47206043035504,-4.21824095594001,
15.5892882468078));
#184581=CARTESIAN_POINT('Ctrl Pts',(7.66771469904878,0.877962534841119,
15.8008448671897));
#184582=CARTESIAN_POINT('Ctrl Pts',(5.25768245471256,5.04345725523755,16.0124014875716));
#184583=CARTESIAN_POINT('Ctrl Pts',(1.19598519098265,7.62458433893572,16.2239581079535));
#184584=CARTESIAN_POINT('Ctrl Pts',(-3.94552092764966,6.6418361607326,16.4355147283354));
#184585=CARTESIAN_POINT('Ctrl Pts',(-6.76574644210875,2.71243983296901,
16.6470713487173));
#184586=CARTESIAN_POINT('Ctrl Pts',(-7.25397792594533,-0.831013482971238,
16.8057388140037));
#184587=CARTESIAN_POINT('Ctrl Pts',(-5.96721292964101,-4.21011305692988,
16.9644062792902));
#184588=CARTESIAN_POINT('Ctrl Pts',(-3.22941224766971,-6.54273809846264,
17.1230737445766));
#184589=CARTESIAN_POINT('Ctrl Pts',(0.287315719605487,-7.29726878887394,
17.281741209863));
#184590=CARTESIAN_POINT('Ctrl Pts',(3.75220410825254,-6.26352484540415,
17.4404086751494));
#184591=CARTESIAN_POINT('Ctrl Pts',(6.26800584722447,-3.7208543999388,17.5990761404359));
#184592=CARTESIAN_POINT('Ctrl Pts',(7.67185086544985,0.9076493126936,17.8106327608178));
#184593=CARTESIAN_POINT('Ctrl Pts',(5.32489154541977,5.58660871621691,18.0221893811997));
#184594=CARTESIAN_POINT('Ctrl Pts',(0.805715678220419,7.24089139028274,
18.2337460015816));
#184595=CARTESIAN_POINT('Ctrl Pts',(-3.96657026414156,6.62049750836153,
18.4453026219635));
#184596=CARTESIAN_POINT('Ctrl Pts',(-7.28467029558708,2.57190623101386,
18.6568592423454));
#184597=CARTESIAN_POINT('Ctrl Pts',(-6.93262114598217,-2.25198108621383,
18.8684158627273));
#184598=CARTESIAN_POINT('Ctrl Pts',(-5.03729766256775,-5.28549065060871,
19.0270833280137));
#184599=CARTESIAN_POINT('Ctrl Pts',(-1.88440410108215,-7.0556150180995,
19.1857507933002));
#184600=CARTESIAN_POINT('Ctrl Pts',(1.71216705625404,-7.09260243224952,
19.3444182585866));
#184601=CARTESIAN_POINT('Ctrl Pts',(4.89576720374872,-5.41886940113016,
19.503085723873));
#184602=CARTESIAN_POINT('Ctrl Pts',(6.89386514584056,-2.40528636755529,
19.6617531891595));
#184603=CARTESIAN_POINT('Ctrl Pts',(7.19651283393127,1.15881741333419,19.8204206544458));
#184604=CARTESIAN_POINT('Ctrl Pts',(5.3090478383308,5.6120525680763,20.0319772748278));
#184605=CARTESIAN_POINT('Ctrl Pts',(0.509337346907726,7.7009897016967,20.2435338952097));
#184606=CARTESIAN_POINT('Ctrl Pts',(-4.02040297608755,6.07585761764272,
20.4550905155916));
#184607=CARTESIAN_POINT('Ctrl Pts',(-7.28716117403683,2.5420363770418,20.6666471359734));
#184608=CARTESIAN_POINT('Ctrl Pts',(-7.24102205384756,-2.69234518444979,
20.8782037563553));
#184609=CARTESIAN_POINT('Ctrl Pts',(-3.88018004147492,-6.17064482952338,
21.0897603767373));
#184610=CARTESIAN_POINT('Ctrl Pts',(-0.481436928319875,-7.28553344944846,
21.2484278420237));
#184611=CARTESIAN_POINT('Ctrl Pts',(3.07346940853279,-6.62468624876828,
21.4070953073102));
#184612=CARTESIAN_POINT('Ctrl Pts',(5.85866375653926,-4.34886011252219,
21.5657627725966));
#184613=CARTESIAN_POINT('Ctrl Pts',(7.23076101275068,-1.02409827472313,
21.724430237883));
#184614=CARTESIAN_POINT('Ctrl Pts',(6.83420758004411,2.56989998090389,21.8830977031693));
#184615=CARTESIAN_POINT('Ctrl Pts',(4.78316007615802,5.50036675615653,22.0417651684559));
#184616=CARTESIAN_POINT('Ctrl Pts',(0.480871141789132,7.7103752127592,22.2533217888377));
#184617=CARTESIAN_POINT('Ctrl Pts',(-4.54273890266845,6.23924596251632,
22.4648784092197));
#184618=CARTESIAN_POINT('Ctrl Pts',(-6.97955867591758,2.08936511156489,
22.6764350296014));
#184619=CARTESIAN_POINT('Ctrl Pts',(-7.22379777980997,-2.71687551334363,
22.8879916499834));
#184620=CARTESIAN_POINT('Ctrl Pts',(-3.83484522790946,-6.70634662499014,
23.0995482703654));
#184621=CARTESIAN_POINT('Ctrl Pts',(0.974108399536885,-7.22383330319408,
23.3111048907473));
#184622=CARTESIAN_POINT('Ctrl Pts',(4.29798968114909,-5.90237781404394,
23.4697723560337));
#184623=CARTESIAN_POINT('Ctrl Pts',(6.60410948866788,-3.11743804453164,
23.6284398213202));
#184624=CARTESIAN_POINT('Ctrl Pts',(7.28456049178172,0.414371490388069,
23.7871072866066));
#184625=CARTESIAN_POINT('Ctrl Pts',(6.20799117870954,3.84623551344313,23.9457747518929));
#184626=CARTESIAN_POINT('Ctrl Pts',(3.60093471970036,6.35169649018581,24.1044422171794));
#184627=CARTESIAN_POINT('Ctrl Pts',(0.148641251043096,7.28769926279015,
24.2631096824659));
#184628=CARTESIAN_POINT('Ctrl Pts',(-4.57060869449693,6.22821476334319,
24.4746663028478));
#184629=CARTESIAN_POINT('Ctrl Pts',(-7.48529396902207,1.88017050182036,
24.6862229232297));
#184630=CARTESIAN_POINT('Ctrl Pts',(-6.69760208823655,-2.86737024948825,
24.8977795436115));
#184631=CARTESIAN_POINT('Ctrl Pts',(-3.80590427361161,-6.71414622857579,
25.1093361639936));
#184632=CARTESIAN_POINT('Ctrl Pts',(1.35212671216194,-7.60610783060528,
25.3208927843753));
#184633=CARTESIAN_POINT('Ctrl Pts',(5.37604808188003,-4.92247516882494,
25.5324494047574));
#184634=CARTESIAN_POINT('Ctrl Pts',(7.08154981624727,-1.77832262511345,
25.6911168700437));
#184635=CARTESIAN_POINT('Ctrl Pts',(7.06798540710253,1.83746139681678,25.8497843353302));
#184636=CARTESIAN_POINT('Ctrl Pts',(5.32771060717042,4.98518053602045,26.0084518006166));
#184637=CARTESIAN_POINT('Ctrl Pts',(2.30240347260139,6.93048485671525,26.167119265903));
#184638=CARTESIAN_POINT('Ctrl Pts',(-1.30451174193647,7.18394239078603,
26.3257867311895));
#184639=CARTESIAN_POINT('Ctrl Pts',(-4.55490242328604,5.69082759189972,
26.4844541964758));
#184640=CARTESIAN_POINT('Ctrl Pts',(-7.49962539392981,1.85384517348665,
26.6960108168578));
#184641=CARTESIAN_POINT('Ctrl Pts',(-6.9518873900729,-3.35200367457123,
26.9075674372397));
#184642=CARTESIAN_POINT('Ctrl Pts',(-3.30546598448613,-6.49257887941348,
27.1191240576216));
#184643=CARTESIAN_POINT('Ctrl Pts',(1.3793449751289,-7.5935547906221,27.3306806780035));
#184644=CARTESIAN_POINT('Ctrl Pts',(5.91120873762003,-4.97380480485731,
27.5422372983854));
#184645=CARTESIAN_POINT('Ctrl Pts',(7.28150105130914,-0.33525692560751,
27.7537939187673));
#184646=CARTESIAN_POINT('Ctrl Pts',(6.57663582428421,3.17153596759111,27.9124613840537));
#184647=CARTESIAN_POINT('Ctrl Pts',(4.24968613157374,5.93909503905403,28.0711288493402));
#184648=CARTESIAN_POINT('Ctrl Pts',(0.896820584063796,7.24101085004523,
28.2297963146266));
#184649=CARTESIAN_POINT('Ctrl Pts',(-2.67235615860355,6.79641042473009,
28.388463779913));
#184650=CARTESIAN_POINT('Ctrl Pts',(-5.60417935245751,4.68016590993002,
28.5471312451994));
#184651=CARTESIAN_POINT('Ctrl Pts',(-7.14327651483552,1.45129438742917,
28.7057987104858));
#184652=CARTESIAN_POINT('Ctrl Pts',(-6.94602533424502,-3.3813983841842,
28.9173553308678));
#184653=CARTESIAN_POINT('Ctrl Pts',(-3.19021829660363,-7.02760088071376,
29.1289119512497));
#184654=CARTESIAN_POINT('Ctrl Pts',(1.621636284852,-7.10281505036224,29.3404685716316));
#184655=CARTESIAN_POINT('Ctrl Pts',(5.92406490744834,-4.9467284027863,29.5520251920136));
#184656=CARTESIAN_POINT('Ctrl Pts',(7.72529037506664,-0.0318056196188755,
29.7635818123952));
#184657=CARTESIAN_POINT('Ctrl Pts',(5.80562811966761,4.4076452786617,29.9751384327773));
#184658=CARTESIAN_POINT('Ctrl Pts',(3.01771567371964,6.64862175729444,30.1338058980636));
#184659=CARTESIAN_POINT('Ctrl Pts',(-0.542048797792806,7.28277867304903,
30.2924733633502));
#184660=CARTESIAN_POINT('Ctrl Pts',(-3.95052789288905,6.13431778260462,
30.4511408286365));
#184661=CARTESIAN_POINT('Ctrl Pts',(-6.40614816070303,3.5062726424121,30.609808293923));
#184662=CARTESIAN_POINT('Ctrl Pts',(-7.30142245391351,0.00305097852067317,
30.7684757592094));
#184663=CARTESIAN_POINT('Ctrl Pts',(-6.41451232295641,-3.46217943281746,
30.9271432244959));
#184664=CARTESIAN_POINT('Ctrl Pts',(-3.16688493518839,-7.04641488870857,
31.1386998448778));
#184665=CARTESIAN_POINT('Ctrl Pts',(2.05289915213799,-7.43977634003499,
31.3502564652597));
#184666=CARTESIAN_POINT('Ctrl Pts',(5.79569591456842,-4.41470211292401,
31.5618130856415));
#184667=CARTESIAN_POINT('Ctrl Pts',(7.71781440523383,-0.00277938102652562,
31.7733697060235));
#184668=CARTESIAN_POINT('Ctrl Pts',(5.95196273323992,4.92496320784834,31.9849263264054));
#184669=CARTESIAN_POINT('Ctrl Pts',(1.63378349280986,7.10376000896753,32.1964829467872));
#184670=CARTESIAN_POINT('Ctrl Pts',(-1.94254742766151,7.03827312984283,
32.3551504120736));
#184671=CARTESIAN_POINT('Ctrl Pts',(-5.08207139110319,5.24454311408885,
32.5138178773602));
#184672=CARTESIAN_POINT('Ctrl Pts',(-6.96336145416715,2.17901871242365,
32.6724853426466));
#184673=CARTESIAN_POINT('Ctrl Pts',(-7.16510371778309,-1.4120803140109,
32.831152807933));
#184674=CARTESIAN_POINT('Ctrl Pts',(-5.60808871082753,-4.67548074217737,
32.9898202732195));
#184675=CARTESIAN_POINT('Ctrl Pts',(-2.70702760250579,-6.76791373509264,
33.1484877385058));
#184676=CARTESIAN_POINT('Ctrl Pts',(2.08286845720673,-7.43927294609562,
33.3600443588877));
#184677=CARTESIAN_POINT('Ctrl Pts',(6.34270751989519,-4.39712727080515,
33.5716009792697));
#184678=CARTESIAN_POINT('Ctrl Pts',(7.27839608796281,0.323475295391082,
33.7831575996516));
#184679=CARTESIAN_POINT('Ctrl Pts',(5.92762625552265,4.94246030772449,33.9947142200335));
#184680=CARTESIAN_POINT('Ctrl Pts',(1.41470968505858,7.5947165505724,34.2062708404153));
#184681=CARTESIAN_POINT('Ctrl Pts',(-3.29674459808255,6.5010868184787,34.4178274607972));
#184682=CARTESIAN_POINT('Ctrl Pts',(-6.00074570958766,4.15954686087893,
34.5764949260837));
#184683=CARTESIAN_POINT('Ctrl Pts',(-7.26212184340316,0.770888079667298,
34.7351623913702));
#184684=CARTESIAN_POINT('Ctrl Pts',(-6.74260426573862,-2.78815584322628,
34.8938298566566));
#184685=CARTESIAN_POINT('Ctrl Pts',(-4.59678504746441,-5.67470257610159,
35.0524973219429));
#184686=CARTESIAN_POINT('Ctrl Pts',(-1.31051506173837,-7.18284967348886,
35.2111647872294));
#184687=CARTESIAN_POINT('Ctrl Pts',(2.25752519810666,-6.93081775451478,
35.3698322525159));
#184688=CARTESIAN_POINT('Ctrl Pts',(6.36539585962406,-4.37754023703014,
35.5813888728977));
#184689=CARTESIAN_POINT('Ctrl Pts',(7.68713950594037,0.687425003039892,
35.7929454932797));
#184690=CARTESIAN_POINT('Ctrl Pts',(5.38121221862192,4.91143980296563,36.0045021136616));
#184691=CARTESIAN_POINT('Ctrl Pts',(1.38481388060976,7.59255934679895,36.2160587340434));
#184692=CARTESIAN_POINT('Ctrl Pts',(-3.77949506399831,6.73769545451185,
36.4276153544254));
#184693=CARTESIAN_POINT('Ctrl Pts',(-6.69635649186656,2.87949031952191,
36.6391719748073));
#184694=CARTESIAN_POINT('Ctrl Pts',(-7.27236513221127,-0.650756899909756,
36.7978394400936));
#184695=CARTESIAN_POINT('Ctrl Pts',(-6.06984555801552,-4.06074586765109,
36.9565069053802));
#184696=CARTESIAN_POINT('Ctrl Pts',(-3.39076980577527,-6.46058862757227,
37.1151743706665));
#184697=CARTESIAN_POINT('Ctrl Pts',(0.106152327585571,-7.30215131198709,
37.273841835953));
#184698=CARTESIAN_POINT('Ctrl Pts',(3.59562521266251,-6.35470365076517,
37.4325093012393));
#184699=CARTESIAN_POINT('Ctrl Pts',(6.17374629198885,-3.87524341023087,
37.5911767665259));
#184700=CARTESIAN_POINT('Ctrl Pts',(7.6920110484677,0.717000004733298,37.8027333869076));
#184701=CARTESIAN_POINT('Ctrl Pts',(5.4618784117509,5.45275628777254,38.0142900072896));
#184702=CARTESIAN_POINT('Ctrl Pts',(0.985143555367147,7.21866871765976,
38.2258466276716));
#184703=CARTESIAN_POINT('Ctrl Pts',(-3.80106741782214,6.71688569232528,
38.4374032480534));
#184704=CARTESIAN_POINT('Ctrl Pts',(-7.21860777051966,2.75187660187186,
38.6489598684354));
#184705=CARTESIAN_POINT('Ctrl Pts',(-6.98636728977761,-2.079261132881,38.8605164888174));
#184706=CARTESIAN_POINT('Ctrl Pts',(-5.16690111965938,-5.15886731547199,
39.0191839541036));
#184707=CARTESIAN_POINT('Ctrl Pts',(-2.05890237191696,-7.00668274740058,
39.1778514193902));
#184708=CARTESIAN_POINT('Ctrl Pts',(1.53564353401614,-7.13290433322274,
39.3365188846766));
#184709=CARTESIAN_POINT('Ctrl Pts',(4.75979552383996,-5.53868474197975,
39.4951863499629));
#184710=CARTESIAN_POINT('Ctrl Pts',(6.83205747267912,-2.57561057790029,
39.6538538152494));
#184711=CARTESIAN_POINT('Ctrl Pts',(7.22305188360824,0.979885836762448,
39.8125212805359));
#184712=CARTESIAN_POINT('Ctrl Pts',(5.44667094866521,5.4785854518756,40.0240779009177));
#184713=CARTESIAN_POINT('Ctrl Pts',(0.70027339451393,7.68597970928423,40.2356345212996));
#184714=CARTESIAN_POINT('Ctrl Pts',(-3.86839828499266,6.17374931372075,
40.4471911416815));
#184715=CARTESIAN_POINT('Ctrl Pts',(-7.22183907457001,2.72207775414406,
40.6587477620636));
#184716=CARTESIAN_POINT('Ctrl Pts',(-7.30560046055917,-2.51183695474356,
40.8703043824454));
#184717=CARTESIAN_POINT('Ctrl Pts',(-4.0321040698922,-6.07246173606261,
41.0818610028273));
#184718=CARTESIAN_POINT('Ctrl Pts',(-0.662072407292881,-7.27134370570371,
41.2405284681137));
#184719=CARTESIAN_POINT('Ctrl Pts',(2.90813762291469,-6.69891167772874,
41.3991959334001));
#184720=CARTESIAN_POINT('Ctrl Pts',(5.74894686808211,-4.49289830715243,
41.5578633986865));
#184721=CARTESIAN_POINT('Ctrl Pts',(7.20312249887356,-1.2032075324176,41.716530863973));
#184722=CARTESIAN_POINT('Ctrl Pts',(6.895872888007,2.39952417604162,41.8751983292594));
#184723=CARTESIAN_POINT('Ctrl Pts',(4.91817373664537,5.37998344444512,42.0338657945458));
#184724=CARTESIAN_POINT('Ctrl Pts',(0.672048847298596,7.69606869276473,
42.2454224149276));
#184725=CARTESIAN_POINT('Ctrl Pts',(-4.38651904627686,6.35004862771582,
42.4569790353096));
#184726=CARTESIAN_POINT('Ctrl Pts',(-6.92556390782915,2.26191300436849,
42.6685356556916));
#184727=CARTESIAN_POINT('Ctrl Pts',(-7.28899018731462,-2.53678713479404,
42.8800922760735));
#184728=CARTESIAN_POINT('Ctrl Pts',(-4.00007615653303,-6.60912352102177,
43.0916488964554));
#184729=CARTESIAN_POINT('Ctrl Pts',(0.79455576613854,-7.24578055880295,
43.3032055168372));
#184730=CARTESIAN_POINT('Ctrl Pts',(4.15020425571326,-6.00721098198628,
43.4618729821236));
#184731=CARTESIAN_POINT('Ctrl Pts',(6.52471965689241,-3.28035295661377,
43.6205404474101));
#184732=CARTESIAN_POINT('Ctrl Pts',(7.2925996967946,0.233484323109056,43.7792079126966));
#184733=CARTESIAN_POINT('Ctrl Pts',(6.30152038869049,3.69100567502789,43.937875377983));
#184734=CARTESIAN_POINT('Ctrl Pts',(3.75743735449865,6.26038686999263,44.0965428432694));
#184735=CARTESIAN_POINT('Ctrl Pts',(0.329432956660445,7.28176684936425,
44.2552103085558));
#184736=CARTESIAN_POINT('Ctrl Pts',(-4.41465400982639,6.33971242730919,
44.4667669289379));
#184737=CARTESIAN_POINT('Ctrl Pts',(-7.43633439938857,2.06533208401449,
44.6783235493196));
#184738=CARTESIAN_POINT('Ctrl Pts',(-6.76669096150921,-2.70029249845544,
44.8898801697016));
#184739=CARTESIAN_POINT('Ctrl Pts',(-3.97133751784657,-6.61763908395221,
45.1014367900834));
#184740=CARTESIAN_POINT('Ctrl Pts',(1.16297162300613,-7.63731711283647,
45.3129934104654));
#184741=CARTESIAN_POINT('Ctrl Pts',(5.25224641083348,-5.05436161866343,
45.5245500308472));
#184742=CARTESIAN_POINT('Ctrl Pts',(7.03524116617045,-1.95349597184172,
45.6832174961336));
#184743=CARTESIAN_POINT('Ctrl Pts',(7.11140532561285,1.66150793145855,45.8418849614201));
#184744=CARTESIAN_POINT('Ctrl Pts',(5.44977010852736,4.85144755338035,46.0005524267066));
#184745=CARTESIAN_POINT('Ctrl Pts',(2.47367298599438,6.87121090774512,46.159219891993));
#184746=CARTESIAN_POINT('Ctrl Pts',(-1.12585644665751,7.21411540452755,
46.3178873572794));
#184747=CARTESIAN_POINT('Ctrl Pts',(-4.41227083275708,5.80207445140952,
46.4765548225659));
#184748=CARTESIAN_POINT('Ctrl Pts',(-7.45135195258497,2.03943046573758,
46.6881114429478));
#184749=CARTESIAN_POINT('Ctrl Pts',(-7.03285233929692,-3.17858157919814,
46.8996680633297));
#184750=CARTESIAN_POINT('Ctrl Pts',(-3.46563939458162,-6.40842269937884,
47.1112246837114));
#184751=CARTESIAN_POINT('Ctrl Pts',(1.19070073991183,-7.62577738708096,
47.3227813040936));
#184752=CARTESIAN_POINT('Ctrl Pts',(5.78555262545727,-5.11828609161979,
47.5343379244752));
#184753=CARTESIAN_POINT('Ctrl Pts',(7.2714528460407,-0.516662245363808,
47.7458945448574));
#184754=CARTESIAN_POINT('Ctrl Pts',(6.65222829110491,3.00910509262411,47.9045620101436));
#184755=CARTESIAN_POINT('Ctrl Pts',(4.39785033760639,5.82843611756107,48.0632294754302));
#184756=CARTESIAN_POINT('Ctrl Pts',(1.0722670766346,7.22290518291542,48.2218969407165));
#184757=CARTESIAN_POINT('Ctrl Pts',(-2.49574161037706,6.84901064311975,
48.3805644060031));
#184758=CARTESIAN_POINT('Ctrl Pts',(-6.49768330440811,4.16528213733704,
48.592121026385));
#184759=CARTESIAN_POINT('Ctrl Pts',(-7.97288646550528,-2.23495874205941,
48.8565668018623));
#184760=CARTESIAN_POINT('Ctrl Pts',(-2.42543815460554,-7.91903654965738,
49.173901732435));
#184761=CARTESIAN_POINT('Ctrl Pts',(4.01126713847677,-6.59282808396492,
49.4383475079127));
#184762=CARTESIAN_POINT('Ctrl Pts',(6.78562435075981,-2.66063041889896,
49.6499041282944));
#184763=CARTESIAN_POINT('Ctrl Pts',(7.25070165219227,0.905871586941507,
49.8085715935808));
#184764=CARTESIAN_POINT('Ctrl Pts',(5.92324844439043,4.24730823449819,49.9672390588673));
#184765=CARTESIAN_POINT('Ctrl Pts',(2.26526197427776,7.37794179712212,50.1787956792492));
#184766=CARTESIAN_POINT('Ctrl Pts',(-4.29604199495613,7.07721117740128,
50.4432414547267));
#184767=CARTESIAN_POINT('Ctrl Pts',(-8.28235171648892,0.208719700560167,
50.7605763852993));
#184768=CARTESIAN_POINT('Ctrl Pts',(-5.26568578465025,-5.64120008672477,
51.0250221607768));
#184769=CARTESIAN_POINT('Ctrl Pts',(-0.745136697720609,-7.2447524332675,
51.2365787811588));
#184770=CARTESIAN_POINT('Ctrl Pts',(4.0286543160041,-6.58750570256803,51.4481354015405));
#184771=CARTESIAN_POINT('Ctrl Pts',(7.3055312760722,-2.50563241722382,51.6596920219226));
#184772=CARTESIAN_POINT('Ctrl Pts',(6.91307482008316,2.31299330946768,51.8712486423043));
#184773=CARTESIAN_POINT('Ctrl Pts',(4.98963050516779,5.33044231299205,52.0299161075908));
#184774=CARTESIAN_POINT('Ctrl Pts',(1.82176990436786,7.07192741460845,52.1885835728774));
#184775=CARTESIAN_POINT('Ctrl Pts',(-1.77534079788555,7.07717881730109,
52.3472510381637));
#184776=CARTESIAN_POINT('Ctrl Pts',(-4.94373338993647,5.37503621483437,
52.5059185034503));
#184777=CARTESIAN_POINT('Ctrl Pts',(-6.91503055541669,2.34386587105855,
52.6645859687366));
#184778=CARTESIAN_POINT('Ctrl Pts',(-7.18589952197611,-1.22282769156393,
52.823253434023));
#184779=CARTESIAN_POINT('Ctrl Pts',(-5.25890681105704,-5.65906747048718,
53.034810054405));
#184780=CARTESIAN_POINT('Ctrl Pts',(-0.440777264060952,-7.70522238742984,
53.2463666747867));
#184781=CARTESIAN_POINT('Ctrl Pts',(4.07431222385627,-6.0398361779948,53.4579232951687));
#184782=CARTESIAN_POINT('Ctrl Pts',(7.30949717848282,-2.47708659804833,
53.6694799155507));
#184783=CARTESIAN_POINT('Ctrl Pts',(7.21677412840871,2.75667963275689,53.8810365359325));
#184784=CARTESIAN_POINT('Ctrl Pts',(3.82511233426199,6.2049310571903,54.0925931563145));
#184785=CARTESIAN_POINT('Ctrl Pts',(0.416581274069471,7.28952962351591,
54.2512606216008));
#184786=CARTESIAN_POINT('Ctrl Pts',(-3.13230276561864,6.59707200248025,
54.4099280868873));
#184787=CARTESIAN_POINT('Ctrl Pts',(-5.89713374135158,4.29654982490879,
54.5685955521736));
#184788=CARTESIAN_POINT('Ctrl Pts',(-7.23958841483069,0.959708817476291,
54.7272630174602));
#184789=CARTESIAN_POINT('Ctrl Pts',(-6.81106660114069,-2.6306180109872,
54.8859304827466));
#184790=CARTESIAN_POINT('Ctrl Pts',(-4.73402111891364,-5.54271583276722,
55.0445979480329));
#184791=CARTESIAN_POINT('Ctrl Pts',(-0.412234995645997,-7.71434930458152,
55.2561545684149));
#184792=CARTESIAN_POINT('Ctrl Pts',(4.5980840745598,-6.19857159670066,55.4677111887967));
#184793=CARTESIAN_POINT('Ctrl Pts',(6.99787621844488,-2.02716903160589,
55.6792678091788));
#184794=CARTESIAN_POINT('Ctrl Pts',(7.19933337051351,2.7810548274256,55.8908244295606));
#184795=CARTESIAN_POINT('Ctrl Pts',(3.77501142994787,6.74020857855475,56.1023810499424));
#184796=CARTESIAN_POINT('Ctrl Pts',(-1.03835704366409,7.2148783365985,56.3139376703245));
#184797=CARTESIAN_POINT('Ctrl Pts',(-4.35034664296364,5.86389488721425,
56.4726051356107));
#184798=CARTESIAN_POINT('Ctrl Pts',(-6.63159105256981,3.05854249758164,
56.6312726008973));
#184799=CARTESIAN_POINT('Ctrl Pts',(-7.28058439972057,-0.479182731052562,
56.7899400661836));
#184800=CARTESIAN_POINT('Ctrl Pts',(-6.17351645531762,-3.90133011619834,
56.9486075314703));
#184801=CARTESIAN_POINT('Ctrl Pts',(-3.54426633105253,-6.383490842283,57.1072749967566));
#184802=CARTESIAN_POINT('Ctrl Pts',(-0.0837797822335151,-7.28873347808429,
57.265942462043));
#184803=CARTESIAN_POINT('Ctrl Pts',(4.62585458842083,-6.18729280891253,
57.4774990824248));
#184804=CARTESIAN_POINT('Ctrl Pts',(7.50172979603139,-1.81348200596989,
57.6890557028069));
#184805=CARTESIAN_POINT('Ctrl Pts',(6.67181921361558,2.92686082019994,57.9006123231887));
#184806=CARTESIAN_POINT('Ctrl Pts',(3.74600221126334,6.7477503178319,58.1121689435707));
#184807=CARTESIAN_POINT('Ctrl Pts',(-1.41976237131267,7.59377361958786,
58.3237255639525));
#184808=CARTESIAN_POINT('Ctrl Pts',(-5.41964188346264,4.87443705687105,
58.5352821843343));
#184809=CARTESIAN_POINT('Ctrl Pts',(-7.09709525436815,1.7152312116475,58.6939496496209));
#184810=CARTESIAN_POINT('Ctrl Pts',(-7.05135335594398,-1.90028891209286,
58.8526171149072));
#184811=CARTESIAN_POINT('Ctrl Pts',(-5.28313490415875,-5.03239613652711,
59.0112845801937));
#184812=CARTESIAN_POINT('Ctrl Pts',(-2.24063568138787,-6.95070024120576,
59.16995204548));
#184813=CARTESIAN_POINT('Ctrl Pts',(1.36839230042598,-7.17204863836807,
59.3286195107666));
#184814=CARTESIAN_POINT('Ctrl Pts',(4.6053665576827,-5.65006669303664,59.4872869760529));
#184815=CARTESIAN_POINT('Ctrl Pts',(7.51582637584101,-1.78703018014501,
59.6988435964349));
#184816=CARTESIAN_POINT('Ctrl Pts',(6.92178153689894,3.41373802070961,59.9104002168167));
#184817=CARTESIAN_POINT('Ctrl Pts',(3.24755553856133,6.52173818118763,60.1219568371987));
#184818=CARTESIAN_POINT('Ctrl Pts',(-1.44686784289751,7.58097885261414,
60.3335134575804));
#184819=CARTESIAN_POINT('Ctrl Pts',(-5.95523814593559,4.92100209324587,
60.5450700779626));
#184820=CARTESIAN_POINT('Ctrl Pts',(-7.2841962650308,0.270443226750529,
60.7566266983443));
#184821=CARTESIAN_POINT('Ctrl Pts',(-6.54815087122025,-3.22993797567694,
60.9152941636308));
#184822=CARTESIAN_POINT('Ctrl Pts',(-4.19666392570424,-5.97667917781263,
61.0739616289173));
#184823=CARTESIAN_POINT('Ctrl Pts',(-0.832344982766427,-7.24870520300951,
61.2326290942037));
#184824=CARTESIAN_POINT('Ctrl Pts',(2.73273377903013,-6.7723591305212,61.3912965594901));
#184825=CARTESIAN_POINT('Ctrl Pts',(5.64560773197164,-4.63010717971888,
61.5499640247765));
#184826=CARTESIAN_POINT('Ctrl Pts',(7.15590917899213,-1.38766659843069,
61.7086314900631));
#184827=CARTESIAN_POINT('Ctrl Pts',(6.91565812021998,3.44307939797683,61.9201881104448));
#184828=CARTESIAN_POINT('Ctrl Pts',(3.12755108137218,7.05571336946174,62.131744730827));
#184829=CARTESIAN_POINT('Ctrl Pts',(-1.68478230696036,7.08810231713357,
62.3433013512086));
#184830=CARTESIAN_POINT('Ctrl Pts',(-5.96785284504113,4.89381235219824,
62.5548579715907));
#184831=CARTESIAN_POINT('Ctrl Pts',(-7.72526750394742,-0.0369454867507081,
62.7664145919723));
#184832=CARTESIAN_POINT('Ctrl Pts',(-5.76617316348448,-4.45913689127116,
62.9779712123546));
#184833=CARTESIAN_POINT('Ctrl Pts',(-2.95842794681348,-6.6752140971279,
63.1366386776407));
#184834=CARTESIAN_POINT('Ctrl Pts',(0.60683912552941,-7.27766641001998,
63.2953061429274));
#184835=CARTESIAN_POINT('Ctrl Pts',(4.00496272239341,-6.09891784521749,
63.4539736082136));
#184836=CARTESIAN_POINT('Ctrl Pts',(6.43709792822806,-3.44912341939349,
63.6126410735002));
#184837=CARTESIAN_POINT('Ctrl Pts',(7.30116047104696,0.0619268520408896,
63.7713085387865));
#184838=CARTESIAN_POINT('Ctrl Pts',(6.38344726014772,3.51912714224657,63.929976004073));
#184839=CARTESIAN_POINT('Ctrl Pts',(3.10405121203629,7.07431898132906,64.1415326244549));
#184840=CARTESIAN_POINT('Ctrl Pts',(-2.1190268233751,7.42121231608492,64.3530892448369));
#184841=CARTESIAN_POINT('Ctrl Pts',(-5.83475426225583,4.36294952745141,
64.5646458652188));
#184842=CARTESIAN_POINT('Ctrl Pts',(-7.71753351631633,-0.0659040448481696,
64.7762024856005));
#184843=CARTESIAN_POINT('Ctrl Pts',(-5.90789820339546,-4.97773661364814,
64.9877591059827));
#184844=CARTESIAN_POINT('Ctrl Pts',(-1.5705001473999,-7.11801826728487,
65.1993157263643));
#184845=CARTESIAN_POINT('Ctrl Pts',(2.00510636243311,-7.02070706085311,
65.3579831916509));
#184846=CARTESIAN_POINT('Ctrl Pts',(5.12854302045228,-5.1991084415673,65.5166506569372));
#184847=CARTESIAN_POINT('Ctrl Pts',(6.98247749603737,-2.11696322778764,
65.6753181222237));
#184848=CARTESIAN_POINT('Ctrl Pts',(7.15225342400797,1.47578896139401,65.8339855875101));
#184849=CARTESIAN_POINT('Ctrl Pts',(5.56625802311303,4.72520378175507,65.9926530527966));
#184850=CARTESIAN_POINT('Ctrl Pts',(2.64669056104292,6.79173643779485,66.151320518083));
#184851=CARTESIAN_POINT('Ctrl Pts',(-2.14899046180211,7.42044223558275,
66.3628771384648));
#184852=CARTESIAN_POINT('Ctrl Pts',(-6.38158780187974,4.34050734885831,
66.574433758847));
#184853=CARTESIAN_POINT('Ctrl Pts',(-7.27522915446962,-0.388235276547787,
66.7859903792287));
#184854=CARTESIAN_POINT('Ctrl Pts',(-5.88340697707009,-4.99501644249114,
66.9975469996106));
#184855=CARTESIAN_POINT('Ctrl Pts',(-1.34706583454681,-7.60700575876824,
67.2091036199925));
#184856=CARTESIAN_POINT('Ctrl Pts',(3.35446931300563,-6.47149058521199,
67.4206602403744));
#184857=CARTESIAN_POINT('Ctrl Pts',(6.03752522859704,-4.10597957533119,
67.5793277056609));
#184858=CARTESIAN_POINT('Ctrl Pts',(7.26869464646582,-0.706229591737301,
67.7379951709472));
#184859=CARTESIAN_POINT('Ctrl Pts',(6.71752456355499,2.84805003967782,67.8966626362337));
#184860=CARTESIAN_POINT('Ctrl Pts',(4.54610201023635,5.71538612976684,68.0553301015202));
#184861=CARTESIAN_POINT('Ctrl Pts',(1.24654067328318,7.19422793000284,68.2139975668065));
#184862=CARTESIAN_POINT('Ctrl Pts',(-2.31911537984757,6.91045285211747,
68.372665032093));
#184863=CARTESIAN_POINT('Ctrl Pts',(-6.40410093183477,4.32071917988316,
68.584221652475));
#184864=CARTESIAN_POINT('Ctrl Pts',(-7.68071748065629,-0.755808111186017,
68.7957782728568));
#184865=CARTESIAN_POINT('Ctrl Pts',(-5.33729063949043,-4.95913445165674,
69.0073348932388));
#184866=CARTESIAN_POINT('Ctrl Pts',(-1.31719041161549,-7.6045825880282,
69.2188915136204));
#184867=CARTESIAN_POINT('Ctrl Pts',(3.83930631857219,-6.70379369974262,
69.4304481340026));
#184868=CARTESIAN_POINT('Ctrl Pts',(6.72171682947581,-2.81978325952998,
69.6420047543843));
#184869=CARTESIAN_POINT('Ctrl Pts',(7.26628585314707,0.715450249379216,
69.8006722196709));
#184870=CARTESIAN_POINT('Ctrl Pts',(6.03346730846074,4.11460257346222,69.9593396849572));
#184871=CARTESIAN_POINT('Ctrl Pts',(3.33314067339355,6.49050834232903,70.1180071502437));
#184872=CARTESIAN_POINT('Ctrl Pts',(-0.171132320066243,7.30091746486942,
70.2766746155301));
#184873=CARTESIAN_POINT('Ctrl Pts',(-3.65203538103765,6.32245337939566,
70.4353420808165));
#184874=CARTESIAN_POINT('Ctrl Pts',(-6.20798885225487,3.82014779513346,
70.5940095461031));
#184875=CARTESIAN_POINT('Ctrl Pts',(-7.68532563280746,-0.785425295142584,
70.805566166485));
#184876=CARTESIAN_POINT('Ctrl Pts',(-5.41313628853616,-5.50114737489614,
71.0171227868668));
#184877=CARTESIAN_POINT('Ctrl Pts',(-0.920863286333173,-7.22714996993175,
71.2286794072488));
#184878=CARTESIAN_POINT('Ctrl Pts',(3.86069262536099,-6.68279278229367,
71.4402360276305));
#184879=CARTESIAN_POINT('Ctrl Pts',(7.24281175153894,-2.68752691303847,
71.6517926480126));
#184880=CARTESIAN_POINT('Ctrl Pts',(6.96758661695657,2.14135272703773,71.8633492683943));
#184881=CARTESIAN_POINT('Ctrl Pts',(5.12078609007939,5.20464494260962,72.0220167336809));
#184882=CARTESIAN_POINT('Ctrl Pts',(1.99646611371851,7.02472811976237,72.1806841989672));
#184883=CARTESIAN_POINT('Ctrl Pts',(-1.59906073563403,7.11895568564848,
72.3393516642537));
#184884=CARTESIAN_POINT('Ctrl Pts',(-4.80889757630398,5.49610645825061,
72.4980191295401));
#184885=CARTESIAN_POINT('Ctrl Pts',(-6.85470811288226,2.51470790474134,
72.6566865948267));
#184886=CARTESIAN_POINT('Ctrl Pts',(-7.21404553293573,-1.04412729832816,
72.815354060113));
#184887=CARTESIAN_POINT('Ctrl Pts',(-5.39769956561297,-5.52684018005931,
73.026910680495));
#184888=CARTESIAN_POINT('Ctrl Pts',(-0.631845655261508,-7.69190730485752,
73.2384673008768));
#184889=CARTESIAN_POINT('Ctrl Pts',(3.92318728070288,-6.13907871268419,
73.4500239212587));
#184890=CARTESIAN_POINT('Ctrl Pts',(7.24577773808827,-2.65770048892236,
73.6615805416405));
#184891=CARTESIAN_POINT('Ctrl Pts',(7.28295751464004,2.5767523777974,73.8731371620225));
#184892=CARTESIAN_POINT('Ctrl Pts',(3.97790360703262,6.10810426069667,74.0846937824044));
#184893=CARTESIAN_POINT('Ctrl Pts',(0.597336160113752,7.27694775787233,
74.2433612476908));
#184894=CARTESIAN_POINT('Ctrl Pts',(-2.96763823370572,6.6727659492638,74.4020287129772));
#184895=CARTESIAN_POINT('Ctrl Pts',(-5.78870296013572,4.4415586599514,74.5606961782637));
#184896=CARTESIAN_POINT('Ctrl Pts',(-7.21354498832617,1.13905697890869,
74.7193636435501));
#184897=CARTESIAN_POINT('Ctrl Pts',(-6.87424567478813,-2.4607977490316,
74.8780311088366));
#184898=CARTESIAN_POINT('Ctrl Pts',(-4.87010077296131,-5.42353881036963,
75.0366985741231));
#184899=CARTESIAN_POINT('Ctrl Pts',(-0.603532440634412,-7.70174470945635,
75.2482551945048));
#184900=CARTESIAN_POINT('Ctrl Pts',(4.44285646893518,-6.31076012181055,
75.4598118148867));
#184901=CARTESIAN_POINT('Ctrl Pts',(6.94541914943549,-2.20019060961902,
75.6713684352688));
#184902=CARTESIAN_POINT('Ctrl Pts',(7.26612585956091,2.60155374951464,75.8829250556504));
#184903=CARTESIAN_POINT('Ctrl Pts',(3.9411010357416,6.64445976755175,76.0944816760327));
#184904=CARTESIAN_POINT('Ctrl Pts',(-0.859006836306801,7.23842261971224,
76.3060382964143));
#184905=CARTESIAN_POINT('Ctrl Pts',(-4.20350001419982,5.97003909447874,
76.4647057617009));
#184906=CARTESIAN_POINT('Ctrl Pts',(-6.55365419606634,3.22215747259319,
76.6233732269872));
#184907=CARTESIAN_POINT('Ctrl Pts',(-7.29023306121847,-0.298374267641428,
76.7820406922739));
#184908=CARTESIAN_POINT('Ctrl Pts',(-6.2684233986423,-3.74693877654286,
76.9407081575602));
#184909=CARTESIAN_POINT('Ctrl Pts',(-3.70157536819349,-6.29357759565777,
77.0993756228467));
#184910=CARTESIAN_POINT('Ctrl Pts',(-0.264617112092581,-7.28441024039501,
77.258043088133));
#184911=CARTESIAN_POINT('Ctrl Pts',(4.47089830846142,-6.30017390965787,
77.4695997085149));
#184912=CARTESIAN_POINT('Ctrl Pts',(7.45442002495854,-1.99907203724375,
77.6811563288968));
#184913=CARTESIAN_POINT('Ctrl Pts',(6.7423921741066,2.76040461717969,77.8927129492787));
#184914=CARTESIAN_POINT('Ctrl Pts',(3.9122878899729,6.65271902191615,78.1042695696606));
#184915=CARTESIAN_POINT('Ctrl Pts',(-1.23089278942452,7.62666545204912,
78.3158261900425));
#184916=CARTESIAN_POINT('Ctrl Pts',(-5.29701847508189,5.00741949920571,
78.5273828104243));
#184917=CARTESIAN_POINT('Ctrl Pts',(-7.05234807878031,1.89081086698427,
78.6860502757109));
#184918=CARTESIAN_POINT('Ctrl Pts',(-7.09633602667755,-1.72473102143047,
78.8447177409972));
#184919=CARTESIAN_POINT('Ctrl Pts',(-5.40638235949169,-4.89975051134758,
79.0033852062838));
#184920=CARTESIAN_POINT('Ctrl Pts',(-2.4124209002896,-6.89296072088419,
79.1620526715701));
#184921=CARTESIAN_POINT('Ctrl Pts',(1.19000324852048,-7.20379562643837,
79.3207201368566));
#184922=CARTESIAN_POINT('Ctrl Pts',(4.46374735160504,-5.762604823118,79.479387602143));
#184923=CARTESIAN_POINT('Ctrl Pts',(7.46916864160353,-1.97297814985959,
79.6909442225248));
#184924=CARTESIAN_POINT('Ctrl Pts',(7.00435893377828,3.24092931817309,79.9025008429068));
#184925=CARTESIAN_POINT('Ctrl Pts',(3.40838641667833,6.43914496766489,80.1140574632888));
#184926=CARTESIAN_POINT('Ctrl Pts',(-1.25830740500682,7.61454722180501,
80.3256140836704));
#184927=CARTESIAN_POINT('Ctrl Pts',(-5.83129435071655,5.06726051943635,
80.5371707040526));
#184928=CARTESIAN_POINT('Ctrl Pts',(-7.27524254505289,0.45111049315681,
80.7487273244343));
#184929=CARTESIAN_POINT('Ctrl Pts',(-6.62628248831729,-3.06645716487308,
80.9073947897209));
#184930=CARTESIAN_POINT('Ctrl Pts',(-4.3436774267066,-5.87070255697951,
81.0660622550072));
#184931=CARTESIAN_POINT('Ctrl Pts',(-1.01195855279319,-7.2258193430159,
81.2247297202939));
#184932=CARTESIAN_POINT('Ctrl Pts',(2.56384254658913,-6.83808405155319,
81.3833971855802));
#184933=CARTESIAN_POINT('Ctrl Pts',(5.52897756315095,-4.76877198712165,
81.5420646508666));
#184934=CARTESIAN_POINT('Ctrl Pts',(7.11927210416887,-1.56480652899543,
81.700732116153));
#184935=CARTESIAN_POINT('Ctrl Pts',(6.99896548152559,3.27041360762663,81.9122887365349));
#184936=CARTESIAN_POINT('Ctrl Pts',(3.30166900737668,6.97593353497021,82.1238453569169));
#184937=CARTESIAN_POINT('Ctrl Pts',(-1.50837888309741,7.12772607673909,
82.3354019772986));
#184938=CARTESIAN_POINT('Ctrl Pts',(-5.84457985362841,5.040392172555,82.5469585976806));
#184939=CARTESIAN_POINT('Ctrl Pts',(-7.72380553529811,0.15476120132443,
82.7585152180625));
#184940=CARTESIAN_POINT('Ctrl Pts',(-5.87504698961766,-4.31468163786957,
82.9700718384444));
#184941=CARTESIAN_POINT('Ctrl Pts',(-3.1231562138444,-6.59974805753279,
83.1287393037308));
#184942=CARTESIAN_POINT('Ctrl Pts',(0.426063761775637,-7.29048364449903,
83.2874067690173));
#184943=CARTESIAN_POINT('Ctrl Pts',(3.85239056755428,-6.19641930517066,
83.4460742343038));
#184944=CARTESIAN_POINT('Ctrl Pts',(6.34952905775618,-3.60779196247734,
83.6047416995901));
#184945=CARTESIAN_POINT('Ctrl Pts',(7.30044898119642,-0.119263707518461,
83.7634091648767));
#184946=CARTESIAN_POINT('Ctrl Pts',(6.46880555178464,3.35964425193858,83.9220766301628));
#184947=CARTESIAN_POINT('Ctrl Pts',(3.27863805495089,6.99511654521669,84.1336332505451));
#184948=CARTESIAN_POINT('Ctrl Pts',(-1.93422387439578,7.47150887855398,
84.3451898709266));
#184949=CARTESIAN_POINT('Ctrl Pts',(-5.72469512022691,4.50639009190849,
84.5567464913088));
#184950=CARTESIAN_POINT('Ctrl Pts',(-7.71679250871388,0.12561964834773,
84.7683031116905));
#184951=CARTESIAN_POINT('Ctrl Pts',(-6.02959695876113,-4.82960490013786,
84.9798597320726));
#184952=CARTESIAN_POINT('Ctrl Pts',(-1.74664355286513,-7.07685601560598,
85.1914163524544));
#184953=CARTESIAN_POINT('Ctrl Pts',(1.83027665600578,-7.06830011540703,
85.3500838177409));
#184954=CARTESIAN_POINT('Ctrl Pts',(4.99795282841499,-5.32476756532573,
85.5087512830274));
#184955=CARTESIAN_POINT('Ctrl Pts',(6.92779700763227,-2.28957505042186,
85.6674187483137));
#184956=CARTESIAN_POINT('Ctrl Pts',(7.18667145538067,1.2978580400887,85.8260862136001));
#184957=CARTESIAN_POINT('Ctrl Pts',(5.68179560826557,4.5856273098538,85.9847536788866));
#184958=CARTESIAN_POINT('Ctrl Pts',(2.81440621039045,6.72396999170129,86.1434211441729));
#184959=CARTESIAN_POINT('Ctrl Pts',(-1.96419739535731,7.47148255492902,
86.3549777645549));
#184960=CARTESIAN_POINT('Ctrl Pts',(-6.27191716258488,4.49752398818139,
86.5665343849368));
#184961=CARTESIAN_POINT('Ctrl Pts',(-7.28262268868008,-0.207587702725921,
86.7780910053187));
#184962=CARTESIAN_POINT('Ctrl Pts',(-6.0055420565309,-4.84748713518995,
86.9896476257005));
#184963=CARTESIAN_POINT('Ctrl Pts',(-1.53541180788712,-7.57123725402508,
87.2012042460826));
#184964=CARTESIAN_POINT('Ctrl Pts',(3.19285241050017,-6.55273593632057,
87.4127608664643));
#184965=CARTESIAN_POINT('Ctrl Pts',(5.93378011989038,-4.25453083756324,
87.5714283317508));
#184966=CARTESIAN_POINT('Ctrl Pts',(7.24893206726411,-0.886378014165637,
87.7300957970374));
#184967=CARTESIAN_POINT('Ctrl Pts',(6.78612783456396,2.68048396813518,87.8887632623237));
#184968=CARTESIAN_POINT('Ctrl Pts',(4.68652417010452,5.60081898500862,88.0474307276101));
#184969=CARTESIAN_POINT('Ctrl Pts',(1.42467490292049,7.16108096448926,88.2060981928966));
#184970=CARTESIAN_POINT('Ctrl Pts',(-2.14692484031357,6.96587169681071,
88.3647656581829));
#184971=CARTESIAN_POINT('Ctrl Pts',(-6.2949143853457,4.47830055464174,88.5763222785649));
#184972=CARTESIAN_POINT('Ctrl Pts',(-7.69710713562227,-0.564985540828742,
88.7878788989468));
#184973=CARTESIAN_POINT('Ctrl Pts',(-5.45870349896631,-4.82516756085981,
88.9994355193286));
#184974=CARTESIAN_POINT('Ctrl Pts',(-1.50548545536504,-7.56955616019048,
89.2109921397107));
#184975=CARTESIAN_POINT('Ctrl Pts',(3.67177574156303,-6.79699829926463,
89.4225487600925));
#184976=CARTESIAN_POINT('Ctrl Pts',(6.64967680960369,-2.98570813948777,
89.6341053804744));
#184977=CARTESIAN_POINT('Ctrl Pts',(7.28180167568186,0.534923840390631,
89.7927728457607));
#184978=CARTESIAN_POINT('Ctrl Pts',(6.13370953240971,3.96362075277572,89.9514403110474));
#184979=CARTESIAN_POINT('Ctrl Pts',(3.49317025910436,6.40580102964331,90.1101077763336));
#184980=CARTESIAN_POINT('Ctrl Pts',(0.0100858356748187,7.30291588173718,
90.2687752416203));
#184981=CARTESIAN_POINT('Ctrl Pts',(-3.49402507240063,6.41112844610182,
90.4274427069065));
#184982=CARTESIAN_POINT('Ctrl Pts',(-6.11128390418936,3.97301696557805,
90.586110172193));
#184983=CARTESIAN_POINT('Ctrl Pts',(-7.70244879166303,-0.594479258170914,
90.7976667925749));
#184984=CARTESIAN_POINT('Ctrl Pts',(-5.54797533933734,-5.3651315503526,
91.0092234129566));
#184985=CARTESIAN_POINT('Ctrl Pts',(-1.0999147271144,-7.2020742479624,91.2207800333388));
#184986=CARTESIAN_POINT('Ctrl Pts',(3.69367658136524,-6.77653452959786,
91.4323366537205));
#184987=CARTESIAN_POINT('Ctrl Pts',(7.17389309592108,-2.86642300166554,
91.6438932741026));
#184988=CARTESIAN_POINT('Ctrl Pts',(7.01857685474278,1.96779920245041,91.8554498944844));
#184989=CARTESIAN_POINT('Ctrl Pts',(5.24835772874336,5.07597481362446,92.0141173597708));
#184990=CARTESIAN_POINT('Ctrl Pts',(2.17016344940649,6.97302464538271,92.1727848250574));
#184991=CARTESIAN_POINT('Ctrl Pts',(-1.42191810959926,7.15644284387873,
92.3314522903436));
#184992=CARTESIAN_POINT('Ctrl Pts',(-4.67103607877668,5.6137424281515,92.4901197556303));
#184993=CARTESIAN_POINT('Ctrl Pts',(-6.7901973045322,2.68402677631578,92.6487872209163));
#184994=CARTESIAN_POINT('Ctrl Pts',(-7.23773325362728,-0.864795977685073,
92.8074546862032));
#184995=CARTESIAN_POINT('Ctrl Pts',(-5.53318091736492,-5.39119949546233,
93.0190113065847));
#184996=CARTESIAN_POINT('Ctrl Pts',(-0.822518600318388,-7.67386017329631,
93.2305679269669));
#184997=CARTESIAN_POINT('Ctrl Pts',(3.7696437407526,-6.23453863249735,93.4421245473486));
#184998=CARTESIAN_POINT('Ctrl Pts',(7.17759831039387,-2.83667934145,93.6536811677308));
#184999=CARTESIAN_POINT('Ctrl Pts',(7.34465462839491,2.39523911495703,93.8652377881125));
#185000=CARTESIAN_POINT('Ctrl Pts',(4.12824572376432,6.00751555059719,94.0767944084945));
#185001=CARTESIAN_POINT('Ctrl Pts',(0.77772276897837,7.25988463091326,94.2354618737807));
#185002=CARTESIAN_POINT('Ctrl Pts',(-2.80114571582029,6.74435065760574,
94.3941293390673));
#185003=CARTESIAN_POINT('Ctrl Pts',(-5.67670789282248,4.58383194552335,
94.5527968043538));
#185004=CARTESIAN_POINT('Ctrl Pts',(-7.18305822535622,1.31770430691009,
94.7114642696399));
#185005=CARTESIAN_POINT('Ctrl Pts',(-6.93319317044822,-2.28946327644473,
94.8701317349268));
#185006=CARTESIAN_POINT('Ctrl Pts',(-5.00317805612032,-5.3010195757933,
95.0287992002129));
#185007=CARTESIAN_POINT('Ctrl Pts',(-0.794465437437333,-7.68440215607981,
95.240355820595));
#185008=CARTESIAN_POINT('Ctrl Pts',(4.28490662509514,-6.41905264174572,
95.4519124409768));
#185009=CARTESIAN_POINT('Ctrl Pts',(6.88866860112665,-2.37186857879187,
95.6634690613587));
#185010=CARTESIAN_POINT('Ctrl Pts',(7.32848383063589,2.42047858723411,95.8750256817408));
#185011=CARTESIAN_POINT('Ctrl Pts',(4.10468304959734,6.54456291005869,96.0865823021226));
#185012=CARTESIAN_POINT('Ctrl Pts',(-0.679028220406464,7.25757857856497,
96.2981389225044));
#185013=CARTESIAN_POINT('Ctrl Pts',(-4.05427435445187,6.07236054551145,
96.4568063877909));
#185014=CARTESIAN_POINT('Ctrl Pts',(-6.47127337767883,3.38407271816423,
96.6154738530771));
#185015=CARTESIAN_POINT('Ctrl Pts',(-7.29616857577915,-0.117923577904248,
96.7741413183638));
#185016=CARTESIAN_POINT('Ctrl Pts',(-6.35800508006628,-3.58921836875169,
96.9328087836501));
#185017=CARTESIAN_POINT('Ctrl Pts',(-3.85933553387998,-6.20169133701876,
97.0914762489367));
#185018=CARTESIAN_POINT('Ctrl Pts',(-0.440438479635075,-7.27223127969294,
97.2501437142229));
#185019=CARTESIAN_POINT('Ctrl Pts',(4.30252989486086,-6.41644447484644,
97.461700334605));
#185020=CARTESIAN_POINT('Ctrl Pts',(8.19966432523079,-1.11131240077915,
97.7261461100822));
#185021=CARTESIAN_POINT('Ctrl Pts',(5.85497146417381,5.04026049610663,97.9905918855599));
#185022=CARTESIAN_POINT('Ctrl Pts',(1.51099084548737,7.12682197675247,98.2021485059416));
#185023=CARTESIAN_POINT('Ctrl Pts',(-2.06992536476643,7.0058668122941,98.3608159712281));
#185024=CARTESIAN_POINT('Ctrl Pts',(-5.17287422036002,5.15049374409499,
98.5194834365144));
#185025=CARTESIAN_POINT('Ctrl Pts',(-7.00278762888398,2.05811838864922,
98.6781509018009));
#185026=CARTESIAN_POINT('Ctrl Pts',(-7.13636830945152,-1.54513735705454,
98.8368339328175));
#185027=CARTESIAN_POINT('Ctrl Pts',(-6.06394139514141,-3.69210156778035,
98.9426278087385));
#185028=CARTESIAN_POINT('Ctrl Pts',(-5.30378086654358,-4.57361536730065,
98.9955325295642));
#185029=CARTESIAN_POINT('Ctrl Pts',(2.10208451021625,-7.84862588447231,
-3.290770433928E-15));
#185030=CARTESIAN_POINT('Ctrl Pts',(2.29962771051048,-7.78108676365297,
-5.16703836131539E-15));
#185031=CARTESIAN_POINT('Ctrl Pts',(2.49411343411202,-7.70593369986541,
-3.15384150650199E-16));
#185032=CARTESIAN_POINT('Ctrl Pts',(2.68517636753987,-7.62347406731538,
-1.58206781009085E-15));
#185033=CARTESIAN_POINT('Ctrl Pts',(2.88113552763045,-7.53890130353552,
-2.88121182275299E-15));
#185034=CARTESIAN_POINT('Ctrl Pts',(3.07349491021749,-7.44664244674981,
-5.00442052337E-15));
#185035=CARTESIAN_POINT('Ctrl Pts',(3.26183706294806,-7.3469783482138,-5.12090370108353E-15));
#185036=CARTESIAN_POINT('Ctrl Pts',(3.44701891521803,-7.24898657046175,
-5.23543234108555E-15));
#185037=CARTESIAN_POINT('Ctrl Pts',(3.62831770409081,-7.14383543019674,
-3.83143952960435E-15));
#185038=CARTESIAN_POINT('Ctrl Pts',(3.80530588214224,-7.03174992031122,
-3.38618022510673E-15));
#185039=CARTESIAN_POINT('Ctrl Pts',(3.98682476188306,-6.91679514528841,
-2.92952277466898E-15));
#185040=CARTESIAN_POINT('Ctrl Pts',(4.16381029498468,-6.79454614842656,
-2.24677972717022E-15));
#185041=CARTESIAN_POINT('Ctrl Pts',(4.33575872179093,-6.66520704214514,
-3.27515792264421E-15));
#185042=CARTESIAN_POINT('Ctrl Pts',(4.42173293519406,-6.60053748900443,
-3.78934702038121E-15));
#185043=CARTESIAN_POINT('Ctrl Pts',(4.50644714130402,-6.53409484017392,
-2.34365924677727E-15));
#185044=CARTESIAN_POINT('Ctrl Pts',(4.58983358603305,-6.46590148664305,
-2.80331313717852E-15));
#185045=CARTESIAN_POINT('Ctrl Pts',(4.63152680839756,-6.43180480987762,
-3.03314008237915E-15));
#185046=CARTESIAN_POINT('Ctrl Pts',(4.67288803734242,-6.3972704267277,2.90312324695387E-16));
#185047=CARTESIAN_POINT('Ctrl Pts',(4.71390847258368,-6.36230096370932,
-1.38777878078145E-16));
#185048=CARTESIAN_POINT('Ctrl Pts',(4.73461573528928,-6.34464825346536,
-3.55384150073381E-16));
#185049=CARTESIAN_POINT('Ctrl Pts',(4.75523615107994,-6.32688467152668,
1.18624335832746E-15));
#185050=CARTESIAN_POINT('Ctrl Pts',(4.77576856551071,-6.30901054537397,
7.49400541621981E-16));
#185051=CARTESIAN_POINT('Ctrl Pts',(4.79591021739563,-6.29147659056661,
3.20871496867989E-16));
#185052=CARTESIAN_POINT('Ctrl Pts',(4.81596202834693,-6.27384070654854,
1.48999836866843E-15));
#185053=CARTESIAN_POINT('Ctrl Pts',(4.83591612347545,-6.25610961852038,
1.33226762955019E-15));
#185054=CARTESIAN_POINT('Ctrl Pts',(4.98978344512459,-6.11938404879417,
-1.0694073052437E-16));
#185055=CARTESIAN_POINT('Ctrl Pts',(5.13797274440312,-5.97688834344088,
-6.37152335888765E-16));
#185056=CARTESIAN_POINT('Ctrl Pts',(5.28010241489011,-5.82886074576049,
3.13638004456607E-15));
#185057=CARTESIAN_POINT('Ctrl Pts',(5.32388371551095,-5.78326266105362,
5.08932056714925E-15));
#185058=CARTESIAN_POINT('Ctrl Pts',(5.36708977798512,-5.73713940061267,
3.61201614627145E-15));
#185059=CARTESIAN_POINT('Ctrl Pts',(5.40970872589629,-5.69049723734325,
2.96984659087229E-15));
#185060=CARTESIAN_POINT('Ctrl Pts',(5.54848269366366,-5.53862305040551,
1.23002056944179E-15));
#185061=CARTESIAN_POINT('Ctrl Pts',(5.68103508731973,-5.38124932257935,
1.45242263650514E-15));
#185062=CARTESIAN_POINT('Ctrl Pts',(5.80714429668145,-5.21882934647248,
1.88737914186277E-15));
#185063=CARTESIAN_POINT('Ctrl Pts',(5.93327032734641,-5.05638770568561,
4.98380169643257E-15));
#185064=CARTESIAN_POINT('Ctrl Pts',(6.05295174788962,-4.88889779050302,
3.62171887105232E-16));
#185065=CARTESIAN_POINT('Ctrl Pts',(6.16592022815171,-4.71679013773437,
1.30451205393456E-15));
#185066=CARTESIAN_POINT('Ctrl Pts',(6.27792279739088,-4.5461540518891,3.75006097235274E-15));
#185067=CARTESIAN_POINT('Ctrl Pts',(6.38332694768264,-4.37097818866154,
-2.53100327216846E-15));
#185068=CARTESIAN_POINT('Ctrl Pts',(6.48182164283881,-4.19166967163302,
-2.4980018054066E-15));
#185069=CARTESIAN_POINT('Ctrl Pts',(6.52326227113616,-4.11622746032462,
-3.45241306837116E-15));
#185070=CARTESIAN_POINT('Ctrl Pts',(6.56347915093949,-4.04005358422469,
-2.64250873965109E-15));
#185071=CARTESIAN_POINT('Ctrl Pts',(6.60244631812086,-3.96317813022292,
-8.32667268468867E-16));
#185072=CARTESIAN_POINT('Ctrl Pts',(6.61905364025482,-3.9304147675987,9.32549959876183E-17));
#185073=CARTESIAN_POINT('Ctrl Pts',(6.63543635568491,-3.89751882078441,
-2.52119858109353E-16));
#185074=CARTESIAN_POINT('Ctrl Pts',(6.65157567526072,-3.86452741946229,
-7.7715611723761E-16));
#185075=CARTESIAN_POINT('Ctrl Pts',(6.74048447841371,-3.68278332596983,
-3.66949276078462E-15));
#185076=CARTESIAN_POINT('Ctrl Pts',(6.82211074143566,-3.49795239268472,
-5.08282477872157E-15));
#185077=CARTESIAN_POINT('Ctrl Pts',(6.89625206046576,-3.31046675549432,
-4.88498130835069E-15));
#185078=CARTESIAN_POINT('Ctrl Pts',(6.9699232370716,-3.12416999588444,-4.68839239630173E-15));
#185079=CARTESIAN_POINT('Ctrl Pts',(7.03620429877872,-2.93525142177202,
-7.13421723312083E-15));
#185080=CARTESIAN_POINT('Ctrl Pts',(7.09484826120896,-2.74411884411799,
-5.49560397189452E-15));
#185081=CARTESIAN_POINT('Ctrl Pts',(7.13726862362652,-2.60586227212168,
-4.31030602266199E-15));
#185082=CARTESIAN_POINT('Ctrl Pts',(7.17569194887325,-2.46644687839578,
-7.62442829405664E-15));
#185083=CARTESIAN_POINT('Ctrl Pts',(7.21000787802524,-2.32602464360175,
-9.10382880192628E-15));
#185084=CARTESIAN_POINT('Ctrl Pts',(7.25913415483096,-2.12499783923887,
-1.13420163587531E-14));
#185085=CARTESIAN_POINT('Ctrl Pts',(7.29984486455965,-1.92190694651327,
-8.44330237013337E-15));
#185086=CARTESIAN_POINT('Ctrl Pts',(7.33208917201402,-1.71725913517378,
-9.43689570931383E-15));
#185087=CARTESIAN_POINT('Ctrl Pts',(7.36433347946838,-1.51261132383428,
-1.04304890484943E-14));
#185088=CARTESIAN_POINT('Ctrl Pts',(7.38811133250517,-1.30640578628499,
-2.38941095831012E-14));
#185089=CARTESIAN_POINT('Ctrl Pts',(7.40331446894898,-1.09916311536333,
-1.06026298851702E-14));
#185090=CARTESIAN_POINT('Ctrl Pts',(7.40617088924807,-1.06022561228647,
-9.55573486110841E-15));
#185091=CARTESIAN_POINT('Ctrl Pts',(7.40872267048525,-1.0212752751884,-1.0646464482034E-14));
#185092=CARTESIAN_POINT('Ctrl Pts',(7.41096959872409,-0.982324841880129,
-1.04360964314765E-14));
#185093=CARTESIAN_POINT('Ctrl Pts',(7.42235430710878,-0.784971265113983,
-9.37020617843963E-15));
#185094=CARTESIAN_POINT('Ctrl Pts',(7.42592266440482,-0.587537835352548,
-1.293591650313E-14));
#185095=CARTESIAN_POINT('Ctrl Pts',(7.42170473423292,-0.390466204597829,
-1.06026298851702E-14));
#185096=CARTESIAN_POINT('Ctrl Pts',(7.41749426002231,-0.193742933913072,
-8.27346777709736E-15));
#185097=CARTESIAN_POINT('Ctrl Pts',(7.40552490615871,0.00262049832885516,
-6.9361844842518E-15));
#185098=CARTESIAN_POINT('Ctrl Pts',(7.3857749724574,0.198180275996753,-7.7715611723761E-15));
#185099=CARTESIAN_POINT('Ctrl Pts',(7.36615089037624,0.3924938968305,-8.60161462695303E-15));
#185100=CARTESIAN_POINT('Ctrl Pts',(7.33884495154307,0.586014712140499,
-6.51498341349402E-15));
#185101=CARTESIAN_POINT('Ctrl Pts',(7.3037865412977,0.778293044380834,-5.38458166943201E-15));
#185102=CARTESIAN_POINT('Ctrl Pts',(7.26872813105233,0.97057137662117,-4.25417992536999E-15));
#185103=CARTESIAN_POINT('Ctrl Pts',(7.22591719058655,1.16160786872303,-3.07562274669201E-15));
#185104=CARTESIAN_POINT('Ctrl Pts',(7.17523488235407,1.35092889849934,-3.49720252756924E-15));
#185105=CARTESIAN_POINT('Ctrl Pts',(7.15288410775808,1.43441901192123,-2.89610734490173E-15));
#185106=CARTESIAN_POINT('Ctrl Pts',(7.12900186354509,1.51757513502465,-7.5026934907553E-15));
#185107=CARTESIAN_POINT('Ctrl Pts',(7.10360232537748,1.60035343100048,-3.33066907387547E-15));
#185108=CARTESIAN_POINT('Ctrl Pts',(7.09112003500542,1.64103380558275,-1.28037903052207E-15));
#185109=CARTESIAN_POINT('Ctrl Pts',(7.07827076461064,1.68162450295897,-1.8855884437478E-15));
#185110=CARTESIAN_POINT('Ctrl Pts',(7.06505739175309,1.72211611694885,-4.44089209850063E-16));
#185111=CARTESIAN_POINT('Ctrl Pts',(7.0544290607665,1.7546860202056,7.15397557075437E-16));
#185112=CARTESIAN_POINT('Ctrl Pts',(7.04356771062853,1.78718385328651,1.24968543471361E-16));
#185113=CARTESIAN_POINT('Ctrl Pts',(7.0324785567182,1.8195956752456,3.33066907387547E-16));
#185114=CARTESIAN_POINT('Ctrl Pts',(6.96943089491119,2.00387389935086,1.51621535828537E-15));
#185115=CARTESIAN_POINT('Ctrl Pts',(6.89898792830898,2.1854825028391,1.33828956628801E-15));
#185116=CARTESIAN_POINT('Ctrl Pts',(6.82139528078071,2.36395748737489,1.4432899320127E-15));
#185117=CARTESIAN_POINT('Ctrl Pts',(6.74433218910303,2.54121441227158,1.54757368914425E-15));
#185118=CARTESIAN_POINT('Ctrl Pts',(6.66021621392354,2.71538095692703,1.6559467280731E-15));
#185119=CARTESIAN_POINT('Ctrl Pts',(6.56924627918247,2.88597335464335,1.77635683940025E-15));
#185120=CARTESIAN_POINT('Ctrl Pts',(6.50266459558114,3.01083140892107,1.86448604337962E-15));
#185121=CARTESIAN_POINT('Ctrl Pts',(6.43241042807166,3.13377426257987,2.03877470991558E-15));
#185122=CARTESIAN_POINT('Ctrl Pts',(6.3585495483742,3.25459937292915,0.));
#185123=CARTESIAN_POINT('Ctrl Pts',(6.34340397157949,3.27937522172788,-7.56577460625889E-16));
#185124=CARTESIAN_POINT('Ctrl Pts',(6.32810731413255,3.30406089503788,2.43515525521077E-15));
#185125=CARTESIAN_POINT('Ctrl Pts',(6.31266697535328,3.32864399987372,1.77635683940025E-15));
#185126=CARTESIAN_POINT('Ctrl Pts',(6.21101507324467,3.49048755797315,1.06570322610702E-15));
#185127=CARTESIAN_POINT('Ctrl Pts',(6.10306202439148,3.64801466098077,-3.81869933772724E-15));
#185128=CARTESIAN_POINT('Ctrl Pts',(5.98901561316641,3.80076293866515,-2.77555756156289E-15));
#185129=CARTESIAN_POINT('Ctrl Pts',(5.8769084671812,3.95091385776383,-1.13531658097703E-15));
#185130=CARTESIAN_POINT('Ctrl Pts',(5.75891294518698,4.09644756264395,-7.79843788104419E-16));
#185131=CARTESIAN_POINT('Ctrl Pts',(5.63519336749352,4.23688737897504,1.77635683940025E-15));
#185132=CARTESIAN_POINT('Ctrl Pts',(5.57235559782876,4.30821743841185,-1.38140305958728E-15));
#185133=CARTESIAN_POINT('Ctrl Pts',(5.50804072164468,4.37823279464964,-1.50833598234392E-15));
#185134=CARTESIAN_POINT('Ctrl Pts',(5.44226749982665,4.44686660289082,-6.66133814775094E-16));
#185135=CARTESIAN_POINT('Ctrl Pts',(5.39900343271652,4.49201229598133,-4.7094403649886E-16));
#185136=CARTESIAN_POINT('Ctrl Pts',(5.35510834142393,4.53656016442929,-5.35226817025197E-16));
#185137=CARTESIAN_POINT('Ctrl Pts',(5.31059519289858,4.58050191706158,-5.55111512312578E-16));
#185138=CARTESIAN_POINT('Origin',(0.,0.,100.));
#185139=CARTESIAN_POINT('',(-4.,4.89858719658941E-16,100.));
#185140=CARTESIAN_POINT('Origin',(0.,0.,100.));
#185141=CARTESIAN_POINT('Origin',(0.,0.,0.));
#185142=CARTESIAN_POINT('',(-4.,-4.89858719658941E-16,0.));
#185143=CARTESIAN_POINT('Origin',(0.,0.,0.));
#185144=CARTESIAN_POINT('Origin',(0.,0.,0.));
#185145=CARTESIAN_POINT('Origin',(0.,0.,0.));
#185146=CARTESIAN_POINT('',(0.,0.,0.));
#185147=CARTESIAN_POINT('Origin',(7.,0.,120.));
#185148=CARTESIAN_POINT('',(-7.,-8.57252759403147E-16,120.));
#185149=CARTESIAN_POINT('Origin',(0.,0.,120.));
#185150=CARTESIAN_POINT('Origin',(0.,0.,140.));
#185151=CARTESIAN_POINT('',(-10.,-1.22464679914735E-15,160.));
#185152=CARTESIAN_POINT('Origin',(0.,0.,160.));
#185153=CARTESIAN_POINT('',(-8.5,-1.04094977927525E-15,140.));
#185154=CARTESIAN_POINT('Origin',(13.,0.,160.));
#185155=CARTESIAN_POINT('',(-13.,-1.59204083889156E-15,160.));
#185156=CARTESIAN_POINT('Origin',(0.,0.,160.));
#185157=CARTESIAN_POINT('Origin',(0.,0.,163.));
#185158=CARTESIAN_POINT('',(-13.,-1.59204083889156E-15,166.));
#185159=CARTESIAN_POINT('Origin',(0.,0.,166.));
#185160=CARTESIAN_POINT('',(-13.,-1.59204083889156E-15,163.));
#185161=CARTESIAN_POINT('Origin',(0.,0.,166.));
#185162=CARTESIAN_POINT('',(0.,0.,196.));
#185163=CARTESIAN_POINT('',(-13.,1.59204083889156E-15,166.));
#185164=CARTESIAN_POINT('',(0.,0.,0.));
#185165=CARTESIAN_POINT('Origin',(80.,-9.,143.));
#185166=CARTESIAN_POINT('',(77.5,-9.,146.));
#185167=CARTESIAN_POINT('Origin',(80.,-9.,146.));
#185168=CARTESIAN_POINT('',(77.5,-9.,140.));
#185169=CARTESIAN_POINT('',(77.5,-9.,143.));
#185170=CARTESIAN_POINT('Origin',(80.,-9.,140.));
#185171=CARTESIAN_POINT('Origin',(80.,9.,143.));
#185172=CARTESIAN_POINT('',(77.5,9.,146.));
#185173=CARTESIAN_POINT('Origin',(80.,9.,146.));
#185174=CARTESIAN_POINT('',(77.5,9.,140.));
#185175=CARTESIAN_POINT('',(77.5,9.,143.));
#185176=CARTESIAN_POINT('Origin',(80.,9.,140.));
#185177=CARTESIAN_POINT('Origin',(80.,0.,140.));
#185178=CARTESIAN_POINT('',(60.,12.,140.));
#185179=CARTESIAN_POINT('',(60.,-12.,140.));
#185180=CARTESIAN_POINT('',(60.,12.,140.));
#185181=CARTESIAN_POINT('',(100.,12.,140.));
#185182=CARTESIAN_POINT('',(100.,12.,140.));
#185183=CARTESIAN_POINT('',(100.,-12.,140.));
#185184=CARTESIAN_POINT('',(100.,-12.,140.));
#185185=CARTESIAN_POINT('',(60.,-12.,140.));
#185186=CARTESIAN_POINT('',(90.,4.,140.));
#185187=CARTESIAN_POINT('',(70.,4.,140.));
#185188=CARTESIAN_POINT('',(90.,4.,140.));
#185189=CARTESIAN_POINT('',(70.,-4.,140.));
#185190=CARTESIAN_POINT('',(70.,4.,140.));
#185191=CARTESIAN_POINT('',(90.,-4.,140.));
#185192=CARTESIAN_POINT('',(70.,-4.,140.));
#185193=CARTESIAN_POINT('',(90.,-4.,140.));
#185194=CARTESIAN_POINT('Origin',(100.,12.,140.));
#185195=CARTESIAN_POINT('',(60.,12.,146.));
#185196=CARTESIAN_POINT('',(60.,12.,140.));
#185197=CARTESIAN_POINT('',(100.,12.,146.));
#185198=CARTESIAN_POINT('',(100.,12.,146.));
#185199=CARTESIAN_POINT('',(100.,12.,140.));
#185200=CARTESIAN_POINT('Origin',(100.,-12.,140.));
#185201=CARTESIAN_POINT('',(100.,-12.,146.));
#185202=CARTESIAN_POINT('',(100.,-12.,146.));
#185203=CARTESIAN_POINT('',(100.,-12.,140.));
#185204=CARTESIAN_POINT('Origin',(60.,-12.,140.));
#185205=CARTESIAN_POINT('',(60.,-12.,146.));
#185206=CARTESIAN_POINT('',(60.,-12.,146.));
#185207=CARTESIAN_POINT('',(60.,-12.,140.));
#185208=CARTESIAN_POINT('Origin',(60.,12.,140.));
#185209=CARTESIAN_POINT('',(60.,12.,146.));
#185210=CARTESIAN_POINT('Origin',(80.,0.,146.));
#185211=CARTESIAN_POINT('Origin',(90.,4.,106.));
#185212=CARTESIAN_POINT('',(90.,4.,106.));
#185213=CARTESIAN_POINT('',(70.,4.,106.));
#185214=CARTESIAN_POINT('',(90.,4.,106.));
#185215=CARTESIAN_POINT('',(70.,4.,106.));
#185216=CARTESIAN_POINT('',(90.,4.,106.));
#185217=CARTESIAN_POINT('Origin',(90.,-4.,106.));
#185218=CARTESIAN_POINT('',(90.,-4.,106.));
#185219=CARTESIAN_POINT('',(90.,-4.,106.));
#185220=CARTESIAN_POINT('',(90.,-4.,106.));
#185221=CARTESIAN_POINT('Origin',(70.,-4.,106.));
#185222=CARTESIAN_POINT('',(70.,-4.,106.));
#185223=CARTESIAN_POINT('',(70.,-4.,106.));
#185224=CARTESIAN_POINT('',(70.,-4.,106.));
#185225=CARTESIAN_POINT('Origin',(70.,4.,106.));
#185226=CARTESIAN_POINT('',(70.,4.,106.));
#185227=CARTESIAN_POINT('Origin',(80.,0.,106.));
#185228=CARTESIAN_POINT('',(0.,0.,0.));
#185229=CARTESIAN_POINT('Origin',(-40.,-40.,12.));
#185230=CARTESIAN_POINT('',(-40.,-40.,12.));
#185231=CARTESIAN_POINT('',(40.,-40.,12.));
#185232=CARTESIAN_POINT('',(-20.,-40.,12.));
#185233=CARTESIAN_POINT('',(-40.,-40.,0.));
#185234=CARTESIAN_POINT('',(-40.,-40.,6.));
#185235=CARTESIAN_POINT('',(40.,-40.,0.));
#185236=CARTESIAN_POINT('',(-20.,-40.,0.));
#185237=CARTESIAN_POINT('',(40.,-40.,6.));
#185238=CARTESIAN_POINT('Origin',(40.,-50.,0.));
#185239=CARTESIAN_POINT('',(40.,50.,0.));
#185240=CARTESIAN_POINT('',(40.,-50.,0.));
#185241=CARTESIAN_POINT('',(40.,50.,12.));
#185242=CARTESIAN_POINT('',(40.,50.,0.));
#185243=CARTESIAN_POINT('',(40.,-50.,12.));
#185244=CARTESIAN_POINT('Origin',(0.,0.,0.));
#185245=CARTESIAN_POINT('',(-40.,50.,0.));
#185246=CARTESIAN_POINT('',(-40.,50.,0.));
#185247=CARTESIAN_POINT('',(40.,50.,0.));
#185248=CARTESIAN_POINT('',(27.5,-35.,0.));
#185249=CARTESIAN_POINT('Origin',(30.,-35.,0.));
#185250=CARTESIAN_POINT('',(-32.5,-35.,0.));
#185251=CARTESIAN_POINT('Origin',(-30.,-35.,0.));
#185252=CARTESIAN_POINT('',(-32.5,35.,0.));
#185253=CARTESIAN_POINT('Origin',(-30.,35.,0.));
#185254=CARTESIAN_POINT('',(27.5,35.,0.));
#185255=CARTESIAN_POINT('Origin',(30.,35.,0.));
#185256=CARTESIAN_POINT('',(-7.,8.57252759403147E-16,0.));
#185257=CARTESIAN_POINT('Origin',(0.,0.,0.));
#185258=CARTESIAN_POINT('Origin',(30.,-35.,6.));
#185259=CARTESIAN_POINT('',(27.5,-35.,12.));
#185260=CARTESIAN_POINT('Origin',(30.,-35.,12.));
#185261=CARTESIAN_POINT('',(27.5,-35.,6.));
#185262=CARTESIAN_POINT('Origin',(-30.,-35.,6.));
#185263=CARTESIAN_POINT('',(-32.5,-35.,12.));
#185264=CARTESIAN_POINT('Origin',(-30.,-35.,12.));
#185265=CARTESIAN_POINT('',(-32.5,-35.,6.));
#185266=CARTESIAN_POINT('Origin',(-30.,35.,6.));
#185267=CARTESIAN_POINT('',(-32.5,35.,12.));
#185268=CARTESIAN_POINT('Origin',(-30.,35.,12.));
#185269=CARTESIAN_POINT('',(-32.5,35.,6.));
#185270=CARTESIAN_POINT('Origin',(30.,35.,6.));
#185271=CARTESIAN_POINT('',(27.5,35.,12.));
#185272=CARTESIAN_POINT('Origin',(30.,35.,12.));
#185273=CARTESIAN_POINT('',(27.5,35.,6.));
#185274=CARTESIAN_POINT('Origin',(0.,0.,6.));
#185275=CARTESIAN_POINT('',(-7.,8.57252759403147E-16,12.));
#185276=CARTESIAN_POINT('Origin',(0.,0.,12.));
#185277=CARTESIAN_POINT('',(-7.,8.57252759403147E-16,6.));
#185278=CARTESIAN_POINT('Origin',(40.,50.,0.));
#185279=CARTESIAN_POINT('',(-40.,50.,12.));
#185280=CARTESIAN_POINT('',(-40.,50.,0.));
#185281=CARTESIAN_POINT('',(40.,50.,12.));
#185282=CARTESIAN_POINT('Origin',(-40.,50.,0.));
#185283=CARTESIAN_POINT('',(-40.,50.,12.));
#185284=CARTESIAN_POINT('Origin',(0.,0.,12.));
#185285=CARTESIAN_POINT('',(0.,0.,0.));
#185286=CARTESIAN_POINT('Origin',(0.,0.,0.));
#185287=CARTESIAN_POINT('',(-6.,-7.34788079488412E-16,0.));
#185288=CARTESIAN_POINT('Origin',(0.,0.,0.));
#185289=CARTESIAN_POINT('',(-6.,-7.34788079488412E-16,12.));
#185290=CARTESIAN_POINT('',(-6.,-7.34788079488412E-16,0.));
#185291=CARTESIAN_POINT('Origin',(0.,0.,12.));
#185292=CARTESIAN_POINT('Origin',(0.,0.,0.));
#185293=CARTESIAN_POINT('',(-7.,-8.57252759403147E-16,12.));
#185294=CARTESIAN_POINT('Origin',(0.,0.,12.));
#185295=CARTESIAN_POINT('',(-7.,-8.57252759403147E-16,0.));
#185296=CARTESIAN_POINT('',(-7.,-8.57252759403147E-16,0.));
#185297=CARTESIAN_POINT('Origin',(0.,0.,0.));
#185298=CARTESIAN_POINT('Origin',(0.,0.,12.));
#185299=CARTESIAN_POINT('Origin',(0.,0.,0.));
#185300=CARTESIAN_POINT('',(0.,0.,0.));
#185301=CARTESIAN_POINT('Origin',(0.,0.,4.30282021618968));
#185302=CARTESIAN_POINT('',(3.09910619832133,6.0156321173694,9.04578901356831));
#185303=CARTESIAN_POINT('',(3.09910619832133,6.0156321173694,8.6514415183394));
#185304=CARTESIAN_POINT('',(3.09910619832133,6.0156321173694,4.30282021618968));
#185305=CARTESIAN_POINT('',(-3.92879376257849,-5.50970675908658,8.00008340518918));
#185306=CARTESIAN_POINT('Ctrl Pts',(-3.92879376257849,-5.50970675908658,
8.00008340518918));
#185307=CARTESIAN_POINT('Ctrl Pts',(-3.78617121598613,-5.61140628611332,
8.00834306925214));
#185308=CARTESIAN_POINT('Ctrl Pts',(-3.63945998519003,-5.7076623902655,
8.01660273331509));
#185309=CARTESIAN_POINT('Ctrl Pts',(-3.48911231632171,-5.79813627332889,
8.02486239737804));
#185310=CARTESIAN_POINT('Ctrl Pts',(-3.33888110786677,-5.88854007465504,
8.03311566344428));
#185311=CARTESIAN_POINT('Ctrl Pts',(-3.18501937441404,-5.97317039562586,
8.04136892951052));
#185312=CARTESIAN_POINT('Ctrl Pts',(-3.02800917015506,-6.05173111311606,
8.04962219557676));
#185313=CARTESIAN_POINT('Ctrl Pts',(-2.87109023696789,-6.13024616274076,
8.05787066396477));
#185314=CARTESIAN_POINT('Ctrl Pts',(-2.71102679497344,-6.20269848060912,
8.06611913235277));
#185315=CARTESIAN_POINT('Ctrl Pts',(-2.54832651194958,-6.26883729159522,
8.07436760074078));
#185316=CARTESIAN_POINT('Ctrl Pts',(-2.38568936503828,-6.33495043730688,
8.08261286829705));
#185317=CARTESIAN_POINT('Ctrl Pts',(-2.22041774337426,-6.39475482519885,
8.09085813585333));
#185318=CARTESIAN_POINT('Ctrl Pts',(-2.05304049370703,-6.44804728047176,
8.0991034034096));
#185319=CARTESIAN_POINT('Ctrl Pts',(-1.88566464369749,-6.50133929009751,
8.10734860201653));
#185320=CARTESIAN_POINT('Ctrl Pts',(-1.71618353484674,-6.54811935906065,
8.11559380062346));
#185321=CARTESIAN_POINT('Ctrl Pts',(-1.54514286689777,-6.58823364194645,
8.12383899923038));
#185322=CARTESIAN_POINT('Ctrl Pts',(-1.37409597703566,-6.62834938406172,
8.1320844977713));
#185323=CARTESIAN_POINT('Ctrl Pts',(-1.20148975947593,-6.6617987752453,
8.14032999631221));
#185324=CARTESIAN_POINT('Ctrl Pts',(-1.02788174576766,-6.68847875953252,
8.14857549485312));
#185325=CARTESIAN_POINT('Ctrl Pts',(-0.854237005138767,-6.71516438799274,
8.15682273773616));
#185326=CARTESIAN_POINT('Ctrl Pts',(-0.679590395912993,-6.73507770216261,
8.16506998061919));
#185327=CARTESIAN_POINT('Ctrl Pts',(-0.504506353298766,-6.74816733191177,
8.17331722350222));
#185328=CARTESIAN_POINT('Ctrl Pts',(-0.329354600483387,-6.76126202380966,
8.18156765583911));
#185329=CARTESIAN_POINT('Ctrl Pts',(-0.153765429952902,-6.76752774692309,
8.189818088176));
#185330=CARTESIAN_POINT('Ctrl Pts',(0.0216948116684557,-6.76696522343263,
8.19806852051288));
#185331=CARTESIAN_POINT('Ctrl Pts',(0.19735801950094,-6.76640204923487,
8.20632849665853));
#185332=CARTESIAN_POINT('Ctrl Pts',(0.37289164614926,-6.75899484888137,
8.21458847280418));
#185333=CARTESIAN_POINT('Ctrl Pts',(0.547731437659107,-6.74479645891556,
8.22284844894983));
#185334=CARTESIAN_POINT('Ctrl Pts',(0.722677486175284,-6.73058944003067,
8.23111344500731));
#185335=CARTESIAN_POINT('Ctrl Pts',(0.896928507983267,-6.70958304496605,
8.23937844106479));
#185336=CARTESIAN_POINT('Ctrl Pts',(1.06992855532672,-6.6818816127268,8.24764343712227));
#185337=CARTESIAN_POINT('Ctrl Pts',(1.24319209235441,-6.65413798950699,
8.25592102127574));
#185338=CARTESIAN_POINT('Ctrl Pts',(1.41520050044158,-6.61967902065648,
8.2641986054292));
#185339=CARTESIAN_POINT('Ctrl Pts',(1.5854098301569,-6.57865979287893,8.27247618958267));
#185340=CARTESIAN_POINT('Ctrl Pts',(1.72771248155696,-6.54436587443809,
8.27939662205364));
#185341=CARTESIAN_POINT('Ctrl Pts',(1.86875779235141,-6.50548745357604,
8.28631705452462));
#185342=CARTESIAN_POINT('Ctrl Pts',(2.00823823124676,-6.4621411472173,8.2932374869956));
#185343=CARTESIAN_POINT('Ctrl Pts',(2.1705257283394,-6.41170709622862,8.30128950972658));
#185344=CARTESIAN_POINT('Ctrl Pts',(2.33121798580858,-6.3550604691712,8.30934153245757));
#185345=CARTESIAN_POINT('Ctrl Pts',(2.48978960024624,-6.29231569030875,
8.31739355518856));
#185346=CARTESIAN_POINT('Ctrl Pts',(2.6481615005552,-6.22964993579682,8.32543543674321));
#185347=CARTESIAN_POINT('Ctrl Pts',(2.80441772782733,-6.16090144600992,
8.33347731829786));
#185348=CARTESIAN_POINT('Ctrl Pts',(2.95804508144256,-6.086235149594,8.34151919985251));
#185349=CARTESIAN_POINT('Ctrl Pts',(3.11151292919324,-6.01164637656101,
8.34955273180509));
#185350=CARTESIAN_POINT('Ctrl Pts',(3.26235700045555,-5.93115218531975,
8.35758626375767));
#185351=CARTESIAN_POINT('Ctrl Pts',(3.41008134960162,-5.84496656868961,
8.36561979571025));
#185352=CARTESIAN_POINT('Ctrl Pts',(3.55768493839698,-5.7588514062896,8.37364676048455));
#185353=CARTESIAN_POINT('Ctrl Pts',(3.70217355859849,-5.66705426565699,
8.38167372525886));
#185354=CARTESIAN_POINT('Ctrl Pts',(3.84307339962506,-5.56983624939678,
8.38970069003316));
#185355=CARTESIAN_POINT('Ctrl Pts',(3.98388912949794,-5.47267626811692,
8.39772286305424));
#185356=CARTESIAN_POINT('Ctrl Pts',(4.12112003699627,-5.37010206484599,
8.40574503607532));
#185357=CARTESIAN_POINT('Ctrl Pts',(4.25431910137204,-5.26241940401001,
8.4137672090964));
#185358=CARTESIAN_POINT('Ctrl Pts',(4.39087135540917,-5.1520259104312,8.42199133449427));
#185359=CARTESIAN_POINT('Ctrl Pts',(4.52318574229823,-5.03626356696928,
8.43021545989213));
#185360=CARTESIAN_POINT('Ctrl Pts',(4.65081416021784,-4.91550777103619,
8.43843958528999));
#185361=CARTESIAN_POINT('Ctrl Pts',(4.77526750401165,-4.79775607567458,
8.4464591151269));
#185362=CARTESIAN_POINT('Ctrl Pts',(4.89526499102733,-4.67525671345183,
8.45447864496381));
#185363=CARTESIAN_POINT('Ctrl Pts',(5.01042671483032,-4.5483967653795,8.46249817480072));
#185364=CARTESIAN_POINT('Ctrl Pts',(5.12560049249289,-4.42152353900644,
8.47051854403359));
#185365=CARTESIAN_POINT('Ctrl Pts',(5.23593724688707,-4.29028909578871,
8.47853891326647));
#185366=CARTESIAN_POINT('Ctrl Pts',(5.34109607102384,-4.15511513199017,
8.48655928249934));
#185367=CARTESIAN_POINT('Ctrl Pts',(5.44628688845443,-4.01990004315647,
8.49458209183206));
#185368=CARTESIAN_POINT('Ctrl Pts',(5.54629640999215,-3.8807433442112,8.50260490116477));
#185369=CARTESIAN_POINT('Ctrl Pts',(5.64082603077095,-3.73809720186311,
8.51062771049748));
#185370=CARTESIAN_POINT('Ctrl Pts',(5.73952354912554,-3.5891616604252,8.51900425284312));
#185371=CARTESIAN_POINT('Ctrl Pts',(5.83224671071703,-3.43642236636971,
8.52738079518875));
#185372=CARTESIAN_POINT('Ctrl Pts',(5.91870864162228,-3.28042329823238,
8.53575733753439));
#185373=CARTESIAN_POINT('Ctrl Pts',(6.00166713683383,-3.1307453091847,8.54379446255339));
#185374=CARTESIAN_POINT('Ctrl Pts',(6.07886173514008,-2.97806688554535,
8.5518315875724));
#185375=CARTESIAN_POINT('Ctrl Pts',(6.15008830340139,-2.82288909813429,
8.5598687125914));
#185376=CARTESIAN_POINT('Ctrl Pts',(6.22136913836607,-2.66759308255128,
8.56791196100354));
#185377=CARTESIAN_POINT('Ctrl Pts',(6.28667274832479,-2.50979425618822,
8.57595520941568));
#185378=CARTESIAN_POINT('Ctrl Pts',(6.3458446220462,-2.35000958143735,8.58399845782782));
#185379=CARTESIAN_POINT('Ctrl Pts',(6.4051010791394,-2.18999650211348,8.59205320368002));
#185380=CARTESIAN_POINT('Ctrl Pts',(6.45820819723198,-2.02799226391842,
8.60010794953221));
#185381=CARTESIAN_POINT('Ctrl Pts',(6.50506220907525,-1.8645253165514,8.6081626953844));
#185382=CARTESIAN_POINT('Ctrl Pts',(6.51084720576157,-1.84434229034639,
8.60915720313797));
#185383=CARTESIAN_POINT('Ctrl Pts',(6.51653694186991,-1.82413697333543,
8.61015171089155));
#185384=CARTESIAN_POINT('Ctrl Pts',(6.52213127688102,-1.80391036560313,
8.61114621864512));
#185385=CARTESIAN_POINT('Ctrl Pts',(6.56888345588548,-1.63487544304732,
8.61945737706236));
#185386=CARTESIAN_POINT('Ctrl Pts',(6.60912320732425,-1.46379381995098,
8.62776853547959));
#185387=CARTESIAN_POINT('Ctrl Pts',(6.64267135078699,-1.29120344076129,
8.63607969389682));
#185388=CARTESIAN_POINT('Ctrl Pts',(6.67617888760101,-1.11882196484241,
8.64438079249389));
#185389=CARTESIAN_POINT('Ctrl Pts',(6.70301088339192,-0.944935711135553,
8.65268189109096));
#185390=CARTESIAN_POINT('Ctrl Pts',(6.7230378912973,-0.770097728980386,
8.66098298968802));
#185391=CARTESIAN_POINT('Ctrl Pts',(6.74304441839381,-0.595438546539786,
8.66927559908817));
#185392=CARTESIAN_POINT('Ctrl Pts',(6.75625978152564,-0.419829920320681,
8.67756820848831));
#185393=CARTESIAN_POINT('Ctrl Pts',(6.76260551695485,-0.243835235459976,
8.68586081788846));
#185394=CARTESIAN_POINT('Ctrl Pts',(6.76894595353476,-0.0679875106046658,
8.69414650275038));
#185395=CARTESIAN_POINT('Ctrl Pts',(6.76842817879555,0.108245282101846,
8.7024321876123));
#185396=CARTESIAN_POINT('Ctrl Pts',(6.7610254959682,0.284294289193273,8.71071787247422));
#185397=CARTESIAN_POINT('Ctrl Pts',(6.75362760620306,0.460229308712769,
8.71899819255099));
#185398=CARTESIAN_POINT('Ctrl Pts',(6.73935370606844,0.635980430749615,
8.72727851262777));
#185399=CARTESIAN_POINT('Ctrl Pts',(6.71822917679434,0.810978253758559,
8.73555883270454));
#185400=CARTESIAN_POINT('Ctrl Pts',(6.6971135375181,0.985902431089819,8.74383566811063));
#185401=CARTESIAN_POINT('Ctrl Pts',(6.66915305511013,1.16007359379113,8.75211250351671));
#185402=CARTESIAN_POINT('Ctrl Pts',(6.6344250344493,1.33292665299801,8.7603893389228));
#185403=CARTESIAN_POINT('Ctrl Pts',(6.59970459738207,1.50574196610449,8.76866436690782));
#185404=CARTESIAN_POINT('Ctrl Pts',(6.55821963485177,1.67723940584398,8.77693939489285));
#185405=CARTESIAN_POINT('Ctrl Pts',(6.51009875741734,1.84686306170035,8.78521442287787));
#185406=CARTESIAN_POINT('Ctrl Pts',(6.46198020926171,2.01647850696694,8.79348905031228));
#185407=CARTESIAN_POINT('Ctrl Pts',(6.4072264819389,2.18422001211556,8.80176367774668));
#185408=CARTESIAN_POINT('Ctrl Pts',(6.34601639486469,2.34954568291588,8.81003830518109));
#185409=CARTESIAN_POINT('Ctrl Pts',(6.28479886740995,2.51489144984675,8.81831393843627));
#185410=CARTESIAN_POINT('Ctrl Pts',(6.21712353870525,2.6778204690414,8.82658957169144));
#185411=CARTESIAN_POINT('Ctrl Pts',(6.14321787351347,2.83780957052172,8.83486520494662));
#185412=CARTESIAN_POINT('Ctrl Pts',(6.06925881749105,2.99791425111225,8.84314681667357));
#185413=CARTESIAN_POINT('Ctrl Pts',(5.98906057847584,3.15507445174475,8.85142842840052));
#185414=CARTESIAN_POINT('Ctrl Pts',(5.90289761555557,3.30878961861712,8.85971004012748));
#185415=CARTESIAN_POINT('Ctrl Pts',(5.81670262731503,3.46256191882476,8.86799472998985));
#185416=CARTESIAN_POINT('Ctrl Pts',(5.7245386747233,3.61288633158087,8.87627941985222));
#185417=CARTESIAN_POINT('Ctrl Pts',(5.62672438706186,3.75929004893787,8.88456410971459));
#185418=CARTESIAN_POINT('Ctrl Pts',(5.52880186651922,3.90585576406153,8.89285796670249));
#185419=CARTESIAN_POINT('Ctrl Pts',(5.42521672004798,4.04849182860883,8.90115182369039));
#185420=CARTESIAN_POINT('Ctrl Pts',(5.31632948052648,4.18675648378133,8.9094456806783));
#185421=CARTESIAN_POINT('Ctrl Pts',(5.23051499394649,4.29572343388429,8.91598210388374));
#185422=CARTESIAN_POINT('Ctrl Pts',(5.14140818171798,4.4019758686728,8.92251852708918));
#185423=CARTESIAN_POINT('Ctrl Pts',(5.0492019292571,4.50531340503482,8.92905495029462));
#185424=CARTESIAN_POINT('Ctrl Pts',(4.9291557516156,4.63985174615666,8.93756492223598));
#185425=CARTESIAN_POINT('Ctrl Pts',(4.80363577572484,4.76969374884127,8.94607489417734));
#185426=CARTESIAN_POINT('Ctrl Pts',(4.67303313686358,4.89438967612663,8.95458486611871));
#185427=CARTESIAN_POINT('Ctrl Pts',(4.54258179068798,5.0189411531781,8.96308497993989));
#185428=CARTESIAN_POINT('Ctrl Pts',(4.40705976086991,5.13835822431179,8.97158509376107));
#185429=CARTESIAN_POINT('Ctrl Pts',(4.26689595798769,5.25222694518319,8.98008520758225));
#185430=CARTESIAN_POINT('Ctrl Pts',(4.12682955979059,5.36601653473343,8.9885794143797));
#185431=CARTESIAN_POINT('Ctrl Pts',(3.98212806882856,5.47426525584026,8.99707362117715));
#185432=CARTESIAN_POINT('Ctrl Pts',(3.83325529781371,5.57659778196197,9.0055678279746));
#185433=CARTESIAN_POINT('Ctrl Pts',(3.6844893612837,5.67885687193658,9.01405593913615));
#185434=CARTESIAN_POINT('Ctrl Pts',(3.53155838193464,5.77520805237895,9.0225440502977));
#185435=CARTESIAN_POINT('Ctrl Pts',(3.3749573045159,5.86531774013095,9.03103216145925));
#185436=CARTESIAN_POINT('Ctrl Pts',(3.28420531444393,5.91753726264669,9.03595111216227));
#185437=CARTESIAN_POINT('Ctrl Pts',(3.19222136425885,5.96766146652434,9.04087006286529));
#185438=CARTESIAN_POINT('Ctrl Pts',(3.09910619832133,6.0156321173694,9.04578901356831));
#185439=CARTESIAN_POINT('',(3.92888236737287,-5.50964357679755,8.));
#185440=CARTESIAN_POINT('Origin',(0.,0.,8.));
#185441=CARTESIAN_POINT('Ctrl Pts',(3.92888236737205,-5.50964357679814,
8.));
#185442=CARTESIAN_POINT('Ctrl Pts',(4.08455174303594,-5.39863700138894,
8.00899352209616));
#185443=CARTESIAN_POINT('Ctrl Pts',(4.23547548564298,-5.28105696228342,
8.01798704419231));
#185444=CARTESIAN_POINT('Ctrl Pts',(4.38113219096226,-5.15732195284667,
8.02698056628847));
#185445=CARTESIAN_POINT('Ctrl Pts',(4.52683306677746,-5.03354942068334,
8.03597681567637));
#185446=CARTESIAN_POINT('Ctrl Pts',(4.66726353054798,-4.90361834910203,
8.04497306506428));
#185447=CARTESIAN_POINT('Ctrl Pts',(4.80193642306303,-4.76798653404775,
8.05396931445219));
#185448=CARTESIAN_POINT('Ctrl Pts',(4.93663304510132,-4.63233082050693,
8.0629671489899));
#185449=CARTESIAN_POINT('Ctrl Pts',(5.06556989731732,-4.49097252926221,
8.07196498352761));
#185450=CARTESIAN_POINT('Ctrl Pts',(5.18829690835927,-4.34440608031865,
8.08096281806532));
#185451=CARTESIAN_POINT('Ctrl Pts',(5.31100285047716,-4.19786479288889,
8.08995910791705));
#185452=CARTESIAN_POINT('Ctrl Pts',(5.42750092637609,-4.04611732175522,
8.09895539776879));
#185453=CARTESIAN_POINT('Ctrl Pts',(5.53738107052083,-3.88969148903067,
8.10795168762053));
#185454=CARTESIAN_POINT('Ctrl Pts',(5.64720908640168,-3.7333398663206,8.11694370954037));
#185455=CARTESIAN_POINT('Ctrl Pts',(5.75042530410842,-3.57231451577492,
8.12593573146022));
#185456=CARTESIAN_POINT('Ctrl Pts',(5.84666223591746,-3.40717327107041,
8.13492775338006));
#185457=CARTESIAN_POINT('Ctrl Pts',(5.93237701301114,-3.26008789841009,
8.14293662419496));
#185458=CARTESIAN_POINT('Ctrl Pts',(6.01255575491793,-3.10973797526773,
8.15094549500986));
#185459=CARTESIAN_POINT('Ctrl Pts',(6.08696823580306,-2.95653626670206,
8.15895436582476));
#185460=CARTESIAN_POINT('Ctrl Pts',(6.16290650334216,-2.80019324206262,
8.16712745409428));
#185461=CARTESIAN_POINT('Ctrl Pts',(6.23286194654829,-2.64083088712788,
8.17530054236379));
#185462=CARTESIAN_POINT('Ctrl Pts',(6.29659359585751,-2.47895100568894,
8.18347363063331));
#185463=CARTESIAN_POINT('Ctrl Pts',(6.36030468714056,-2.31712334211782,
8.19164408249589));
#185464=CARTESIAN_POINT('Ctrl Pts',(6.41779585019016,-2.15278010606025,
8.19981453435846));
#185465=CARTESIAN_POINT('Ctrl Pts',(6.46887395681812,-1.98644373965142,
8.20798498622104));
#185466=CARTESIAN_POINT('Ctrl Pts',(6.51994510918165,-1.82013001987444,
8.21615432567976));
#185467=CARTESIAN_POINT('Ctrl Pts',(6.56460483900829,-1.65182405680871,
8.22432366513848));
#185468=CARTESIAN_POINT('Ctrl Pts',(6.60270966236539,-1.48206413980866,
8.2324930045972));
#185469=CARTESIAN_POINT('Ctrl Pts',(6.64082696565672,-1.31224862374234,
8.24066501964422));
#185470=CARTESIAN_POINT('Ctrl Pts',(6.67238499141571,-1.1409785555763,8.24883703469122));
#185471=CARTESIAN_POINT('Ctrl Pts',(6.69729114048687,-0.968803581514901,
8.25700904973823));
#185472=CARTESIAN_POINT('Ctrl Pts',(6.72220180218756,-0.796597411869245,
8.26518254543471));
#185473=CARTESIAN_POINT('Ctrl Pts',(6.74045814160945,-0.623486369340189,
8.2733560411312));
#185474=CARTESIAN_POINT('Ctrl Pts',(6.75201938147832,-0.450025857191645,
8.28152953682767));
#185475=CARTESIAN_POINT('Ctrl Pts',(6.76358901971194,-0.276439339124579,
8.28970896994945));
#185476=CARTESIAN_POINT('Ctrl Pts',(6.76845382921612,-0.10250320643135,
8.29788840307123));
#185477=CARTESIAN_POINT('Ctrl Pts',(6.76662514637511,0.0712258972851174,
8.306067836193));
#185478=CARTESIAN_POINT('Ctrl Pts',(6.76574272000883,0.155058445100922,
8.31001480134518));
#185479=CARTESIAN_POINT('Ctrl Pts',(6.76330247670826,0.23884281946348,8.31396176649735));
#185480=CARTESIAN_POINT('Ctrl Pts',(6.75931001498592,0.322516854305433,
8.31790873164953));
#185481=CARTESIAN_POINT('Ctrl Pts',(6.74991754506057,0.51936429091016,8.327194168572));
#185482=CARTESIAN_POINT('Ctrl Pts',(6.73192447125622,0.715743860383588,
8.33647960549447));
#185483=CARTESIAN_POINT('Ctrl Pts',(6.7054056754185,0.910946610985172,8.34576504241694));
#185484=CARTESIAN_POINT('Ctrl Pts',(6.6788814416537,1.10618938973627,8.35505238340509));
#185485=CARTESIAN_POINT('Ctrl Pts',(6.64382801984104,1.30025468391843,8.36433972439324));
#185486=CARTESIAN_POINT('Ctrl Pts',(6.6003718822135,1.49244095912886,8.37362706538139));
#185487=CARTESIAN_POINT('Ctrl Pts',(6.55694837666439,1.68448291784108,8.38290743232039));
#185488=CARTESIAN_POINT('Ctrl Pts',(6.50513480897838,1.87464849745314,8.39218779925939));
#185489=CARTESIAN_POINT('Ctrl Pts',(6.44510829319222,2.06224830925495,8.40146816619839));
#185490=CARTESIAN_POINT('Ctrl Pts',(6.38514056272315,2.24966440034135,8.41073944466531));
#185491=CARTESIAN_POINT('Ctrl Pts',(6.31697600347113,2.43451956542231,8.42001072313222));
#185492=CARTESIAN_POINT('Ctrl Pts',(6.24084145515054,2.61613970033608,8.42928200159913));
#185493=CARTESIAN_POINT('Ctrl Pts',(6.16488429767093,2.79733666667287,8.43853167831073));
#185494=CARTESIAN_POINT('Ctrl Pts',(6.08099430017188,2.97531348152076,8.44778135502232));
#185495=CARTESIAN_POINT('Ctrl Pts',(5.9894460394904,3.14941663487585,8.45703103173391));
#185496=CARTESIAN_POINT('Ctrl Pts',(5.92401704556043,3.27384711645205,8.46364172031403));
#185497=CARTESIAN_POINT('Ctrl Pts',(5.85467733362457,3.39629930313006,8.47025240889415));
#185498=CARTESIAN_POINT('Ctrl Pts',(5.78154241060723,3.51654039566589,8.47686309747428));
#185499=CARTESIAN_POINT('Ctrl Pts',(5.69008649737165,3.66690301960275,8.48512982609403));
#185500=CARTESIAN_POINT('Ctrl Pts',(5.59273632757111,3.81373627669594,8.49339655471379));
#185501=CARTESIAN_POINT('Ctrl Pts',(5.48980022029091,3.95656195974408,8.50166328333354));
#185502=CARTESIAN_POINT('Ctrl Pts',(5.38687329625559,4.09937490087632,8.50992927445316));
#185503=CARTESIAN_POINT('Ctrl Pts',(5.27836163360689,4.23818069531259,8.51819526557278));
#185504=CARTESIAN_POINT('Ctrl Pts',(5.16461605766672,4.37253130084749,8.5264612566924));
#185505=CARTESIAN_POINT('Ctrl Pts',(5.05086105281971,4.50689304333724,8.53472793301897));
#185506=CARTESIAN_POINT('Ctrl Pts',(4.93187149831131,4.63679859343608,8.54299460934555));
#185507=CARTESIAN_POINT('Ctrl Pts',(4.80803765128304,4.76183398953016,8.55126128567213));
#185508=CARTESIAN_POINT('Ctrl Pts',(4.68412876548718,4.88694515248648,8.55953297130124));
#185509=CARTESIAN_POINT('Ctrl Pts',(4.55536997067134,5.00718001583141,8.56780465693035));
#185510=CARTESIAN_POINT('Ctrl Pts',(4.42218796782023,5.12216190463227,8.57607634255946));
#185511=CARTESIAN_POINT('Ctrl Pts',(4.28896000624874,5.23718347162058,8.58435088259892));
#185512=CARTESIAN_POINT('Ctrl Pts',(4.15130606590586,5.34694822772878,8.59262542263838));
#185513=CARTESIAN_POINT('Ctrl Pts',(4.00968498910448,5.45112055344131,8.60089996267783));
#185514=CARTESIAN_POINT('Ctrl Pts',(3.86793510529871,5.55538762582232,8.60918202856541));
#185515=CARTESIAN_POINT('Ctrl Pts',(3.7222111669496,5.65405190789338,8.61746409445299));
#185516=CARTESIAN_POINT('Ctrl Pts',(3.57300063748498,5.74682133396645,8.62574616034057));
#185517=CARTESIAN_POINT('Ctrl Pts',(3.51251876950539,5.78442503526304,8.62910326132673));
#185518=CARTESIAN_POINT('Ctrl Pts',(3.45146432374767,5.82106070438347,8.63246036231289));
#185519=CARTESIAN_POINT('Ctrl Pts',(3.38987086665649,5.85671106572568,8.63581746329905));
#185520=CARTESIAN_POINT('Ctrl Pts',(3.29431822886113,5.91201703855918,8.64102548164583));
#185521=CARTESIAN_POINT('Ctrl Pts',(3.19735717007827,5.96501562526646,8.64623349999262));
#185522=CARTESIAN_POINT('Ctrl Pts',(3.09910619832133,6.0156321173694,8.6514415183394));
#185523=CARTESIAN_POINT('Origin',(0.,0.,4.30282021618968));
#185524=CARTESIAN_POINT('',(3.09910619832133,6.01563211736941,11.0457552630241));
#185525=CARTESIAN_POINT('',(3.09910619832133,6.01563211736941,10.651525285013));
#185526=CARTESIAN_POINT('',(3.09910619832133,6.0156321173694,4.30282021618968));
#185527=CARTESIAN_POINT('',(-6.767,9.95106571471428E-13,9.69717978381004));
#185528=CARTESIAN_POINT('Ctrl Pts',(-6.767,9.95106540770597E-13,9.69717978381004));
#185529=CARTESIAN_POINT('Ctrl Pts',(-6.76700000000003,-0.186007249525989,
9.70592929562122));
#185530=CARTESIAN_POINT('Ctrl Pts',(-6.75932637294525,-0.372014355749146,
9.71467880743241));
#185531=CARTESIAN_POINT('Ctrl Pts',(-6.74400518264186,-0.557389537486834,
9.7234283192436));
#185532=CARTESIAN_POINT('Ctrl Pts',(-6.72868405705092,-0.742763936251198,
9.73217779409927));
#185533=CARTESIAN_POINT('Ctrl Pts',(-6.70571545645732,-0.927506130241735,
9.74092726895495));
#185534=CARTESIAN_POINT('Ctrl Pts',(-6.67517739404809,-1.11098863990114,
9.74967674381062));
#185535=CARTESIAN_POINT('Ctrl Pts',(-6.64463945808679,-1.29447038982067,
9.75842618243764));
#185536=CARTESIAN_POINT('Ctrl Pts',(-6.60653217008324,-1.47669218313825,
9.76717562106466));
#185537=CARTESIAN_POINT('Ctrl Pts',(-6.56098496092636,-1.65703510599448,
9.77592505969168));
#185538=CARTESIAN_POINT('Ctrl Pts',(-6.51543793658249,-1.83737729708868,
9.78467446281685));
#185539=CARTESIAN_POINT('Ctrl Pts',(-6.46245112167367,-2.01584035511099,
9.79342386594202));
#185540=CARTESIAN_POINT('Ctrl Pts',(-6.40220448374193,-2.19181813760969,
9.80217326906719));
#185541=CARTESIAN_POINT('Ctrl Pts',(-6.34195808526434,-2.3677952206733,
9.8109226374173));
#185542=CARTESIAN_POINT('Ctrl Pts',(-6.27445201433025,-2.54128677684361,
9.8196720057674));
#185543=CARTESIAN_POINT('Ctrl Pts',(-6.19991555071813,-2.71170355385015,
9.8284213741175));
#185544=CARTESIAN_POINT('Ctrl Pts',(-6.12537937716595,-2.88211966767684,
9.83717070841928));
#185545=CARTESIAN_POINT('Ctrl Pts',(-6.04381298052414,-3.04946076371996,
9.84592004272107));
#185546=CARTESIAN_POINT('Ctrl Pts',(-5.95549339335716,-3.2131584837476,
9.85466937702285));
#185547=CARTESIAN_POINT('Ctrl Pts',(-5.86717414255289,-3.37685558033701,
9.86341867800303));
#185548=CARTESIAN_POINT('Ctrl Pts',(-5.77210188876474,-3.53690907646959,
9.87216797898322));
#185549=CARTESIAN_POINT('Ctrl Pts',(-5.67059953346867,-3.69277536969484,
9.88091727996341));
#185550=CARTESIAN_POINT('Ctrl Pts',(-5.56909755631257,-3.84864108225107,
9.88966654834868));
#185551=CARTESIAN_POINT('Ctrl Pts',(-5.46116568196725,-4.00031938297687,
9.89841581673395));
#185552=CARTESIAN_POINT('Ctrl Pts',(-5.34717048533482,-4.1472951186001,
9.90716508511923));
#185553=CARTESIAN_POINT('Ctrl Pts',(-5.23317570391725,-4.29427031888051,
9.91591432163626));
#185554=CARTESIAN_POINT('Ctrl Pts',(-5.11311782003413,-4.43654276189662,
9.92466355815329));
#185555=CARTESIAN_POINT('Ctrl Pts',(-4.98740458984665,-4.57362924351948,
9.93341279467033));
#185556=CARTESIAN_POINT('Ctrl Pts',(-4.86169180711645,-4.71071523720369,
9.94216200004577));
#185557=CARTESIAN_POINT('Ctrl Pts',(-4.73032391204063,-4.84261509523345,
9.95091120542122));
#185558=CARTESIAN_POINT('Ctrl Pts',(-4.59374707013479,-4.96888084538441,
9.95966041079667));
#185559=CARTESIAN_POINT('Ctrl Pts',(-4.45717070301335,-5.09514615659559,
9.9684095857571));
#185560=CARTESIAN_POINT('Ctrl Pts',(-4.31538563570942,-5.21577720459608,
9.97715876071754));
#185561=CARTESIAN_POINT('Ctrl Pts',(-4.16887341029423,-5.33036429232954,
9.98590793567797));
#185562=CARTESIAN_POINT('Ctrl Pts',(-4.02236168203631,-5.44495099123671,
9.99465708094999));
#185563=CARTESIAN_POINT('Ctrl Pts',(-3.87112305348101,-5.55349359438646,
10.003406226222));
#185564=CARTESIAN_POINT('Ctrl Pts',(-3.71567117017709,-5.65562346298928,
10.012155371494));
#185565=CARTESIAN_POINT('Ctrl Pts',(-3.56021980145775,-5.75775299351671,
10.0209044878042));
#185566=CARTESIAN_POINT('Ctrl Pts',(-3.40055544538315,-5.85346967463892,
10.0296536041143));
#185567=CARTESIAN_POINT('Ctrl Pts',(-3.23722035986829,-5.94244842986914,
10.0384027204245));
#185568=CARTESIAN_POINT('Ctrl Pts',(-3.07388580147158,-6.0314268979454,
10.0471518084993));
#185569=CARTESIAN_POINT('Ctrl Pts',(-2.90688078896558,-6.11366734656791,
10.0559008965742));
#185570=CARTESIAN_POINT('Ctrl Pts',(-2.73677250721353,-6.18889046952361,
10.064649984649));
#185571=CARTESIAN_POINT('Ctrl Pts',(-2.56666476031449,-6.26411335596341,
10.0733990452151));
#185572=CARTESIAN_POINT('Ctrl Pts',(-2.39345402575116,-6.33231884500575,
10.0821481057811));
#185573=CARTESIAN_POINT('Ctrl Pts',(-2.21772856065524,-6.3932752976275,
10.0908971663471));
#185574=CARTESIAN_POINT('Ctrl Pts',(-2.04200363348448,-6.45423156365132,
10.0996462001308));
#185575=CARTESIAN_POINT('Ctrl Pts',(-1.86376426189216,-6.50793874375676,
10.1083952339145));
#185576=CARTESIAN_POINT('Ctrl Pts',(-1.68361577753094,-6.55421443909557,
10.1171442676982));
#185577=CARTESIAN_POINT('Ctrl Pts',(-1.50346782967715,-6.60048999661888,
10.125893275426));
#185578=CARTESIAN_POINT('Ctrl Pts',(-1.32141105794878,-6.63933404237735,
10.1346422831539));
#185579=CARTESIAN_POINT('Ctrl Pts',(-1.13806375486889,-6.67061465607584,
10.1433912908817));
#185580=CARTESIAN_POINT('Ctrl Pts',(-0.954716982602104,-6.70189517921308,
10.1521402732801));
#185581=CARTESIAN_POINT('Ctrl Pts',(-0.770079968901649,-6.72561226592233,
10.1608892556785));
#185582=CARTESIAN_POINT('Ctrl Pts',(-0.584779765558184,-6.74168536983103,
10.1696382380769));
#185583=CARTESIAN_POINT('Ctrl Pts',(-0.391489830651259,-6.75845151013853,
10.1787644570867));
#185584=CARTESIAN_POINT('Ctrl Pts',(-0.197478578238317,-6.76689983031625,
10.1878906760966));
#185585=CARTESIAN_POINT('Ctrl Pts',(-0.00346287645134736,-6.76699911397118,
10.1970168951065));
#185586=CARTESIAN_POINT('Ctrl Pts',(0.184489834654779,-6.76709529501189,
10.2058579197723));
#185587=CARTESIAN_POINT('Ctrl Pts',(0.372446404250258,-6.75935639738163,
10.2146989444381));
#185588=CARTESIAN_POINT('Ctrl Pts',(0.559755019489222,-6.74380925873179,
10.2235399691039));
#185589=CARTESIAN_POINT('Ctrl Pts',(0.745134705522643,-6.72842222659796,
10.2322899477137));
#185590=CARTESIAN_POINT('Ctrl Pts',(0.929879431229419,-6.70538706057512,
10.2410399263234));
#185591=CARTESIAN_POINT('Ctrl Pts',(1.11336163626909,-6.67478200894113,
10.2497899049331));
#185592=CARTESIAN_POINT('Ctrl Pts',(1.29684196300825,-6.64417727060993,
10.2585397939697));
#185593=CARTESIAN_POINT('Ctrl Pts',(1.47905951217638,-6.60600284890562,
10.2672896830062));
#185594=CARTESIAN_POINT('Ctrl Pts',(1.65939532067234,-6.56038841607193,
10.2760395720427));
#185595=CARTESIAN_POINT('Ctrl Pts',(1.83972934300957,-6.51477443503213,
10.2847893744149));
#185596=CARTESIAN_POINT('Ctrl Pts',(2.01818138406424,-6.46172066062091,
10.2935391767871));
#185597=CARTESIAN_POINT('Ctrl Pts',(2.19414528354364,-6.40140730423422,
10.3022889791592));
#185598=CARTESIAN_POINT('Ctrl Pts',(2.37010749864153,-6.34109452518585,
10.3110386977755));
#185599=CARTESIAN_POINT('Ctrl Pts',(2.54358134866603,-6.27352239616446,
10.3197884163918));
#185600=CARTESIAN_POINT('Ctrl Pts',(2.71397759435689,-6.19892043966761,
10.3285381350082));
#185601=CARTESIAN_POINT('Ctrl Pts',(2.88437226558249,-6.12431917249456,
10.3372877727769));
#185602=CARTESIAN_POINT('Ctrl Pts',(3.05168912681073,-6.04268832278739,
10.3460374105456));
#185603=CARTESIAN_POINT('Ctrl Pts',(3.21535986273964,-5.95430516123275,
10.3547870483143));
#185604=CARTESIAN_POINT('Ctrl Pts',(3.3790291407296,-5.86592278697373,10.3635366081434));
#185605=CARTESIAN_POINT('Ctrl Pts',(3.53905210621699,-5.77078835741864,
10.3722861679724));
#185606=CARTESIAN_POINT('Ctrl Pts',(3.69488522831832,-5.66922500431541,
10.3810357278015));
#185607=CARTESIAN_POINT('Ctrl Pts',(3.85071701407077,-5.56766252216998,
10.3897852125986));
#185608=CARTESIAN_POINT('Ctrl Pts',(4.00235878822544,-5.45967138329268,
10.3985346973957));
#185609=CARTESIAN_POINT('Ctrl Pts',(4.14929549611466,-5.34561838199498,
10.4072841821929));
#185610=CARTESIAN_POINT('Ctrl Pts',(4.29623099276228,-5.23156632086902,
10.4160335948654));
#185611=CARTESIAN_POINT('Ctrl Pts',(4.43846127436164,-5.11145267304846,
10.424783007538));
#185612=CARTESIAN_POINT('Ctrl Pts',(4.57550326054575,-4.98568540049763,
10.4335324202106));
#185613=CARTESIAN_POINT('Ctrl Pts',(4.71254416257903,-4.85991912290241,
10.4422817636659));
#185614=CARTESIAN_POINT('Ctrl Pts',(4.84439664018874,-4.72849950385303,
10.4510311071211));
#185615=CARTESIAN_POINT('Ctrl Pts',(4.97061286794848,-4.59187289860957,
10.4597804505764));
#185616=CARTESIAN_POINT('Ctrl Pts',(5.09682813912776,-4.4552473288458,10.4685297277212));
#185617=CARTESIAN_POINT('Ctrl Pts',(5.21740705147919,-4.31341506235689,
10.477279004866));
#185618=CARTESIAN_POINT('Ctrl Pts',(5.33194007545767,-4.16685781275633,
10.4860282820108));
#185619=CARTESIAN_POINT('Ctrl Pts',(5.44647226944537,-4.0203016252177,10.4947774957519));
#185620=CARTESIAN_POINT('Ctrl Pts',(5.55495848628148,-3.86902074887883,
10.503526709493));
#185621=CARTESIAN_POINT('Ctrl Pts',(5.65703027291807,-3.71352898080634,
10.5122759232341));
#185622=CARTESIAN_POINT('Ctrl Pts',(5.7591013537701,-3.55803828789568,10.521025076478));
#185623=CARTESIAN_POINT('Ctrl Pts',(5.85475793592759,-3.398337001067,10.5297742297219));
#185624=CARTESIAN_POINT('Ctrl Pts',(5.943675144274,-3.23496750823551,10.5385233829658));
#185625=CARTESIAN_POINT('Ctrl Pts',(6.03259176732643,-3.0715990907772,10.5472724786187));
#185626=CARTESIAN_POINT('Ctrl Pts',(6.11476896835928,-2.90456276731427,
10.5560215742716));
#185627=CARTESIAN_POINT('Ctrl Pts',(6.18992765547891,-2.7344258300304,10.5647706699246));
#185628=CARTESIAN_POINT('Ctrl Pts',(6.26508587283059,-2.56428995616159,
10.5735197108926));
#185629=CARTESIAN_POINT('Ctrl Pts',(6.33322554827165,-2.39105376935189,
10.5822687518606));
#185630=CARTESIAN_POINT('Ctrl Pts',(6.39411526733035,-2.21530561054066,
10.5910177928287));
#185631=CARTESIAN_POINT('Ctrl Pts',(6.45500462602846,-2.03955849185101,
10.5997667820177));
#185632=CARTESIAN_POINT('Ctrl Pts',(6.50864402040734,-1.86129970164564,
10.6085157712067));
#185633=CARTESIAN_POINT('Ctrl Pts',(6.55485128368592,-1.68113463136095,
10.6172647603957));
#185634=CARTESIAN_POINT('Ctrl Pts',(6.60199809554315,-1.49730620116918,
10.6261916458672));
#185635=CARTESIAN_POINT('Ctrl Pts',(6.64140720707861,-1.31149343245761,
10.6351185313386));
#185636=CARTESIAN_POINT('Ctrl Pts',(6.67293928722871,-1.12435326697601,
10.64404541681));
#185637=CARTESIAN_POINT('Ctrl Pts',(6.70384625876246,-0.940923067007366,
10.6527953309875));
#185638=CARTESIAN_POINT('Ctrl Pts',(6.72718554579787,-0.756217899522463,
10.6615452451649));
#185639=CARTESIAN_POINT('Ctrl Pts',(6.74287786815321,-0.570865181255318,
10.6702951593424));
#185640=CARTESIAN_POINT('Ctrl Pts',(6.75856988190841,-0.385516108074804,
10.6790449014469));
#185641=CARTESIAN_POINT('Ctrl Pts',(6.766615207734,-0.199519795227242,10.6877946435514));
#185642=CARTESIAN_POINT('Ctrl Pts',(6.76698651789579,-0.0135080204565767,
10.6965443856558));
#185643=CARTESIAN_POINT('Ctrl Pts',(6.76735782124905,0.172500343511997,
10.7052939673208));
#185644=CARTESIAN_POINT('Ctrl Pts',(6.76005538995189,0.358523882209922,
10.7140435489858));
#185645=CARTESIAN_POINT('Ctrl Pts',(6.74510402742369,0.543930748563345,
10.7227931306508));
#185646=CARTESIAN_POINT('Ctrl Pts',(6.73015291918042,0.729334461614151,
10.7315425635074));
#185647=CARTESIAN_POINT('Ctrl Pts',(6.7075531630661,0.914121237633547,10.7402919963641));
#185648=CARTESIAN_POINT('Ctrl Pts',(6.67738151874594,1.09766345166003,10.7490414292208));
#185649=CARTESIAN_POINT('Ctrl Pts',(6.64721034747591,1.28120278799551,10.7577907248983));
#185650=CARTESIAN_POINT('Ctrl Pts',(6.60946757205166,1.4634973186022,10.7665400205758));
#185651=CARTESIAN_POINT('Ctrl Pts',(6.56428138111549,1.64392790278058,10.7752893162534));
#185652=CARTESIAN_POINT('Ctrl Pts',(6.51909583859879,1.82435589778951,10.784038486379));
#185653=CARTESIAN_POINT('Ctrl Pts',(6.46646716392908,2.00291972192159,10.7927876565046));
#185654=CARTESIAN_POINT('Ctrl Pts',(6.4065740987292,2.17901292274557,10.8015368266302));
#185655=CARTESIAN_POINT('Ctrl Pts',(6.34668181342117,2.35510383058867,10.8102858828293));
#185656=CARTESIAN_POINT('Ctrl Pts',(6.27952541914095,2.52872390822468,10.8190349390284));
#185657=CARTESIAN_POINT('Ctrl Pts',(6.20533299175567,2.6992835089017,10.8277839952275));
#185658=CARTESIAN_POINT('Ctrl Pts',(6.12831602991598,2.87633637965519,10.8368661313857));
#185659=CARTESIAN_POINT('Ctrl Pts',(6.04371690605318,3.05009086601368,10.8459482675439));
#185660=CARTESIAN_POINT('Ctrl Pts',(5.95184520316677,3.2199111288265,10.8550304037021));
#185661=CARTESIAN_POINT('Ctrl Pts',(5.8633354950932,3.38351691182938,10.8637801840457));
#185662=CARTESIAN_POINT('Ctrl Pts',(5.76807618099414,3.5434710371193,10.8725299643892));
#185663=CARTESIAN_POINT('Ctrl Pts',(5.66639083309061,3.69923018027626,10.8812797447328));
#185664=CARTESIAN_POINT('Ctrl Pts',(5.56470914082247,3.85498372381983,10.8900292105177));
#185665=CARTESIAN_POINT('Ctrl Pts',(5.45660203372114,4.00654234701933,10.8987786763026));
#185666=CARTESIAN_POINT('Ctrl Pts',(5.34243669839265,4.15339127986607,10.9075281420875));
#185667=CARTESIAN_POINT('Ctrl Pts',(5.22827486050639,4.30023571401221,10.9162773398335));
#185668=CARTESIAN_POINT('Ctrl Pts',(5.10805534167158,4.44237052028415,10.9250265375796));
#185669=CARTESIAN_POINT('Ctrl Pts',(4.98218644339998,4.5793129662867,10.9337757353256));
#185670=CARTESIAN_POINT('Ctrl Pts',(4.85632073219634,4.71625194483312,10.9425247115372));
#185671=CARTESIAN_POINT('Ctrl Pts',(4.72480612170366,4.84799861524462,10.9512736877488));
#185672=CARTESIAN_POINT('Ctrl Pts',(4.58808925235359,4.97410554898441,10.9600226639605));
#185673=CARTESIAN_POINT('Ctrl Pts',(4.45136349474098,5.10022068121163,10.9687722089622));
#185674=CARTESIAN_POINT('Ctrl Pts',(4.30943501210132,5.22069514871791,10.9775217539639));
#185675=CARTESIAN_POINT('Ctrl Pts',(4.16278587431836,5.33511975166214,10.9862712989656));
#185676=CARTESIAN_POINT('Ctrl Pts',(4.01614535740492,5.4495376280781,10.9950203296193));
#185677=CARTESIAN_POINT('Ctrl Pts',(3.86478496657957,5.55790617532761,11.0037693602731));
#185678=CARTESIAN_POINT('Ctrl Pts',(3.70921874747218,5.65985735539341,11.0125183909268));
#185679=CARTESIAN_POINT('Ctrl Pts',(3.55365041605934,5.76180991977025,11.0212675403764));
#185680=CARTESIAN_POINT('Ctrl Pts',(3.39387638174568,5.85734478552786,11.030016689826));
#185681=CARTESIAN_POINT('Ctrl Pts',(3.23043927904597,5.94613749121201,11.0387658392756));
#185682=CARTESIAN_POINT('Ctrl Pts',(3.18691767070467,5.96978206944128,11.0410956471918));
#185683=CARTESIAN_POINT('Ctrl Pts',(3.14313645919646,5.99294880633417,11.043425455108));
#185684=CARTESIAN_POINT('Ctrl Pts',(3.09910619832133,6.01563211736941,11.0457552630241));
#185685=CARTESIAN_POINT('Ctrl Pts',(3.09910619832133,6.0156321173694,9.04578901356831));
#185686=CARTESIAN_POINT('Ctrl Pts',(2.93854643732489,6.09834857023698,9.05427082790305));
#185687=CARTESIAN_POINT('Ctrl Pts',(2.77462202131184,6.17465935559691,9.06275264223778));
#185688=CARTESIAN_POINT('Ctrl Pts',(2.6078694041067,6.244301896219,9.07123445657252));
#185689=CARTESIAN_POINT('Ctrl Pts',(2.49793806071349,6.29021360768847,9.07682607642148));
#185690=CARTESIAN_POINT('Ctrl Pts',(2.38677808018559,6.33322817998522,9.08241769627043));
#185691=CARTESIAN_POINT('Ctrl Pts',(2.27454838086761,6.3732816243355,9.08800931611939));
#185692=CARTESIAN_POINT('Ctrl Pts',(2.10237858916949,6.43472697447443,9.09658733094523));
#185693=CARTESIAN_POINT('Ctrl Pts',(1.92776963553591,6.48917305710021,9.10516534577107));
#185694=CARTESIAN_POINT('Ctrl Pts',(1.75130881270765,6.53645212959848,9.11374336059692));
#185695=CARTESIAN_POINT('Ctrl Pts',(1.57475862025023,6.58375514686313,9.12232571980919));
#185696=CARTESIAN_POINT('Ctrl Pts',(1.39635498702721,6.62388383109445,9.13090807902146));
#185697=CARTESIAN_POINT('Ctrl Pts',(1.21669707763909,6.65672120651485,9.13949043823373));
#185698=CARTESIAN_POINT('Ctrl Pts',(1.02921542872602,6.69098858339106,9.14844654187627));
#185699=CARTESIAN_POINT('Ctrl Pts',(0.840368190626526,6.717315330712,9.1574026455188));
#185700=CARTESIAN_POINT('Ctrl Pts',(0.650843588111725,6.7356285247788,9.16635874916134));
#185701=CARTESIAN_POINT('Ctrl Pts',(0.468914041976044,6.75320783132086,
9.17495594366384));
#185702=CARTESIAN_POINT('Ctrl Pts',(0.286360676529203,6.763403362385,9.18355313816635));
#185703=CARTESIAN_POINT('Ctrl Pts',(0.103793877473092,6.76620394541867,
9.19215033266886));
#185704=CARTESIAN_POINT('Ctrl Pts',(-0.0788866154034073,6.76900627252073,
9.20075288109055));
#185705=CARTESIAN_POINT('Ctrl Pts',(-0.261580248477637,6.76440446413929,
9.20935542951224));
#185706=CARTESIAN_POINT('Ctrl Pts',(-0.443678625344181,6.75243943159898,
9.21795797793393));
#185707=CARTESIAN_POINT('Ctrl Pts',(-0.625968327623834,6.7404618277506,
9.22656956480044));
#185708=CARTESIAN_POINT('Ctrl Pts',(-0.807661215189427,6.72110557014409,
9.23518115166695));
#185709=CARTESIAN_POINT('Ctrl Pts',(-0.988154744929942,6.6944633242757,
9.24379273853346));
#185710=CARTESIAN_POINT('Ctrl Pts',(-1.0103084152377,6.69119327059525,9.24484971967036));
#185711=CARTESIAN_POINT('Ctrl Pts',(-1.03244403022776,6.68781351690102,
9.24590670080725));
#185712=CARTESIAN_POINT('Ctrl Pts',(-1.05456048731491,6.68432428736025,
9.24696368194414));
#185713=CARTESIAN_POINT('Ctrl Pts',(-1.24425019003177,6.65439766250844,
9.25602925862511));
#185714=CARTESIAN_POINT('Ctrl Pts',(-1.43270925910908,6.61638521402429,
9.26509483530608));
#185715=CARTESIAN_POINT('Ctrl Pts',(-1.61927316818519,6.57040663937899,
9.27416041198704));
#185716=CARTESIAN_POINT('Ctrl Pts',(-1.80566893266155,6.5244695038795,9.28321781812865));
#185717=CARTESIAN_POINT('Ctrl Pts',(-1.99017272058708,6.47058063306388,
9.29227522427025));
#185718=CARTESIAN_POINT('Ctrl Pts',(-2.17213145945179,6.40891050981833,
9.30133263041186));
#185719=CARTESIAN_POINT('Ctrl Pts',(-2.35376430771272,6.34735083861166,
9.3103738146145));
#185720=CARTESIAN_POINT('Ctrl Pts',(-2.53286098808698,6.27803781958628,
9.31941499881713));
#185721=CARTESIAN_POINT('Ctrl Pts',(-2.70878498740475,6.20119124781768,
9.32845618301977));
#185722=CARTESIAN_POINT('Ctrl Pts',(-2.88448220283226,6.12444373907953,
9.33748571221835));
#185723=CARTESIAN_POINT('Ctrl Pts',(-3.05701468582643,6.04018215231809,
9.34651524141693));
#185724=CARTESIAN_POINT('Ctrl Pts',(-3.22576480942988,5.9486746754419,9.35554477061551));
#185725=CARTESIAN_POINT('Ctrl Pts',(-3.39411795280301,5.85738246749987,
9.36455305808398));
#185726=CARTESIAN_POINT('Ctrl Pts',(-3.55870629230085,5.75887850510299,
9.37356134555245));
#185727=CARTESIAN_POINT('Ctrl Pts',(-3.71893623776688,5.65347700618162,
9.38256963302093));
#185728=CARTESIAN_POINT('Ctrl Pts',(-3.85736858815834,5.56241427013669,
9.39035243793692));
#185729=CARTESIAN_POINT('Ctrl Pts',(-3.99254793695919,5.46620380645547,
9.39813524285292));
#185730=CARTESIAN_POINT('Ctrl Pts',(-4.1241052636902,5.36507639964267,9.40591804776891));
#185731=CARTESIAN_POINT('Ctrl Pts',(-4.26134633016998,5.2595799327701,9.41403709726176));
#185732=CARTESIAN_POINT('Ctrl Pts',(-4.39458133961908,5.14877973427311,
9.4221561467546));
#185733=CARTESIAN_POINT('Ctrl Pts',(-4.52338049145663,5.03302274279678,
9.43027519624744));
#185734=CARTESIAN_POINT('Ctrl Pts',(-4.65217030132519,4.91727414732468,
9.43839365685513));
#185735=CARTESIAN_POINT('Ctrl Pts',(-4.77652462189025,4.79656971991791,
9.44651211746282));
#185736=CARTESIAN_POINT('Ctrl Pts',(-4.89604821773083,4.67129541451349,
9.4546305780705));
#185737=CARTESIAN_POINT('Ctrl Pts',(-5.0155859867208,4.54600625403854,9.46275000136806));
#185738=CARTESIAN_POINT('Ctrl Pts',(-5.13029163829269,4.41614640248504,
9.47086942466562));
#185739=CARTESIAN_POINT('Ctrl Pts',(-5.23980819879691,4.28213720469355,
9.47898884796318));
#185740=CARTESIAN_POINT('Ctrl Pts',(-5.34940462715595,4.14803027714225,
9.4871141925654));
#185741=CARTESIAN_POINT('Ctrl Pts',(-5.45380417410579,4.00976824360599,
9.49523953716763));
#185742=CARTESIAN_POINT('Ctrl Pts',(-5.55269104690452,3.8678044337358,9.50336488176986));
#185743=CARTESIAN_POINT('Ctrl Pts',(-5.65161816392444,3.72578284852292,
9.51149353316253));
#185744=CARTESIAN_POINT('Ctrl Pts',(-5.74502793731403,3.5800567923771,9.51962218455519));
#185745=CARTESIAN_POINT('Ctrl Pts',(-5.83264917564189,3.43110661359918,
9.52775083594785));
#185746=CARTESIAN_POINT('Ctrl Pts',(-5.92036613308567,3.28199371879828,
9.5358883672347));
#185747=CARTESIAN_POINT('Ctrl Pts',(-6.00228175205012,3.12964998894373,
9.54402589852156));
#185748=CARTESIAN_POINT('Ctrl Pts',(-6.07817152326886,2.97457895066234,
9.55216342980841));
#185749=CARTESIAN_POINT('Ctrl Pts',(-6.11767907733684,2.89385031845155,
9.55639975773683));
#185750=CARTESIAN_POINT('Ctrl Pts',(-6.15555433183113,2.81238286858704,
9.56063608566525));
#185751=CARTESIAN_POINT('Ctrl Pts',(-6.19177088937875,2.73024948556756,
9.56487241359367));
#185752=CARTESIAN_POINT('Ctrl Pts',(-6.2709848012202,2.55060495272671,9.57413823369852));
#185753=CARTESIAN_POINT('Ctrl Pts',(-6.34239258434351,2.36747498292763,
9.58340405380337));
#185754=CARTESIAN_POINT('Ctrl Pts',(-6.40572310947491,2.18151333819876,
9.59266987390822));
#185755=CARTESIAN_POINT('Ctrl Pts',(-6.46892235210657,1.99593718702969,
9.60191648621362));
#185756=CARTESIAN_POINT('Ctrl Pts',(-6.52407771530158,1.80754126517537,
9.61116309851903));
#185757=CARTESIAN_POINT('Ctrl Pts',(-6.57096762095635,1.61699521469397,
9.62040971082443));
#185758=CARTESIAN_POINT('Ctrl Pts',(-6.61777937428698,1.42676675104699,
9.62964091162));
#185759=CARTESIAN_POINT('Ctrl Pts',(-6.65635312271435,1.23439549741426,
9.63887211241557));
#185760=CARTESIAN_POINT('Ctrl Pts',(-6.68651729066465,1.04056500116173,
9.64810331321114));
#185761=CARTESIAN_POINT('Ctrl Pts',(-6.71658029407039,0.84738457335817,
9.65730355441831));
#185762=CARTESIAN_POINT('Ctrl Pts',(-6.73828996916701,0.652754858681284,
9.66650379562548));
#185763=CARTESIAN_POINT('Ctrl Pts',(-6.75152608207339,0.457366989498324,
9.67570403683265));
#185764=CARTESIAN_POINT('Ctrl Pts',(-6.76182492117774,0.305338350736371,
9.68286261915845));
#185765=CARTESIAN_POINT('Ctrl Pts',(-6.76699468300774,0.152851025931063,
9.69002120148424));
#185766=CARTESIAN_POINT('Ctrl Pts',(-6.76699999589956,0.000235574698585379,
9.69717978381004));
#185767=CARTESIAN_POINT('',(-6.7669997504469,0.00183778443585837,9.30282021621592));
#185768=CARTESIAN_POINT('Ctrl Pts',(3.09910619832133,6.0156321173694,8.6514415183394));
#185769=CARTESIAN_POINT('Ctrl Pts',(2.94209720223375,6.09651930320018,8.659764140677));
#185770=CARTESIAN_POINT('Ctrl Pts',(2.78179285456176,6.1713209246991,8.66808676301459));
#185771=CARTESIAN_POINT('Ctrl Pts',(2.6186994290156,6.23976780821798,8.67640938535219));
#185772=CARTESIAN_POINT('Ctrl Pts',(2.45571880527167,6.30816735119083,8.68472625143813));
#185773=CARTESIAN_POINT('Ctrl Pts',(2.28995326589144,6.37022078068447,8.69304311752408));
#185774=CARTESIAN_POINT('Ctrl Pts',(2.12193190900749,6.42570571793759,8.70135998361003));
#185775=CARTESIAN_POINT('Ctrl Pts',(1.95399641886819,6.48116229980169,8.70967259938977));
#185776=CARTESIAN_POINT('Ctrl Pts',(1.78380773696813,6.53005697086354,8.71798521516951));
#185777=CARTESIAN_POINT('Ctrl Pts',(1.61191331302807,6.57221610047044,8.72629783094925));
#185778=CARTESIAN_POINT('Ctrl Pts',(1.44007570477806,6.61436129536098,8.73460769918785));
#185779=CARTESIAN_POINT('Ctrl Pts',(1.26653381432395,6.64977530391236,8.74291756742645));
#185780=CARTESIAN_POINT('Ctrl Pts',(1.09184880431173,6.67833476163954,8.75122743566505));
#185781=CARTESIAN_POINT('Ctrl Pts',(0.914481883555387,6.70733268810837,
8.75966488396853));
#185782=CARTESIAN_POINT('Ctrl Pts',(0.735936808451345,6.72926377155085,
8.76810233227201));
#185783=CARTESIAN_POINT('Ctrl Pts',(0.556810674542134,6.74405300043794,
8.77653978057549));
#185784=CARTESIAN_POINT('Ctrl Pts',(0.380370682180497,6.75862045285219,
8.78485070250368));
#185785=CARTESIAN_POINT('Ctrl Pts',(0.203367291180232,6.7662587470079,8.79316162443186));
#185786=CARTESIAN_POINT('Ctrl Pts',(0.0263751707729974,6.76694859965455,
8.80147254636005));
#185787=CARTESIAN_POINT('Ctrl Pts',(-0.150657686527601,6.7676386110792,
8.8097853811482));
#185788=CARTESIAN_POINT('Ctrl Pts',(-0.327678921432271,6.76137699179026,
8.81809821593635));
#185789=CARTESIAN_POINT('Ctrl Pts',(-0.504114683114431,6.74819660252044,
8.8264110507245));
#185790=CARTESIAN_POINT('Ctrl Pts',(-0.680619953403618,6.73501102070639,
8.83472716043583));
#185791=CARTESIAN_POINT('Ctrl Pts',(-0.856538945274694,6.71490126194879,
8.84304327014717));
#185792=CARTESIAN_POINT('Ctrl Pts',(-1.03130353000278,6.68795200558466,
8.8513593798585));
#185793=CARTESIAN_POINT('Ctrl Pts',(-1.21057499376556,6.660307774099,8.85988994778267));
#185794=CARTESIAN_POINT('Ctrl Pts',(-1.38863132264786,6.62546659988185,
8.86842051570684));
#185795=CARTESIAN_POINT('Ctrl Pts',(-1.56487190523667,6.5835753903332,8.87695108363102));
#185796=CARTESIAN_POINT('Ctrl Pts',(-1.73699120549985,6.54266378207148,
8.88528216924358));
#185797=CARTESIAN_POINT('Ctrl Pts',(-1.9073784162457,6.4950283321297,8.89361325485615));
#185798=CARTESIAN_POINT('Ctrl Pts',(-2.07549093628096,6.44085602799935,
8.90194434046872));
#185799=CARTESIAN_POINT('Ctrl Pts',(-2.2496414702677,6.38473804410611,8.9105746495487));
#185800=CARTESIAN_POINT('Ctrl Pts',(-2.42135049050345,6.32160507907051,
8.91920495862867));
#185801=CARTESIAN_POINT('Ctrl Pts',(-2.59003914532514,6.25171866175082,
8.92783526770865));
#185802=CARTESIAN_POINT('Ctrl Pts',(-2.75872780014682,6.18183224443113,
8.93646557678862));
#185803=CARTESIAN_POINT('Ctrl Pts',(-2.92439574511086,6.10519260033339,
8.9450958858686));
#185804=CARTESIAN_POINT('Ctrl Pts',(-3.08649419652116,6.02211279991011,
8.95372619494857));
#185805=CARTESIAN_POINT('Ctrl Pts',(-3.23773100661891,5.94459988174059,
8.96177821767956));
#185806=CARTESIAN_POINT('Ctrl Pts',(-3.38633099540894,5.8612399075377,8.96983024041054));
#185807=CARTESIAN_POINT('Ctrl Pts',(-3.53179615922495,5.77223569249246,
8.97788226314153));
#185808=CARTESIAN_POINT('Ctrl Pts',(-3.67707811592324,5.68334357442821,
8.98592414469618));
#185809=CARTESIAN_POINT('Ctrl Pts',(-3.81923278735326,5.5888215515979,8.99396602625083));
#185810=CARTESIAN_POINT('Ctrl Pts',(-3.95778285138489,5.48892010337951,
9.00200790780548));
#185811=CARTESIAN_POINT('Ctrl Pts',(-4.09618906377005,5.38912237931247,
9.01004143975806));
#185812=CARTESIAN_POINT('Ctrl Pts',(-4.23099781455493,5.28395656086194,
9.01807497171063));
#185813=CARTESIAN_POINT('Ctrl Pts',(-4.36175719359503,5.17371850646341,
9.02610850366321));
#185814=CARTESIAN_POINT('Ctrl Pts',(-4.49240968065308,5.06357056846203,
9.03413546843751));
#185815=CARTESIAN_POINT('Ctrl Pts',(-4.6190190988995,4.94835888673088,9.04216243321181));
#185816=CARTESIAN_POINT('Ctrl Pts',(-4.74116342286366,4.82842193658547,
9.05018939798611));
#185817=CARTESIAN_POINT('Ctrl Pts',(-4.86323483191242,4.70855658364808,
9.0582115710072));
#185818=CARTESIAN_POINT('Ctrl Pts',(-4.98084618571305,4.58397183896925,
9.06623374402828));
#185819=CARTESIAN_POINT('Ctrl Pts',(-5.09360950959622,4.45504558492402,
9.07425591704936));
#185820=CARTESIAN_POINT('Ctrl Pts',(-5.20921156822271,4.32287370611286,
9.08248004244723));
#185821=CARTESIAN_POINT('Ctrl Pts',(-5.31971797713956,4.18613910650498,
9.09070416784509));
#185822=CARTESIAN_POINT('Ctrl Pts',(-5.42475163585204,4.04528845563832,
9.09892829324295));
#185823=CARTESIAN_POINT('Ctrl Pts',(-5.52717232123493,3.90794181480693,
9.10694782307986));
#185824=CARTESIAN_POINT('Ctrl Pts',(-5.62438910319465,3.76668181360193,
9.11496735291676));
#185825=CARTESIAN_POINT('Ctrl Pts',(-5.71609406999345,3.62195493939194,
9.12298688275367));
#185826=CARTESIAN_POINT('Ctrl Pts',(-5.8078086354572,3.47721291676829,9.13100725198655));
#185827=CARTESIAN_POINT('Ctrl Pts',(-5.89401003617417,3.3290036155374,9.13902762121942));
#185828=CARTESIAN_POINT('Ctrl Pts',(-5.97443471743049,3.17780093888231,
9.1470479904523));
#185829=CARTESIAN_POINT('Ctrl Pts',(-6.05488386691842,3.02655226065091,
9.15507079978502));
#185830=CARTESIAN_POINT('Ctrl Pts',(-6.12955262288142,2.87230872547832,
9.16309360911774));
#185831=CARTESIAN_POINT('Ctrl Pts',(-6.19822433073136,2.7155670026589,9.17111641845046));
#185832=CARTESIAN_POINT('Ctrl Pts',(-6.26992383708833,2.55191439369433,
9.17949296079609));
#185833=CARTESIAN_POINT('Ctrl Pts',(-6.33508527033752,2.38553872161157,
9.18786950314173));
#185834=CARTESIAN_POINT('Ctrl Pts',(-6.39351927512407,2.21702509652395,
9.19624604548737));
#185835=CARTESIAN_POINT('Ctrl Pts',(-6.44958553521713,2.05533964012063,
9.20428317050638));
#185836=CARTESIAN_POINT('Ctrl Pts',(-6.49945880191981,1.89168645707455,
9.21232029552539));
#185837=CARTESIAN_POINT('Ctrl Pts',(-6.54302387842973,1.72659419850132,
9.2203574205444));
#185838=CARTESIAN_POINT('Ctrl Pts',(-6.5866221466704,1.561376158035,9.22840066895652));
#185839=CARTESIAN_POINT('Ctrl Pts',(-6.62390257490159,1.39471722264299,
9.23644391736865));
#185840=CARTESIAN_POINT('Ctrl Pts',(-6.65480157814796,1.22715319152884,
9.24448716578078));
#185841=CARTESIAN_POINT('Ctrl Pts',(-6.68574475004606,1.05934963562248,
9.25254191163297));
#185842=CARTESIAN_POINT('Ctrl Pts',(-6.71028824433949,0.890638770314056,
9.26059665748516));
#185843=CARTESIAN_POINT('Ctrl Pts',(-6.72842043818449,0.721559011461451,
9.26865140333735));
#185844=CARTESIAN_POINT('Ctrl Pts',(-6.73065919378264,0.700682979586886,
9.26964591109093));
#185845=CARTESIAN_POINT('Ctrl Pts',(-6.73280027753,0.679801320340407,9.27064041884451));
#185846=CARTESIAN_POINT('Ctrl Pts',(-6.7348437224623,0.658915043089906,
9.27163492659808));
#185847=CARTESIAN_POINT('Ctrl Pts',(-6.75620283932173,0.440601141158822,
9.2820300231287));
#185848=CARTESIAN_POINT('Ctrl Pts',(-6.76694013810318,0.221339368319224,
9.29242511965931));
#185849=CARTESIAN_POINT('Ctrl Pts',(-6.76699975044675,0.00183778498507086,
9.30282021618991));
#185850=CARTESIAN_POINT('Ctrl Pts',(-6.7669997504469,0.00183778443585837,
9.30282021621592));
#185851=CARTESIAN_POINT('Ctrl Pts',(-6.7670466121356,-0.170714028257617,
9.31099187822504));
#185852=CARTESIAN_POINT('Ctrl Pts',(-6.7604893996205,-0.343535385381546,
9.31916354023416));
#185853=CARTESIAN_POINT('Ctrl Pts',(-6.74729237457982,-0.516076168735846,
9.32733520224329));
#185854=CARTESIAN_POINT('Ctrl Pts',(-6.73411098419024,-0.688412541251919,
9.3354971832005));
#185855=CARTESIAN_POINT('Ctrl Pts',(-6.71430546902278,-0.860468642160045,
9.34365916415771));
#185856=CARTESIAN_POINT('Ctrl Pts',(-6.68789204202812,-1.03169231565278,
9.35182114511491));
#185857=CARTESIAN_POINT('Ctrl Pts',(-6.6615043985982,-1.20274884852148,
9.35997515872413));
#185858=CARTESIAN_POINT('Ctrl Pts',(-6.62852174184835,-1.37297421433712,
9.36812917233336));
#185859=CARTESIAN_POINT('Ctrl Pts',(-6.58901222851907,-1.54181933196669,
9.37628318594258));
#185860=CARTESIAN_POINT('Ctrl Pts',(-6.54953304674473,-1.71053482676543,
9.38443093969459));
#185861=CARTESIAN_POINT('Ctrl Pts',(-6.5035370695623,-1.87787183037223,
9.3925786934466));
#185862=CARTESIAN_POINT('Ctrl Pts',(-6.45114387794042,-2.04328942299221,
9.40072644719861));
#185863=CARTESIAN_POINT('Ctrl Pts',(-6.39877942289436,-2.20861628750336,
9.40886973207717));
#185864=CARTESIAN_POINT('Ctrl Pts',(-6.34002485152426,-2.37202549135048,
9.41701301695572));
#185865=CARTESIAN_POINT('Ctrl Pts',(-6.27505014849156,-2.53298926841708,
9.42515630183427));
#185866=CARTESIAN_POINT('Ctrl Pts',(-6.21009406395858,-2.6939069213169,
9.43329725325473));
#185867=CARTESIAN_POINT('Ctrl Pts',(-6.13892153218648,-2.85238020490531,
9.44143820467518));
#185868=CARTESIAN_POINT('Ctrl Pts',(-6.06175145907753,-3.00789930821686,
9.44957915609563));
#185869=CARTESIAN_POINT('Ctrl Pts',(-5.98458893522756,-3.16340319767749,
9.45771931111732));
#185870=CARTESIAN_POINT('Ctrl Pts',(-5.90143020041023,-3.31595315609132,
9.46585946613901));
#185871=CARTESIAN_POINT('Ctrl Pts',(-5.81254108315226,-3.46506207111318,
9.4739996211607));
#185872=CARTESIAN_POINT('Ctrl Pts',(-5.72364388599234,-3.61418453993612,
9.4821405161116));
#185873=CARTESIAN_POINT('Ctrl Pts',(-5.62901545650814,-3.75986503006738,
9.4902814110625));
#185874=CARTESIAN_POINT('Ctrl Pts',(-5.52896607630542,-3.90164364429452,
9.4984223060134));
#185875=CARTESIAN_POINT('Ctrl Pts',(-5.42884492179168,-4.0435239689204,
9.50656904115167));
#185876=CARTESIAN_POINT('Ctrl Pts',(-5.32329525781112,-4.18149652761971,
9.51471577628994));
#185877=CARTESIAN_POINT('Ctrl Pts',(-5.21266937519114,-4.31513232531106,
9.5228625114282));
#185878=CARTESIAN_POINT('Ctrl Pts',(-5.10200169492407,-4.44881861445864,
9.53101232463782));
#185879=CARTESIAN_POINT('Ctrl Pts',(-4.98625421496092,-4.57816460423707,
9.53916213784745));
#185880=CARTESIAN_POINT('Ctrl Pts',(-4.86581739319278,-4.70277684949037,
9.54731195105707));
#185881=CARTESIAN_POINT('Ctrl Pts',(-4.74524373195729,-4.82753067829775,
9.55547102402697));
#185882=CARTESIAN_POINT('Ctrl Pts',(-4.61997034650439,-4.94753976429741,
9.56363009699687));
#185883=CARTESIAN_POINT('Ctrl Pts',(-4.49042285896871,-5.0624491649449,
9.57178916996678));
#185884=CARTESIAN_POINT('Ctrl Pts',(-4.39645591943421,-5.14579840550515,
9.57770733272705));
#185885=CARTESIAN_POINT('Ctrl Pts',(-4.30024097346765,-5.22646537689021,
9.58362549548732));
#185886=CARTESIAN_POINT('Ctrl Pts',(-4.20195024913151,-5.30432871377931,
9.5895436582476));
#185887=CARTESIAN_POINT('Ctrl Pts',(-4.0606351949001,-5.41627479769963,
9.59805235016198));
#185888=CARTESIAN_POINT('Ctrl Pts',(-3.91473401575087,-5.52265723072521,
9.60656104207637));
#185889=CARTESIAN_POINT('Ctrl Pts',(-3.76470895516439,-5.6231001665367,
9.61506973399076));
#185890=CARTESIAN_POINT('Ctrl Pts',(-3.61481639142518,-5.72345439468645,
9.62357091132826));
#185891=CARTESIAN_POINT('Ctrl Pts',(-3.46080747525354,-5.8178794036784,
9.63207208866576));
#185892=CARTESIAN_POINT('Ctrl Pts',(-3.30317592279674,-5.90604079083915,
9.64057326600325));
#185893=CARTESIAN_POINT('Ctrl Pts',(-3.14566475190075,-5.9941348500746,
9.64906795108092));
#185894=CARTESIAN_POINT('Ctrl Pts',(-2.98453674275637,-6.07597466717417,
9.65756263615859));
#185895=CARTESIAN_POINT('Ctrl Pts',(-2.82031328098179,-6.15126994994674,
9.66605732123625));
#185896=CARTESIAN_POINT('Ctrl Pts',(-2.65621759810112,-6.22650664701027,
9.67454539677438));
#185897=CARTESIAN_POINT('Ctrl Pts',(-2.4890315615849,-6.29520883418608,
9.68303347231251));
#185898=CARTESIAN_POINT('Ctrl Pts',(-2.31929997642462,-6.35713273570379,
9.69152154785064));
#185899=CARTESIAN_POINT('Ctrl Pts',(-2.14964906063651,-6.41902720626879,
9.70000558920901));
#185900=CARTESIAN_POINT('Ctrl Pts',(-1.97745531220279,-6.47414970339247,
9.70848963056739));
#185901=CARTESIAN_POINT('Ctrl Pts',(-1.80328302776581,-6.52230475535848,
9.71697367192576));
#185902=CARTESIAN_POINT('Ctrl Pts',(-1.62918098751762,-6.57044038625199,
9.72545429164559));
#185903=CARTESIAN_POINT('Ctrl Pts',(-1.45310231492341,-6.61161409100884,
9.73393491136541));
#185904=CARTESIAN_POINT('Ctrl Pts',(-1.27562634308607,-6.64568028367487,
9.74241553108523));
#185905=CARTESIAN_POINT('Ctrl Pts',(-1.23319641108622,-6.65382463258785,
9.74444302874761));
#185906=CARTESIAN_POINT('Ctrl Pts',(-1.19068667308345,-6.66156296771806,
9.74647052640999));
#185907=CARTESIAN_POINT('Ctrl Pts',(-1.14810514809912,-6.66889372901595,
9.74849802407237));
#185908=CARTESIAN_POINT('Ctrl Pts',(-0.967949600006465,-6.69990899490988,
9.75707603889821));
#185909=CARTESIAN_POINT('Ctrl Pts',(-0.786591102187406,-6.72361042674612,
9.76565405372405));
#185910=CARTESIAN_POINT('Ctrl Pts',(-0.604637011330119,-6.73993346291562,
9.77423206854989));
#185911=CARTESIAN_POINT('Ctrl Pts',(-0.422590768744204,-6.75626476598362,
9.78281442776222));
#185912=CARTESIAN_POINT('Ctrl Pts',(-0.239948640404219,-6.76521018946188,
9.79139678697455));
#185913=CARTESIAN_POINT('Ctrl Pts',(-0.0573209745920767,-6.76675722232384,
9.79997914618688));
#185914=CARTESIAN_POINT('Ctrl Pts',(0.133259757644712,-6.76837162534605,
9.8089352498294));
#185915=CARTESIAN_POINT('Ctrl Pts',(0.323824359734286,-6.76192884701384,
9.81789135347192));
#185916=CARTESIAN_POINT('Ctrl Pts',(0.513682295249814,-6.74747504623373,
9.82684745711444));
#185917=CARTESIAN_POINT('Ctrl Pts',(0.69593181631616,-6.73360047068539,
9.83544465161694));
#185918=CARTESIAN_POINT('Ctrl Pts',(0.877529900041484,-6.71234450500837,
9.84404184611944));
#185919=CARTESIAN_POINT('Ctrl Pts',(1.05787328418431,-6.68380079854338,
9.85263904062193));
#185920=CARTESIAN_POINT('Ctrl Pts',(1.23832897751235,-6.65523931643094,
9.86124158904365));
#185921=CARTESIAN_POINT('Ctrl Pts',(1.41752810691512,-6.61938109244112,
9.86984413746536));
#185922=CARTESIAN_POINT('Ctrl Pts',(1.59487830026516,-6.57637074740646,
9.87844668588707));
#185923=CARTESIAN_POINT('Ctrl Pts',(1.77241483025084,-6.53331521266639,
9.88705827275358));
#185924=CARTESIAN_POINT('Ctrl Pts',(1.94809824320536,-6.4830926229974,9.89566985962008));
#185925=CARTESIAN_POINT('Ctrl Pts',(2.12135080736073,-6.42589758338164,
9.90428144648658));
#185926=CARTESIAN_POINT('Ctrl Pts',(2.14261572578531,-6.41887749766084,
9.90533842762343));
#185927=CARTESIAN_POINT('Ctrl Pts',(2.16384404715849,-6.41175243221178,
9.90639540876027));
#185928=CARTESIAN_POINT('Ctrl Pts',(2.18503472365863,-6.40452279693078,
9.90745238989712));
#185929=CARTESIAN_POINT('Ctrl Pts',(2.36678413813419,-6.34251524473282,
9.91651796657808));
#185930=CARTESIAN_POINT('Ctrl Pts',(2.54593475176408,-6.27275261438359,
9.92558354325904));
#185931=CARTESIAN_POINT('Ctrl Pts',(2.72185240231887,-6.19546677014662,
9.93464911994));
#185932=CARTESIAN_POINT('Ctrl Pts',(2.89761150343534,-6.11825058138286,
9.94370652608159));
#185933=CARTESIAN_POINT('Ctrl Pts',(3.07014324523132,-6.0335248106319,9.95276393222317));
#185934=CARTESIAN_POINT('Ctrl Pts',(3.23883345735384,-5.94156939162755,
9.96182133836476));
#185935=CARTESIAN_POINT('Ctrl Pts',(3.40722154298656,-5.84977866604324,
9.97086252256739));
#185936=CARTESIAN_POINT('Ctrl Pts',(3.57178163311142,-5.75078426082011,
9.97990370677001));
#185937=CARTESIAN_POINT('Ctrl Pts',(3.73192432653554,-5.64491185236867,
9.98894489097264));
#185938=CARTESIAN_POINT('Ctrl Pts',(3.89186057977518,-5.53917592419656,
9.99797442017125));
#185939=CARTESIAN_POINT('Ctrl Pts',(4.04739060635348,-5.42657981625096,
10.0070039493699));
#185940=CARTESIAN_POINT('Ctrl Pts',(4.19795190901923,-5.30749364291299,
10.0160334785685));
#185941=CARTESIAN_POINT('Ctrl Pts',(4.34815902017713,-5.18868761666828,
10.0250417660369));
#185942=CARTESIAN_POINT('Ctrl Pts',(4.49342055584514,-5.06342214512154,
10.0340500535054));
#185943=CARTESIAN_POINT('Ctrl Pts',(4.63320559190143,-4.93210856968633,
10.0430583409739));
#185944=CARTESIAN_POINT('Ctrl Pts',(4.75397434729608,-4.81865882199413,
10.0508411458899));
#185945=CARTESIAN_POINT('Ctrl Pts',(4.87065564734211,-4.70069533661137,
10.0586239508059));
#185946=CARTESIAN_POINT('Ctrl Pts',(4.98292550652445,-4.57850875246822,
10.0664067557219));
#185947=CARTESIAN_POINT('Ctrl Pts',(5.10004581894295,-4.45104327765228,
10.0745258052147));
#185948=CARTESIAN_POINT('Ctrl Pts',(5.21231002407704,-4.31903948992084,
10.0826448547076));
#185949=CARTESIAN_POINT('Ctrl Pts',(5.31935417212587,-4.18291288356417,
10.0907639042004));
#185950=CARTESIAN_POINT('Ctrl Pts',(5.42639055612429,-4.04679615064619,
10.0988823648081));
#185951=CARTESIAN_POINT('Ctrl Pts',(5.52820741067156,-3.90655748276577,
10.1070008254158));
#185952=CARTESIAN_POINT('Ctrl Pts',(5.6244815288003,-3.76264488520831,10.1151192860235));
#185953=CARTESIAN_POINT('Ctrl Pts',(5.72076706314787,-3.61871522244435,
10.1232387093211));
#185954=CARTESIAN_POINT('Ctrl Pts',(5.81150834959695,-3.47111106775377,
10.1313581326187));
#185955=CARTESIAN_POINT('Ctrl Pts',(5.89642594444674,-3.32030873288244,
10.1394775559163));
#185956=CARTESIAN_POINT('Ctrl Pts',(5.9814054677032,-3.1693964214116,10.1476029005185));
#185957=CARTESIAN_POINT('Ctrl Pts',(6.06055263682131,-3.01528159103643,
10.1557282451207));
#185958=CARTESIAN_POINT('Ctrl Pts',(6.133634063267,-2.85846500379676,10.163853589723));
#185959=CARTESIAN_POINT('Ctrl Pts',(6.20674523183145,-2.70158459654443,
10.1719822411157));
#185960=CARTESIAN_POINT('Ctrl Pts',(6.2737855953791,-2.54200057835911,10.1801108925084));
#185961=CARTESIAN_POINT('Ctrl Pts',(6.33457033879776,-2.38023268249633,
10.1882395439011));
#185962=CARTESIAN_POINT('Ctrl Pts',(6.39542148463189,-2.21828806829228,
10.1963770751879));
#185963=CARTESIAN_POINT('Ctrl Pts',(6.45000324561459,-2.05415515866025,
10.2045146064748));
#185964=CARTESIAN_POINT('Ctrl Pts',(6.49818077163492,-1.88836851783601,
10.2126521377616));
#185965=CARTESIAN_POINT('Ctrl Pts',(6.52326157216328,-1.80206143625145,
10.21688846569));
#185966=CARTESIAN_POINT('Ctrl Pts',(6.54660756825064,-1.71530635134659,
10.2211247936183));
#185967=CARTESIAN_POINT('Ctrl Pts',(6.56820525017969,-1.62817959436664,
10.2253611215467));
#185968=CARTESIAN_POINT('Ctrl Pts',(6.6112308218627,-1.45461103546927,10.2338004731193));
#185969=CARTESIAN_POINT('Ctrl Pts',(6.64740423022982,-1.27920682544239,
10.242239824692));
#185970=CARTESIAN_POINT('Ctrl Pts',(6.67657888614868,-1.10253497769171,
10.2506791762646));
#185971=CARTESIAN_POINT('Ctrl Pts',(6.70573136685457,-0.925997415529906,
10.2591121132143));
#185972=CARTESIAN_POINT('Ctrl Pts',(6.72789564526412,-0.748194464282019,
10.267545050164));
#185973=CARTESIAN_POINT('Ctrl Pts',(6.74297595893689,-0.569705377540964,
10.2759779871137));
#185974=CARTESIAN_POINT('Ctrl Pts',(6.75804713251623,-0.391324472033178,
10.2844058129076));
#185975=CARTESIAN_POINT('Ctrl Pts',(6.76604287311658,-0.21225859168572,
10.2928336387016));
#185976=CARTESIAN_POINT('Ctrl Pts',(6.76691907851943,-0.0330935759595899,
10.3012614644955));
#185977=CARTESIAN_POINT('Ctrl Pts',(6.76779488763841,0.145990408305047,
10.3096854786132));
#185978=CARTESIAN_POINT('Ctrl Pts',(6.7615575801646,0.325173105515606,10.3181094927308));
#185979=CARTESIAN_POINT('Ctrl Pts',(6.74821511557709,0.503866801741148,
10.3265335068485));
#185980=CARTESIAN_POINT('Ctrl Pts',(6.73487663477628,0.682507143688387,
10.334955005728));
#185981=CARTESIAN_POINT('Ctrl Pts',(6.71443725230049,0.860658443502518,
10.3433765046076));
#185982=CARTESIAN_POINT('Ctrl Pts',(6.68695695545498,1.0377358410946,10.3517980034871));
#185983=CARTESIAN_POINT('Ctrl Pts',(6.65947627551724,1.21481570725446,10.3602196197676));
#185984=CARTESIAN_POINT('Ctrl Pts',(6.62495452963571,1.39082131068888,10.368641236048));
#185985=CARTESIAN_POINT('Ctrl Pts',(6.58350332138551,1.56517507560848,10.3770628523284));
#185986=CARTESIAN_POINT('Ctrl Pts',(6.54205075252875,1.73953456356692,10.3854847450424));
#185987=CARTESIAN_POINT('Ctrl Pts',(6.49366834479376,1.91224178021917,10.3939066377564));
#185988=CARTESIAN_POINT('Ctrl Pts',(6.4385184055237,2.08273131770102,10.4023285304705));
#185989=CARTESIAN_POINT('Ctrl Pts',(6.38335894358225,2.25325029339914,10.4107518773822));
#185990=CARTESIAN_POINT('Ctrl Pts',(6.3214297230832,2.42155050901785,10.419175224294));
#185991=CARTESIAN_POINT('Ctrl Pts',(6.25294243045065,2.58708329233327,10.4275985712057));
#185992=CARTESIAN_POINT('Ctrl Pts',(6.18443373173197,2.75266781384539,10.4360245508816));
#185993=CARTESIAN_POINT('Ctrl Pts',(6.10936300174402,2.91548287032578,10.4444505305575));
#185994=CARTESIAN_POINT('Ctrl Pts',(6.027989562113,3.07500094943997,10.4528765102334));
#185995=CARTESIAN_POINT('Ctrl Pts',(5.94654295224503,3.23466246572113,10.4613100664716));
#185996=CARTESIAN_POINT('Ctrl Pts',(5.85878246027435,3.39102078335486,10.4697436227097));
#185997=CARTESIAN_POINT('Ctrl Pts',(5.76501331348837,3.54357312543453,10.4781771789479));
#185998=CARTESIAN_POINT('Ctrl Pts',(5.67119887575865,3.69619915102077,10.4866148086338));
#185999=CARTESIAN_POINT('Ctrl Pts',(5.57137017663366,3.84501525498488,10.4950524383197));
#186000=CARTESIAN_POINT('Ctrl Pts',(5.46587535680585,3.98954829321097,10.5034900680056));
#186001=CARTESIAN_POINT('Ctrl Pts',(5.36026250784733,4.13424303709131,10.5119371378337));
#186002=CARTESIAN_POINT('Ctrl Pts',(5.24897107439376,4.27464487543108,10.5203842076617));
#186003=CARTESIAN_POINT('Ctrl Pts',(5.13238976466265,4.41031340196885,10.5288312774898));
#186004=CARTESIAN_POINT('Ctrl Pts',(5.06596562387541,4.48761280208648,10.5336441360586));
#186005=CARTESIAN_POINT('Ctrl Pts',(4.99782491158918,4.56337625664566,10.5384569946274));
#186006=CARTESIAN_POINT('Ctrl Pts',(4.92804479460896,4.63752773601707,10.5432698531962));
#186007=CARTESIAN_POINT('Ctrl Pts',(4.80851785790511,4.76454241533947,10.5515138382511));
#186008=CARTESIAN_POINT('Ctrl Pts',(4.68391210280518,4.88710868455191,10.559757823306));
#186009=CARTESIAN_POINT('Ctrl Pts',(4.55459000775174,5.00479758444715,10.5680018083609));
#186010=CARTESIAN_POINT('Ctrl Pts',(4.42545716313932,5.12231425796298,10.5762337291371));
#186011=CARTESIAN_POINT('Ctrl Pts',(4.29162199506258,5.2349675498427,10.5844656499132));
#186012=CARTESIAN_POINT('Ctrl Pts',(4.1534854404704,5.34236349341754,10.5926975706893));
#186013=CARTESIAN_POINT('Ctrl Pts',(4.01546585408141,5.44966849864093,10.6009225210225));
#186014=CARTESIAN_POINT('Ctrl Pts',(3.87315241089694,5.5517248007974,10.6091474713556));
#186015=CARTESIAN_POINT('Ctrl Pts',(3.72698151371424,5.6481765018838,10.6173724216887));
#186016=CARTESIAN_POINT('Ctrl Pts',(3.58093181984589,5.74454822627121,10.6255905519827));
#186017=CARTESIAN_POINT('Ctrl Pts',(3.43103134131578,5.83532441488182,10.6338086822767));
#186018=CARTESIAN_POINT('Ctrl Pts',(3.27774791139971,5.9201906750809,10.6420268125707));
#186019=CARTESIAN_POINT('Ctrl Pts',(3.21869317985551,5.95288666978797,10.6451929700514));
#186020=CARTESIAN_POINT('Ctrl Pts',(3.15913664059974,5.98470590510722,10.6483591275322));
#186021=CARTESIAN_POINT('Ctrl Pts',(3.09910619832133,6.01563211736941,10.651525285013));
#186022=CARTESIAN_POINT('Origin',(0.,0.,4.30282021618968));
#186023=CARTESIAN_POINT('',(3.09910619832134,6.0156321173694,13.0454981451509));
#186024=CARTESIAN_POINT('',(3.09910619832132,6.01563211736941,12.6513039064363));
#186025=CARTESIAN_POINT('',(3.09910619832133,6.0156321173694,4.30282021618968));
#186026=CARTESIAN_POINT('',(-6.76699966505605,-0.00196815110624866,11.69717978381));
#186027=CARTESIAN_POINT('Ctrl Pts',(-6.76699960802935,-0.0023032435072958,
11.69717978381));
#186028=CARTESIAN_POINT('Ctrl Pts',(-6.76693681242208,-0.186798651139549,
11.7058298775953));
#186029=CARTESIAN_POINT('Ctrl Pts',(-6.75932464309069,-0.371131808236207,
11.7144799713807));
#186030=CARTESIAN_POINT('Ctrl Pts',(-6.74422821643248,-0.554684382938594,
11.723130065166));
#186031=CARTESIAN_POINT('Ctrl Pts',(-6.72911430810714,-0.738449511584034,
11.7317901757629));
#186032=CARTESIAN_POINT('Ctrl Pts',(-6.70649887319034,-0.92143195827289,
11.7404502863597));
#186033=CARTESIAN_POINT('Ctrl Pts',(-6.67649843439857,-1.10302205575116,
11.7491103969565));
#186034=CARTESIAN_POINT('Ctrl Pts',(-6.64643861478435,-1.28497158028351,
11.7577876487857));
#186035=CARTESIAN_POINT('Ctrl Pts',(-6.60896462059164,-1.46552295301023,
11.7664649006148));
#186036=CARTESIAN_POINT('Ctrl Pts',(-6.56424377347403,-1.64407806457217,
11.7751421524439));
#186037=CARTESIAN_POINT('Ctrl Pts',(-6.53831776864942,-1.74759177198564,
11.7801726133427));
#186038=CARTESIAN_POINT('Ctrl Pts',(-6.50995711894902,-1.85043486796765,
11.7852030742415));
#186039=CARTESIAN_POINT('Ctrl Pts',(-6.47920190307687,-1.95249371296429,
11.7902335351403));
#186040=CARTESIAN_POINT('Ctrl Pts',(-6.42760020303839,-2.12373003033185,
11.7986737403866));
#186041=CARTESIAN_POINT('Ctrl Pts',(-6.36916780679982,-2.29304635343699,
11.8071139456329));
#186042=CARTESIAN_POINT('Ctrl Pts',(-6.30406874060674,-2.45987932909422,
11.8155541508792));
#186043=CARTESIAN_POINT('Ctrl Pts',(-6.23901899736336,-2.62658590210163,
11.8239879613207));
#186044=CARTESIAN_POINT('Ctrl Pts',(-6.16731277392029,-2.79081256881585,
11.8324217717622));
#186045=CARTESIAN_POINT('Ctrl Pts',(-6.08916353704902,-2.95201226607761,
11.8408555822037));
#186046=CARTESIAN_POINT('Ctrl Pts',(-6.0110614969762,-3.11311460973843,
11.8492842992001));
#186047=CARTESIAN_POINT('Ctrl Pts',(-5.9265243461337,-3.27119332916337,
11.8577130161965));
#186048=CARTESIAN_POINT('Ctrl Pts',(-5.83581333221124,-3.42572207739997,
11.8661417331929));
#186049=CARTESIAN_POINT('Ctrl Pts',(-5.74514317202579,-3.58018123015341,
11.8745666541277));
#186050=CARTESIAN_POINT('Ctrl Pts',(-5.64830486138084,-3.73109331244725,
11.8829915750626));
#186051=CARTESIAN_POINT('Ctrl Pts',(-5.54560536888083,-3.87795694827059,
11.8914164959975));
#186052=CARTESIAN_POINT('Ctrl Pts',(-5.44293637211757,-4.02477697419219,
11.8998389152241));
#186053=CARTESIAN_POINT('Ctrl Pts',(-5.33440985519956,-4.16755067799563,
11.9082613344507));
#186054=CARTESIAN_POINT('Ctrl Pts',(-5.22037606490862,-4.30580570171591,
11.9166837536773));
#186055=CARTESIAN_POINT('Ctrl Pts',(-5.10634048214024,-4.444062898643,11.9251063052944));
#186056=CARTESIAN_POINT('Ctrl Pts',(-4.98679766004418,-4.57780101213762,
11.9335288569116));
#186057=CARTESIAN_POINT('Ctrl Pts',(-4.86213850888825,-4.70658030000402,
11.9419514085287));
#186058=CARTESIAN_POINT('Ctrl Pts',(-4.73747514726915,-4.83536393749453,
11.9503742446243));
#186059=CARTESIAN_POINT('Ctrl Pts',(-4.60769534391517,-4.95918817560475,
11.9587970807199));
#186060=CARTESIAN_POINT('Ctrl Pts',(-4.4732273948143,-5.07764962106316,
11.9672199168155));
#186061=CARTESIAN_POINT('Ctrl Pts',(-4.33873613058136,-5.1961316063176,
11.9756442133301));
#186062=CARTESIAN_POINT('Ctrl Pts',(-4.19955535026871,-5.30924872459061,
11.9840685098446));
#186063=CARTESIAN_POINT('Ctrl Pts',(-4.05614726551665,-5.41663718190925,
11.9924928063591));
#186064=CARTESIAN_POINT('Ctrl Pts',(-3.91269428786376,-5.52405925643556,
12.0009197400409));
#186065=CARTESIAN_POINT('Ctrl Pts',(-3.76501163431016,-5.62574889475977,
12.0093466737227));
#186066=CARTESIAN_POINT('Ctrl Pts',(-3.61359167504872,-5.72138481541127,
12.0177736074045));
#186067=CARTESIAN_POINT('Ctrl Pts',(-3.46203557008112,-5.81710672485853,
12.0262081179661));
#186068=CARTESIAN_POINT('Ctrl Pts',(-3.30673572726618,-5.90676386224585,
12.0346426285277));
#186069=CARTESIAN_POINT('Ctrl Pts',(-3.14821136361916,-5.99007964971913,
12.0430771390894));
#186070=CARTESIAN_POINT('Ctrl Pts',(-2.98961043129991,-6.07343567945597,
12.0515157235944));
#186071=CARTESIAN_POINT('Ctrl Pts',(-2.82778217076928,-6.15044410274545,
12.0599543080993));
#186072=CARTESIAN_POINT('Ctrl Pts',(-2.66326757435415,-6.2208757283355,
12.0683928926043));
#186073=CARTESIAN_POINT('Ctrl Pts',(-2.49856908691915,-6.29138608094275,
12.0768409095848));
#186074=CARTESIAN_POINT('Ctrl Pts',(-2.33117857343359,-6.35530482272349,
12.0852889265654));
#186075=CARTESIAN_POINT('Ctrl Pts',(-2.16165519938208,-6.41245162157068,
12.0937369435459));
#186076=CARTESIAN_POINT('Ctrl Pts',(-2.0652996875405,-6.44493333144601,
12.0985387179605));
#186077=CARTESIAN_POINT('Ctrl Pts',(-1.96825538871769,-6.47522815707328,
12.1033404923752));
#186078=CARTESIAN_POINT('Ctrl Pts',(-1.87062672729887,-6.50331028377973,
12.1081422667898));
#186079=CARTESIAN_POINT('Ctrl Pts',(-1.70310221153925,-6.55149741048647,
12.1163818034373));
#186080=CARTESIAN_POINT('Ctrl Pts',(-1.53348245935107,-6.59327404759384,
12.1246213400847));
#186081=CARTESIAN_POINT('Ctrl Pts',(-1.36229741557804,-6.62845643807888,
12.1328608767322));
#186082=CARTESIAN_POINT('Ctrl Pts',(-1.19130237552393,-6.66359977851093,
12.1410912680561));
#186083=CARTESIAN_POINT('Ctrl Pts',(-1.01874584882209,-6.69216337498689,
12.14932165938));
#186084=CARTESIAN_POINT('Ctrl Pts',(-0.845173570896423,-6.7140130052792,
12.157552050704));
#186085=CARTESIAN_POINT('Ctrl Pts',(-0.671762982778306,-6.73584228173067,
12.1657747750755));
#186086=CARTESIAN_POINT('Ctrl Pts',(-0.497338878882295,-6.75097000343168,
12.1739974994471));
#186087=CARTESIAN_POINT('Ctrl Pts',(-0.322457933687271,-6.75931282609424,
12.1822202238186));
#186088=CARTESIAN_POINT('Ctrl Pts',(-0.147731946550763,-6.76764825636994,
12.1904356622197));
#186089=CARTESIAN_POINT('Ctrl Pts',(0.0274497209401242,-6.76921075308692,
12.1986511006208));
#186090=CARTESIAN_POINT('Ctrl Pts',(0.202524641810431,-6.76396871440574,
12.2068665390219));
#186091=CARTESIAN_POINT('Ctrl Pts',(0.377509587208122,-6.75872936974209,
12.2150777552993));
#186092=CARTESIAN_POINT('Ctrl Pts',(0.552387540366576,-6.74669246493872,
12.2232889715768));
#186093=CARTESIAN_POINT('Ctrl Pts',(0.726595016490422,-6.72787846813624,
12.2315001878543));
#186094=CARTESIAN_POINT('Ctrl Pts',(0.900744071880028,-6.70907078063536,
12.2397086504883));
#186095=CARTESIAN_POINT('Ctrl Pts',(1.07422274467752,-6.68349056674038,
12.2479171131223));
#186096=CARTESIAN_POINT('Ctrl Pts',(1.2464715234989,-6.65121024634663,12.2561255757563));
#186097=CARTESIAN_POINT('Ctrl Pts',(1.32321147796168,-6.6368287782514,12.2597825947091));
#186098=CARTESIAN_POINT('Ctrl Pts',(1.39970739264354,-6.62111811727423,
12.2634396136618));
#186099=CARTESIAN_POINT('Ctrl Pts',(1.47591029112141,-6.60408796220659,
12.2670966326146));
#186100=CARTESIAN_POINT('Ctrl Pts',(1.66051062433008,-6.56283267713372,
12.2759557039979));
#186101=CARTESIAN_POINT('Ctrl Pts',(1.84319879724182,-6.51387371439261,
12.2848147753813));
#186102=CARTESIAN_POINT('Ctrl Pts',(2.02335685831665,-6.457423326986,12.2936738467646));
#186103=CARTESIAN_POINT('Ctrl Pts',(2.20385339789918,-6.40086688136156,
12.3025495624504));
#186104=CARTESIAN_POINT('Ctrl Pts',(2.38181007859704,-6.3367909609365,12.3114252781362));
#186105=CARTESIAN_POINT('Ctrl Pts',(2.55662797381253,-6.26545628055286,
12.320300993822));
#186106=CARTESIAN_POINT('Ctrl Pts',(2.7319447475375,-6.19391803211355,12.3292020381723));
#186107=CARTESIAN_POINT('Ctrl Pts',(2.90410456971904,-6.11507966997994,
12.3381030825226));
#186108=CARTESIAN_POINT('Ctrl Pts',(3.07252943976385,-6.02924969144457,
12.3470041268729));
#186109=CARTESIAN_POINT('Ctrl Pts',(3.24118328471917,-5.94330302639106,
12.3559172722616));
#186110=CARTESIAN_POINT('Ctrl Pts',(3.40609180655076,-5.85034588128721,
12.3648304176504));
#186111=CARTESIAN_POINT('Ctrl Pts',(3.5667040062172,-5.75073139105229,12.3737435630391));
#186112=CARTESIAN_POINT('Ctrl Pts',(3.72767280825489,-5.65089572980107,
12.3826764980129));
#186113=CARTESIAN_POINT('Ctrl Pts',(3.88432598718312,-5.54437329570926,
12.3916094329867));
#186114=CARTESIAN_POINT('Ctrl Pts',(4.03614143131697,-5.43156067317733,
12.4005423679605));
#186115=CARTESIAN_POINT('Ctrl Pts',(4.18064802691937,-5.3241791869519,12.4090452447868));
#186116=CARTESIAN_POINT('Ctrl Pts',(4.32077158341717,-5.21109902508388,
12.4175481216131));
#186117=CARTESIAN_POINT('Ctrl Pts',(4.45609154240944,-5.09269448972418,
12.4260509984394));
#186118=CARTESIAN_POINT('Ctrl Pts',(4.58695297837985,-4.97819114788188,
12.4342737224163));
#186119=CARTESIAN_POINT('Ctrl Pts',(4.71357229982678,-4.85848830038076,
12.4424964463933));
#186120=CARTESIAN_POINT('Ctrl Pts',(4.83551168253833,-4.73393237890397,
12.4507191703703));
#186121=CARTESIAN_POINT('Ctrl Pts',(4.95732199654481,-4.60950829564987,
12.4589331908725));
#186122=CARTESIAN_POINT('Ctrl Pts',(5.07446198707429,-4.48024162167048,
12.4671472113747));
#186123=CARTESIAN_POINT('Ctrl Pts',(5.18652721610824,-4.34651865710577,
12.475361231877));
#186124=CARTESIAN_POINT('Ctrl Pts',(5.29849632742207,-4.21291038597981,
12.4835682072598));
#186125=CARTESIAN_POINT('Ctrl Pts',(5.40539911670082,-4.07485370976442,
12.4917751826426));
#186126=CARTESIAN_POINT('Ctrl Pts',(5.5068682599934,-3.93277141047853,12.4999821580254));
#186127=CARTESIAN_POINT('Ctrl Pts',(5.60827074008092,-3.79078245643184,
12.5081837415889));
#186128=CARTESIAN_POINT('Ctrl Pts',(5.70424647705759,-3.6447734382238,12.5163853251524));
#186129=CARTESIAN_POINT('Ctrl Pts',(5.79446863718678,-3.49519988164609,
12.524586908716));
#186130=CARTESIAN_POINT('Ctrl Pts',(5.88464962833072,-3.34569457649945,
12.5327847498411));
#186131=CARTESIAN_POINT('Ctrl Pts',(5.96908208815702,-3.19262827995006,
12.5409825909663));
#186132=CARTESIAN_POINT('Ctrl Pts',(6.04748266452477,-3.03648520863719,
12.5491804320915));
#186133=CARTESIAN_POINT('Ctrl Pts',(6.12587632227628,-2.88035591648308,
12.5573775497817));
#186134=CARTESIAN_POINT('Ctrl Pts',(6.1982389883186,-2.72115070687866,12.5655746674719));
#186135=CARTESIAN_POINT('Ctrl Pts',(6.26433325423851,-2.55937841669448,
12.5737717851621));
#186136=CARTESIAN_POINT('Ctrl Pts',(6.33042678478087,-2.39760792642003,
12.5819688116496));
#186137=CARTESIAN_POINT('Ctrl Pts',(6.39025191740379,-2.23327074422573,
12.5901658381371));
#186138=CARTESIAN_POINT('Ctrl Pts',(6.44361944974623,-2.06689559166691,
12.5983628646246));
#186139=CARTESIAN_POINT('Ctrl Pts',(6.49699609214695,-1.90049203818212,
12.6065612903784));
#186140=CARTESIAN_POINT('Ctrl Pts',(6.54391282847634,-1.73205016292751,
12.6147597161322));
#186141=CARTESIAN_POINT('Ctrl Pts',(6.58423036489251,-1.56211379291891,
12.622958141886));
#186142=CARTESIAN_POINT('Ctrl Pts',(6.62456211470853,-1.39211751415121,
12.6311594578835));
#186143=CARTESIAN_POINT('Ctrl Pts',(6.65828994749948,-1.22062604003942,
12.6393607738809));
#186144=CARTESIAN_POINT('Ctrl Pts',(6.68532569457477,-1.04819337789283,
12.6475620898783));
#186145=CARTESIAN_POINT('Ctrl Pts',(6.71239223083345,-0.875564343852308,
12.6557727457998));
#186146=CARTESIAN_POINT('Ctrl Pts',(6.73275140000822,-0.701992335270251,
12.6639834017212));
#186147=CARTESIAN_POINT('Ctrl Pts',(6.74636682694953,-0.528037532979418,
12.6721940576426));
#186148=CARTESIAN_POINT('Ctrl Pts',(6.75999027713044,-0.353980223358749,
12.6804095519036));
#186149=CARTESIAN_POINT('Ctrl Pts',(6.76686204957201,-0.179540028349648,
12.6886250461647));
#186150=CARTESIAN_POINT('Ctrl Pts',(6.76699794245695,-0.00527700516096534,
12.6968405404257));
#186151=CARTESIAN_POINT('Ctrl Pts',(6.76713404618214,0.169256390256702,
12.7050687811746));
#186152=CARTESIAN_POINT('Ctrl Pts',(6.76051339906589,0.343611706188307,
12.7132970219234));
#186153=CARTESIAN_POINT('Ctrl Pts',(6.74720380957269,0.517232783268677,
12.7215252626722));
#186154=CARTESIAN_POINT('Ctrl Pts',(6.73510751985823,0.675026594262806,
12.7290034184778));
#186155=CARTESIAN_POINT('Ctrl Pts',(6.71748690659344,0.832213821742122,
12.7364815742833));
#186156=CARTESIAN_POINT('Ctrl Pts',(6.69442928804816,0.988385303069121,
12.7439597300889));
#186157=CARTESIAN_POINT('Ctrl Pts',(6.66954798240274,1.15690879357467,12.7520293527126));
#186158=CARTESIAN_POINT('Ctrl Pts',(6.63825329605563,1.32480105408137,12.7600989753363));
#186159=CARTESIAN_POINT('Ctrl Pts',(6.60057929905731,1.49152335444544,12.76816859796));
#186160=CARTESIAN_POINT('Ctrl Pts',(6.56295259957615,1.65803634463562,12.7762280896408));
#186161=CARTESIAN_POINT('Ctrl Pts',(6.51896260661402,1.82338193789948,12.7842875813216));
#186162=CARTESIAN_POINT('Ctrl Pts',(6.46869516395212,1.98702588706401,12.7923470730023));
#186163=CARTESIAN_POINT('Ctrl Pts',(6.41847979680908,2.15050030614881,12.8003982152985));
#186164=CARTESIAN_POINT('Ctrl Pts',(6.36200003066915,2.31227623564346,12.8084493575947));
#186165=CARTESIAN_POINT('Ctrl Pts',(6.29939281912488,2.47182910217473,12.8165004998909));
#186166=CARTESIAN_POINT('Ctrl Pts',(6.23683674710517,2.63125164094448,12.8245450657627));
#186167=CARTESIAN_POINT('Ctrl Pts',(6.16816332754824,2.78845438547341,12.8325896316345));
#186168=CARTESIAN_POINT('Ctrl Pts',(6.09355943013832,2.94292753416941,12.8406341975064));
#186169=CARTESIAN_POINT('Ctrl Pts',(6.01900014046277,3.09730831909588,12.8486739533097));
#186170=CARTESIAN_POINT('Ctrl Pts',(5.93851759428498,3.24896242225308,12.8567137091131));
#186171=CARTESIAN_POINT('Ctrl Pts',(5.85234686621959,3.39739976415048,12.8647534649164));
#186172=CARTESIAN_POINT('Ctrl Pts',(5.76619954440878,3.54579678652997,12.8727910369089));
#186173=CARTESIAN_POINT('Ctrl Pts',(5.67436729919539,3.6909784619495,12.8808286089013));
#186174=CARTESIAN_POINT('Ctrl Pts',(5.57713129273385,3.83247903368158,12.8888661808938));
#186175=CARTESIAN_POINT('Ctrl Pts',(5.47990580844396,3.97396429325349,12.8969028831189));
#186176=CARTESIAN_POINT('Ctrl Pts',(5.37727793763501,4.11176893377874,12.9049395853439));
#186177=CARTESIAN_POINT('Ctrl Pts',(5.26957222086834,4.24545611319358,12.912976287569));
#186178=CARTESIAN_POINT('Ctrl Pts',(5.16185682403204,4.37915530776643,12.921013712094));
#186179=CARTESIAN_POINT('Ctrl Pts',(5.04906290737038,4.50873601391433,12.929051136619));
#186180=CARTESIAN_POINT('Ctrl Pts',(4.93155524625363,4.63379454153379,12.937088561144));
#186181=CARTESIAN_POINT('Ctrl Pts',(4.81401374286677,4.758889086077,12.9451283004517));
#186182=CARTESIAN_POINT('Ctrl Pts',(4.69175604904061,4.8794585882599,12.9531680397593));
#186183=CARTESIAN_POINT('Ctrl Pts',(4.56518360805953,4.99513639700705,12.961207779067));
#186184=CARTESIAN_POINT('Ctrl Pts',(4.43848484523008,5.11092965453992,12.9692555421966));
#186185=CARTESIAN_POINT('Ctrl Pts',(4.30746301304585,5.22182121893857,12.9773033053262));
#186186=CARTESIAN_POINT('Ctrl Pts',(4.172552946396,5.32748448233518,12.9853510684558));
#186187=CARTESIAN_POINT('Ctrl Pts',(4.037566819994,5.43320731668764,12.9934033687625));
#186188=CARTESIAN_POINT('Ctrl Pts',(3.89868839502885,5.53369576138043,13.0014556690692));
#186189=CARTESIAN_POINT('Ctrl Pts',(3.75638081995438,5.62866699454488,13.0095079693759));
#186190=CARTESIAN_POINT('Ctrl Pts',(3.61388392645767,5.7237645723822,13.0175709820343));
#186191=CARTESIAN_POINT('Ctrl Pts',(3.46794909182187,5.81333009010918,13.0256339946927));
#186192=CARTESIAN_POINT('Ctrl Pts',(3.31906400050988,5.89712668682973,13.0336970073511));
#186193=CARTESIAN_POINT('Ctrl Pts',(3.24642723501661,5.93800864278306,13.037630719951));
#186194=CARTESIAN_POINT('Ctrl Pts',(3.17308856489218,5.97751821573234,13.041564432551));
#186195=CARTESIAN_POINT('Ctrl Pts',(3.09910619832134,6.0156321173694,13.0454981451509));
#186196=CARTESIAN_POINT('Ctrl Pts',(3.09910619832133,6.01563211736941,11.0457552630241));
#186197=CARTESIAN_POINT('Ctrl Pts',(2.9337533076482,6.10081787314656,11.0545047109264));
#186198=CARTESIAN_POINT('Ctrl Pts',(2.76488627843059,6.17918207037044,11.0632541588287));
#186199=CARTESIAN_POINT('Ctrl Pts',(2.59307866646686,6.25045854554004,11.072003606731));
#186200=CARTESIAN_POINT('Ctrl Pts',(2.42127244185365,6.32173444515041,11.0807529839813));
#186201=CARTESIAN_POINT('Ctrl Pts',(2.24652594672458,6.3859226274184,11.0895023612316));
#186202=CARTESIAN_POINT('Ctrl Pts',(2.06943269687119,6.44280508110562,11.0982517384819));
#186203=CARTESIAN_POINT('Ctrl Pts',(1.89234081822068,6.49968709436169,11.1070010479873));
#186204=CARTESIAN_POINT('Ctrl Pts',(1.71290249405572,6.54926340459549,11.1157503574927));
#186205=CARTESIAN_POINT('Ctrl Pts',(1.53172716625035,6.59136563150389,11.124499666998));
#186206=CARTESIAN_POINT('Ctrl Pts',(1.35055318107315,6.63346754640714,11.1332489116653));
#186207=CARTESIAN_POINT('Ctrl Pts',(1.16764249714404,6.66809542395778,11.1419981563325));
#186208=CARTESIAN_POINT('Ctrl Pts',(0.983616340614246,6.6951316562467,11.1507474009997));
#186209=CARTESIAN_POINT('Ctrl Pts',(0.79959148671368,6.72216769715963,11.1594965837354));
#186210=CARTESIAN_POINT('Ctrl Pts',(0.614451459526498,6.74161215869373,
11.1682457664711));
#186211=CARTESIAN_POINT('Ctrl Pts',(0.428825047910016,6.75339900185714,
11.1769949492068));
#186212=CARTESIAN_POINT('Ctrl Pts',(0.24319988859665,6.76518576550223,11.1857440729174));
#186213=CARTESIAN_POINT('Ctrl Pts',(0.0570886373913931,6.76931499599835,
11.1944931966279));
#186214=CARTESIAN_POINT('Ctrl Pts',(-0.128876626811801,6.76577266947846,
11.2032423203384));
#186215=CARTESIAN_POINT('Ctrl Pts',(-0.314840698188869,6.7622303656799,
11.21199138793));
#186216=CARTESIAN_POINT('Ctrl Pts',(-0.500658497952018,6.75101660879217,
11.2207404555215));
#186217=CARTESIAN_POINT('Ctrl Pts',(-0.685698951927038,6.7321694829621,
11.2294895231131));
#186218=CARTESIAN_POINT('Ctrl Pts',(-0.870738280460472,6.71332247176285,
11.2382385374916));
#186219=CARTESIAN_POINT('Ctrl Pts',(-1.05499998761293,6.68684221356179,
11.2469875518701));
#186220=CARTESIAN_POINT('Ctrl Pts',(-1.23785829161442,6.65281863948518,
11.2557365662486));
#186221=CARTESIAN_POINT('Ctrl Pts',(-1.43007412917425,6.61705395368857,
11.2649332999478));
#186222=CARTESIAN_POINT('Ctrl Pts',(-1.62073882535812,6.57295372727785,
11.274130033647));
#186223=CARTESIAN_POINT('Ctrl Pts',(-1.80913696091533,6.52068343478274,
11.2833267673462));
#186224=CARTESIAN_POINT('Ctrl Pts',(-1.9883835618613,6.47095219815193,11.2920767650599));
#186225=CARTESIAN_POINT('Ctrl Pts',(-2.16557827572549,6.41382586850885,
11.3008267627735));
#186226=CARTESIAN_POINT('Ctrl Pts',(-2.34011918621715,6.34949849943272,
11.3095767604872));
#186227=CARTESIAN_POINT('Ctrl Pts',(-2.51465655691113,6.28517243495545,
11.3183265807455));
#186228=CARTESIAN_POINT('Ctrl Pts',(-2.68653996295343,6.21364572242368,
11.3270764010038));
#186229=CARTESIAN_POINT('Ctrl Pts',(-2.85518555380003,6.13516132252214,
11.3358262212621));
#186230=CARTESIAN_POINT('Ctrl Pts',(-3.02382794858707,6.05667841000498,
11.3445758756996));
#186231=CARTESIAN_POINT('Ctrl Pts',(-3.18923239109303,5.97123819492069,
11.3533255301372));
#186232=CARTESIAN_POINT('Ctrl Pts',(-3.35083705967724,5.87913088810699,
11.3620751845747));
#186233=CARTESIAN_POINT('Ctrl Pts',(-3.51243888042421,5.7870252044309,11.3708246848236));
#186234=CARTESIAN_POINT('Ctrl Pts',(-3.67024081223708,5.68825280605772,
11.3795741850725));
#186235=CARTESIAN_POINT('Ctrl Pts',(-3.82370687544415,5.58314917682495,
11.3883236853215));
#186236=CARTESIAN_POINT('Ctrl Pts',(-3.97717043817821,5.47804726008016,
11.3970730430119));
#186237=CARTESIAN_POINT('Ctrl Pts',(-4.12629803722459,5.36661448084237,
11.4058224007024));
#186238=CARTESIAN_POINT('Ctrl Pts',(-4.27058317206899,5.24922931204583,
11.4145717583929));
#186239=CARTESIAN_POINT('Ctrl Pts',(-4.4148661477481,5.13184589986811,11.4233209851529));
#186240=CARTESIAN_POINT('Ctrl Pts',(-4.55430658194374,5.0085104572307,11.432070211913));
#186241=CARTESIAN_POINT('Ctrl Pts',(-4.68843089001792,4.8796418710317,11.4408194386731));
#186242=CARTESIAN_POINT('Ctrl Pts',(-4.8225533691777,4.75077504208027,11.449568546129));
#186243=CARTESIAN_POINT('Ctrl Pts',(-4.95135966065056,4.61637541908176,
11.4583176535849));
#186244=CARTESIAN_POINT('Ctrl Pts',(-5.07441230869156,4.47689945401945,
11.4670667610408));
#186245=CARTESIAN_POINT('Ctrl Pts',(-5.19746344226316,4.33742520555636,
11.4758157608172));
#186246=CARTESIAN_POINT('Ctrl Pts',(-5.31476088454655,4.19287495491478,
11.4845647605935));
#186247=CARTESIAN_POINT('Ctrl Pts',(-5.42590627628732,4.04373961586869,
11.4933137603699));
#186248=CARTESIAN_POINT('Ctrl Pts',(-5.53706380672551,3.894587989069,11.5020637156646));
#186249=CARTESIAN_POINT('Ctrl Pts',(-5.64206777071753,3.74085050155452,
11.5108136709593));
#186250=CARTESIAN_POINT('Ctrl Pts',(-5.74056148163902,3.58304938223331,
11.519563626254));
#186251=CARTESIAN_POINT('Ctrl Pts',(-5.83905138951775,3.42525435593466,
11.5283132436951));
#186252=CARTESIAN_POINT('Ctrl Pts',(-5.93103139557543,3.26339625497381,
11.5370628611362));
#186253=CARTESIAN_POINT('Ctrl Pts',(-6.01618907820737,3.09802485065217,
11.5458124785773));
#186254=CARTESIAN_POINT('Ctrl Pts',(-6.10134392544891,2.93265895249834,
11.5545618046932));
#186255=CARTESIAN_POINT('Ctrl Pts',(-6.17967677261754,2.7637802398621,11.563311130809));
#186256=CARTESIAN_POINT('Ctrl Pts',(-6.2509215700916,2.59196229227271,11.5720604569249));
#186257=CARTESIAN_POINT('Ctrl Pts',(-6.32216437407699,2.42014915229234,
11.5808095382274));
#186258=CARTESIAN_POINT('Ctrl Pts',(-6.38631941548876,2.2453972066298,11.5895586195298));
#186259=CARTESIAN_POINT('Ctrl Pts',(-6.443168810375,2.06829994947802,11.5983077008323));
#186260=CARTESIAN_POINT('Ctrl Pts',(-6.5000233452454,1.89118668024558,11.6070575731746));
#186261=CARTESIAN_POINT('Ctrl Pts',(-6.5495708241107,1.71172794807804,11.615807445517));
#186262=CARTESIAN_POINT('Ctrl Pts',(-6.59164294296062,1.53053334250434,
11.6245573178594));
#186263=CARTESIAN_POINT('Ctrl Pts',(-6.63371214082116,1.34935131693688,
11.6333065827143));
#186264=CARTESIAN_POINT('Ctrl Pts',(-6.66830695239675,1.16643393829848,
11.6420558475692));
#186265=CARTESIAN_POINT('Ctrl Pts',(-6.69530988153977,0.982402458341779,
11.6508051124241));
#186266=CARTESIAN_POINT('Ctrl Pts',(-6.72231419690474,0.79836153094786,
11.6595548264311));
#186267=CARTESIAN_POINT('Ctrl Pts',(-6.7417258082927,0.613206671363291,
11.6683045404381));
#186268=CARTESIAN_POINT('Ctrl Pts',(-6.75347878028174,0.427566795114224,
11.6770542544452));
#186269=CARTESIAN_POINT('Ctrl Pts',(-6.76248992368214,0.285234494205681,
11.6837627642334));
#186270=CARTESIAN_POINT('Ctrl Pts',(-6.76699999999998,0.142617266092119,
11.6904712740217));
#186271=CARTESIAN_POINT('Ctrl Pts',(-6.767,1.00878458448079E-12,11.69717978381));
#186272=CARTESIAN_POINT('',(-6.76699818449147,0.00495692335195666,11.3028202161557));
#186273=CARTESIAN_POINT('Ctrl Pts',(3.09910619832133,6.01563211736941,10.651525285013));
#186274=CARTESIAN_POINT('Ctrl Pts',(2.93889730946949,6.09816780950944,10.6599751073476));
#186275=CARTESIAN_POINT('Ctrl Pts',(2.77531112510111,6.17433926859913,10.6684249296823));
#186276=CARTESIAN_POINT('Ctrl Pts',(2.60889777959418,6.24387230615974,10.6768747520169));
#186277=CARTESIAN_POINT('Ctrl Pts',(2.44248443408725,6.31340534372035,10.6853245743516));
#186278=CARTESIAN_POINT('Ctrl Pts',(2.27324429892826,6.37629978527336,10.6937743966863));
#186279=CARTESIAN_POINT('Ctrl Pts',(2.10175175536633,6.43233461185086,10.7022242190209));
#186280=CARTESIAN_POINT('Ctrl Pts',(1.92198972526209,6.49107147569867,10.7110814975086));
#186281=CARTESIAN_POINT('Ctrl Pts',(1.73994024598263,6.54221110080664,10.7199387759964));
#186282=CARTESIAN_POINT('Ctrl Pts',(1.55624274932444,6.58562051026136,10.7287960544841));
#186283=CARTESIAN_POINT('Ctrl Pts',(1.37220179041347,6.6291110830081,10.7376698935722));
#186284=CARTESIAN_POINT('Ctrl Pts',(1.18650690895843,6.6648424965498,10.7465437326602));
#186285=CARTESIAN_POINT('Ctrl Pts',(0.999805918544201,6.69273315807854,
10.7554175717483));
#186286=CARTESIAN_POINT('Ctrl Pts',(0.812574071119657,6.72070312263168,
10.7643166423024));
#186287=CARTESIAN_POINT('Ctrl Pts',(0.624330648419938,6.74078768343343,
10.7732157128564));
#186288=CARTESIAN_POINT('Ctrl Pts',(0.435729855818093,6.75295701842895,
10.7821147834104));
#186289=CARTESIAN_POINT('Ctrl Pts',(0.246873554445342,6.76514283995023,
10.7910259100675));
#186290=CARTESIAN_POINT('Ctrl Pts',(0.0576591754872288,6.76939200528491,
10.7999370367245));
#186291=CARTESIAN_POINT('Ctrl Pts',(-0.131259506601047,6.76572685983752,
10.8088481633815));
#186292=CARTESIAN_POINT('Ctrl Pts',(-0.320596891080043,6.76205359129111,
10.8177790398589));
#186293=CARTESIAN_POINT('Ctrl Pts',(-0.509637007248433,6.75043093280429,
10.8267099163363));
#186294=CARTESIAN_POINT('Ctrl Pts',(-0.697728744206054,6.73093333791894,
10.8356407928137));
#186295=CARTESIAN_POINT('Ctrl Pts',(-0.877011172364044,6.7123489162382,
10.8441533901577));
#186296=CARTESIAN_POINT('Ctrl Pts',(-1.05543183885851,6.68661035022064,
10.8526659875017));
#186297=CARTESIAN_POINT('Ctrl Pts',(-1.23243601784636,6.65382525032894,
10.8611785848456));
#186298=CARTESIAN_POINT('Ctrl Pts',(-1.40341669656413,6.62215583628817,
10.8694014961907));
#186299=CARTESIAN_POINT('Ctrl Pts',(-1.57340328579009,6.58384963638255,
10.8776244075358));
#186300=CARTESIAN_POINT('Ctrl Pts',(-1.74184244167911,6.53898110628601,
10.8858473188808));
#186301=CARTESIAN_POINT('Ctrl Pts',(-1.9101033665741,6.49416005305242,10.8940615292938));
#186302=CARTESIAN_POINT('Ctrl Pts',(-2.07681977496709,6.44279058857545,
10.9022757397067));
#186303=CARTESIAN_POINT('Ctrl Pts',(-2.24144668537069,6.38499849308054,
10.9104899501196));
#186304=CARTESIAN_POINT('Ctrl Pts',(-2.40593244616417,6.32725594800073,
10.9186971177435));
#186305=CARTESIAN_POINT('Ctrl Pts',(-2.56833194039352,6.26310185713325,
10.9269042853675));
#186306=CARTESIAN_POINT('Ctrl Pts',(-2.72811348288888,6.19271231565619,
10.9351114529914));
#186307=CARTESIAN_POINT('Ctrl Pts',(-2.8877900958395,6.12236899943411,10.9433132309166));
#186308=CARTESIAN_POINT('Ctrl Pts',(-3.04485185446441,6.04579853317224,
10.9515150088419));
#186309=CARTESIAN_POINT('Ctrl Pts',(-3.19878518083012,5.9632258356448,10.9597167867672));
#186310=CARTESIAN_POINT('Ctrl Pts',(-3.35264830393675,5.88069079645045,
10.9679148241669));
#186311=CARTESIAN_POINT('Ctrl Pts',(-3.50338552179908,5.79215914876494,
10.9761128615666));
#186312=CARTESIAN_POINT('Ctrl Pts',(-3.65050600445879,5.69790267654778,
10.9843108989663));
#186313=CARTESIAN_POINT('Ctrl Pts',(-3.79761354436566,5.6036544964338,10.9925082151533));
#186314=CARTESIAN_POINT('Ctrl Pts',(-3.94110467640356,5.50368268109398,
11.0007055313402));
#186315=CARTESIAN_POINT('Ctrl Pts',(-4.08051551316418,5.3983036360348,11.0089028475272));
#186316=CARTESIAN_POINT('Ctrl Pts',(-4.21992482153698,5.29292574626635,
11.0171000738454));
#186317=CARTESIAN_POINT('Ctrl Pts',(-4.35525363684475,5.18214096035967,
11.0252973001635));
#186318=CARTESIAN_POINT('Ctrl Pts',(-4.48606937660464,5.06630738786052,
11.0334945264817));
#186319=CARTESIAN_POINT('Ctrl Pts',(-4.61690746497943,4.9504540263061,11.0416931532174));
#186320=CARTESIAN_POINT('Ctrl Pts',(-4.7432306730703,4.82955039760395,11.0498917799532));
#186321=CARTESIAN_POINT('Ctrl Pts',(-4.86464162644933,4.70399307463526,
11.0580904066889));
#186322=CARTESIAN_POINT('Ctrl Pts',(-4.98609539491333,4.578391474381,11.0662919246374));
#186323=CARTESIAN_POINT('Ctrl Pts',(-5.10263320865769,4.4481331685404,11.0744934425859));
#186324=CARTESIAN_POINT('Ctrl Pts',(-5.21389646118121,4.31364957919417,
11.0826949605344));
#186325=CARTESIAN_POINT('Ctrl Pts',(-5.32528642644745,4.17901283250201,
11.0909058188249));
#186326=CARTESIAN_POINT('Ctrl Pts',(-5.43138960068738,4.04014146555799,
11.0991166771154));
#186327=CARTESIAN_POINT('Ctrl Pts',(-5.53188876505622,3.89749864541924,
11.1073275354059));
#186328=CARTESIAN_POINT('Ctrl Pts',(-5.63244715625975,3.75477176206682,
11.115543232574));
#186329=CARTESIAN_POINT('Ctrl Pts',(-5.72739475955337,3.60826929567592,
11.123758929742));
#186330=CARTESIAN_POINT('Ctrl Pts',(-5.8164592843317,3.45848093730638,11.13197462691));
#186331=CARTESIAN_POINT('Ctrl Pts',(-5.9056619794547,3.30846020460872,11.1402030695086));
#186332=CARTESIAN_POINT('Ctrl Pts',(-5.98896318609218,3.15514370804712,
11.1484315121071));
#186333=CARTESIAN_POINT('Ctrl Pts',(-6.06613732808664,2.99904433391604,
11.1566599547056));
#186334=CARTESIAN_POINT('Ctrl Pts',(-6.1362523542124,2.85722336367187,11.1641357419688));
#186335=CARTESIAN_POINT('Ctrl Pts',(-6.20131046664306,2.71310577237175,
11.171611529232));
#186336=CARTESIAN_POINT('Ctrl Pts',(-6.2611780300233,2.56708758642038,11.1790873164952));
#186337=CARTESIAN_POINT('Ctrl Pts',(-6.33388635258981,2.38975053167341,
11.1881665560881));
#186338=CARTESIAN_POINT('Ctrl Pts',(-6.39914195040219,2.20911460084561,
11.1972457956809));
#186339=CARTESIAN_POINT('Ctrl Pts',(-6.45666022227768,2.02579065405515,
11.2063250352738));
#186340=CARTESIAN_POINT('Ctrl Pts',(-6.51389912282271,1.843357127878,11.2153601761975));
#186341=CARTESIAN_POINT('Ctrl Pts',(-6.56347555581142,1.65826183282316,
11.2243953171212));
#186342=CARTESIAN_POINT('Ctrl Pts',(-6.60515402599733,1.4711319766939,11.2334304580448));
#186343=CARTESIAN_POINT('Ctrl Pts',(-6.64670601382407,1.28457000670751,
11.2424381798734));
#186344=CARTESIAN_POINT('Ctrl Pts',(-6.68040777661328,1.09598600498177,
11.2514459017019));
#186345=CARTESIAN_POINT('Ctrl Pts',(-6.70607263333926,0.906023640076943,
11.2604536235304));
#186346=CARTESIAN_POINT('Ctrl Pts',(-6.73161310095464,0.71698196021121,
11.269417687897));
#186347=CARTESIAN_POINT('Ctrl Pts',(-6.74919427707081,0.52657545879325,
11.2783817522635));
#186348=CARTESIAN_POINT('Ctrl Pts',(-6.75868014845368,0.335457375680179,
11.28734581663));
#186349=CARTESIAN_POINT('Ctrl Pts',(-6.76413854164175,0.225483541872191,
11.2925039498053));
#186350=CARTESIAN_POINT('Ctrl Pts',(-6.7669173753356,0.115274427227421,
11.2976620829805));
#186351=CARTESIAN_POINT('Ctrl Pts',(-6.76699818449147,0.00495692335193946,
11.3028202161557));
#186352=CARTESIAN_POINT('Ctrl Pts',(-6.76699818449201,0.00495692262024367,
11.3028202161899));
#186353=CARTESIAN_POINT('Ctrl Pts',(-6.76712508573948,-0.168283730312138,
11.3109204571108));
#186354=CARTESIAN_POINT('Ctrl Pts',(-6.76059500658483,-0.341555143110208,
11.3190206980317));
#186355=CARTESIAN_POINT('Ctrl Pts',(-6.74742764060013,-0.514304612914761,
11.3271209389526));
#186356=CARTESIAN_POINT('Ctrl Pts',(-6.73425896758729,-0.687071230295947,
11.3352219839252));
#186357=CARTESIAN_POINT('Ctrl Pts',(-6.71445172225605,-0.859315435977075,
11.3433230288978));
#186358=CARTESIAN_POINT('Ctrl Pts',(-6.6880775739972,-1.03048889571683,
11.3514240738704));
#186359=CARTESIAN_POINT('Ctrl Pts',(-6.66169577561294,-1.20171200628977,
11.3595274686443));
#186360=CARTESIAN_POINT('Ctrl Pts',(-6.62874333622474,-1.3718633902453,
11.3676308634183));
#186361=CARTESIAN_POINT('Ctrl Pts',(-6.58934320424099,-1.54040421212198,
11.3757342581923));
#186362=CARTESIAN_POINT('Ctrl Pts',(-6.54992412541367,-1.70902608237146,
11.3838415497489));
#186363=CARTESIAN_POINT('Ctrl Pts',(-6.50405126239577,-1.87603549180717,
11.3919488413056));
#186364=CARTESIAN_POINT('Ctrl Pts',(-6.45189762645819,-2.04090813553752,
11.4000561328623));
#186365=CARTESIAN_POINT('Ctrl Pts',(-6.39967184979173,-2.2060088368611,
11.4081746387075));
#186366=CARTESIAN_POINT('Ctrl Pts',(-6.34114805599682,-2.36896651875642,
11.4162931445527));
#186367=CARTESIAN_POINT('Ctrl Pts',(-6.27654808583317,-2.52927521757202,
11.4244116503979));
#186368=CARTESIAN_POINT('Ctrl Pts',(-6.211902004502,-2.68969834401427,11.432535951196));
#186369=CARTESIAN_POINT('Ctrl Pts',(-6.14117125563026,-2.84746838735584,
11.4406602519941));
#186370=CARTESIAN_POINT('Ctrl Pts',(-6.06462381628711,-3.00210375685505,
11.4487845527922));
#186371=CARTESIAN_POINT('Ctrl Pts',(-5.98793678504328,-3.15702111939447,
11.4569236690643));
#186372=CARTESIAN_POINT('Ctrl Pts',(-5.90541204317221,-3.30879206499058,
11.4650627853363));
#186373=CARTESIAN_POINT('Ctrl Pts',(-5.81736185239714,-3.45696255089269,
11.4732019016083));
#186374=CARTESIAN_POINT('Ctrl Pts',(-5.73155896045956,-3.60135129188561,
11.4811332837871));
#186375=CARTESIAN_POINT('Ctrl Pts',(-5.64050946324707,-3.74232091358637,
11.4890646659659));
#186376=CARTESIAN_POINT('Ctrl Pts',(-5.54453817086657,-3.87948262939836,
11.4969960481447));
#186377=CARTESIAN_POINT('Ctrl Pts',(-5.44370899934471,-4.02358720303489,
11.505328901379));
#186378=CARTESIAN_POINT('Ctrl Pts',(-5.33712880616364,-4.16394350491165,
11.5136617546133));
#186379=CARTESIAN_POINT('Ctrl Pts',(-5.22510181678832,-4.30006976736372,
11.5219946078476));
#186380=CARTESIAN_POINT('Ctrl Pts',(-5.11320722602375,-4.43603514958382,
11.5303176129355));
#186381=CARTESIAN_POINT('Ctrl Pts',(-4.99587888182987,-4.56778018490212,
11.5386406180234));
#186382=CARTESIAN_POINT('Ctrl Pts',(-4.87346418341003,-4.69485205869361,
11.5469636231113));
#186383=CARTESIAN_POINT('Ctrl Pts',(-4.75117168868107,-4.82179707964647,
11.5552783195406));
#186384=CARTESIAN_POINT('Ctrl Pts',(-4.62380319581286,-4.94407798442775,
11.5635930159698));
#186385=CARTESIAN_POINT('Ctrl Pts',(-4.49174639335769,-5.06127487277249,
11.5719077123991));
#186386=CARTESIAN_POINT('Ctrl Pts',(-4.35979719460836,-5.17837626569962,
11.580215633773));
#186387=CARTESIAN_POINT('Ctrl Pts',(-4.22316755740045,-5.29040166670229,
11.5885235551469));
#186388=CARTESIAN_POINT('Ctrl Pts',(-4.08228220897734,-5.39696775664512,
11.5968314765208));
#186389=CARTESIAN_POINT('Ctrl Pts',(-3.94148582705851,-5.5034665520637,
11.6051341515953));
#186390=CARTESIAN_POINT('Ctrl Pts',(-3.79643936632356,-5.60451269747081,
11.6134368266698));
#186391=CARTESIAN_POINT('Ctrl Pts',(-3.64760100598947,-5.69976279340681,
11.6217395017442));
#186392=CARTESIAN_POINT('Ctrl Pts',(-3.49882347594604,-5.79497396059482,
11.6300387835125));
#186393=CARTESIAN_POINT('Ctrl Pts',(-3.34625742689429,-5.88439361116354,
11.6383380652807));
#186394=CARTESIAN_POINT('Ctrl Pts',(-3.19039065887923,-5.96772121028925,
11.6466373470489));
#186395=CARTESIAN_POINT('Ctrl Pts',(-3.03455704324672,-6.0510310858907,
11.6549348635854));
#186396=CARTESIAN_POINT('Ctrl Pts',(-2.87542441393954,-6.12825132756268,
11.6632323801219));
#186397=CARTESIAN_POINT('Ctrl Pts',(-2.71350606206983,-6.19912686199519,
11.6715298966584));
#186398=CARTESIAN_POINT('Ctrl Pts',(-2.55159524091372,-6.26999910005427,
11.679827027283));
#186399=CARTESIAN_POINT('Ctrl Pts',(-2.38689927413735,-6.33452707955494,
11.6881241579076));
#186400=CARTESIAN_POINT('Ctrl Pts',(-2.2199525381012,-6.39250340074826,
11.6964212885322));
#186401=CARTESIAN_POINT('Ctrl Pts',(-2.0529858234046,-6.45048666001813,
11.7047194120816));
#186402=CARTESIAN_POINT('Ctrl Pts',(-1.88376813156692,-6.50191658512377,
11.713017535631));
#186403=CARTESIAN_POINT('Ctrl Pts',(-1.71285032473928,-6.5466352246815,
11.7213156591804));
#186404=CARTESIAN_POINT('Ctrl Pts',(-1.54181229773543,-6.59138531843833,
11.7296196194643));
#186405=CARTESIAN_POINT('Ctrl Pts',(-1.36907210323849,-6.62941460582099,
11.7379235797483));
#186406=CARTESIAN_POINT('Ctrl Pts',(-1.19519304639963,-6.66061578097986,
11.7462275400323));
#186407=CARTESIAN_POINT('Ctrl Pts',(-1.02125075704963,-6.69182830269589,
11.7545345201179));
#186408=CARTESIAN_POINT('Ctrl Pts',(-0.846169123591691,-6.71620770889585,
11.7628415002036));
#186409=CARTESIAN_POINT('Ctrl Pts',(-0.67051819155781,-6.73369841578832,
11.7711484802892));
#186410=CARTESIAN_POINT('Ctrl Pts',(-0.494679437028176,-6.75120782538951,
11.7794643429792));
#186411=CARTESIAN_POINT('Ctrl Pts',(-0.318270514757428,-6.76181379111098,
11.7877802056691));
#186412=CARTESIAN_POINT('Ctrl Pts',(-0.141864212426566,-6.76551280726248,
11.7960960683591));
#186413=CARTESIAN_POINT('Ctrl Pts',(-0.00886637605910517,-6.76830160300468,
11.8023656388375));
#186414=CARTESIAN_POINT('Ctrl Pts',(0.124129918561489,-6.76716550414954,
11.8086352093159));
#186415=CARTESIAN_POINT('Ctrl Pts',(0.256880684272667,-6.7621225450333,
11.8149047797942));
#186416=CARTESIAN_POINT('Ctrl Pts',(0.435807109389025,-6.75532545695744,
11.823355140338));
#186417=CARTESIAN_POINT('Ctrl Pts',(0.614615459470383,-6.74141665938708,
11.8318055008817));
#186418=CARTESIAN_POINT('Ctrl Pts',(0.792717641896063,-6.72040830160094,
11.8402558614254));
#186419=CARTESIAN_POINT('Ctrl Pts',(0.970662638890027,-6.69941848490027,
11.8486987640393));
#186420=CARTESIAN_POINT('Ctrl Pts',(1.14790238269182,-6.67134163545978,
11.8571416666532));
#186421=CARTESIAN_POINT('Ctrl Pts',(1.32385153293246,-6.63624186710765,
11.8655845692671));
#186422=CARTESIAN_POINT('Ctrl Pts',(1.49966934960006,-6.60116829824544,
11.8740211698525));
#186423=CARTESIAN_POINT('Ctrl Pts',(1.67419816896492,-6.5590823249825,11.8824577704379));
#186424=CARTESIAN_POINT('Ctrl Pts',(1.846860113013,-6.51009959393569,11.8908943710233));
#186425=CARTESIAN_POINT('Ctrl Pts',(2.01939848651896,-6.46115191880502,
11.8993249337101));
#186426=CARTESIAN_POINT('Ctrl Pts',(2.190072331533,-6.405317421545,11.9077554963969));
#186427=CARTESIAN_POINT('Ctrl Pts',(2.35831606067142,-6.34276236020074,
11.9161860590837));
#186428=CARTESIAN_POINT('Ctrl Pts',(2.52648744799916,-6.28023419642008,
11.9246129967785));
#186429=CARTESIAN_POINT('Ctrl Pts',(2.69223049229545,-6.21099134466006,
11.9330399344733));
#186430=CARTESIAN_POINT('Ctrl Pts',(2.85499618850421,-6.13524944591713,
11.9414668721681));
#186431=CARTESIAN_POINT('Ctrl Pts',(3.01771161748824,-6.05953093868196,
11.9498912073565));
#186432=CARTESIAN_POINT('Ctrl Pts',(3.17745123182088,-5.97731752685017,
11.9583155425449));
#186433=CARTESIAN_POINT('Ctrl Pts',(3.33368704687592,-5.88887252990687,
11.9667398777332));
#186434=CARTESIAN_POINT('Ctrl Pts',(3.37769782421941,-5.86395805644734,
11.9691129670285));
#186435=CARTESIAN_POINT('Ctrl Pts',(3.42143070900545,-5.83854938012263,
11.9714860563238));
#186436=CARTESIAN_POINT('Ctrl Pts',(3.46487424383564,-5.81265304954669,
11.973859145619));
#186437=CARTESIAN_POINT('Ctrl Pts',(3.62265528470566,-5.71860108050327,
11.9824778848755));
#186438=CARTESIAN_POINT('Ctrl Pts',(3.77654702435987,-5.61815541635785,
11.9910966241321));
#186439=CARTESIAN_POINT('Ctrl Pts',(3.92604282991348,-5.51166732465639,
11.9997153633886));
#186440=CARTESIAN_POINT('Ctrl Pts',(4.07562842444101,-5.40511527492981,
12.0083392791633));
#186441=CARTESIAN_POINT('Ctrl Pts',(4.22081256797821,-5.29251373143548,
12.016963194938));
#186442=CARTESIAN_POINT('Ctrl Pts',(4.36112037061277,-5.17425531965967,
12.0255871107127));
#186443=CARTESIAN_POINT('Ctrl Pts',(4.50649807242136,-5.05172374407595,
12.0345226441069));
#186444=CARTESIAN_POINT('Ctrl Pts',(4.64664018478396,-4.92311910217486,
12.0434581775012));
#186445=CARTESIAN_POINT('Ctrl Pts',(4.78105925776186,-4.78892068986005,
12.0523937108955));
#186446=CARTESIAN_POINT('Ctrl Pts',(4.91103314005587,-4.65916017105989,
12.0610337493951));
#186447=CARTESIAN_POINT('Ctrl Pts',(5.03565626845823,-4.52417018231745,
12.0696737878948));
#186448=CARTESIAN_POINT('Ctrl Pts',(5.1545280269216,-4.3844189831356,12.0783138263945));
#186449=CARTESIAN_POINT('Ctrl Pts',(5.2794980217072,-4.23749841210341,12.087397107236));
#186450=CARTESIAN_POINT('Ctrl Pts',(5.39811079960517,-4.08531559718512,
12.0964803880776));
#186451=CARTESIAN_POINT('Ctrl Pts',(5.509951105094,-3.92845107128413,12.1055636689191));
#186452=CARTESIAN_POINT('Ctrl Pts',(5.62179141058283,-3.77158654538314,
12.1146469497607));
#186453=CARTESIAN_POINT('Ctrl Pts',(5.72685906044004,-3.6100406519454,12.1237302306022));
#186454=CARTESIAN_POINT('Ctrl Pts',(5.82479323757426,-3.4444263295227,12.1328135114438));
#186455=CARTESIAN_POINT('Ctrl Pts',(5.92231027499043,-3.27951742285762,
12.1418581030624));
#186456=CARTESIAN_POINT('Ctrl Pts',(6.01284529465068,-3.11042281667467,
12.1509026946811));
#186457=CARTESIAN_POINT('Ctrl Pts',(6.0960680090668,-2.93772766417046,12.1599472862997));
#186458=CARTESIAN_POINT('Ctrl Pts',(6.17921435137585,-2.76519099114829,
12.1689835778464));
#186459=CARTESIAN_POINT('Ctrl Pts',(6.2550616825633,-2.58906058270296,12.1780198693931));
#186460=CARTESIAN_POINT('Ctrl Pts',(6.32332611385161,-2.4099451981077,12.1870561609397));
#186461=CARTESIAN_POINT('Ctrl Pts',(6.39146974364527,-2.23114677808337,
12.1960764617647));
#186462=CARTESIAN_POINT('Ctrl Pts',(6.45205718452823,-2.04937415189009,
12.2050967625896));
#186463=CARTESIAN_POINT('Ctrl Pts',(6.50485306452033,-1.86525483754914,
12.2141170634146));
#186464=CARTESIAN_POINT('Ctrl Pts',(6.55758245756461,-1.68136738848343,
12.2231260047874));
#186465=CARTESIAN_POINT('Ctrl Pts',(6.60253980586729,-1.49513937689381,
12.2321349461602));
#186466=CARTESIAN_POINT('Ctrl Pts',(6.63953905318681,-1.30721465766234,
12.2411438875331));
#186467=CARTESIAN_POINT('Ctrl Pts',(6.67645428235687,-1.11971667919699,
12.2501323713389));
#186468=CARTESIAN_POINT('Ctrl Pts',(6.70544743656993,-0.930529916784176,
12.2591208551446));
#186469=CARTESIAN_POINT('Ctrl Pts',(6.7263832312889,-0.740309142072052,
12.2681093389504));
#186470=CARTESIAN_POINT('Ctrl Pts',(6.74475156096796,-0.573416127088918,
12.2759955183898));
#186471=CARTESIAN_POINT('Ctrl Pts',(6.75691828104992,-0.405727484273719,
12.2838816978292));
#186472=CARTESIAN_POINT('Ctrl Pts',(6.76282418892797,-0.237693057641016,
12.2917678772685));
#186473=CARTESIAN_POINT('Ctrl Pts',(6.76890630704458,-0.0646451111544109,
12.2998893508555));
#186474=CARTESIAN_POINT('Ctrl Pts',(6.76834408385886,0.108692148906018,
12.3080108244426));
#186475=CARTESIAN_POINT('Ctrl Pts',(6.76113132972388,0.281766112629207,
12.3161322980296));
#186476=CARTESIAN_POINT('Ctrl Pts',(6.75391908983964,0.454827736625934,
12.3242531925765));
#186477=CARTESIAN_POINT('Ctrl Pts',(6.74005727872453,0.627625735809023,
12.3323740871235));
#186478=CARTESIAN_POINT('Ctrl Pts',(6.71959179976489,0.799609307432327,
12.3404949816704));
#186479=CARTESIAN_POINT('Ctrl Pts',(6.69912387426174,0.97161343881346,12.3486168470288));
#186480=CARTESIAN_POINT('Ctrl Pts',(6.67205075343001,1.14280258529562,12.3567387123872));
#186481=CARTESIAN_POINT('Ctrl Pts',(6.63846999344241,1.31263290609553,12.3648605777456));
#186482=CARTESIAN_POINT('Ctrl Pts',(6.60486473266487,1.48258713645004,12.3729883688817));
#186483=CARTESIAN_POINT('Ctrl Pts',(6.5647424207357,1.65118020140671,12.3811161600178));
#186484=CARTESIAN_POINT('Ctrl Pts',(6.51825150012339,1.81787963879327,12.3892439511538));
#186485=CARTESIAN_POINT('Ctrl Pts',(6.47174164026241,1.98464698539859,12.3973750533505));
#186486=CARTESIAN_POINT('Ctrl Pts',(6.41885811208877,2.14951881834082,12.4055061555472));
#186487=CARTESIAN_POINT('Ctrl Pts',(6.35979859513314,2.31197985054857,12.4136372577439));
#186488=CARTESIAN_POINT('Ctrl Pts',(6.30067461642269,2.47461820427479,12.4217772348035));
#186489=CARTESIAN_POINT('Ctrl Pts',(6.23536132314184,2.6348401629617,12.4299172118631));
#186490=CARTESIAN_POINT('Ctrl Pts',(6.16410399743514,2.79215166293025,12.4380571889228));
#186491=CARTESIAN_POINT('Ctrl Pts',(6.12714738672581,2.87373906193492,12.4422788736463));
#186492=CARTESIAN_POINT('Ctrl Pts',(6.08859268529131,2.95454400240605,12.4465005583698));
#186493=CARTESIAN_POINT('Ctrl Pts',(6.04847883432448,3.0345004186404,12.4507222430933));
#186494=CARTESIAN_POINT('Ctrl Pts',(5.96828790539243,3.19433995379777,12.4591617424552));
#186495=CARTESIAN_POINT('Ctrl Pts',(5.88169770739263,3.35111725224016,12.4676012418171));
#186496=CARTESIAN_POINT('Ctrl Pts',(5.78896636304306,3.50430555853169,12.476040741179));
#186497=CARTESIAN_POINT('Ctrl Pts',(5.69630145699581,3.65738411152374,12.4844741939768));
#186498=CARTESIAN_POINT('Ctrl Pts',(5.59750434589849,3.80687851312266,12.4929076467747));
#186499=CARTESIAN_POINT('Ctrl Pts',(5.49287909107333,3.95228646366244,12.5013410995726));
#186500=CARTESIAN_POINT('Ctrl Pts',(5.38831415579666,4.09761058222556,12.5097696902359));
#186501=CARTESIAN_POINT('Ctrl Pts',(5.27792796886108,4.23885267598187,12.5181982808992));
#186502=CARTESIAN_POINT('Ctrl Pts',(5.16206813503634,4.37553900328205,12.5266268715625));
#186503=CARTESIAN_POINT('Ctrl Pts',(5.04625890084728,4.51216563536141,12.5350517811951));
#186504=CARTESIAN_POINT('Ctrl Pts',(4.92498100096567,4.64424021375626,12.5434766908276));
#186505=CARTESIAN_POINT('Ctrl Pts',(4.79862281664325,4.77132141692328,12.5519016004601));
#186506=CARTESIAN_POINT('Ctrl Pts',(4.67229083962043,4.89837626283309,12.5603247627256));
#186507=CARTESIAN_POINT('Ctrl Pts',(4.54088091140313,5.02043955963395,12.568747924991));
#186508=CARTESIAN_POINT('Ctrl Pts',(4.40481919147689,5.13710588662497,12.5771710872565));
#186509=CARTESIAN_POINT('Ctrl Pts',(4.26877963526478,5.25375320930587,12.5855928774346));
#186510=CARTESIAN_POINT('Ctrl Pts',(4.12809005261554,5.36500509961155,12.5940146676128));
#186511=CARTESIAN_POINT('Ctrl Pts',(3.98321083474644,5.47049544794241,12.6024364577909));
#186512=CARTESIAN_POINT('Ctrl Pts',(3.83830037511403,5.57600854421835,12.6108600640444));
#186513=CARTESIAN_POINT('Ctrl Pts',(3.68919874271934,5.67575741680091,12.6192836702978));
#186514=CARTESIAN_POINT('Ctrl Pts',(3.53639718849143,5.76941798843089,12.6277072765513));
#186515=CARTESIAN_POINT('Ctrl Pts',(3.39371871989328,5.8568735578177,12.6355728198463));
#186516=CARTESIAN_POINT('Ctrl Pts',(3.24781480299861,5.93902108971557,12.6434383631413));
#186517=CARTESIAN_POINT('Ctrl Pts',(3.09910619832131,6.01563211736941,12.6513039064363));
#186518=CARTESIAN_POINT('Origin',(0.,0.,4.30282021618968));
#186519=CARTESIAN_POINT('',(3.09910619832132,6.01563211736941,15.0460438035976));
#186520=CARTESIAN_POINT('',(3.09910619832135,6.0156321173694,14.6512308626299));
#186521=CARTESIAN_POINT('',(3.09910619832133,6.0156321173694,4.30282021618968));
#186522=CARTESIAN_POINT('',(-6.76699998297921,-0.000479957709509463,13.6971797837721));
#186523=CARTESIAN_POINT('Ctrl Pts',(-6.76699998297915,-0.000479958513274169,
13.69717978381));
#186524=CARTESIAN_POINT('Ctrl Pts',(-6.76699972950591,-0.00405371203792415,
13.6973484975525));
#186525=CARTESIAN_POINT('Ctrl Pts',(-6.76699664500473,-0.00762745138731119,
13.697517211295));
#186526=CARTESIAN_POINT('Ctrl Pts',(-6.76699072954348,-0.0112011728210126,
13.6976859250374));
#186527=CARTESIAN_POINT('Ctrl Pts',(-6.76667360689047,-0.202785222755277,
13.7067305197719));
#186528=CARTESIAN_POINT('Ctrl Pts',(-6.75821599951017,-0.394404825866598,
13.7157751145064));
#186529=CARTESIAN_POINT('Ctrl Pts',(-6.74163256529473,-0.585388208420326,
13.7248197092409));
#186530=CARTESIAN_POINT('Ctrl Pts',(-6.72506434899353,-0.776196333624015,
13.7338560041344));
#186531=CARTESIAN_POINT('Ctrl Pts',(-6.7003852138105,-0.966369167097182,
13.7428922990279));
#186532=CARTESIAN_POINT('Ctrl Pts',(-6.66766176604375,-1.15523831897938,
13.7519285939214));
#186533=CARTESIAN_POINT('Ctrl Pts',(-6.63499622498392,-1.34377325208668,
13.7609488983824));
#186534=CARTESIAN_POINT('Ctrl Pts',(-6.59431483746394,-1.53100887622529,
13.7699692028435));
#186535=CARTESIAN_POINT('Ctrl Pts',(-6.54573550536322,-1.71628543483517,
13.7789895073046));
#186536=CARTESIAN_POINT('Ctrl Pts',(-6.49721734948933,-1.90132867363011,
13.7879984524454));
#186537=CARTESIAN_POINT('Ctrl Pts',(-6.44082115783899,-2.0844175408772,
13.7970073975862));
#186538=CARTESIAN_POINT('Ctrl Pts',(-6.37671557869513,-2.26490340377396,
13.806016342727));
#186539=CARTESIAN_POINT('Ctrl Pts',(-6.31275556972657,-2.44497942155189,
13.815004830464));
#186540=CARTESIAN_POINT('Ctrl Pts',(-6.24112119699352,-2.62246400982848,
13.8239933182009));
#186541=CARTESIAN_POINT('Ctrl Pts',(-6.16203034063119,-2.79672506355929,
13.8329818059378));
#186542=CARTESIAN_POINT('Ctrl Pts',(-6.09263899295528,-2.94961516896424,
13.8408679675793));
#186543=CARTESIAN_POINT('Ctrl Pts',(-6.0175086694995,-3.10002398845393,
13.8487541292207));
#186544=CARTESIAN_POINT('Ctrl Pts',(-5.93681807242098,-3.24753447633365,
13.8566402908622));
#186545=CARTESIAN_POINT('Ctrl Pts',(-5.85371987056364,-3.39944630672915,
13.8647617557625));
#186546=CARTESIAN_POINT('Ctrl Pts',(-5.7647603992845,-3.54821548016966,
13.8728832206629));
#186547=CARTESIAN_POINT('Ctrl Pts',(-5.67021640192898,-3.69336363702461,
13.8810046855632));
#186548=CARTESIAN_POINT('Ctrl Pts',(-5.57567914694529,-3.83850144268993,
13.8891255712842));
#186549=CARTESIAN_POINT('Ctrl Pts',(-5.47555835902103,-3.98001843929452,
13.8972464570051));
#186550=CARTESIAN_POINT('Ctrl Pts',(-5.37017465501147,-4.11746441085682,
13.905367342726));
#186551=CARTESIAN_POINT('Ctrl Pts',(-5.26477835462964,-4.25492681115105,
13.9134891991255));
#186552=CARTESIAN_POINT('Ctrl Pts',(-5.15411810930141,-4.38831692759934,
13.921611055525));
#186553=CARTESIAN_POINT('Ctrl Pts',(-5.03855539966497,-4.51721689588921,
13.9297329119245));
#186554=CARTESIAN_POINT('Ctrl Pts',(-4.92290837689637,-4.64621090801118,
13.9378606939305));
#186555=CARTESIAN_POINT('Ctrl Pts',(-4.8023519907143,-4.77070795606198,
13.9459884759366));
#186556=CARTESIAN_POINT('Ctrl Pts',(-4.6772856720309,-4.89032593414942,
13.9541162579426));
#186557=CARTESIAN_POINT('Ctrl Pts',(-4.55216840597195,-5.00999264016071,
13.9622473509053));
#186558=CARTESIAN_POINT('Ctrl Pts',(-4.42253781936197,-5.12477607187367,
13.970378443868));
#186559=CARTESIAN_POINT('Ctrl Pts',(-4.28882691649475,-5.23433402452978,
13.9785095368308));
#186560=CARTESIAN_POINT('Ctrl Pts',(-4.15497007375995,-5.3440115551168,
13.9866495045419));
#186561=CARTESIAN_POINT('Ctrl Pts',(-4.01702431125062,-5.448451994301,13.9947894722531));
#186562=CARTESIAN_POINT('Ctrl Pts',(-3.8754527347774,-5.54735568541502,
14.0029294399643));
#186563=CARTESIAN_POINT('Ctrl Pts',(-3.80202759922334,-5.59865141233813,
14.0071511788719));
#186564=CARTESIAN_POINT('Ctrl Pts',(-3.72762759464339,-5.6484585394406,
14.0113729177794));
#186565=CARTESIAN_POINT('Ctrl Pts',(-3.65231993181482,-5.69674013060699,
14.015594656687));
#186566=CARTESIAN_POINT('Ctrl Pts',(-3.50176290752131,-5.79326593450448,
14.0240348661343));
#186567=CARTESIAN_POINT('Ctrl Pts',(-3.34726540711925,-5.88389109853242,
14.0324750755817));
#186568=CARTESIAN_POINT('Ctrl Pts',(-3.18931839142901,-5.96829432904349,
14.040915285029));
#186569=CARTESIAN_POINT('Ctrl Pts',(-3.03149104400764,-6.05263361160064,
14.0493490997671));
#186570=CARTESIAN_POINT('Ctrl Pts',(-2.87021968423866,-6.13076020114868,
14.0577829145051));
#186571=CARTESIAN_POINT('Ctrl Pts',(-2.70602223773671,-6.20239733078061,
14.0662167292432));
#186572=CARTESIAN_POINT('Ctrl Pts',(-2.54192395356688,-6.27399119722549,
14.074645450621));
#186573=CARTESIAN_POINT('Ctrl Pts',(-2.37490341057726,-6.33910328406654,
14.0830741719989));
#186574=CARTESIAN_POINT('Ctrl Pts',(-2.20550136003658,-6.39750363429962,
14.0915028933767));
#186575=CARTESIAN_POINT('Ctrl Pts',(-2.03617560196672,-6.45587768315675,
14.0999278187676));
#186576=CARTESIAN_POINT('Ctrl Pts',(-1.86447078962731,-6.50754591386063,
14.1083527441584));
#186577=CARTESIAN_POINT('Ctrl Pts',(-1.69094616812693,-6.55232707184988,
14.1167776695493));
#186578=CARTESIAN_POINT('Ctrl Pts',(-1.51747307193208,-6.59709493280481,
14.125200093296));
#186579=CARTESIAN_POINT('Ctrl Pts',(-1.34218156673801,-6.63497971598868,
14.1336225170427));
#186580=CARTESIAN_POINT('Ctrl Pts',(-1.16564490395299,-6.66585035519764,
14.1420449407894));
#186581=CARTESIAN_POINT('Ctrl Pts',(-0.989105464758191,-6.69672147991223,
14.1504674969964));
#186582=CARTESIAN_POINT('Ctrl Pts',(-0.811321156116721,-6.72057817626419,
14.1588900532034));
#186583=CARTESIAN_POINT('Ctrl Pts',(-0.63287490980961,-6.73734059911873,
14.1673126094104));
#186584=CARTESIAN_POINT('Ctrl Pts',(-0.454422635556327,-6.75410358821091,
14.1757354501328));
#186585=CARTESIAN_POINT('Ctrl Pts',(-0.275308711152397,-6.76377179460825,
14.1841582908553));
#186586=CARTESIAN_POINT('Ctrl Pts',(-0.0961208310274312,-6.76631729863761,
14.1925811315778));
#186587=CARTESIAN_POINT('Ctrl Pts',(0.083098118706693,-6.76886324403509,
14.2010054327471));
#186588=CARTESIAN_POINT('Ctrl Pts',(0.262390716203052,-6.76428402007166,
14.2094297339163));
#186589=CARTESIAN_POINT('Ctrl Pts',(0.441169254230898,-6.7526038451194,
14.2178540350856));
#186590=CARTESIAN_POINT('Ctrl Pts',(0.620003758002324,-6.74092001374573,
14.226280973441));
#186591=CARTESIAN_POINT('Ctrl Pts',(0.798323548744178,-6.72213082122644,
14.2347079117964));
#186592=CARTESIAN_POINT('Ctrl Pts',(0.975545655055304,-6.69631239376589,
14.2431348501518));
#186593=CARTESIAN_POINT('Ctrl Pts',(1.15292710631738,-6.67047075229361,
14.2515693653841));
#186594=CARTESIAN_POINT('Ctrl Pts',(1.32920857065779,-6.63758729532144,
14.2600038806164));
#186595=CARTESIAN_POINT('Ctrl Pts',(1.50381575322244,-6.59778956775374,
14.2684383958486));
#186596=CARTESIAN_POINT('Ctrl Pts',(1.67850727255218,-6.55797261754266,
14.276876985024));
#186597=CARTESIAN_POINT('Ctrl Pts',(1.85152257409379,-6.51123481817353,
14.2853155741994));
#186598=CARTESIAN_POINT('Ctrl Pts',(2.02230163697252,-6.45775387337566,
14.2937541633748));
#186599=CARTESIAN_POINT('Ctrl Pts',(2.19327159220824,-6.40421314898048,
14.3022021849838));
#186600=CARTESIAN_POINT('Ctrl Pts',(2.36199999830811,-6.34391432577537,
14.3106502065929));
#186601=CARTESIAN_POINT('Ctrl Pts',(2.52794480242968,-6.27708404244111,
14.3190982282019));
#186602=CARTESIAN_POINT('Ctrl Pts',(2.62226516868471,-6.23909878080919,
14.3238999482468));
#186603=CARTESIAN_POINT('Ctrl Pts',(2.71568665118124,-6.19900433459048,
14.3287016682916));
#186604=CARTESIAN_POINT('Ctrl Pts',(2.80811313774876,-6.15684899974027,
14.3335033883365));
#186605=CARTESIAN_POINT('Ctrl Pts',(2.96671275895864,-6.08451237430408,
14.341742920191));
#186606=CARTESIAN_POINT('Ctrl Pts',(3.12273526239712,-6.00594335354235,
14.3499824520455));
#186607=CARTESIAN_POINT('Ctrl Pts',(3.27565856692249,-5.92134697116689,
14.3582219839));
#186608=CARTESIAN_POINT('Ctrl Pts',(3.42841213726711,-5.83684448486372,
14.36645237045));
#186609=CARTESIAN_POINT('Ctrl Pts',(3.57807304941933,-5.74632812852416,
14.374682757));
#186610=CARTESIAN_POINT('Ctrl Pts',(3.72413943959445,-5.65005083467902,
14.38291314355));
#186611=CARTESIAN_POINT('Ctrl Pts',(3.87006976318593,-5.55386322691732,
14.3911358631714));
#186612=CARTESIAN_POINT('Ctrl Pts',(4.01241193785822,-5.45192556392291,
14.3993585827928));
#186613=CARTESIAN_POINT('Ctrl Pts',(4.15068887620276,-5.3445365423923,14.4075813024142));
#186614=CARTESIAN_POINT('Ctrl Pts',(4.28884329121644,-5.23724267527265,
14.4157967361136));
#186615=CARTESIAN_POINT('Ctrl Pts',(4.42293936919019,-5.12450729432345,
14.4240121698129));
#186616=CARTESIAN_POINT('Ctrl Pts',(4.55252930136011,-5.00667214427484,
14.4322276035123));
#186617=CARTESIAN_POINT('Ctrl Pts',(4.68205263436727,-4.88889755234371,
14.4404388151166));
#186618=CARTESIAN_POINT('Ctrl Pts',(4.8070741710293,-4.76602864988975,14.4486500267209));
#186619=CARTESIAN_POINT('Ctrl Pts',(4.92717916063223,-4.63844742548964,
14.4568612383253));
#186620=CARTESIAN_POINT('Ctrl Pts',(5.047243873648,-4.51090898479337,14.4650696963422));
#186621=CARTESIAN_POINT('Ctrl Pts',(5.1623950803399,-4.37866162901597,14.4732781543592));
#186622=CARTESIAN_POINT('Ctrl Pts',(5.2722548332316,-4.24212422890538,14.4814866123762));
#186623=CARTESIAN_POINT('Ctrl Pts',(5.32119975171067,-4.18129383613775,
14.4851436596379));
#186624=CARTESIAN_POINT('Ctrl Pts',(5.36909487682439,-4.11961238541116,
14.4888007068995));
#186625=CARTESIAN_POINT('Ctrl Pts',(5.41590930921471,-4.05711909541258,
14.4924577541612));
#186626=CARTESIAN_POINT('Ctrl Pts',(5.52931569949832,-3.90573119912038,
14.501316828337));
#186627=CARTESIAN_POINT('Ctrl Pts',(5.63625969591771,-3.74973455536902,
14.5101759025128));
#186628=CARTESIAN_POINT('Ctrl Pts',(5.73640989029452,-3.58969226682891,
14.5190349766885));
#186629=CARTESIAN_POINT('Ctrl Pts',(5.83674824673813,-3.42934929102628,
14.5279106952824));
#186630=CARTESIAN_POINT('Ctrl Pts',(5.93026715513365,-3.26494570012286,
14.5367864138762));
#186631=CARTESIAN_POINT('Ctrl Pts',(6.01668117519077,-3.09706903960906,
14.5456621324701));
#186632=CARTESIAN_POINT('Ctrl Pts',(6.10334179644595,-2.92871330653758,
14.5545631798571));
#186633=CARTESIAN_POINT('Ctrl Pts',(6.18285683619363,-2.75686490219078,
14.5634642272441));
#186634=CARTESIAN_POINT('Ctrl Pts',(6.2549878243912,-2.58213406249906,14.5723652746311));
#186635=CARTESIAN_POINT('Ctrl Pts',(6.32721687565693,-2.40716567383327,
14.5812784231142));
#186636=CARTESIAN_POINT('Ctrl Pts',(6.39204172953085,-2.22930726402084,
14.5901915715972));
#186637=CARTESIAN_POINT('Ctrl Pts',(6.44927345651298,-2.04918541940869,
14.5991047200803));
#186638=CARTESIAN_POINT('Ctrl Pts',(6.5066322535791,-1.86866365504693,14.6080376581903));
#186639=CARTESIAN_POINT('Ctrl Pts',(6.55636412420428,-1.68586865215733,
14.6169705963003));
#186640=CARTESIAN_POINT('Ctrl Pts',(6.59833033935322,-1.50144121855332,
14.6259035344103));
#186641=CARTESIAN_POINT('Ctrl Pts',(6.63827609132687,-1.32589304262804,
14.6344063962689));
#186642=CARTESIAN_POINT('Ctrl Pts',(6.67118630300886,-1.14886610272031,
14.6429092581274));
#186643=CARTESIAN_POINT('Ctrl Pts',(6.69698490228194,-0.970918234769417,
14.651412119986));
#186644=CARTESIAN_POINT('Ctrl Pts',(6.72193353269149,-0.798833093918143,
14.6596348438513));
#186645=CARTESIAN_POINT('Ctrl Pts',(6.7402782696263,-0.625556742266962,
14.6678575677165));
#186646=CARTESIAN_POINT('Ctrl Pts',(6.75191179983549,-0.451637074698601,
14.6760802915818));
#186647=CARTESIAN_POINT('Ctrl Pts',(6.76353301634702,-0.277901495206955,
14.6842943119723));
#186648=CARTESIAN_POINT('Ctrl Pts',(6.76845714790904,-0.103524310693517,
14.6925083323629));
#186649=CARTESIAN_POINT('Ctrl Pts',(6.7666281705844,0.0709380085259613,
14.7007223527535));
#186650=CARTESIAN_POINT('Ctrl Pts',(6.76480076196337,0.245250692391744,
14.7089293280248));
#186651=CARTESIAN_POINT('Ctrl Pts',(6.75623178366827,0.419648008867386,
14.7171363032961));
#186652=CARTESIAN_POINT('Ctrl Pts',(6.74091713069847,0.593569909156351,
14.7253432785674));
#186653=CARTESIAN_POINT('Ctrl Pts',(6.72561253915008,0.767377546227373,
14.7335448620197));
#186654=CARTESIAN_POINT('Ctrl Pts',(6.7035711318405,0.940710033193421,14.7417464454721));
#186655=CARTESIAN_POINT('Ctrl Pts',(6.67484085652982,1.11300877804275,14.7499480289244));
#186656=CARTESIAN_POINT('Ctrl Pts',(6.64612369103792,1.28522890181048,14.7581458699388));
#186657=CARTESIAN_POINT('Ctrl Pts',(6.61072379710433,1.45641587010172,14.7663437109531));
#186658=CARTESIAN_POINT('Ctrl Pts',(6.56874081204955,1.62601757189602,14.7745415519675));
#186659=CARTESIAN_POINT('Ctrl Pts',(6.52676153186233,1.79560430686884,14.782738669548));
#186660=CARTESIAN_POINT('Ctrl Pts',(6.47820039550589,1.96360570398415,14.7909357871284));
#186661=CARTESIAN_POINT('Ctrl Pts',(6.42320795310195,2.12948082668239,14.7991329047089));
#186662=CARTESIAN_POINT('Ctrl Pts',(6.36821612255023,2.29535410383497,14.8073299310873));
#186663=CARTESIAN_POINT('Ctrl Pts',(6.30679324037308,2.45910081274998,14.8155269574657));
#186664=CARTESIAN_POINT('Ctrl Pts',(6.23913940853569,2.62019625998834,14.823723983844));
#186665=CARTESIAN_POINT('Ctrl Pts',(6.17147402790334,2.78131920690025,14.8319224094895));
#186666=CARTESIAN_POINT('Ctrl Pts',(6.09757571745006,2.93978965960707,14.8401208351349));
#186667=CARTESIAN_POINT('Ctrl Pts',(6.01769231631652,3.09510390554908,14.8483192607803));
#186668=CARTESIAN_POINT('Ctrl Pts',(5.93778075336619,3.25047290543593,14.8565205766702));
#186669=CARTESIAN_POINT('Ctrl Pts',(5.8518800606913,3.40268316318726,14.8647218925602));
#186670=CARTESIAN_POINT('Ctrl Pts',(5.76028353595834,3.55125647980646,14.8729232084501));
#186671=CARTESIAN_POINT('Ctrl Pts',(5.66858269811658,3.69999899656273,14.881133864266));
#186672=CARTESIAN_POINT('Ctrl Pts',(5.5711732576536,3.84509599170721,14.8893445200818));
#186673=CARTESIAN_POINT('Ctrl Pts',(5.46839187287259,3.98609825828479,14.8975551758977));
#186674=CARTESIAN_POINT('Ctrl Pts',(5.36554992151172,4.12718361408185,14.9057706700541));
#186675=CARTESIAN_POINT('Ctrl Pts',(5.25732993785621,4.26416915041607,14.9139861642105));
#186676=CARTESIAN_POINT('Ctrl Pts',(5.14410813426136,4.39663968310187,14.9222016583669));
#186677=CARTESIAN_POINT('Ctrl Pts',(5.03071066495481,4.52931574625675,14.9304298990137));
#186678=CARTESIAN_POINT('Ctrl Pts',(4.91229611070893,4.65746254342381,14.9386581396604));
#186679=CARTESIAN_POINT('Ctrl Pts',(4.7892776596528,4.78070167431002,14.9468863803072));
#186680=CARTESIAN_POINT('Ctrl Pts',(4.67747352753613,4.8927063691607,14.9543645374166));
#186681=CARTESIAN_POINT('Ctrl Pts',(4.56186720603265,5.00065773557728,14.9618426945261));
#186682=CARTESIAN_POINT('Ctrl Pts',(4.44279111096107,5.10430172936175,14.9693208516355));
#186683=CARTESIAN_POINT('Ctrl Pts',(4.31429865585947,5.21614173561904,14.9773903702576));
#186684=CARTESIAN_POINT('Ctrl Pts',(4.18134476669475,5.32333164869652,14.9854598888797));
#186685=CARTESIAN_POINT('Ctrl Pts',(4.04430565237376,5.42548438300007,14.9935294075019));
#186686=CARTESIAN_POINT('Ctrl Pts',(3.90741731585645,5.52752472337146,15.0015900476056));
#186687=CARTESIAN_POINT('Ctrl Pts',(3.76645298746382,5.62453868532145,15.0096506877093));
#186688=CARTESIAN_POINT('Ctrl Pts',(3.62182548495932,5.71617609565164,15.0177113278131));
#186689=CARTESIAN_POINT('Ctrl Pts',(3.47736266831416,5.80770915939901,15.0257627893483));
#186690=CARTESIAN_POINT('Ctrl Pts',(3.32924529483506,5.89387766213528,15.0338142508835));
#186691=CARTESIAN_POINT('Ctrl Pts',(3.17791859704343,5.97437213358571,15.0418657124187));
#186692=CARTESIAN_POINT('Ctrl Pts',(3.15174294605904,5.98829561980201,15.0432584094783));
#186693=CARTESIAN_POINT('Ctrl Pts',(3.1254713474183,6.00204943887579,15.044651106538));
#186694=CARTESIAN_POINT('Ctrl Pts',(3.09910619832132,6.01563211736941,15.0460438035976));
#186695=CARTESIAN_POINT('Ctrl Pts',(3.09910619832134,6.0156321173694,13.0454981451509));
#186696=CARTESIAN_POINT('Ctrl Pts',(2.99647924970002,6.0685030054792,13.0509549173467));
#186697=CARTESIAN_POINT('Ctrl Pts',(2.89261356534081,6.11868781655653,13.0564116895426));
#186698=CARTESIAN_POINT('Ctrl Pts',(2.78766713702072,6.16613338593764,13.0618684617384));
#186699=CARTESIAN_POINT('Ctrl Pts',(2.62740565609552,6.2385865159209,13.0702013836603));
#186700=CARTESIAN_POINT('Ctrl Pts',(2.46411195497162,6.30488082417588,13.0785343055822));
#186701=CARTESIAN_POINT('Ctrl Pts',(2.29829356235286,6.3647573167598,13.0868672275041));
#186702=CARTESIAN_POINT('Ctrl Pts',(2.13267112688792,6.42456304984061,13.0951903019318));
#186703=CARTESIAN_POINT('Ctrl Pts',(1.96453026791125,6.47796595860846,13.1035133763595));
#186704=CARTESIAN_POINT('Ctrl Pts',(1.79440086093049,6.52475398389027,13.1118364507872));
#186705=CARTESIAN_POINT('Ctrl Pts',(1.62444127744431,6.57149530527709,13.1201512171063));
#186706=CARTESIAN_POINT('Ctrl Pts',(1.45249743406288,6.61163480676236,13.1284659834254));
#186707=CARTESIAN_POINT('Ctrl Pts',(1.27911705083958,6.64500929798081,13.1367807497445));
#186708=CARTESIAN_POINT('Ctrl Pts',(1.10587793243847,6.67835659672524,13.1450887414564));
#186709=CARTESIAN_POINT('Ctrl Pts',(0.931204946609093,6.70494980266404,
13.1533967331684));
#186710=CARTESIAN_POINT('Ctrl Pts',(0.755658991091057,6.72467608804939,
13.1617047248803));
#186711=CARTESIAN_POINT('Ctrl Pts',(0.580223881354881,6.74438991757655,
13.1700074706392));
#186712=CARTESIAN_POINT('Ctrl Pts',(0.403917245247942,6.75724542895902,
13.1783102163982));
#186713=CARTESIAN_POINT('Ctrl Pts',(0.227308369897301,6.7631811971124,13.1866129621571));
#186714=CARTESIAN_POINT('Ctrl Pts',(0.0507716689739177,6.76911453950622,
13.194912314848));
#186715=CARTESIAN_POINT('Ctrl Pts',(-0.126066677897103,6.76813376176002,
13.203211667539));
#186716=CARTESIAN_POINT('Ctrl Pts',(-0.3026337917841,6.7602294183016,13.2115110202299));
#186717=CARTESIAN_POINT('Ctrl Pts',(-0.47916335280551,6.75232675596454,
13.2198086077876));
#186718=CARTESIAN_POINT('Ctrl Pts',(-0.655421448412094,6.73750347707007,
13.2281061953454));
#186719=CARTESIAN_POINT('Ctrl Pts',(-0.830836484566319,6.71580224067933,
13.2364037829031));
#186720=CARTESIAN_POINT('Ctrl Pts',(-1.00624336252497,6.69410201356883,
13.244700984557));
#186721=CARTESIAN_POINT('Ctrl Pts',(-1.18080691393567,6.66552450927124,
13.2529981862108));
#186722=CARTESIAN_POINT('Ctrl Pts',(-1.35396174730041,6.63016414478912,
13.2612953878647));
#186723=CARTESIAN_POINT('Ctrl Pts',(-1.52713730035547,6.59479954908926,
13.2695935823609));
#186724=CARTESIAN_POINT('Ctrl Pts',(-1.69890345874809,6.55265054611699,
13.2778917768571));
#186725=CARTESIAN_POINT('Ctrl Pts',(-1.86870589449789,6.50386248931117,
13.2861899713533));
#186726=CARTESIAN_POINT('Ctrl Pts',(-2.03862775430338,6.4550401192896,13.2944940020675));
#186727=CARTESIAN_POINT('Ctrl Pts',(-2.20658279695294,6.39956946139631,
13.3027980327818));
#186728=CARTESIAN_POINT('Ctrl Pts',(-2.3720318454969,6.33764577141612,13.311102063496));
#186729=CARTESIAN_POINT('Ctrl Pts',(-2.53754105587863,6.27569956427416,
13.3194091137849));
#186730=CARTESIAN_POINT('Ctrl Pts',(-2.70054213272634,6.20729577702732,
13.3277161640738));
#186731=CARTESIAN_POINT('Ctrl Pts',(-2.8605165032443,6.13267758280729,13.3360232143626));
#186732=CARTESIAN_POINT('Ctrl Pts',(-3.02066191340138,6.05797960912652,
13.3443391462922));
#186733=CARTESIAN_POINT('Ctrl Pts',(-3.17777383920727,5.97705410703056,
13.3526550782218));
#186734=CARTESIAN_POINT('Ctrl Pts',(-3.33135793194182,5.89019043234498,
13.3609710101514));
#186735=CARTESIAN_POINT('Ctrl Pts',(-3.4471329132116,5.8247107323924,13.3672397378969));
#186736=CARTESIAN_POINT('Ctrl Pts',(-3.5609037198362,5.7558576388238,13.3735084656424));
#186737=CARTESIAN_POINT('Ctrl Pts',(-3.67246982934681,5.68377113829695,
13.3797771933879));
#186738=CARTESIAN_POINT('Ctrl Pts',(-3.82286136738246,5.58659826265044,
13.3882274621237));
#186739=CARTESIAN_POINT('Ctrl Pts',(-3.96952145393238,5.48337026741117,
13.3966777308594));
#186740=CARTESIAN_POINT('Ctrl Pts',(-4.11195058525543,5.3743977694638,13.4051279995952));
#186741=CARTESIAN_POINT('Ctrl Pts',(-4.25425401802717,5.2655214434512,13.4135708106815));
#186742=CARTESIAN_POINT('Ctrl Pts',(-4.39233367591338,5.15091092014112,
13.4220136217678));
#186743=CARTESIAN_POINT('Ctrl Pts',(-4.52571894571774,5.03092009719609,
13.4304564328541));
#186744=CARTESIAN_POINT('Ctrl Pts',(-4.65900465923298,4.9110188331737,13.4388929423829));
#186745=CARTESIAN_POINT('Ctrl Pts',(-4.78760272359501,4.7857454957332,13.4473294519118));
#186746=CARTESIAN_POINT('Ctrl Pts',(-4.91107524620995,4.65549448781371,
13.4557659614406));
#186747=CARTESIAN_POINT('Ctrl Pts',(-5.03445941757595,4.52533668151498,
13.4641964341919));
#186748=CARTESIAN_POINT('Ctrl Pts',(-5.15272513525066,4.39020854936282,
13.4726269069431));
#186749=CARTESIAN_POINT('Ctrl Pts',(-5.26547090893323,4.25054174278737,
13.4810573796944));
#186750=CARTESIAN_POINT('Ctrl Pts',(-5.37816821350532,4.11093497860337,
13.4894842282077));
#186751=CARTESIAN_POINT('Ctrl Pts',(-5.48535009686753,3.96679368724348,
13.497911076721));
#186752=CARTESIAN_POINT('Ctrl Pts',(-5.58665453466185,3.81858352145691,
13.5063379252343));
#186753=CARTESIAN_POINT('Ctrl Pts',(-5.68792770338291,3.67041910287187,
13.5147621726795));
#186754=CARTESIAN_POINT('Ctrl Pts',(-5.78332685750545,3.51818858788166,
13.5231864201247));
#186755=CARTESIAN_POINT('Ctrl Pts',(-5.87253238503921,3.3623878994943,13.5316106675698));
#186756=CARTESIAN_POINT('Ctrl Pts',(-5.89766708894574,3.31848922774924,
13.5339842981174));
#186757=CARTESIAN_POINT('Ctrl Pts',(-5.92231034895509,3.27430729443035,
13.536357928665));
#186758=CARTESIAN_POINT('Ctrl Pts',(-5.94645565075077,3.22985358703058,
13.5387315592127));
#186759=CARTESIAN_POINT('Ctrl Pts',(-6.03409394712244,3.06850347358454,
13.5473469386835));
#186760=CARTESIAN_POINT('Ctrl Pts',(-6.11512962430521,2.90364278619995,
13.5559623181544));
#186761=CARTESIAN_POINT('Ctrl Pts',(-6.18930641017625,2.73583171283455,
13.5645776976252));
#186762=CARTESIAN_POINT('Ctrl Pts',(-6.26352739573469,2.56792064596175,
13.5731982107383));
#186763=CARTESIAN_POINT('Ctrl Pts',(-6.3308812104885,2.39705596330387,13.5818187238514));
#186764=CARTESIAN_POINT('Ctrl Pts',(-6.39115998598896,2.22381722124226,
13.5904392369645));
#186765=CARTESIAN_POINT('Ctrl Pts',(-6.45335842450229,2.04506144598328,
13.5993342825318));
#186766=CARTESIAN_POINT('Ctrl Pts',(-6.50802365181356,1.86377824369163,
13.6082293280991));
#186767=CARTESIAN_POINT('Ctrl Pts',(-6.5549832821678,1.68061987686112,13.6171243736664));
#186768=CARTESIAN_POINT('Ctrl Pts',(-6.60057818246509,1.50278441667421,
13.62576091345));
#186769=CARTESIAN_POINT('Ctrl Pts',(-6.63890906905846,1.32318156436215,
13.6343974532337));
#186770=CARTESIAN_POINT('Ctrl Pts',(-6.66987032856565,1.142417962096,13.6430339930174));
#186771=CARTESIAN_POINT('Ctrl Pts',(-6.70222166989695,0.953538533730723,
13.6520582914765));
#186772=CARTESIAN_POINT('Ctrl Pts',(-6.72652632290179,0.763392101546304,
13.6610825899356));
#186773=CARTESIAN_POINT('Ctrl Pts',(-6.74272428641475,0.572676346108998,
13.6701068883947));
#186774=CARTESIAN_POINT('Ctrl Pts',(-6.7589222499277,0.381960590671692,
13.6791311868538));
#186775=CARTESIAN_POINT('Ctrl Pts',(-6.76701354094034,0.190675889789615,
13.6881554853129));
#186776=CARTESIAN_POINT('Ctrl Pts',(-6.76699998297921,-0.000479957709508635,
13.6971797837721));
#186777=CARTESIAN_POINT('',(-6.76699751798627,-0.00579582329898324,13.3028202162226));
#186778=CARTESIAN_POINT('Ctrl Pts',(3.09910619832131,6.01563211736941,12.6513039064363));
#186779=CARTESIAN_POINT('Ctrl Pts',(2.93978775740063,6.09770907256395,12.6597306285985));
#186780=CARTESIAN_POINT('Ctrl Pts',(2.7772501800563,6.1734306902204,12.6681573507607));
#186781=CARTESIAN_POINT('Ctrl Pts',(2.61203227770273,6.2425616841357,12.676584072923));
#186782=CARTESIAN_POINT('Ctrl Pts',(2.44666622100594,6.31175466925688,12.685018351503));
#186783=CARTESIAN_POINT('Ctrl Pts',(2.27861534458493,6.37434509232258,12.6934526300829));
#186784=CARTESIAN_POINT('Ctrl Pts',(2.10843755082295,6.43014619540487,12.7018869086629));
#186785=CARTESIAN_POINT('Ctrl Pts',(1.93817900638068,6.48597377654246,12.7103251893734));
#186786=CARTESIAN_POINT('Ctrl Pts',(1.76579185105679,6.53500551641699,12.7187634700838));
#186787=CARTESIAN_POINT('Ctrl Pts',(1.59184762273827,6.57710499733603,12.7272017507942));
#186788=CARTESIAN_POINT('Ctrl Pts',(1.41770634921698,6.61925216883287,12.7356495904464));
#186789=CARTESIAN_POINT('Ctrl Pts',(1.24200480411557,6.65445131830971,12.7440974300985));
#186790=CARTESIAN_POINT('Ctrl Pts',(1.06532440572475,6.68261722011423,12.7525452697506));
#186791=CARTESIAN_POINT('Ctrl Pts',(0.953184147250487,6.70049431082314,
12.7579071714147));
#186792=CARTESIAN_POINT('Ctrl Pts',(0.840649698346499,6.71553907890543,
12.7632690730787));
#186793=CARTESIAN_POINT('Ctrl Pts',(0.727870451699451,6.7277406018323,12.7686309747428));
#186794=CARTESIAN_POINT('Ctrl Pts',(0.554564637076018,6.74649045992548,
12.7768705113902));
#186795=CARTESIAN_POINT('Ctrl Pts',(0.380293753517344,6.75856551206301,
12.7851100480377));
#186796=CARTESIAN_POINT('Ctrl Pts',(0.20561140489293,6.76387558653898,12.7933495846851));
#186797=CARTESIAN_POINT('Ctrl Pts',(0.0311229417577409,6.76917976719455,
12.8015799760091));
#186798=CARTESIAN_POINT('Ctrl Pts',(-0.143775724472965,6.76773391047996,
12.809810367333));
#186799=CARTESIAN_POINT('Ctrl Pts',(-0.318523926401962,6.7594993533774,
12.8180407586569));
#186800=CARTESIAN_POINT('Ctrl Pts',(-0.493109343101404,6.75127246710781,
12.8262634830284));
#186801=CARTESIAN_POINT('Ctrl Pts',(-0.667544221215973,6.73626949137306,
12.8344862074));
#186802=CARTESIAN_POINT('Ctrl Pts',(-0.841265839795262,6.71450376325709,
12.8427089317715));
#186803=CARTESIAN_POINT('Ctrl Pts',(-1.01483352756912,6.69275732126156,
12.8509243701726));
#186804=CARTESIAN_POINT('Ctrl Pts',(-1.18768886365077,6.66426011422477,
12.8591398085737));
#186805=CARTESIAN_POINT('Ctrl Pts',(-1.35927233151704,6.62907744175404,
12.8673552469747));
#186806=CARTESIAN_POINT('Ctrl Pts',(-1.53076761825765,6.5939128505571,12.8755664632522));
#186807=CARTESIAN_POINT('Ctrl Pts',(-1.70099199077603,6.55206970800288,
12.8837776795297));
#186808=CARTESIAN_POINT('Ctrl Pts',(-1.86939381828759,6.50366479395642,
12.8919888958072));
#186809=CARTESIAN_POINT('Ctrl Pts',(-2.0377391719983,6.45527611256917,12.9001973584412));
#186810=CARTESIAN_POINT('Ctrl Pts',(-2.20426285656253,6.40033014149029,
12.9084058210752));
#186811=CARTESIAN_POINT('Ctrl Pts',(-2.36842606338852,6.3389941617154,12.9166142837092));
#186812=CARTESIAN_POINT('Ctrl Pts',(-2.44156374890655,6.31166787048091,
12.920271302662));
#186813=CARTESIAN_POINT('Ctrl Pts',(-2.51423310581203,6.2830739131063,12.9239283216148));
#186814=CARTESIAN_POINT('Ctrl Pts',(-2.58638754591579,6.25323024222935,
12.9275853405676));
#186815=CARTESIAN_POINT('Ctrl Pts',(-2.76118055184715,6.18093441493019,
12.9364444119509));
#186816=CARTESIAN_POINT('Ctrl Pts',(-2.93276884545542,6.10137685054242,
12.9453034833343));
#186817=CARTESIAN_POINT('Ctrl Pts',(-3.10058001914121,6.01487261252492,
12.9541625547176));
#186818=CARTESIAN_POINT('Ctrl Pts',(-3.26870647417205,5.9282058515245,12.9630382704035));
#186819=CARTESIAN_POINT('Ctrl Pts',(-3.43304139711229,5.83456645337312,
12.9719139860894));
#186820=CARTESIAN_POINT('Ctrl Pts',(-3.59303943281136,5.73431396369806,
12.9807897017753));
#186821=CARTESIAN_POINT('Ctrl Pts',(-3.75349405552794,5.63377538310285,
12.9896907461256));
#186822=CARTESIAN_POINT('Ctrl Pts',(-3.90958680346882,5.52658608439311,
12.9985917904759));
#186823=CARTESIAN_POINT('Ctrl Pts',(-4.06080113035424,5.41314910008155,
13.0074928348262));
#186824=CARTESIAN_POINT('Ctrl Pts',(-4.21222103428513,5.29955789731357,
13.016405980215));
#186825=CARTESIAN_POINT('Ctrl Pts',(-4.35874906540356,5.17970220284822,
13.0253191256039));
#186826=CARTESIAN_POINT('Ctrl Pts',(-4.49990293266634,5.05402439612047,
13.0342322709927));
#186827=CARTESIAN_POINT('Ctrl Pts',(-4.64137019955671,4.92806755079045,
13.0431652059665));
#186828=CARTESIAN_POINT('Ctrl Pts',(-4.77743924181069,4.79626291060941,
13.0520981409403));
#186829=CARTESIAN_POINT('Ctrl Pts',(-4.90766367778078,4.659090708045,13.061031075914));
#186830=CARTESIAN_POINT('Ctrl Pts',(-5.0316187207818,4.52852238466734,13.0695339527401));
#186831=CARTESIAN_POINT('Ctrl Pts',(-5.15027854017729,4.39309129018316,
13.0780368295662));
#186832=CARTESIAN_POINT('Ctrl Pts',(-5.2632929832141,4.25323829250716,13.0865397063923));
#186833=CARTESIAN_POINT('Ctrl Pts',(-5.37091165595206,4.12006244715601,
13.0946366212104));
#186834=CARTESIAN_POINT('Ctrl Pts',(-5.47364117613993,3.98259047815141,
13.1027335360284));
#186835=CARTESIAN_POINT('Ctrl Pts',(-5.57111288479381,3.84122249093754,
13.1108304508465));
#186836=CARTESIAN_POINT('Ctrl Pts',(-5.66844891615202,3.70005128314268,
13.1189160950351));
#186837=CARTESIAN_POINT('Ctrl Pts',(-5.76054150709384,3.55499516330702,
13.1270017392237));
#186838=CARTESIAN_POINT('Ctrl Pts',(-5.84706149027389,3.40648806382116,
13.1350873834124));
#186839=CARTESIAN_POINT('Ctrl Pts',(-5.93351204297753,3.25810013817573,
13.1431665390407));
#186840=CARTESIAN_POINT('Ctrl Pts',(-6.01439870058324,3.10626706157592,
13.1512456946691));
#186841=CARTESIAN_POINT('Ctrl Pts',(-6.08943463889467,2.95145299448082,
13.1593248502974));
#186842=CARTESIAN_POINT('Ctrl Pts',(-6.1644250602964,2.79673283782478,13.1673991050981));
#186843=CARTESIAN_POINT('Ctrl Pts',(-6.2335716645703,2.63903562198289,13.1754733598989));
#186844=CARTESIAN_POINT('Ctrl Pts',(-6.29663282907075,2.47885135009514,
13.1835476146996));
#186845=CARTESIAN_POINT('Ctrl Pts',(-6.35966808884399,2.31873287987628,
13.1916185526988));
#186846=CARTESIAN_POINT('Ctrl Pts',(-6.41662274988487,2.15612973203305,
13.199689490698));
#186847=CARTESIAN_POINT('Ctrl Pts',(-6.46730278219813,1.99155309328482,
13.2077604286972));
#186848=CARTESIAN_POINT('Ctrl Pts',(-6.51798247269528,1.82697756453877,
13.2158313122612));
#186849=CARTESIAN_POINT('Ctrl Pts',(-6.56238749793609,1.66042892221144,
13.2239021958253));
#186850=CARTESIAN_POINT('Ctrl Pts',(-6.60037323290307,1.49243498564484,
13.2319730793893));
#186851=CARTESIAN_POINT('Ctrl Pts',(-6.63835735458364,1.32444818392333,
13.240043620176));
#186852=CARTESIAN_POINT('Ctrl Pts',(-6.66992265171161,1.1550165732352,13.2481141609628));
#186853=CARTESIAN_POINT('Ctrl Pts',(-6.69497542089426,0.984679193251125,
13.2561847017495));
#186854=CARTESIAN_POINT('Ctrl Pts',(-6.72004235822306,0.81424548200425,
13.2642598066864));
#186855=CARTESIAN_POINT('Ctrl Pts',(-6.73858935704497,0.642905345832317,
13.2723349116234));
#186856=CARTESIAN_POINT('Ctrl Pts',(-6.75057444037095,0.471204546890744,
13.2804100165603));
#186857=CARTESIAN_POINT('Ctrl Pts',(-6.76166152477046,0.312368667526999,
13.2878800831035));
#186858=CARTESIAN_POINT('Ctrl Pts',(-6.76713371623367,0.153224434099281,
13.2953501496467));
#186859=CARTESIAN_POINT('Ctrl Pts',(-6.76699751798686,-0.00579582260286099,
13.3028202161899));
#186860=CARTESIAN_POINT('Ctrl Pts',(-6.76699751798627,-0.00579582329897739,
13.3028202162226));
#186861=CARTESIAN_POINT('Ctrl Pts',(-6.76681198988727,-0.222411844982174,
13.3129958764175));
#186862=CARTESIAN_POINT('Ctrl Pts',(-6.75622188990783,-0.438543524588682,
13.3231715366123));
#186863=CARTESIAN_POINT('Ctrl Pts',(-6.7353881739906,-0.653326216883703,
13.3333471968072));
#186864=CARTESIAN_POINT('Ctrl Pts',(-6.71431012283039,-0.870627854023666,
13.343642195886));
#186865=CARTESIAN_POINT('Ctrl Pts',(-6.68274685485897,-1.08654879994134,
13.3539371949648));
#186866=CARTESIAN_POINT('Ctrl Pts',(-6.64091266108794,-1.30021845387683,
13.3642321940437));
#186867=CARTESIAN_POINT('Ctrl Pts',(-6.5985826378675,-1.51642057461325,
13.3746492120564));
#186868=CARTESIAN_POINT('Ctrl Pts',(-6.54573678032153,-1.73031785842102,
13.3850662300692));
#186869=CARTESIAN_POINT('Ctrl Pts',(-6.48264491585991,-1.9410316573605,
13.3954832480819));
#186870=CARTESIAN_POINT('Ctrl Pts',(-6.46454534874988,-2.00148047397829,
13.3984716447352));
#186871=CARTESIAN_POINT('Ctrl Pts',(-6.44560285358692,-2.06166743370604,
13.4014600413885));
#186872=CARTESIAN_POINT('Ctrl Pts',(-6.42582451980347,-2.12157211536458,
13.4044484380418));
#186873=CARTESIAN_POINT('Ctrl Pts',(-6.37241879311197,-2.28332755397866,
13.4125177474518));
#186874=CARTESIAN_POINT('Ctrl Pts',(-6.3128033732122,-2.44336160887837,
13.4205870568618));
#186875=CARTESIAN_POINT('Ctrl Pts',(-6.247104180371,-2.6011494304617,13.4286563662718));
#186876=CARTESIAN_POINT('Ctrl Pts',(-6.1814869322611,-2.75874044779092,
13.436715611062));
#186877=CARTESIAN_POINT('Ctrl Pts',(-6.10980115115273,-2.91409046625502,
13.4447748558523));
#186878=CARTESIAN_POINT('Ctrl Pts',(-6.03222299244041,-3.06668791523907,
13.4528341006425));
#186879=CARTESIAN_POINT('Ctrl Pts',(-5.95472457035731,-3.21912852102893,
13.4608850619542));
#186880=CARTESIAN_POINT('Ctrl Pts',(-5.87134599053485,-3.36882185760112,
13.468936023266));
#186881=CARTESIAN_POINT('Ctrl Pts',(-5.78231210247125,-3.51527463359758,
13.4769869845777));
#186882=CARTESIAN_POINT('Ctrl Pts',(-5.69335021641091,-3.6616089727439,
13.48503143505));
#186883=CARTESIAN_POINT('Ctrl Pts',(-5.59874231767048,-3.8047076500584,
13.4930758855224));
#186884=CARTESIAN_POINT('Ctrl Pts',(-5.49875990269619,-3.94410047190745,
13.5011203359947));
#186885=CARTESIAN_POINT('Ctrl Pts',(-5.398836458621,-4.08341107809853,13.5091600417479));
#186886=CARTESIAN_POINT('Ctrl Pts',(-5.29354502568335,-4.2190198775832,
13.5171997475012));
#186887=CARTESIAN_POINT('Ctrl Pts',(-5.18320121548749,-4.35048435921439,
13.5252394532544));
#186888=CARTESIAN_POINT('Ctrl Pts',(-5.07047569751661,-4.48478642618439,
13.5334526914393));
#186889=CARTESIAN_POINT('Ctrl Pts',(-4.95247742482353,-4.61476289528958,
13.5416659296241));
#186890=CARTESIAN_POINT('Ctrl Pts',(-4.82958762202021,-4.73997599163004,
13.549879167809));
#186891=CARTESIAN_POINT('Ctrl Pts',(-4.70933300468522,-4.86250408299535,
13.5579162855557));
#186892=CARTESIAN_POINT('Ctrl Pts',(-4.58439479463962,-4.98047074881998,
13.5659534033025));
#186893=CARTESIAN_POINT('Ctrl Pts',(-4.45516846992223,-5.09350202754557,
13.5739905210492));
#186894=CARTESIAN_POINT('Ctrl Pts',(-4.32592847386177,-5.20654526427888,
13.5820284890731));
#186895=CARTESIAN_POINT('Ctrl Pts',(-4.1923997409979,-5.31465182818817,
13.590066457097));
#186896=CARTESIAN_POINT('Ctrl Pts',(-4.05501163878879,-5.41748738893663,
13.5981044251209));
#186897=CARTESIAN_POINT('Ctrl Pts',(-3.91758178012598,-5.5203542045628,
13.6061448361296));
#186898=CARTESIAN_POINT('Ctrl Pts',(-3.77629051625435,-5.61794660447148,
13.6141852471383));
#186899=CARTESIAN_POINT('Ctrl Pts',(-3.63159691743829,-5.70997310232305,
13.6222256581469));
#186900=CARTESIAN_POINT('Ctrl Pts',(-3.48143472688355,-5.80547767626098,
13.6305699507756));
#186901=CARTESIAN_POINT('Ctrl Pts',(-3.32760837488391,-5.89498717056716,
13.6389142434043));
#186902=CARTESIAN_POINT('Ctrl Pts',(-3.17065877865388,-5.97822815802016,
13.647258536033));
#186903=CARTESIAN_POINT('Ctrl Pts',(-3.01915787748253,-6.0585793339164,
13.655313146451));
#186904=CARTESIAN_POINT('Ctrl Pts',(-2.86474731244965,-6.13308984738742,
13.6633677568689));
#186905=CARTESIAN_POINT('Ctrl Pts',(-2.70793328800325,-6.20156321484543,
13.6714223672869));
#186906=CARTESIAN_POINT('Ctrl Pts',(-2.55100055311482,-6.27008841761438,
13.6794830751592));
#186907=CARTESIAN_POINT('Ctrl Pts',(-2.3916610814457,-6.33256723913197,
13.6875437830316));
#186908=CARTESIAN_POINT('Ctrl Pts',(-2.230436169122,-6.38885306572881,13.6956044909039));
#186909=CARTESIAN_POINT('Ctrl Pts',(-2.0689839393402,-6.44521825196582,
13.7036765638909));
#186910=CARTESIAN_POINT('Ctrl Pts',(-1.90564131873512,-6.49537291335649,
13.711748636878));
#186911=CARTESIAN_POINT('Ctrl Pts',(-1.74094027670692,-6.53922135677786,
13.7198207098651));
#186912=CARTESIAN_POINT('Ctrl Pts',(-1.72368912874173,-6.54381413880395,
13.7206661964738));
#186913=CARTESIAN_POINT('Ctrl Pts',(-1.70642308228228,-6.54833778267619,
13.7215116830826));
#186914=CARTESIAN_POINT('Ctrl Pts',(-1.68914275140194,-6.55279221136962,
13.7223571696914));
#186915=CARTESIAN_POINT('Ctrl Pts',(-1.51883177720467,-6.596694037991,13.7306900916133));
#186916=CARTESIAN_POINT('Ctrl Pts',(-1.34658947508686,-6.63400834483046,
13.7390230135352));
#186917=CARTESIAN_POINT('Ctrl Pts',(-1.17296026482133,-6.6645669939727,
13.7473559354571));
#186918=CARTESIAN_POINT('Ctrl Pts',(-0.999536242203163,-6.69508953019757,
13.7556790098848));
#186919=CARTESIAN_POINT('Ctrl Pts',(-0.824728916187795,-6.71887225278418,
13.7640020843125));
#186920=CARTESIAN_POINT('Ctrl Pts',(-0.649096675008562,-6.73579709511004,
13.7723251587402));
#186921=CARTESIAN_POINT('Ctrl Pts',(-0.473639750263407,-6.7527050430264,
13.7806399250593));
#186922=CARTESIAN_POINT('Ctrl Pts',(-0.297359895085378,-6.76276871604712,
13.7889546913784));
#186923=CARTESIAN_POINT('Ctrl Pts',(-0.120824698974208,-6.7659212522847,
13.7972694576975));
#186924=CARTESIAN_POINT('Ctrl Pts',(0.055566661873148,-6.76907121993602,
13.8055774494094));
#186925=CARTESIAN_POINT('Ctrl Pts',(0.232212602718064,-6.7653212648013,
13.8138854411213));
#186926=CARTESIAN_POINT('Ctrl Pts',(0.408541186671082,-6.75465640123859,
13.8221934328333));
#186927=CARTESIAN_POINT('Ctrl Pts',(0.584758430663995,-6.7439982718392,
13.8304961785922));
#186928=CARTESIAN_POINT('Ctrl Pts',(0.760658370785872,-6.7264339564995,
13.8387989243511));
#186929=CARTESIAN_POINT('Ctrl Pts',(0.935669618472968,-6.7020005494678,
13.84710167011));
#186930=CARTESIAN_POINT('Ctrl Pts',(1.11060934463241,-6.67757712759202,
13.855401022801));
#186931=CARTESIAN_POINT('Ctrl Pts',(1.28466075797919,-6.64629025556816,
13.8637003754919));
#186932=CARTESIAN_POINT('Ctrl Pts',(1.45725784371774,-6.6082288532498,13.8719997281828));
#186933=CARTESIAN_POINT('Ctrl Pts',(1.62981822094923,-6.57017554595373,
13.8802973157406));
#186934=CARTESIAN_POINT('Ctrl Pts',(1.80092454724439,-6.5253506536969,13.8885949032983));
#186935=CARTESIAN_POINT('Ctrl Pts',(1.97002100750952,-6.47389420905001,
13.896892490856));
#186936=CARTESIAN_POINT('Ctrl Pts',(2.13910960344286,-6.4224401575375,13.9051896925099));
#186937=CARTESIAN_POINT('Ctrl Pts',(2.30618818685144,-6.36435526966563,
13.9134868941637));
#186938=CARTESIAN_POINT('Ctrl Pts',(2.47071592772062,-6.29982950598726,
13.9217840958176));
#186939=CARTESIAN_POINT('Ctrl Pts',(2.63526335596345,-6.23529602116221,
13.9300822903138));
#186940=CARTESIAN_POINT('Ctrl Pts',(2.79725900980732,-6.16432025236565,
13.93838048481));
#186941=CARTESIAN_POINT('Ctrl Pts',(2.95618169245446,-6.08714044533204,
13.9466786793062));
#186942=CARTESIAN_POINT('Ctrl Pts',(3.11521614729845,-6.00990635682997,
13.9549827100204));
#186943=CARTESIAN_POINT('Ctrl Pts',(3.27117299899495,-5.92645966338178,
13.9632867407347));
#186944=CARTESIAN_POINT('Ctrl Pts',(3.42355453364015,-5.83708517628379,
13.9715907714489));
#186945=CARTESIAN_POINT('Ctrl Pts',(3.57599147841468,-5.74767819015697,
13.9798978217378));
#186946=CARTESIAN_POINT('Ctrl Pts',(3.72485021859095,-5.65233929653858,
13.9882048720267));
#186947=CARTESIAN_POINT('Ctrl Pts',(3.86966155518096,-5.55139698169339,
13.9965119223155));
#186948=CARTESIAN_POINT('Ctrl Pts',(4.01462771956415,-5.45034674245351,
14.0048278542451));
#186949=CARTESIAN_POINT('Ctrl Pts',(4.15553755291809,-5.34368131701438,
14.0131437861747));
#186950=CARTESIAN_POINT('Ctrl Pts',(4.29195364006265,-5.23177053697436,
14.0214597181043));
#186951=CARTESIAN_POINT('Ctrl Pts',(4.3947870107126,-5.14740979210572,14.0277284458498));
#186952=CARTESIAN_POINT('Ctrl Pts',(4.49506748575086,-5.06006924447631,
14.0339971735954));
#186953=CARTESIAN_POINT('Ctrl Pts',(4.59262151425816,-4.96992118919134,
14.0402659013409));
#186954=CARTESIAN_POINT('Ctrl Pts',(4.72412471404781,-4.84840126934609,
14.0487161700766));
#186955=CARTESIAN_POINT('Ctrl Pts',(4.85091351288786,-4.7215556920617,14.0571664388124));
#186956=CARTESIAN_POINT('Ctrl Pts',(4.97254906232811,-4.58977611902147,
14.0656167075482));
#186957=CARTESIAN_POINT('Ctrl Pts',(5.09407726426018,-4.45811284593517,
14.0740595186345));
#186958=CARTESIAN_POINT('Ctrl Pts',(5.2104610577621,-4.32152449875464,14.0825023297208));
#186959=CARTESIAN_POINT('Ctrl Pts',(5.32129747799463,-4.18044042544419,
14.090945140807));
#186960=CARTESIAN_POINT('Ctrl Pts',(5.43205117198079,-4.03946165466683,
14.0993816503359));
#186961=CARTESIAN_POINT('Ctrl Pts',(5.53726554229373,-3.89399410670221,
14.1078181598647));
#186962=CARTESIAN_POINT('Ctrl Pts',(5.63657680515809,-3.74450142469646,
14.1162546693936));
#186963=CARTESIAN_POINT('Ctrl Pts',(5.73581700545794,-3.59511571276694,
14.1246851421449));
#186964=CARTESIAN_POINT('Ctrl Pts',(5.82916234070514,-3.44171088734183,
14.1331156148961));
#186965=CARTESIAN_POINT('Ctrl Pts',(5.91629127695028,-3.28478104693175,
14.1415460876474));
#186966=CARTESIAN_POINT('Ctrl Pts',(6.00338275669556,-3.1279186702461,14.1499729361607));
#186967=CARTESIAN_POINT('Ctrl Pts',(6.08426300432896,-2.9675345889329,14.158399784674));
#186968=CARTESIAN_POINT('Ctrl Pts',(6.15865519724923,-2.80414963249023,
14.1668266331873));
#186969=CARTESIAN_POINT('Ctrl Pts',(6.2330244279481,-2.64081510716667,14.1752508806325));
#186970=CARTESIAN_POINT('Ctrl Pts',(6.30090946041277,-2.47448185532352,
14.1836751280776));
#186971=CARTESIAN_POINT('Ctrl Pts',(6.3620804464561,-2.3056932564461,14.1920993755228));
#186972=CARTESIAN_POINT('Ctrl Pts',(6.37931608940755,-2.25813508855148,
14.1944730060704));
#186973=CARTESIAN_POINT('Ctrl Pts',(6.39601899827916,-2.21038211659263,
14.196846636618));
#186974=CARTESIAN_POINT('Ctrl Pts',(6.41218472486389,-2.16244677488769,
14.1992202671656));
#186975=CARTESIAN_POINT('Ctrl Pts',(6.47088335321927,-1.98839095419338,
14.2078390481797));
#186976=CARTESIAN_POINT('Ctrl Pts',(6.52246944331495,-1.81200728260076,
14.2164578291937));
#186977=CARTESIAN_POINT('Ctrl Pts',(6.56678655545798,-1.6338920818268,14.2250766102078));
#186978=CARTESIAN_POINT('Ctrl Pts',(6.6111302886318,-1.45566988829057,14.2337005684733));
#186979=CARTESIAN_POINT('Ctrl Pts',(6.64819625633659,-1.27571438498409,
14.2423245267389));
#186980=CARTESIAN_POINT('Ctrl Pts',(6.67787902854769,-1.09463266901869,
14.2509484850044));
#186981=CARTESIAN_POINT('Ctrl Pts',(6.70863413762619,-0.907009091037845,
14.2598839973366));
#186982=CARTESIAN_POINT('Ctrl Pts',(6.73146259370863,-0.718176768294806,
14.2688195096687));
#186983=CARTESIAN_POINT('Ctrl Pts',(6.7463057891222,-0.528816792146654,
14.2777550220009));
#186984=CARTESIAN_POINT('Ctrl Pts',(6.76065823142376,-0.345717529746228,
14.2863951039785));
#186985=CARTESIAN_POINT('Ctrl Pts',(6.76754502205472,-0.16212525272967,
14.295035185956));
#186986=CARTESIAN_POINT('Ctrl Pts',(6.76696633971174,0.0213437861759871,
14.3036752679336));
#186987=CARTESIAN_POINT('Ctrl Pts',(6.76635797703756,0.214222861357321,
14.3127584954431));
#186988=CARTESIAN_POINT('Ctrl Pts',(6.7574982435815,0.406965331762482,14.3218417229525));
#186989=CARTESIAN_POINT('Ctrl Pts',(6.74044920709308,0.598860156128475,
14.330924950462));
#186990=CARTESIAN_POINT('Ctrl Pts',(6.72340017060467,0.790754980494468,
14.3400081779715));
#186991=CARTESIAN_POINT('Ctrl Pts',(6.69816191523472,0.981801778793228,
14.3490914054809));
#186992=CARTESIAN_POINT('Ctrl Pts',(6.66485893493886,1.17130029341997,14.3581746329904));
#186993=CARTESIAN_POINT('Ctrl Pts',(6.63169759884853,1.35999283313652,14.3672192277249));
#186994=CARTESIAN_POINT('Ctrl Pts',(6.59051023319254,1.54732463590756,14.3762638224594));
#186995=CARTESIAN_POINT('Ctrl Pts',(6.5414264608003,1.73263638941978,14.3853084171939));
#186996=CARTESIAN_POINT('Ctrl Pts',(6.49238773050414,1.91777809019567,14.3943447120874));
#186997=CARTESIAN_POINT('Ctrl Pts',(6.43546712139934,2.10090321289551,14.4033810069809));
#186998=CARTESIAN_POINT('Ctrl Pts',(6.37084485522845,2.28136468601783,14.4124173018744));
#186999=CARTESIAN_POINT('Ctrl Pts',(6.3063369432251,2.46150681841201,14.4214376063355));
#187000=CARTESIAN_POINT('Ctrl Pts',(6.23415466900139,2.63899448988547,14.4304579107966));
#187001=CARTESIAN_POINT('Ctrl Pts',(6.15452730999182,2.81319792950388,14.4394782152577));
#187002=CARTESIAN_POINT('Ctrl Pts',(6.07500022616442,2.98718199374854,14.4484871603985));
#187003=CARTESIAN_POINT('Ctrl Pts',(5.98804686670153,3.15788986416072,14.4574961055393));
#187004=CARTESIAN_POINT('Ctrl Pts',(5.89394459667191,3.32471142978785,14.4665050506801));
#187005=CARTESIAN_POINT('Ctrl Pts',(5.8000560129413,3.49115417901724,14.475493538417));
#187006=CARTESIAN_POINT('Ctrl Pts',(5.69905103909432,3.6537280320524,14.484482026154));
#187007=CARTESIAN_POINT('Ctrl Pts',(5.59125270914414,3.81184760221187,14.4934705138909));
#187008=CARTESIAN_POINT('Ctrl Pts',(5.49667450204816,3.95057577600994,14.5013566755323));
#187009=CARTESIAN_POINT('Ctrl Pts',(5.39686774681314,4.08587540680076,14.5092428371738));
#187010=CARTESIAN_POINT('Ctrl Pts',(5.29208000568106,4.21736626503683,14.5171289988152));
#187011=CARTESIAN_POINT('Ctrl Pts',(5.18417003098441,4.35277499731603,14.5252501348754));
#187012=CARTESIAN_POINT('Ctrl Pts',(5.07102484814056,4.48408297360082,14.5333712709357));
#187013=CARTESIAN_POINT('Ctrl Pts',(4.95299907767393,4.61086641929271,14.5414924069959));
#187014=CARTESIAN_POINT('Ctrl Pts',(4.83498371114816,4.73763868905696,14.5496128271802));
#187015=CARTESIAN_POINT('Ctrl Pts',(4.71208886415114,4.85988695540559,14.5577332473644));
#187016=CARTESIAN_POINT('Ctrl Pts',(4.5847075292805,4.97722270658634,14.5658536675486));
#187017=CARTESIAN_POINT('Ctrl Pts',(4.45727339209945,5.09460709596643,14.5739774538221));
#187018=CARTESIAN_POINT('Ctrl Pts',(4.32534932020104,5.20707465256417,14.5821012400956));
#187019=CARTESIAN_POINT('Ctrl Pts',(4.1893633935718,5.31427543100662,14.5902250263692));
#187020=CARTESIAN_POINT('Ctrl Pts',(4.05334626534985,5.42150080636957,14.5983506766229));
#187021=CARTESIAN_POINT('Ctrl Pts',(3.9132657186847,5.52345677640222,14.6064763268765));
#187022=CARTESIAN_POINT('Ctrl Pts',(3.76958042428815,5.6198356225804,14.6146019771302));
#187023=CARTESIAN_POINT('Ctrl Pts',(3.62577782930959,5.71629314970361,14.6227342609334));
#187024=CARTESIAN_POINT('Ctrl Pts',(3.47836491883093,5.80716426430875,14.6308665447365));
#187025=CARTESIAN_POINT('Ctrl Pts',(3.32782717117971,5.89218595419035,14.6389988285396));
#187026=CARTESIAN_POINT('Ctrl Pts',(3.2523509209764,5.93481392251282,14.6430761732364));
#187027=CARTESIAN_POINT('Ctrl Pts',(3.17608952358117,5.97597219538194,14.6471535179331));
#187028=CARTESIAN_POINT('Ctrl Pts',(3.09910619832135,6.0156321173694,14.6512308626299));
#187029=CARTESIAN_POINT('Origin',(0.,0.,4.30282021618968));
#187030=CARTESIAN_POINT('',(3.09910619832131,6.01563211736941,17.0457499898821));
#187031=CARTESIAN_POINT('',(3.09910619832134,6.0156321173694,16.6515631567322));
#187032=CARTESIAN_POINT('',(3.09910619832133,6.0156321173694,4.30282021618968));
#187033=CARTESIAN_POINT('',(-6.76699967914366,0.00208385931223479,15.6971797838561));
#187034=CARTESIAN_POINT('Ctrl Pts',(-6.76699967914366,0.0020838593122393,
15.6971797838561));
#187035=CARTESIAN_POINT('Ctrl Pts',(-6.7670521202577,-0.16821026745595,
15.7051773033024));
#187036=CARTESIAN_POINT('Ctrl Pts',(-6.76067197387033,-0.338604812283096,
15.7131748227487));
#187037=CARTESIAN_POINT('Ctrl Pts',(-6.74786284543056,-0.508562699436209,
15.721172342195));
#187038=CARTESIAN_POINT('Ctrl Pts',(-6.73505487207517,-0.678505260355175,
15.7291691404518));
#187039=CARTESIAN_POINT('Ctrl Pts',(-6.71581909033154,-0.848010863801087,
15.7371659387085));
#187040=CARTESIAN_POINT('Ctrl Pts',(-6.690211171013,-1.01654487714655,15.7451627369653));
#187041=CARTESIAN_POINT('Ctrl Pts',(-6.67000489770966,-1.14952890807099,
15.7514727182299));
#187042=CARTESIAN_POINT('Ctrl Pts',(-6.64583223149171,-1.28190798807919,
15.7577826994946));
#187043=CARTESIAN_POINT('Ctrl Pts',(-6.61774319506431,-1.41342279738939,
15.7640926807593));
#187044=CARTESIAN_POINT('Ctrl Pts',(-6.57937648024145,-1.59305840706321,
15.772711461697));
#187045=CARTESIAN_POINT('Ctrl Pts',(-6.53370534698295,-1.77106534870478,
15.7813302426348));
#187046=CARTESIAN_POINT('Ctrl Pts',(-6.48089964856677,-1.94685098176699,
15.7899490235725));
#187047=CARTESIAN_POINT('Ctrl Pts',(-6.42806223008849,-2.12274220819063,
15.7985729817596));
#187048=CARTESIAN_POINT('Ctrl Pts',(-6.36808178102674,-2.29640917181106,
15.8071969399466));
#187049=CARTESIAN_POINT('Ctrl Pts',(-6.30117751899081,-2.46727600283486,
15.8158208981337));
#187050=CARTESIAN_POINT('Ctrl Pts',(-6.23185623424901,-2.64431566945536,
15.8247564105045));
#187051=CARTESIAN_POINT('Ctrl Pts',(-6.15510167929091,-2.81834877879652,
15.8336919228754));
#187052=CARTESIAN_POINT('Ctrl Pts',(-6.07121110395118,-2.98875973126979,
15.8426274352463));
#187053=CARTESIAN_POINT('Ctrl Pts',(-5.99009416167758,-3.15353646976019,
15.8512675171415));
#187054=CARTESIAN_POINT('Ctrl Pts',(-5.90230570237236,-3.31492648760728,
15.8599075990367));
#187055=CARTESIAN_POINT('Ctrl Pts',(-5.80816043205675,-3.47239994751331,
15.868547680932));
#187056=CARTESIAN_POINT('Ctrl Pts',(-5.70918649535935,-3.63795014668964,
15.8776309085406));
#187057=CARTESIAN_POINT('Ctrl Pts',(-5.6031867602438,-3.79917114959769,
15.8867141361493));
#187058=CARTESIAN_POINT('Ctrl Pts',(-5.49057753511751,-3.95548319815202,
15.895797363758));
#187059=CARTESIAN_POINT('Ctrl Pts',(-5.37796830999122,-4.11179524670636,
15.9048805913667));
#187060=CARTESIAN_POINT('Ctrl Pts',(-5.25874986119406,-4.26319805706581,
15.9139638189754));
#187061=CARTESIAN_POINT('Ctrl Pts',(-5.13338667445239,-4.40915300829475,
15.9230470465841));
#187062=CARTESIAN_POINT('Ctrl Pts',(-5.00855668194227,-4.55448718447732,
15.9320916414435));
#187063=CARTESIAN_POINT('Ctrl Pts',(-4.87751949739731,-4.69455452798562,
15.9411362363029));
#187064=CARTESIAN_POINT('Ctrl Pts',(-4.74072311736272,-4.82885424552271,
15.9501808311623));
#187065=CARTESIAN_POINT('Ctrl Pts',(-4.6040522695395,-4.96303072192927,
15.9592171261822));
#187066=CARTESIAN_POINT('Ctrl Pts',(-4.4616329473042,-5.09144997275945,
15.9682534212022));
#187067=CARTESIAN_POINT('Ctrl Pts',(-4.31395041021026,-5.21364755792399,
15.9772897162221));
#187068=CARTESIAN_POINT('Ctrl Pts',(-4.16652920894673,-5.33562890487904,
15.9863100208094));
#187069=CARTESIAN_POINT('Ctrl Pts',(-4.01386357408612,-5.45141041972696,
15.9953303253966));
#187070=CARTESIAN_POINT('Ctrl Pts',(-3.85647211850355,-5.56056757887221,
16.0043506299839));
#187071=CARTESIAN_POINT('Ctrl Pts',(-3.69927886688481,-5.66958727578012,
16.0133595752498));
#187072=CARTESIAN_POINT('Ctrl Pts',(-3.53737186609623,-5.77199912975818,
16.0223685205158));
#187073=CARTESIAN_POINT('Ctrl Pts',(-3.37130104557159,-5.86742006849074,
16.0313774657817));
#187074=CARTESIAN_POINT('Ctrl Pts',(-3.2056073367235,-5.96262432647187,
16.0403659536401));
#187075=CARTESIAN_POINT('Ctrl Pts',(-3.03576888732917,-6.05086923855594,
16.0493544414985));
#187076=CARTESIAN_POINT('Ctrl Pts',(-2.86236227854642,-6.1318163040289,
16.0583429293568));
#187077=CARTESIAN_POINT('Ctrl Pts',(-2.71022184515229,-6.20283621330161,
16.0662290903742));
#187078=CARTESIAN_POINT('Ctrl Pts',(-2.55533529787698,-6.26823905314927,
16.0741152513916));
#187079=CARTESIAN_POINT('Ctrl Pts',(-2.39810960016431,-6.32782421892389,
16.0820014124089));
#187080=CARTESIAN_POINT('Ctrl Pts',(-2.23619267053671,-6.38918726093253,
16.0901228772652));
#187081=CARTESIAN_POINT('Ctrl Pts',(-2.07186682032972,-6.4443512810337,
16.0982443421215));
#187082=CARTESIAN_POINT('Ctrl Pts',(-1.90565336498755,-6.49313285344691,
16.1063658069778));
#187083=CARTESIAN_POINT('Ctrl Pts',(-1.73945176311115,-6.54191094701602,
16.1144866926541));
#187084=CARTESIAN_POINT('Ctrl Pts',(-1.57136317559847,-6.58430739639462,
16.1226075783304));
#187085=CARTESIAN_POINT('Ctrl Pts',(-1.40192394512038,-6.62018868704647,
16.1307284640067));
#187086=CARTESIAN_POINT('Ctrl Pts',(-1.23246446180843,-6.65607426653873,
16.1388503203611));
#187087=CARTESIAN_POINT('Ctrl Pts',(-1.06165437255065,-6.68544306195228,
16.1469721767155));
#187088=CARTESIAN_POINT('Ctrl Pts',(-0.890040024330387,-6.70821270943982,
16.1550940330699));
#187089=CARTESIAN_POINT('Ctrl Pts',(-0.7183004684055,-6.73099896938039,
16.1632218150301));
#187090=CARTESIAN_POINT('Ctrl Pts',(-0.545755844942392,-6.74717641700141,
16.1713495969904));
#187091=CARTESIAN_POINT('Ctrl Pts',(-0.372958076489848,-6.75671453246184,
16.1794773789507));
#187092=CARTESIAN_POINT('Ctrl Pts',(-0.200089916648785,-6.76625653339601,
16.1876084718673));
#187093=CARTESIAN_POINT('Ctrl Pts',(-0.0269687721454283,-6.76915380498501,
16.1957395647838));
#187094=CARTESIAN_POINT('Ctrl Pts',(0.145853877943232,-6.76542797214551,
16.2038706577004));
#187095=CARTESIAN_POINT('Ctrl Pts',(0.318865156731585,-6.76169807271519,
16.212010625365));
#187096=CARTESIAN_POINT('Ctrl Pts',(0.491576925299634,-6.75133065236554,
16.2201505930297));
#187097=CARTESIAN_POINT('Ctrl Pts',(0.663442506852932,-6.73439923379218,
16.2282905606944));
#187098=CARTESIAN_POINT('Ctrl Pts',(0.752579428421628,-6.72561786805402,
16.2325122998741));
#187099=CARTESIAN_POINT('Ctrl Pts',(0.841488875622032,-6.71507169204958,
16.2367340390539));
#187100=CARTESIAN_POINT('Ctrl Pts',(0.930095770580004,-6.70277635443323,
16.2409557782336));
#187101=CARTESIAN_POINT('Ctrl Pts',(1.10724095198241,-6.67819519950748,
16.2493959876912));
#187102=CARTESIAN_POINT('Ctrl Pts',(1.28354234272565,-6.64656898103088,
16.2578361971488));
#187103=CARTESIAN_POINT('Ctrl Pts',(1.45841803467938,-6.60797289916673,
16.2662764066064));
#187104=CARTESIAN_POINT('Ctrl Pts',(1.63316123238882,-6.56940605955255,
16.274710221355));
#187105=CARTESIAN_POINT('Ctrl Pts',(1.80648056009455,-6.52387995489371,
16.2831440361035));
#187106=CARTESIAN_POINT('Ctrl Pts',(1.97780258155493,-6.47152114640713,
16.291577850852));
#187107=CARTESIAN_POINT('Ctrl Pts',(2.14902113800454,-6.41919395851806,
16.3000065722405));
#187108=CARTESIAN_POINT('Ctrl Pts',(2.31824447484924,-6.36004239062506,
16.308435293629));
#187109=CARTESIAN_POINT('Ctrl Pts',(2.48491225687541,-6.29424340772029,
16.3168640150175));
#187110=CARTESIAN_POINT('Ctrl Pts',(2.65150497784993,-6.22847405826234,
16.3252889404193));
#187111=CARTESIAN_POINT('Ctrl Pts',(2.81554412915676,-6.15606338525117,
16.3337138658211));
#187112=CARTESIAN_POINT('Ctrl Pts',(2.97648699809208,-6.07723737813399,
16.3421387912228));
#187113=CARTESIAN_POINT('Ctrl Pts',(3.13738207766922,-5.99843477711309,
16.3505612149805));
#187114=CARTESIAN_POINT('Ctrl Pts',(3.29518240916876,-5.91322078735922,
16.3589836387382));
#187115=CARTESIAN_POINT('Ctrl Pts',(3.44936727774601,-5.82186863328391,
16.3674060624958));
#187116=CARTESIAN_POINT('Ctrl Pts',(3.60355457120818,-5.73051504250173,
16.375828618714));
#187117=CARTESIAN_POINT('Ctrl Pts',(3.75412599791343,-5.63302325874053,
16.3842511749322));
#187118=CARTESIAN_POINT('Ctrl Pts',(3.90058679873038,-5.52971171269989,
16.3926737311504));
#187119=CARTESIAN_POINT('Ctrl Pts',(4.04705254702083,-5.42639667677572,
16.4010965718841));
#187120=CARTESIAN_POINT('Ctrl Pts',(4.18940711987043,-5.31726167872461,
16.4095194126179));
#187121=CARTESIAN_POINT('Ctrl Pts',(4.32718590777588,-5.20266769259251,
16.4179422533516));
#187122=CARTESIAN_POINT('Ctrl Pts',(4.46498858531797,-5.08805383686558,
16.4263665545323));
#187123=CARTESIAN_POINT('Ctrl Pts',(4.59821363965822,-4.96797931922905,
16.4347908557129));
#187124=CARTESIAN_POINT('Ctrl Pts',(4.72643035747701,-4.84284472969346,
16.4432151568935));
#187125=CARTESIAN_POINT('Ctrl Pts',(4.85468721291069,-4.71767096738813,
16.4516420952603));
#187126=CARTESIAN_POINT('Ctrl Pts',(4.97793236736254,-4.58743420794316,
16.4600690336272));
#187127=CARTESIAN_POINT('Ctrl Pts',(5.09577246137279,-4.45257139436469,
16.468495971994));
#187128=CARTESIAN_POINT('Ctrl Pts',(5.21371850843952,-4.31758732216517,
16.4769304872376));
#187129=CARTESIAN_POINT('Ctrl Pts',(5.3262495646675,-4.17796913610944,16.4853650024813));
#187130=CARTESIAN_POINT('Ctrl Pts',(5.43301230000867,-4.03418719793151,
16.4937995177249));
#187131=CARTESIAN_POINT('Ctrl Pts',(5.53982660266573,-3.89033581184556,
16.5022381069117));
#187132=CARTESIAN_POINT('Ctrl Pts',(5.64086683560098,-3.74231693511833,
16.5106766960985));
#187133=CARTESIAN_POINT('Ctrl Pts',(5.73582313106234,-3.59062975105624,
16.5191152852852));
#187134=CARTESIAN_POINT('Ctrl Pts',(5.83088556617843,-3.43877301504117,
16.5275633069055));
#187135=CARTESIAN_POINT('Ctrl Pts',(5.9198503052829,-3.28324006553135,16.5360113285258));
#187136=CARTESIAN_POINT('Ctrl Pts',(6.00245295327843,-3.12455557538654,
16.544459350146));
#187137=CARTESIAN_POINT('Ctrl Pts',(6.049402972765,-3.03436185780838,16.5492610700584));
#187138=CARTESIAN_POINT('Ctrl Pts',(6.09429851404738,-2.94315041219203,
16.5540627899708));
#187139=CARTESIAN_POINT('Ctrl Pts',(6.13709797108092,-2.85102043018889,
16.5588645098832));
#187140=CARTESIAN_POINT('Ctrl Pts',(6.21053988270025,-2.69292959295087,
16.567104041734));
#187141=CARTESIAN_POINT('Ctrl Pts',(6.27797104774454,-2.53178012643929,
16.5753435735848));
#187142=CARTESIAN_POINT('Ctrl Pts',(6.33912819305863,-2.36806730309111,
16.5835831054356));
#187143=CARTESIAN_POINT('Ctrl Pts',(6.40021745821566,-2.20453618953507,
16.5918134919819));
#187144=CARTESIAN_POINT('Ctrl Pts',(6.45504644613494,-2.03844771477305,
16.6000438785282));
#187145=CARTESIAN_POINT('Ctrl Pts',(6.50339839124998,-1.87032039091893,
16.6082742650745));
#187146=CARTESIAN_POINT('Ctrl Pts',(6.55170529462805,-1.70234968427394,
16.6164969846923));
#187147=CARTESIAN_POINT('Ctrl Pts',(6.59354707346849,-1.53234425099341,
16.6247197043101));
#187148=CARTESIAN_POINT('Ctrl Pts',(6.62875554495046,-1.3608412564618,16.632942423928));
#187149=CARTESIAN_POINT('Ctrl Pts',(6.66393281918988,-1.18949022594039,
16.6411578576237));
#187150=CARTESIAN_POINT('Ctrl Pts',(6.69248842935787,-1.0166446262052,16.6493732913195));
#187151=CARTESIAN_POINT('Ctrl Pts',(6.71430442928295,-0.842855284679038,
16.6575887250153));
#187152=CARTESIAN_POINT('Ctrl Pts',(6.73610921747826,-0.669155257378234,
16.6657999366161));
#187153=CARTESIAN_POINT('Ctrl Pts',(6.75118124934669,-0.494512806498292,
16.674011148217));
#187154=CARTESIAN_POINT('Ctrl Pts',(6.75945386287016,-0.319487833461174,
16.6822223598178));
#187155=CARTESIAN_POINT('Ctrl Pts',(6.76772370221547,-0.144521554143462,
16.6904308178313));
#187156=CARTESIAN_POINT('Ctrl Pts',(6.76919864868656,0.0308266366642572,
16.6986392758448));
#187157=CARTESIAN_POINT('Ctrl Pts',(6.76386398338847,0.205992752834478,
16.7068477338583));
#187158=CARTESIAN_POINT('Ctrl Pts',(6.76148727351153,0.284033082478986,
16.7105047811415));
#187159=CARTESIAN_POINT('Ctrl Pts',(6.75775961671522,0.362037242752052,
16.7141618284247));
#187160=CARTESIAN_POINT('Ctrl Pts',(6.75268304404148,0.439955346273543,
16.7178188757079));
#187161=CARTESIAN_POINT('Ctrl Pts',(6.74038521729946,0.628709334201627,
16.7266779498838));
#187162=CARTESIAN_POINT('Ctrl Pts',(6.72018099636176,0.816761881881035,
16.7355370240597));
#187163=CARTESIAN_POINT('Ctrl Pts',(6.6921848122862,1.00346969969496,16.7443960982357));
#187164=CARTESIAN_POINT('Ctrl Pts',(6.66413602901304,1.19052830393664,16.7532718168297));
#187165=CARTESIAN_POINT('Ctrl Pts',(6.6282660647866,1.37623687292825,16.7621475354237));
#187166=CARTESIAN_POINT('Ctrl Pts',(6.58474016644733,1.55996344199958,16.7710232540177));
#187167=CARTESIAN_POINT('Ctrl Pts',(6.5410900574927,1.74421431478603,16.7799243014047));
#187168=CARTESIAN_POINT('Ctrl Pts',(6.48974035393471,1.92647161523584,16.7888253487917));
#187169=CARTESIAN_POINT('Ctrl Pts',(6.43090674026688,2.10611668669852,16.7977263961787));
#187170=CARTESIAN_POINT('Ctrl Pts',(6.37199314149442,2.28600598809953,16.8066395446617));
#187171=CARTESIAN_POINT('Ctrl Pts',(6.30557539532221,2.46327572216089,16.8155526931447));
#187172=CARTESIAN_POINT('Ctrl Pts',(6.23191745348678,2.63732702805831,16.8244658416277));
#187173=CARTESIAN_POINT('Ctrl Pts',(6.15809597087899,2.8117647754485,16.8333987797376));
#187174=CARTESIAN_POINT('Ctrl Pts',(6.07700224068373,2.98296956206476,16.8423317178475));
#187175=CARTESIAN_POINT('Ctrl Pts',(5.98894759872456,3.15036436935973,16.8512646559574));
#187176=CARTESIAN_POINT('Ctrl Pts',(5.90513234697211,3.30969995466581,16.8597675178158));
#187177=CARTESIAN_POINT('Ctrl Pts',(5.81501076015396,3.46558362627804,16.8682703796742));
#187178=CARTESIAN_POINT('Ctrl Pts',(5.71888781512685,3.61754214322289,16.8767732415327));
#187179=CARTESIAN_POINT('Ctrl Pts',(5.62593516252746,3.76448881897351,16.884995665057));
#187180=CARTESIAN_POINT('Ctrl Pts',(5.52719150557644,3.9080460880147,16.8932180885814));
#187181=CARTESIAN_POINT('Ctrl Pts',(5.42293159249036,4.04772799767598,16.9014405121058));
#187182=CARTESIAN_POINT('Ctrl Pts',(5.31877753311522,4.18726809014164,16.9096545875124));
#187183=CARTESIAN_POINT('Ctrl Pts',(5.20911858104267,4.32294037191763,16.9178686629189));
#187184=CARTESIAN_POINT('Ctrl Pts',(5.09427405997421,4.45428566684647,16.9260827383254));
#187185=CARTESIAN_POINT('Ctrl Pts',(4.97952524718653,4.58552150220118,16.9342899683463));
#187186=CARTESIAN_POINT('Ctrl Pts',(4.85959970585535,4.71243726296862,16.9424971983672));
#187187=CARTESIAN_POINT('Ctrl Pts',(4.73485855607681,4.83460478777182,16.9507044283881));
#187188=CARTESIAN_POINT('Ctrl Pts',(4.61020636846293,4.95668518585319,16.9589058052246));
#187189=CARTESIAN_POINT('Ctrl Pts',(4.48074567080274,5.07402384514603,16.9671071820611));
#187190=CARTESIAN_POINT('Ctrl Pts',(4.34687611502017,5.1862276310115,16.9753085588977));
#187191=CARTESIAN_POINT('Ctrl Pts',(4.21306369010708,5.29838353220441,16.9835064356718));
#187192=CARTESIAN_POINT('Ctrl Pts',(4.07484642885521,5.40540869456424,16.991704312446));
#187193=CARTESIAN_POINT('Ctrl Pts',(3.93265907105681,5.5069484863066,16.9999021892202));
#187194=CARTESIAN_POINT('Ctrl Pts',(3.79048911022339,5.60847585441139,17.0080990629645));
#187195=CARTESIAN_POINT('Ctrl Pts',(3.64435030833864,5.70451897517738,17.0162959367087));
#187196=CARTESIAN_POINT('Ctrl Pts',(3.4947087676297,5.79476484677783,17.024492810453));
#187197=CARTESIAN_POINT('Ctrl Pts',(3.36535225195713,5.87277721853478,17.0315785369294));
#187198=CARTESIAN_POINT('Ctrl Pts',(3.23337889068404,5.94645811785487,17.0386642634057));
#187199=CARTESIAN_POINT('Ctrl Pts',(3.09910619832132,6.01563211736941,17.0457499898821));
#187200=CARTESIAN_POINT('Ctrl Pts',(3.09910619832132,6.01563211736941,15.0460438035976));
#187201=CARTESIAN_POINT('Ctrl Pts',(2.94683466579232,6.09407867811004,15.0540873050715));
#187202=CARTESIAN_POINT('Ctrl Pts',(2.79144048604734,6.16681301554515,15.0621308065454));
#187203=CARTESIAN_POINT('Ctrl Pts',(2.63340158188346,6.23357723209825,15.0701743080193));
#187204=CARTESIAN_POINT('Ctrl Pts',(2.47544989763591,6.30030460222159,15.078213370374));
#187205=CARTESIAN_POINT('Ctrl Pts',(2.31485673767434,6.36106826587078,15.0862524327287));
#187206=CARTESIAN_POINT('Ctrl Pts',(2.15212302068412,6.41565705940097,15.0942914950835));
#187207=CARTESIAN_POINT('Ctrl Pts',(1.98938880463277,6.4702460203405,15.1023305820919));
#187208=CARTESIAN_POINT('Ctrl Pts',(1.82451436543312,6.51865993475011,15.1103696691003));
#187209=CARTESIAN_POINT('Ctrl Pts',(1.65801933962676,6.56073630543277,15.1184087561087));
#187210=CARTESIAN_POINT('Ctrl Pts',(1.49156455312839,6.60280250689848,15.1264459001924));
#187211=CARTESIAN_POINT('Ctrl Pts',(1.32349032463615,6.63853413246334,15.1344830442761));
#187212=CARTESIAN_POINT('Ctrl Pts',(1.15432930022063,6.66781919870749,15.1425201883598));
#187213=CARTESIAN_POINT('Ctrl Pts',(0.985145296468844,6.69710824312207,
15.150558424233));
#187214=CARTESIAN_POINT('Ctrl Pts',(0.814874571008829,6.71994892092555,
15.1585966601062));
#187215=CARTESIAN_POINT('Ctrl Pts',(0.644057893040867,6.73628075650145,
15.1666348959795));
#187216=CARTESIAN_POINT('Ctrl Pts',(0.473184164145204,6.75261804673425,
15.1746758165368));
#187217=CARTESIAN_POINT('Ctrl Pts',(0.301764491440067,6.76244213216339,
15.1827167370941));
#187218=CARTESIAN_POINT('Ctrl Pts',(0.130342518113964,6.76574458784632,
15.1907576576514));
#187219=CARTESIAN_POINT('Ctrl Pts',(-0.0412818148417761,6.76905094200093,
15.1988080703273));
#187220=CARTESIAN_POINT('Ctrl Pts',(-0.212908080014956,6.76582028224575,
15.2068584830033));
#187221=CARTESIAN_POINT('Ctrl Pts',(-0.383993985147717,6.75609632993568,
15.2149088956792));
#187222=CARTESIAN_POINT('Ctrl Pts',(-0.555182441695757,6.74636654894516,
15.2229641338912));
#187223=CARTESIAN_POINT('Ctrl Pts',(-0.725829522287586,6.73013575926323,
15.2310193721033));
#187224=CARTESIAN_POINT('Ctrl Pts',(-0.895400813033327,6.707499264556,15.2390746103153));
#187225=CARTESIAN_POINT('Ctrl Pts',(-1.06525494352509,6.68482501286535,
15.2471432844192));
#187226=CARTESIAN_POINT('Ctrl Pts',(-1.23402933192111,6.655723773479,15.2552119585232));
#187227=CARTESIAN_POINT('Ctrl Pts',(-1.40120124622319,6.62034168812929,
15.2632806326271));
#187228=CARTESIAN_POINT('Ctrl Pts',(-1.56659776926395,6.58533536592975,
15.2712636161798));
#187229=CARTESIAN_POINT('Ctrl Pts',(-1.73042538138055,6.54418113218147,
15.2792465997324));
#187230=CARTESIAN_POINT('Ctrl Pts',(-1.89219669410863,6.4970670822152,15.2872295832851));
#187231=CARTESIAN_POINT('Ctrl Pts',(-2.0610593416958,6.44788776184194,15.2955625053317));
#187232=CARTESIAN_POINT('Ctrl Pts',(-2.22822032661907,6.39205789325241,
15.3038954273784));
#187233=CARTESIAN_POINT('Ctrl Pts',(-2.39312566877512,6.3297107780253,15.312228349425));
#187234=CARTESIAN_POINT('Ctrl Pts',(-2.55783613280683,6.26743734196901,
15.3205514239785));
#187235=CARTESIAN_POINT('Ctrl Pts',(-2.72029594151521,6.19866212387286,
15.3288744985321));
#187236=CARTESIAN_POINT('Ctrl Pts',(-2.87996466079607,6.12356861254659,
15.3371975730856));
#187237=CARTESIAN_POINT('Ctrl Pts',(-3.03947399848063,6.04855005969535,
15.3455123395315));
#187238=CARTESIAN_POINT('Ctrl Pts',(-3.19619748457894,5.96722592621008,
15.3538271059774));
#187239=CARTESIAN_POINT('Ctrl Pts',(-3.34961290893504,5.87982842949484,
15.3621418724233));
#187240=CARTESIAN_POINT('Ctrl Pts',(-3.50290333529777,5.79250214147169,
15.3704498642628));
#187241=CARTESIAN_POINT('Ctrl Pts',(-3.65289076950655,5.69911252176903,
15.3787578561022));
#187242=CARTESIAN_POINT('Ctrl Pts',(-3.79907574206022,5.59993861627872,
15.3870658479417));
#187243=CARTESIAN_POINT('Ctrl Pts',(-3.94516840838345,5.5008273326107,15.3953685938287));
#187244=CARTESIAN_POINT('Ctrl Pts',(-4.08746311084286,5.39593923673922,
15.4036713397158));
#187245=CARTESIAN_POINT('Ctrl Pts',(-4.22548743446519,5.28559787925423,
15.4119740856028));
#187246=CARTESIAN_POINT('Ctrl Pts',(-4.36345535194457,5.17530161476604,
15.4202734384222));
#187247=CARTESIAN_POINT('Ctrl Pts',(-4.497156096631,5.05955674617516,15.4285727912416));
#187248=CARTESIAN_POINT('Ctrl Pts',(-4.62614832778306,4.93872864706596,
15.4368721440609));
#187249=CARTESIAN_POINT('Ctrl Pts',(-4.75511312445184,4.81792624606614,
15.4451697317472));
#187250=CARTESIAN_POINT('Ctrl Pts',(-4.87937114888155,4.69204300608057,
15.4534673194335));
#187251=CARTESIAN_POINT('Ctrl Pts',(-4.99851592060525,4.56148304737131,
15.4617649071197));
#187252=CARTESIAN_POINT('Ctrl Pts',(-5.11765515114784,4.4309291607403,15.4700621089021));
#187253=CARTESIAN_POINT('Ctrl Pts',(-5.23168136849243,4.29569924589025,
15.4783593106844));
#187254=CARTESIAN_POINT('Ctrl Pts',(-5.34022646277026,4.15623270839449,
15.4866565124667));
#187255=CARTESIAN_POINT('Ctrl Pts',(-5.44878454554038,4.01674948235046,
15.4949547070912));
#187256=CARTESIAN_POINT('Ctrl Pts',(-5.55185998515246,3.87302889839739,
15.5032529017157));
#187257=CARTESIAN_POINT('Ctrl Pts',(-5.64912620083537,3.72554186220412,
15.5115510963401));
#187258=CARTESIAN_POINT('Ctrl Pts',(-5.74646082498203,3.5779510966584,15.5198551271816));
#187259=CARTESIAN_POINT('Ctrl Pts',(-5.83797786940588,3.42658887645757,
15.5281591580231));
#187260=CARTESIAN_POINT('Ctrl Pts',(-5.92339471510942,3.27195416364806,
15.5364631888646));
#187261=CARTESIAN_POINT('Ctrl Pts',(-6.00884262072878,3.11726322140131,
15.5447702392803));
#187262=CARTESIAN_POINT('Ctrl Pts',(-6.0881857447487,2.95929772285178,15.5530772896959));
#187263=CARTESIAN_POINT('Ctrl Pts',(-6.16118828164667,2.79857963225987,
15.5613843401116));
#187264=CARTESIAN_POINT('Ctrl Pts',(-6.23426887057748,2.63768970690413,
15.5697002721662));
#187265=CARTESIAN_POINT('Ctrl Pts',(-6.30099519032929,2.47404162937591,
15.5780162042207));
#187266=CARTESIAN_POINT('Ctrl Pts',(-6.36117987073296,2.30817669431562,
15.5863321362753));
#187267=CARTESIAN_POINT('Ctrl Pts',(-6.40654836119194,2.18314418316346,
15.592600862495));
#187268=CARTESIAN_POINT('Ctrl Pts',(-6.44820059210438,2.05685234661173,
15.5988695887148));
#187269=CARTESIAN_POINT('Ctrl Pts',(-6.48607526764064,1.92953792979057,
15.6051383149346));
#187270=CARTESIAN_POINT('Ctrl Pts',(-6.54100728234485,1.74488585507684,
15.6142302412945));
#187271=CARTESIAN_POINT('Ctrl Pts',(-6.58807826959424,1.55779126982591,
15.6233221676544));
#187272=CARTESIAN_POINT('Ctrl Pts',(-6.62709478667593,1.36890601883865,
15.6324140940143));
#187273=CARTESIAN_POINT('Ctrl Pts',(-6.6660529089167,1.18030346669301,15.641492412763));
#187274=CARTESIAN_POINT('Ctrl Pts',(-6.69698057155371,0.989915816809847,
15.6505707315118));
#187275=CARTESIAN_POINT('Ctrl Pts',(-6.71973467568172,0.798407720679577,
15.6596490502605));
#187276=CARTESIAN_POINT('Ctrl Pts',(-6.74243203827094,0.607377185168806,
15.6687047305537));
#187277=CARTESIAN_POINT('Ctrl Pts',(-6.75699649243608,0.415232002965931,
15.6777604108468));
#187278=CARTESIAN_POINT('Ctrl Pts',(-6.76333634483653,0.222644305144609,
15.68681609114));
#187279=CARTESIAN_POINT('Ctrl Pts',(-6.76575487404414,0.149175879889805,
15.6902706553633));
#187280=CARTESIAN_POINT('Ctrl Pts',(-6.7669770269594,0.075643168492496,
15.6937252195867));
#187281=CARTESIAN_POINT('Ctrl Pts',(-6.76699967914336,0.00208386029358956,
15.69717978381));
#187282=CARTESIAN_POINT('',(-6.76699999457021,0.000271084328258356,15.3028202162169));
#187283=CARTESIAN_POINT('Ctrl Pts',(3.09910619832135,6.0156321173694,14.6512308626299));
#187284=CARTESIAN_POINT('Ctrl Pts',(2.94269490714649,6.09621138028141,14.6595150299666));
#187285=CARTESIAN_POINT('Ctrl Pts',(2.78330245775587,6.17060202482753,14.6677991973033));
#187286=CARTESIAN_POINT('Ctrl Pts',(2.62147298918087,6.23860307817344,14.6760833646399));
#187287=CARTESIAN_POINT('Ctrl Pts',(2.45659527075519,6.30788501195809,14.6845235740873));
#187288=CARTESIAN_POINT('Ctrl Pts',(2.28884715097256,6.37067805532276,14.6929637835347));
#187289=CARTESIAN_POINT('Ctrl Pts',(2.11876740895101,6.42674985251231,14.701403992982));
#187290=CARTESIAN_POINT('Ctrl Pts',(1.94881652753641,6.48277916700679,14.7098378077201));
#187291=CARTESIAN_POINT('Ctrl Pts',(1.77653786095828,6.53209728252431,14.7182716224581));
#187292=CARTESIAN_POINT('Ctrl Pts',(1.60248911927806,6.57452033403164,14.7267054371961));
#187293=CARTESIAN_POINT('Ctrl Pts',(1.42854548933681,6.61691776535537,14.735134158574));
#187294=CARTESIAN_POINT('Ctrl Pts',(1.25283423865705,6.65242835557688,14.7435628799518));
#187295=CARTESIAN_POINT('Ctrl Pts',(1.07592753892944,6.68091827004142,14.7519916013297));
#187296=CARTESIAN_POINT('Ctrl Pts',(0.899100511491493,6.70939535369333,
14.7604165267205));
#187297=CARTESIAN_POINT('Ctrl Pts',(0.721079437181532,6.73085801303605,
14.7688414521114));
#187298=CARTESIAN_POINT('Ctrl Pts',(0.542446357160277,6.74522356557613,
14.7772663775022));
#187299=CARTESIAN_POINT('Ctrl Pts',(0.36386631931795,6.75958485249974,14.7856888012489));
#187300=CARTESIAN_POINT('Ctrl Pts',(0.184674970220197,6.76685320847487,
14.7941112249956));
#187301=CARTESIAN_POINT('Ctrl Pts',(0.00545954463865506,6.76699779764796,
14.8025336487423));
#187302=CARTESIAN_POINT('Ctrl Pts',(-0.173758699481983,6.76714238909503,
14.8109562049493));
#187303=CARTESIAN_POINT('Ctrl Pts',(-0.353000687448234,6.76016298296884,
14.8193787611563));
#187304=CARTESIAN_POINT('Ctrl Pts',(-0.531678429810775,6.74608086575265,
14.8278013173633));
#187305=CARTESIAN_POINT('Ctrl Pts',(-0.710362207939442,6.73199827284001,
14.8362241580858));
#187306=CARTESIAN_POINT('Ctrl Pts',(-0.88848136990042,6.71081251647774,
14.8446469988082));
#187307=CARTESIAN_POINT('Ctrl Pts',(-1.06545213723992,6.68259685625662,
14.8530698395307));
#187308=CARTESIAN_POINT('Ctrl Pts',(-1.24245358976082,6.65437630368709,
14.8614941407));
#187309=CARTESIAN_POINT('Ctrl Pts',(-1.41830592127252,6.61912346960152,
14.8699184418693));
#187310=CARTESIAN_POINT('Ctrl Pts',(-1.59243428027399,6.57696298172707,
14.8783427430386));
#187311=CARTESIAN_POINT('Ctrl Pts',(-1.76661714930328,6.53478929571891,
14.886769681394));
#187312=CARTESIAN_POINT('Ctrl Pts',(-1.93907464577638,6.48570372313361,
14.8951966197494));
#187313=CARTESIAN_POINT('Ctrl Pts',(-2.10924548398185,6.42988121883307,
14.9036235581048));
#187314=CARTESIAN_POINT('Ctrl Pts',(-2.27956932716175,6.37400852308413,
14.912058073337));
#187315=CARTESIAN_POINT('Ctrl Pts',(-2.44760208662373,6.31138689614873,
14.9204925885693));
#187316=CARTESIAN_POINT('Ctrl Pts',(-2.61279984093959,6.24224046246106,
14.9289271038016));
#187317=CARTESIAN_POINT('Ctrl Pts',(-2.77807738718611,6.17306063045351,
14.937365692977));
#187318=CARTESIAN_POINT('Ctrl Pts',(-2.94051689298704,6.09734984249978,
14.9458042821524));
#187319=CARTESIAN_POINT('Ctrl Pts',(-3.09959709972066,6.01537919165561,
14.9542428713278));
#187320=CARTESIAN_POINT('Ctrl Pts',(-3.25885512213654,5.93331691616809,
14.9626908929368));
#187321=CARTESIAN_POINT('Ctrl Pts',(-3.41474604975449,5.84498095638228,
14.9711389145458));
#187322=CARTESIAN_POINT('Ctrl Pts',(-3.56677471626288,5.75068753484554,
14.9795869361548));
#187323=CARTESIAN_POINT('Ctrl Pts',(-3.65318537300047,5.69709266574515,
14.9843886561997));
#187324=CARTESIAN_POINT('Ctrl Pts',(-3.73834881761911,5.6415739688035,14.9891903762446));
#187325=CARTESIAN_POINT('Ctrl Pts',(-3.822178642059,5.58419550411589,14.9939920962895));
#187326=CARTESIAN_POINT('Ctrl Pts',(-3.96602678446965,5.48573668453899,
15.002231628144));
#187327=CARTESIAN_POINT('Ctrl Pts',(-4.10626736969548,5.38157963553009,
15.0104711599985));
#187328=CARTESIAN_POINT('Ctrl Pts',(-4.24242120299033,5.27201587027373,
15.018710691853));
#187329=CARTESIAN_POINT('Ctrl Pts',(-4.37842391504549,5.16257371313982,
15.026941078403));
#187330=CARTESIAN_POINT('Ctrl Pts',(-4.51034863228934,5.0477370100724,15.035171464953));
#187331=CARTESIAN_POINT('Ctrl Pts',(-4.63774429064585,4.92784099729099,
15.043401851503));
#187332=CARTESIAN_POINT('Ctrl Pts',(-4.76502127493901,4.80805667235828,
15.0516245711244));
#187333=CARTESIAN_POINT('Ctrl Pts',(-4.88777734489452,4.68322266610921,
15.0598472907458));
#187334=CARTESIAN_POINT('Ctrl Pts',(-5.00559369260521,4.55371505306941,
15.0680700103672));
#187335=CARTESIAN_POINT('Ctrl Pts',(-5.12330564654278,4.42432219310621,
15.0762854440665));
#187336=CARTESIAN_POINT('Ctrl Pts',(-5.23608636332162,4.2902642423217,15.0845008777659));
#187337=CARTESIAN_POINT('Ctrl Pts',(-5.34355326109191,4.15195466568145,
15.0927163114652));
#187338=CARTESIAN_POINT('Ctrl Pts',(-5.45096492922155,4.01371616942388,
15.1009275230696));
#187339=CARTESIAN_POINT('Ctrl Pts',(-5.55306799931583,3.87123067929587,
15.1091387346739));
#187340=CARTESIAN_POINT('Ctrl Pts',(-5.64951935821436,3.72494564002767,
15.1173499462783));
#187341=CARTESIAN_POINT('Ctrl Pts',(-5.74593837264833,3.57870965669112,
15.1255584042953));
#187342=CARTESIAN_POINT('Ctrl Pts',(-5.83670925573151,3.42867695926469,
15.1337668623123));
#187343=CARTESIAN_POINT('Ctrl Pts',(-5.92153147632753,3.27532501820237,
15.1419753203293));
#187344=CARTESIAN_POINT('Ctrl Pts',(-5.95932162752477,3.20700338032947,
15.1456323675909));
#187345=CARTESIAN_POINT('Ctrl Pts',(-5.99593160958208,3.138023284743,15.1492894148526));
#187346=CARTESIAN_POINT('Ctrl Pts',(-6.03133770514223,3.06842866733606,
15.1529464621142));
#187347=CARTESIAN_POINT('Ctrl Pts',(-6.11593347616295,2.90214627371737,
15.1616842437833));
#187348=CARTESIAN_POINT('Ctrl Pts',(-6.19357452955852,2.73250963683915,
15.1704220254524));
#187349=CARTESIAN_POINT('Ctrl Pts',(-6.26403344654619,2.5601121031218,15.1791598071215));
#187350=CARTESIAN_POINT('Ctrl Pts',(-6.33460020912402,2.38745069487214,
15.1879109629845));
#187351=CARTESIAN_POINT('Ctrl Pts',(-6.39796277023565,2.21202020841254,
15.1966621188475));
#187352=CARTESIAN_POINT('Ctrl Pts',(-6.4539431889,2.03443021862419,15.2054132747105));
#187353=CARTESIAN_POINT('Ctrl Pts',(-6.51006016205904,1.85640702894389,
15.2141857774962));
#187354=CARTESIAN_POINT('Ctrl Pts',(-6.5587588865186,1.67621406763521,15.2229582802819));
#187355=CARTESIAN_POINT('Ctrl Pts',(-6.599911682748,1.49447475051487,15.2317307830675));
#187356=CARTESIAN_POINT('Ctrl Pts',(-6.64111555804406,1.3125098576003,15.2405141743297));
#187357=CARTESIAN_POINT('Ctrl Pts',(-6.67475474703704,1.12899505147279,
15.2492975655919));
#187358=CARTESIAN_POINT('Ctrl Pts',(-6.7007531753093,0.944561212194508,
15.258080956854));
#187359=CARTESIAN_POINT('Ctrl Pts',(-6.72680535944485,0.759746026776842,
15.2668825091671));
#187360=CARTESIAN_POINT('Ctrl Pts',(-6.74518515453027,0.57400828762247,
15.2756840614802));
#187361=CARTESIAN_POINT('Ctrl Pts',(-6.75586838666445,0.387983687888932,
15.2844856137933));
#187362=CARTESIAN_POINT('Ctrl Pts',(-6.76328650286802,0.258813781233941,
15.2905971479255));
#187363=CARTESIAN_POINT('Ctrl Pts',(-6.76699481745752,0.129505585506803,
15.2967086820577));
#187364=CARTESIAN_POINT('Ctrl Pts',(-6.76699999457019,0.000271084898373194,
15.3028202161899));
#187365=CARTESIAN_POINT('Ctrl Pts',(-6.76699999457022,0.00027108432828991,
15.3028202162169));
#187366=CARTESIAN_POINT('Ctrl Pts',(-6.76700255864279,-0.0637351207553848,
15.3058470867909));
#187367=CARTESIAN_POINT('Ctrl Pts',(-6.76609702024371,-0.127738852254252,
15.3088739573649));
#187368=CARTESIAN_POINT('Ctrl Pts',(-6.76428353672319,-0.191721764063444,
15.3119008279389));
#187369=CARTESIAN_POINT('Ctrl Pts',(-6.75935707096965,-0.365536204764654,
15.3201235518042));
#187370=CARTESIAN_POINT('Ctrl Pts',(-6.74772026327342,-0.539391915402444,
15.3283462756694));
#187371=CARTESIAN_POINT('Ctrl Pts',(-6.72936133136258,-0.712730714900107,
15.3365689995347));
#187372=CARTESIAN_POINT('Ctrl Pts',(-6.71102183175931,-0.885886041149936,
15.3447830199252));
#187373=CARTESIAN_POINT('Ctrl Pts',(-6.68597441393982,-1.0585251920136,
15.3529970403158));
#187374=CARTESIAN_POINT('Ctrl Pts',(-6.65425929575064,-1.23009033201476,
15.3612110607064));
#187375=CARTESIAN_POINT('Ctrl Pts',(-6.62257137944063,-1.40150832155665,
15.3694180359777));
#187376=CARTESIAN_POINT('Ctrl Pts',(-6.58422721718039,-1.57185378408319,
15.3776250112489));
#187377=CARTESIAN_POINT('Ctrl Pts',(-6.53931879045859,-1.74057426062642,
15.3858319865202));
#187378=CARTESIAN_POINT('Ctrl Pts',(-6.49443986767699,-1.90918389118343,
15.3940335699726));
#187379=CARTESIAN_POINT('Ctrl Pts',(-6.44300536253492,-2.07617031684357,
15.4022351534249));
#187380=CARTESIAN_POINT('Ctrl Pts',(-6.38515828866142,-2.24099143879185,
15.4104367368772));
#187381=CARTESIAN_POINT('Ctrl Pts',(-6.32733761079827,-2.40573735174945,
15.4186345778916));
#187382=CARTESIAN_POINT('Ctrl Pts',(-6.26311031225825,-2.56831959163386,
15.426832418906));
#187383=CARTESIAN_POINT('Ctrl Pts',(-6.192669219541,-2.72821130731281,15.4350302599204));
#187384=CARTESIAN_POINT('Ctrl Pts',(-6.12223434303097,-2.88808891304543,
15.4432273775009));
#187385=CARTESIAN_POINT('Ctrl Pts',(-6.045586901243,-3.04527613601308,15.4514244950813));
#187386=CARTESIAN_POINT('Ctrl Pts',(-5.96296796355096,-3.19926586354822,
15.4596216126618));
#187387=CARTESIAN_POINT('Ctrl Pts',(-5.88034994508676,-3.35325387777588,
15.4678186390402));
#187388=CARTESIAN_POINT('Ctrl Pts',(-5.79176073175118,-3.50404415072474,
15.4760156654186));
#187389=CARTESIAN_POINT('Ctrl Pts',(-5.69748742591885,-3.65115406844145,
15.484212691797));
#187390=CARTESIAN_POINT('Ctrl Pts',(-5.60319802723507,-3.79828909844242,
15.4924111174424));
#187391=CARTESIAN_POINT('Ctrl Pts',(-5.50322279654648,-3.94174221941773,
15.5006095430878));
#187392=CARTESIAN_POINT('Ctrl Pts',(-5.3978922690997,-4.08105967258428,
15.5088079687332));
#187393=CARTESIAN_POINT('Ctrl Pts',(-5.29252460879435,-4.22042624024224,
15.5170092846231));
#187394=CARTESIAN_POINT('Ctrl Pts',(-5.18179810721346,-4.355653949734,15.525210600513));
#187395=CARTESIAN_POINT('Ctrl Pts',(-5.06608371039833,-4.48632197231058,
15.533411916403));
#187396=CARTESIAN_POINT('Ctrl Pts',(-4.95023753425529,-4.61713880389165,
15.5416225722188));
#187397=CARTESIAN_POINT('Ctrl Pts',(-4.82939235263694,-4.74338530551013,
15.5498332280347));
#187398=CARTESIAN_POINT('Ctrl Pts',(-4.7039568591392,-4.86467664571421,
15.5580438838505));
#187399=CARTESIAN_POINT('Ctrl Pts',(-4.57844744954418,-4.98603945996645,
15.566259378007));
#187400=CARTESIAN_POINT('Ctrl Pts',(-4.4483426031316,-5.10244105345704,
15.5744748721634));
#187401=CARTESIAN_POINT('Ctrl Pts',(-4.31408414827224,-5.21353689558501,
15.5826903663198));
#187402=CARTESIAN_POINT('Ctrl Pts',(-4.17961738894967,-5.32480510495633,
15.5909186069665));
#187403=CARTESIAN_POINT('Ctrl Pts',(-4.0409844276511,-5.43075089450466,
15.5991468476133));
#187404=CARTESIAN_POINT('Ctrl Pts',(-3.89865721400434,-5.53107231264354,
15.6073750882601));
#187405=CARTESIAN_POINT('Ctrl Pts',(-3.76930449933599,-5.62224846541956,
15.6148532453695));
#187406=CARTESIAN_POINT('Ctrl Pts',(-3.63690088303125,-5.70877939325665,
15.622331402479));
#187407=CARTESIAN_POINT('Ctrl Pts',(-3.5018174165147,-5.79047180991275,
15.6298095595885));
#187408=CARTESIAN_POINT('Ctrl Pts',(-3.35605553343491,-5.87862205355248,
15.6378788688115));
#187409=CARTESIAN_POINT('Ctrl Pts',(-3.20669577456135,-5.96142638875208,
15.6459481780346));
#187410=CARTESIAN_POINT('Ctrl Pts',(-3.0541751126488,-6.03856799094592,
15.6540174872576));
#187411=CARTESIAN_POINT('Ctrl Pts',(-2.9018446854553,-6.11561337659549,
15.6620767318589));
#187412=CARTESIAN_POINT('Ctrl Pts',(-2.74636152851422,-6.1870099163823,
15.6701359764602));
#187413=CARTESIAN_POINT('Ctrl Pts',(-2.58819214117367,-6.25248354179096,
15.6781952210615));
#187414=CARTESIAN_POINT('Ctrl Pts',(-2.43018532403631,-6.31788987187298,
15.6862461821823));
#187415=CARTESIAN_POINT('Ctrl Pts',(-2.26949811273403,-6.37738526072649,
15.6942971433031));
#187416=CARTESIAN_POINT('Ctrl Pts',(-2.10662211081361,-6.43074119229123,
15.7023481044239));
#187417=CARTESIAN_POINT('Ctrl Pts',(-1.94387782730077,-6.48405397472254,
15.7103925547035));
#187418=CARTESIAN_POINT('Ctrl Pts',(-1.77894862901381,-6.53123706628902,
15.7184370049832));
#187419=CARTESIAN_POINT('Ctrl Pts',(-1.61234653503897,-6.5721098325384,
15.7264814552628));
#187420=CARTESIAN_POINT('Ctrl Pts',(-1.44584270513383,-6.61295849150163,
15.7345211608216));
#187421=CARTESIAN_POINT('Ctrl Pts',(-1.27766830523149,-6.64750414568251,
15.7425608663805));
#187422=CARTESIAN_POINT('Ctrl Pts',(-1.10835086511779,-6.6756158786881,
15.7506005719393));
#187423=CARTESIAN_POINT('Ctrl Pts',(-0.935378798600986,-6.70433438841799,
15.7588138102434));
#187424=CARTESIAN_POINT('Ctrl Pts',(-0.7612141661803,-6.72633794998259,
15.7670270485475));
#187425=CARTESIAN_POINT('Ctrl Pts',(-0.586431261825836,-6.74154191377265,
15.7752402868516));
#187426=CARTESIAN_POINT('Ctrl Pts',(-0.415396318507402,-6.75641985103232,
15.7832774044003));
#187427=CARTESIAN_POINT('Ctrl Pts',(-0.2437697384752,-6.76478682785258,
15.7913145219491));
#187428=CARTESIAN_POINT('Ctrl Pts',(-0.0720951450436325,-6.76661594078319,
15.7993516394978));
#187429=CARTESIAN_POINT('Ctrl Pts',(0.0995976104685821,-6.76844524722232,
15.8073896073225));
#187430=CARTESIAN_POINT('Ctrl Pts',(0.271338015873839,-6.7637353084702,
15.8154275751471));
#187431=CARTESIAN_POINT('Ctrl Pts',(0.442582475717851,-6.75251136631309,
15.8234655429718));
#187432=CARTESIAN_POINT('Ctrl Pts',(0.613878981976963,-6.74128401285758,
15.8315059537801));
#187433=CARTESIAN_POINT('Ctrl Pts',(0.78467887003604,-6.7235387396435,15.8395463645884));
#187434=CARTESIAN_POINT('Ctrl Pts',(0.954443842041111,-6.69935265174105,
15.8475867753967));
#187435=CARTESIAN_POINT('Ctrl Pts',(1.13062497246815,-6.67425246613189,
15.8559310683835));
#187436=CARTESIAN_POINT('Ctrl Pts',(1.30569098949103,-6.64221516367928,
15.8642753613702));
#187437=CARTESIAN_POINT('Ctrl Pts',(1.47905316260374,-6.60338479434539,
15.872619654357));
#187438=CARTESIAN_POINT('Ctrl Pts',(1.6463968468264,-6.56590247079471,15.8806742645731));
#187439=CARTESIAN_POINT('Ctrl Pts',(1.81215266868717,-6.52209099479459,
15.8887288747892));
#187440=CARTESIAN_POINT('Ctrl Pts',(1.97580830523767,-6.47213029387959,
15.8967834850054));
#187441=CARTESIAN_POINT('Ctrl Pts',(2.13958783141684,-6.42213177200825,
15.9048441926752));
#187442=CARTESIAN_POINT('Ctrl Pts',(2.30126365622871,-6.36597487819626,
15.912904900345));
#187443=CARTESIAN_POINT('Ctrl Pts',(2.46034442297168,-6.30388723886715,
15.9209656080148));
#187444=CARTESIAN_POINT('Ctrl Pts',(2.61964948406537,-6.24171205968621,
15.9290376807996));
#187445=CARTESIAN_POINT('Ctrl Pts',(2.77635184768708,-6.173589598907,15.9371097535843));
#187446=CARTESIAN_POINT('Ctrl Pts',(2.92998516313957,-6.09979310663747,
15.945181826369));
#187447=CARTESIAN_POINT('Ctrl Pts',(2.9460770855717,-6.09206348480468,15.9460273146587));
#187448=CARTESIAN_POINT('Ctrl Pts',(2.96213536453561,-6.08427165198964,
15.9468728029483));
#187449=CARTESIAN_POINT('Ctrl Pts',(2.97815948344574,-6.07641794901916,
15.947718291238));
#187450=CARTESIAN_POINT('Ctrl Pts',(3.13608920923335,-5.99901380820487,
15.9560512132847));
#187451=CARTESIAN_POINT('Ctrl Pts',(3.29120217217887,-5.91534937231047,
15.9643841353313));
#187452=CARTESIAN_POINT('Ctrl Pts',(3.44297545180372,-5.82565095403741,
15.972717057378));
#187453=CARTESIAN_POINT('Ctrl Pts',(3.59456937221747,-5.73605853754265,
15.9810401319315));
#187454=CARTESIAN_POINT('Ctrl Pts',(3.74283117444873,-5.64044651910953,
15.989363206485));
#187455=CARTESIAN_POINT('Ctrl Pts',(3.88725988849627,-5.53908833286561,
15.9976862810386));
#187456=CARTESIAN_POINT('Ctrl Pts',(4.03154443354709,-5.43783132254171,
16.0060010474844));
#187457=CARTESIAN_POINT('Ctrl Pts',(4.1720032303848,-5.33083977066663,16.0143158139303));
#187458=CARTESIAN_POINT('Ctrl Pts',(4.30816161806241,-5.21843199367912,
16.0226305803762));
#187459=CARTESIAN_POINT('Ctrl Pts',(4.44420906823032,-5.10611580296157,
16.0309385722157));
#187460=CARTESIAN_POINT('Ctrl Pts',(4.57596282375651,-4.98839240089722,
16.0392465640551));
#187461=CARTESIAN_POINT('Ctrl Pts',(4.70297865677638,-4.86562233983546,
16.0475545558946));
#187462=CARTESIAN_POINT('Ctrl Pts',(4.82991428762037,-4.74292980002278,
16.0558573017816));
#187463=CARTESIAN_POINT('Ctrl Pts',(4.95211770855952,-4.61519719293271,
16.0641600476686));
#187464=CARTESIAN_POINT('Ctrl Pts',(5.06917897636533,-4.48282427779361,
16.0724627935556));
#187465=CARTESIAN_POINT('Ctrl Pts',(5.18619240496172,-4.35050545924621,
16.080762146375));
#187466=CARTESIAN_POINT('Ctrl Pts',(5.29806763756567,-4.21355037148143,
16.0890614991944));
#187467=CARTESIAN_POINT('Ctrl Pts',(5.40443251595799,-4.07239464939929,
16.0973608520137));
#187468=CARTESIAN_POINT('Ctrl Pts',(5.51077477232521,-3.93126894877101,
16.1056584397));
#187469=CARTESIAN_POINT('Ctrl Pts',(5.61160880004059,-3.78594467138048,
16.1139560273863));
#187470=CARTESIAN_POINT('Ctrl Pts',(5.70660342840626,-3.63688964788622,
16.1222536150725));
#187471=CARTESIAN_POINT('Ctrl Pts',(5.80159363876482,-3.48784155663819,
16.1305508168549));
#187472=CARTESIAN_POINT('Ctrl Pts',(5.89074480412844,-3.33506335849959,
16.1388480186372));
#187473=CARTESIAN_POINT('Ctrl Pts',(5.97376960617619,-3.17905106790148,
16.1471452204195));
#187474=CARTESIAN_POINT('Ctrl Pts',(6.05680434296129,-3.02302010889235,
16.155443415044));
#187475=CARTESIAN_POINT('Ctrl Pts',(6.13371109278212,-2.86375459368289,
16.1637416096684));
#187476=CARTESIAN_POINT('Ctrl Pts',(6.20424885240915,-2.7017744497607,16.1720398042929));
#187477=CARTESIAN_POINT('Ctrl Pts',(6.27483622206506,-2.53968038331447,
16.1803438351343));
#187478=CARTESIAN_POINT('Ctrl Pts',(6.33904551176145,-2.37486819250092,
16.1886478659758));
#187479=CARTESIAN_POINT('Ctrl Pts',(6.39668383955284,-2.2078779080383,16.1969518968173));
#187480=CARTESIAN_POINT('Ctrl Pts',(6.45434312622656,-2.04082690131227,
16.205258947233));
#187481=CARTESIAN_POINT('Ctrl Pts',(6.50542658214326,-1.87159655358223,
16.2135659976486));
#187482=CARTESIAN_POINT('Ctrl Pts',(6.54979138952807,-1.70074153052836,
16.2218730480643));
#187483=CARTESIAN_POINT('Ctrl Pts',(6.59420363037961,-1.52970383461893,
16.2301889801188));
#187484=CARTESIAN_POINT('Ctrl Pts',(6.63188278992028,-1.35703833151356,
16.2385049121734));
#187485=CARTESIAN_POINT('Ctrl Pts',(6.66273708283519,-1.18331042630952,
16.246820844228));
#187486=CARTESIAN_POINT('Ctrl Pts',(6.68599570420465,-1.05235064124515,
16.2530895704478));
#187487=CARTESIAN_POINT('Ctrl Pts',(6.70537717616939,-0.920787368008855,
16.2593582966677));
#187488=CARTESIAN_POINT('Ctrl Pts',(6.72086170282644,-0.788864355564967,
16.2656270228876));
#187489=CARTESIAN_POINT('Ctrl Pts',(6.74173490843623,-0.611031592291495,
16.2740772916105));
#187490=CARTESIAN_POINT('Ctrl Pts',(6.75556340138393,-0.432218917407917,
16.2825275603333));
#187491=CARTESIAN_POINT('Ctrl Pts',(6.76226850387909,-0.253009251698049,
16.2909778290562));
#187492=CARTESIAN_POINT('Ctrl Pts',(6.7689676888938,-0.0739577445986757,
16.2994206401303));
#187493=CARTESIAN_POINT('Ctrl Pts',(6.76855600151117,0.105489725193847,
16.3078634512043));
#187494=CARTESIAN_POINT('Ctrl Pts',(6.76100653137315,0.284744943290698,
16.3163062622783));
#187495=CARTESIAN_POINT('Ctrl Pts',(6.75346269601888,0.463866368635023,
16.3247427717956));
#187496=CARTESIAN_POINT('Ctrl Pts',(6.7387917119032,0.642795498124919,16.3331792813128));
#187497=CARTESIAN_POINT('Ctrl Pts',(6.7170187358054,0.820943544246058,16.3416157908301));
#187498=CARTESIAN_POINT('Ctrl Pts',(6.69526133944356,0.998964115854307,
16.3500462635708));
#187499=CARTESIAN_POINT('Ctrl Pts',(6.66641212781071,1.17620439058877,16.3584767363116));
#187500=CARTESIAN_POINT('Ctrl Pts',(6.63054815899308,1.3520799204461,16.3669072090523));
#187501=CARTESIAN_POINT('Ctrl Pts',(6.59469960799836,1.52787984189022,16.3753340575557));
#187502=CARTESIAN_POINT('Ctrl Pts',(6.55184237770201,1.70231586376412,16.3837609060591));
#187503=CARTESIAN_POINT('Ctrl Pts',(6.50210487543775,1.8748123076214,16.3921877545625));
#187504=CARTESIAN_POINT('Ctrl Pts',(6.45238272536407,2.04725550798714,16.4006120019987));
#187505=CARTESIAN_POINT('Ctrl Pts',(6.39578463023035,2.21776000601221,16.4090362494349));
#187506=CARTESIAN_POINT('Ctrl Pts',(6.33248934685054,2.38576354067716,16.4174604968711));
#187507=CARTESIAN_POINT('Ctrl Pts',(6.31465515768734,2.43310050888888,16.4198341274848));
#187508=CARTESIAN_POINT('Ctrl Pts',(6.29628958400892,2.48023902117158,16.4222077580986));
#187509=CARTESIAN_POINT('Ctrl Pts',(6.27739733281748,2.52716673884728,16.4245813887123));
#187510=CARTESIAN_POINT('Ctrl Pts',(6.2087985485342,2.69756381588811,16.43320016965));
#187511=CARTESIAN_POINT('Ctrl Pts',(6.13328276638273,2.86510393147769,16.4418189505877));
#187512=CARTESIAN_POINT('Ctrl Pts',(6.05111893817697,3.02923234434667,16.4504377315255));
#187513=CARTESIAN_POINT('Ctrl Pts',(5.96890575465943,3.19345934815483,16.4590616897125));
#187514=CARTESIAN_POINT('Ctrl Pts',(5.88003669155476,3.35427028728933,16.4676856478995));
#187515=CARTESIAN_POINT('Ctrl Pts',(5.78482645847453,3.51113540686386,16.4763096060865));
#187516=CARTESIAN_POINT('Ctrl Pts',(5.68617660453564,3.67366752797623,16.4852451184573));
#187517=CARTESIAN_POINT('Ctrl Pts',(5.58071906132451,3.83196311045958,16.4941806308282));
#187518=CARTESIAN_POINT('Ctrl Pts',(5.46885222716344,3.98546663735246,16.5031161431991));
#187519=CARTESIAN_POINT('Ctrl Pts',(5.36068399143239,4.13389495220571,16.5117562250943));
#187520=CARTESIAN_POINT('Ctrl Pts',(5.24652372156556,4.27784280467942,16.5203963069895));
#187521=CARTESIAN_POINT('Ctrl Pts',(5.12677230880462,4.41684216309278,16.5290363888848));
#187522=CARTESIAN_POINT('Ctrl Pts',(5.00087890272786,4.56297073284985,16.5381196164935));
#187523=CARTESIAN_POINT('Ctrl Pts',(4.86880602404354,4.70362957665082,16.5472028441022));
#187524=CARTESIAN_POINT('Ctrl Pts',(4.73106322116098,4.8383189019925,16.5562860717109));
#187525=CARTESIAN_POINT('Ctrl Pts',(4.5933204182784,4.9730082273342,16.5653692993196));
#187526=CARTESIAN_POINT('Ctrl Pts',(4.44990800226056,5.10172780024531,16.5744525269283));
#187527=CARTESIAN_POINT('Ctrl Pts',(4.30137593202973,5.22402661663926,16.583535754537));
#187528=CARTESIAN_POINT('Ctrl Pts',(4.15346353630972,5.34581520343023,16.5925810869988));
#187529=CARTESIAN_POINT('Ctrl Pts',(4.00033806783277,5.46134965052688,16.6016264194606));
#187530=CARTESIAN_POINT('Ctrl Pts',(3.84252688496662,5.57021329378945,16.6106717519224));
#187531=CARTESIAN_POINT('Ctrl Pts',(3.6848976564009,5.67895141864648,16.6197066552301));
#187532=CARTESIAN_POINT('Ctrl Pts',(3.52259369810313,5.78103396443803,16.6287415585378));
#187533=CARTESIAN_POINT('Ctrl Pts',(3.35617245869314,5.87608674438266,16.6377764618455));
#187534=CARTESIAN_POINT('Ctrl Pts',(3.27152300636822,5.92443493475067,16.6423720268077));
#187535=CARTESIAN_POINT('Ctrl Pts',(3.18580882221027,5.97096505098928,16.64696759177));
#187536=CARTESIAN_POINT('Ctrl Pts',(3.09910619832134,6.0156321173694,16.6515631567322));
#187537=CARTESIAN_POINT('Origin',(0.,0.,4.30282021618968));
#187538=CARTESIAN_POINT('',(3.09910619832135,6.0156321173694,19.0455979788775));
#187539=CARTESIAN_POINT('',(3.09910619832135,6.0156321173694,18.651395695404));
#187540=CARTESIAN_POINT('',(3.09910619832133,6.0156321173694,4.30282021618968));
#187541=CARTESIAN_POINT('',(-6.76699994441487,0.000867346018274939,17.6971797838443));
#187542=CARTESIAN_POINT('Ctrl Pts',(-6.76699994441487,0.000867346018275612,
17.6971797838443));
#187543=CARTESIAN_POINT('Ctrl Pts',(-6.76702404334501,-0.18715157087484,
17.7059864133287));
#187544=CARTESIAN_POINT('Ctrl Pts',(-6.75920775618406,-0.375012429148591,
17.7147930428132));
#187545=CARTESIAN_POINT('Ctrl Pts',(-6.74361644380036,-0.562073179315164,
17.7235996722976));
#187546=CARTESIAN_POINT('Ctrl Pts',(-6.727845109072,-0.751293793514222,
17.7325079859796));
#187547=CARTESIAN_POINT('Ctrl Pts',(-6.70411814837521,-0.939695425552969,
17.7414162996615));
#187548=CARTESIAN_POINT('Ctrl Pts',(-6.67255619747866,-1.12662451219967,
17.7503246133435));
#187549=CARTESIAN_POINT('Ctrl Pts',(-6.64123700124072,-1.31211585798045,
17.7591644098842));
#187550=CARTESIAN_POINT('Ctrl Pts',(-6.60220304049159,-1.4961569841258,
17.768004206425));
#187551=CARTESIAN_POINT('Ctrl Pts',(-6.55562269889953,-1.67812396135485,
17.7768440029657));
#187552=CARTESIAN_POINT('Ctrl Pts',(-6.50850079192844,-1.86220657388466,
17.7857865752183));
#187553=CARTESIAN_POINT('Ctrl Pts',(-6.45365603276216,-2.04416623577394,
17.7947291474709));
#187554=CARTESIAN_POINT('Ctrl Pts',(-6.3913134435766,-2.22337614135733,
17.8036717197235));
#187555=CARTESIAN_POINT('Ctrl Pts',(-6.32897085439105,-2.4025860469407,
17.812614291976));
#187556=CARTESIAN_POINT('Ctrl Pts',(-6.25913057640139,-2.57904594931731,
17.8215568642286));
#187557=CARTESIAN_POINT('Ctrl Pts',(-6.18206664089352,-2.75215207565852,
17.8304994364812));
#187558=CARTESIAN_POINT('Ctrl Pts',(-6.10924520366856,-2.91572842080022,
17.8389497052045));
#187559=CARTESIAN_POINT('Ctrl Pts',(-6.02986569785643,-3.0765515969184,
17.8473999739279));
#187560=CARTESIAN_POINT('Ctrl Pts',(-5.94415800561399,-3.2340801790146,
17.8558502426512));
#187561=CARTESIAN_POINT('Ctrl Pts',(-5.85852595331781,-3.39146973679255,
17.8642930537257));
#187562=CARTESIAN_POINT('Ctrl Pts',(-5.76657700391438,-3.5455702059956,
17.8727358648002));
#187563=CARTESIAN_POINT('Ctrl Pts',(-5.66858825745251,-3.69586203306773,
17.8811786758748));
#187564=CARTESIAN_POINT('Ctrl Pts',(-5.5706726479638,-3.84604168512263,
17.8896151853925));
#187565=CARTESIAN_POINT('Ctrl Pts',(-5.46672640834872,-3.99241808495695,
17.8980516949103));
#187566=CARTESIAN_POINT('Ctrl Pts',(-5.35707170480776,-4.13449776267301,
17.906488204428));
#187567=CARTESIAN_POINT('Ctrl Pts',(-5.24749546510767,-4.2764757747344,
17.9149186771692));
#187568=CARTESIAN_POINT('Ctrl Pts',(-5.13221911119824,-4.41416293547453,
17.9233491499105));
#187569=CARTESIAN_POINT('Ctrl Pts',(-5.01160722528569,-4.54709599848786,
17.9317796226517));
#187570=CARTESIAN_POINT('Ctrl Pts',(-4.89104719009637,-4.67997191393729,
17.9402064711555));
#187571=CARTESIAN_POINT('Ctrl Pts',(-4.76515641793399,-4.80809756087588,
17.9486333196593));
#187572=CARTESIAN_POINT('Ctrl Pts',(-4.63433917106564,-4.9310434440924,
17.9570601681632));
#187573=CARTESIAN_POINT('Ctrl Pts',(-4.50356230280935,-5.0539513783057,
17.9654844155998));
#187574=CARTESIAN_POINT('Ctrl Pts',(-4.36786223367588,-5.17168251038182,
17.9739086630364));
#187575=CARTESIAN_POINT('Ctrl Pts',(-4.22767967387173,-5.28384458279498,
17.9823329104731));
#187576=CARTESIAN_POINT('Ctrl Pts',(-4.18818159198645,-5.31544756341387,
17.9847065410841));
#187577=CARTESIAN_POINT('Ctrl Pts',(-4.14832785889437,-5.34660865436738,
17.987080171695));
#187578=CARTESIAN_POINT('Ctrl Pts',(-4.10812882024542,-5.37731964795371,
17.989453802306));
#187579=CARTESIAN_POINT('Ctrl Pts',(-3.96216393994695,-5.48883292422435,
17.9980725832432));
#187580=CARTESIAN_POINT('Ctrl Pts',(-3.81170926135031,-5.59435881379705,
18.0066913641804));
#187581=CARTESIAN_POINT('Ctrl Pts',(-3.65727921692777,-5.69355756354744,
18.0153101451176));
#187582=CARTESIAN_POINT('Ctrl Pts',(-3.5027564073157,-5.79281590138417,
18.0239341033042));
#187583=CARTESIAN_POINT('Ctrl Pts',(-3.3442537221211,-5.88573935001357,
18.0325580614908));
#187584=CARTESIAN_POINT('Ctrl Pts',(-3.18231218815861,-5.97203299866111,
18.0411820196773));
#187585=CARTESIAN_POINT('Ctrl Pts',(-3.01452025911462,-6.06144414240245,
18.0501175320485));
#187586=CARTESIAN_POINT('Ctrl Pts',(-2.84303670269073,-6.14373736649845,
18.0590530444196));
#187587=CARTESIAN_POINT('Ctrl Pts',(-2.66848766103472,-6.21863832385398,
18.0679885567907));
#187588=CARTESIAN_POINT('Ctrl Pts',(-2.49970964899563,-6.29106286747998,
18.0766286386854));
#187589=CARTESIAN_POINT('Ctrl Pts',(-2.32806591376774,-6.35657606920946,
18.0852687205801));
#187590=CARTESIAN_POINT('Ctrl Pts',(-2.1541400863151,-6.41498008481168,
18.0939088024748));
#187591=CARTESIAN_POINT('Ctrl Pts',(-1.97129368541882,-6.47637961475592,
18.1029920300841));
#187592=CARTESIAN_POINT('Ctrl Pts',(-1.78592532647418,-6.52992144075028,
18.1120752576934));
#187593=CARTESIAN_POINT('Ctrl Pts',(-1.59872828859884,-6.57543586838423,
18.1211584853027));
#187594=CARTESIAN_POINT('Ctrl Pts',(-1.4115312507235,-6.62095029601817,
18.1302417129121));
#187595=CARTESIAN_POINT('Ctrl Pts',(-1.22250592083238,-6.65843728287001,
18.1393249405214));
#187596=CARTESIAN_POINT('Ctrl Pts',(-1.03235542493084,-6.68778971534063,
18.1484081681307));
#187597=CARTESIAN_POINT('Ctrl Pts',(-0.843013676403518,-6.71701730615583,
18.1574527629905));
#187598=CARTESIAN_POINT('Ctrl Pts',(-0.652381594078926,-6.73820724818045,
18.1664973578504));
#187599=CARTESIAN_POINT('Ctrl Pts',(-0.461125177944495,-6.75127044120332,
18.1755419527102));
#187600=CARTESIAN_POINT('Ctrl Pts',(-0.270044269677354,-6.76432164669032,
18.1845782477305));
#187601=CARTESIAN_POINT('Ctrl Pts',(-0.0783404085832252,-6.76926097605705,
18.1936145427508));
#187602=CARTESIAN_POINT('Ctrl Pts',(0.113315738675922,-6.76605117800393,
18.2026508377712));
#187603=CARTESIAN_POINT('Ctrl Pts',(0.304632735353686,-6.76284705994016,
18.2116711423589));
#187604=CARTESIAN_POINT('Ctrl Pts',(0.495901949248468,-6.75152261437507,
18.2206914469466));
#187605=CARTESIAN_POINT('Ctrl Pts',(0.68645333433179,-6.73209260332809,
18.2297117515343));
#187606=CARTESIAN_POINT('Ctrl Pts',(0.876764756961635,-6.71268706060559,
18.2387206968006));
#187607=CARTESIAN_POINT('Ctrl Pts',(1.06635991882635,-6.68519634689232,
18.247729642067));
#187608=CARTESIAN_POINT('Ctrl Pts',(1.25457193988328,-6.64968707892766,
18.2567385873333));
#187609=CARTESIAN_POINT('Ctrl Pts',(1.44235657128392,-6.61425844499342,
18.2657270751921));
#187610=CARTESIAN_POINT('Ctrl Pts',(1.62876409788658,-6.57084764644693,
18.2747155630509));
#187611=CARTESIAN_POINT('Ctrl Pts',(1.81313637854058,-6.5195724915682,18.2837040509097));
#187612=CARTESIAN_POINT('Ctrl Pts',(1.97489767975534,-6.47458560013447,
18.2915902119249));
#187613=CARTESIAN_POINT('Ctrl Pts',(2.13509227952748,-6.4235457708254,18.2994763729402));
#187614=CARTESIAN_POINT('Ctrl Pts',(2.2932805652048,-6.36656526309548,18.3073625339555));
#187615=CARTESIAN_POINT('Ctrl Pts',(2.45618880411828,-6.30788459576963,
18.3154839988117));
#187616=CARTESIAN_POINT('Ctrl Pts',(2.61689573669985,-6.24292817977151,
18.3236054636678));
#187617=CARTESIAN_POINT('Ctrl Pts',(2.77488605225846,-6.17189568908787,
18.331726928524));
#187618=CARTESIAN_POINT('Ctrl Pts',(2.9328651007826,-6.10086826406613,18.3398478142002));
#187619=CARTESIAN_POINT('Ctrl Pts',(3.0881275841925,-6.02376577761723,18.3479686998764));
#187620=CARTESIAN_POINT('Ctrl Pts',(3.24017923388035,-5.94083559209734,
18.3560895855526));
#187621=CARTESIAN_POINT('Ctrl Pts',(3.39224905808847,-5.85789549404877,
18.3642114419069));
#187622=CARTESIAN_POINT('Ctrl Pts',(3.54110696346878,-5.76912648627449,
18.3723332982612));
#187623=CARTESIAN_POINT('Ctrl Pts',(3.68628434527089,-5.67482129461455,
18.3804551546155));
#187624=CARTESIAN_POINT('Ctrl Pts',(3.83156764669412,-5.58044729905385,
18.3885829365756));
#187625=CARTESIAN_POINT('Ctrl Pts',(3.97316475393407,-5.48052925204528,
18.3967107185358));
#187626=CARTESIAN_POINT('Ctrl Pts',(4.11063654134957,-5.37540288954434,
18.4048385004959));
#187627=CARTESIAN_POINT('Ctrl Pts',(4.24816432966186,-5.27023370247055,
18.4129695934124));
#187628=CARTESIAN_POINT('Ctrl Pts',(4.38156316650945,-5.15985220409469,
18.4211006863288));
#187629=CARTESIAN_POINT('Ctrl Pts',(4.51042817341628,-5.04463345471727,
18.4292317792453));
#187630=CARTESIAN_POINT('Ctrl Pts',(4.63943383109268,-4.92928894889007,
18.4373717469098));
#187631=CARTESIAN_POINT('Ctrl Pts',(4.76389551196001,-4.80909690089357,
18.4455117145744));
#187632=CARTESIAN_POINT('Ctrl Pts',(4.88344573534646,-4.68446867317164,
18.453651682239));
#187633=CARTESIAN_POINT('Ctrl Pts',(4.94544965021429,-4.61983108569663,
18.4578734214194));
#187634=CARTESIAN_POINT('Ctrl Pts',(5.00613308562027,-4.55400075606294,
18.4620951605998));
#187635=CARTESIAN_POINT('Ctrl Pts',(5.06544918373611,-4.48703839597871,
18.4663168997802));
#187636=CARTESIAN_POINT('Ctrl Pts',(5.18403545136421,-4.35316552493365,
18.4747571092379));
#187637=CARTESIAN_POINT('Ctrl Pts',(5.29739924020634,-4.21448946552642,
18.4831973186955));
#187638=CARTESIAN_POINT('Ctrl Pts',(5.40514739632277,-4.07144576582142,
18.4916375281531));
#187639=CARTESIAN_POINT('Ctrl Pts',(5.51281391724793,-3.92851044291105,
18.5000713429017));
#187640=CARTESIAN_POINT('Ctrl Pts',(5.61487308693035,-3.78121434165384,
18.5085051576502));
#187641=CARTESIAN_POINT('Ctrl Pts',(5.71097158788152,-3.63002651814144,
18.5169389723987));
#187642=CARTESIAN_POINT('Ctrl Pts',(5.80701205290538,-3.47893000016915,
18.5253676937873));
#187643=CARTESIAN_POINT('Ctrl Pts',(5.89709884742175,-3.32394672632612,
18.5337964151758));
#187644=CARTESIAN_POINT('Ctrl Pts',(5.98092138447731,-3.16557552313983,
18.5422251365644));
#187645=CARTESIAN_POINT('Ctrl Pts',(6.06470617093795,-3.0072756445322,18.5506500619661));
#187646=CARTESIAN_POINT('Ctrl Pts',(6.14223216933314,-2.8455911731076,18.5590749873678));
#187647=CARTESIAN_POINT('Ctrl Pts',(6.2132340610868,-2.68104671763677,18.5674999127695));
#187648=CARTESIAN_POINT('Ctrl Pts',(6.28421486998781,-2.51655112095579,
18.5759223365272));
#187649=CARTESIAN_POINT('Ctrl Pts',(6.34867530351902,-2.34919753963772,
18.5843447602848));
#187650=CARTESIAN_POINT('Ctrl Pts',(6.40639747157322,-2.17953215994173,
18.5927671840425));
#187651=CARTESIAN_POINT('Ctrl Pts',(6.46412054743138,-2.0098641118965,18.6011897402607));
#187652=CARTESIAN_POINT('Ctrl Pts',(6.51510503239564,-1.83788450632087,
18.6096122964789));
#187653=CARTESIAN_POINT('Ctrl Pts',(6.55918215221633,-1.66415699200729,
18.6180348526971));
#187654=CARTESIAN_POINT('Ctrl Pts',(6.60326076097057,-1.490423609145,18.6264576934308));
#187655=CARTESIAN_POINT('Ctrl Pts',(6.64043145714047,-1.31494252310655,
18.6348805341646));
#187656=CARTESIAN_POINT('Ctrl Pts',(6.6705760365812,-1.13829009491813,18.6433033748983));
#187657=CARTESIAN_POINT('Ctrl Pts',(6.70072584282811,-0.96160703674508,
18.6517276760789));
#187658=CARTESIAN_POINT('Ctrl Pts',(6.72384704737116,-0.783752560304833,
18.6601519772595));
#187659=CARTESIAN_POINT('Ctrl Pts',(6.73987295860478,-0.605311078593489,
18.6685762784401));
#187660=CARTESIAN_POINT('Ctrl Pts',(6.75590388667142,-0.426813736650358,
18.677003216807));
#187661=CARTESIAN_POINT('Ctrl Pts',(6.7648350632393,-0.247729355165734,
18.6854301551738));
#187662=CARTESIAN_POINT('Ctrl Pts',(6.76665181398804,-0.0686456717677405,
18.6938570935406));
#187663=CARTESIAN_POINT('Ctrl Pts',(6.76847019822405,0.110599030371753,
18.7022916087843));
#187664=CARTESIAN_POINT('Ctrl Pts',(6.76316137150845,0.289842699303895,
18.7107261240279));
#187665=CARTESIAN_POINT('Ctrl Pts',(6.75076280115442,0.468498241778733,
18.7191606392716));
#187666=CARTESIAN_POINT('Ctrl Pts',(6.73835824218467,0.647240076411422,
18.7275992284584));
#187667=CARTESIAN_POINT('Ctrl Pts',(6.71885714116907,0.825392886096013,
18.7360378176452));
#187668=CARTESIAN_POINT('Ctrl Pts',(6.69234872533146,1.00237594671579,18.7444764068319));
#187669=CARTESIAN_POINT('Ctrl Pts',(6.6658106790824,1.17955683435537,18.7529244284522));
#187670=CARTESIAN_POINT('Ctrl Pts',(6.63224972462385,1.35556503167329,18.7613724500725));
#187671=CARTESIAN_POINT('Ctrl Pts',(6.59180620945051,1.52983002227362,18.7698204716928));
#187672=CARTESIAN_POINT('Ctrl Pts',(6.56881876447694,1.62887944626843,18.7746221916051));
#187673=CARTESIAN_POINT('Ctrl Pts',(6.54360875772431,1.72736595802387,18.7794239115174));
#187674=CARTESIAN_POINT('Ctrl Pts',(6.51620908773702,1.82518714790935,18.7842256314298));
#187675=CARTESIAN_POINT('Ctrl Pts',(6.46919250666082,1.99304383769265,18.7924651632806));
#187676=CARTESIAN_POINT('Ctrl Pts',(6.41562069152411,2.15931522187927,18.8007046951314));
#187677=CARTESIAN_POINT('Ctrl Pts',(6.3556157227279,2.32345384826425,18.8089442269823));
#187678=CARTESIAN_POINT('Ctrl Pts',(6.29567735525339,2.48741029224537,18.8171746135286));
#187679=CARTESIAN_POINT('Ctrl Pts',(6.22932017288087,2.64923836061656,18.8254050000749));
#187680=CARTESIAN_POINT('Ctrl Pts',(6.15671669937133,2.80840319108247,18.8336353866212));
#187681=CARTESIAN_POINT('Ctrl Pts',(6.08418085885108,2.96741975325275,18.841858106239));
#187682=CARTESIAN_POINT('Ctrl Pts',(6.00541046200375,3.12377769638829,18.8500808258568));
#187683=CARTESIAN_POINT('Ctrl Pts',(5.92062706979467,3.27695958174869,18.8583035454745));
#187684=CARTESIAN_POINT('Ctrl Pts',(5.83591880177912,3.43000573692301,18.8665189791703));
#187685=CARTESIAN_POINT('Ctrl Pts',(5.74520832919491,3.57988113311468,18.8747344128661));
#187686=CARTESIAN_POINT('Ctrl Pts',(5.64876426078085,3.72609062237152,18.8829498465619));
#187687=CARTESIAN_POINT('Ctrl Pts',(5.55236975712871,3.8722249713046,18.8911610581628));
#187688=CARTESIAN_POINT('Ctrl Pts',(5.45024772159885,4.01469686907089,18.8993722697636));
#187689=CARTESIAN_POINT('Ctrl Pts',(5.34271162281037,4.15303762509889,18.9075834813644));
#187690=CARTESIAN_POINT('Ctrl Pts',(5.23521158569582,4.29133198927065,18.915791939378));
#187691=CARTESIAN_POINT('Ctrl Pts',(5.12230132030412,4.42549769075964,18.9240003973915));
#187692=CARTESIAN_POINT('Ctrl Pts',(5.00433641114425,4.55509671511988,18.932208855405));
#187693=CARTESIAN_POINT('Ctrl Pts',(4.95178046825714,4.61283591036879,18.9358659026882));
#187694=CARTESIAN_POINT('Ctrl Pts',(4.89822177462262,4.66966909417137,18.9395229499713));
#187695=CARTESIAN_POINT('Ctrl Pts',(4.84369431543715,4.72555968945498,18.9431799972545));
#187696=CARTESIAN_POINT('Ctrl Pts',(4.71153409293054,4.86102379541277,18.9520437182105));
#187697=CARTESIAN_POINT('Ctrl Pts',(4.57381795780396,4.9908074714394,18.9609074391665));
#187698=CARTESIAN_POINT('Ctrl Pts',(4.43105198088476,5.114495805326,18.9697711601225));
#187699=CARTESIAN_POINT('Ctrl Pts',(4.28806313149874,5.23837722950404,18.9786487182643));
#187700=CARTESIAN_POINT('Ctrl Pts',(4.14000889170728,5.3561441374664,18.9875262764061));
#187701=CARTESIAN_POINT('Ctrl Pts',(3.98742611781988,5.46742370362202,18.996403834548));
#187702=CARTESIAN_POINT('Ctrl Pts',(3.83446239597519,5.57898109749263,19.0053035569719));
#187703=CARTESIAN_POINT('Ctrl Pts',(3.67694773369977,5.68401859646539,19.0142032793958));
#187704=CARTESIAN_POINT('Ctrl Pts',(3.51544806098211,5.78220666619044,19.0231030018197));
#187705=CARTESIAN_POINT('Ctrl Pts',(3.37937896955083,5.86493353004133,19.0306013275056));
#187706=CARTESIAN_POINT('Ctrl Pts',(3.240481567078,5.94279899309329,19.0380996531916));
#187707=CARTESIAN_POINT('Ctrl Pts',(3.09910619832135,6.0156321173694,19.0455979788775));
#187708=CARTESIAN_POINT('Ctrl Pts',(3.09910619832132,6.01563211736941,17.0457499898821));
#187709=CARTESIAN_POINT('Ctrl Pts',(2.94375339480714,6.09566607338664,17.0539481383937));
#187710=CARTESIAN_POINT('Ctrl Pts',(2.78532240288702,6.16966581280104,17.0621462869052));
#187711=CARTESIAN_POINT('Ctrl Pts',(2.62432626980797,6.23740335633313,17.0703444354168));
#187712=CARTESIAN_POINT('Ctrl Pts',(2.46327734983215,6.30516310943417,17.0785452719111));
#187713=CARTESIAN_POINT('Ctrl Pts',(2.29966194389878,6.36665643748943,17.0867461084053));
#187714=CARTESIAN_POINT('Ctrl Pts',(2.1340116865812,6.42170406679838,17.0949469448996));
#187715=CARTESIAN_POINT('Ctrl Pts',(1.96613111823765,6.47749285604629,17.1032581972565));
#187716=CARTESIAN_POINT('Ctrl Pts',(1.79616087133529,6.52666100722362,17.1115694496133));
#187717=CARTESIAN_POINT('Ctrl Pts',(1.62466786371038,6.56907476990685,17.1198807019702));
#187718=CARTESIAN_POINT('Ctrl Pts',(1.45516451230489,6.61099644951404,17.1280955274513));
#187719=CARTESIAN_POINT('Ctrl Pts',(1.28417390863389,6.64631961986173,17.1363103529325));
#187720=CARTESIAN_POINT('Ctrl Pts',(1.11225114611088,6.67496714508581,17.1445251784136));
#187721=CARTESIAN_POINT('Ctrl Pts',(0.937301300133083,6.70411907384759,
17.1528846442083));
#187722=CARTESIAN_POINT('Ctrl Pts',(0.761386555647095,6.7263580488944,17.1612441100031));
#187723=CARTESIAN_POINT('Ctrl Pts',(0.585094191029671,6.74165808889945,
17.1696035757979));
#187724=CARTESIAN_POINT('Ctrl Pts',(0.408801826412231,6.7569581289045,17.1779630415926));
#187725=CARTESIAN_POINT('Ctrl Pts',(0.232132228866702,6.76531927755589,
17.1863225073874));
#187726=CARTESIAN_POINT('Ctrl Pts',(0.0556692259077685,6.76677101262388,
17.1946819731822));
#187727=CARTESIAN_POINT('Ctrl Pts',(-0.114668756466932,6.76817235805198,
17.2027512824047));
#187728=CARTESIAN_POINT('Ctrl Pts',(-0.285371928049203,6.76314019090073,
17.2108205916273));
#187729=CARTESIAN_POINT('Ctrl Pts',(-0.4559028109087,6.75162511007576,17.2188899008498));
#187730=CARTESIAN_POINT('Ctrl Pts',(-0.626220995408382,6.74012439168629,
17.2269491454505));
#187731=CARTESIAN_POINT('Ctrl Pts',(-0.796366951182522,6.72215687333881,
17.2350083900513));
#187732=CARTESIAN_POINT('Ctrl Pts',(-0.965799633635627,6.69772499194087,
17.2430676346521));
#187733=CARTESIAN_POINT('Ctrl Pts',(-1.13505816920609,6.67331822220333,
17.2511185957723));
#187734=CARTESIAN_POINT('Ctrl Pts',(-1.30360452418155,6.64246036435025,
17.2591695568926));
#187735=CARTESIAN_POINT('Ctrl Pts',(-1.47089931757245,6.60520584066575,
17.2672205180128));
#187736=CARTESIAN_POINT('Ctrl Pts',(-1.63805881906315,6.56798144484834,
17.2752649682919));
#187737=CARTESIAN_POINT('Ctrl Pts',(-1.8039684111023,6.52437075988779,17.283309418571));
#187738=CARTESIAN_POINT('Ctrl Pts',(-1.96809559704538,6.47447980311087,
17.29135386885));
#187739=CARTESIAN_POINT('Ctrl Pts',(-2.13212597865205,6.42461827266535,
17.2993935744083));
#187740=CARTESIAN_POINT('Ctrl Pts',(-2.29437569085549,6.36848395257984,
17.3074332799666));
#187741=CARTESIAN_POINT('Ctrl Pts',(-2.45432427650537,6.30623353086106,
17.3154729855249));
#187742=CARTESIAN_POINT('Ctrl Pts',(-2.61772526686236,6.24263946707075,
17.3236862238293));
#187743=CARTESIAN_POINT('Ctrl Pts',(-2.77872427492111,6.17266236142368,
17.3318994621338));
#187744=CARTESIAN_POINT('Ctrl Pts',(-2.93678424587852,6.09652255742237,
17.3401127004382));
#187745=CARTESIAN_POINT('Ctrl Pts',(-3.09145485437162,6.02201545898311,
17.3481498179864));
#187746=CARTESIAN_POINT('Ctrl Pts',(-3.24331085003061,5.94160746277927,
17.3561869355346));
#187747=CARTESIAN_POINT('Ctrl Pts',(-3.39187102761633,5.85555291428717,
17.3642240530828));
#187748=CARTESIAN_POINT('Ctrl Pts',(-3.54044692192388,5.76948926177122,
17.3722620209069));
#187749=CARTESIAN_POINT('Ctrl Pts',(-3.6857259805172,5.67777805470077,17.380299988731));
#187750=CARTESIAN_POINT('Ctrl Pts',(-3.82725363847947,5.58071846510337,
17.3883379565551));
#187751=CARTESIAN_POINT('Ctrl Pts',(-3.96882431101462,5.48362937613566,
17.3963783673629));
#187752=CARTESIAN_POINT('Ctrl Pts',(-4.10664100548792,5.38118888022057,
17.4044187781706));
#187753=CARTESIAN_POINT('Ctrl Pts',(-4.24028018494763,5.2737380436594,17.4124591889784));
#187754=CARTESIAN_POINT('Ctrl Pts',(-4.37897017165631,5.16222617150669,
17.4208034819661));
#187755=CARTESIAN_POINT('Ctrl Pts',(-4.51316035369398,5.04531811311258,
17.4291477749539));
#187756=CARTESIAN_POINT('Ctrl Pts',(-4.64241799654051,4.92343824429603,
17.4374920679417));
#187757=CARTESIAN_POINT('Ctrl Pts',(-4.76718829547796,4.80578959055451,
17.4455466781572));
#187758=CARTESIAN_POINT('Ctrl Pts',(-4.88736258487101,4.68350885586968,
17.4536012883728));
#187759=CARTESIAN_POINT('Ctrl Pts',(-5.00259214754638,4.55701226740803,
17.4616558985883));
#187760=CARTESIAN_POINT('Ctrl Pts',(-5.11790894062829,4.43041991924218,
17.4697166062575));
#187761=CARTESIAN_POINT('Ctrl Pts',(-5.2282733145682,4.29960564627444,17.4777773139268));
#187762=CARTESIAN_POINT('Ctrl Pts',(-5.33337892833046,4.16501599118666,
17.485838021596));
#187763=CARTESIAN_POINT('Ctrl Pts',(-5.43863273471159,4.03023657274805,
17.4939100943802));
#187764=CARTESIAN_POINT('Ctrl Pts',(-5.53861277116244,3.89167145183154,
17.5019821671643));
#187765=CARTESIAN_POINT('Ctrl Pts',(-5.63305748741487,3.74979364011931,
17.5100542399485));
#187766=CARTESIAN_POINT('Ctrl Pts',(-5.64294985387348,3.73493301729684,
17.5108997282429));
#187767=CARTESIAN_POINT('Ctrl Pts',(-5.65278153541568,3.72003607051119,
17.5117452165373));
#187768=CARTESIAN_POINT('Ctrl Pts',(-5.66255226178623,3.70510335652593,
17.5125907048317));
#187769=CARTESIAN_POINT('Ctrl Pts',(-5.76270161227652,3.55204394722865,
17.5212569083792));
#187770=CARTESIAN_POINT('Ctrl Pts',(-5.85673922726422,3.39477230473128,
17.5299231119266));
#187771=CARTESIAN_POINT('Ctrl Pts',(-5.94431510077504,3.23379142535474,
17.538589315474));
#187772=CARTESIAN_POINT('Ctrl Pts',(-6.03176681242811,3.07303877875789,
17.5472432323963));
#187773=CARTESIAN_POINT('Ctrl Pts',(-6.11277490536546,2.90858764615479,
17.5558971493186));
#187774=CARTESIAN_POINT('Ctrl Pts',(-6.18703289001532,2.74096935733852,
17.5645510662408));
#187775=CARTESIAN_POINT('Ctrl Pts',(-6.26119068053347,2.57357723098794,
17.5731933066855));
#187776=CARTESIAN_POINT('Ctrl Pts',(-6.32861640146307,2.40302674588132,
17.5818355471302));
#187777=CARTESIAN_POINT('Ctrl Pts',(-6.38904937959031,2.22987376888396,
17.5904777875749));
#187778=CARTESIAN_POINT('Ctrl Pts',(-6.45122769478795,2.05172004032724,
17.5993696205945));
#187779=CARTESIAN_POINT('Ctrl Pts',(-6.506003115993,1.87081150365074,17.6082614536141));
#187780=CARTESIAN_POINT('Ctrl Pts',(-6.55314366955184,1.68777873141376,
17.6171532866337));
#187781=CARTESIAN_POINT('Ctrl Pts',(-6.59882611067744,1.51040737680431,
17.6257700848626));
#187782=CARTESIAN_POINT('Ctrl Pts',(-6.63733882160785,1.33104155455838,
17.6343868830915));
#187783=CARTESIAN_POINT('Ctrl Pts',(-6.66852001686367,1.15027378683886,
17.6430036813205));
#187784=CARTESIAN_POINT('Ctrl Pts',(-6.70119409496568,0.960851280346185,
17.6520330317354));
#187785=CARTESIAN_POINT('Ctrl Pts',(-6.72581725199615,0.76988958644922,
17.6610623821503));
#187786=CARTESIAN_POINT('Ctrl Pts',(-6.74226255994324,0.578086994134694,
17.6700917325652));
#187787=CARTESIAN_POINT('Ctrl Pts',(-6.75870786789032,0.386284401820168,
17.6791210829802));
#187788=CARTESIAN_POINT('Ctrl Pts',(-6.76697523599835,0.193641289184741,
17.6881504333951));
#187789=CARTESIAN_POINT('Ctrl Pts',(-6.76699994441478,0.000867346750888167,
17.69717978381));
#187790=CARTESIAN_POINT('',(-6.76699928623195,0.00189866213851385,17.3028202161899));
#187791=CARTESIAN_POINT('Ctrl Pts',(3.09910619832134,6.0156321173694,16.6515631567322));
#187792=CARTESIAN_POINT('Ctrl Pts',(2.9290300129029,6.10325119881144,16.6605778338385));
#187793=CARTESIAN_POINT('Ctrl Pts',(2.75514883870212,6.18369867620815,16.6695925109447));
#187794=CARTESIAN_POINT('Ctrl Pts',(2.57805891666819,6.25666854022072,16.6786071880509));
#187795=CARTESIAN_POINT('Ctrl Pts',(2.40120466740917,6.32954129531744,16.6876098683482));
#187796=CARTESIAN_POINT('Ctrl Pts',(2.2211504107763,6.3949562038783,16.6966125486454));
#187797=CARTESIAN_POINT('Ctrl Pts',(2.03851437663987,6.45265434811385,16.7056152289427));
#187798=CARTESIAN_POINT('Ctrl Pts',(1.85627011947858,6.51022872266437,16.7145985973726));
#187799=CARTESIAN_POINT('Ctrl Pts',(1.6714553648832,6.5601192991368,16.7235819658025));
#187800=CARTESIAN_POINT('Ctrl Pts',(1.48470549405131,6.60211622102594,16.7325653342325));
#187801=CARTESIAN_POINT('Ctrl Pts',(1.41593201403153,6.61758222619944,16.7358735962756));
#187802=CARTESIAN_POINT('Ctrl Pts',(1.34689628536527,6.63197817138038,16.7391818583187));
#187803=CARTESIAN_POINT('Ctrl Pts',(1.27763067473933,6.64529524242265,16.7424901203618));
#187804=CARTESIAN_POINT('Ctrl Pts',(1.10759026829054,6.67798736990515,16.7506115852181));
#187805=CARTESIAN_POINT('Ctrl Pts',(0.936239495903021,6.70415924339922,
16.7587330500744));
#187806=CARTESIAN_POINT('Ctrl Pts',(0.764123403043425,6.72371953794337,
16.7668545149307));
#187807=CARTESIAN_POINT('Ctrl Pts',(0.592019584594924,6.74327843755057,
16.7749754006069));
#187808=CARTESIAN_POINT('Ctrl Pts',(0.419150918231919,6.75622665602547,
16.7830962862832));
#187809=CARTESIAN_POINT('Ctrl Pts',(0.246068696353916,6.76252461708456,
16.7912171719595));
#187810=CARTESIAN_POINT('Ctrl Pts',(0.0729657862011396,6.76882333093009,
16.7993390283139));
#187811=CARTESIAN_POINT('Ctrl Pts',(-0.100350364313188,6.76847019242484,
16.8074608846682));
#187812=CARTESIAN_POINT('Ctrl Pts',(-0.273327376901988,6.76147773382682,
16.8155827410226));
#187813=CARTESIAN_POINT('Ctrl Pts',(-0.446430591379407,6.7544801736175,
16.8237105229828));
#187814=CARTESIAN_POINT('Ctrl Pts',(-0.619193807480665,6.7408336334022,
16.8318383049431));
#187815=CARTESIAN_POINT('Ctrl Pts',(-0.791068043069388,6.72060267767961,
16.8399660869034));
#187816=CARTESIAN_POINT('Ctrl Pts',(-0.963012293833378,6.70036348061762,
16.8480971798199));
#187817=CARTESIAN_POINT('Ctrl Pts',(-1.13406648073328,6.67353457827942,
16.8562282727365));
#187818=CARTESIAN_POINT('Ctrl Pts',(-1.30369099925242,6.6402318316809,16.864359365653));
#187819=CARTESIAN_POINT('Ctrl Pts',(-1.47350065584488,6.60689273652619,
16.8724993333177));
#187820=CARTESIAN_POINT('Ctrl Pts',(-1.64187717144924,6.56706576828125,
16.8806393009823));
#187821=CARTESIAN_POINT('Ctrl Pts',(-1.80829457108359,6.52091709379821,
16.888779268647));
#187822=CARTESIAN_POINT('Ctrl Pts',(-1.89460582994727,6.49698239587435,
16.8930010078268));
#187823=CARTESIAN_POINT('Ctrl Pts',(-1.98039038954802,6.47134802511404,
16.8972227470067));
#187824=CARTESIAN_POINT('Ctrl Pts',(-2.06557696693827,6.44404227124979,
16.9014444861866));
#187825=CARTESIAN_POINT('Ctrl Pts',(-2.2358841615612,6.38945190642762,16.9098846956442));
#187826=CARTESIAN_POINT('Ctrl Pts',(-2.40415211785132,6.3280654831791,16.9183249051018));
#187827=CARTESIAN_POINT('Ctrl Pts',(-2.56982043884364,6.26005686173069,
16.9267651145594));
#187828=CARTESIAN_POINT('Ctrl Pts',(-2.73536324153929,6.1920997668884,16.935198929308));
#187829=CARTESIAN_POINT('Ctrl Pts',(-2.89831002782752,6.11753060167729,
16.9436327440565));
#187830=CARTESIAN_POINT('Ctrl Pts',(-3.05811755351506,6.03657237419408,
16.9520665588051));
#187831=CARTESIAN_POINT('Ctrl Pts',(-3.21782856803923,5.95566303910617,
16.9604952801935));
#187832=CARTESIAN_POINT('Ctrl Pts',(-3.37440380490131,5.8683724845296,16.968924001582));
#187833=CARTESIAN_POINT('Ctrl Pts',(-3.52732156913216,5.77497112961918,
16.9773527229705));
#187834=CARTESIAN_POINT('Ctrl Pts',(-3.6801704648151,5.68161183925057,16.9857776483722));
#187835=CARTESIAN_POINT('Ctrl Pts',(-3.82936488805848,5.58214740942622,
16.9942025737739));
#187836=CARTESIAN_POINT('Ctrl Pts',(-3.97440891114378,5.47689353621384,
17.0026274991757));
#187837=CARTESIAN_POINT('Ctrl Pts',(-4.11940986577368,5.37167091642127,
17.0110499229333));
#187838=CARTESIAN_POINT('Ctrl Pts',(-4.26026260829009,5.26066247711803,
17.019472346691));
#187839=CARTESIAN_POINT('Ctrl Pts',(-4.39650098195543,5.14422667809895,
17.0278947704486));
#187840=CARTESIAN_POINT('Ctrl Pts',(-4.53274149825916,5.02778904787912,
17.0363173266668));
#187841=CARTESIAN_POINT('Ctrl Pts',(-4.66436724294385,4.90592409895155,
17.044739882885));
#187842=CARTESIAN_POINT('Ctrl Pts',(-4.79094538165991,4.77903037759247,
17.0531624391032));
#187843=CARTESIAN_POINT('Ctrl Pts',(-4.91752779620949,4.65213236973942,
17.0615852798369));
#187844=CARTESIAN_POINT('Ctrl Pts',(-5.03906202911034,4.5202054867929,17.0700081205706));
#187845=CARTESIAN_POINT('Ctrl Pts',(-5.15515224362191,4.3836850189173,17.0784309613044));
#187846=CARTESIAN_POINT('Ctrl Pts',(-5.27126258716118,4.24714087958678,
17.086855262485));
#187847=CARTESIAN_POINT('Ctrl Pts',(-5.38192681428208,4.1060018214728,17.0952795636656));
#187848=CARTESIAN_POINT('Ctrl Pts',(-5.48678927499912,3.96073635221466,
17.1037038648463));
#187849=CARTESIAN_POINT('Ctrl Pts',(-5.59168456239499,3.81542540831408,
17.1121308032131));
#187850=CARTESIAN_POINT('Ctrl Pts',(-5.69077426719004,3.66598574821698,
17.1205577415798));
#187851=CARTESIAN_POINT('Ctrl Pts',(-5.78374577315878,3.51291528953772,
17.1289846799466));
#187852=CARTESIAN_POINT('Ctrl Pts',(-5.87680087219783,3.35970720127529,
17.1374191951903));
#187853=CARTESIAN_POINT('Ctrl Pts',(-5.96372660715476,3.20286207672421,
17.1458537104339));
#187854=CARTESIAN_POINT('Ctrl Pts',(-6.04425552838593,3.04290389391058,
17.1542882256775));
#187855=CARTESIAN_POINT('Ctrl Pts',(-6.12482334577584,2.8828684499245,17.1627268148643));
#187856=CARTESIAN_POINT('Ctrl Pts',(-6.19898804473388,2.71971725021237,
17.171165404051));
#187857=CARTESIAN_POINT('Ctrl Pts',(-6.26652993601944,2.55399521553432,
17.1796039932378));
#187858=CARTESIAN_POINT('Ctrl Pts',(-6.33414732385861,2.38808794111488,
17.1880520148581));
#187859=CARTESIAN_POINT('Ctrl Pts',(-6.39512699364902,2.21960440168293,
17.1965000364784));
#187860=CARTESIAN_POINT('Ctrl Pts',(-6.44929842583447,2.04910683336157,
17.2049480580986));
#187861=CARTESIAN_POINT('Ctrl Pts',(-6.48008859852863,1.9521987517259,17.2097497780111));
#187862=CARTESIAN_POINT('Ctrl Pts',(-6.50868021828342,1.85464027326941,
17.2145514979236));
#187863=CARTESIAN_POINT('Ctrl Pts',(-6.53504930254438,1.7565362544833,17.2193532178361));
#187864=CARTESIAN_POINT('Ctrl Pts',(-6.58542900941581,1.56910268036138,
17.2285271898738));
#187865=CARTESIAN_POINT('Ctrl Pts',(-6.62778878429327,1.37932214171602,
17.2377011619115));
#187866=CARTESIAN_POINT('Ctrl Pts',(-6.66192816455315,1.18785610674587,
17.2468751339492));
#187867=CARTESIAN_POINT('Ctrl Pts',(-6.69662651964657,0.993255138036172,
17.2561993143226));
#187868=CARTESIAN_POINT('Ctrl Pts',(-6.72283281816732,0.7969131662594,17.2655234946961));
#187869=CARTESIAN_POINT('Ctrl Pts',(-6.74038839512921,0.599544229233806,
17.2748476750695));
#187870=CARTESIAN_POINT('Ctrl Pts',(-6.75794397209109,0.402175292208195,
17.284171855443));
#187871=CARTESIAN_POINT('Ctrl Pts',(-6.7668486980841,0.203779598658603,
17.2934960358164));
#187872=CARTESIAN_POINT('Ctrl Pts',(-6.76699808730845,0.00508786436940122,
17.3028202161899));
#187873=CARTESIAN_POINT('Ctrl Pts',(-6.767,1.1633950350217E-12,17.3028202161899));
#187874=CARTESIAN_POINT('Ctrl Pts',(-6.76700000000003,-0.186007249525797,
17.3115697280011));
#187875=CARTESIAN_POINT('Ctrl Pts',(-6.75932637294526,-0.372014355748932,
17.3203192398123));
#187876=CARTESIAN_POINT('Ctrl Pts',(-6.74400518264188,-0.557389537486598,
17.3290687516235));
#187877=CARTESIAN_POINT('Ctrl Pts',(-6.72868405705094,-0.742763936251031,
17.3378182264791));
#187878=CARTESIAN_POINT('Ctrl Pts',(-6.70571545645734,-0.927506130241638,
17.3465677013348));
#187879=CARTESIAN_POINT('Ctrl Pts',(-6.67517739404809,-1.11098863990111,
17.3553171761905));
#187880=CARTESIAN_POINT('Ctrl Pts',(-6.64463945808678,-1.29447038982072,
17.3640666148175));
#187881=CARTESIAN_POINT('Ctrl Pts',(-6.60653217008321,-1.47669218313838,
17.3728160534445));
#187882=CARTESIAN_POINT('Ctrl Pts',(-6.56098496092631,-1.65703510599469,
17.3815654920716));
#187883=CARTESIAN_POINT('Ctrl Pts',(-6.51543793658245,-1.83737729708882,
17.3903148951967));
#187884=CARTESIAN_POINT('Ctrl Pts',(-6.46245112167364,-2.01584035511107,
17.3990642983219));
#187885=CARTESIAN_POINT('Ctrl Pts',(-6.40220448374192,-2.19181813760969,
17.4078137014471));
#187886=CARTESIAN_POINT('Ctrl Pts',(-6.34195808526437,-2.36779522067322,
17.4165630697972));
#187887=CARTESIAN_POINT('Ctrl Pts',(-6.27445201433031,-2.54128677684345,
17.4253124381473));
#187888=CARTESIAN_POINT('Ctrl Pts',(-6.19991555071823,-2.71170355384991,
17.4340618064974));
#187889=CARTESIAN_POINT('Ctrl Pts',(-6.12537937716609,-2.88211966767653,
17.4428111407991));
#187890=CARTESIAN_POINT('Ctrl Pts',(-6.04381298052433,-3.04946076371958,
17.4515604751009));
#187891=CARTESIAN_POINT('Ctrl Pts',(-5.9554933933574,-3.21315848374716,
17.4603098094027));
#187892=CARTESIAN_POINT('Ctrl Pts',(-5.86717414255315,-3.37685558033655,
17.4690591103829));
#187893=CARTESIAN_POINT('Ctrl Pts',(-5.77210188876502,-3.53690907646913,
17.4778084113631));
#187894=CARTESIAN_POINT('Ctrl Pts',(-5.67059953346898,-3.69277536969437,
17.4865577123433));
#187895=CARTESIAN_POINT('Ctrl Pts',(-5.56909755631284,-3.84864108225068,
17.4953069807285));
#187896=CARTESIAN_POINT('Ctrl Pts',(-5.46116568196749,-4.00031938297655,
17.5040562491138));
#187897=CARTESIAN_POINT('Ctrl Pts',(-5.347170485335,-4.14729511859987,17.5128055174991));
#187898=CARTESIAN_POINT('Ctrl Pts',(-5.23317570391736,-4.29427031888038,
17.5215547540161));
#187899=CARTESIAN_POINT('Ctrl Pts',(-5.11311782003418,-4.43654276189658,
17.5303039905332));
#187900=CARTESIAN_POINT('Ctrl Pts',(-4.98740458984661,-4.57362924351952,
17.5390532270502));
#187901=CARTESIAN_POINT('Ctrl Pts',(-4.86169180711658,-4.71071523720354,
17.5478024324256));
#187902=CARTESIAN_POINT('Ctrl Pts',(-4.73032391204094,-4.84261509523313,
17.5565516378011));
#187903=CARTESIAN_POINT('Ctrl Pts',(-4.5937470701353,-4.96888084538393,
17.5653008431765));
#187904=CARTESIAN_POINT('Ctrl Pts',(-4.45717070301363,-5.09514615659536,
17.574050018137));
#187905=CARTESIAN_POINT('Ctrl Pts',(-4.31538563570945,-5.21577720459607,
17.5827991930974));
#187906=CARTESIAN_POINT('Ctrl Pts',(-4.16887341029399,-5.33036429232972,
17.5915483680579));
#187907=CARTESIAN_POINT('Ctrl Pts',(-4.02236168203613,-5.44495099123684,
17.6002975133299));
#187908=CARTESIAN_POINT('Ctrl Pts',(-3.87112305348091,-5.55349359438653,
17.6090466586019));
#187909=CARTESIAN_POINT('Ctrl Pts',(-3.71567117017705,-5.6556234629893,
17.6177958038739));
#187910=CARTESIAN_POINT('Ctrl Pts',(-3.56021980145756,-5.75775299351683,
17.6265449201841));
#187911=CARTESIAN_POINT('Ctrl Pts',(-3.40055544538278,-5.85346967463914,
17.6352940364942));
#187912=CARTESIAN_POINT('Ctrl Pts',(-3.23722035986775,-5.94244842986944,
17.6440431528044));
#187913=CARTESIAN_POINT('Ctrl Pts',(-3.07388580147109,-6.03142689794565,
17.6527922408793));
#187914=CARTESIAN_POINT('Ctrl Pts',(-2.90688078896514,-6.11366734656812,
17.6615413289541));
#187915=CARTESIAN_POINT('Ctrl Pts',(-2.73677250721314,-6.18889046952379,
17.6702904170289));
#187916=CARTESIAN_POINT('Ctrl Pts',(-2.56666476031418,-6.26411335596354,
17.679039477595));
#187917=CARTESIAN_POINT('Ctrl Pts',(-2.39345402575093,-6.33231884500583,
17.687788538161));
#187918=CARTESIAN_POINT('Ctrl Pts',(-2.21772856065511,-6.39327529762755,
17.696537598727));
#187919=CARTESIAN_POINT('Ctrl Pts',(-2.04200363348415,-6.45423156365143,
17.7052866325107));
#187920=CARTESIAN_POINT('Ctrl Pts',(-1.86376426189162,-6.50793874375692,
17.7140356662944));
#187921=CARTESIAN_POINT('Ctrl Pts',(-1.6836157775302,-6.55421443909576,
17.7227847000781));
#187922=CARTESIAN_POINT('Ctrl Pts',(-1.50346782967657,-6.60048999661901,
17.731533707806));
#187923=CARTESIAN_POINT('Ctrl Pts',(-1.32141105794836,-6.63933404237743,
17.7402827155338));
#187924=CARTESIAN_POINT('Ctrl Pts',(-1.13806375486863,-6.67061465607588,
17.7490317232616));
#187925=CARTESIAN_POINT('Ctrl Pts',(-0.954716982601851,-6.70189517921312,
17.75778070566));
#187926=CARTESIAN_POINT('Ctrl Pts',(-0.770079968901402,-6.72561226592235,
17.7665296880584));
#187927=CARTESIAN_POINT('Ctrl Pts',(-0.584779765557945,-6.74168536983105,
17.7752786704568));
#187928=CARTESIAN_POINT('Ctrl Pts',(-0.391489830651026,-6.75845151013855,
17.7844048894666));
#187929=CARTESIAN_POINT('Ctrl Pts',(-0.197478578238093,-6.76689983031626,
17.7935311084765));
#187930=CARTESIAN_POINT('Ctrl Pts',(-0.00346287645113099,-6.76699911397118,
17.8026573274864));
#187931=CARTESIAN_POINT('Ctrl Pts',(0.184489834654988,-6.76709529501188,
17.8114983521522));
#187932=CARTESIAN_POINT('Ctrl Pts',(0.372446404250464,-6.75935639738162,
17.820339376818));
#187933=CARTESIAN_POINT('Ctrl Pts',(0.55975501948942,-6.74380925873178,
17.8291804014838));
#187934=CARTESIAN_POINT('Ctrl Pts',(0.745134705522872,-6.72842222659793,
17.8379303800935));
#187935=CARTESIAN_POINT('Ctrl Pts',(0.929879431229677,-6.70538706057508,
17.8466803587033));
#187936=CARTESIAN_POINT('Ctrl Pts',(1.11336163626937,-6.67478200894109,
17.855430337313));
#187937=CARTESIAN_POINT('Ctrl Pts',(1.29684196300853,-6.64417727060987,
17.8641802263496));
#187938=CARTESIAN_POINT('Ctrl Pts',(1.47905951217666,-6.60600284890556,
17.8729301153861));
#187939=CARTESIAN_POINT('Ctrl Pts',(1.65939532067261,-6.56038841607186,
17.8816800044226));
#187940=CARTESIAN_POINT('Ctrl Pts',(1.8397293430099,-6.51477443503204,17.8904298067948));
#187941=CARTESIAN_POINT('Ctrl Pts',(2.01818138406464,-6.46172066062079,
17.899179609167));
#187942=CARTESIAN_POINT('Ctrl Pts',(2.1941452835441,-6.40140730423406,17.9079294115391));
#187943=CARTESIAN_POINT('Ctrl Pts',(2.37010749864208,-6.34109452518564,
17.9166791301554));
#187944=CARTESIAN_POINT('Ctrl Pts',(2.54358134866666,-6.2735223961642,17.9254288487718));
#187945=CARTESIAN_POINT('Ctrl Pts',(2.7139775943576,-6.19892043966729,17.9341785673881));
#187946=CARTESIAN_POINT('Ctrl Pts',(2.88437226558316,-6.12431917249424,
17.9429282051568));
#187947=CARTESIAN_POINT('Ctrl Pts',(3.05168912681136,-6.04268832278707,
17.9516778429255));
#187948=CARTESIAN_POINT('Ctrl Pts',(3.21535986274024,-5.95430516123243,
17.9604274806942));
#187949=CARTESIAN_POINT('Ctrl Pts',(3.37902914073013,-5.86592278697342,
17.9691770405233));
#187950=CARTESIAN_POINT('Ctrl Pts',(3.53905210621745,-5.77078835741835,
17.9779266003523));
#187951=CARTESIAN_POINT('Ctrl Pts',(3.69488522831872,-5.66922500431515,
17.9866761601814));
#187952=CARTESIAN_POINT('Ctrl Pts',(3.85071701407118,-5.5676625221697,17.9954256449785));
#187953=CARTESIAN_POINT('Ctrl Pts',(4.00235878822585,-5.45967138329237,
18.0041751297756));
#187954=CARTESIAN_POINT('Ctrl Pts',(4.14929549611509,-5.34561838199464,
18.0129246145728));
#187955=CARTESIAN_POINT('Ctrl Pts',(4.2962309927627,-5.23156632086868,18.0216740272453));
#187956=CARTESIAN_POINT('Ctrl Pts',(4.43846127436203,-5.11145267304811,
18.0304234399179));
#187957=CARTESIAN_POINT('Ctrl Pts',(4.57550326054613,-4.98568540049728,
18.0391728525905));
#187958=CARTESIAN_POINT('Ctrl Pts',(4.71254416257948,-4.85991912290199,
18.0479221960458));
#187959=CARTESIAN_POINT('Ctrl Pts',(4.84439664018924,-4.72849950385252,
18.056671539501));
#187960=CARTESIAN_POINT('Ctrl Pts',(4.97061286794903,-4.59187289860897,
18.0654208829563));
#187961=CARTESIAN_POINT('Ctrl Pts',(5.09682813912833,-4.45524732884515,
18.0741701601011));
#187962=CARTESIAN_POINT('Ctrl Pts',(5.21740705147979,-4.31341506235618,
18.0829194372459));
#187963=CARTESIAN_POINT('Ctrl Pts',(5.33194007545827,-4.16685781275556,
18.0916687143907));
#187964=CARTESIAN_POINT('Ctrl Pts',(5.44647226944609,-4.02030162521673,
18.1004179281319));
#187965=CARTESIAN_POINT('Ctrl Pts',(5.5549584862823,-3.86902074887766,18.109167141873));
#187966=CARTESIAN_POINT('Ctrl Pts',(5.65703027291897,-3.71352898080495,
18.1179163556141));
#187967=CARTESIAN_POINT('Ctrl Pts',(5.75910135377104,-3.55803828789415,
18.126665508858));
#187968=CARTESIAN_POINT('Ctrl Pts',(5.85475793592856,-3.39833700106534,
18.1354146621019));
#187969=CARTESIAN_POINT('Ctrl Pts',(5.94367514427499,-3.23496750823369,
18.1441638153458));
#187970=CARTESIAN_POINT('Ctrl Pts',(6.03259176732734,-3.0715990907754,18.1529129109987));
#187971=CARTESIAN_POINT('Ctrl Pts',(6.11476896836012,-2.90456276731249,
18.1616620066516));
#187972=CARTESIAN_POINT('Ctrl Pts',(6.18992765547968,-2.73442583002864,
18.1704111023045));
#187973=CARTESIAN_POINT('Ctrl Pts',(6.26508587283129,-2.56428995615988,
18.1791601432726));
#187974=CARTESIAN_POINT('Ctrl Pts',(6.33322554827227,-2.39105376935023,
18.1879091842406));
#187975=CARTESIAN_POINT('Ctrl Pts',(6.39411526733091,-2.21530561053905,
18.1966582252086));
#187976=CARTESIAN_POINT('Ctrl Pts',(6.45500462602902,-2.03955849184926,
18.2054072143977));
#187977=CARTESIAN_POINT('Ctrl Pts',(6.50864402040789,-1.86129970164375,
18.2141562035867));
#187978=CARTESIAN_POINT('Ctrl Pts',(6.55485128368644,-1.68113463135892,
18.2229051927757));
#187979=CARTESIAN_POINT('Ctrl Pts',(6.6019980955436,-1.49730620116719,18.2318320782471));
#187980=CARTESIAN_POINT('Ctrl Pts',(6.64140720707899,-1.31149343245565,
18.2407589637186));
#187981=CARTESIAN_POINT('Ctrl Pts',(6.67293928722903,-1.12435326697408,
18.24968584919));
#187982=CARTESIAN_POINT('Ctrl Pts',(6.70384625876272,-0.940923067005458,
18.2584357633674));
#187983=CARTESIAN_POINT('Ctrl Pts',(6.72718554579808,-0.756217899520573,
18.2671856775449));
#187984=CARTESIAN_POINT('Ctrl Pts',(6.74287786815337,-0.570865181253446,
18.2759355917224));
#187985=CARTESIAN_POINT('Ctrl Pts',(6.75856988190852,-0.385516108072936,
18.2846853338269));
#187986=CARTESIAN_POINT('Ctrl Pts',(6.76661520773406,-0.199519795225378,
18.2934350759313));
#187987=CARTESIAN_POINT('Ctrl Pts',(6.76698651789579,-0.0135080204547203,
18.3021848180358));
#187988=CARTESIAN_POINT('Ctrl Pts',(6.767357821249,0.172500343513846,18.3109343997008));
#187989=CARTESIAN_POINT('Ctrl Pts',(6.76005538995179,0.358523882211763,
18.3196839813658));
#187990=CARTESIAN_POINT('Ctrl Pts',(6.74510402742355,0.543930748565174,
18.3284335630307));
#187991=CARTESIAN_POINT('Ctrl Pts',(6.73015291918022,0.729334461615976,
18.3371829958874));
#187992=CARTESIAN_POINT('Ctrl Pts',(6.70755316306585,0.914121237635365,
18.3459324287441));
#187993=CARTESIAN_POINT('Ctrl Pts',(6.67738151874564,1.09766345166185,18.3546818616008));
#187994=CARTESIAN_POINT('Ctrl Pts',(6.64721034747557,1.28120278799726,18.3634311572783));
#187995=CARTESIAN_POINT('Ctrl Pts',(6.60946757205128,1.4634973186039,18.3721804529558));
#187996=CARTESIAN_POINT('Ctrl Pts',(6.56428138111508,1.64392790278223,18.3809297486333));
#187997=CARTESIAN_POINT('Ctrl Pts',(6.51909583859835,1.8243558977911,18.3896789187589));
#187998=CARTESIAN_POINT('Ctrl Pts',(6.4664671639286,2.00291972192313,18.3984280888845));
#187999=CARTESIAN_POINT('Ctrl Pts',(6.40657409872869,2.17901292274706,18.4071772590101));
#188000=CARTESIAN_POINT('Ctrl Pts',(6.34668181342065,2.35510383059007,18.4159263152092));
#188001=CARTESIAN_POINT('Ctrl Pts',(6.27952541914042,2.52872390822599,18.4246753714083));
#188002=CARTESIAN_POINT('Ctrl Pts',(6.20533299175513,2.69928350890293,18.4334244276074));
#188003=CARTESIAN_POINT('Ctrl Pts',(6.12831602991544,2.87633637965634,18.4425065637656));
#188004=CARTESIAN_POINT('Ctrl Pts',(6.04371690605263,3.05009086601475,18.4515886999238));
#188005=CARTESIAN_POINT('Ctrl Pts',(5.95184520316622,3.2199111288275,18.460670836082));
#188006=CARTESIAN_POINT('Ctrl Pts',(5.86333549509262,3.3835169118304,18.4694206164256));
#188007=CARTESIAN_POINT('Ctrl Pts',(5.76807618099351,3.54347103712033,18.4781703967692));
#188008=CARTESIAN_POINT('Ctrl Pts',(5.66639083308993,3.6992301802773,18.4869201771127));
#188009=CARTESIAN_POINT('Ctrl Pts',(5.56470914082176,3.85498372382086,18.4956696428977));
#188010=CARTESIAN_POINT('Ctrl Pts',(5.4566020337204,4.00654234702035,18.5044191086826));
#188011=CARTESIAN_POINT('Ctrl Pts',(5.34243669839187,4.15339127986707,18.5131685744675));
#188012=CARTESIAN_POINT('Ctrl Pts',(5.2282748605056,4.30023571401317,18.5219177722135));
#188013=CARTESIAN_POINT('Ctrl Pts',(5.10805534167078,4.44237052028507,18.5306669699595));
#188014=CARTESIAN_POINT('Ctrl Pts',(4.98218644339917,4.57931296628758,18.5394161677055));
#188015=CARTESIAN_POINT('Ctrl Pts',(4.85632073219553,4.71625194483394,18.5481651439171));
#188016=CARTESIAN_POINT('Ctrl Pts',(4.72480612170287,4.84799861524539,18.5569141201288));
#188017=CARTESIAN_POINT('Ctrl Pts',(4.58808925235281,4.97410554898513,18.5656630963404));
#188018=CARTESIAN_POINT('Ctrl Pts',(4.4513634947402,5.10022068121231,18.5744126413421));
#188019=CARTESIAN_POINT('Ctrl Pts',(4.30943501210053,5.22069514871856,18.5831621863438));
#188020=CARTESIAN_POINT('Ctrl Pts',(4.16278587431757,5.33511975166276,18.5919117313455));
#188021=CARTESIAN_POINT('Ctrl Pts',(4.01614535740402,5.44953762807877,18.6006607619993));
#188022=CARTESIAN_POINT('Ctrl Pts',(3.86478496657856,5.55790617532831,18.609409792653));
#188023=CARTESIAN_POINT('Ctrl Pts',(3.70921874747106,5.65985735539415,18.6181588233067));
#188024=CARTESIAN_POINT('Ctrl Pts',(3.5536504160581,5.76180991977102,18.6269079727564));
#188025=CARTESIAN_POINT('Ctrl Pts',(3.39387638174431,5.85734478552866,18.635657122206));
#188026=CARTESIAN_POINT('Ctrl Pts',(3.23043927904447,5.94613749121282,18.6444062716556));
#188027=CARTESIAN_POINT('Ctrl Pts',(3.18691767070367,5.96978206944181,18.6467360795717));
#188028=CARTESIAN_POINT('Ctrl Pts',(3.14313645919597,5.99294880633443,18.6490658874879));
#188029=CARTESIAN_POINT('Ctrl Pts',(3.09910619832135,6.0156321173694,18.651395695404));
#188030=CARTESIAN_POINT('Origin',(0.,0.,4.30282021618968));
#188031=CARTESIAN_POINT('',(3.09910619832133,6.01563211736941,21.0459783413229));
#188032=CARTESIAN_POINT('',(3.09910619832131,6.01563211736942,20.6513174420499));
#188033=CARTESIAN_POINT('',(3.09910619832133,6.0156321173694,4.30282021618968));
#188034=CARTESIAN_POINT('',(-6.76699485396139,-0.00834544546909593,19.6971797837639));
#188035=CARTESIAN_POINT('Ctrl Pts',(-6.76699485396019,-0.00834544644487561,
19.69717978381));
#188036=CARTESIAN_POINT('Ctrl Pts',(-6.76663983601997,-0.296215555059323,
19.7107704646661));
#188037=CARTESIAN_POINT('Ctrl Pts',(-6.74791479279641,-0.583282457482189,
19.7243611455222));
#188038=CARTESIAN_POINT('Ctrl Pts',(-6.71113050647912,-0.867765132397808,
19.7379518263783));
#188039=CARTESIAN_POINT('Ctrl Pts',(-6.68857677325034,-1.04219141602641,
19.746284748425));
#188040=CARTESIAN_POINT('Ctrl Pts',(-6.65918964291552,-1.21596185562541,
19.7546176704717));
#188041=CARTESIAN_POINT('Ctrl Pts',(-6.62301540300872,-1.38850854210884,
19.7629505925184));
#188042=CARTESIAN_POINT('Ctrl Pts',(-6.58688391228112,-1.56085132025203,
19.771273667072));
#188043=CARTESIAN_POINT('Ctrl Pts',(-6.54398136066317,-1.73197288854462,
19.7795967416257));
#188044=CARTESIAN_POINT('Ctrl Pts',(-6.49440571141654,-1.9013109833797,
19.7879198161793));
#188045=CARTESIAN_POINT('Ctrl Pts',(-6.44487954867015,-2.07048004463076,
19.7962345826252));
#188046=CARTESIAN_POINT('Ctrl Pts',(-6.38869365649649,-2.23786884743151,
19.8045493490712));
#188047=CARTESIAN_POINT('Ctrl Pts',(-6.32599695399928,-2.40292562057002,
19.8128641155172));
#188048=CARTESIAN_POINT('Ctrl Pts',(-6.263351334775,-2.56784791071574,19.8211721073567));
#188049=CARTESIAN_POINT('Ctrl Pts',(-6.1942055985028,-2.73044163336407,
19.8294800991962));
#188050=CARTESIAN_POINT('Ctrl Pts',(-6.11875843919035,-2.89017026537138,
19.8377880910357));
#188051=CARTESIAN_POINT('Ctrl Pts',(-6.04335891981515,-3.04979803921418,
19.8460908369228));
#188052=CARTESIAN_POINT('Ctrl Pts',(-5.96166605513343,-3.20656401404263,
19.8543935828099));
#188053=CARTESIAN_POINT('Ctrl Pts',(-5.87392668322694,-3.35995153537586,
19.862696328697));
#188054=CARTESIAN_POINT('Ctrl Pts',(-5.78622316760571,-3.5132763721172,
19.8709956815165));
#188055=CARTESIAN_POINT('Ctrl Pts',(-5.69247824091975,-3.66322520490996,
19.8792950343359));
#188056=CARTESIAN_POINT('Ctrl Pts',(-5.59298485550267,-3.80930563306724,
19.8875943871553));
#188057=CARTESIAN_POINT('Ctrl Pts',(-5.49351263065923,-3.95535499236859,
19.8958919748417));
#188058=CARTESIAN_POINT('Ctrl Pts',(-5.38829457851184,-4.09753729874758,
19.904189562528));
#188059=CARTESIAN_POINT('Ctrl Pts',(-5.27766730990099,-4.23538862042227,
19.9124871502144));
#188060=CARTESIAN_POINT('Ctrl Pts',(-5.16704518633951,-4.37323353091222,
19.9207843519968));
#188061=CARTESIAN_POINT('Ctrl Pts',(-5.05101456549176,-4.50674758687055,
19.9290815537792));
#188062=CARTESIAN_POINT('Ctrl Pts',(-4.92995283800137,-4.63549932748159,
19.9373787555616));
#188063=CARTESIAN_POINT('Ctrl Pts',(-4.80887662427978,-4.76426647450985,
19.9456769501861));
#188064=CARTESIAN_POINT('Ctrl Pts',(-4.68276834305796,-4.88826991765115,
19.9539751448107));
#188065=CARTESIAN_POINT('Ctrl Pts',(-4.55204291185383,-5.00711437143604,
19.9622733394352));
#188066=CARTESIAN_POINT('Ctrl Pts',(-4.42122553992976,-5.12604240991092,
19.9705773702768));
#188067=CARTESIAN_POINT('Ctrl Pts',(-4.28578478702871,-5.23980397450223,
19.9788814011184));
#188068=CARTESIAN_POINT('Ctrl Pts',(-4.14617007011083,-5.34804288966694,
19.9871854319599));
#188069=CARTESIAN_POINT('Ctrl Pts',(-4.00650458543936,-5.4563211634802,
19.9954924823757));
#188070=CARTESIAN_POINT('Ctrl Pts',(-3.8626623910893,-5.55907257800273,
20.0037995327914));
#188071=CARTESIAN_POINT('Ctrl Pts',(-3.71512284945592,-5.6559836645318,
20.0121065832071));
#188072=CARTESIAN_POINT('Ctrl Pts',(-3.56742556315202,-5.75299836536822,
20.0204225152618));
#188073=CARTESIAN_POINT('Ctrl Pts',(-3.41602332625222,-5.84416007711451,
20.0287384473164));
#188074=CARTESIAN_POINT('Ctrl Pts',(-3.2614220687476,-5.92920020656126,
20.037054379371));
#188075=CARTESIAN_POINT('Ctrl Pts',(-3.14488035700249,-5.99330526244966,
20.04332310559));
#188076=CARTESIAN_POINT('Ctrl Pts',(-3.02652135922019,-6.05393268165057,
20.0495918318089));
#188077=CARTESIAN_POINT('Ctrl Pts',(-2.90656953784754,-6.1109853969435,
20.0558605580279));
#188078=CARTESIAN_POINT('Ctrl Pts',(-2.74487398933406,-6.18789269178828,
20.0643108267512));
#188079=CARTESIAN_POINT('Ctrl Pts',(-2.57998689571232,-6.25844371075106,
20.0727610954746));
#188080=CARTESIAN_POINT('Ctrl Pts',(-2.4124349855146,-6.32237664495443,
20.0812113641979));
#188081=CARTESIAN_POINT('Ctrl Pts',(-2.24503094556222,-6.38625315617428,
20.0896541752724));
#188082=CARTESIAN_POINT('Ctrl Pts',(-2.07496708493001,-6.44352310651362,
20.0980969863469));
#188083=CARTESIAN_POINT('Ctrl Pts',(-1.90279177887941,-6.49397200842666,
20.1065397974214));
#188084=CARTESIAN_POINT('Ctrl Pts',(-1.73074498126691,-6.54438325621996,
20.1149763069391));
#188085=CARTESIAN_POINT('Ctrl Pts',(-1.55659019695295,-6.5879835114835,
20.1234128164569));
#188086=CARTESIAN_POINT('Ctrl Pts',(-1.38089307407099,-6.62460740859281,
20.1318493259746));
#188087=CARTESIAN_POINT('Ctrl Pts',(-1.20532167193471,-6.66120509933301,
20.1402797987158));
#188088=CARTESIAN_POINT('Ctrl Pts',(-1.02821045640877,-6.69083632168633,
20.1487102714571));
#188089=CARTESIAN_POINT('Ctrl Pts',(-0.850137643089211,-6.71338625343446,
20.1571407441983));
#188090=CARTESIAN_POINT('Ctrl Pts',(-0.672141382789677,-6.73592649102801,
20.1655675927021));
#188091=CARTESIAN_POINT('Ctrl Pts',(-0.493184677152069,-6.75139146520927,
20.1739944412059));
#188092=CARTESIAN_POINT('Ctrl Pts',(-0.313853936722314,-6.75971779783771,
20.1824212897097));
#188093=CARTESIAN_POINT('Ctrl Pts',(-0.134578549287333,-6.76804156042465,
20.1908455371464));
#188094=CARTESIAN_POINT('Ctrl Pts',(0.0450703118637604,-6.76923106028667,
20.199269784583));
#188095=CARTESIAN_POINT('Ctrl Pts',(0.224502763877788,-6.76327491005735,
20.2076940320197));
#188096=CARTESIAN_POINT('Ctrl Pts',(0.275059963663833,-6.76159669480855,
20.2100676626307));
#188097=CARTESIAN_POINT('Ctrl Pts',(0.325599975128035,-6.75935150617513,
20.2124412932416));
#188098=CARTESIAN_POINT('Ctrl Pts',(0.376109601451067,-6.75653983690589,
20.2148149238526));
#188099=CARTESIAN_POINT('Ctrl Pts',(0.559512782420949,-6.74633051394407,
20.2234337047898));
#188100=CARTESIAN_POINT('Ctrl Pts',(0.742433063246356,-6.72865299871907,
20.232052485727));
#188101=CARTESIAN_POINT('Ctrl Pts',(0.92425870073124,-6.70358373216316,
20.2406712666643));
#188102=CARTESIAN_POINT('Ctrl Pts',(1.10619355977141,-6.67849940665122,
20.2492952248508));
#188103=CARTESIAN_POINT('Ctrl Pts',(1.28703216188696,-6.64601451010209,
20.2579191830374));
#188104=CARTESIAN_POINT('Ctrl Pts',(1.46617172243524,-6.60625684335171,
20.2665431412239));
#188105=CARTESIAN_POINT('Ctrl Pts',(1.65178298408685,-6.56506286775372,
20.2754786535951));
#188106=CARTESIAN_POINT('Ctrl Pts',(1.83556980291674,-6.51606092819704,
20.2844141659662));
#188107=CARTESIAN_POINT('Ctrl Pts',(2.01687810760223,-6.45944979847935,
20.2933496783373));
#188108=CARTESIAN_POINT('Ctrl Pts',(2.19219190446229,-6.40471037486297,
20.301989760232));
#188109=CARTESIAN_POINT('Ctrl Pts',(2.36518818459376,-6.34285701194278,
20.3106298421267));
#188110=CARTESIAN_POINT('Ctrl Pts',(2.53529492169012,-6.27411895488541,
20.3192699240214));
#188111=CARTESIAN_POINT('Ctrl Pts',(2.71412635289166,-6.20185535538658,
20.3283531516307));
#188112=CARTESIAN_POINT('Ctrl Pts',(2.88976369075558,-6.12198244898684,
20.3374363792401));
#188113=CARTESIAN_POINT('Ctrl Pts',(3.06156991882546,-6.03482217071415,
20.3465196068494));
#188114=CARTESIAN_POINT('Ctrl Pts',(3.23337614689534,-5.94766189244147,
20.3556028344587));
#188115=CARTESIAN_POINT('Ctrl Pts',(3.40135094365678,-5.85321446168417,
20.3646860620681));
#188116=CARTESIAN_POINT('Ctrl Pts',(3.56489050922797,-5.7518557576852,20.3737692896774));
#188117=CARTESIAN_POINT('Ctrl Pts',(3.72773450893392,-5.65092815214488,
20.3828138845372));
#188118=CARTESIAN_POINT('Ctrl Pts',(3.88633176894871,-5.54305547919057,
20.391858479397));
#188119=CARTESIAN_POINT('Ctrl Pts',(4.04011840715542,-5.42860315883966,
20.4009030742569));
#188120=CARTESIAN_POINT('Ctrl Pts',(4.19376392191441,-5.31425586650832,
20.4099393692772));
#188121=CARTESIAN_POINT('Ctrl Pts',(4.34260743776402,-5.19334112330998,
20.4189756642976));
#188122=CARTESIAN_POINT('Ctrl Pts',(4.48611524534255,-5.06626677204282,
20.4280119593179));
#188123=CARTESIAN_POINT('Ctrl Pts',(4.62936910460195,-4.93941728880516,
20.4370322639056));
#188124=CARTESIAN_POINT('Ctrl Pts',(4.76730593209654,-4.80643012073239,
20.4460525684933));
#188125=CARTESIAN_POINT('Ctrl Pts',(4.89942631473796,-4.66775221990769,
20.455072873081));
#188126=CARTESIAN_POINT('Ctrl Pts',(5.03138031742258,-4.52924895696012,
20.4640818183473));
#188127=CARTESIAN_POINT('Ctrl Pts',(5.15753232919754,-4.38506943460008,
20.4730907636137));
#188128=CARTESIAN_POINT('Ctrl Pts',(5.27741906373368,-4.23569793844419,
20.48209970888));
#188129=CARTESIAN_POINT('Ctrl Pts',(5.39703356087553,-4.08666563333435,
20.4910881967388));
#188130=CARTESIAN_POINT('Ctrl Pts',(5.51041103070356,-3.93246507321833,
20.5000766845976));
#188131=CARTESIAN_POINT('Ctrl Pts',(5.61712811593769,-3.77361374933131,
20.5090651724564));
#188132=CARTESIAN_POINT('Ctrl Pts',(5.71075767081434,-3.63424357524459,
20.5169513334716));
#188133=CARTESIAN_POINT('Ctrl Pts',(5.79926076377863,-3.49129401593223,
20.5248374944869));
#188134=CARTESIAN_POINT('Ctrl Pts',(5.88237643834799,-3.34513623602514,
20.5327236555021));
#188135=CARTESIAN_POINT('Ctrl Pts',(5.9679720822497,-3.19461746387762,20.5408451203583));
#188136=CARTESIAN_POINT('Ctrl Pts',(6.04781427862262,-3.04076273422171,
20.5489665852145));
#188137=CARTESIAN_POINT('Ctrl Pts',(6.12164141212632,-2.88405884498567,
20.5570880500707));
#188138=CARTESIAN_POINT('Ctrl Pts',(6.19546328066884,-2.72736613104327,
20.5652089357469));
#188139=CARTESIAN_POINT('Ctrl Pts',(6.26327078470796,-2.56782499350459,
20.5733298214231));
#188140=CARTESIAN_POINT('Ctrl Pts',(6.32484930615309,-2.40594477377492,
20.5814507070993));
#188141=CARTESIAN_POINT('Ctrl Pts',(6.38643518799235,-2.24404520473005,
20.5895725634535));
#188142=CARTESIAN_POINT('Ctrl Pts',(6.44179047561554,-2.07980633945318,
20.5976944198078));
#188143=CARTESIAN_POINT('Ctrl Pts',(6.49074954730195,-1.91375529109643,
20.605816276162));
#188144=CARTESIAN_POINT('Ctrl Pts',(6.53974433892135,-1.74758309394911,
20.6139440581222));
#188145=CARTESIAN_POINT('Ctrl Pts',(6.58233349046603,-1.57959642463423,
20.6220718400824));
#188146=CARTESIAN_POINT('Ctrl Pts',(6.61840174449271,-1.41033589917293,
20.6301996220426));
#188147=CARTESIAN_POINT('Ctrl Pts',(6.65448469138549,-1.24100642326463,
20.638330714959));
#188148=CARTESIAN_POINT('Ctrl Pts',(6.68404138340067,-1.07040241741154,
20.6464618078755));
#188149=CARTESIAN_POINT('Ctrl Pts',(6.70700815262058,-0.899072099823535,
20.6545929007919));
#188150=CARTESIAN_POINT('Ctrl Pts',(6.72999998910926,-0.727554782354139,
20.6627328684565));
#188151=CARTESIAN_POINT('Ctrl Pts',(6.74638750209217,-0.555309933885106,
20.670872836121));
#188152=CARTESIAN_POINT('Ctrl Pts',(6.75615904125024,-0.382889030049986,
20.6790128037856));
#188153=CARTESIAN_POINT('Ctrl Pts',(6.76122698395185,-0.293464094319782,
20.683234542966));
#188154=CARTESIAN_POINT('Ctrl Pts',(6.76451614724316,-0.203991791134683,
20.6874562821465));
#188155=CARTESIAN_POINT('Ctrl Pts',(6.76603041614926,-0.114548713406617,
20.6916780213269));
#188156=CARTESIAN_POINT('Ctrl Pts',(6.76905778145923,0.0642681860494812,
20.7001182307845));
#188157=CARTESIAN_POINT('Ctrl Pts',(6.76499423030045,0.243337685477338,
20.7085584402422));
#188158=CARTESIAN_POINT('Ctrl Pts',(6.75382433733469,0.422073240594176,
20.7169986496998));
#188159=CARTESIAN_POINT('Ctrl Pts',(6.74266290721768,0.600673377048167,
20.7254324644483));
#188160=CARTESIAN_POINT('Ctrl Pts',(6.72440588887434,0.77893974191567,20.7338662791969));
#188161=CARTESIAN_POINT('Ctrl Pts',(6.69908991008622,0.956286241969934,
20.7423000939454));
#188162=CARTESIAN_POINT('Ctrl Pts',(6.67378922015581,1.1335256387032,20.7507288153339));
#188163=CARTESIAN_POINT('Ctrl Pts',(6.64143811580303,1.30984594883357,20.7591575367225));
#188164=CARTESIAN_POINT('Ctrl Pts',(6.60212504588006,1.48466625157417,20.767586258111));
#188165=CARTESIAN_POINT('Ctrl Pts',(6.56282968112112,1.65940782166567,20.7760111835128));
#188166=CARTESIAN_POINT('Ctrl Pts',(6.51657867549774,1.83265040651704,20.7844361089145));
#188167=CARTESIAN_POINT('Ctrl Pts',(6.46351163328897,2.00382293787105,20.7928610343162));
#188168=CARTESIAN_POINT('Ctrl Pts',(6.41046034847175,2.1749446423373,20.8012834580739));
#188169=CARTESIAN_POINT('Ctrl Pts',(6.35059716183571,2.34399720090213,20.8097058818317));
#188170=CARTESIAN_POINT('Ctrl Pts',(6.2841117396454,2.51042399678836,20.8181283055894));
#188171=CARTESIAN_POINT('Ctrl Pts',(6.2176252718308,2.67685341008899,20.8265508618076));
#188172=CARTESIAN_POINT('Ctrl Pts',(6.14451647787865,2.84065666612478,20.8349734180258));
#188173=CARTESIAN_POINT('Ctrl Pts',(6.06502369189752,3.00129582292745,20.843395974244));
#188174=CARTESIAN_POINT('Ctrl Pts',(5.98552822063503,3.16194040615128,20.8518188149777));
#188175=CARTESIAN_POINT('Ctrl Pts',(5.89964847514893,3.31942037797676,20.8602416557115));
#188176=CARTESIAN_POINT('Ctrl Pts',(5.80766947296926,3.47322102561023,20.8686644964452));
#188177=CARTESIAN_POINT('Ctrl Pts',(5.71567452243535,3.62704834093037,20.8770887976259));
#188178=CARTESIAN_POINT('Ctrl Pts',(5.61757837795056,3.77719477387768,20.8855130988065));
#188179=CARTESIAN_POINT('Ctrl Pts',(5.51371042578661,3.92317299396446,20.8939373999871));
#188180=CARTESIAN_POINT('Ctrl Pts',(5.40980995826953,4.06919691181726,20.9023643383539));
#188181=CARTESIAN_POINT('Ctrl Pts',(5.30013427404017,4.21104974363724,20.9107912767208));
#188182=CARTESIAN_POINT('Ctrl Pts',(5.1850544373151,4.34827546069462,20.9192182150876));
#188183=CARTESIAN_POINT('Ctrl Pts',(5.0698711293515,4.48562456092064,20.9276527303312));
#188184=CARTESIAN_POINT('Ctrl Pts',(4.94927417435992,4.61833797749989,20.9360872455749));
#188185=CARTESIAN_POINT('Ctrl Pts',(4.82367382787709,4.74599407945834,20.9445217608185));
#188186=CARTESIAN_POINT('Ctrl Pts',(4.69801281535095,4.8737118404076,20.9529603500053));
#188187=CARTESIAN_POINT('Ctrl Pts',(4.56734383109422,4.99636718310635,20.9613989391921));
#188188=CARTESIAN_POINT('Ctrl Pts',(4.43211230911361,5.113576975015,20.9698375283789));
#188189=CARTESIAN_POINT('Ctrl Pts',(4.29672962888685,5.23091778095292,20.9782855499991));
#188190=CARTESIAN_POINT('Ctrl Pts',(4.15677447785778,5.34280066117938,20.9867335716194));
#188191=CARTESIAN_POINT('Ctrl Pts',(4.01272448631571,5.44888348167974,20.9951815932397));
#188192=CARTESIAN_POINT('Ctrl Pts',(3.93084878288709,5.50917925439849,20.999983313152));
#188193=CARTESIAN_POINT('Ctrl Pts',(3.84765073651829,5.56760204548384,21.0047850330642));
#188194=CARTESIAN_POINT('Ctrl Pts',(3.76322193724153,5.62409545180949,21.0095867529764));
#188195=CARTESIAN_POINT('Ctrl Pts',(3.61833740143535,5.72104129282245,21.0178267725729));
#188196=CARTESIAN_POINT('Ctrl Pts',(3.46950353234122,5.81251924285318,21.0260667921695));
#188197=CARTESIAN_POINT('Ctrl Pts',(3.3171691651141,5.89819275117525,21.034306811766));
#188198=CARTESIAN_POINT('Ctrl Pts',(3.24524477833348,5.93864333800981,21.0381973216183));
#188199=CARTESIAN_POINT('Ctrl Pts',(3.17254053868331,5.97780054540071,21.0420878314706));
#188200=CARTESIAN_POINT('Ctrl Pts',(3.09910619832133,6.01563211736941,21.0459783413229));
#188201=CARTESIAN_POINT('Ctrl Pts',(3.09910619832135,6.0156321173694,19.0455979788775));
#188202=CARTESIAN_POINT('Ctrl Pts',(2.93087086387512,6.10230283751758,19.0545209146099));
#188203=CARTESIAN_POINT('Ctrl Pts',(2.75912628990419,6.18184612462039,19.0634438503423));
#188204=CARTESIAN_POINT('Ctrl Pts',(2.58447961075416,6.25401903911365,19.0723667860748));
#188205=CARTESIAN_POINT('Ctrl Pts',(2.40953089484065,6.32631677060092,19.0813051532751));
#188206=CARTESIAN_POINT('Ctrl Pts',(2.23167027991639,6.39121854946046,19.0902435204755));
#188207=CARTESIAN_POINT('Ctrl Pts',(2.05152271824015,6.44853033927457,19.0991818876758));
#188208=CARTESIAN_POINT('Ctrl Pts',(2.03168758008735,6.45484065098886,19.1001660461436));
#188209=CARTESIAN_POINT('Ctrl Pts',(2.01182472940436,6.46105899903421,19.1011502046114));
#188210=CARTESIAN_POINT('Ctrl Pts',(1.99193500915975,6.4671851619761,19.1021343630793));
#188211=CARTESIAN_POINT('Ctrl Pts',(1.82575478240771,6.51836975051142,19.1103570869451));
#188212=CARTESIAN_POINT('Ctrl Pts',(1.65737931666312,6.56321309957973,19.118579810811));
#188213=CARTESIAN_POINT('Ctrl Pts',(1.48733340744237,6.60152469775778,19.1268025346769));
#188214=CARTESIAN_POINT('Ctrl Pts',(1.31746748605568,6.63979574440708,19.1350165550681));
#188215=CARTESIAN_POINT('Ctrl Pts',(1.14593498910629,6.67154872924817,19.1432305754594));
#188216=CARTESIAN_POINT('Ctrl Pts',(0.973277093441284,6.69664249451787,
19.1514445958506));
#188217=CARTESIAN_POINT('Ctrl Pts',(0.800767285486102,6.72171473700568,
19.1596515711225));
#188218=CARTESIAN_POINT('Ctrl Pts',(0.627134354172668,6.74013908371461,
19.1678585463945));
#188219=CARTESIAN_POINT('Ctrl Pts',(0.452931017569774,6.75182512312954,
19.1760655216665));
#188220=CARTESIAN_POINT('Ctrl Pts',(0.27884212908225,6.7635034850498,19.1842671051195));
#188221=CARTESIAN_POINT('Ctrl Pts',(0.104183938388189,6.76845233367149,
19.1924686885725));
#188222=CARTESIAN_POINT('Ctrl Pts',(-0.0704842496347184,6.76663291235408,
19.2006702720255));
#188223=CARTESIAN_POINT('Ctrl Pts',(-0.245072735382784,6.76481432125091,
19.2088681130405));
#188224=CARTESIAN_POINT('Ctrl Pts',(-0.419670851407023,6.75623361679936,
19.2170659540556));
#188225=CARTESIAN_POINT('Ctrl Pts',(-0.593717726144586,6.74090411307428,
19.2252637950706));
#188226=CARTESIAN_POINT('Ctrl Pts',(-0.767749241788536,6.72557596213007,
19.2334609126517));
#188227=CARTESIAN_POINT('Ctrl Pts',(-0.941229255217668,6.70350022109188,
19.2416580302329));
#188228=CARTESIAN_POINT('Ctrl Pts',(-1.11360008529399,6.6747422309804,19.249855147814));
#188229=CARTESIAN_POINT('Ctrl Pts',(-1.28596899755269,6.64598456083362,
19.2580521741931));
#188230=CARTESIAN_POINT('Ctrl Pts',(-1.45722839692184,6.61054484768785,
19.2662492005722));
#188231=CARTESIAN_POINT('Ctrl Pts',(-1.62682901058059,6.56853989637982,
19.2744462269513));
#188232=CARTESIAN_POINT('Ctrl Pts',(-1.79645857578088,6.52652777464907,
19.2826446525974));
#188233=CARTESIAN_POINT('Ctrl Pts',(-1.96442844280939,6.47794826822932,
19.2908430782435));
#188234=CARTESIAN_POINT('Ctrl Pts',(-2.13020270807044,6.42296858333663,
19.2990415038897));
#188235=CARTESIAN_POINT('Ctrl Pts',(-2.2960354148162,6.36796951609646,19.3072428197803));
#188236=CARTESIAN_POINT('Ctrl Pts',(-2.45967063753727,6.30656588870649,
19.315444135671));
#188237=CARTESIAN_POINT('Ctrl Pts',(-2.6205906716912,6.23897375627155,19.3236454515617));
#188238=CARTESIAN_POINT('Ctrl Pts',(-2.78169396682649,6.17130464771249,
19.3318561073783));
#188239=CARTESIAN_POINT('Ctrl Pts',(-2.94007556466262,6.09743309322177,
19.3400667631949));
#188240=CARTESIAN_POINT('Ctrl Pts',(-3.09523972006855,6.0176224603501,19.3482774190115));
#188241=CARTESIAN_POINT('Ctrl Pts',(-3.25049530995233,5.93776479700593,
19.3564929131687));
#188242=CARTESIAN_POINT('Ctrl Pts',(-3.40252936611668,5.85196125513129,
19.3647084073258));
#188243=CARTESIAN_POINT('Ctrl Pts',(-3.55087366035497,5.76051952936515,
19.372923901483));
#188244=CARTESIAN_POINT('Ctrl Pts',(-3.69944811349518,5.66893593007904,
19.3811521421305));
#188245=CARTESIAN_POINT('Ctrl Pts',(-3.84432106669312,5.57169686530648,
19.389380382778));
#188246=CARTESIAN_POINT('Ctrl Pts',(-3.98505493432114,5.46915223507654,
19.3976086234255));
#188247=CARTESIAN_POINT('Ctrl Pts',(-4.11295955168128,5.37595553755833,
19.4050867805266));
#188248=CARTESIAN_POINT('Ctrl Pts',(-4.23744558640654,5.27837712711518,
19.4125649376277));
#188249=CARTESIAN_POINT('Ctrl Pts',(-4.35821077628466,5.17670627228127,
19.4200430947288));
#188250=CARTESIAN_POINT('Ctrl Pts',(-4.48683218786717,5.06842135277147,
19.4280077335734));
#188251=CARTESIAN_POINT('Ctrl Pts',(-4.61167523612472,4.95512057304004,
19.435972372418));
#188252=CARTESIAN_POINT('Ctrl Pts',(-4.73230501151206,4.83710432779963,
19.4439370112626));
#188253=CARTESIAN_POINT('Ctrl Pts',(-4.85278451605925,4.7192350976744,19.4518917284028));
#188254=CARTESIAN_POINT('Ctrl Pts',(-4.96906091709185,4.59666234869501,
19.459846445543));
#188255=CARTESIAN_POINT('Ctrl Pts',(-5.08072985480975,4.46972853118005,
19.4678011626832));
#188256=CARTESIAN_POINT('Ctrl Pts',(-5.1922852483202,4.34292377909727,19.4757477915218));
#188257=CARTESIAN_POINT('Ctrl Pts',(-5.29924224750309,4.21176706368885,
19.4836944203604));
#188258=CARTESIAN_POINT('Ctrl Pts',(-5.40123123878462,4.07663956037043,
19.4916410491989));
#188259=CARTESIAN_POINT('Ctrl Pts',(-5.50313979131656,3.9416186321565,19.4995814105288));
#188260=CARTESIAN_POINT('Ctrl Pts',(-5.60008790270674,3.80263345049269,
19.5075217718587));
#188261=CARTESIAN_POINT('Ctrl Pts',(-5.69174453248446,3.66010015941276,
19.5154621331886));
#188262=CARTESIAN_POINT('Ctrl Pts',(-5.78335296646968,3.51764181659285,
19.5233983192394));
#188263=CARTESIAN_POINT('Ctrl Pts',(-5.86967524803693,3.37163939676288,
19.5313345052903));
#188264=CARTESIAN_POINT('Ctrl Pts',(-5.95042229290487,3.22253992001663,
19.5392706913411));
#188265=CARTESIAN_POINT('Ctrl Pts',(-6.03114767276121,3.07348044772997,
19.5472047480563));
#188266=CARTESIAN_POINT('Ctrl Pts',(-6.10630060867933,2.9213259069648,19.5551388047715));
#188267=CARTESIAN_POINT('Ctrl Pts',(-6.17563692211747,2.76654976571532,
19.5630728614866));
#188268=CARTESIAN_POINT('Ctrl Pts',(-6.24496888588621,2.61178333402511,
19.5710064204752));
#188269=CARTESIAN_POINT('Ctrl Pts',(-6.30848479697542,2.45439597819545,
19.5789399794639));
#188270=CARTESIAN_POINT('Ctrl Pts',(-6.36598788997289,2.29488282592349,
19.5868735384525));
#188271=CARTESIAN_POINT('Ctrl Pts',(-6.42349919835585,2.13534688423325,
19.5948082308975));
#188272=CARTESIAN_POINT('Ctrl Pts',(-6.47499585125896,1.9736849021302,19.6027429233424));
#188273=CARTESIAN_POINT('Ctrl Pts',(-6.52033047943041,1.81040863868101,
19.6106776157874));
#188274=CARTESIAN_POINT('Ctrl Pts',(-6.56570281025044,1.64699658614895,
19.6186189071377));
#188275=CARTESIAN_POINT('Ctrl Pts',(-6.60490278171912,1.48196794055604,
19.626560198488));
#188276=CARTESIAN_POINT('Ctrl Pts',(-6.63783372887719,1.31584664295669,
19.6345014898384));
#188277=CARTESIAN_POINT('Ctrl Pts',(-6.67077947895482,1.14965067151956,
19.6424463509098));
#188278=CARTESIAN_POINT('Ctrl Pts',(-6.69745053486376,0.982361447262679,
19.6503912119812));
#188279=CARTESIAN_POINT('Ctrl Pts',(-6.71780204686565,0.81450884533425,
19.6583360730526));
#188280=CARTESIAN_POINT('Ctrl Pts',(-6.7381790135413,0.646446301597885,
19.6662908711669));
#188281=CARTESIAN_POINT('Ctrl Pts',(-6.75222062424673,0.477819353365059,
19.6742456692812));
#188282=CARTESIAN_POINT('Ctrl Pts',(-6.75993413374877,0.309159355961101,
19.6822004673955));
#188283=CARTESIAN_POINT('Ctrl Pts',(-6.76477578602296,0.20329404785716,
19.6871935728516));
#188284=CARTESIAN_POINT('Ctrl Pts',(-6.76712528464591,0.0974156878556726,
19.6921866783078));
#188285=CARTESIAN_POINT('Ctrl Pts',(-6.76699485396139,-0.0083454454691123,
19.6971797837639));
#188286=CARTESIAN_POINT('',(-6.767,1.11697001474453E-12,19.3028202161899));
#188287=CARTESIAN_POINT('Ctrl Pts',(3.09910619832135,6.0156321173694,18.651395695404));
#188288=CARTESIAN_POINT('Ctrl Pts',(2.93375330764827,6.10081787314653,18.6601451433063));
#188289=CARTESIAN_POINT('Ctrl Pts',(2.76488627843071,6.17918207037039,18.6688945912086));
#188290=CARTESIAN_POINT('Ctrl Pts',(2.59307866646703,6.25045854553997,18.6776440391109));
#188291=CARTESIAN_POINT('Ctrl Pts',(2.42127244185377,6.32173444515037,18.6863934163612));
#188292=CARTESIAN_POINT('Ctrl Pts',(2.24652594672465,6.38592262741838,18.6951427936115));
#188293=CARTESIAN_POINT('Ctrl Pts',(2.06943269687121,6.44280508110562,18.7038921708618));
#188294=CARTESIAN_POINT('Ctrl Pts',(1.89234081822076,6.49968709436167,18.7126414803672));
#188295=CARTESIAN_POINT('Ctrl Pts',(1.71290249405587,6.54926340459545,18.7213907898725));
#188296=CARTESIAN_POINT('Ctrl Pts',(1.53172716625056,6.59136563150384,18.7301400993779));
#188297=CARTESIAN_POINT('Ctrl Pts',(1.35055318107333,6.6334675464071,18.7388893440451));
#188298=CARTESIAN_POINT('Ctrl Pts',(1.1676424971442,6.66809542395776,18.7476385887124));
#188299=CARTESIAN_POINT('Ctrl Pts',(0.983616340614383,6.69513165624668,
18.7563878333796));
#188300=CARTESIAN_POINT('Ctrl Pts',(0.799591486713904,6.7221676971596,18.7651370161153));
#188301=CARTESIAN_POINT('Ctrl Pts',(0.61445145952681,6.7416121586937,18.773886198851));
#188302=CARTESIAN_POINT('Ctrl Pts',(0.428825047910416,6.75339900185711,
18.7826353815867));
#188303=CARTESIAN_POINT('Ctrl Pts',(0.243199888597155,6.7651857655022,18.7913845052972));
#188304=CARTESIAN_POINT('Ctrl Pts',(0.0570886373920018,6.76931499599834,
18.8001336290078));
#188305=CARTESIAN_POINT('Ctrl Pts',(-0.128876626811089,6.76577266947847,
18.8088827527183));
#188306=CARTESIAN_POINT('Ctrl Pts',(-0.314840698188165,6.76223036567993,
18.8176318203099));
#188307=CARTESIAN_POINT('Ctrl Pts',(-0.500658497951326,6.75101660879223,
18.8263808879014));
#188308=CARTESIAN_POINT('Ctrl Pts',(-0.685698951926357,6.73216948296217,
18.8351299554929));
#188309=CARTESIAN_POINT('Ctrl Pts',(-0.870738280459992,6.71332247176291,
18.8438789698715));
#188310=CARTESIAN_POINT('Ctrl Pts',(-1.05499998761265,6.68684221356184,
18.85262798425));
#188311=CARTESIAN_POINT('Ctrl Pts',(-1.23785829161434,6.6528186394852,18.8613769986285));
#188312=CARTESIAN_POINT('Ctrl Pts',(-1.43007412917417,6.61705395368858,
18.8705737323277));
#188313=CARTESIAN_POINT('Ctrl Pts',(-1.62073882535804,6.57295372727787,
18.8797704660269));
#188314=CARTESIAN_POINT('Ctrl Pts',(-1.80913696091525,6.52068343478276,
18.8889671997261));
#188315=CARTESIAN_POINT('Ctrl Pts',(-1.98838356186127,6.47095219815194,
18.8977171974398));
#188316=CARTESIAN_POINT('Ctrl Pts',(-2.16557827572552,6.41382586850884,
18.9064671951534));
#188317=CARTESIAN_POINT('Ctrl Pts',(-2.34011918621723,6.34949849943269,
18.9152171928671));
#188318=CARTESIAN_POINT('Ctrl Pts',(-2.51465655691125,6.2851724349554,18.9239670131254));
#188319=CARTESIAN_POINT('Ctrl Pts',(-2.68653996295358,6.21364572242362,
18.9327168333837));
#188320=CARTESIAN_POINT('Ctrl Pts',(-2.85518555380022,6.13516132252206,
18.941466653642));
#188321=CARTESIAN_POINT('Ctrl Pts',(-3.02382794858724,6.05667841000489,
18.9502163080796));
#188322=CARTESIAN_POINT('Ctrl Pts',(-3.18923239109318,5.97123819492061,
18.9589659625171));
#188323=CARTESIAN_POINT('Ctrl Pts',(-3.35083705967737,5.87913088810691,
18.9677156169546));
#188324=CARTESIAN_POINT('Ctrl Pts',(-3.51243888042435,5.78702520443082,
18.9764651172035));
#188325=CARTESIAN_POINT('Ctrl Pts',(-3.67024081223721,5.68825280605763,
18.9852146174525));
#188326=CARTESIAN_POINT('Ctrl Pts',(-3.82370687544429,5.58314917682486,
18.9939641177014));
#188327=CARTESIAN_POINT('Ctrl Pts',(-3.97717043817844,5.47804726008001,
19.0027134753919));
#188328=CARTESIAN_POINT('Ctrl Pts',(-4.1262980372249,5.36661448084213,19.0114628330823));
#188329=CARTESIAN_POINT('Ctrl Pts',(-4.27058317206938,5.24922931204552,
19.0202121907728));
#188330=CARTESIAN_POINT('Ctrl Pts',(-4.41486614774846,5.1318458998678,19.0289614175329));
#188331=CARTESIAN_POINT('Ctrl Pts',(-4.55430658194406,5.0085104572304,19.0377106442929));
#188332=CARTESIAN_POINT('Ctrl Pts',(-4.68843089001821,4.87964187103142,
19.046459871053));
#188333=CARTESIAN_POINT('Ctrl Pts',(-4.82255336917803,4.75077504207994,
19.0552089785089));
#188334=CARTESIAN_POINT('Ctrl Pts',(-4.95135966065092,4.61637541908138,
19.0639580859648));
#188335=CARTESIAN_POINT('Ctrl Pts',(-5.07441230869194,4.47689945401902,
19.0727071934207));
#188336=CARTESIAN_POINT('Ctrl Pts',(-5.19746344226353,4.33742520555592,
19.0814561931971));
#188337=CARTESIAN_POINT('Ctrl Pts',(-5.31476088454691,4.19287495491432,
19.0902051929734));
#188338=CARTESIAN_POINT('Ctrl Pts',(-5.42590627628767,4.04373961586823,
19.0989541927498));
#188339=CARTESIAN_POINT('Ctrl Pts',(-5.53706380672587,3.89458798906849,
19.1077041480445));
#188340=CARTESIAN_POINT('Ctrl Pts',(-5.64206777071789,3.74085050155397,
19.1164541033392));
#188341=CARTESIAN_POINT('Ctrl Pts',(-5.74056148163939,3.58304938223271,
19.1252040586339));
#188342=CARTESIAN_POINT('Ctrl Pts',(-5.8390513895182,3.42525435593392,19.133953676075));
#188343=CARTESIAN_POINT('Ctrl Pts',(-5.93103139557593,3.26339625497292,
19.1427032935161));
#188344=CARTESIAN_POINT('Ctrl Pts',(-6.01618907820791,3.09802485065112,
19.1514529109572));
#188345=CARTESIAN_POINT('Ctrl Pts',(-6.10134392544933,2.93265895249744,
19.1602022370731));
#188346=CARTESIAN_POINT('Ctrl Pts',(-6.17967677261787,2.76378023986136,
19.168951563189));
#188347=CARTESIAN_POINT('Ctrl Pts',(-6.25092157009184,2.59196229227213,
19.1777008893048));
#188348=CARTESIAN_POINT('Ctrl Pts',(-6.3221643740772,2.42014915229179,19.1864499706073));
#188349=CARTESIAN_POINT('Ctrl Pts',(-6.38631941548894,2.24539720662929,
19.1951990519098));
#188350=CARTESIAN_POINT('Ctrl Pts',(-6.44316881037515,2.06829994947755,
19.2039481332122));
#188351=CARTESIAN_POINT('Ctrl Pts',(-6.50002334524552,1.89118668024518,
19.2126980055546));
#188352=CARTESIAN_POINT('Ctrl Pts',(-6.54957082411079,1.71172794807769,
19.2214478778969));
#188353=CARTESIAN_POINT('Ctrl Pts',(-6.59164294296068,1.53053334250405,
19.2301977502393));
#188354=CARTESIAN_POINT('Ctrl Pts',(-6.63371214082121,1.34935131693663,
19.2389470150942));
#188355=CARTESIAN_POINT('Ctrl Pts',(-6.66830695239679,1.16643393829825,
19.2476962799491));
#188356=CARTESIAN_POINT('Ctrl Pts',(-6.6953098815398,0.98240245834158,19.256445544804));
#188357=CARTESIAN_POINT('Ctrl Pts',(-6.72231419690476,0.798361530947684,
19.265195258811));
#188358=CARTESIAN_POINT('Ctrl Pts',(-6.74172580829272,0.613206671363136,
19.273944972818));
#188359=CARTESIAN_POINT('Ctrl Pts',(-6.75347878028175,0.427566795114092,
19.2826946868251));
#188360=CARTESIAN_POINT('Ctrl Pts',(-6.76248992368215,0.285234494205629,
19.2894031966133));
#188361=CARTESIAN_POINT('Ctrl Pts',(-6.76699999999998,0.142617266092147,
19.2961117064016));
#188362=CARTESIAN_POINT('Ctrl Pts',(-6.767,1.11697004507078E-12,19.3028202161899));
#188363=CARTESIAN_POINT('Ctrl Pts',(-6.7669994896834,-0.00262804578583102,
19.3028202161899));
#188364=CARTESIAN_POINT('Ctrl Pts',(-6.76692411827146,-0.196703167631038,
19.3119234788422));
#188365=CARTESIAN_POINT('Ctrl Pts',(-6.75849556223852,-0.390555835714825,
19.3210267414945));
#188366=CARTESIAN_POINT('Ctrl Pts',(-6.74179607552328,-0.583502078881353,
19.3301300041467));
#188367=CARTESIAN_POINT('Ctrl Pts',(-6.7242794658459,-0.785889379036061,
19.3396786987497));
#188368=CARTESIAN_POINT('Ctrl Pts',(-6.69766236172528,-0.987279027706483,
19.3492273933527));
#188369=CARTESIAN_POINT('Ctrl Pts',(-6.66209914580194,-1.18689678216142,
19.3587760879557));
#188370=CARTESIAN_POINT('Ctrl Pts',(-6.6279912981864,-1.37834549605109,
19.3679340173497));
#188371=CARTESIAN_POINT('Ctrl Pts',(-6.58565503867919,-1.56816428165398,
19.3770919467436));
#188372=CARTESIAN_POINT('Ctrl Pts',(-6.53527762040866,-1.75568659623117,
19.3862498761375));
#188373=CARTESIAN_POINT('Ctrl Pts',(-6.48482247995173,-1.94349821988346,
19.3954219343677));
#188374=CARTESIAN_POINT('Ctrl Pts',(-6.42630144353643,-2.1290060880081,
19.4045939925979));
#188375=CARTESIAN_POINT('Ctrl Pts',(-6.35995131213566,-2.31155971310799,
19.4137660508281));
#188376=CARTESIAN_POINT('Ctrl Pts',(-6.29348779166628,-2.49442531325727,
19.4229537836488));
#188377=CARTESIAN_POINT('Ctrl Pts',(-6.21916849175762,-2.67432637534773,
19.4321415164695));
#188378=CARTESIAN_POINT('Ctrl Pts',(-6.13727880330701,-2.8506311389723,
19.4413292492902));
#188379=CARTESIAN_POINT('Ctrl Pts',(-6.12722177115829,-2.87228347041101,
19.4424576126544));
#188380=CARTESIAN_POINT('Ctrl Pts',(-6.11705061400901,-2.89388158903475,
19.4435859760186));
#188381=CARTESIAN_POINT('Ctrl Pts',(-6.10676590851729,-2.91542434965667,
19.4447143393827));
#188382=CARTESIAN_POINT('Ctrl Pts',(-6.03166496039581,-3.07273383694952,
19.4529538712336));
#188383=CARTESIAN_POINT('Ctrl Pts',(-5.95037766933127,-3.22735753787452,
19.4611934030844));
#188384=CARTESIAN_POINT('Ctrl Pts',(-5.86311817374967,-3.37877703920314,
19.4694329349352));
#188385=CARTESIAN_POINT('Ctrl Pts',(-5.77595553010974,-3.53002847546775,
19.4776633214816));
#188386=CARTESIAN_POINT('Ctrl Pts',(-5.68283405700541,-3.67808248794971,
19.4858937080279));
#188387=CARTESIAN_POINT('Ctrl Pts',(-5.58401543055536,-3.82244171588261,
19.4941240945742));
#188388=CARTESIAN_POINT('Ctrl Pts',(-5.48528885753931,-3.96666646752155,
19.502346814192));
#188389=CARTESIAN_POINT('Ctrl Pts',(-5.38087590025924,-4.10720299712672,
19.5105695338098));
#188390=CARTESIAN_POINT('Ctrl Pts',(-5.27108355841995,-4.24357951735971,
19.5187922534277));
#188391=CARTESIAN_POINT('Ctrl Pts',(-5.16138850050598,-4.37983519816995,
19.5270076871234));
#188392=CARTESIAN_POINT('Ctrl Pts',(-5.04632378049846,-4.51193794011583,
19.5352231208192));
#188393=CARTESIAN_POINT('Ctrl Pts',(-4.92623892718506,-4.63944598333536,
19.543438554515));
#188394=CARTESIAN_POINT('Ctrl Pts',(-4.80621578816163,-4.76688849732172,
19.5516497661158));
#188395=CARTESIAN_POINT('Ctrl Pts',(-4.68117789746008,-4.88974075689622,
19.5598609777166));
#188396=CARTESIAN_POINT('Ctrl Pts',(-4.55151444305599,-5.0075947594282,
19.5680721893174));
#188397=CARTESIAN_POINT('Ctrl Pts',(-4.42189447061963,-5.12540924023094,
19.576280647331));
#188398=CARTESIAN_POINT('Ctrl Pts',(-4.28765228761291,-5.23822856387882,
19.5844891053445));
#188399=CARTESIAN_POINT('Ctrl Pts',(-4.14921331450017,-5.34568217075936,
19.592697563358));
#188400=CARTESIAN_POINT('Ctrl Pts',(-4.08753572905468,-5.39355509895859,
19.5963546106412));
#188401=CARTESIAN_POINT('Ctrl Pts',(-4.02502558672144,-5.44036350152121,
19.6000116579243));
#188402=CARTESIAN_POINT('Ctrl Pts',(-3.96172264090319,-5.48607717012394,
19.6036687052075));
#188403=CARTESIAN_POINT('Ctrl Pts',(-3.8083733814779,-5.59681699645,19.6125277793834));
#188404=CARTESIAN_POINT('Ctrl Pts',(-3.65052916837581,-5.70101476812618,
19.6213868535593));
#188405=CARTESIAN_POINT('Ctrl Pts',(-3.48875881748808,-5.79834898168429,
19.6302459277351));
#188406=CARTESIAN_POINT('Ctrl Pts',(-3.32668453265651,-5.89586606664766,
19.6391216463291));
#188407=CARTESIAN_POINT('Ctrl Pts',(-3.16066959080951,-5.98649368944297,
19.6479973649231));
#188408=CARTESIAN_POINT('Ctrl Pts',(-2.99130644250467,-6.06995673518602,
19.656873083517));
#188409=CARTESIAN_POINT('Ctrl Pts',(-2.82145997962814,-6.15365796087912,
19.665774130904));
#188410=CARTESIAN_POINT('Ctrl Pts',(-2.64824642373677,-6.23015357956474,
19.674675178291));
#188411=CARTESIAN_POINT('Ctrl Pts',(-2.4722800904021,-6.29921583648325,
19.683576225678));
#188412=CARTESIAN_POINT('Ctrl Pts',(-2.29607452842366,-6.36837198448732,
19.692489374161));
#188413=CARTESIAN_POINT('Ctrl Pts',(-2.11710895690211,-6.43007449522048,
19.701402522644));
#188414=CARTESIAN_POINT('Ctrl Pts',(-1.93601317239168,-6.4841454330024,
19.710315671127));
#188415=CARTESIAN_POINT('Ctrl Pts',(-1.75451530572022,-6.53833642305153,
19.7192486092369));
#188416=CARTESIAN_POINT('Ctrl Pts',(-1.57087801530508,-6.58486187421657,
19.7281815473467));
#188417=CARTESIAN_POINT('Ctrl Pts',(-1.38574443851102,-6.62359429246205,
19.7371144854566));
#188418=CARTESIAN_POINT('Ctrl Pts',(-1.20952411665315,-6.66046193866512,
19.7456173473152));
#188419=CARTESIAN_POINT('Ctrl Pts',(-1.03194837503492,-6.69026924440987,
19.7541202091737));
#188420=CARTESIAN_POINT('Ctrl Pts',(-0.853576295393243,-6.71294991102591,
19.7626230710323));
#188421=CARTESIAN_POINT('Ctrl Pts',(-0.681080919051054,-6.73488333318191,
19.7708457948981));
#188422=CARTESIAN_POINT('Ctrl Pts',(-0.507510078536465,-6.75019302760903,
19.779068518764));
#188423=CARTESIAN_POINT('Ctrl Pts',(-0.333413462753453,-6.75878128532465,
19.7872912426299));
#188424=CARTESIAN_POINT('Ctrl Pts',(-0.159501122340489,-6.76736045266042,
19.7955052630211));
#188425=CARTESIAN_POINT('Ctrl Pts',(0.0149355298302086,-6.76923233283801,
19.8037192834123));
#188426=CARTESIAN_POINT('Ctrl Pts',(0.189339128267373,-6.76435064839981,
19.8119333038036));
#188427=CARTESIAN_POINT('Ctrl Pts',(0.363593141715594,-6.759473150955,19.8201402790755));
#188428=CARTESIAN_POINT('Ctrl Pts',(0.537813801340364,-6.74785363512641,
19.8283472543475));
#188429=CARTESIAN_POINT('Ctrl Pts',(0.711441072268215,-6.72949779706405,
19.8365542296195));
#188430=CARTESIAN_POINT('Ctrl Pts',(0.884954273543917,-6.71115401842099,
19.8447558130725));
#188431=CARTESIAN_POINT('Ctrl Pts',(1.05787450718939,-6.68608277044488,
19.8529573965254));
#188432=CARTESIAN_POINT('Ctrl Pts',(1.22964410578536,-6.65434176858292,
19.8611589799784));
#188433=CARTESIAN_POINT('Ctrl Pts',(1.40133532475278,-6.62261525035461,
19.8693568209935));
#188434=CARTESIAN_POINT('Ctrl Pts',(1.57187660265974,-6.58422510659389,
19.8775546620085));
#188435=CARTESIAN_POINT('Ctrl Pts',(1.74071765662254,-6.53928062097985,
19.8857525030236));
#188436=CARTESIAN_POINT('Ctrl Pts',(1.90954381088925,-6.4943401015764,19.8939496206047));
#188437=CARTESIAN_POINT('Ctrl Pts',(2.07666969147306,-6.44284647633123,
19.9021467381859));
#188438=CARTESIAN_POINT('Ctrl Pts',(2.24155707918389,-6.38495973838211,
19.910343855767));
#188439=CARTESIAN_POINT('Ctrl Pts',(2.40644263233884,-6.32707364448745,
19.9185408821461));
#188440=CARTESIAN_POINT('Ctrl Pts',(2.56908940329754,-6.26279469741363,
19.9267379085252));
#188441=CARTESIAN_POINT('Ctrl Pts',(2.72897628063101,-6.19233215030923,
19.9349349349043));
#188442=CARTESIAN_POINT('Ctrl Pts',(2.88889045133025,-6.12185757495022,
19.9431333605504));
#188443=CARTESIAN_POINT('Ctrl Pts',(3.04604346141292,-6.04519744127166,
19.9513317861966));
#188444=CARTESIAN_POINT('Ctrl Pts',(3.199936012489,-5.96260836513485,19.9595302118427));
#188445=CARTESIAN_POINT('Ctrl Pts',(3.35388281631086,-5.8799901733318,19.9677315277334));
#188446=CARTESIAN_POINT('Ctrl Pts',(3.50456655546273,-5.79143904501214,
19.975932843624));
#188447=CARTESIAN_POINT('Ctrl Pts',(3.65151423670819,-5.69725660112983,
19.9841341595147));
#188448=CARTESIAN_POINT('Ctrl Pts',(3.7986292667642,-5.60296689920965,19.9923448153313));
#188449=CARTESIAN_POINT('Ctrl Pts',(3.94199943627073,-5.50303326327248,
20.0005554711479));
#188450=CARTESIAN_POINT('Ctrl Pts',(4.08118149837881,-5.3978001609258,20.0087661269645));
#188451=CARTESIAN_POINT('Ctrl Pts',(4.22044557710406,-5.29250504726142,
20.0169816211216));
#188452=CARTESIAN_POINT('Ctrl Pts',(4.35551635177849,-5.18190446923081,
20.0251971152787));
#188453=CARTESIAN_POINT('Ctrl Pts',(4.48598528528534,-5.06638184705846,
20.0334126094359));
#188454=CARTESIAN_POINT('Ctrl Pts',(4.61665664374337,-4.95067998941199,
20.0416408500834));
#188455=CARTESIAN_POINT('Ctrl Pts',(4.74271163374992,-4.83004107454375,
20.0498690907309));
#188456=CARTESIAN_POINT('Ctrl Pts',(4.86377914350231,-4.70488484909375,
20.0580973313784));
#188457=CARTESIAN_POINT('Ctrl Pts',(4.97381018130919,-4.59113782148561,
20.0655754884795));
#188458=CARTESIAN_POINT('Ctrl Pts',(5.07972197530185,-4.47366011755974,
20.0730536455807));
#188459=CARTESIAN_POINT('Ctrl Pts',(5.18126633726378,-4.35278854785495,
20.0805318026818));
#188460=CARTESIAN_POINT('Ctrl Pts',(5.29083783267295,-4.22236201910318,
20.0886011119043));
#188461=CARTESIAN_POINT('Ctrl Pts',(5.39568211999948,-4.08755634077539,
20.0966704211268));
#188462=CARTESIAN_POINT('Ctrl Pts',(5.49541878552054,-3.94875440762628,
20.1047397303493));
#188463=CARTESIAN_POINT('Ctrl Pts',(5.59503105231212,-3.81012559821299,
20.1127989749501));
#188464=CARTESIAN_POINT('Ctrl Pts',(5.68954815809697,-3.66751075082367,
20.1208582195509));
#188465=CARTESIAN_POINT('Ctrl Pts',(5.77862738107788,-3.52132852637425,
20.1289174641516));
#188466=CARTESIAN_POINT('Ctrl Pts',(5.86761504634572,-3.37529655144108,
20.1369684252719));
#188467=CARTESIAN_POINT('Ctrl Pts',(5.95117575886275,-3.22570481206129,
20.1450193863922));
#188468=CARTESIAN_POINT('Ctrl Pts',(6.02900793362165,-3.073003796992,20.1530703475124));
#188469=CARTESIAN_POINT('Ctrl Pts',(6.1067771652212,-2.92042627178219,20.1611147977915));
#188470=CARTESIAN_POINT('Ctrl Pts',(6.17882691105941,-2.76474480628899,
20.1691592480706));
#188471=CARTESIAN_POINT('Ctrl Pts',(6.24489974717524,-2.60643744366341,
20.1772036983497));
#188472=CARTESIAN_POINT('Ctrl Pts',(6.31093361267745,-2.44822345276856,
20.185243403908));
#188473=CARTESIAN_POINT('Ctrl Pts',(6.37099744283874,-2.28738699139377,
20.1932831094662));
#188474=CARTESIAN_POINT('Ctrl Pts',(6.42488054552516,-2.12442909407031,
20.2013228150244));
#188475=CARTESIAN_POINT('Ctrl Pts',(6.47992668617561,-1.95795383765508,
20.2095360533289));
#188476=CARTESIAN_POINT('Ctrl Pts',(6.52852206974812,-1.78926487949218,
20.2177492916333));
#188477=CARTESIAN_POINT('Ctrl Pts',(6.57049450686606,-1.618916593047,20.2259625299378));
#188478=CARTESIAN_POINT('Ctrl Pts',(6.61156690710525,-1.45222117382998,
20.233999647486));
#188479=CARTESIAN_POINT('Ctrl Pts',(6.64629743937475,-1.28393724887201,
20.2420367650341));
#188480=CARTESIAN_POINT('Ctrl Pts',(6.67457569905664,-1.11459779183461,
20.2500738825823));
#188481=CARTESIAN_POINT('Ctrl Pts',(6.70285695039861,-0.945240419759346,
20.2581118504064));
#188482=CARTESIAN_POINT('Ctrl Pts',(6.72468450832059,-0.774827661776648,
20.2661498182305));
#188483=CARTESIAN_POINT('Ctrl Pts',(6.73999949411888,-0.603900504451883,
20.2741877860546));
#188484=CARTESIAN_POINT('Ctrl Pts',(6.75531913460856,-0.432921397149721,
20.2822281968624));
#188485=CARTESIAN_POINT('Ctrl Pts',(6.76412222974144,-0.261427951225687,
20.2902686076701));
#188486=CARTESIAN_POINT('Ctrl Pts',(6.76640196070452,-0.0899639159557847,
20.2983090184778));
#188487=CARTESIAN_POINT('Ctrl Pts',(6.76876785264016,0.0879804927781306,
20.3066533114656));
#188488=CARTESIAN_POINT('Ctrl Pts',(6.76410764778107,0.265892778929249,
20.3149976044534));
#188489=CARTESIAN_POINT('Ctrl Pts',(6.75247289523313,0.443169041271924,
20.3233418974412));
#188490=CARTESIAN_POINT('Ctrl Pts',(6.74124205795728,0.614290932093335,
20.3313965076568));
#188491=CARTESIAN_POINT('Ctrl Pts',(6.72351292290034,0.78481986124143,20.3394511178723));
#188492=CARTESIAN_POINT('Ctrl Pts',(6.69938426918256,0.954221889200478,
20.3475057280878));
#188493=CARTESIAN_POINT('Ctrl Pts',(6.67523734973306,1.12375215688774,20.3555664357571));
#188494=CARTESIAN_POINT('Ctrl Pts',(6.64468133183714,1.29215345978572,20.3636271434263));
#188495=CARTESIAN_POINT('Ctrl Pts',(6.60786535590953,1.45890521904977,20.3716878510956));
#188496=CARTESIAN_POINT('Ctrl Pts',(6.5709974716616,1.62589208830386,20.3797599238797));
#188497=CARTESIAN_POINT('Ctrl Pts',(6.52785211311753,1.79122441563057,20.3878319966639));
#188498=CARTESIAN_POINT('Ctrl Pts',(6.47862735450224,1.95439929428337,20.395904069448));
#188499=CARTESIAN_POINT('Ctrl Pts',(6.47347143503538,1.97149062305806,20.3967495577424));
#188500=CARTESIAN_POINT('Ctrl Pts',(6.46824886099491,1.98855830321337,20.3975950460369));
#188501=CARTESIAN_POINT('Ctrl Pts',(6.46295988947777,2.00560177178859,20.3984405343313));
#188502=CARTESIAN_POINT('Ctrl Pts',(6.41082497459428,2.17360414816904,20.4067747558567));
#188503=CARTESIAN_POINT('Ctrl Pts',(6.35206824183237,2.33978817453824,20.4151089773821));
#188504=CARTESIAN_POINT('Ctrl Pts',(6.28683273756299,2.50360203105571,20.4234431989075));
#188505=CARTESIAN_POINT('Ctrl Pts',(6.22167602151371,2.66721804128795,20.4317673547717));
#188506=CARTESIAN_POINT('Ctrl Pts',(6.1500562503023,2.82846926380757,20.440091510636));
#188507=CARTESIAN_POINT('Ctrl Pts',(6.07216642814117,2.98681835218604,20.4484156665002));
#188508=CARTESIAN_POINT('Ctrl Pts',(5.99305939178687,3.14764202264083,20.4568699071481));
#188509=CARTESIAN_POINT('Ctrl Pts',(5.90748478019005,3.30547174461127,20.4653241477961));
#188510=CARTESIAN_POINT('Ctrl Pts',(5.81569669955021,3.45976312756247,20.473778388444));
#188511=CARTESIAN_POINT('Ctrl Pts',(5.72550545878816,3.61137029888859,20.4820855504242));
#188512=CARTESIAN_POINT('Ctrl Pts',(5.62931534185075,3.75956091274163,20.4903927124045));
#188513=CARTESIAN_POINT('Ctrl Pts',(5.52741478724101,3.90384102773019,20.4986998743848));
#188514=CARTESIAN_POINT('Ctrl Pts',(5.42557323608984,4.04803760023145,20.5070022262707));
#188515=CARTESIAN_POINT('Ctrl Pts',(5.3180280348611,4.18832790165481,20.5153045781566));
#188516=CARTESIAN_POINT('Ctrl Pts',(5.20511163705089,4.32424581237439,20.5236069300425));
#188517=CARTESIAN_POINT('Ctrl Pts',(5.09224185037621,4.46010761708739,20.5319058547729));
#188518=CARTESIAN_POINT('Ctrl Pts',(4.9740055072949,4.59160036058793,20.5402047795033));
#188519=CARTESIAN_POINT('Ctrl Pts',(4.85077626894283,4.71828979490038,20.5485037042337));
#188520=CARTESIAN_POINT('Ctrl Pts',(4.72355437961419,4.84908399120271,20.5570715157184));
#188521=CARTESIAN_POINT('Ctrl Pts',(4.59101084937444,4.97475808421853,20.5656393272031));
#188522=CARTESIAN_POINT('Ctrl Pts',(4.45359967091374,5.09487379345524,20.5742071386878));
#188523=CARTESIAN_POINT('Ctrl Pts',(4.32052411644,5.21119958868343,20.5825046169332));
#188524=CARTESIAN_POINT('Ctrl Pts',(4.18288370146673,5.32231219823381,20.5908020951786));
#188525=CARTESIAN_POINT('Ctrl Pts',(4.04112586324388,5.42785323654034,20.5990995734239));
#188526=CARTESIAN_POINT('Ctrl Pts',(3.89244028363945,5.53855209206316,20.6078025515283));
#188527=CARTESIAN_POINT('Ctrl Pts',(3.73922506593886,5.64312087543043,20.6165055296326));
#188528=CARTESIAN_POINT('Ctrl Pts',(3.58203235262422,5.74119614930142,20.6252085077369));
#188529=CARTESIAN_POINT('Ctrl Pts',(3.42483963930957,5.83927142317241,20.6339114858412));
#188530=CARTESIAN_POINT('Ctrl Pts',(3.2636698169091,5.93085297522223,20.6426144639456));
#188531=CARTESIAN_POINT('Ctrl Pts',(3.09910619832131,6.01563211736942,20.6513174420499));
#188532=CARTESIAN_POINT('Origin',(0.,0.,4.30282021618968));
#188533=CARTESIAN_POINT('',(3.09910619832132,6.01563211736941,23.0457234660332));
#188534=CARTESIAN_POINT('',(3.09910619832133,6.01563211736941,22.651395695404));
#188535=CARTESIAN_POINT('',(3.09910619832133,6.0156321173694,4.30282021618968));
#188536=CARTESIAN_POINT('',(-6.76699496442947,0.0082553852872212,21.6971797838552));
#188537=CARTESIAN_POINT('Ctrl Pts',(-6.76699496442947,0.0082553852872167,
21.6971797838552));
#188538=CARTESIAN_POINT('Ctrl Pts',(-6.76720014876307,-0.159935595989462,
21.7051103156268));
#188539=CARTESIAN_POINT('Ctrl Pts',(-6.76113088550322,-0.328408545218613,
21.7130408473984));
#188540=CARTESIAN_POINT('Ctrl Pts',(-6.74875105755394,-0.496636852402841,
21.7209713791701));
#188541=CARTESIAN_POINT('Ctrl Pts',(-6.73638286209287,-0.664707086808642,
21.7288944591566));
#188542=CARTESIAN_POINT('Ctrl Pts',(-6.71771592388165,-0.83253275655728,
21.7368175391432));
#188543=CARTESIAN_POINT('Ctrl Pts',(-6.69276612089855,-0.999585239463147,
21.7447406191297));
#188544=CARTESIAN_POINT('Ctrl Pts',(-6.66783403685853,-1.16651908442071,
21.7526580722741));
#188545=CARTESIAN_POINT('Ctrl Pts',(-6.63662802108039,-1.33268045684481,
21.7605755254185));
#188546=CARTESIAN_POINT('Ctrl Pts',(-6.59921591081262,-1.49754411036121,
21.7684929785628));
#188547=CARTESIAN_POINT('Ctrl Pts',(-6.56085853100868,-1.66657327574465,
21.7766104772863));
#188548=CARTESIAN_POINT('Ctrl Pts',(-6.51597730961295,-1.8342378645121,
21.7847279760097));
#188549=CARTESIAN_POINT('Ctrl Pts',(-6.46470159579191,-1.999980569247,21.7928454747331));
#188550=CARTESIAN_POINT('Ctrl Pts',(-6.41471783401116,-2.16154719120139,
21.8007584435094));
#188551=CARTESIAN_POINT('Ctrl Pts',(-6.35865807491377,-2.32128723103019,
21.8086714122856));
#188552=CARTESIAN_POINT('Ctrl Pts',(-6.29669306076058,-2.47869834763523,
21.8165843810619));
#188553=CARTESIAN_POINT('Ctrl Pts',(-6.23472660831995,-2.63611311795413,
21.8244975335083));
#188554=CARTESIAN_POINT('Ctrl Pts',(-6.16685476853288,-2.79119849962973,
21.8324106859548));
#188555=CARTESIAN_POINT('Ctrl Pts',(-6.09329676179189,-2.94347134736121,
21.8403238384012));
#188556=CARTESIAN_POINT('Ctrl Pts',(-6.01972182361219,-3.0957792449602,
21.8482388122816));
#188557=CARTESIAN_POINT('Ctrl Pts',(-5.94045828250411,-3.24527297503472,
21.8561537861621));
#188558=CARTESIAN_POINT('Ctrl Pts',(-5.85577156912129,-3.39149352502268,
21.8640687600425));
#188559=CARTESIAN_POINT('Ctrl Pts',(-5.76728249953132,-3.54427924437017,
21.8723391090327));
#188560=CARTESIAN_POINT('Ctrl Pts',(-5.6728722352669,-3.69349064921928,
21.8806094580229));
#188561=CARTESIAN_POINT('Ctrl Pts',(-5.57289370828325,-3.83863839351624,
21.8888798070131));
#188562=CARTESIAN_POINT('Ctrl Pts',(-5.47705412758578,-3.97777726035392,
21.8968077771819));
#188563=CARTESIAN_POINT('Ctrl Pts',(-5.37609834351553,-4.11318190804607,
21.9047357473506));
#188564=CARTESIAN_POINT('Ctrl Pts',(-5.27037764387939,-4.2444562067356,
21.9126637175194));
#188565=CARTESIAN_POINT('Ctrl Pts',(-5.16458109587965,-4.37582468698817,
21.9205973755389));
#188566=CARTESIAN_POINT('Ctrl Pts',(-5.05401308107522,-4.50305663475895,
21.9285310335585));
#188567=CARTESIAN_POINT('Ctrl Pts',(-4.93906107671895,-4.62579341091232,
21.936464691578));
#188568=CARTESIAN_POINT('Ctrl Pts',(-4.82394961633868,-4.74870044175967,
21.9444093547955));
#188569=CARTESIAN_POINT('Ctrl Pts',(-4.70444230869804,-4.86709959820524,
21.952354018013));
#188570=CARTESIAN_POINT('Ctrl Pts',(-4.58095924754832,-4.98067278309884,
21.9602986812305));
#188571=CARTESIAN_POINT('Ctrl Pts',(-4.56534243794244,-4.99503629812918,
21.9613034367953));
#188572=CARTESIAN_POINT('Ctrl Pts',(-4.54966207515606,-5.00932268186436,
21.9623081923601));
#188573=CARTESIAN_POINT('Ctrl Pts',(-4.53391904016846,-5.02353134131737,
21.9633129479249));
#188574=CARTESIAN_POINT('Ctrl Pts',(-4.4033544651371,-5.14137060069203,
21.9716458699717));
#188575=CARTESIAN_POINT('Ctrl Pts',(-4.26802527448159,-5.25426780731966,
21.9799787920184));
#188576=CARTESIAN_POINT('Ctrl Pts',(-4.12833594852465,-5.36182163971529,
21.9883117140651));
#188577=CARTESIAN_POINT('Ctrl Pts',(-3.98881170147592,-5.46924836956314,
21.9966347886187));
#188578=CARTESIAN_POINT('Ctrl Pts',(-3.84493785689512,-5.57134409384086,
22.0049578631723));
#188579=CARTESIAN_POINT('Ctrl Pts',(-3.69715448022344,-5.66774538501543,
22.0132809377259));
#188580=CARTESIAN_POINT('Ctrl Pts',(-3.54951862117828,-5.76405044825161,
22.0215957041719));
#188581=CARTESIAN_POINT('Ctrl Pts',(-3.39798129469385,-5.85467221420411,
22.0299104706178));
#188582=CARTESIAN_POINT('Ctrl Pts',(-3.24301445245601,-5.93928836319314,
22.0382252370638));
#188583=CARTESIAN_POINT('Ctrl Pts',(-3.08817387225721,-6.02383556964355,
22.0465332289033));
#188584=CARTESIAN_POINT('Ctrl Pts',(-2.9299096481701,-6.10238674317606,
22.0548412207429));
#188585=CARTESIAN_POINT('Ctrl Pts',(-2.7687216283401,-6.17466351672395,
22.0631492125824));
#188586=CARTESIAN_POINT('Ctrl Pts',(-2.60763538818261,-6.24689465222535,
22.0714519584695));
#188587=CARTESIAN_POINT('Ctrl Pts',(-2.4436293481048,-6.31285914132132,
22.0797547043565));
#188588=CARTESIAN_POINT('Ctrl Pts',(-2.27722700900109,-6.3723250191336,
22.0880574502436));
#188589=CARTESIAN_POINT('Ctrl Pts',(-2.1108926732303,-6.43176659513673,
22.096356803063));
#188590=CARTESIAN_POINT('Ctrl Pts',(-1.94216431686134,-6.4847147347854,
22.1046561558825));
#188591=CARTESIAN_POINT('Ctrl Pts',(-1.7715846998492,-6.53098588662234,
22.1129555087019));
#188592=CARTESIAN_POINT('Ctrl Pts',(-1.60104136225905,-6.57724719736178,
22.1212530963882));
#188593=CARTESIAN_POINT('Ctrl Pts',(-1.42864788400555,-6.61683425838779,
22.1295506840746));
#188594=CARTESIAN_POINT('Ctrl Pts',(-1.2549616774216,-6.64961353675559,
22.137848271761));
#188595=CARTESIAN_POINT('Ctrl Pts',(-1.08128354863033,-6.68239129062573,
22.1461454735434));
#188596=CARTESIAN_POINT('Ctrl Pts',(-0.906313153192367,-6.70836182841414,
22.1544426753258));
#188597=CARTESIAN_POINT('Ctrl Pts',(-0.730617766375759,-6.72744280387846,
22.1627398771082));
#188598=CARTESIAN_POINT('Ctrl Pts',(-0.55490135587092,-6.74652606256995,
22.1710380717327));
#188599=CARTESIAN_POINT('Ctrl Pts',(-0.378460127035671,-6.75871807925165,
22.1793362663573));
#188600=CARTESIAN_POINT('Ctrl Pts',(-0.201866337928561,-6.7639883930719,
22.1876344609818));
#188601=CARTESIAN_POINT('Ctrl Pts',(-0.025148348350608,-6.7692624135653,
22.1959384918234));
#188602=CARTESIAN_POINT('Ctrl Pts',(0.151722067725539,-6.76760499335631,
22.204242522665));
#188603=CARTESIAN_POINT('Ctrl Pts',(0.328171877683939,-6.75903781752236,
22.2125465535066));
#188604=CARTESIAN_POINT('Ctrl Pts',(0.504685849649502,-6.75046752642749,
22.2208536039223));
#188605=CARTESIAN_POINT('Ctrl Pts',(0.680778563572517,-6.7349824960736,
22.229160654338));
#188606=CARTESIAN_POINT('Ctrl Pts',(0.855882010926367,-6.71265632841222,
22.2374677047538));
#188607=CARTESIAN_POINT('Ctrl Pts',(1.0311726734178,-6.69030629030961,22.2457836368084));
#188608=CARTESIAN_POINT('Ctrl Pts',(1.20547161169683,-6.66110055214837,
22.254099568863));
#188609=CARTESIAN_POINT('Ctrl Pts',(1.37821981766227,-6.62516408356827,
22.2624155009176));
#188610=CARTESIAN_POINT('Ctrl Pts',(1.5084410846112,-6.59807441023697,22.2686842271366));
#188611=CARTESIAN_POINT('Ctrl Pts',(1.63778134385809,-6.56716108539172,
22.2749529533555));
#188612=CARTESIAN_POINT('Ctrl Pts',(1.76600695449821,-6.5324963403483,22.2812216795745));
#188613=CARTESIAN_POINT('Ctrl Pts',(1.93885560497011,-6.48576812147069,
22.2896719482978));
#188614=CARTESIAN_POINT('Ctrl Pts',(2.10999522057186,-6.43213574420275,
22.2981222170212));
#188615=CARTESIAN_POINT('Ctrl Pts',(2.278855405123,-6.37174285753448,22.3065724857445));
#188616=CARTESIAN_POINT('Ctrl Pts',(2.44756656483243,-6.31140326963762,
22.3150152968191));
#188617=CARTESIAN_POINT('Ctrl Pts',(2.61400199236264,-6.24431517555305,
22.3234581078936));
#188618=CARTESIAN_POINT('Ctrl Pts',(2.7776056207408,-6.1706722498954,22.3319009189681));
#188619=CARTESIAN_POINT('Ctrl Pts',(2.9410871384213,-6.09708428994431,22.3403374284858));
#188620=CARTESIAN_POINT('Ctrl Pts',(3.10174076892398,-6.01695138680906,
22.3487739380036));
#188621=CARTESIAN_POINT('Ctrl Pts',(3.25902926810792,-5.93051576421613,
22.3572104475213));
#188622=CARTESIAN_POINT('Ctrl Pts',(3.41620521890647,-5.84414199096255,
22.3656409202625));
#188623=CARTESIAN_POINT('Ctrl Pts',(3.57002055150506,-5.75147465334733,
22.3740713930037));
#188624=CARTESIAN_POINT('Ctrl Pts',(3.71996134355306,-5.65280254409005,
22.3825018657449));
#188625=CARTESIAN_POINT('Ctrl Pts',(3.86983767646135,-5.55417285370484,
22.3909287142488));
#188626=CARTESIAN_POINT('Ctrl Pts',(4.0158425128803,-5.44954371980091,22.3993555627526));
#188627=CARTESIAN_POINT('Ctrl Pts',(4.15748915962667,-5.33924834481285,
22.4077824112565));
#188628=CARTESIAN_POINT('Ctrl Pts',(4.29909208511144,-5.22898701406836,
22.4162066586931));
#188629=CARTESIAN_POINT('Ctrl Pts',(4.4363392422887,-5.11306313357175,22.4246309061297));
#188630=CARTESIAN_POINT('Ctrl Pts',(4.56877511030842,-4.9918516595975,22.4330551535663));
#188631=CARTESIAN_POINT('Ctrl Pts',(4.60609047084215,-4.95769890385387,
22.4354287841773));
#188632=CARTESIAN_POINT('Ctrl Pts',(4.64302406530954,-4.92312661393061,
22.4378024147883));
#188633=CARTESIAN_POINT('Ctrl Pts',(4.67956618893992,-4.88814374618119,
22.4401760453993));
#188634=CARTESIAN_POINT('Ctrl Pts',(4.81225261331216,-4.76111906412091,
22.4487948263365));
#188635=CARTESIAN_POINT('Ctrl Pts',(4.93971555115588,-4.62873506524635,
22.4574136072737));
#188636=CARTESIAN_POINT('Ctrl Pts',(5.06153999065129,-4.49144764224606,
22.466032388211));
#188637=CARTESIAN_POINT('Ctrl Pts',(5.18343760934638,-4.35407775152597,
22.4746563463975));
#188638=CARTESIAN_POINT('Ctrl Pts',(5.29968976835802,-4.21179878595593,
22.483280304584));
#188639=CARTESIAN_POINT('Ctrl Pts',(5.4099216612736,-4.06509982889507,22.4919042627705));
#188640=CARTESIAN_POINT('Ctrl Pts',(5.52413585637278,-3.91310113904741,
22.5008397751416));
#188641=CARTESIAN_POINT('Ctrl Pts',(5.63188647995301,-3.75635743750224,
22.5097752875127));
#188642=CARTESIAN_POINT('Ctrl Pts',(5.73280591916584,-3.59544507581149,
22.5187107998839));
#188643=CARTESIAN_POINT('Ctrl Pts',(5.83038870830528,-3.43985288085604,
22.5273508817785));
#188644=CARTESIAN_POINT('Ctrl Pts',(5.92158468450929,-3.28036355404071,
22.5359909636732));
#188645=CARTESIAN_POINT('Ctrl Pts',(6.00610837780384,-3.11752324034233,
22.5446310455679));
#188646=CARTESIAN_POINT('Ctrl Pts',(6.09496725135797,-2.94633092395816,
22.5537142731773));
#188647=CARTESIAN_POINT('Ctrl Pts',(6.17645126152661,-2.77143520727055,
22.5627975007866));
#188648=CARTESIAN_POINT('Ctrl Pts',(6.25028584452666,-2.59349491260532,
22.571880728396));
#188649=CARTESIAN_POINT('Ctrl Pts',(6.32412042752671,-2.41555461794009,
22.5809639560053));
#188650=CARTESIAN_POINT('Ctrl Pts',(6.39030548178426,-2.23457012104382,
22.5900471836147));
#188651=CARTESIAN_POINT('Ctrl Pts',(6.44862675758667,-2.05121962289202,
22.599130411224));
#188652=CARTESIAN_POINT('Ctrl Pts',(6.50669998155796,-1.86864895039006,
22.6081750060838));
#188653=CARTESIAN_POINT('Ctrl Pts',(6.5570306414638,-1.68356402629343,22.6172196009436));
#188654=CARTESIAN_POINT('Ctrl Pts',(6.59942801012511,-1.49660914709759,
22.6262641958035));
#188655=CARTESIAN_POINT('Ctrl Pts',(6.64178647252687,-1.30982582843211,
22.6353004908238));
#188656=CARTESIAN_POINT('Ctrl Pts',(6.67622612575914,-1.12117621242904,
22.6443367858441));
#188657=CARTESIAN_POINT('Ctrl Pts',(6.70260675191163,-0.931317201187977,
22.6533730808644));
#188658=CARTESIAN_POINT('Ctrl Pts',(6.72894069547753,-0.741794160354964,
22.6623933854521));
#188659=CARTESIAN_POINT('Ctrl Pts',(6.74724405682532,-0.551066233153369,
22.6714136900398));
#188660=CARTESIAN_POINT('Ctrl Pts',(6.75742810502057,-0.359797728561595,
22.6804339946275));
#188661=CARTESIAN_POINT('Ctrl Pts',(6.76759932838547,-0.168770089495615,
22.6894429398939));
#188662=CARTESIAN_POINT('Ctrl Pts',(6.76967163096781,0.0227965315663232,
22.6984518851602));
#188663=CARTESIAN_POINT('Ctrl Pts',(6.76360800458227,0.214232958133704,
22.7074608304266));
#188664=CARTESIAN_POINT('Ctrl Pts',(6.7575581474086,0.40523467310241,22.7164493182854));
#188665=CARTESIAN_POINT('Ctrl Pts',(6.74340924642376,0.596106546372357,
22.7254378061442));
#188666=CARTESIAN_POINT('Ctrl Pts',(6.72117622024647,0.786180142456833,
22.734426294003));
#188667=CARTESIAN_POINT('Ctrl Pts',(6.70166979969549,0.952943563292714,
22.7423124550182));
#188668=CARTESIAN_POINT('Ctrl Pts',(6.67594125548238,1.11909233995013,22.7501986160335));
#188669=CARTESIAN_POINT('Ctrl Pts',(6.64403371932614,1.28417480759331,22.7580847770488));
#188670=CARTESIAN_POINT('Ctrl Pts',(6.61117413998988,1.45418293407427,22.766206241905));
#188671=CARTESIAN_POINT('Ctrl Pts',(6.57177443920997,1.62298375675467,22.7743277067611));
#188672=CARTESIAN_POINT('Ctrl Pts',(6.52595244571703,1.79003733934237,22.7824491716173));
#188673=CARTESIAN_POINT('Ctrl Pts',(6.48013372000638,1.95707900855186,22.7905700572936));
#188674=CARTESIAN_POINT('Ctrl Pts',(6.42789371072715,2.12237333271924,22.7986909429698));
#188675=CARTESIAN_POINT('Ctrl Pts',(6.36940060920412,2.28539381277498,22.806811828646));
#188676=CARTESIAN_POINT('Ctrl Pts',(6.31090051608323,2.44843377843862,22.8149336850003));
#188677=CARTESIAN_POINT('Ctrl Pts',(6.24614596722672,2.60919901453646,22.8230555413545));
#188678=CARTESIAN_POINT('Ctrl Pts',(6.1753539321172,2.76718138420392,22.8311773977088));
#188679=CARTESIAN_POINT('Ctrl Pts',(6.10451024801452,2.9252790158541,22.839305179669));
#188680=CARTESIAN_POINT('Ctrl Pts',(6.02762042981907,3.08058939140805,22.8474329616291));
#188681=CARTESIAN_POINT('Ctrl Pts',(5.94494848823246,3.23262686870331,22.8555607435893));
#188682=CARTESIAN_POINT('Ctrl Pts',(5.86224286916956,3.38472628041598,22.8636918365058));
#188683=CARTESIAN_POINT('Ctrl Pts',(5.77375061871918,3.53354982178732,22.8718229294222));
#188684=CARTESIAN_POINT('Ctrl Pts',(5.67977988231148,3.67863962471044,22.8799540223387));
#188685=CARTESIAN_POINT('Ctrl Pts',(5.58570658077237,3.82388778708964,22.8880939900032));
#188686=CARTESIAN_POINT('Ctrl Pts',(5.48614306060679,3.96539377232738,22.8962339576678));
#188687=CARTESIAN_POINT('Ctrl Pts',(5.38143910172155,4.1027310653347,22.9043739253323));
#188688=CARTESIAN_POINT('Ctrl Pts',(5.3271351015356,4.17396012357099,22.9085956645127));
#188689=CARTESIAN_POINT('Ctrl Pts',(5.27144901479941,4.24406840679247,22.9128174036931));
#188690=CARTESIAN_POINT('Ctrl Pts',(5.21443360200505,4.3130002562347,22.9170391428736));
#188691=CARTESIAN_POINT('Ctrl Pts',(5.10043797033807,4.45082140553485,22.9254800152801));
#188692=CARTESIAN_POINT('Ctrl Pts',(4.98089045055199,4.58422245634782,22.9339208876866));
#188693=CARTESIAN_POINT('Ctrl Pts',(4.85616084904731,4.71274769197123,22.9423617600932));
#188694=CARTESIAN_POINT('Ctrl Pts',(4.72888071563014,4.84390107449051,22.9509752355882));
#188695=CARTESIAN_POINT('Ctrl Pts',(4.59620447748548,4.96997679336693,22.9595887110832));
#188696=CARTESIAN_POINT('Ctrl Pts',(4.45856823506176,5.09052632772863,22.9682021865782));
#188697=CARTESIAN_POINT('Ctrl Pts',(4.32388824965514,5.2084866065237,22.9766306552253));
#188698=CARTESIAN_POINT('Ctrl Pts',(4.18445941432856,5.32115543001297,22.9850591238723));
#188699=CARTESIAN_POINT('Ctrl Pts',(4.0407274065947,5.42814987132766,22.9934875925194));
#188700=CARTESIAN_POINT('Ctrl Pts',(3.89226297234072,5.53866714196594,23.0021935714383));
#188701=CARTESIAN_POINT('Ctrl Pts',(3.73920742249339,5.64312973429293,23.0108995503573));
#188702=CARTESIAN_POINT('Ctrl Pts',(3.58208886976396,5.74116088688631,23.0196055292763));
#188703=CARTESIAN_POINT('Ctrl Pts',(3.42497031703453,5.83919203947969,23.0283115081953));
#188704=CARTESIAN_POINT('Ctrl Pts',(3.26378908609646,5.9307915306607,23.0370174871142));
#188705=CARTESIAN_POINT('Ctrl Pts',(3.09910619832133,6.01563211736941,23.0457234660332));
#188706=CARTESIAN_POINT('Ctrl Pts',(3.09910619832133,6.01563211736941,21.0459783413229));
#188707=CARTESIAN_POINT('Ctrl Pts',(2.94382747564148,6.09562790875683,21.0542049202976));
#188708=CARTESIAN_POINT('Ctrl Pts',(2.78528255985401,6.16969361804676,21.0624314992722));
#188709=CARTESIAN_POINT('Ctrl Pts',(2.62396313098396,6.23755613098887,21.0706580782469));
#188710=CARTESIAN_POINT('Ctrl Pts',(2.46280817665563,6.30534945415147,21.0788762697457));
#188711=CARTESIAN_POINT('Ctrl Pts',(2.29888467345399,6.36695204846957,21.0870944612445));
#188712=CARTESIAN_POINT('Ctrl Pts',(2.13270787261217,6.42213719334133,21.0953126527434));
#188713=CARTESIAN_POINT('Ctrl Pts',(1.96663049601534,6.47728932072006,21.1035259272654));
#188714=CARTESIAN_POINT('Ctrl Pts',(1.79830284291209,6.52603153246958,21.1117392017873));
#188715=CARTESIAN_POINT('Ctrl Pts',(1.62825953586144,6.56818543312202,21.1199524763093));
#188716=CARTESIAN_POINT('Ctrl Pts',(1.45828312583814,6.61032274993653,21.128162519633));
#188717=CARTESIAN_POINT('Ctrl Pts',(1.28659275059701,6.64587683065302,21.1363725629566));
#188718=CARTESIAN_POINT('Ctrl Pts',(1.11373770206829,6.67471926982638,21.1445826062802));
#188719=CARTESIAN_POINT('Ctrl Pts',(0.945596086519667,6.7027752297781,21.1525687771206));
#188720=CARTESIAN_POINT('Ctrl Pts',(0.776352808330789,6.72448073582025,
21.1605549479609));
#188721=CARTESIAN_POINT('Ctrl Pts',(0.606522686664242,6.73976403374492,
21.1685411188012));
#188722=CARTESIAN_POINT('Ctrl Pts',(0.418129816635969,6.75671782457585,
21.1774001929771));
#188723=CARTESIAN_POINT('Ctrl Pts',(0.229210887468987,6.7657516186024,21.186259267153));
#188724=CARTESIAN_POINT('Ctrl Pts',(0.0404191399853253,6.76687928761278,
21.1951183413288));
#188725=CARTESIAN_POINT('Ctrl Pts',(-0.148727309209687,6.76800907528636,
21.2039940599228));
#188726=CARTESIAN_POINT('Ctrl Pts',(-0.337745839968023,6.7612030514985,
21.2128697785167));
#188727=CARTESIAN_POINT('Ctrl Pts',(-0.525986565538072,6.74652704232878,
21.2217454971107));
#188728=CARTESIAN_POINT('Ctrl Pts',(-0.714764476951838,6.73180915197556,
21.2306465444977));
#188729=CARTESIAN_POINT('Ctrl Pts',(-0.902759881300691,6.70917635351106,
21.2395475918846));
#188730=CARTESIAN_POINT('Ctrl Pts',(-1.08932826356542,6.67874635947478,
21.2484486392716));
#188731=CARTESIAN_POINT('Ctrl Pts',(-1.27615028810489,6.64827499544421,
21.2573617877546));
#188732=CARTESIAN_POINT('Ctrl Pts',(-1.4615411604175,6.60998530905217,21.2662749362377));
#188733=CARTESIAN_POINT('Ctrl Pts',(-1.64486848209565,6.56404575521898,
21.2751880847207));
#188734=CARTESIAN_POINT('Ctrl Pts',(-1.82860284055769,6.51800420301439,
21.2841210228305));
#188735=CARTESIAN_POINT('Ctrl Pts',(-2.01026423175698,6.46427887393469,
21.2930539609404));
#188736=CARTESIAN_POINT('Ctrl Pts',(-2.18923453205078,6.40308840823524,
21.3019868990503));
#188737=CARTESIAN_POINT('Ctrl Pts',(-2.3595883083182,6.34484395713719,21.3104897609089));
#188738=CARTESIAN_POINT('Ctrl Pts',(-2.52750384596131,6.27983632908412,
21.3189926227674));
#188739=CARTESIAN_POINT('Ctrl Pts',(-2.69246653831701,6.2082938831891,21.327495484626));
#188740=CARTESIAN_POINT('Ctrl Pts',(-2.85199431731393,6.13910849748365,
21.3357182084918));
#188741=CARTESIAN_POINT('Ctrl Pts',(-3.00906597722489,6.06367828421869,
21.3439409323577));
#188742=CARTESIAN_POINT('Ctrl Pts',(-3.16315895579046,5.98219979776692,
21.3521636562236));
#188743=CARTESIAN_POINT('Ctrl Pts',(-3.31708883215837,5.90080755353285,
21.3603776766148));
#188744=CARTESIAN_POINT('Ctrl Pts',(-3.46804599099936,5.81337995062288,
21.368591697006));
#188745=CARTESIAN_POINT('Ctrl Pts',(-3.61552752086404,5.72016168878772,
21.3768057173973));
#188746=CARTESIAN_POINT('Ctrl Pts',(-3.76288255664704,5.62702337973334,
21.3850126926692));
#188747=CARTESIAN_POINT('Ctrl Pts',(-3.90676759891499,5.5281044937726,21.3932196679412));
#188748=CARTESIAN_POINT('Ctrl Pts',(-4.04670396952207,5.42369578636693,
21.4014266432131));
#188749=CARTESIAN_POINT('Ctrl Pts',(-4.18654840472603,5.31935567339859,
21.4096282266661));
#188750=CARTESIAN_POINT('Ctrl Pts',(-4.32244904911747,5.20953313685444,
21.4178298101191));
#188751=CARTESIAN_POINT('Ctrl Pts',(-4.45395581245558,5.094562456256,21.4260313935721));
#188752=CARTESIAN_POINT('Ctrl Pts',(-4.58540256836945,4.97964423755557,
21.4342292345871));
#188753=CARTESIAN_POINT('Ctrl Pts',(-4.71245916808593,4.85958279046807,
21.4424270756022));
#188754=CARTESIAN_POINT('Ctrl Pts',(-4.83470819332551,4.73475296983815,
21.4506249166172));
#188755=CARTESIAN_POINT('Ctrl Pts',(-4.95694643046984,4.60993416505063,
21.4588220341984));
#188756=CARTESIAN_POINT('Ctrl Pts',(-5.07437768126029,4.48034807498078,
21.4670191517796));
#188757=CARTESIAN_POINT('Ctrl Pts',(-5.18662078474238,4.34640700294834,
21.4752162693607));
#188758=CARTESIAN_POINT('Ctrl Pts',(-5.29886263939499,4.21246742115944,
21.4834132957398));
#188759=CARTESIAN_POINT('Ctrl Pts',(-5.40591623041273,4.07417322825725,
21.4916103221189));
#188760=CARTESIAN_POINT('Ctrl Pts',(-5.5074402518264,3.93197035499537,21.499807348498));
#188761=CARTESIAN_POINT('Ctrl Pts',(-5.6089816038196,3.78974320710201,21.5080057741441));
#188762=CARTESIAN_POINT('Ctrl Pts',(-5.70499129713191,3.64360634158288,
21.5162041997903));
#188763=CARTESIAN_POINT('Ctrl Pts',(-5.79517095851232,3.49403528339589,
21.5244026254364));
#188764=CARTESIAN_POINT('Ctrl Pts',(-5.88538241151737,3.34441149594749,
21.5326039413271));
#188765=CARTESIAN_POINT('Ctrl Pts',(-5.96975955324907,3.19135141125988,
21.5408052572177));
#188766=CARTESIAN_POINT('Ctrl Pts',(-6.04804960264305,3.0353558282299,21.5490065731084));
#188767=CARTESIAN_POINT('Ctrl Pts',(-6.126428811298,2.87918259234359,21.557217228925));
#188768=CARTESIAN_POINT('Ctrl Pts',(-6.19870691723301,2.72006750035543,
21.5654278847415));
#188769=CARTESIAN_POINT('Ctrl Pts',(-6.26467858903202,2.55853301251396,
21.5736385405581));
#188770=CARTESIAN_POINT('Ctrl Pts',(-6.33068913633892,2.39690333631233,
21.5818540347153));
#188771=CARTESIAN_POINT('Ctrl Pts',(-6.39038571927823,2.23285175900436,
21.5900695288724));
#188772=CARTESIAN_POINT('Ctrl Pts',(-6.44361273654199,2.06691652019957,
21.5982850230296));
#188773=CARTESIAN_POINT('Ctrl Pts',(-6.49692233650246,1.90072382981839,
21.6065132636771));
#188774=CARTESIAN_POINT('Ctrl Pts',(-6.54374221538474,1.7326419830069,21.6147415043246));
#188775=CARTESIAN_POINT('Ctrl Pts',(-6.58396749668861,1.56322135430268,
21.6229697449721));
#188776=CARTESIAN_POINT('Ctrl Pts',(-6.62052585538449,1.40924505099579,
21.6304479020732));
#188777=CARTESIAN_POINT('Ctrl Pts',(-6.65163775084048,1.25416323714382,
21.6379260591743));
#188778=CARTESIAN_POINT('Ctrl Pts',(-6.67726167823053,1.09839222522469,
21.6454042162755));
#188779=CARTESIAN_POINT('Ctrl Pts',(-6.72073983845508,0.834083131951578,
21.6580930015533));
#188780=CARTESIAN_POINT('Ctrl Pts',(-6.74855195933655,0.56700790866886,
21.6707817868311));
#188781=CARTESIAN_POINT('Ctrl Pts',(-6.7604070780163,0.29863881111992,21.683470572109));
#188782=CARTESIAN_POINT('Ctrl Pts',(-6.76467657868595,0.201988404434906,
21.6880403093427));
#188783=CARTESIAN_POINT('Ctrl Pts',(-6.76687673293707,0.105170525308029,
21.6926100465764));
#188784=CARTESIAN_POINT('Ctrl Pts',(-6.7669949644283,0.00825538624319681,
21.6971797838101));
#188785=CARTESIAN_POINT('',(-6.767,9.7407047434505E-13,21.3028202161899));
#188786=CARTESIAN_POINT('Ctrl Pts',(3.09910619832131,6.01563211736942,20.6513174420499));
#188787=CARTESIAN_POINT('Ctrl Pts',(2.9420188085974,6.09655968967987,20.6596250383763));
#188788=CARTESIAN_POINT('Ctrl Pts',(2.78183949938961,6.17128913350124,20.6679326347026));
#188789=CARTESIAN_POINT('Ctrl Pts',(2.61909714245077,6.23960088133899,20.676240231029));
#188790=CARTESIAN_POINT('Ctrl Pts',(2.45618547297322,6.30798369878435,20.6845564703433));
#188791=CARTESIAN_POINT('Ctrl Pts',(2.29070575261917,6.36993535452906,20.6928727096575));
#188792=CARTESIAN_POINT('Ctrl Pts',(2.12320456495112,6.42528531470554,20.7011889489718));
#188793=CARTESIAN_POINT('Ctrl Pts',(2.02142093381408,6.45891922505858,20.7062423879748));
#188794=CARTESIAN_POINT('Ctrl Pts',(1.91889116698867,6.49011643561359,20.7112958269778));
#188795=CARTESIAN_POINT('Ctrl Pts',(1.81573999407531,6.51884784865511,20.7163492659808));
#188796=CARTESIAN_POINT('Ctrl Pts',(1.64325248018074,6.56689199460364,20.7247995347042));
#188797=CARTESIAN_POINT('Ctrl Pts',(1.46871052826714,6.60812677290956,20.7332498034276));
#188798=CARTESIAN_POINT('Ctrl Pts',(1.29267795625606,6.64238456440228,20.7417000721509));
#188799=CARTESIAN_POINT('Ctrl Pts',(1.11680073896188,6.67661212223178,20.7501428832254));
#188800=CARTESIAN_POINT('Ctrl Pts',(0.939435847604214,6.7038749030657,20.7585856942999));
#188801=CARTESIAN_POINT('Ctrl Pts',(0.761160312578012,6.72405561982916,
20.7670285053745));
#188802=CARTESIAN_POINT('Ctrl Pts',(0.583017839087675,6.74422127408185,
20.7754650148922));
#188803=CARTESIAN_POINT('Ctrl Pts',(0.40396640524696,6.7573153642745,20.7839015244099));
#188804=CARTESIAN_POINT('Ctrl Pts',(0.224591636110605,6.76327195941352,
20.7923380339276));
#188805=CARTESIAN_POINT('Ctrl Pts',(0.0453452192734122,6.7692242922882,
20.8007685066689));
#188806=CARTESIAN_POINT('Ctrl Pts',(-0.134223740770821,6.76804930638651,
20.8091989794101));
#188807=CARTESIAN_POINT('Ctrl Pts',(-0.313525903762525,6.75973302044318,
20.8176294521513));
#188808=CARTESIAN_POINT('Ctrl Pts',(-0.492750985240562,6.75142030964863,
20.8260563006551));
#188809=CARTESIAN_POINT('Ctrl Pts',(-0.671709167696662,6.73597243434907,
20.834483149159));
#188810=CARTESIAN_POINT('Ctrl Pts',(-0.84981185785603,6.71342750063239,
20.8429099976628));
#188811=CARTESIAN_POINT('Ctrl Pts',(-1.02785957407512,6.69088952573166,
20.8513342450994));
#188812=CARTESIAN_POINT('Ctrl Pts',(-1.20505199602207,6.66125890259825,
20.8597584925361));
#188813=CARTESIAN_POINT('Ctrl Pts',(-1.38080602384894,6.6246255535315,20.8681827399727));
#188814=CARTESIAN_POINT('Ctrl Pts',(-1.43032678443763,6.61430367737806,
20.8705563705837));
#188815=CARTESIAN_POINT('Ctrl Pts',(-1.47973339825789,6.60342617115657,
20.8729300011946));
#188816=CARTESIAN_POINT('Ctrl Pts',(-1.52901294840639,6.59199578303913,
20.8753036318056));
#188817=CARTESIAN_POINT('Ctrl Pts',(-1.70794965635648,6.55049142648222,
20.8839224127428));
#188818=CARTESIAN_POINT('Ctrl Pts',(-1.88513012267368,6.5017122707146,20.89254119368));
#188819=CARTESIAN_POINT('Ctrl Pts',(-2.05996476989152,6.44583851386348,
20.9011599746173));
#188820=CARTESIAN_POINT('Ctrl Pts',(-2.23490443921883,6.38993119398638,
20.9097839328038));
#188821=CARTESIAN_POINT('Ctrl Pts',(-2.40749518753538,6.32692086059346,
20.9184078909903));
#188822=CARTESIAN_POINT('Ctrl Pts',(-2.57716506940687,6.25703677510602,
20.9270318491768));
#188823=CARTESIAN_POINT('Ctrl Pts',(-2.75296454520189,6.18462801605229,
20.935967361548));
#188824=CARTESIAN_POINT('Ctrl Pts',(-2.92562784627793,6.10483973798158,
20.9449028739191));
#188825=CARTESIAN_POINT('Ctrl Pts',(-3.09454466900673,6.01797991783971,
20.9538383862902));
#188826=CARTESIAN_POINT('Ctrl Pts',(-3.25787667741909,5.93399190146027,
20.9624784681849));
#188827=CARTESIAN_POINT('Ctrl Pts',(-3.41770573619125,5.84339265523882,
20.9711185500796));
#188828=CARTESIAN_POINT('Ctrl Pts',(-3.5735075963264,5.7465061088454,20.9797586319743));
#188829=CARTESIAN_POINT('Ctrl Pts',(-3.73730046019193,5.6446502973034,20.9888418595836));
#188830=CARTESIAN_POINT('Ctrl Pts',(-3.89664184339482,5.53584552154564,
20.997925087193));
#188831=CARTESIAN_POINT('Ctrl Pts',(-4.05095936177605,5.42051817165472,
21.0070083148023));
#188832=CARTESIAN_POINT('Ctrl Pts',(-4.2052768801573,5.30519082176379,21.0160915424117));
#188833=CARTESIAN_POINT('Ctrl Pts',(-4.35457025457998,5.18334116900584,
21.025174770021));
#188834=CARTESIAN_POINT('Ctrl Pts',(-4.49830907481029,5.05544305352948,
21.0342579976303));
#188835=CARTESIAN_POINT('Ctrl Pts',(-4.64143654563083,4.92808891383698,
21.0433025924902));
#188836=CARTESIAN_POINT('Ctrl Pts',(-4.77918936808601,4.7946206990437,21.05234718735));
#188837=CARTESIAN_POINT('Ctrl Pts',(-4.91107466523752,4.65549510068072,
21.0613917822098));
#188838=CARTESIAN_POINT('Ctrl Pts',(-5.04283893686909,4.51649717195373,
21.0704280772301));
#188839=CARTESIAN_POINT('Ctrl Pts',(-5.16874626961175,4.37185239709217,
21.0794643722505));
#188840=CARTESIAN_POINT('Ctrl Pts',(-5.28834078624878,4.22205408876978,
21.0885006672708));
#188841=CARTESIAN_POINT('Ctrl Pts',(-5.40772367101038,4.0725208603007,21.0975209718586));
#188842=CARTESIAN_POINT('Ctrl Pts',(-5.52081589854251,3.9178524946821,21.1065412764463));
#188843=CARTESIAN_POINT('Ctrl Pts',(-5.62720208567325,3.75857495428715,
21.115561581034));
#188844=CARTESIAN_POINT('Ctrl Pts',(-5.73345430006742,3.59949799301376,
21.1245705263003));
#188845=CARTESIAN_POINT('Ctrl Pts',(-5.83301719554953,3.43582363770394,
21.1335794715666));
#188846=CARTESIAN_POINT('Ctrl Pts',(-5.92551738190147,3.26810843712132,
21.142588416833));
#188847=CARTESIAN_POINT('Ctrl Pts',(-6.01780751991234,3.1007740822542,21.1515769046918));
#188848=CARTESIAN_POINT('Ctrl Pts',(-6.10306684718191,2.92941740593767,
21.1605653925506));
#188849=CARTESIAN_POINT('Ctrl Pts',(-6.18096700465798,2.75462082460171,
21.1695538804094));
#188850=CARTESIAN_POINT('Ctrl Pts',(-6.24931367148559,2.60126088164081,
21.1774400414246));
#188851=CARTESIAN_POINT('Ctrl Pts',(-6.3119960736473,2.44525354068808,21.1853262024399));
#188852=CARTESIAN_POINT('Ctrl Pts',(-6.36882075883218,2.28700921333262,
21.1932123634551));
#188853=CARTESIAN_POINT('Ctrl Pts',(-6.42522204905894,2.12994394838879,
21.2010397654856));
#188854=CARTESIAN_POINT('Ctrl Pts',(-6.47584228433969,1.97069819679649,
21.208867167516));
#188855=CARTESIAN_POINT('Ctrl Pts',(-6.52050999703648,1.80976196737233,
21.2166945695465));
#188856=CARTESIAN_POINT('Ctrl Pts',(-6.56517995872835,1.6488176348964,21.2245223656824));
#188857=CARTESIAN_POINT('Ctrl Pts',(-6.60389668221933,1.48618302928765,
21.2323501618183));
#188858=CARTESIAN_POINT('Ctrl Pts',(-6.63653857191159,1.32236333264716,
21.2401779579542));
#188859=CARTESIAN_POINT('Ctrl Pts',(-6.66918049363267,1.15854347526379,
21.2480057617708));
#188860=CARTESIAN_POINT('Ctrl Pts',(-6.69574750043971,0.993538910979629,
21.2558335655875));
#188861=CARTESIAN_POINT('Ctrl Pts',(-6.71616928443157,0.827864205566292,
21.2636613694042));
#188862=CARTESIAN_POINT('Ctrl Pts',(-6.73660316178977,0.662091390952241,
21.2714938086875));
#188863=CARTESIAN_POINT('Ctrl Pts',(-6.75088450933278,0.495648033274671,
21.2793262479709));
#188864=CARTESIAN_POINT('Ctrl Pts',(-6.75899497096985,0.329053160453232,
21.2871586872542));
#188865=CARTESIAN_POINT('Ctrl Pts',(-6.76433416341804,0.21938220377068,
21.2923148549971));
#188866=CARTESIAN_POINT('Ctrl Pts',(-6.76700014338094,0.109645646085917,
21.2974710227399));
#188867=CARTESIAN_POINT('Ctrl Pts',(-6.76699999999422,-8.84868392606215E-6,
21.3026271904827));
#188868=CARTESIAN_POINT('Ctrl Pts',(-6.767,9.7407047898921E-13,21.3028202161899));
#188869=CARTESIAN_POINT('Ctrl Pts',(-6.76700000000003,-0.186007249526034,
21.3115697280011));
#188870=CARTESIAN_POINT('Ctrl Pts',(-6.75932637294525,-0.372014355749215,
21.3203192398123));
#188871=CARTESIAN_POINT('Ctrl Pts',(-6.74400518264185,-0.557389537486927,
21.3290687516235));
#188872=CARTESIAN_POINT('Ctrl Pts',(-6.7286840570509,-0.742763936251391,
21.3378182264791));
#188873=CARTESIAN_POINT('Ctrl Pts',(-6.70571545645729,-0.927506130242027,
21.3465677013348));
#188874=CARTESIAN_POINT('Ctrl Pts',(-6.67517739404803,-1.11098863990153,
21.3553171761905));
#188875=CARTESIAN_POINT('Ctrl Pts',(-6.64463945808673,-1.29447038982095,
21.3640666148175));
#188876=CARTESIAN_POINT('Ctrl Pts',(-6.6065321700832,-1.47669218313842,
21.3728160534445));
#188877=CARTESIAN_POINT('Ctrl Pts',(-6.56098496092634,-1.65703510599455,
21.3815654920715));
#188878=CARTESIAN_POINT('Ctrl Pts',(-6.51543793658252,-1.83737729708858,
21.3903148951967));
#188879=CARTESIAN_POINT('Ctrl Pts',(-6.46245112167374,-2.01584035511074,
21.3990642983219));
#188880=CARTESIAN_POINT('Ctrl Pts',(-6.40220448374207,-2.19181813760928,
21.407813701447));
#188881=CARTESIAN_POINT('Ctrl Pts',(-6.34195808526455,-2.36779522067275,
21.4165630697971));
#188882=CARTESIAN_POINT('Ctrl Pts',(-6.27445201433053,-2.54128677684292,
21.4253124381472));
#188883=CARTESIAN_POINT('Ctrl Pts',(-6.19991555071849,-2.71170355384933,
21.4340618064973));
#188884=CARTESIAN_POINT('Ctrl Pts',(-6.12537937716646,-2.88211966767575,
21.4428111407991));
#188885=CARTESIAN_POINT('Ctrl Pts',(-6.04381298052481,-3.04946076371861,
21.4515604751009));
#188886=CARTESIAN_POINT('Ctrl Pts',(-5.95549339335802,-3.21315848374601,
21.4603098094026));
#188887=CARTESIAN_POINT('Ctrl Pts',(-5.86717414255374,-3.37685558033555,
21.4690591103828));
#188888=CARTESIAN_POINT('Ctrl Pts',(-5.77210188876556,-3.53690907646826,
21.477808411363));
#188889=CARTESIAN_POINT('Ctrl Pts',(-5.67059953346946,-3.69277536969363,
21.4865577123432));
#188890=CARTESIAN_POINT('Ctrl Pts',(-5.56909755631333,-3.84864108224997,
21.4953069807285));
#188891=CARTESIAN_POINT('Ctrl Pts',(-5.46116568196798,-4.00031938297587,
21.5040562491138));
#188892=CARTESIAN_POINT('Ctrl Pts',(-5.34717048533551,-4.14729511859921,
21.512805517499));
#188893=CARTESIAN_POINT('Ctrl Pts',(-5.23317570391784,-4.2942703188798,
21.5215547540161));
#188894=CARTESIAN_POINT('Ctrl Pts',(-5.11311782003462,-4.43654276189607,
21.5303039905331));
#188895=CARTESIAN_POINT('Ctrl Pts',(-4.98740458984701,-4.57362924351909,
21.5390532270502));
#188896=CARTESIAN_POINT('Ctrl Pts',(-4.86169180711693,-4.71071523720318,
21.5478024324256));
#188897=CARTESIAN_POINT('Ctrl Pts',(-4.73032391204123,-4.84261509523285,
21.556551637801));
#188898=CARTESIAN_POINT('Ctrl Pts',(-4.59374707013553,-4.96888084538372,
21.5653008431765));
#188899=CARTESIAN_POINT('Ctrl Pts',(-4.45717070301427,-5.09514615659478,
21.5740500181369));
#188900=CARTESIAN_POINT('Ctrl Pts',(-4.31538563571052,-5.21577720459517,
21.5827991930973));
#188901=CARTESIAN_POINT('Ctrl Pts',(-4.16887341029552,-5.33036429232853,
21.5915483680578));
#188902=CARTESIAN_POINT('Ctrl Pts',(-4.02236168203746,-5.44495099123586,
21.6002975133298));
#188903=CARTESIAN_POINT('Ctrl Pts',(-3.87112305348203,-5.55349359438575,
21.6090466586018));
#188904=CARTESIAN_POINT('Ctrl Pts',(-3.71567117017795,-5.65562346298871,
21.6177958038738));
#188905=CARTESIAN_POINT('Ctrl Pts',(-3.5602198014585,-5.75775299351625,
21.626544920184));
#188906=CARTESIAN_POINT('Ctrl Pts',(-3.40055544538377,-5.85346967463857,
21.6352940364942));
#188907=CARTESIAN_POINT('Ctrl Pts',(-3.23722035986878,-5.94244842986888,
21.6440431528043));
#188908=CARTESIAN_POINT('Ctrl Pts',(-3.07388580147188,-6.03142689794526,
21.6527922408792));
#188909=CARTESIAN_POINT('Ctrl Pts',(-2.90688078896568,-6.11366734656787,
21.6615413289541));
#188910=CARTESIAN_POINT('Ctrl Pts',(-2.73677250721342,-6.18889046952366,
21.6702904170289));
#188911=CARTESIAN_POINT('Ctrl Pts',(-2.56666476031447,-6.26411335596342,
21.6790394775949));
#188912=CARTESIAN_POINT('Ctrl Pts',(-2.39345402575123,-6.33231884500572,
21.687788538161));
#188913=CARTESIAN_POINT('Ctrl Pts',(-2.2177285606554,-6.39327529762745,
21.696537598727));
#188914=CARTESIAN_POINT('Ctrl Pts',(-2.04200363348465,-6.45423156365126,
21.7052866325107));
#188915=CARTESIAN_POINT('Ctrl Pts',(-1.86376426189232,-6.50793874375671,
21.7140356662944));
#188916=CARTESIAN_POINT('Ctrl Pts',(-1.68361577753111,-6.55421443909553,
21.7227847000781));
#188917=CARTESIAN_POINT('Ctrl Pts',(-1.50346782967731,-6.60048999661884,
21.7315337078059));
#188918=CARTESIAN_POINT('Ctrl Pts',(-1.32141105794894,-6.63933404237732,
21.7402827155338));
#188919=CARTESIAN_POINT('Ctrl Pts',(-1.13806375486904,-6.67061465607581,
21.7490317232616));
#188920=CARTESIAN_POINT('Ctrl Pts',(-0.954716982601926,-6.70189517921312,
21.75778070566));
#188921=CARTESIAN_POINT('Ctrl Pts',(-0.770079968901146,-6.72561226592239,
21.7665296880584));
#188922=CARTESIAN_POINT('Ctrl Pts',(-0.584779765557352,-6.7416853698311,
21.7752786704568));
#188923=CARTESIAN_POINT('Ctrl Pts',(-0.391489830650432,-6.75845151013858,
21.7844048894667));
#188924=CARTESIAN_POINT('Ctrl Pts',(-0.197478578237495,-6.76689983031628,
21.7935311084765));
#188925=CARTESIAN_POINT('Ctrl Pts',(-0.00346287645053296,-6.76699911397118,
21.8026573274864));
#188926=CARTESIAN_POINT('Ctrl Pts',(0.184489834655586,-6.76709529501186,
21.8114983521522));
#188927=CARTESIAN_POINT('Ctrl Pts',(0.37244640425106,-6.75935639738159,
21.820339376818));
#188928=CARTESIAN_POINT('Ctrl Pts',(0.559755019490015,-6.74380925873173,
21.8291804014838));
#188929=CARTESIAN_POINT('Ctrl Pts',(0.745134705523545,-6.72842222659786,
21.8379303800936));
#188930=CARTESIAN_POINT('Ctrl Pts',(0.929879431230425,-6.70538706057498,
21.8466803587033));
#188931=CARTESIAN_POINT('Ctrl Pts',(1.1133616362702,-6.67478200894095,21.8554303373131));
#188932=CARTESIAN_POINT('Ctrl Pts',(1.2968419630093,-6.64417727060972,21.8641802263496));
#188933=CARTESIAN_POINT('Ctrl Pts',(1.47905951217738,-6.6060028489054,21.8729301153861));
#188934=CARTESIAN_POINT('Ctrl Pts',(1.65939532067327,-6.56038841607169,
21.8816800044227));
#188935=CARTESIAN_POINT('Ctrl Pts',(1.83972934301042,-6.51477443503189,
21.8904298067948));
#188936=CARTESIAN_POINT('Ctrl Pts',(2.01818138406502,-6.46172066062067,
21.899179609167));
#188937=CARTESIAN_POINT('Ctrl Pts',(2.19414528354434,-6.40140730423398,
21.9079294115391));
#188938=CARTESIAN_POINT('Ctrl Pts',(2.37010749864218,-6.3410945251856,21.9166791301554));
#188939=CARTESIAN_POINT('Ctrl Pts',(2.54358134866663,-6.27352239616421,
21.9254288487718));
#188940=CARTESIAN_POINT('Ctrl Pts',(2.71397759435744,-6.19892043966737,
21.9341785673881));
#188941=CARTESIAN_POINT('Ctrl Pts',(2.88437226558304,-6.1243191724943,21.9429282051568));
#188942=CARTESIAN_POINT('Ctrl Pts',(3.05168912681129,-6.04268832278711,
21.9516778429255));
#188943=CARTESIAN_POINT('Ctrl Pts',(3.21535986274021,-5.95430516123244,
21.9604274806942));
#188944=CARTESIAN_POINT('Ctrl Pts',(3.3790291407302,-5.86592278697338,21.9691770405233));
#188945=CARTESIAN_POINT('Ctrl Pts',(3.53905210621761,-5.77078835741826,
21.9779266003523));
#188946=CARTESIAN_POINT('Ctrl Pts',(3.69488522831897,-5.66922500431499,
21.9866761601814));
#188947=CARTESIAN_POINT('Ctrl Pts',(3.85071701407147,-5.56766252216951,
21.9954256449785));
#188948=CARTESIAN_POINT('Ctrl Pts',(4.00235878822617,-5.45967138329214,
22.0041751297757));
#188949=CARTESIAN_POINT('Ctrl Pts',(4.14929549611544,-5.34561838199437,
22.0129246145728));
#188950=CARTESIAN_POINT('Ctrl Pts',(4.29623099276303,-5.23156632086841,
22.0216740272454));
#188951=CARTESIAN_POINT('Ctrl Pts',(4.43846127436234,-5.11145267304785,
22.030423439918));
#188952=CARTESIAN_POINT('Ctrl Pts',(4.57550326054642,-4.98568540049701,
22.0391728525905));
#188953=CARTESIAN_POINT('Ctrl Pts',(4.71254416257969,-4.85991912290178,
22.0479221960458));
#188954=CARTESIAN_POINT('Ctrl Pts',(4.84439664018937,-4.72849950385238,
22.056671539501));
#188955=CARTESIAN_POINT('Ctrl Pts',(4.9706128679491,-4.5918728986089,22.0654208829563));
#188956=CARTESIAN_POINT('Ctrl Pts',(5.09682813912844,-4.45524732884502,
22.0741701601011));
#188957=CARTESIAN_POINT('Ctrl Pts',(5.21740705147993,-4.31341506235601,
22.0829194372459));
#188958=CARTESIAN_POINT('Ctrl Pts',(5.33194007545845,-4.16685781275533,
22.0916687143908));
#188959=CARTESIAN_POINT('Ctrl Pts',(5.44647226944631,-4.02030162521645,
22.1004179281319));
#188960=CARTESIAN_POINT('Ctrl Pts',(5.55495848628254,-3.86902074887732,
22.109167141873));
#188961=CARTESIAN_POINT('Ctrl Pts',(5.65703027291924,-3.71352898080455,
22.1179163556141));
#188962=CARTESIAN_POINT('Ctrl Pts',(5.75910135377131,-3.55803828789372,
22.126665508858));
#188963=CARTESIAN_POINT('Ctrl Pts',(5.85475793592884,-3.39833700106486,
22.1354146621019));
#188964=CARTESIAN_POINT('Ctrl Pts',(5.94367514427526,-3.23496750823319,
22.1441638153458));
#188965=CARTESIAN_POINT('Ctrl Pts',(6.0325917673276,-3.0715990907749,22.1529129109987));
#188966=CARTESIAN_POINT('Ctrl Pts',(6.11476896836036,-2.90456276731199,
22.1616620066516));
#188967=CARTESIAN_POINT('Ctrl Pts',(6.1899276554799,-2.73442583002816,22.1704111023046));
#188968=CARTESIAN_POINT('Ctrl Pts',(6.26508587283143,-2.56428995615952,
22.1791601432726));
#188969=CARTESIAN_POINT('Ctrl Pts',(6.33322554827235,-2.39105376935,22.1879091842406));
#188970=CARTESIAN_POINT('Ctrl Pts',(6.39411526733094,-2.21530561053896,
22.1966582252086));
#188971=CARTESIAN_POINT('Ctrl Pts',(6.45500462602905,-2.03955849184917,
22.2054072143977));
#188972=CARTESIAN_POINT('Ctrl Pts',(6.50864402040791,-1.86129970164366,
22.2141562035867));
#188973=CARTESIAN_POINT('Ctrl Pts',(6.55485128368646,-1.68113463135883,
22.2229051927757));
#188974=CARTESIAN_POINT('Ctrl Pts',(6.60199809554362,-1.49730620116709,
22.2318320782471));
#188975=CARTESIAN_POINT('Ctrl Pts',(6.64140720707901,-1.31149343245555,
22.2407589637186));
#188976=CARTESIAN_POINT('Ctrl Pts',(6.67293928722905,-1.12435326697399,
22.24968584919));
#188977=CARTESIAN_POINT('Ctrl Pts',(6.70384625876274,-0.940923067005333,
22.2584357633675));
#188978=CARTESIAN_POINT('Ctrl Pts',(6.7271855457981,-0.756217899520418,
22.2671856775449));
#188979=CARTESIAN_POINT('Ctrl Pts',(6.74287786815338,-0.570865181253259,
22.2759355917224));
#188980=CARTESIAN_POINT('Ctrl Pts',(6.75856988190853,-0.385516108072748,
22.2846853338269));
#188981=CARTESIAN_POINT('Ctrl Pts',(6.76661520773406,-0.199519795225191,
22.2934350759313));
#188982=CARTESIAN_POINT('Ctrl Pts',(6.76698651789579,-0.013508020454534,
22.3021848180358));
#188983=CARTESIAN_POINT('Ctrl Pts',(6.767357821249,0.172500343514016,22.3109343997008));
#188984=CARTESIAN_POINT('Ctrl Pts',(6.76005538995178,0.358523882211916,
22.3196839813658));
#188985=CARTESIAN_POINT('Ctrl Pts',(6.74510402742353,0.543930748565311,
22.3284335630307));
#188986=CARTESIAN_POINT('Ctrl Pts',(6.73015291918021,0.729334461616112,
22.3371829958874));
#188987=CARTESIAN_POINT('Ctrl Pts',(6.70755316306583,0.914121237635499,
22.3459324287441));
#188988=CARTESIAN_POINT('Ctrl Pts',(6.67738151874562,1.09766345166198,22.3546818616008));
#188989=CARTESIAN_POINT('Ctrl Pts',(6.64721034747555,1.28120278799735,22.3634311572783));
#188990=CARTESIAN_POINT('Ctrl Pts',(6.60946757205127,1.46349731860394,22.3721804529558));
#188991=CARTESIAN_POINT('Ctrl Pts',(6.56428138111508,1.64392790278222,22.3809297486333));
#188992=CARTESIAN_POINT('Ctrl Pts',(6.51909583859833,1.82435589779116,22.3896789187589));
#188993=CARTESIAN_POINT('Ctrl Pts',(6.46646716392857,2.00291972192325,22.3984280888845));
#188994=CARTESIAN_POINT('Ctrl Pts',(6.40657409872863,2.17901292274723,22.4071772590101));
#188995=CARTESIAN_POINT('Ctrl Pts',(6.34668181342056,2.35510383059032,22.4159263152092));
#188996=CARTESIAN_POINT('Ctrl Pts',(6.2795254191403,2.5287239082263,22.4246753714084));
#188997=CARTESIAN_POINT('Ctrl Pts',(6.20533299175497,2.69928350890331,22.4334244276075));
#188998=CARTESIAN_POINT('Ctrl Pts',(6.12831602991527,2.8763363796567,22.4425065637657));
#188999=CARTESIAN_POINT('Ctrl Pts',(6.04371690605246,3.0500908660151,22.4515886999238));
#189000=CARTESIAN_POINT('Ctrl Pts',(5.95184520316605,3.21991112882783,22.460670836082));
#189001=CARTESIAN_POINT('Ctrl Pts',(5.86333549509244,3.3835169118307,22.4694206164256));
#189002=CARTESIAN_POINT('Ctrl Pts',(5.76807618099333,3.54347103712061,22.4781703967692));
#189003=CARTESIAN_POINT('Ctrl Pts',(5.66639083308976,3.69923018027756,22.4869201771128));
#189004=CARTESIAN_POINT('Ctrl Pts',(5.56470914082156,3.85498372382113,22.4956696428977));
#189005=CARTESIAN_POINT('Ctrl Pts',(5.45660203372019,4.00654234702063,22.5044191086826));
#189006=CARTESIAN_POINT('Ctrl Pts',(5.34243669839164,4.15339127986736,22.5131685744675));
#189007=CARTESIAN_POINT('Ctrl Pts',(5.2282748605054,4.30023571401342,22.5219177722135));
#189008=CARTESIAN_POINT('Ctrl Pts',(5.1080553416706,4.44237052028527,22.5306669699595));
#189009=CARTESIAN_POINT('Ctrl Pts',(4.98218644339902,4.57931296628774,22.5394161677055));
#189010=CARTESIAN_POINT('Ctrl Pts',(4.85632073219533,4.71625194483416,22.5481651439172));
#189011=CARTESIAN_POINT('Ctrl Pts',(4.7248061217026,4.84799861524566,22.5569141201288));
#189012=CARTESIAN_POINT('Ctrl Pts',(4.58808925235248,4.97410554898544,22.5656630963404));
#189013=CARTESIAN_POINT('Ctrl Pts',(4.45136349473985,5.10022068121262,22.5744126413421));
#189014=CARTESIAN_POINT('Ctrl Pts',(4.30943501210018,5.22069514871886,22.5831621863438));
#189015=CARTESIAN_POINT('Ctrl Pts',(4.1627858743172,5.33511975166305,22.5919117313455));
#189016=CARTESIAN_POINT('Ctrl Pts',(4.01614535740374,5.44953762807897,22.6006607619993));
#189017=CARTESIAN_POINT('Ctrl Pts',(3.86478496657836,5.55790617532845,22.609409792653));
#189018=CARTESIAN_POINT('Ctrl Pts',(3.70921874747095,5.65985735539422,22.6181588233068));
#189019=CARTESIAN_POINT('Ctrl Pts',(3.55365041605811,5.76180991977101,22.6269079727564));
#189020=CARTESIAN_POINT('Ctrl Pts',(3.39387638174445,5.85734478552857,22.635657122206));
#189021=CARTESIAN_POINT('Ctrl Pts',(3.23043927904474,5.94613749121267,22.6444062716556));
#189022=CARTESIAN_POINT('Ctrl Pts',(3.18691767070385,5.96978206944171,22.6467360795717));
#189023=CARTESIAN_POINT('Ctrl Pts',(3.14313645919605,5.99294880633439,22.6490658874879));
#189024=CARTESIAN_POINT('Ctrl Pts',(3.09910619832133,6.01563211736941,22.651395695404));
#189025=CARTESIAN_POINT('Origin',(0.,0.,4.30282021618968));
#189026=CARTESIAN_POINT('',(3.09910619832135,6.0156321173694,25.0456877277983));
#189027=CARTESIAN_POINT('',(3.09910619832136,6.01563211736939,24.6515493092843));
#189028=CARTESIAN_POINT('',(3.09910619832133,6.0156321173694,4.30282021618968));
#189029=CARTESIAN_POINT('',(-6.76699999294629,0.000308974082675706,23.6971797837786));
#189030=CARTESIAN_POINT('Ctrl Pts',(-6.76699999294632,0.000308973411543368,
23.69717978381));
#189031=CARTESIAN_POINT('Ctrl Pts',(-6.76700839696929,-0.183752247735036,
23.7057925480764));
#189032=CARTESIAN_POINT('Ctrl Pts',(-6.75950283386235,-0.367668115774533,
23.7144053123428));
#189033=CARTESIAN_POINT('Ctrl Pts',(-6.7445446979283,-0.550822855051619,
23.7230180766092));
#189034=CARTESIAN_POINT('Ctrl Pts',(-6.72956763452131,-0.734209351573671,
23.7316417391495));
#189035=CARTESIAN_POINT('Ctrl Pts',(-6.70711919469231,-0.916832496864108,
23.7402654016899));
#189036=CARTESIAN_POINT('Ctrl Pts',(-6.67731230024053,-1.0980844434999,
23.7488890642302));
#189037=CARTESIAN_POINT('Ctrl Pts',(-6.64746597549211,-1.27957616077112,
23.7575241346538));
#189038=CARTESIAN_POINT('Ctrl Pts',(-6.61024180931559,-1.45969276150695,
23.7661592050773));
#189039=CARTESIAN_POINT('Ctrl Pts',(-6.56580334377247,-1.63783865228118,
23.7747942755009));
#189040=CARTESIAN_POINT('Ctrl Pts',(-6.52126396669316,-1.81638907942465,
23.7834489545723));
#189041=CARTESIAN_POINT('Ctrl Pts',(-6.46947760092728,-1.99295955446352,
23.7921036336437));
#189042=CARTESIAN_POINT('Ctrl Pts',(-6.41065772653007,-2.16696943062896,
23.8007583127152));
#189043=CARTESIAN_POINT('Ctrl Pts',(-6.35176769229646,-2.34118686426656,
23.8094233150128));
#189044=CARTESIAN_POINT('Ctrl Pts',(-6.28582750625708,-2.51283732057656,
23.8180883173104));
#189045=CARTESIAN_POINT('Ctrl Pts',(-6.21309833977904,-2.68136122524268,
23.826753319608));
#189046=CARTESIAN_POINT('Ctrl Pts',(-6.14021525281721,-2.85024178573469,
23.8354366600966));
#189047=CARTESIAN_POINT('Ctrl Pts',(-6.06051458184177,-3.01598229024215,
23.8441200005852));
#189048=CARTESIAN_POINT('Ctrl Pts',(-5.9743039486526,-3.17804677893734,
23.8528033410738));
#189049=CARTESIAN_POINT('Ctrl Pts',(-5.91486003936267,-3.28979339775612,
23.8587906733232));
#189050=CARTESIAN_POINT('Ctrl Pts',(-5.8523219878451,-3.39979286924712,
23.8647780055727));
#189051=CARTESIAN_POINT('Ctrl Pts',(-5.78680234959432,-3.50787792927999,
23.8707653378221));
#189052=CARTESIAN_POINT('Ctrl Pts',(-5.69849954641467,-3.65354744207876,
23.8788346470446));
#189053=CARTESIAN_POINT('Ctrl Pts',(-5.60453087510633,-3.79614752730647,
23.8869039562671));
#189054=CARTESIAN_POINT('Ctrl Pts',(-5.50513669195987,-3.93519491294106,
23.8949732654896));
#189055=CARTESIAN_POINT('Ctrl Pts',(-5.40586648037442,-4.07406886869366,
23.9030325100904));
#189056=CARTESIAN_POINT('Ctrl Pts',(-5.30118443589483,-4.20939864200793,
23.9110917546911));
#189057=CARTESIAN_POINT('Ctrl Pts',(-5.19137689545073,-4.34072516169595,
23.9191509992919));
#189058=CARTESIAN_POINT('Ctrl Pts',(-5.08168221776986,-4.47191670090961,
23.9272019604122));
#189059=CARTESIAN_POINT('Ctrl Pts',(-4.96687276507901,-4.59911289086791,
23.9352529215324));
#189060=CARTESIAN_POINT('Ctrl Pts',(-4.84727823237034,-4.72188338885965,
23.9433038826527));
#189061=CARTESIAN_POINT('Ctrl Pts',(-4.72778041619019,-4.84455460190833,
23.9513483329318));
#189062=CARTESIAN_POINT('Ctrl Pts',(-4.60350548104269,-4.9628069806052,
23.9593927832109));
#189063=CARTESIAN_POINT('Ctrl Pts',(-4.47482340490097,-5.07624314773736,
23.96743723349));
#189064=CARTESIAN_POINT('Ctrl Pts',(-4.34621722711222,-5.18961240875088,
23.9754769390482));
#189065=CARTESIAN_POINT('Ctrl Pts',(-4.21320936213674,-5.29817086699351,
23.9835166446065));
#189066=CARTESIAN_POINT('Ctrl Pts',(-4.07620657592594,-5.40155801138691,
23.9915563501647));
#189067=CARTESIAN_POINT('Ctrl Pts',(-3.93624665782077,-5.50717671201804,
23.9997695884692));
#189068=CARTESIAN_POINT('Ctrl Pts',(-3.79211767990105,-5.6073980352704,
24.0079828267737));
#189069=CARTESIAN_POINT('Ctrl Pts',(-3.64428929020167,-5.7018807922756,
24.0161960650781));
#189070=CARTESIAN_POINT('Ctrl Pts',(-3.499630861829,-5.79433750620236,24.0242331826263));
#189071=CARTESIAN_POINT('Ctrl Pts',(-3.35143040432046,-5.88129907050107,
24.0322703001745));
#189072=CARTESIAN_POINT('Ctrl Pts',(-3.20015715330492,-5.96248968084234,
24.0403074177227));
#189073=CARTESIAN_POINT('Ctrl Pts',(-3.04886789854126,-6.04368888063394,
24.0483453855468));
#189074=CARTESIAN_POINT('Ctrl Pts',(-2.89450553215143,-6.11911573401304,
24.0563833533709));
#189075=CARTESIAN_POINT('Ctrl Pts',(-2.73756343398679,-6.18854065550987,
24.064421321195));
#189076=CARTESIAN_POINT('Ctrl Pts',(-2.5805736363313,-6.25798667735801,
24.0724617320027));
#189077=CARTESIAN_POINT('Ctrl Pts',(-2.42100288772765,-6.32142698527623,
24.0805021428104));
#189078=CARTESIAN_POINT('Ctrl Pts',(-2.25936391204472,-6.37868040529936,
24.0885425536182));
#189079=CARTESIAN_POINT('Ctrl Pts',(-2.09161589473576,-6.43809768168619,
24.096886846606));
#189080=CARTESIAN_POINT('Ctrl Pts',(-1.92164068113192,-6.49085112549008,
24.1052311395937));
#189081=CARTESIAN_POINT('Ctrl Pts',(-1.75002671196019,-6.53679550754235,
24.1135754325815));
#189082=CARTESIAN_POINT('Ctrl Pts',(-1.58437054058157,-6.5811448717804,
24.1216300427971));
#189083=CARTESIAN_POINT('Ctrl Pts',(-1.41718786297993,-6.61915000585643,
24.1296846530126));
#189084=CARTESIAN_POINT('Ctrl Pts',(-1.24901604404221,-6.65073288606039,
24.1377392632281));
#189085=CARTESIAN_POINT('Ctrl Pts',(-1.08071691666178,-6.68233967495084,
24.1457999708974));
#189086=CARTESIAN_POINT('Ctrl Pts',(-0.91142752395205,-6.70751447511549,
24.1538606785666));
#189087=CARTESIAN_POINT('Ctrl Pts',(-0.741688760649546,-6.72623124656937,
24.1619213862359));
#189088=CARTESIAN_POINT('Ctrl Pts',(-0.571710675859674,-6.7449744075497,
24.1699934590201));
#189089=CARTESIAN_POINT('Ctrl Pts',(-0.401282325415514,-6.75724134637748,
24.1780655318042));
#189090=CARTESIAN_POINT('Ctrl Pts',(-0.230943592428832,-6.76305804034803,
24.1861376045884));
#189091=CARTESIAN_POINT('Ctrl Pts',(-0.213101904342152,-6.76366729484757,
24.1869830928828));
#189092=CARTESIAN_POINT('Ctrl Pts',(-0.195261193462865,-6.76420583064769,
24.1878285811772));
#189093=CARTESIAN_POINT('Ctrl Pts',(-0.177422075508533,-6.76467371032205,
24.1886740694716));
#189094=CARTESIAN_POINT('Ctrl Pts',(-0.00160417208491934,-6.76928501585913,
24.1970069915184));
#189095=CARTESIAN_POINT('Ctrl Pts',(0.174619392753329,-6.7670435200554,
24.2053399135651));
#189096=CARTESIAN_POINT('Ctrl Pts',(0.350680364474882,-6.75790738927161,
24.2136728356118));
#189097=CARTESIAN_POINT('Ctrl Pts',(0.526533274823219,-6.74878205517886,
24.2219959101654));
#189098=CARTESIAN_POINT('Ctrl Pts',(0.702223630309831,-6.73277833501112,
24.230318984719));
#189099=CARTESIAN_POINT('Ctrl Pts',(0.877180786330981,-6.70990632334698,
24.2386420592726));
#189100=CARTESIAN_POINT('Ctrl Pts',(1.05196329981107,-6.68705714256514,
24.2469568257185));
#189101=CARTESIAN_POINT('Ctrl Pts',(1.22601372910066,-6.65735337434626,
24.2552715921645));
#189102=CARTESIAN_POINT('Ctrl Pts',(1.39876393947533,-6.62085707757111,
24.2635863586104));
#189103=CARTESIAN_POINT('Ctrl Pts',(1.57137339849106,-6.58439051681398,
24.27189435045));
#189104=CARTESIAN_POINT('Ctrl Pts',(1.7426844105235,-6.54114252673414,24.2802023422896));
#189105=CARTESIAN_POINT('Ctrl Pts',(1.91213623161894,-6.49122669699111,
24.2885103341291));
#189106=CARTESIAN_POINT('Ctrl Pts',(2.08148105499195,-6.44134238582405,
24.2968130800162));
#189107=CARTESIAN_POINT('Ctrl Pts',(2.24896869415922,-6.38479872366975,
24.3051158259033));
#189108=CARTESIAN_POINT('Ctrl Pts',(2.41405061273598,-6.32175993210348,
24.3134185717903));
#189109=CARTESIAN_POINT('Ctrl Pts',(2.57906506759386,-6.25874690248225,
24.3217179246098));
#189110=CARTESIAN_POINT('Ctrl Pts',(2.74167543632087,-6.18924415636571,
24.3300172774292));
#189111=CARTESIAN_POINT('Ctrl Pts',(2.90135003577383,-6.11346521785437,
24.3383166302486));
#189112=CARTESIAN_POINT('Ctrl Pts',(3.06099067511859,-6.03770239625179,
24.346614217935));
#189113=CARTESIAN_POINT('Ctrl Pts',(3.21769647498928,-5.95566619063638,
24.3549118056213));
#189114=CARTESIAN_POINT('Ctrl Pts',(3.37095714884444,-5.86761765119836,
24.3632093933076));
#189115=CARTESIAN_POINT('Ctrl Pts',(3.52421069485756,-5.77957320671872,
24.3715065950901));
#189116=CARTESIAN_POINT('Ctrl Pts',(3.67401913257895,-5.68551715906454,
24.3798037968725));
#189117=CARTESIAN_POINT('Ctrl Pts',(3.81989797014447,-5.58575585732908,
24.3881009986549));
#189118=CARTESIAN_POINT('Ctrl Pts',(3.96579426355371,-5.48598261816857,
24.3963991932795));
#189119=CARTESIAN_POINT('Ctrl Pts',(4.1077597330308,-5.38050296145721,24.404697387904));
#189120=CARTESIAN_POINT('Ctrl Pts',(4.24533984304617,-5.26966589235453,
24.4129955825286));
#189121=CARTESIAN_POINT('Ctrl Pts',(4.38301671475655,-5.15875087024924,
24.4212996133702));
#189122=CARTESIAN_POINT('Ctrl Pts',(4.51630179276322,-5.04247112521428,
24.4296036442117));
#189123=CARTESIAN_POINT('Ctrl Pts',(4.6447738641648,-4.92121577974098,24.4379076750533));
#189124=CARTESIAN_POINT('Ctrl Pts',(4.77329265154732,-4.7999163424869,24.446214725469));
#189125=CARTESIAN_POINT('Ctrl Pts',(4.89699469616931,-4.67363794283716,
24.4545217758847));
#189126=CARTESIAN_POINT('Ctrl Pts',(5.01549636385109,-4.54280587568922,
24.4628288263005));
#189127=CARTESIAN_POINT('Ctrl Pts',(5.13412472981551,-4.41183392698056,
24.4711447583551));
#189128=CARTESIAN_POINT('Ctrl Pts',(5.24754138153794,-4.27629884613848,
24.4794606904097));
#189129=CARTESIAN_POINT('Ctrl Pts',(5.35540292711717,-4.13665909741483,
24.4877766224643));
#189130=CARTESIAN_POINT('Ctrl Pts',(5.43671125122884,-4.03139568878183,
24.4940453486833));
#189131=CARTESIAN_POINT('Ctrl Pts',(5.51486374138773,-3.92380050024206,
24.5003140749022));
#189132=CARTESIAN_POINT('Ctrl Pts',(5.58972988068549,-3.8140803427526,24.5065828011212));
#189133=CARTESIAN_POINT('Ctrl Pts',(5.69064974434689,-3.66617711923118,
24.5150330698445));
#189134=CARTESIAN_POINT('Ctrl Pts',(5.78578146237337,-3.51414042581447,
24.5234833385679));
#189135=CARTESIAN_POINT('Ctrl Pts',(5.87478513907061,-3.35845032265703,
24.5319336072912));
#189136=CARTESIAN_POINT('Ctrl Pts',(5.9637102670035,-3.2028976212978,24.5403764183657));
#189137=CARTESIAN_POINT('Ctrl Pts',(6.04651796933681,-3.04369822324832,
24.5488192294402));
#189138=CARTESIAN_POINT('Ctrl Pts',(6.12291176800583,-2.88136087313196,
24.5572620405147));
#189139=CARTESIAN_POINT('Ctrl Pts',(6.19924854776807,-2.71914468858655,
24.5656985500325));
#189140=CARTESIAN_POINT('Ctrl Pts',(6.26918082619156,-2.55379551987639,
24.5741350595503));
#189141=CARTESIAN_POINT('Ctrl Pts',(6.33245799631534,-2.38584675218295,
24.582571569068));
#189142=CARTESIAN_POINT('Ctrl Pts',(6.39568988821887,-2.21801816087034,
24.5910020418092));
#189143=CARTESIAN_POINT('Ctrl Pts',(6.45227605395097,-2.04759399048648,
24.5994325145504));
#189144=CARTESIAN_POINT('Ctrl Pts',(6.50201388768062,-1.87512783681763,
24.6078629872917));
#189145=CARTESIAN_POINT('Ctrl Pts',(6.55173033925025,-1.70273582588116,
24.6162898357955));
#189146=CARTESIAN_POINT('Ctrl Pts',(6.59460423622901,-1.52830389968372,
24.6247166842993));
#189147=CARTESIAN_POINT('Ctrl Pts',(6.63048253802696,-1.35240168327296,
24.6331435328031));
#189148=CARTESIAN_POINT('Ctrl Pts',(6.66634976547441,-1.17655376159469,
24.6415677802398));
#189149=CARTESIAN_POINT('Ctrl Pts',(6.69522563768748,-0.999236779253724,
24.6499920276764));
#189150=CARTESIAN_POINT('Ctrl Pts',(6.71700794767396,-0.821031808692466,
24.658416275113));
#189151=CARTESIAN_POINT('Ctrl Pts',(6.72314536922414,-0.770820466215451,
24.660789905724));
#189152=CARTESIAN_POINT('Ctrl Pts',(6.72871994764906,-0.720538683170418,
24.6631635363349));
#189153=CARTESIAN_POINT('Ctrl Pts',(6.73373013494738,-0.670199574531021,
24.6655371669459));
#189154=CARTESIAN_POINT('Ctrl Pts',(6.75192239560458,-0.487415552479185,
24.6741559478831));
#189155=CARTESIAN_POINT('Ctrl Pts',(6.76266131817743,-0.303957112434016,
24.6827747288204));
#189156=CARTESIAN_POINT('Ctrl Pts',(6.76592810289956,-0.120440468256793,
24.6913935097576));
#189157=CARTESIAN_POINT('Ctrl Pts',(6.76919684995943,0.0631864132535379,
24.7000174679442));
#189158=CARTESIAN_POINT('Ctrl Pts',(6.764984496136,0.246871264546113,24.7086414261308));
#189159=CARTESIAN_POINT('Ctrl Pts',(6.75332436868675,0.429998803837523,
24.7172653843173));
#189160=CARTESIAN_POINT('Ctrl Pts',(6.74124300061684,0.619742116296643,
24.7262008966885));
#189161=CARTESIAN_POINT('Ctrl Pts',(6.72116572968514,0.808886738339662,
24.7351364090596));
#189162=CARTESIAN_POINT('Ctrl Pts',(6.69318809927988,0.996755771319217,
24.7440719214307));
#189163=CARTESIAN_POINT('Ctrl Pts',(6.66613547958873,1.17841338232209,24.7527120033254));
#189164=CARTESIAN_POINT('Ctrl Pts',(6.63169665312615,1.35887811205017,24.7613520852201));
#189165=CARTESIAN_POINT('Ctrl Pts',(6.59000992100219,1.53754942720316,24.7699921671148));
#189166=CARTESIAN_POINT('Ctrl Pts',(6.54618509610065,1.72538470961921,24.7790753947241));
#189167=CARTESIAN_POINT('Ctrl Pts',(6.49434945907513,1.91123739957196,24.7881586223334));
#189168=CARTESIAN_POINT('Ctrl Pts',(6.43472287136891,2.09442845871658,24.7972418499427));
#189169=CARTESIAN_POINT('Ctrl Pts',(6.37509628366268,2.27761951786121,24.8063250775521));
#189170=CARTESIAN_POINT('Ctrl Pts',(6.30767891246507,2.45814859470026,24.8154083051614));
#189171=CARTESIAN_POINT('Ctrl Pts',(6.23274904006528,2.6353611523974,24.8244915327707));
#189172=CARTESIAN_POINT('Ctrl Pts',(6.15813785911683,2.81181999031096,24.8335361276305));
#189173=CARTESIAN_POINT('Ctrl Pts',(6.07600985101772,2.98515375718911,24.8425807224903));
#189174=CARTESIAN_POINT('Ctrl Pts',(5.98663911895625,3.1547489693132,24.8516253173502));
#189175=CARTESIAN_POINT('Ctrl Pts',(5.89735039860957,3.32418855113367,24.8606616123705));
#189176=CARTESIAN_POINT('Ctrl Pts',(5.8008323345595,3.48989621735583,24.8696979073908));
#189177=CARTESIAN_POINT('Ctrl Pts',(5.69740559785817,3.65128175487656,24.8787342024111));
#189178=CARTESIAN_POINT('Ctrl Pts',(5.59416188287733,3.81238170803407,24.8877545069988));
#189179=CARTESIAN_POINT('Ctrl Pts',(5.48403403607998,3.96917460523001,24.8967748115865));
#189180=CARTESIAN_POINT('Ctrl Pts',(5.36738665833089,4.12109808909854,24.9057951161742));
#189181=CARTESIAN_POINT('Ctrl Pts',(5.2508861752956,4.27283025484989,24.9148040614404));
#189182=CARTESIAN_POINT('Ctrl Pts',(5.1278826902548,4.41970505667135,24.9238130067067));
#189183=CARTESIAN_POINT('Ctrl Pts',(4.99878326161908,4.56119007533746,24.9328219519729));
#189184=CARTESIAN_POINT('Ctrl Pts',(4.86997699045438,4.70235381147973,24.9418104398317));
#189185=CARTESIAN_POINT('Ctrl Pts',(4.73510256676615,4.83815201927206,24.9507989276906));
#189186=CARTESIAN_POINT('Ctrl Pts',(4.59460601424922,4.96808661094238,24.9597874155494));
#189187=CARTESIAN_POINT('Ctrl Pts',(4.4713396258809,5.08208633230481,24.9676735765647));
#189188=CARTESIAN_POINT('Ctrl Pts',(4.34374619449053,5.19157281657845,24.9755597375801));
#189189=CARTESIAN_POINT('Ctrl Pts',(4.21215220819276,5.29623099713531,24.9834458985954));
#189190=CARTESIAN_POINT('Ctrl Pts',(4.0766388920244,5.40400626491476,24.9915669371101));
#189191=CARTESIAN_POINT('Ctrl Pts',(3.93694281200398,5.50661181659955,24.9996879756248));
#189192=CARTESIAN_POINT('Ctrl Pts',(3.79350453484897,5.60371415617181,25.0078090141395));
#189193=CARTESIAN_POINT('Ctrl Pts',(3.65006223752656,5.70081921724678,25.0159302802638));
#189194=CARTESIAN_POINT('Ctrl Pts',(3.50287783391915,5.79242054855094,25.0240515463882));
#189195=CARTESIAN_POINT('Ctrl Pts',(3.352421546756,5.87822751965642,25.0321728125125));
#189196=CARTESIAN_POINT('Ctrl Pts',(3.26896149081178,5.92582576060665,25.0366777842744));
#189197=CARTESIAN_POINT('Ctrl Pts',(3.18449515555498,5.97164181984657,25.0411827560364));
#189198=CARTESIAN_POINT('Ctrl Pts',(3.09910619832135,6.0156321173694,25.0456877277983));
#189199=CARTESIAN_POINT('Ctrl Pts',(3.09910619832133,6.01563211736941,23.0457234660332));
#189200=CARTESIAN_POINT('Ctrl Pts',(2.93978497401097,6.09771050649808,23.0541460000253));
#189201=CARTESIAN_POINT('Ctrl Pts',(2.77718683976508,6.17346302929853,23.0625685340173));
#189202=CARTESIAN_POINT('Ctrl Pts',(2.61184465515892,6.24264018643697,23.0709910680093));
#189203=CARTESIAN_POINT('Ctrl Pts',(2.44649484453277,6.31182053420933,23.0794139904709));
#189204=CARTESIAN_POINT('Ctrl Pts',(2.27840103887654,6.37442478275776,23.0878369129326));
#189205=CARTESIAN_POINT('Ctrl Pts',(2.10811606767989,6.43025160045778,23.0962598353942));
#189206=CARTESIAN_POINT('Ctrl Pts',(1.93779946839276,6.48608878722109,23.1046843222978));
#189207=CARTESIAN_POINT('Ctrl Pts',(1.76529120912389,6.53514592952525,23.1131088092014));
#189208=CARTESIAN_POINT('Ctrl Pts',(1.59115961664177,6.57727147640786,23.121533296105));
#189209=CARTESIAN_POINT('Ctrl Pts',(1.41697136254522,6.6194107307485,23.1299605242976));
#189210=CARTESIAN_POINT('Ctrl Pts',(1.24115904616213,6.65461381438227,23.1383877524902));
#189211=CARTESIAN_POINT('Ctrl Pts',(1.06430188866369,6.68278014674932,23.1468149806829));
#189212=CARTESIAN_POINT('Ctrl Pts',(0.887285161789312,6.71097189219064,
23.1552498123424));
#189213=CARTESIAN_POINT('Ctrl Pts',(0.709222039900094,6.73211414831943,
23.163684644002));
#189214=CARTESIAN_POINT('Ctrl Pts',(0.530698714041943,6.74615800844557,
23.1721194756615));
#189215=CARTESIAN_POINT('Ctrl Pts',(0.352087138154694,6.76020881091976,
23.1805584769394));
#189216=CARTESIAN_POINT('Ctrl Pts',(0.173015237454392,6.76715420118122,
23.1889974782174));
#189217=CARTESIAN_POINT('Ctrl Pts',(-0.00592953159499168,6.76699740214632,
23.1974364794953));
#189218=CARTESIAN_POINT('Ctrl Pts',(-0.185070786124451,6.76684043094247,
23.2058847469911));
#189219=CARTESIAN_POINT('Ctrl Pts',(-0.364084296715714,6.75956569786196,
23.2143330144869));
#189220=CARTESIAN_POINT('Ctrl Pts',(-0.542385286372779,6.74522847656967,
23.2227812819826));
#189221=CARTESIAN_POINT('Ctrl Pts',(-0.627977410903571,6.73834599525178,
23.2268368128295));
#189222=CARTESIAN_POINT('Ctrl Pts',(-0.713405440737646,6.72983679143008,
23.2308923436763));
#189223=CARTESIAN_POINT('Ctrl Pts',(-0.798605406967611,6.71971118456457,
23.2349478745231));
#189224=CARTESIAN_POINT('Ctrl Pts',(-0.971704284021721,6.69913921422855,
23.2431874063739));
#189225=CARTESIAN_POINT('Ctrl Pts',(-1.14424758579368,6.6718459625022,23.2514269382247));
#189226=CARTESIAN_POINT('Ctrl Pts',(-1.31567558325423,6.63786763649507,
23.2596664700755));
#189227=CARTESIAN_POINT('Ctrl Pts',(-1.48691330761874,6.60392702405506,
23.2678968566218));
#189228=CARTESIAN_POINT('Ctrl Pts',(-1.65703784651904,6.56331618031817,
23.2761272431681));
#189229=CARTESIAN_POINT('Ctrl Pts',(-1.82549413225624,6.51612309376504,
23.2843576297144));
#189230=CARTESIAN_POINT('Ctrl Pts',(-1.99379349434351,6.46897396942656,
23.2925803493322));
#189231=CARTESIAN_POINT('Ctrl Pts',(-2.16042735747433,6.41525490893963,
23.3008030689501));
#189232=CARTESIAN_POINT('Ctrl Pts',(-2.32485030793808,6.35510503813117,
23.3090257885679));
#189233=CARTESIAN_POINT('Ctrl Pts',(-2.48912756782124,6.29500846444199,
23.3172412222637));
#189234=CARTESIAN_POINT('Ctrl Pts',(-2.65119748659542,6.22849255921135,
23.3254566559595));
#189235=CARTESIAN_POINT('Ctrl Pts',(-2.81052942031948,6.15574637046708,
23.3336720896553));
#189236=CARTESIAN_POINT('Ctrl Pts',(-2.96977946980147,6.0830375676152,23.3418833012561));
#189237=CARTESIAN_POINT('Ctrl Pts',(-3.126294013654,6.00410500553679,23.3500945128569));
#189238=CARTESIAN_POINT('Ctrl Pts',(-3.27956163182627,5.91918613519232,
23.3583057244577));
#189239=CARTESIAN_POINT('Ctrl Pts',(-3.4327778524966,5.83429574195121,23.3665141824712));
#189240=CARTESIAN_POINT('Ctrl Pts',(-3.5827490055672,5.743423211815,23.3747226404847));
#189241=CARTESIAN_POINT('Ctrl Pts',(-3.72898748627362,5.64685233800342,
23.3829310984982));
#189242=CARTESIAN_POINT('Ctrl Pts',(-3.79413992266111,5.60382790501903,
23.3865881457814));
#189243=CARTESIAN_POINT('Ctrl Pts',(-3.85855179997451,5.55967301280929,
23.3902451930646));
#189244=CARTESIAN_POINT('Ctrl Pts',(-3.92218173829601,5.51441560020437,
23.3939022403478));
#189245=CARTESIAN_POINT('Ctrl Pts',(-4.07632312607218,5.40478103870544,
23.4027613145236));
#189246=CARTESIAN_POINT('Ctrl Pts',(-4.2257136889359,5.28878780201047,23.4116203886995));
#189247=CARTESIAN_POINT('Ctrl Pts',(-4.36986620126125,5.16687123732289,
23.4204794628753));
#189248=CARTESIAN_POINT('Ctrl Pts',(-4.51428954715842,5.04472561593595,
23.4293551814694));
#189249=CARTESIAN_POINT('Ctrl Pts',(-4.65345497742721,4.91663459381182,
23.4382309000634));
#189250=CARTESIAN_POINT('Ctrl Pts',(-4.78691160083519,4.78307080501527,
23.4471066186575));
#189251=CARTESIAN_POINT('Ctrl Pts',(-4.92074907173697,4.6491258629052,23.4560076660445));
#189252=CARTESIAN_POINT('Ctrl Pts',(-5.04884495019561,4.50967708541114,
23.4649087134315));
#189253=CARTESIAN_POINT('Ctrl Pts',(-5.17078616801533,4.36523302982342,
23.4738097608185));
#189254=CARTESIAN_POINT('Ctrl Pts',(-5.2928931665935,4.22059260056061,23.4827229093015));
#189255=CARTESIAN_POINT('Ctrl Pts',(-5.40882862802352,4.07094352971808,
23.4916360577845));
#189256=CARTESIAN_POINT('Ctrl Pts',(-5.51822168701323,3.91682504242619,
23.5005492062675));
#189257=CARTESIAN_POINT('Ctrl Pts',(-5.62785762850645,3.76236436995018,
23.5094821443774));
#189258=CARTESIAN_POINT('Ctrl Pts',(-5.73092196238738,3.60341464482035,
23.5184150824873));
#189259=CARTESIAN_POINT('Ctrl Pts',(-5.82708730349631,3.44054393336752,
23.5273480205972));
#189260=CARTESIAN_POINT('Ctrl Pts',(-5.91862276483766,3.28551463133511,
23.5358508824557));
#189261=CARTESIAN_POINT('Ctrl Pts',(-6.00390780897173,3.12693316730652,
23.5443537443141));
#189262=CARTESIAN_POINT('Ctrl Pts',(-6.08270000961948,2.96530767256539,
23.5528566061726));
#189263=CARTESIAN_POINT('Ctrl Pts',(-6.16234304813474,2.80193686432688,
23.561451286216));
#189264=CARTESIAN_POINT('Ctrl Pts',(-6.23549062257036,2.63517054773899,
23.5700459662594));
#189265=CARTESIAN_POINT('Ctrl Pts',(-6.30185609129933,2.4655422942131,23.5786406463028));
#189266=CARTESIAN_POINT('Ctrl Pts',(-6.36812013874254,2.29617327061358,
23.587222191752));
#189267=CARTESIAN_POINT('Ctrl Pts',(-6.42762262986473,2.12395131678241,
23.5958037372013));
#189268=CARTESIAN_POINT('Ctrl Pts',(-6.48012336589972,1.94943329270854,
23.6043852826505));
#189269=CARTESIAN_POINT('Ctrl Pts',(-6.53251894362134,1.77526482603999,
23.6129496393722));
#189270=CARTESIAN_POINT('Ctrl Pts',(-6.57794065302999,1.59880975946691,
23.6215139960939));
#189271=CARTESIAN_POINT('Ctrl Pts',(-6.61619694518648,1.42064315804677,
23.6300783528156));
#189272=CARTESIAN_POINT('Ctrl Pts',(-6.65440773370976,1.24268847543072,
23.6386325227334));
#189273=CARTESIAN_POINT('Ctrl Pts',(-6.68547002714938,1.06302661767811,
23.6471866926511));
#189274=CARTESIAN_POINT('Ctrl Pts',(-6.70924196611391,0.882247833738351,
23.6557408625689));
#189275=CARTESIAN_POINT('Ctrl Pts',(-6.73297736412048,0.701746933312983,
23.6642818834725));
#189276=CARTESIAN_POINT('Ctrl Pts',(-6.74944472068829,0.520132838360479,
23.672822904376));
#189277=CARTESIAN_POINT('Ctrl Pts',(-6.75855317738062,0.338005840952967,
23.6813639252796));
#189278=CARTESIAN_POINT('Ctrl Pts',(-6.76417538046449,0.225587788030584,
23.6866358781126));
#189279=CARTESIAN_POINT('Ctrl Pts',(-6.76699484875476,0.112974553477846,
23.6919078309456));
#189280=CARTESIAN_POINT('Ctrl Pts',(-6.76699999294629,0.000308974082697571,
23.6971797837786));
#189281=CARTESIAN_POINT('',(-6.76699999999747,5.85319020961543E-6,23.3029481390095));
#189282=CARTESIAN_POINT('Ctrl Pts',(3.09910619832133,6.01563211736941,22.651395695404));
#189283=CARTESIAN_POINT('Ctrl Pts',(2.93375330764819,6.10081787314657,22.6601451433063));
#189284=CARTESIAN_POINT('Ctrl Pts',(2.76488627843058,6.17918207037045,22.6688945912086));
#189285=CARTESIAN_POINT('Ctrl Pts',(2.59307866646683,6.25045854554005,22.6776440391109));
#189286=CARTESIAN_POINT('Ctrl Pts',(2.42127244185357,6.32173444515044,22.6863934163612));
#189287=CARTESIAN_POINT('Ctrl Pts',(2.24652594672445,6.38592262741845,22.6951427936115));
#189288=CARTESIAN_POINT('Ctrl Pts',(2.069432696871,6.44280508110568,22.7038921708618));
#189289=CARTESIAN_POINT('Ctrl Pts',(1.89234081822056,6.49968709436173,22.7126414803672));
#189290=CARTESIAN_POINT('Ctrl Pts',(1.71290249405566,6.54926340459551,22.7213907898726));
#189291=CARTESIAN_POINT('Ctrl Pts',(1.53172716625035,6.59136563150389,22.7301400993779));
#189292=CARTESIAN_POINT('Ctrl Pts',(1.35055318107313,6.63346754640714,22.7388893440451));
#189293=CARTESIAN_POINT('Ctrl Pts',(1.167642497144,6.66809542395779,22.7476385887124));
#189294=CARTESIAN_POINT('Ctrl Pts',(0.983616340614175,6.69513165624671,
22.7563878333796));
#189295=CARTESIAN_POINT('Ctrl Pts',(0.799591486713775,6.72216769715961,
22.7651370161153));
#189296=CARTESIAN_POINT('Ctrl Pts',(0.61445145952676,6.7416121586937,22.773886198851));
#189297=CARTESIAN_POINT('Ctrl Pts',(0.428825047910446,6.75339900185711,
22.7826353815867));
#189298=CARTESIAN_POINT('Ctrl Pts',(0.243199888597073,6.76518576550221,
22.7913845052972));
#189299=CARTESIAN_POINT('Ctrl Pts',(0.05708863739181,6.76931499599835,22.8001336290078));
#189300=CARTESIAN_POINT('Ctrl Pts',(-0.128876626811393,6.76577266947846,
22.8088827527183));
#189301=CARTESIAN_POINT('Ctrl Pts',(-0.314840698188196,6.76223036567992,
22.8176318203099));
#189302=CARTESIAN_POINT('Ctrl Pts',(-0.500658497951085,6.75101660879224,
22.8263808879014));
#189303=CARTESIAN_POINT('Ctrl Pts',(-0.685698951925846,6.73216948296222,
22.8351299554929));
#189304=CARTESIAN_POINT('Ctrl Pts',(-0.870738280459626,6.71332247176297,
22.8438789698714));
#189305=CARTESIAN_POINT('Ctrl Pts',(-1.05499998761242,6.68684221356188,
22.85262798425));
#189306=CARTESIAN_POINT('Ctrl Pts',(-1.23785829161425,6.65281863948521,
22.8613769986285));
#189307=CARTESIAN_POINT('Ctrl Pts',(-1.43007412917408,6.6170539536886,22.8705737323277));
#189308=CARTESIAN_POINT('Ctrl Pts',(-1.62073882535796,6.57295372727789,
22.8797704660269));
#189309=CARTESIAN_POINT('Ctrl Pts',(-1.80913696091517,6.52068343478279,
22.8889671997261));
#189310=CARTESIAN_POINT('Ctrl Pts',(-1.98838356186115,6.47095219815198,
22.8977171974398));
#189311=CARTESIAN_POINT('Ctrl Pts',(-2.16557827572535,6.4138258685089,22.9064671951534));
#189312=CARTESIAN_POINT('Ctrl Pts',(-2.34011918621702,6.34949849943277,
22.9152171928671));
#189313=CARTESIAN_POINT('Ctrl Pts',(-2.51465655691096,6.28517243495551,
22.9239670131254));
#189314=CARTESIAN_POINT('Ctrl Pts',(-2.68653996295322,6.21364572242377,
22.9327168333837));
#189315=CARTESIAN_POINT('Ctrl Pts',(-2.85518555379979,6.13516132252225,
22.941466653642));
#189316=CARTESIAN_POINT('Ctrl Pts',(-3.02382794858676,6.05667841000513,
22.9502163080795));
#189317=CARTESIAN_POINT('Ctrl Pts',(-3.18923239109266,5.97123819492089,
22.958965962517));
#189318=CARTESIAN_POINT('Ctrl Pts',(-3.3508370596768,5.87913088810723,22.9677156169545));
#189319=CARTESIAN_POINT('Ctrl Pts',(-3.51243888042388,5.7870252044311,22.9764651172035));
#189320=CARTESIAN_POINT('Ctrl Pts',(-3.67024081223685,5.68825280605787,
22.9852146174524));
#189321=CARTESIAN_POINT('Ctrl Pts',(-3.82370687544402,5.58314917682504,
22.9939641177014));
#189322=CARTESIAN_POINT('Ctrl Pts',(-3.97717043817833,5.47804726008009,
23.0027134753918));
#189323=CARTESIAN_POINT('Ctrl Pts',(-4.12629803722495,5.3666144808421,23.0114628330823));
#189324=CARTESIAN_POINT('Ctrl Pts',(-4.27058317206957,5.24922931204536,
23.0202121907728));
#189325=CARTESIAN_POINT('Ctrl Pts',(-4.4148661477489,5.13184589986744,23.0289614175329));
#189326=CARTESIAN_POINT('Ctrl Pts',(-4.55430658194473,5.00851045722981,
23.037710644293));
#189327=CARTESIAN_POINT('Ctrl Pts',(-4.68843089001908,4.87964187103059,
23.046459871053));
#189328=CARTESIAN_POINT('Ctrl Pts',(-4.8225533691789,4.75077504207906,23.055208978509));
#189329=CARTESIAN_POINT('Ctrl Pts',(-4.95135966065179,4.61637541908045,
23.0639580859649));
#189330=CARTESIAN_POINT('Ctrl Pts',(-5.0744123086928,4.47689945401804,23.0727071934208));
#189331=CARTESIAN_POINT('Ctrl Pts',(-5.1974634422646,4.33742520555465,23.0814561931972));
#189332=CARTESIAN_POINT('Ctrl Pts',(-5.31476088454816,4.19287495491275,
23.0902051929735));
#189333=CARTESIAN_POINT('Ctrl Pts',(-5.42590627628907,4.04373961586634,
23.0989541927499));
#189334=CARTESIAN_POINT('Ctrl Pts',(-5.53706380672721,3.89458798906659,
23.1077041480446));
#189335=CARTESIAN_POINT('Ctrl Pts',(-5.64206777071916,3.74085050155205,
23.1164541033393));
#189336=CARTESIAN_POINT('Ctrl Pts',(-5.74056148164059,3.58304938223079,
23.125204058634));
#189337=CARTESIAN_POINT('Ctrl Pts',(-5.83905138951931,3.42525435593201,
23.1339536760751));
#189338=CARTESIAN_POINT('Ctrl Pts',(-5.93103139557697,3.26339625497102,
23.1427032935162));
#189339=CARTESIAN_POINT('Ctrl Pts',(-6.01618907820888,3.09802485064924,
23.1514529109573));
#189340=CARTESIAN_POINT('Ctrl Pts',(-6.10134392545025,2.93265895249554,
23.1602022370732));
#189341=CARTESIAN_POINT('Ctrl Pts',(-6.17967677261873,2.76378023985943,
23.1689515631891));
#189342=CARTESIAN_POINT('Ctrl Pts',(-6.25092157009265,2.59196229227018,
23.1777008893049));
#189343=CARTESIAN_POINT('Ctrl Pts',(-6.32216437407788,2.42014915229001,
23.1864499706074));
#189344=CARTESIAN_POINT('Ctrl Pts',(-6.3863194154895,2.24539720662769,23.1951990519098));
#189345=CARTESIAN_POINT('Ctrl Pts',(-6.44316881037561,2.06829994947613,
23.2039481332123));
#189346=CARTESIAN_POINT('Ctrl Pts',(-6.50002334524594,1.89118668024373,
23.2126980055546));
#189347=CARTESIAN_POINT('Ctrl Pts',(-6.54957082411117,1.71172794807622,
23.221447877897));
#189348=CARTESIAN_POINT('Ctrl Pts',(-6.59164294296103,1.53053334250255,
23.2301977502393));
#189349=CARTESIAN_POINT('Ctrl Pts',(-6.63371214082149,1.34935131693523,
23.2389470150942));
#189350=CARTESIAN_POINT('Ctrl Pts',(-6.66830695239702,1.16643393829695,
23.2476962799491));
#189351=CARTESIAN_POINT('Ctrl Pts',(-6.69530988153997,0.982402458340393,
23.256445544804));
#189352=CARTESIAN_POINT('Ctrl Pts',(-6.7223141969049,0.798361530946461,
23.2651952588111));
#189353=CARTESIAN_POINT('Ctrl Pts',(-6.74172580829283,0.61320667136188,
23.2739449728181));
#189354=CARTESIAN_POINT('Ctrl Pts',(-6.75347878028183,0.427566795112802,
23.2826946868251));
#189355=CARTESIAN_POINT('Ctrl Pts',(-6.76248992368218,0.285234494204722,
23.2894031966134));
#189356=CARTESIAN_POINT('Ctrl Pts',(-6.76699999999998,0.142617266091624,
23.2961117064016));
#189357=CARTESIAN_POINT('Ctrl Pts',(-6.767,9.78733067650232E-13,23.3028202161899));
#189358=CARTESIAN_POINT('Ctrl Pts',(-6.76699999999747,5.85319020961541E-6,
23.3029481390095));
#189359=CARTESIAN_POINT('Ctrl Pts',(-6.76700016116128,-0.186319119314029,
23.3117377397451));
#189360=CARTESIAN_POINT('Ctrl Pts',(-6.75930048283915,-0.372762212440499,
23.3205273404807));
#189361=CARTESIAN_POINT('Ctrl Pts',(-6.74389773019003,-0.558688110431761,
23.3293169412162));
#189362=CARTESIAN_POINT('Ctrl Pts',(-6.72852054297525,-0.744305409275513,
23.3380919530036));
#189363=CARTESIAN_POINT('Ctrl Pts',(-6.70546582398969,-0.929406947033604,
23.346866964791));
#189364=CARTESIAN_POINT('Ctrl Pts',(-6.67478228873816,-1.11335995883966,
23.3556419765784));
#189365=CARTESIAN_POINT('Ctrl Pts',(-6.64413163720242,-1.29711582717739,
23.3644075841367));
#189366=CARTESIAN_POINT('Ctrl Pts',(-6.60586852253467,-1.47972534840579,
23.373173191695));
#189367=CARTESIAN_POINT('Ctrl Pts',(-6.56009335561501,-1.66056140073645,
23.3819387992533));
#189368=CARTESIAN_POINT('Ctrl Pts',(-6.51438605881939,-1.84112933028069,
23.3906914101824));
#189369=CARTESIAN_POINT('Ctrl Pts',(-6.46118900554621,-2.0199287666356,
23.3994440211115));
#189370=CARTESIAN_POINT('Ctrl Pts',(-6.4006535329081,-2.19634317711761,
23.4081966320406));
#189371=CARTESIAN_POINT('Ctrl Pts',(-6.37673047331703,-2.26606052251466,
23.4116555830276));
#189372=CARTESIAN_POINT('Ctrl Pts',(-6.35166189231806,-2.33540549336483,
23.4151145340147));
#189373=CARTESIAN_POINT('Ctrl Pts',(-6.32545932362219,-2.40434052188975,
23.4185734850018));
#189374=CARTESIAN_POINT('Ctrl Pts',(-6.26393684423442,-2.56619693836351,
23.4266949498579));
#189375=CARTESIAN_POINT('Ctrl Pts',(-6.19617809871287,-2.7257425637015,
23.4348164147141));
#189376=CARTESIAN_POINT('Ctrl Pts',(-6.12239174810059,-2.88246566029672,
23.4429378795703));
#189377=CARTESIAN_POINT('Ctrl Pts',(-6.04861065954114,-3.03917758022842,
23.4510587652465));
#189378=CARTESIAN_POINT('Ctrl Pts',(-5.96880297808581,-3.19306704104957,
23.4591796509227));
#189379=CARTESIAN_POINT('Ctrl Pts',(-5.88322467762074,-3.3436441785325,
23.4673005365989));
#189380=CARTESIAN_POINT('Ctrl Pts',(-5.79763614810189,-3.49423931428872,
23.4754223929531));
#189381=CARTESIAN_POINT('Ctrl Pts',(-5.70627580809272,-3.64152102058143,
23.4835442493073));
#189382=CARTESIAN_POINT('Ctrl Pts',(-5.6094445389146,-3.78502588694465,
23.4916661056616));
#189383=CARTESIAN_POINT('Ctrl Pts',(-5.51254262284014,-3.92863545268345,
23.4997938876217));
#189384=CARTESIAN_POINT('Ctrl Pts',(-5.41016201047141,-4.06846237107829,
23.5079216695819));
#189385=CARTESIAN_POINT('Ctrl Pts',(-5.30264607079231,-4.20407345890993,
23.5160494515421));
#189386=CARTESIAN_POINT('Ctrl Pts',(-5.19508633311552,-4.33973978965838,
23.5241805444585));
#189387=CARTESIAN_POINT('Ctrl Pts',(-5.08238733648211,-4.47118658883518,
23.532311637375));
#189388=CARTESIAN_POINT('Ctrl Pts',(-4.96493116889428,-4.59801560329476,
23.5404427302914));
#189389=CARTESIAN_POINT('Ctrl Pts',(-4.84734680280835,-4.72498304632309,
23.548582697956));
#189390=CARTESIAN_POINT('Ctrl Pts',(-4.72499515374034,-4.84732237923032,
23.5567226656205));
#189391=CARTESIAN_POINT('Ctrl Pts',(-4.59829395183759,-4.96467337621458,
23.5648626332851));
#189392=CARTESIAN_POINT('Ctrl Pts',(-4.53258123032184,-5.02553667718263,
23.5690843724656));
#189393=CARTESIAN_POINT('Ctrl Pts',(-4.46569905689552,-5.08505882860822,
23.573306111646));
#189394=CARTESIAN_POINT('Ctrl Pts',(-4.39770895395443,-5.14319404225712,
23.5775278508265));
#189395=CARTESIAN_POINT('Ctrl Pts',(-4.26178139298135,-5.25941945531155,
23.5859680602842));
#189396=CARTESIAN_POINT('Ctrl Pts',(-4.12114276942399,-5.37033913632986,
23.5944082697418));
#189397=CARTESIAN_POINT('Ctrl Pts',(-3.97623544461375,-5.47556761340752,
23.6028484791994));
#189398=CARTESIAN_POINT('Ctrl Pts',(-3.83143790857038,-5.58071636432397,
23.6112822939479));
#189399=CARTESIAN_POINT('Ctrl Pts',(-3.68237838725329,-5.6801823115947,
23.6197161086964));
#189400=CARTESIAN_POINT('Ctrl Pts',(-3.5295320477759,-5.77362040003695,
23.628149923445));
#189401=CARTESIAN_POINT('Ctrl Pts',(-3.37677801545152,-5.86700205923167,
23.6365786448335));
#189402=CARTESIAN_POINT('Ctrl Pts',(-3.22024200812601,-5.95436294365884,
23.645007366222));
#189403=CARTESIAN_POINT('Ctrl Pts',(-3.06042821103098,-6.03540124309277,
23.6534360876106));
#189404=CARTESIAN_POINT('Ctrl Pts',(-2.90068638820505,-6.1164030458507,
23.6618610130124));
#189405=CARTESIAN_POINT('Ctrl Pts',(-2.73767001591374,-6.1910877905604,
23.6702859384141));
#189406=CARTESIAN_POINT('Ctrl Pts',(-2.5719082655142,-6.25919937961556,
23.6787108638159));
#189407=CARTESIAN_POINT('Ctrl Pts',(-2.40619573535979,-6.32729074404651,
23.6871332875736));
#189408=CARTESIAN_POINT('Ctrl Pts',(-2.23773976090506,-6.38881271851174,
23.6955557113313));
#189409=CARTESIAN_POINT('Ctrl Pts',(-2.06709025772142,-6.44355700420452,
23.7039781350891));
#189410=CARTESIAN_POINT('Ctrl Pts',(-1.89643807071232,-6.49830215086734,
23.7124006913073));
#189411=CARTESIAN_POINT('Ctrl Pts',(-1.72359260147961,-6.54626928760543,
23.7208232475255));
#189412=CARTESIAN_POINT('Ctrl Pts',(-1.54912036595553,-6.58729952953271,
23.7292458037437));
#189413=CARTESIAN_POINT('Ctrl Pts',(-1.37464223672652,-6.62833115746927,
23.7376686444774));
#189414=CARTESIAN_POINT('Ctrl Pts',(-1.19853755631639,-6.66242534683531,
23.7460914852112));
#189415=CARTESIAN_POINT('Ctrl Pts',(-1.02138466599772,-6.68947399756249,
23.7545143259449));
#189416=CARTESIAN_POINT('Ctrl Pts',(-0.844201058918017,-6.71652733828903,
23.7629386271256));
#189417=CARTESIAN_POINT('Ctrl Pts',(-0.665969209309789,-6.73653265445048,
23.7713629283062));
#189418=CARTESIAN_POINT('Ctrl Pts',(-0.487274607743674,-6.74943349153455,
23.7797872294868));
#189419=CARTESIAN_POINT('Ctrl Pts',(-0.308524066708256,-6.76233836716245,
23.7882141678536));
#189420=CARTESIAN_POINT('Ctrl Pts',(-0.129310817465469,-6.76813430560661,
23.7966411062205));
#189421=CARTESIAN_POINT('Ctrl Pts',(0.0497772355627528,-6.76681691985381,
23.8050680445873));
#189422=CARTESIAN_POINT('Ctrl Pts',(0.229026311261498,-6.76549834960562,
23.8135025598309));
#189423=CARTESIAN_POINT('Ctrl Pts',(0.408149631944036,-6.75705367785012,
23.8219370750746));
#189424=CARTESIAN_POINT('Ctrl Pts',(0.586560849915647,-6.74153063994715,
23.8303715903183));
#189425=CARTESIAN_POINT('Ctrl Pts',(0.765058242033914,-6.7260001042839,
23.838810179505));
#189426=CARTESIAN_POINT('Ctrl Pts',(0.942842514119942,-6.70338442082986,
23.8472487686918));
#189427=CARTESIAN_POINT('Ctrl Pts',(1.1193345924047,-6.67378296547365,23.8556873578786));
#189428=CARTESIAN_POINT('Ctrl Pts',(1.29602394890242,-6.64414842238755,
23.8641353794989));
#189429=CARTESIAN_POINT('Ctrl Pts',(1.47141789791735,-6.60751256786978,
23.8725834011192));
#189430=CARTESIAN_POINT('Ctrl Pts',(1.64494846641265,-6.56402571162291,
23.8810314227395));
#189431=CARTESIAN_POINT('Ctrl Pts',(1.74358045666669,-6.53930848042433,
23.8858331426517));
#189432=CARTESIAN_POINT('Ctrl Pts',(1.84161072736434,-6.51237887841011,
23.8906348625639));
#189433=CARTESIAN_POINT('Ctrl Pts',(1.93893746026169,-6.48327159119483,
23.895436582476));
#189434=CARTESIAN_POINT('Ctrl Pts',(2.10594568446213,-6.43332481702085,
23.9036761143269));
#189435=CARTESIAN_POINT('Ctrl Pts',(2.27125413310745,-6.37685155447372,
23.9119156461777));
#189436=CARTESIAN_POINT('Ctrl Pts',(2.43431757415674,-6.31398344534982,
23.9201551780285));
#189437=CARTESIAN_POINT('Ctrl Pts',(2.59720002618313,-6.25118511543314,
23.9283855645748));
#189438=CARTESIAN_POINT('Ctrl Pts',(2.75784210305396,-6.18200619881975,
23.9366159511212));
#189439=CARTESIAN_POINT('Ctrl Pts',(2.91571204343896,-6.10662855262583,
23.9448463376675));
#189440=CARTESIAN_POINT('Ctrl Pts',(3.07343492177095,-6.03132112367132,
23.9530690572853));
#189441=CARTESIAN_POINT('Ctrl Pts',(3.22839048713255,-5.9498266173217,23.9612917769032));
#189442=CARTESIAN_POINT('Ctrl Pts',(3.38006525720238,-5.86237561548673,
23.969514496521));
#189443=CARTESIAN_POINT('Ctrl Pts',(3.53160563249717,-5.77500210154057,
23.9777299302168));
#189444=CARTESIAN_POINT('Ctrl Pts',(3.67987069931387,-5.68168278852421,
23.9859453639126));
#189445=CARTESIAN_POINT('Ctrl Pts',(3.82437008601423,-5.58269490884103,
23.9941607976084));
#189446=CARTESIAN_POINT('Ctrl Pts',(3.96879521125185,-5.48375790124047,
24.0023720092093));
#189447=CARTESIAN_POINT('Ctrl Pts',(4.10945821772749,-5.3791583295227,24.0105832208102));
#189448=CARTESIAN_POINT('Ctrl Pts',(4.24589597215357,-5.2692178161137,24.0187944324111));
#189449=CARTESIAN_POINT('Ctrl Pts',(4.38228797288418,-5.15931417068741,
24.0270028904246));
#189450=CARTESIAN_POINT('Ctrl Pts',(4.51445726735109,-5.04407337458221,
24.0352113484381));
#189451=CARTESIAN_POINT('Ctrl Pts',(4.64197213069801,-4.92385862285088,
24.0434198064517));
#189452=CARTESIAN_POINT('Ctrl Pts',(4.69878278670445,-4.87030032597276,
24.0470768537347));
#189453=CARTESIAN_POINT('Ctrl Pts',(4.75467002245515,-4.81575528655811,
24.0507339010178));
#189454=CARTESIAN_POINT('Ctrl Pts',(4.80959786119915,-4.7602581246765,24.0543909483008));
#189455=CARTESIAN_POINT('Ctrl Pts',(4.94265870512388,-4.62581811457868,
24.0632500224767));
#189456=CARTESIAN_POINT('Ctrl Pts',(5.06994882290606,-4.48592816802374,
24.0721090966526));
#189457=CARTESIAN_POINT('Ctrl Pts',(5.19106284858699,-4.34110072470334,
24.0809681708285));
#189458=CARTESIAN_POINT('Ctrl Pts',(5.31240442315599,-4.19600117975389,
24.0898438894224));
#189459=CARTESIAN_POINT('Ctrl Pts',(5.42754655013052,-4.04594579822502,
24.0987196080164));
#189460=CARTESIAN_POINT('Ctrl Pts',(5.53612605306277,-3.89147752461706,
24.1075953266103));
#189461=CARTESIAN_POINT('Ctrl Pts',(5.64501541121713,-3.73656844220137,
24.1164963739973));
#189462=CARTESIAN_POINT('Ctrl Pts',(5.74730451823662,-3.57722148048661,
24.1253974213843));
#189463=CARTESIAN_POINT('Ctrl Pts',(5.84267361997403,-3.41400849009776,
24.1342984687713));
#189464=CARTESIAN_POINT('Ctrl Pts',(5.93817237731328,-3.25057360940993,
24.1432116172543));
#189465=CARTESIAN_POINT('Ctrl Pts',(6.02673221148577,-3.08326242809785,
24.1521247657373));
#189466=CARTESIAN_POINT('Ctrl Pts',(6.10808020456531,-2.91266977438181,
24.1610379142203));
#189467=CARTESIAN_POINT('Ctrl Pts',(6.18960881243379,-2.74169835832662,
24.1699708523301));
#189468=CARTESIAN_POINT('Ctrl Pts',(6.2638934397176,-2.56743113195713,24.17890379044));
#189469=CARTESIAN_POINT('Ctrl Pts',(6.33070894983138,-2.39048388250683,
24.1878367285499));
#189470=CARTESIAN_POINT('Ctrl Pts',(6.39430762761436,-2.22205575731238,
24.1963395904085));
#189471=CARTESIAN_POINT('Ctrl Pts',(6.45113939758644,-2.05119976704901,
24.204842452267));
#189472=CARTESIAN_POINT('Ctrl Pts',(6.50105254746634,-1.87845808446219,
24.2133453141256));
#189473=CARTESIAN_POINT('Ctrl Pts',(6.5493212428263,-1.71140760432196,24.2215680379914));
#189474=CARTESIAN_POINT('Ctrl Pts',(6.59121125434896,-1.54227318927006,
24.2297907618573));
#189475=CARTESIAN_POINT('Ctrl Pts',(6.62654128339385,-1.37158288829985,
24.2380134857232));
#189476=CARTESIAN_POINT('Ctrl Pts',(6.66183391679992,-1.20107325723056,
24.2462275061144));
#189477=CARTESIAN_POINT('Ctrl Pts',(6.69058032240031,-1.02901136801331,
24.2544415265056));
#189478=CARTESIAN_POINT('Ctrl Pts',(6.71264883432086,-0.855940784803948,
24.2626555468968));
#189479=CARTESIAN_POINT('Ctrl Pts',(6.73469841820239,-0.683018643264092,
24.2708625221688));
#189480=CARTESIAN_POINT('Ctrl Pts',(6.75008147028002,-0.509089884581408,
24.2790694974408));
#189481=CARTESIAN_POINT('Ctrl Pts',(6.7587172651216,-0.334708724336901,
24.2872764727127));
#189482=CARTESIAN_POINT('Ctrl Pts',(6.7673473864183,-0.160442129034876,
24.2954780561657));
#189483=CARTESIAN_POINT('Ctrl Pts',(6.76923906243111,0.0142759188046485,
24.3036796396187));
#189484=CARTESIAN_POINT('Ctrl Pts',(6.76436332995802,0.188885521730087,
24.3118812230717));
#189485=CARTESIAN_POINT('Ctrl Pts',(6.75948982231459,0.363415449114437,
24.3200790640867));
#189486=CARTESIAN_POINT('Ctrl Pts',(6.74785506825636,0.537836672324922,
24.3282769051018));
#189487=CARTESIAN_POINT('Ctrl Pts',(6.72948219473935,0.7115886386713,24.3364747461168));
#189488=CARTESIAN_POINT('Ctrl Pts',(6.7111109425711,0.88532527194889,24.344671863698));
#189489=CARTESIAN_POINT('Ctrl Pts',(6.68600278450453,1.05839240863413,24.3528689812792));
#189490=CARTESIAN_POINT('Ctrl Pts',(6.65423281064427,1.23023359641381,24.3610660988603));
#189491=CARTESIAN_POINT('Ctrl Pts',(6.62246319026041,1.40207287226859,24.3692631252394));
#189492=CARTESIAN_POINT('Ctrl Pts',(6.58403196589232,1.57268587333772,24.3774601516185));
#189493=CARTESIAN_POINT('Ctrl Pts',(6.5390655364396,1.74152545492391,24.3856571779976));
#189494=CARTESIAN_POINT('Ctrl Pts',(6.49409143102741,1.91039385813992,24.3938556036437));
#189495=CARTESIAN_POINT('Ctrl Pts',(6.44257999030012,2.07748789198836,24.4020540292899));
#189496=CARTESIAN_POINT('Ctrl Pts',(6.38470777286537,2.24227466094422,24.410252454936));
#189497=CARTESIAN_POINT('Ctrl Pts',(6.32681515336021,2.40711952325493,24.4184537708266));
#189498=CARTESIAN_POINT('Ctrl Pts',(6.26255740908018,2.56965516202733,24.4266550867172));
#189499=CARTESIAN_POINT('Ctrl Pts',(6.19215962156899,2.72936773282945,24.4348564026078));
#189500=CARTESIAN_POINT('Ctrl Pts',(6.12168166276171,2.88926218951544,24.4430670584244));
#189501=CARTESIAN_POINT('Ctrl Pts',(6.04504983587016,3.04632682653853,24.451277714241));
#189502=CARTESIAN_POINT('Ctrl Pts',(5.96253614336249,3.2000705834553,24.4594883700576));
#189503=CARTESIAN_POINT('Ctrl Pts',(5.87997382753456,3.3539049378439,24.4677038642148));
#189504=CARTESIAN_POINT('Ctrl Pts',(5.79152291857737,3.50441420246484,24.4759193583719));
#189505=CARTESIAN_POINT('Ctrl Pts',(5.69749925772981,3.65113560528342,24.4841348525291));
#189506=CARTESIAN_POINT('Ctrl Pts',(5.60332971744261,3.79808464905782,24.4923630931766));
#189507=CARTESIAN_POINT('Ctrl Pts',(5.5035703517247,3.94123379239337,24.5005913338241));
#189508=CARTESIAN_POINT('Ctrl Pts',(5.39857866451535,4.0801516397114,24.5088195744716));
#189509=CARTESIAN_POINT('Ctrl Pts',(5.30315798287738,4.20640578454037,24.5162977315728));
#189510=CARTESIAN_POINT('Ctrl Pts',(5.20341608243987,4.32916519283054,24.5237758886739));
#189511=CARTESIAN_POINT('Ctrl Pts',(5.09964747685195,4.44813271068182,24.5312540457751));
#189512=CARTESIAN_POINT('Ctrl Pts',(4.98765384404185,4.57652996951629,24.5393249452127));
#189513=CARTESIAN_POINT('Ctrl Pts',(4.8706025363177,4.70093021253803,24.5473958446503));
#189514=CARTESIAN_POINT('Ctrl Pts',(4.74881340549579,4.82089828141846,24.555466744088));
#189515=CARTESIAN_POINT('Ctrl Pts',(4.62721738093441,4.94067613147553,24.5635248464788));
#189516=CARTESIAN_POINT('Ctrl Pts',(4.50089875728203,5.05603554475185,24.5715829488696));
#189517=CARTESIAN_POINT('Ctrl Pts',(4.37021819506817,5.16657351902546,24.5796410512604));
#189518=CARTESIAN_POINT('Ctrl Pts',(4.23965646947264,5.27701097368975,24.5876918258771));
#189519=CARTESIAN_POINT('Ctrl Pts',(4.10474097640636,5.38263547036333,24.5957426004938));
#189520=CARTESIAN_POINT('Ctrl Pts',(3.96587028875585,5.48307959569835,24.6037933751105));
#189521=CARTESIAN_POINT('Ctrl Pts',(3.82711688633064,5.58343888951083,24.6118373503304));
#189522=CARTESIAN_POINT('Ctrl Pts',(3.68441523993815,5.67862630420322,24.6198813255502));
#189523=CARTESIAN_POINT('Ctrl Pts',(3.53819790618462,5.76831384172799,24.6279253007701));
#189524=CARTESIAN_POINT('Ctrl Pts',(3.39505808443007,5.85611367917093,24.6357999702748));
#189525=CARTESIAN_POINT('Ctrl Pts',(3.24854938851748,5.93864264926404,24.6436746397796));
#189526=CARTESIAN_POINT('Ctrl Pts',(3.09910619832136,6.01563211736939,24.6515493092843));
#189527=CARTESIAN_POINT('Origin',(0.,0.,4.30282021618968));
#189528=CARTESIAN_POINT('',(3.09910619832137,6.01563211736939,27.0457199708935));
#189529=CARTESIAN_POINT('',(3.0991061983213,6.01563211736942,26.6512942524228));
#189530=CARTESIAN_POINT('',(3.09910619832133,6.0156321173694,4.30282021618968));
#189531=CARTESIAN_POINT('',(-6.76699810037806,-0.00507045163499823,25.6971797837853));
#189532=CARTESIAN_POINT('Ctrl Pts',(-6.76699810037766,-0.00507045216101548,
25.6971797838101));
#189533=CARTESIAN_POINT('Ctrl Pts',(-6.76683316558664,-0.225191534474847,
25.7075416747608));
#189534=CARTESIAN_POINT('Ctrl Pts',(-6.75592406321113,-0.444938118573672,
25.7179035657114));
#189535=CARTESIAN_POINT('Ctrl Pts',(-6.73440294215104,-0.663404863373404,
25.7282654566621));
#189536=CARTESIAN_POINT('Ctrl Pts',(-6.71261506930177,-0.884579478032097,
25.7387557820444));
#189537=CARTESIAN_POINT('Ctrl Pts',(-6.67995048580069,-1.10444249683336,
25.7492461074266));
#189538=CARTESIAN_POINT('Ctrl Pts',(-6.63659636700349,-1.32207324361249,
25.7597364328088));
#189539=CARTESIAN_POINT('Ctrl Pts',(-6.61113671010138,-1.44987665187149,
25.7658968644456));
#189540=CARTESIAN_POINT('Ctrl Pts',(-6.58199158231211,-1.576910575339,25.7720572960824));
#189541=CARTESIAN_POINT('Ctrl Pts',(-6.54920683200501,-1.70299115429851,
25.7782177277192));
#189542=CARTESIAN_POINT('Ctrl Pts',(-6.50544691960259,-1.87127900274119,
25.7864404515851));
#189543=CARTESIAN_POINT('Ctrl Pts',(-6.45513814673142,-2.03810301418025,
25.794663175451));
#189544=CARTESIAN_POINT('Ctrl Pts',(-6.39839414167517,-2.20291656850116,
25.8028858993169));
#189545=CARTESIAN_POINT('Ctrl Pts',(-6.34171019822605,-2.36755567325794,
25.8110999197081));
#189546=CARTESIAN_POINT('Ctrl Pts',(-6.27860470223396,-2.530188222065,25.8193139400993));
#189547=CARTESIAN_POINT('Ctrl Pts',(-6.20924188159528,-2.69027958692831,
25.8275279604905));
#189548=CARTESIAN_POINT('Ctrl Pts',(-6.13993855305911,-2.85023364232524,
25.8357349357625));
#189549=CARTESIAN_POINT('Ctrl Pts',(-6.06438873027047,-3.00765052726698,
25.8439419110344));
#189550=CARTESIAN_POINT('Ctrl Pts',(-5.98280588265044,-3.16201245578244,
25.8521488863064));
#189551=CARTESIAN_POINT('Ctrl Pts',(-5.90127663333316,-3.31627297159146,
25.8603504697594));
#189552=CARTESIAN_POINT('Ctrl Pts',(-5.81372242117327,-3.46748221275153,
25.8685520532124));
#189553=CARTESIAN_POINT('Ctrl Pts',(-5.72040412719173,-3.6151439282009,
25.8767536366654));
#189554=CARTESIAN_POINT('Ctrl Pts',(-5.6271284149782,-3.76273826461189,
25.8849514776804));
#189555=CARTESIAN_POINT('Ctrl Pts',(-5.52809405216928,-3.90678799766012,
25.8931493186955));
#189556=CARTESIAN_POINT('Ctrl Pts',(-5.42360704764637,-4.04682290108186,
25.9013471597106));
#189557=CARTESIAN_POINT('Ctrl Pts',(-5.31912926377572,-4.18684544686014,
25.9095442772917));
#189558=CARTESIAN_POINT('Ctrl Pts',(-5.20920000412085,-4.32285357629932,
25.9177413948729));
#189559=CARTESIAN_POINT('Ctrl Pts',(-5.09416786880838,-4.45440711255721,
25.925938512454));
#189560=CARTESIAN_POINT('Ctrl Pts',(-4.9791370133565,-4.58595918513554,
25.9341355388331));
#189561=CARTESIAN_POINT('Ctrl Pts',(-4.85900363072451,-4.71305649241487,
25.9423325652122));
#189562=CARTESIAN_POINT('Ctrl Pts',(-4.73415569167384,-4.83529305078732,
25.9505295915913));
#189563=CARTESIAN_POINT('Ctrl Pts',(-4.6092864405524,-4.95755047545683,
25.9587280172374));
#189564=CARTESIAN_POINT('Ctrl Pts',(-4.4797012860301,-5.07494524706564,
25.9669264428836));
#189565=CARTESIAN_POINT('Ctrl Pts',(-4.345824059073,-5.18710923806144,25.9751248685297));
#189566=CARTESIAN_POINT('Ctrl Pts',(-4.21189963550303,-5.29931277096127,
25.9833261844204));
#189567=CARTESIAN_POINT('Ctrl Pts',(-4.07368040025147,-5.40628161959457,
25.991527500311));
#189568=CARTESIAN_POINT('Ctrl Pts',(-3.93162218596216,-5.50768880628256,
25.9997288162017));
#189569=CARTESIAN_POINT('Ctrl Pts',(-3.78940219114661,-5.60921147878112,
26.0079394720183));
#189570=CARTESIAN_POINT('Ctrl Pts',(-3.64333477526494,-5.70515962682792,
26.0161501278349));
#189571=CARTESIAN_POINT('Ctrl Pts',(-3.49390448966299,-5.79524981490124,
26.0243607836515));
#189572=CARTESIAN_POINT('Ctrl Pts',(-3.34438614841412,-5.88539309093968,
26.0325762778086));
#189573=CARTESIAN_POINT('Ctrl Pts',(-3.19150130104384,-5.9696713531215,
26.0407917719657));
#189574=CARTESIAN_POINT('Ctrl Pts',(-3.03575775758443,-6.04784786823098,
26.0490072661229));
#189575=CARTESIAN_POINT('Ctrl Pts',(-2.87977257515131,-6.12614567564227,
26.0572355067704));
#189576=CARTESIAN_POINT('Ctrl Pts',(-2.72092015958877,-6.19832266890245,
26.0654637474179));
#189577=CARTESIAN_POINT('Ctrl Pts',(-2.55972813214299,-6.2641903618517,
26.0736919880654));
#189578=CARTESIAN_POINT('Ctrl Pts',(-2.41323031367543,-6.32405357889451,
26.0811701451665));
#189579=CARTESIAN_POINT('Ctrl Pts',(-2.26480039920582,-6.37870593032523,
26.0886483022676));
#189580=CARTESIAN_POINT('Ctrl Pts',(-2.1148433226718,-6.42804221521223,
26.0961264593687));
#189581=CARTESIAN_POINT('Ctrl Pts',(-1.95303206298607,-6.48127855850656,
26.1041957685913));
#189582=CARTESIAN_POINT('Ctrl Pts',(-1.78891270112995,-6.52849858136089,
26.1122650778138));
#189583=CARTESIAN_POINT('Ctrl Pts',(-1.62298210502701,-6.56949146332972,
26.1203343870363));
#189584=CARTESIAN_POINT('Ctrl Pts',(-1.45725846947591,-6.61043321603323,
26.1283936316371));
#189585=CARTESIAN_POINT('Ctrl Pts',(-1.28972845234976,-6.64516319362522,
26.1364528762378));
#189586=CARTESIAN_POINT('Ctrl Pts',(-1.12090811357158,-6.67351886195952,
26.1445121208386));
#189587=CARTESIAN_POINT('Ctrl Pts',(-0.952261292294172,-6.70184538567333,
26.1525630819588));
#189588=CARTESIAN_POINT('Ctrl Pts',(-0.782327153444256,-6.72381057677971,
26.1606140430791));
#189589=CARTESIAN_POINT('Ctrl Pts',(-0.611636012282423,-6.73930192145145,
26.1686650041994));
#189590=CARTESIAN_POINT('Ctrl Pts',(-0.441082909659608,-6.75478073821712,
26.1767094544785));
#189591=CARTESIAN_POINT('Ctrl Pts',(-0.269774392908001,-6.76379609521643,
26.1847539047576));
#189592=CARTESIAN_POINT('Ctrl Pts',(-0.0982499412038178,-6.76628671791652,
26.1927983550367));
#189593=CARTESIAN_POINT('Ctrl Pts',(0.0731733431595497,-6.76877587161511,
26.2008380605949));
#189594=CARTESIAN_POINT('Ctrl Pts',(0.24481193678314,-6.76474794657301,
26.2088777661531));
#189595=CARTESIAN_POINT('Ctrl Pts',(0.416122388243194,-6.75419359790662,
26.2169174717114));
#189596=CARTESIAN_POINT('Ctrl Pts',(0.591130484210459,-6.74341143926693,
26.2251307100158));
#189597=CARTESIAN_POINT('Ctrl Pts',(0.765795714195148,-6.72581787950676,
26.2333439483203));
#189598=CARTESIAN_POINT('Ctrl Pts',(0.939539422656506,-6.70145914508731,
26.2415571866247));
#189599=CARTESIAN_POINT('Ctrl Pts',(1.10955745408304,-6.67762274772528,
26.2495943041729));
#189600=CARTESIAN_POINT('Ctrl Pts',(1.27869270165765,-6.64730843924124,
26.2576314217211));
#189601=CARTESIAN_POINT('Ctrl Pts',(1.4464093433712,-6.61061184849092,26.2656685392693));
#189602=CARTESIAN_POINT('Ctrl Pts',(1.61414372843899,-6.57391137547463,
26.2737065070934));
#189603=CARTESIAN_POINT('Ctrl Pts',(1.78045884378302,-6.53082735551139,
26.2817444749175));
#189604=CARTESIAN_POINT('Ctrl Pts',(1.94483058238538,-6.48150622971378,
26.2897824427416));
#189605=CARTESIAN_POINT('Ctrl Pts',(2.10925227857359,-6.4321701137214,26.2978228535493));
#189606=CARTESIAN_POINT('Ctrl Pts',(2.27172906468335,-6.37659322595046,
26.3058632643571));
#189607=CARTESIAN_POINT('Ctrl Pts',(2.43175362115301,-6.31497136383129,
26.3139036751648));
#189608=CARTESIAN_POINT('Ctrl Pts',(2.59782620330735,-6.2510205428757,26.3222479681526));
#189609=CARTESIAN_POINT('Ctrl Pts',(2.76125715770875,-6.18055904831102,
26.3305922611404));
#189610=CARTESIAN_POINT('Ctrl Pts',(2.92150502034155,-6.10385922315703,
26.3389365541282));
#189611=CARTESIAN_POINT('Ctrl Pts',(3.0761896740647,-6.02982213024579,26.3469911643437));
#189612=CARTESIAN_POINT('Ctrl Pts',(3.22790824848203,-5.94997282165125,
26.3550457745593));
#189613=CARTESIAN_POINT('Ctrl Pts',(3.3762017846964,-5.86460147912992,26.3631003847748));
#189614=CARTESIAN_POINT('Ctrl Pts',(3.52460758121271,-5.77916550929621,
26.3711610924441));
#189615=CARTESIAN_POINT('Ctrl Pts',(3.6695828627128,-5.68819937932786,26.3792218001133));
#189616=CARTESIAN_POINT('Ctrl Pts',(3.81069979433565,-5.59203505688673,
26.3872825077826));
#189617=CARTESIAN_POINT('Ctrl Pts',(3.95201569237733,-5.49573514851249,
26.3953545805667));
#189618=CARTESIAN_POINT('Ctrl Pts',(4.08946208910927,-5.39422264460989,
26.4034266533509));
#189619=CARTESIAN_POINT('Ctrl Pts',(4.22264574554371,-5.28786837086946,
26.411498726135));
#189620=CARTESIAN_POINT('Ctrl Pts',(4.23659572165705,-5.27672856874997,
26.4123442144294));
#189621=CARTESIAN_POINT('Ctrl Pts',(4.25049896631731,-5.26553567933751,
26.4131897027239));
#189622=CARTESIAN_POINT('Ctrl Pts',(4.26435505247544,-5.25429015057478,
26.4140351910183));
#189623=CARTESIAN_POINT('Ctrl Pts',(4.40091718655803,-5.14345701997803,
26.422368113065));
#189624=CARTESIAN_POINT('Ctrl Pts',(4.53333104155898,-5.02715422503498,
26.4307010351117));
#189625=CARTESIAN_POINT('Ctrl Pts',(4.66113772746193,-4.90571952781965,
26.4390339571584));
#189626=CARTESIAN_POINT('Ctrl Pts',(4.78879337685559,-4.7844283369682,26.447357031712));
#189627=CARTESIAN_POINT('Ctrl Pts',(4.91185245304282,-4.65801756275112,
26.4556801062656));
#189628=CARTESIAN_POINT('Ctrl Pts',(5.02988801979945,-4.5268659697718,26.4640031808192));
#189629=CARTESIAN_POINT('Ctrl Pts',(5.14780576324589,-4.3958452925431,26.4723179472652));
#189630=CARTESIAN_POINT('Ctrl Pts',(5.26070975639224,-4.26009348182202,
26.4806327137112));
#189631=CARTESIAN_POINT('Ctrl Pts',(5.3682087626124,-4.12002714566439,26.4889474801571));
#189632=CARTESIAN_POINT('Ctrl Pts',(5.47562018207194,-3.98007493108879,
26.4972554719967));
#189633=CARTESIAN_POINT('Ctrl Pts',(5.57763517863231,-3.8358154705114,26.5055634638362));
#189634=CARTESIAN_POINT('Ctrl Pts',(5.67390164120109,-3.6876997120123,26.5138714556757));
#189635=CARTESIAN_POINT('Ctrl Pts',(5.77010731780679,-3.53967747890914,
26.5221742015628));
#189636=CARTESIAN_POINT('Ctrl Pts',(5.86057150514518,-3.38780409146745,
26.5304769474499));
#189637=CARTESIAN_POINT('Ctrl Pts',(5.94498429228834,-3.23256102254002,
26.538779693337));
#189638=CARTESIAN_POINT('Ctrl Pts',(6.02936258261544,-3.07738139650758,
26.5470790461564));
#189639=CARTESIAN_POINT('Ctrl Pts',(6.10769423447064,-2.91883513810672,
26.5553783989759));
#189640=CARTESIAN_POINT('Ctrl Pts',(6.17971420174618,-2.75743021393771,
26.5636777517953));
#189641=CARTESIAN_POINT('Ctrl Pts',(6.25171885158313,-2.59605961788781,
26.5719753394816));
#189642=CARTESIAN_POINT('Ctrl Pts',(6.31741434950007,-2.43183188485109,
26.580272927168));
#189643=CARTESIAN_POINT('Ctrl Pts',(6.37658281042349,-2.26527717107899,
26.5885705148543));
#189644=CARTESIAN_POINT('Ctrl Pts',(6.43574851954211,-2.09873020342796,
26.5968677166367));
#189645=CARTESIAN_POINT('Ctrl Pts',(6.48838768027942,-1.92985679856605,
26.6051649184192));
#189646=CARTESIAN_POINT('Ctrl Pts',(6.534331461314,-1.75920475035799,26.6134621202016));
#189647=CARTESIAN_POINT('Ctrl Pts',(6.58028073997568,-1.58853228194713,
26.6217603148261));
#189648=CARTESIAN_POINT('Ctrl Pts',(6.61953295265388,-1.41608108217307,
26.6300585094507));
#189649=CARTESIAN_POINT('Ctrl Pts',(6.65196976459586,-1.24241186846493,
26.6383567040752));
#189650=CARTESIAN_POINT('Ctrl Pts',(6.68442938972586,-1.06862051117402,
26.6466607349168));
#189651=CARTESIAN_POINT('Ctrl Pts',(6.71006397210905,-0.893609770615906,
26.6549647657583));
#189652=CARTESIAN_POINT('Ctrl Pts',(6.72880657986409,-0.717949170051566,
26.6632687965999));
#189653=CARTESIAN_POINT('Ctrl Pts',(6.74755600294716,-0.542224694458191,
26.6715758470157));
#189654=CARTESIAN_POINT('Ctrl Pts',(6.7594084268463,-0.365850234545319,
26.6798828974314));
#189655=CARTESIAN_POINT('Ctrl Pts',(6.76434899034665,-0.189398354787832,
26.6881899478471));
#189656=CARTESIAN_POINT('Ctrl Pts',(6.7692948361432,-0.012757818190803,
26.6965058799017));
#189657=CARTESIAN_POINT('Ctrl Pts',(6.76731405399805,0.16395995547355,26.7048218119564));
#189658=CARTESIAN_POINT('Ctrl Pts',(6.75844392386799,0.340183373979205,
26.713137744011));
#189659=CARTESIAN_POINT('Ctrl Pts',(6.75175743136825,0.47302432995617,26.7194064702299));
#189660=CARTESIAN_POINT('Ctrl Pts',(6.74115717014622,0.605584394745327,
26.7256751964489));
#189661=CARTESIAN_POINT('Ctrl Pts',(6.72667848189171,0.73762158404906,26.7319439226678));
#189662=CARTESIAN_POINT('Ctrl Pts',(6.70716115058081,0.915608258235449,
26.7403941913911));
#189663=CARTESIAN_POINT('Ctrl Pts',(6.6805587082356,1.09297090926716,26.7488444601145));
#189664=CARTESIAN_POINT('Ctrl Pts',(6.64692513480987,1.26912381280664,26.7572947288378));
#189665=CARTESIAN_POINT('Ctrl Pts',(6.61332124415374,1.44512125543255,26.7657375399124));
#189666=CARTESIAN_POINT('Ctrl Pts',(6.57269865242034,1.61991075439046,26.7741803509869));
#189667=CARTESIAN_POINT('Ctrl Pts',(6.52516297638257,1.79291302958236,26.7826231620614));
#189668=CARTESIAN_POINT('Ctrl Pts',(6.47766278008718,1.96578617910136,26.7910596715791));
#189669=CARTESIAN_POINT('Ctrl Pts',(6.4232598728177,2.13687444532391,26.7994961810969));
#189670=CARTESIAN_POINT('Ctrl Pts',(6.36211074219677,2.30560965994344,26.8079326906146));
#189671=CARTESIAN_POINT('Ctrl Pts',(6.30100536706913,2.47422413543755,26.8163631633558));
#189672=CARTESIAN_POINT('Ctrl Pts',(6.23316351008926,2.64048860682208,26.824793636097));
#189673=CARTESIAN_POINT('Ctrl Pts',(6.15879126699945,2.80385076805656,26.8332241088383));
#189674=CARTESIAN_POINT('Ctrl Pts',(6.08445099633536,2.96714270034071,26.8416509573421));
#189675=CARTESIAN_POINT('Ctrl Pts',(6.00358607333728,3.12753450857203,26.8500778058459));
#189676=CARTESIAN_POINT('Ctrl Pts',(5.91645067090267,3.28449394256945,26.8585046543498));
#189677=CARTESIAN_POINT('Ctrl Pts',(5.82934216405502,3.4414049287949,26.8669289017864));
#189678=CARTESIAN_POINT('Ctrl Pts',(5.73596719831479,3.59488536401621,26.875353149223));
#189679=CARTESIAN_POINT('Ctrl Pts',(5.63662600763035,3.74442735943764,26.8837773966597));
#189680=CARTESIAN_POINT('Ctrl Pts',(5.60863546094804,3.78656257218244,26.8861510272706));
#189681=CARTESIAN_POINT('Ctrl Pts',(5.58017153174439,3.82838527373419,26.8885246578816));
#189682=CARTESIAN_POINT('Ctrl Pts',(5.55124157285383,3.86988449437698,26.8908982884926));
#189683=CARTESIAN_POINT('Ctrl Pts',(5.44619741654609,4.02056741225946,26.8995168982133));
#189684=CARTESIAN_POINT('Ctrl Pts',(5.33505285427677,4.16691585411189,26.9081355079341));
#189685=CARTESIAN_POINT('Ctrl Pts',(5.21819431125555,4.30844950416971,26.9167541176549));
#189686=CARTESIAN_POINT('Ctrl Pts',(5.10126561269086,4.45006812336955,26.9253779015224));
#189687=CARTESIAN_POINT('Ctrl Pts',(4.97861628106307,4.58686594761258,26.9340016853899));
#189688=CARTESIAN_POINT('Ctrl Pts',(4.85067173123851,4.71839726557266,26.9426254692573));
#189689=CARTESIAN_POINT('Ctrl Pts',(4.72256918962313,4.85009100442916,26.9512599021682));
#189690=CARTESIAN_POINT('Ctrl Pts',(4.58915857053572,4.97650501759553,26.959894335079));
#189691=CARTESIAN_POINT('Ctrl Pts',(4.45090196717683,5.09723068720471,26.9685287679899));
#189692=CARTESIAN_POINT('Ctrl Pts',(4.31256466970492,5.21802681891546,26.9771682404278));
#189693=CARTESIAN_POINT('Ctrl Pts',(4.16937597702939,5.33312778630485,26.9858077128658));
#189694=CARTESIAN_POINT('Ctrl Pts',(4.02183034662315,5.44216589814948,26.9944471853038));
#189695=CARTESIAN_POINT('Ctrl Pts',(3.87409389252246,5.55134503114995,27.0030978313431));
#189696=CARTESIAN_POINT('Ctrl Pts',(3.72198948335512,5.65444545512441,27.0117484773824));
#189697=CARTESIAN_POINT('Ctrl Pts',(3.56604131887359,5.75114234844577,27.0203991234217));
#189698=CARTESIAN_POINT('Ctrl Pts',(3.4138854502671,5.8454877987034,27.0288394059123));
#189699=CARTESIAN_POINT('Ctrl Pts',(3.25807084116531,5.93373743027089,27.0372796884029));
#189700=CARTESIAN_POINT('Ctrl Pts',(3.09910619832137,6.01563211736939,27.0457199708935));
#189701=CARTESIAN_POINT('Ctrl Pts',(3.09910619832135,6.0156321173694,25.0456877277983));
#189702=CARTESIAN_POINT('Ctrl Pts',(2.9450685624596,6.09498853125241,25.0538144835559));
#189703=CARTESIAN_POINT('Ctrl Pts',(2.78802739907583,6.16840065421879,25.0619412393135));
#189704=CARTESIAN_POINT('Ctrl Pts',(2.62849061198312,6.23564961352998,25.070067995071));
#189705=CARTESIAN_POINT('Ctrl Pts',(2.46890098615892,6.30292084575872,25.0781974424176));
#189706=CARTESIAN_POINT('Ctrl Pts',(2.30681443123484,6.36402471473129,25.0863268897642));
#189707=CARTESIAN_POINT('Ctrl Pts',(2.14275652578268,6.41879143384608,25.0944563371108));
#189708=CARTESIAN_POINT('Ctrl Pts',(1.97850459579159,6.47362292330762,25.1025953988205));
#189709=CARTESIAN_POINT('Ctrl Pts',(1.81227700760014,6.52210218138668,25.1107344605303));
#189710=CARTESIAN_POINT('Ctrl Pts',(1.64461311299654,6.56410974226969,25.11887352224));
#189711=CARTESIAN_POINT('Ctrl Pts',(1.48306356498732,6.60458537651202,25.1267157696334));
#189712=CARTESIAN_POINT('Ctrl Pts',(1.3201809157762,6.63905298337215,25.1345580170268));
#189713=CARTESIAN_POINT('Ctrl Pts',(1.15645336321713,6.66745113358199,25.1424002644202));
#189714=CARTESIAN_POINT('Ctrl Pts',(0.980241778927664,6.6980146090701,25.1508404738778));
#189715=CARTESIAN_POINT('Ctrl Pts',(0.802687245849629,6.72161091930514,
25.1592806833354));
#189716=CARTESIAN_POINT('Ctrl Pts',(0.624366915154841,6.73813438239844,
25.167720892793));
#189717=CARTESIAN_POINT('Ctrl Pts',(0.446181688529219,6.75464532652046,
25.1761547075415));
#189718=CARTESIAN_POINT('Ctrl Pts',(0.267232151754892,6.76409407510952,
25.18458852229));
#189719=CARTESIAN_POINT('Ctrl Pts',(0.088103036568935,6.76642644643,25.1930223370385));
#189720=CARTESIAN_POINT('Ctrl Pts',(-0.0909178987375423,6.76875740918187,
25.2014510584271));
#189721=CARTESIAN_POINT('Ctrl Pts',(-0.270117863622306,6.76398055847807,
25.2098797798156));
#189722=CARTESIAN_POINT('Ctrl Pts',(-0.448909246482972,6.75209371146625,
25.2183085012042));
#189723=CARTESIAN_POINT('Ctrl Pts',(-0.62762010826532,6.74021221785416,
25.2267334266059));
#189724=CARTESIAN_POINT('Ctrl Pts',(-0.805922422723691,6.72122713460942,
25.2351583520076));
#189725=CARTESIAN_POINT('Ctrl Pts',(-0.983230425147443,6.69518834171709,
25.2435832774093));
#189726=CARTESIAN_POINT('Ctrl Pts',(-1.16048577885641,6.66915728061893,
25.2520057011671));
#189727=CARTESIAN_POINT('Ctrl Pts',(-1.33674707972042,6.6360767351359,25.2604281249248));
#189728=CARTESIAN_POINT('Ctrl Pts',(-1.51143512247197,6.59604827685169,
25.2688505486826));
#189729=CARTESIAN_POINT('Ctrl Pts',(-1.68612591256256,6.55601918903529,
25.2772731049008));
#189730=CARTESIAN_POINT('Ctrl Pts',(-1.8592430686407,6.50904203807539,25.2856956611189));
#189731=CARTESIAN_POINT('Ctrl Pts',(-2.03021833266987,6.45526936089356,
25.2941182173371));
#189732=CARTESIAN_POINT('Ctrl Pts',(-2.20119937227635,6.40149486726035,
25.3025410580709));
#189733=CARTESIAN_POINT('Ctrl Pts',(-2.37003805730619,6.34092448961307,
25.3109638988046));
#189734=CARTESIAN_POINT('Ctrl Pts',(-2.53618188283675,6.27376047177215,
25.3193867395384));
#189735=CARTESIAN_POINT('Ctrl Pts',(-2.70235451625344,6.20658480827799,
25.327811040719));
#189736=CARTESIAN_POINT('Ctrl Pts',(-2.86583104933623,6.13281335024041,
25.3362353418997));
#189737=CARTESIAN_POINT('Ctrl Pts',(-3.02607919064693,6.05269640176456,
25.3446596430804));
#189738=CARTESIAN_POINT('Ctrl Pts',(-3.18637749685227,5.97255437307095,
25.3530865814472));
#189739=CARTESIAN_POINT('Ctrl Pts',(-3.34344509812326,5.88606304265238,
25.361513519814));
#189740=CARTESIAN_POINT('Ctrl Pts',(-3.49677420398641,5.79351872063388,
25.3699404581808));
#189741=CARTESIAN_POINT('Ctrl Pts',(-3.65024117198855,5.70089118963746,
25.3783749734245));
#189742=CARTESIAN_POINT('Ctrl Pts',(-3.79996264216661,5.60219996479436,
25.3868094886681));
#189743=CARTESIAN_POINT('Ctrl Pts',(-3.94545876740386,5.49778538274422,
25.3952440039118));
#189744=CARTESIAN_POINT('Ctrl Pts',(-4.0910251685169,5.39332036755583,25.4036825930986));
#189745=CARTESIAN_POINT('Ctrl Pts',(-4.23236188833583,5.28312668275323,
25.4121211822854));
#189746=CARTESIAN_POINT('Ctrl Pts',(-4.36902169349185,5.16758535892709,
25.4205597714722));
#189747=CARTESIAN_POINT('Ctrl Pts',(-4.50583425339036,5.05191488604247,
25.4290077930925));
#189748=CARTESIAN_POINT('Ctrl Pts',(-4.63795920331072,4.93088505172183,
25.4374558147128));
#189749=CARTESIAN_POINT('Ctrl Pts',(-4.7649848536557,4.80491501948076,25.445903836333));
#189750=CARTESIAN_POINT('Ctrl Pts',(-4.83718419476079,4.73331567476501,
25.4507055562453));
#189751=CARTESIAN_POINT('Ctrl Pts',(-4.90773684972699,4.66012100067557,
25.4555072761575));
#189752=CARTESIAN_POINT('Ctrl Pts',(-4.97657296742492,4.58541279492867,
25.4603089960697));
#189753=CARTESIAN_POINT('Ctrl Pts',(-5.09469259843769,4.45721692927607,
25.4685485279206));
#189754=CARTESIAN_POINT('Ctrl Pts',(-5.20801925773606,4.32427641299698,
25.4767880597714));
#189755=CARTESIAN_POINT('Ctrl Pts',(-5.31615128256397,4.18698274905611,
25.4850275916222));
#189756=CARTESIAN_POINT('Ctrl Pts',(-5.42416328840127,4.04984147148727,
25.4932579781685));
#189757=CARTESIAN_POINT('Ctrl Pts',(-5.52699192193546,3.90835694409848,
25.5014883647148));
#189758=CARTESIAN_POINT('Ctrl Pts',(-5.62427273543654,3.76295697522908,
25.5097187512611));
#189759=CARTESIAN_POINT('Ctrl Pts',(-5.72146292803638,3.61769245214539,
25.5179414708788));
#189760=CARTESIAN_POINT('Ctrl Pts',(-5.81311539604065,3.46852004548224,
25.5261641904966));
#189761=CARTESIAN_POINT('Ctrl Pts',(-5.89890628069536,3.31590013293116,
25.5343869101143));
#189762=CARTESIAN_POINT('Ctrl Pts',(-5.98462114844598,3.16341545261717,
25.5426023438101));
#189763=CARTESIAN_POINT('Ctrl Pts',(-6.06448461081675,3.00748966386387,
25.5508177775059));
#189764=CARTESIAN_POINT('Ctrl Pts',(-6.13821649410676,2.8486114637619,25.5590332112018));
#189765=CARTESIAN_POINT('Ctrl Pts',(-6.21191048493394,2.68981491471812,
25.5672444228026));
#189766=CARTESIAN_POINT('Ctrl Pts',(-6.27947902302974,2.52806929822944,
25.5754556344034));
#189767=CARTESIAN_POINT('Ctrl Pts',(-6.34068801540674,2.36388758008441,
25.5836668460042));
#189768=CARTESIAN_POINT('Ctrl Pts',(-6.40187648166539,2.19976091942762,
25.5918753040177));
#189769=CARTESIAN_POINT('Ctrl Pts',(-6.4567095264163,2.03320011764541,25.6000837620313));
#189770=CARTESIAN_POINT('Ctrl Pts',(-6.5050012852481,1.86473785796304,25.6082922200448));
#189771=CARTESIAN_POINT('Ctrl Pts',(-6.5265163182963,1.78968424276826,25.611949267328));
#189772=CARTESIAN_POINT('Ctrl Pts',(-6.54673362252307,1.71425344630615,
25.6156063146112));
#189773=CARTESIAN_POINT('Ctrl Pts',(-6.56563993181014,1.63849360261803,
25.6192633618944));
#189774=CARTESIAN_POINT('Ctrl Pts',(-6.60796019411089,1.46891124743364,
25.6274493699577));
#189775=CARTESIAN_POINT('Ctrl Pts',(-6.64368652839661,1.29776665582351,
25.635635378021));
#189776=CARTESIAN_POINT('Ctrl Pts',(-6.67272679056475,1.12561368971754,
25.6438213860843));
#189777=CARTESIAN_POINT('Ctrl Pts',(-6.70178059404674,0.953380449634272,
25.6520112112379));
#189778=CARTESIAN_POINT('Ctrl Pts',(-6.72414206363312,0.780138252551122,
25.6602010363916));
#189779=CARTESIAN_POINT('Ctrl Pts',(-6.7397709151484,0.606446214696485,
25.6683908615452));
#189780=CARTESIAN_POINT('Ctrl Pts',(-6.75541550510242,0.432579266900768,
25.6765889339499));
#189781=CARTESIAN_POINT('Ctrl Pts',(-6.76431392100477,0.258261930867931,
25.6847870063546));
#189782=CARTESIAN_POINT('Ctrl Pts',(-6.766477954304,0.084054113034077,25.6929850787592));
#189783=CARTESIAN_POINT('Ctrl Pts',(-6.76684704437416,0.0543418273087019,
25.6943833137679));
#189784=CARTESIAN_POINT('Ctrl Pts',(-6.76702035669943,0.024632717883948,
25.6957815487766));
#189785=CARTESIAN_POINT('Ctrl Pts',(-6.76699810037806,-0.00507045163497854,
25.6971797837853));
#189786=CARTESIAN_POINT('',(-6.76699999946963,-8.47234480375662E-5,25.3028202161501));
#189787=CARTESIAN_POINT('Ctrl Pts',(3.09910619832136,6.01563211736939,24.6515493092843));
#189788=CARTESIAN_POINT('Ctrl Pts',(2.94284574041202,6.09613367468057,24.6597832037901));
#189789=CARTESIAN_POINT('Ctrl Pts',(2.78337708565397,6.17057824749298,24.668017098296));
#189790=CARTESIAN_POINT('Ctrl Pts',(2.62122488019941,6.23870732823905,24.6762509928018));
#189791=CARTESIAN_POINT('Ctrl Pts',(2.46294786818989,6.30520822658461,24.6842881096325));
#189792=CARTESIAN_POINT('Ctrl Pts',(2.3021144789861,6.36569192592313,24.6923252264631));
#189793=CARTESIAN_POINT('Ctrl Pts',(2.13923395749237,6.41996628301984,24.7003623432938));
#189794=CARTESIAN_POINT('Ctrl Pts',(1.97633678479312,6.47424618856069,24.7084002817554));
#189795=CARTESIAN_POINT('Ctrl Pts',(1.811392417538,6.52231536966561,24.7164382202171));
#189796=CARTESIAN_POINT('Ctrl Pts',(1.64492605312687,6.56403132836403,24.7244761586787));
#189797=CARTESIAN_POINT('Ctrl Pts',(1.47840968798621,6.60575981709142,24.7325165114587));
#189798=CARTESIAN_POINT('Ctrl Pts',(1.31037077793987,6.64113119421398,24.7405568642386));
#189799=CARTESIAN_POINT('Ctrl Pts',(1.14134537031516,6.67005395372932,24.7485972170185));
#189800=CARTESIAN_POINT('Ctrl Pts',(0.965170110909029,6.70020015915467,
24.7569776803857));
#189801=CARTESIAN_POINT('Ctrl Pts',(0.787923523518979,6.7233402141603,24.7653581437529));
#189802=CARTESIAN_POINT('Ctrl Pts',(0.610218097680674,6.73943045614858,
24.77373860712));
#189803=CARTESIAN_POINT('Ctrl Pts',(0.439423832667417,6.75489493080549,
24.7817931449852));
#189804=CARTESIAN_POINT('Ctrl Pts',(0.268206116151743,6.7638476589083,24.7898476828504));
#189805=CARTESIAN_POINT('Ctrl Pts',(0.0971077703182675,6.76630320640036,
24.7979022207156));
#189806=CARTESIAN_POINT('Ctrl Pts',(-0.0741196886831647,6.76876060688238,
24.805962836646));
#189807=CARTESIAN_POINT('Ctrl Pts',(-0.245227226744314,6.76471107333792,
24.8140234525764));
#189808=CARTESIAN_POINT('Ctrl Pts',(-0.415677386113846,6.75422099954344,
24.8220840685068));
#189809=CARTESIAN_POINT('Ctrl Pts',(-0.586368499081741,6.74371609665735,
24.8301560791723));
#189810=CARTESIAN_POINT('Ctrl Pts',(-0.756400011002734,6.72675252473188,
24.8382280898378));
#189811=CARTESIAN_POINT('Ctrl Pts',(-0.925244300123992,6.703447768506,24.8463001005033));
#189812=CARTESIAN_POINT('Ctrl Pts',(-0.945204079241676,6.70069281724836,
24.8472543261438));
#189813=CARTESIAN_POINT('Ctrl Pts',(-0.965147284995377,6.69784930783103,
24.8482085517842));
#189814=CARTESIAN_POINT('Ctrl Pts',(-0.985073060579621,6.69491748009789,
24.8491627774246));
#189815=CARTESIAN_POINT('Ctrl Pts',(-1.1590779579849,6.66931484386639,24.8574956994713));
#189816=CARTESIAN_POINT('Ctrl Pts',(-1.33230753138869,6.63689133378378,
24.865828621518));
#189817=CARTESIAN_POINT('Ctrl Pts',(-1.50419476867123,6.59770316836868,
24.8741615435647));
#189818=CARTESIAN_POINT('Ctrl Pts',(-1.6758788769231,6.55856131386171,24.8824846181184));
#189819=CARTESIAN_POINT('Ctrl Pts',(-1.84622347277167,6.51267080574074,
24.890807692672));
#189820=CARTESIAN_POINT('Ctrl Pts',(-2.01466809300645,6.46013943154649,
24.8991307672256));
#189821=CARTESIAN_POINT('Ctrl Pts',(-2.18294457152471,6.40766049426246,
24.9074455336716));
#189822=CARTESIAN_POINT('Ctrl Pts',(-2.34932452287968,6.34855400079885,
24.9157603001176));
#189823=CARTESIAN_POINT('Ctrl Pts',(-2.51325886634617,6.28297850312512,
24.9240750665635));
#189824=CARTESIAN_POINT('Ctrl Pts',(-2.67705964134008,6.21745643427464,
24.9323830584031));
#189825=CARTESIAN_POINT('Ctrl Pts',(-2.8384184572062,6.14547599226639,24.9406910502426));
#189826=CARTESIAN_POINT('Ctrl Pts',(-2.99680234998407,6.06724522951973,
24.9489990420822));
#189827=CARTESIAN_POINT('Ctrl Pts',(-3.15508623371199,5.98906386437357,
24.9573017879693));
#189828=CARTESIAN_POINT('Ctrl Pts',(-3.31039862682985,5.9046401973843,24.9656045338564));
#189829=CARTESIAN_POINT('Ctrl Pts',(-3.46222727349032,5.81423006998345,
24.9739072797435));
#189830=CARTESIAN_POINT('Ctrl Pts',(-3.61399387262131,5.72385689032053,
24.9822066325629));
#189831=CARTESIAN_POINT('Ctrl Pts',(-3.76227926364622,5.62750230276009,
24.9905059853824));
#189832=CARTESIAN_POINT('Ctrl Pts',(-3.9065962477699,5.52546783149718,24.9988053382018));
#189833=CARTESIAN_POINT('Ctrl Pts',(-4.05088253809232,5.42345506125443,
25.0071029258881));
#189834=CARTESIAN_POINT('Ctrl Pts',(-4.19120181906805,5.3157650146793,25.0154005135745));
#189835=CARTESIAN_POINT('Ctrl Pts',(-4.32709612044553,5.20274236959945,
25.0236981012608));
#189836=CARTESIAN_POINT('Ctrl Pts',(-4.46298410165557,5.08972498097284,
25.0319953030432));
#189837=CARTESIAN_POINT('Ctrl Pts',(-4.59444724600527,4.97137571063061,
25.0402925048257));
#189838=CARTESIAN_POINT('Ctrl Pts',(-4.72106076285954,4.8480794417365,25.0485897066081));
#189839=CARTESIAN_POINT('Ctrl Pts',(-4.84768943027238,4.72476841922532,
25.0568879012327));
#189840=CARTESIAN_POINT('Ctrl Pts',(-4.96946706504823,4.59650946175034,
25.0651860958573));
#189841=CARTESIAN_POINT('Ctrl Pts',(-5.08600570305688,4.46372434055609,
25.0734842904819));
#189842=CARTESIAN_POINT('Ctrl Pts',(-5.20262630404737,4.3308458300391,25.0817883213235));
#189843=CARTESIAN_POINT('Ctrl Pts',(-5.31400031585095,4.19343505673715,
25.0900923521651));
#189844=CARTESIAN_POINT('Ctrl Pts',(-5.41977948199487,4.05194760165374,
25.0983963830066));
#189845=CARTESIAN_POINT('Ctrl Pts',(-5.52559711235487,3.9104086978376,25.1067034334224));
#189846=CARTESIAN_POINT('Ctrl Pts',(-5.62581563978829,3.76479044066879,
25.1150104838381));
#189847=CARTESIAN_POINT('Ctrl Pts',(-5.72013003215047,3.61557760465604,
25.1233175342538));
#189848=CARTESIAN_POINT('Ctrl Pts',(-5.81454526251574,3.4662052349386,25.1316334663085));
#189849=CARTESIAN_POINT('Ctrl Pts',(-5.90304356559838,3.31323090579058,
25.1399493983631));
#189850=CARTESIAN_POINT('Ctrl Pts',(-5.98536524279265,3.15716516995384,
25.1482653304177));
#189851=CARTESIAN_POINT('Ctrl Pts',(-6.04742107162982,3.03951950333827,
25.1545340566365));
#189852=CARTESIAN_POINT('Ctrl Pts',(-6.10596799486901,2.92011768554067,
25.1608027828553));
#189853=CARTESIAN_POINT('Ctrl Pts',(-6.16091288811307,2.79918584325556,
25.1670715090741));
#189854=CARTESIAN_POINT('Ctrl Pts',(-6.2362297338961,2.63341602593716,25.1756644948459));
#189855=CARTESIAN_POINT('Ctrl Pts',(-6.30490854911061,2.46448051554261,
25.1842574806176));
#189856=CARTESIAN_POINT('Ctrl Pts',(-6.36669181460124,2.29292920472691,
25.1928504663894));
#189857=CARTESIAN_POINT('Ctrl Pts',(-6.42841383145778,2.12154796073075,
25.2014349335334));
#189858=CARTESIAN_POINT('Ctrl Pts',(-6.48325382472646,1.94755637993255,
25.2100194006774));
#189859=CARTESIAN_POINT('Ctrl Pts',(-6.53100212792579,1.77152482484124,
25.2186038678214));
#189860=CARTESIAN_POINT('Ctrl Pts',(-6.57869426496486,1.5957003350459,25.227178237087));
#189861=CARTESIAN_POINT('Ctrl Pts',(-6.61931127585403,1.41784095939495,
25.2357526063527));
#189862=CARTESIAN_POINT('Ctrl Pts',(-6.65269309676399,1.23853282567268,
25.2443269756183));
#189863=CARTESIAN_POINT('Ctrl Pts',(-6.68605066955921,1.05935493901554,
25.2528951165751));
#189864=CARTESIAN_POINT('Ctrl Pts',(-6.71218347386952,0.878730698365294,
25.2614632575319));
#189865=CARTESIAN_POINT('Ctrl Pts',(-6.73098208979044,0.697258278488218,
25.2700313984888));
#189866=CARTESIAN_POINT('Ctrl Pts',(-6.74976551552573,0.515932497052884,
25.2785926159757));
#189867=CARTESIAN_POINT('Ctrl Pts',(-6.76122654452264,0.333760213529871,
25.2871538334626));
#189868=CARTESIAN_POINT('Ctrl Pts',(-6.76530731846125,0.151346908705136,
25.2957150509495));
#189869=CARTESIAN_POINT('Ctrl Pts',(-6.76643623005296,0.100883810921509,
25.2980834393497));
#189870=CARTESIAN_POINT('Ctrl Pts',(-6.76700063157175,0.0504023040753878,
25.3004518277499));
#189871=CARTESIAN_POINT('Ctrl Pts',(-6.76699999946963,-8.47234480193804E-5,
25.3028202161501));
#189872=CARTESIAN_POINT('Ctrl Pts',(-6.76699999946962,-8.4724297419803E-5,
25.3028202161899));
#189873=CARTESIAN_POINT('Ctrl Pts',(-6.76699793498657,-0.164976700326648,
25.3105554357596));
#189874=CARTESIAN_POINT('Ctrl Pts',(-6.7609652682336,-0.329871544089191,
25.3182906553293));
#189875=CARTESIAN_POINT('Ctrl Pts',(-6.74892353752594,-0.494287451417036,
25.3260258748989));
#189876=CARTESIAN_POINT('Ctrl Pts',(-6.73550633092438,-0.677483891426879,
25.3346446558361));
#189877=CARTESIAN_POINT('Ctrl Pts',(-6.71463052610296,-0.860066816299092,
25.3432634367734));
#189878=CARTESIAN_POINT('Ctrl Pts',(-6.68638325743214,-1.04142591418264,
25.3518822177106));
#189879=CARTESIAN_POINT('Ctrl Pts',(-6.65811902079877,-1.22289395337372,
25.3605061758971));
#189880=CARTESIAN_POINT('Ctrl Pts',(-6.62247453019704,-1.40313639789951,
25.3691301340837));
#189881=CARTESIAN_POINT('Ctrl Pts',(-6.57958811526716,-1.58155279185841,
25.3777540922702));
#189882=CARTESIAN_POINT('Ctrl Pts',(-6.53515236049314,-1.76641476137923,
25.3866896046413));
#189883=CARTESIAN_POINT('Ctrl Pts',(-6.48294176403342,-1.94931593270744,
25.3956251170125));
#189884=CARTESIAN_POINT('Ctrl Pts',(-6.42316651510862,-2.12960581309954,
25.4045606293836));
#189885=CARTESIAN_POINT('Ctrl Pts',(-6.36536758601136,-2.30393485733067,
25.4132007112783));
#189886=CARTESIAN_POINT('Ctrl Pts',(-6.30049636211091,-2.47582224998501,
25.421840793173));
#189887=CARTESIAN_POINT('Ctrl Pts',(-6.22879206359173,-2.64470006400286,
25.4304808750677));
#189888=CARTESIAN_POINT('Ctrl Pts',(-6.15341008550919,-2.82223954124237,
25.439564102677));
#189889=CARTESIAN_POINT('Ctrl Pts',(-6.07047586045127,-2.99645225588371,
25.4486473302863));
#189890=CARTESIAN_POINT('Ctrl Pts',(-5.98032242155961,-3.16670692268664,
25.4577305578956));
#189891=CARTESIAN_POINT('Ctrl Pts',(-5.89016898266796,-3.33696158948953,
25.466813785505));
#189892=CARTESIAN_POINT('Ctrl Pts',(-5.7927965549236,-3.50325789082802,
25.4758970131143));
#189893=CARTESIAN_POINT('Ctrl Pts',(-5.68859152615251,-3.6649986969419,
25.4849802407236));
#189894=CARTESIAN_POINT('Ctrl Pts',(-5.58482970181796,-3.82605158766739,
25.4940248355834));
#189895=CARTESIAN_POINT('Ctrl Pts',(-5.47419818896963,-3.98273685442638,
25.5030694304433));
#189896=CARTESIAN_POINT('Ctrl Pts',(-5.35707221927229,-4.13449709608086,
25.5121140253031));
#189897=CARTESIAN_POINT('Ctrl Pts',(-5.2400537310889,-4.2861180738251,25.5211503203234));
#189898=CARTESIAN_POINT('Ctrl Pts',(-5.11655282982289,-4.43282286147519,
25.5301866153437));
#189899=CARTESIAN_POINT('Ctrl Pts',(-4.98698663541845,-4.57408496840164,
25.5392229103641));
#189900=CARTESIAN_POINT('Ctrl Pts',(-4.85764971855503,-4.7150971009527,
25.5482432149518));
#189901=CARTESIAN_POINT('Ctrl Pts',(-4.72226910160204,-4.8506856100701,
25.5572635195395));
#189902=CARTESIAN_POINT('Ctrl Pts',(-4.58130040763553,-4.9803589805353,
25.5662838241272));
#189903=CARTESIAN_POINT('Ctrl Pts',(-4.44050923635512,-5.10986905258016,
25.5752927693935));
#189904=CARTESIAN_POINT('Ctrl Pts',(-4.29414420624897,-5.23347869097792,
25.5843017146598));
#189905=CARTESIAN_POINT('Ctrl Pts',(-4.14269763601296,-5.35073315505199,
25.5933106599261));
#189906=CARTESIAN_POINT('Ctrl Pts',(-3.99159496887706,-5.46772135906066,
25.6022991477849));
#189907=CARTESIAN_POINT('Ctrl Pts',(-3.83543398241206,-5.57838304940959,
25.6112876356437));
#189908=CARTESIAN_POINT('Ctrl Pts',(-3.67473949711305,-5.68230398943574,
25.6202761235025));
#189909=CARTESIAN_POINT('Ctrl Pts',(-3.53375220255945,-5.77348031172516,
25.6281622845178));
#189910=CARTESIAN_POINT('Ctrl Pts',(-3.38927578092314,-5.85946831997876,
25.6360484455331));
#189911=CARTESIAN_POINT('Ctrl Pts',(-3.24168590658374,-5.94001359283431,
25.6439346065484));
#189912=CARTESIAN_POINT('Ctrl Pts',(-3.08969230979447,-6.02296214049372,
25.6520560714046));
#189913=CARTESIAN_POINT('Ctrl Pts',(-2.93446394824125,-6.10009974434972,
25.6601775362608));
#189914=CARTESIAN_POINT('Ctrl Pts',(-2.77649212342414,-6.1711733477973,
25.6682990011169));
#189915=CARTESIAN_POINT('Ctrl Pts',(-2.61853156432294,-6.242241882651,25.6764198867931));
#189916=CARTESIAN_POINT('Ctrl Pts',(-2.45782826560801,-6.30724712823443,
25.6845407724693));
#189917=CARTESIAN_POINT('Ctrl Pts',(-2.29489524638042,-6.36598341249336,
25.6926616581456));
#189918=CARTESIAN_POINT('Ctrl Pts',(-2.13194275199779,-6.42472671741788,
25.7007835144998));
#189919=CARTESIAN_POINT('Ctrl Pts',(-1.96676035129669,-6.47719944589699,
25.7089053708541));
#189920=CARTESIAN_POINT('Ctrl Pts',(-1.79987797499627,-6.52324522573875,
25.7170272272084));
#189921=CARTESIAN_POINT('Ctrl Pts',(-1.63287384337915,-6.56932460001169,
25.7251550091686));
#189922=CARTESIAN_POINT('Ctrl Pts',(-1.46416761234239,-6.60896756289479,
25.7332827911287));
#189923=CARTESIAN_POINT('Ctrl Pts',(-1.29430183206151,-6.64206833505364,
25.7414105730889));
#189924=CARTESIAN_POINT('Ctrl Pts',(-1.12436685477529,-6.67518259123678,
25.7495416660053));
#189925=CARTESIAN_POINT('Ctrl Pts',(-0.953271748300365,-6.70174928836536,
25.7576727589218));
#189926=CARTESIAN_POINT('Ctrl Pts',(-0.781565761050786,-6.72171436176465,
25.7658038518382));
#189927=CARTESIAN_POINT('Ctrl Pts',(-0.609672363892046,-6.74170122620717,
25.7739438195028));
#189928=CARTESIAN_POINT('Ctrl Pts',(-0.43716711888452,-6.75507204707863,
25.7820837871673));
#189929=CARTESIAN_POINT('Ctrl Pts',(-0.264601621089993,-6.76182482634063,
25.7902237548319));
#189930=CARTESIAN_POINT('Ctrl Pts',(-0.17510169268123,-6.76532710963732,
25.7944454940123));
#189931=CARTESIAN_POINT('Ctrl Pts',(-0.0855855316561024,-6.76705005699934,
25.7986672331927));
#189932=CARTESIAN_POINT('Ctrl Pts',(0.00387034878749698,-6.76699889318746,
25.8028889723731));
#189933=CARTESIAN_POINT('Ctrl Pts',(0.182712843762716,-6.76689660517995,
25.8113291818308));
#189934=CARTESIAN_POINT('Ctrl Pts',(0.361683813194869,-6.75970006616008,
25.8197693912884));
#189935=CARTESIAN_POINT('Ctrl Pts',(0.540196532682286,-6.74540411732893,
25.828209600746));
#189936=CARTESIAN_POINT('Ctrl Pts',(0.718574002337971,-6.73111899979696,
25.8366434154945));
#189937=CARTESIAN_POINT('Ctrl Pts',(0.896493582928289,-6.70974522136511,
25.8450772302431));
#189938=CARTESIAN_POINT('Ctrl Pts',(1.07336991193727,-6.68132966049033,
25.8535110449916));
#189939=CARTESIAN_POINT('Ctrl Pts',(1.25013942157147,-6.65293126037676,
25.8619397663802));
#189940=CARTESIAN_POINT('Ctrl Pts',(1.42586660726584,-6.61749960891584,
25.8703684877687));
#189941=CARTESIAN_POINT('Ctrl Pts',(1.59997218499026,-6.5751333071853,25.8787972091573));
#189942=CARTESIAN_POINT('Ctrl Pts',(1.77399935195162,-6.53278608568234,
25.887222134559));
#189943=CARTESIAN_POINT('Ctrl Pts',(1.94640604361477,-6.48351051976002,
25.8956470599607));
#189944=CARTESIAN_POINT('Ctrl Pts',(2.11662372216021,-6.42745618567631,
25.9040719853625));
#189945=CARTESIAN_POINT('Ctrl Pts',(2.28679085734594,-6.37141849601164,
25.9124944091202));
#189946=CARTESIAN_POINT('Ctrl Pts',(2.45476995922689,-6.30860615643662,
25.9209168328779));
#189947=CARTESIAN_POINT('Ctrl Pts',(2.62000781530578,-6.23921854463655,
25.9293392566357));
#189948=CARTESIAN_POINT('Ctrl Pts',(2.78524827010023,-6.16982984156919,
25.9377618128539));
#189949=CARTESIAN_POINT('Ctrl Pts',(2.94774708298164,-6.09386578261243,
25.9461843690721));
#189950=CARTESIAN_POINT('Ctrl Pts',(3.10697056506046,-6.01157407904518,
25.9546069252903));
#189951=CARTESIAN_POINT('Ctrl Pts',(3.26619942573861,-5.92927959564863,
25.963029766024));
#189952=CARTESIAN_POINT('Ctrl Pts',(3.42215243858913,-5.84065719445277,
25.9714526067578));
#189953=CARTESIAN_POINT('Ctrl Pts',(3.57431995727228,-5.74600085651274,
25.9798754474915));
#189954=CARTESIAN_POINT('Ctrl Pts',(3.72651386047188,-5.65132810599184,
25.9882997486721));
#189955=CARTESIAN_POINT('Ctrl Pts',(3.87492067766104,-5.55061950903333,
25.9967240498528));
#189956=CARTESIAN_POINT('Ctrl Pts',(4.0190589170397,-5.4442129294659,26.0051483510334));
#189957=CARTESIAN_POINT('Ctrl Pts',(4.16324227818725,-5.33777303984063,
26.0135752894002));
#189958=CARTESIAN_POINT('Ctrl Pts',(4.30315412913592,-5.22563180937416,
26.022002227767));
#189959=CARTESIAN_POINT('Ctrl Pts',(4.4383450043898,-5.10816822569579,26.0304291661338));
#189960=CARTESIAN_POINT('Ctrl Pts',(4.57365743323396,-4.99059902749059,
26.0388636813775));
#189961=CARTESIAN_POINT('Ctrl Pts',(4.70424015266259,-4.86769813294548,
26.0472981966211));
#189962=CARTESIAN_POINT('Ctrl Pts',(4.82967877549317,-4.73988311306838,
26.0557327118648));
#189963=CARTESIAN_POINT('Ctrl Pts',(4.9551779862531,-4.6120063574418,26.0641713010516));
#189964=CARTESIAN_POINT('Ctrl Pts',(5.07552791741531,-4.47921098625575,
26.0726098902383));
#189965=CARTESIAN_POINT('Ctrl Pts',(5.190353289939,-4.34194906990161,26.0810484794251));
#189966=CARTESIAN_POINT('Ctrl Pts',(5.30530701125062,-4.20453372577966,
26.0894965010454));
#189967=CARTESIAN_POINT('Ctrl Pts',(5.41472362707429,-4.06264212148597,
26.0979445226657));
#189968=CARTESIAN_POINT('Ctrl Pts',(5.51826941403206,-3.91675780131454,
26.106392544286));
#189969=CARTESIAN_POINT('Ctrl Pts',(5.57712317760059,-3.83383949493065,
26.1111942641982));
#189970=CARTESIAN_POINT('Ctrl Pts',(5.6340811061209,-3.7496318241605,26.1159959841105));
#189971=CARTESIAN_POINT('Ctrl Pts',(5.68908840787477,-3.66422735203274,
26.1207977040227));
#189972=CARTESIAN_POINT('Ctrl Pts',(5.78347842293469,-3.51767718226813,
26.1290372358735));
#189973=CARTESIAN_POINT('Ctrl Pts',(5.87233292907665,-3.36727442526352,
26.1372767677243));
#189974=CARTESIAN_POINT('Ctrl Pts',(5.95532333861317,-3.21347365518519,
26.1455162995752));
#189975=CARTESIAN_POINT('Ctrl Pts',(6.03822163459527,-3.05984359321258,
26.1537466861215));
#189976=CARTESIAN_POINT('Ctrl Pts',(6.1152686264389,-2.90282333842673,26.1619770726678));
#189977=CARTESIAN_POINT('Ctrl Pts',(6.1861786152737,-2.74289685185762,26.1702074592142));
#189978=CARTESIAN_POINT('Ctrl Pts',(6.257022548667,-2.58311934309613,26.178430178832));
#189979=CARTESIAN_POINT('Ctrl Pts',(6.32174072086143,-2.42044131756993,
26.1866528984498));
#189980=CARTESIAN_POINT('Ctrl Pts',(6.38009300521273,-2.25537186398067,
26.1948756180676));
#189981=CARTESIAN_POINT('Ctrl Pts',(6.43839358523597,-2.09044867382006,
26.2030910517634));
#189982=CARTESIAN_POINT('Ctrl Pts',(6.49033940156552,-1.92313861319645,
26.2113064854591));
#189983=CARTESIAN_POINT('Ctrl Pts',(6.53573822131611,-1.75397118061495,
26.2195219191549));
#189984=CARTESIAN_POINT('Ctrl Pts',(6.58111370959868,-1.58489068695753,
26.2277331307558));
#189985=CARTESIAN_POINT('Ctrl Pts',(6.61994881027167,-1.41395506530572,
26.2359443423566));
#189986=CARTESIAN_POINT('Ctrl Pts',(6.65210084986099,-1.24170982249427,
26.2441555539574));
#189987=CARTESIAN_POINT('Ctrl Pts',(6.68424210743033,-1.06952234123305,
26.2523640119709));
#189988=CARTESIAN_POINT('Ctrl Pts',(6.70970470320407,-0.896026463174697,
26.2605724699845));
#189989=CARTESIAN_POINT('Ctrl Pts',(6.72839685881742,-0.721778851349826,
26.268780927998));
#189990=CARTESIAN_POINT('Ctrl Pts',(6.73672462230109,-0.644147735448202,
26.2724379752812));
#189991=CARTESIAN_POINT('Ctrl Pts',(6.74370920349503,-0.566367531857892,
26.2760950225643));
#189992=CARTESIAN_POINT('Ctrl Pts',(6.74934578577647,-0.488487936413445,
26.2797520698475));
#189993=CARTESIAN_POINT('Ctrl Pts',(6.76300021697827,-0.299827233007562,
26.2886111440234));
#189994=CARTESIAN_POINT('Ctrl Pts',(6.76872665841279,-0.110779146266043,
26.2974702181993));
#189995=CARTESIAN_POINT('Ctrl Pts',(6.76655041107128,0.0780034257655365,
26.3063292923751));
#189996=CARTESIAN_POINT('Ctrl Pts',(6.76437007499884,0.267140682269253,
26.3152050109691));
#189997=CARTESIAN_POINT('Ctrl Pts',(6.75425738114367,0.456011167927298,
26.324080729563));
#189998=CARTESIAN_POINT('Ctrl Pts',(6.73628951813857,0.643966247420222,
26.3329564481569));
#189999=CARTESIAN_POINT('Ctrl Pts',(6.7182703799292,0.832457697604004,26.3418574955439));
#190000=CARTESIAN_POINT('Ctrl Pts',(6.69235123899935,1.02002825434488,26.3507585429309));
#190001=CARTESIAN_POINT('Ctrl Pts',(6.65866106849444,1.20603556121554,26.3596595903179));
#190002=CARTESIAN_POINT('Ctrl Pts',(6.62492509574062,1.39229574757126,26.3685727388009));
#190003=CARTESIAN_POINT('Ctrl Pts',(6.58339704213217,1.57698818484015,26.3774858872839));
#190004=CARTESIAN_POINT('Ctrl Pts',(6.53425640339181,1.75948351931275,26.3863990357669));
#190005=CARTESIAN_POINT('Ctrl Pts',(6.48500665899625,1.94238404333004,26.3953319738767));
#190006=CARTESIAN_POINT('Ctrl Pts',(6.42811059001266,2.1230774559697,26.4042649119866));
#190007=CARTESIAN_POINT('Ctrl Pts',(6.36379762001419,2.30094955431485,26.4131978500965));
#190008=CARTESIAN_POINT('Ctrl Pts',(6.30258099756759,2.47025800156024,26.4217007119551));
#190009=CARTESIAN_POINT('Ctrl Pts',(6.2346449015172,2.63701023195201,26.4302035738136));
#190010=CARTESIAN_POINT('Ctrl Pts',(6.16022666131992,2.800695713776,26.4387064356722));
#190011=CARTESIAN_POINT('Ctrl Pts',(6.08824396200822,2.95902413955698,26.4469310180707));
#190012=CARTESIAN_POINT('Ctrl Pts',(6.01005756673814,3.11478638128748,26.4551556004692));
#190013=CARTESIAN_POINT('Ctrl Pts',(5.92587328937933,3.26746304619051,26.4633801828677));
#190014=CARTESIAN_POINT('Ctrl Pts',(5.84180558029627,3.41992830278628,26.4715933768524));
#190015=CARTESIAN_POINT('Ctrl Pts',(5.75175671396695,3.5693161863398,26.479806570837));
#190016=CARTESIAN_POINT('Ctrl Pts',(5.65598008519765,3.7151282987062,26.4880197648217));
#190017=CARTESIAN_POINT('Ctrl Pts',(5.5602806087334,3.86082295297537,26.4962263427158));
#190018=CARTESIAN_POINT('Ctrl Pts',(5.45886275229027,4.00294727321016,26.50443292061));
#190019=CARTESIAN_POINT('Ctrl Pts',(5.35202556453078,4.1410278140347,26.5126394985041));
#190020=CARTESIAN_POINT('Ctrl Pts',(5.24525500932461,4.2790222363532,26.5208409580939));
#190021=CARTESIAN_POINT('Ctrl Pts',(5.13307207247803,4.41297761911667,26.5290424176837));
#190022=CARTESIAN_POINT('Ctrl Pts',(5.01581884608409,4.5424498129608,26.5372438772736));
#190023=CARTESIAN_POINT('Ctrl Pts',(4.8986174267608,4.6718648009156,26.5454417131371));
#190024=CARTESIAN_POINT('Ctrl Pts',(4.7763504207168,4.79680028042478,26.5536395490006));
#190025=CARTESIAN_POINT('Ctrl Pts',(4.64939993165243,4.91684545979945,26.5618373848642));
#190026=CARTESIAN_POINT('Ctrl Pts',(4.52246573338793,5.03687523449148,26.5700341687483));
#190027=CARTESIAN_POINT('Ctrl Pts',(4.39084950547198,5.15201570834916,26.5782309526324));
#190028=CARTESIAN_POINT('Ctrl Pts',(4.25497010847688,5.26189304109921,26.5864277365165));
#190029=CARTESIAN_POINT('Ctrl Pts',(4.11910289066643,5.37176052528977,26.594623785704));
#190030=CARTESIAN_POINT('Ctrl Pts',(3.97897354623155,5.47636558551816,26.6028198348914));
#190031=CARTESIAN_POINT('Ctrl Pts',(3.83503374755571,5.57537488919883,26.6110158840788));
#190032=CARTESIAN_POINT('Ctrl Pts',(3.69104291756391,5.67441929488119,26.6192148390308));
#190033=CARTESIAN_POINT('Ctrl Pts',(3.5432392309082,5.76786377837212,26.6274137939829));
#190034=CARTESIAN_POINT('Ctrl Pts',(3.39210345244099,5.85541827437955,26.6356127489349));
#190035=CARTESIAN_POINT('Ctrl Pts',(3.29574823599213,5.91123783278872,26.6408399167642));
#190036=CARTESIAN_POINT('Ctrl Pts',(3.19803922663916,5.96466424644638,26.6460670845935));
#190037=CARTESIAN_POINT('Ctrl Pts',(3.0991061983213,6.01563211736942,26.6512942524228));
#190038=CARTESIAN_POINT('Origin',(0.,0.,4.30282021618968));
#190039=CARTESIAN_POINT('',(3.09910619832132,6.01563211736941,29.0458282148631));
#190040=CARTESIAN_POINT('',(3.09910619832131,6.01563211736942,28.6513936431573));
#190041=CARTESIAN_POINT('',(3.09910619832133,6.0156321173694,4.30282021618968));
#190042=CARTESIAN_POINT('',(-6.76699906337236,0.00356038167509778,27.6971797838411));
#190043=CARTESIAN_POINT('Ctrl Pts',(-6.76699906337236,0.00356038167514286,
27.6971797838411));
#190044=CARTESIAN_POINT('Ctrl Pts',(-6.76708950334129,-0.168333319875732,
27.7052996038289));
#190045=CARTESIAN_POINT('Ctrl Pts',(-6.76062617083703,-0.340485372879538,
27.7134194238167));
#190046=CARTESIAN_POINT('Ctrl Pts',(-6.7475763930807,-0.512349313984179,
27.7215392438044));
#190047=CARTESIAN_POINT('Ctrl Pts',(-6.73453996609472,-0.684037427112826,
27.7296507566889));
#190048=CARTESIAN_POINT('Ctrl Pts',(-6.71493053232619,-0.85543765128416,
27.7377622695734));
#190049=CARTESIAN_POINT('Ctrl Pts',(-6.68876740218731,-1.02600177360295,
27.7458737824578));
#190050=CARTESIAN_POINT('Ctrl Pts',(-6.66222459940465,-1.19904107878064,
27.7541030075398));
#190051=CARTESIAN_POINT('Ctrl Pts',(-6.62893638057383,-1.3712194460363,
27.7623322326217));
#190052=CARTESIAN_POINT('Ctrl Pts',(-6.58897774974783,-1.54196667062814,
27.7705614577036));
#190053=CARTESIAN_POINT('Ctrl Pts',(-6.54965160517701,-1.71001121821551,
27.7786604262766));
#190054=CARTESIAN_POINT('Ctrl Pts',(-6.50386472768852,-1.87666921735391,
27.7867593948496));
#190055=CARTESIAN_POINT('Ctrl Pts',(-6.45174049729151,-2.04140479954581,
27.7948583634225));
#190056=CARTESIAN_POINT('Ctrl Pts',(-6.39835878820009,-2.21011456962003,
27.8031527167589));
#190057=CARTESIAN_POINT('Ctrl Pts',(-6.33833014407865,-2.37680760350063,
27.8114470700954));
#190058=CARTESIAN_POINT('Ctrl Pts',(-6.27184195620629,-2.54092256402482,
27.8197414234318));
#190059=CARTESIAN_POINT('Ctrl Pts',(-6.20535376833395,-2.70503752454898,
27.8280357767682));
#190060=CARTESIAN_POINT('Ctrl Pts',(-6.13240618107729,-2.86657402209651,
27.8363301301047));
#190061=CARTESIAN_POINT('Ctrl Pts',(-6.05324029813116,-3.02499105669438,
27.8446244834411));
#190062=CARTESIAN_POINT('Ctrl Pts',(-5.96868440802465,-3.19419391113072,
27.853483557617));
#190063=CARTESIAN_POINT('Ctrl Pts',(-5.87711334375679,-3.35968322021457,
27.8623426317929));
#190064=CARTESIAN_POINT('Ctrl Pts',(-5.77888211931975,-3.52091045768087,
27.8712017059688));
#190065=CARTESIAN_POINT('Ctrl Pts',(-5.68046633817515,-3.68244060868903,
27.8800774245627));
#190066=CARTESIAN_POINT('Ctrl Pts',(-5.57536552503268,-3.83969246402432,
27.8889531431566));
#190067=CARTESIAN_POINT('Ctrl Pts',(-5.4639771373322,-3.99214764790972,
27.8978288617505));
#190068=CARTESIAN_POINT('Ctrl Pts',(-5.35227087864533,-4.14503789581464,
27.9067299091375));
#190069=CARTESIAN_POINT('Ctrl Pts',(-5.23424129293976,-4.29310386935633,
27.9156309565245));
#190070=CARTESIAN_POINT('Ctrl Pts',(-5.11032716331366,-4.43585902434901,
27.9245320039115));
#190071=CARTESIAN_POINT('Ctrl Pts',(-4.98624457072872,-4.57880825693295,
27.9334451523945));
#190072=CARTESIAN_POINT('Ctrl Pts',(-4.85626162831484,-4.71643205684519,
27.9423583008775));
#190073=CARTESIAN_POINT('Ctrl Pts',(-4.72085392763827,-4.84828084932198,
27.9512714493605));
#190074=CARTESIAN_POINT('Ctrl Pts',(-4.58514558483985,-4.98042238217127,
27.9602043874704));
#190075=CARTESIAN_POINT('Ctrl Pts',(-4.44398857917533,-5.10676307945052,
27.9691373255803));
#190076=CARTESIAN_POINT('Ctrl Pts',(-4.29789370282457,-5.2268918794271,
27.9780702636902));
#190077=CARTESIAN_POINT('Ctrl Pts',(-4.15883256341283,-5.34123707905477,
27.9865731255487));
#190078=CARTESIAN_POINT('Ctrl Pts',(-4.01529797259374,-5.44995433033329,
27.9950759874073));
#190079=CARTESIAN_POINT('Ctrl Pts',(-3.86775460434358,-5.55272575593096,
28.0035788492659));
#190080=CARTESIAN_POINT('Ctrl Pts',(-3.72507224685697,-5.65211124143562,
28.0118015731317));
#190081=CARTESIAN_POINT('Ctrl Pts',(-3.57836687347787,-5.74612590434581,
28.0200242969976));
#190082=CARTESIAN_POINT('Ctrl Pts',(-3.42808027674972,-5.83442838812506,
28.0282470208635));
#190083=CARTESIAN_POINT('Ctrl Pts',(-3.27795275329339,-5.92263740671639,
28.0364610412547));
#190084=CARTESIAN_POINT('Ctrl Pts',(-3.12425186151364,-6.00514610578454,
28.0446750616459));
#190085=CARTESIAN_POINT('Ctrl Pts',(-2.96745003429532,-6.0816551442811,
28.0528890820371));
#190086=CARTESIAN_POINT('Ctrl Pts',(-2.8107826951253,-6.15809856140418,
28.0610960573091));
#190087=CARTESIAN_POINT('Ctrl Pts',(-2.65102003801491,-6.22855240999417,
28.069303032581));
#190088=CARTESIAN_POINT('Ctrl Pts',(-2.48866095055195,-6.29276216563107,
28.077510007853));
#190089=CARTESIAN_POINT('Ctrl Pts',(-2.32640852976953,-6.35692973673985,
28.085711591306));
#190090=CARTESIAN_POINT('Ctrl Pts',(-2.16156340877717,-6.41486125462091,
28.0939131747589));
#190091=CARTESIAN_POINT('Ctrl Pts',(-1.99464648789654,-6.46634938650256,
28.1021147582119));
#190092=CARTESIAN_POINT('Ctrl Pts',(-1.82780573233528,-6.51781402400156,
28.1103125992269));
#190093=CARTESIAN_POINT('Ctrl Pts',(-1.65889540238528,-6.56284102749984,
28.1185104402419));
#190094=CARTESIAN_POINT('Ctrl Pts',(-1.48845375639599,-6.60127218156248,
28.1267082812569));
#190095=CARTESIAN_POINT('Ctrl Pts',(-1.31802715134927,-6.63969994419589,
28.1349053988381));
#190096=CARTESIAN_POINT('Ctrl Pts',(-1.14606984721851,-6.67153292957121,
28.1431025164193));
#190097=CARTESIAN_POINT('Ctrl Pts',(-0.973132916139615,-6.69666344738375,
28.1512996340004));
#190098=CARTESIAN_POINT('Ctrl Pts',(-0.800197909176538,-6.72179368559131,
28.1594966603795));
#190099=CARTESIAN_POINT('Ctrl Pts',(-0.626283651922684,-6.74022155210216,
28.1676936867586));
#190100=CARTESIAN_POINT('Ctrl Pts',(-0.451948888939349,-6.75189093527039,
28.1758907131377));
#190101=CARTESIAN_POINT('Ctrl Pts',(-0.27758436627546,-6.76356231045164,
28.1840891387838));
#190102=CARTESIAN_POINT('Ctrl Pts',(-0.102799552912786,-6.76847287980788,
28.19228756443));
#190103=CARTESIAN_POINT('Ctrl Pts',(0.0718441828962487,-6.76661861001372,
28.2004859900761));
#190104=CARTESIAN_POINT('Ctrl Pts',(0.24654948700103,-6.76476368652173,
28.2086873059667));
#190105=CARTESIAN_POINT('Ctrl Pts',(0.421113255886029,-6.75613917703564,
28.2168886218574));
#190106=CARTESIAN_POINT('Ctrl Pts',(0.59497657081346,-6.74079311952111,
28.225089937748));
#190107=CARTESIAN_POINT('Ctrl Pts',(0.769037886953337,-6.72542958541586,
28.2333005935646));
#190108=CARTESIAN_POINT('Ctrl Pts',(0.942396797659656,-6.70332924210075,
28.2415112493812));
#190109=CARTESIAN_POINT('Ctrl Pts',(1.11450088340976,-6.67459188122232,
28.2497219051978));
#190110=CARTESIAN_POINT('Ctrl Pts',(1.28670638592829,-6.6458375861133,28.2579373993549));
#190111=CARTESIAN_POINT('Ctrl Pts',(1.45765523873773,-6.6104385500377,28.2661528935121));
#190112=CARTESIAN_POINT('Ctrl Pts',(1.62680772441081,-6.56854516828478,
28.2743683876692));
#190113=CARTESIAN_POINT('Ctrl Pts',(1.79622265327796,-6.5265867881792,28.2825966283167));
#190114=CARTESIAN_POINT('Ctrl Pts',(1.96383530081299,-6.47811402600845,
28.2908248689642));
#190115=CARTESIAN_POINT('Ctrl Pts',(2.12912227518776,-6.42332681227565,
28.2990531096118));
#190116=CARTESIAN_POINT('Ctrl Pts',(2.27934174665302,-6.37353398182954,
28.306531266713));
#190117=CARTESIAN_POINT('Ctrl Pts',(2.42764029131424,-6.31852615803697,
28.3140094238142));
#190118=CARTESIAN_POINT('Ctrl Pts',(2.57364188029135,-6.25848675575897,
28.3214875809154));
#190119=CARTESIAN_POINT('Ctrl Pts',(2.73118496911533,-6.19370120820232,
28.3295568901379));
#190120=CARTESIAN_POINT('Ctrl Pts',(2.88656897566729,-6.12284426780645,
28.3376261993604));
#190121=CARTESIAN_POINT('Ctrl Pts',(3.03927934623883,-6.04607889921444,
28.3456955085829));
#190122=CARTESIAN_POINT('Ctrl Pts',(3.19179924547299,-5.96940927790119,
28.3537547531837));
#190123=CARTESIAN_POINT('Ctrl Pts',(3.34165181482521,-5.8868460570315,28.3618139977845));
#190124=CARTESIAN_POINT('Ctrl Pts',(3.4883393221044,-5.79860136359279,28.3698732423852));
#190125=CARTESIAN_POINT('Ctrl Pts',(3.634876060526,-5.71044737011802,28.3779242035055));
#190126=CARTESIAN_POINT('Ctrl Pts',(3.77825389361887,-5.61662371561286,
28.3859751646258));
#190127=CARTESIAN_POINT('Ctrl Pts',(3.91799678858754,-5.5173897963274,28.3940261257461));
#190128=CARTESIAN_POINT('Ctrl Pts',(4.05762667297448,-5.41823612786935,
28.4020705760252));
#190129=CARTESIAN_POINT('Ctrl Pts',(4.19362716730172,-5.31368111786948,
28.4101150263042));
#190130=CARTESIAN_POINT('Ctrl Pts',(4.32554859867539,-5.20402904685373,
28.4181594765833));
#190131=CARTESIAN_POINT('Ctrl Pts',(4.45739222108193,-5.09444165004824,
28.4261991821415));
#190132=CARTESIAN_POINT('Ctrl Pts',(4.58516128370464,-4.97976341480909,
28.4342388876997));
#190133=CARTESIAN_POINT('Ctrl Pts',(4.70843686644385,-4.86034065418386,
28.4422785932579));
#190134=CARTESIAN_POINT('Ctrl Pts',(4.83437328673022,-4.73834021711699,
28.4504918315624));
#190135=CARTESIAN_POINT('Ctrl Pts',(4.95561971810547,-4.61138834123703,
28.4587050698669));
#190136=CARTESIAN_POINT('Ctrl Pts',(5.07176663562319,-4.47989644900185,
28.4669183081713));
#190137=CARTESIAN_POINT('Ctrl Pts',(5.18542295415974,-4.35122420605082,
28.4749554257195));
#190138=CARTESIAN_POINT('Ctrl Pts',(5.29419599707397,-4.21820498034962,
28.4829925432677));
#190139=CARTESIAN_POINT('Ctrl Pts',(5.3977409055983,-4.08125986872079,28.4910296608158));
#190140=CARTESIAN_POINT('Ctrl Pts',(5.50129676851557,-3.94430026916991,
28.4990676286399));
#190141=CARTESIAN_POINT('Ctrl Pts',(5.59962317029237,-3.80341425466986,
28.5071055964641));
#190142=CARTESIAN_POINT('Ctrl Pts',(5.69241719540748,-3.6590539041437,28.5151435642882));
#190143=CARTESIAN_POINT('Ctrl Pts',(5.78523942345759,-3.51464967810317,
28.5231839750959));
#190144=CARTESIAN_POINT('Ctrl Pts',(5.87252572601679,-3.36676932827826,
28.5312243859036));
#190145=CARTESIAN_POINT('Ctrl Pts',(5.95401803739081,-3.21589151098493,
28.5392647967114));
#190146=CARTESIAN_POINT('Ctrl Pts',(6.03859029851253,-3.05931136315917,
28.5476090896992));
#190147=CARTESIAN_POINT('Ctrl Pts',(6.11692183960478,-2.89950313826752,
28.555953382687));
#190148=CARTESIAN_POINT('Ctrl Pts',(6.18877843488688,-2.73702584640319,
28.5642976756748));
#190149=CARTESIAN_POINT('Ctrl Pts',(6.25814043682762,-2.58018916092742,
28.5723522858903));
#190150=CARTESIAN_POINT('Ctrl Pts',(6.32146945744517,-2.42086598918543,
28.5804068961058));
#190151=CARTESIAN_POINT('Ctrl Pts',(6.37860554822771,-2.25957523887096,
28.5884615063214));
#190152=CARTESIAN_POINT('Ctrl Pts',(6.43578489183809,-2.09816238918004,
28.5965222139907));
#190153=CARTESIAN_POINT('Ctrl Pts',(6.4867618604932,-1.93477934931919,28.6045829216599));
#190154=CARTESIAN_POINT('Ctrl Pts',(6.53142732344164,-1.76995653014417,
28.6126436293292));
#190155=CARTESIAN_POINT('Ctrl Pts',(6.57615576201672,-1.6049013206694,28.6207157021133));
#190156=CARTESIAN_POINT('Ctrl Pts',(6.61455485703562,-1.43840264222174,
28.6287877748974));
#190157=CARTESIAN_POINT('Ctrl Pts',(6.64656702892482,-1.27099792683131,
28.6368598476815));
#190158=CARTESIAN_POINT('Ctrl Pts',(6.64992006070939,-1.25346355479516,
28.637705335976));
#190159=CARTESIAN_POINT('Ctrl Pts',(6.65320306885883,-1.23591924395092,
28.6385508242705));
#190160=CARTESIAN_POINT('Ctrl Pts',(6.65641602025913,-1.21836561230103,
28.6393963125649));
#190161=CARTESIAN_POINT('Ctrl Pts',(6.68808206901938,-1.04536139079481,
28.6477292346116));
#190162=CARTESIAN_POINT('Ctrl Pts',(6.71303982097927,-0.870899705245018,
28.6560621566584));
#190163=CARTESIAN_POINT('Ctrl Pts',(6.73116032192443,-0.695535563828484,
28.6643950787051));
#190164=CARTESIAN_POINT('Ctrl Pts',(6.74925940883177,-0.520378660300522,
28.6727181532587));
#190165=CARTESIAN_POINT('Ctrl Pts',(6.7605373052033,-0.344321768575867,
28.6810412278123));
#190166=CARTESIAN_POINT('Ctrl Pts',(6.76491599548732,-0.167930265288237,
28.6893643023659));
#190167=CARTESIAN_POINT('Ctrl Pts',(6.76929031495499,0.00828516369006133,
28.6976790688119));
#190168=CARTESIAN_POINT('Ctrl Pts',(6.76677914047182,0.184834193098326,
28.7059938352578));
#190169=CARTESIAN_POINT('Ctrl Pts',(6.75735618633986,0.361145913633897,
28.7143086017038));
#190170=CARTESIAN_POINT('Ctrl Pts',(6.74794090973028,0.537313981005039,
28.7226165935433));
#190171=CARTESIAN_POINT('Ctrl Pts',(6.73162509318644,0.713244778819943,
28.7309245853828));
#190172=CARTESIAN_POINT('Ctrl Pts',(6.70843450512467,0.888366754472935,
28.7392325772224));
#190173=CARTESIAN_POINT('Ctrl Pts',(6.68525856039957,1.06337815207409,28.7475353231095));
#190174=CARTESIAN_POINT('Ctrl Pts',(6.65521654073805,1.23758140135111,28.7558380689966));
#190175=CARTESIAN_POINT('Ctrl Pts',(6.61838612327401,1.41040920418651,28.7641408148837));
#190176=CARTESIAN_POINT('Ctrl Pts',(6.58157075722798,1.58316637780612,28.7724401677032));
#190177=CARTESIAN_POINT('Ctrl Pts',(6.53797259358396,1.75454888526294,28.7807395205226));
#190178=CARTESIAN_POINT('Ctrl Pts',(6.48772062103169,1.9239984780244,28.789038873342));
#190179=CARTESIAN_POINT('Ctrl Pts',(6.43747933623078,2.09341203170075,28.7973364610284));
#190180=CARTESIAN_POINT('Ctrl Pts',(6.38058716068607,2.26089315632913,28.8056340487147));
#190181=CARTESIAN_POINT('Ctrl Pts',(6.3172233400068,2.42589741590062,28.8139316364011));
#190182=CARTESIAN_POINT('Ctrl Pts',(6.25386246625003,2.59089400145942,28.8222288381835));
#190183=CARTESIAN_POINT('Ctrl Pts',(6.18403067200167,2.75341362681236,28.8305260399659));
#190184=CARTESIAN_POINT('Ctrl Pts',(6.10795593739177,2.91293035736879,28.8388232417483));
#190185=CARTESIAN_POINT('Ctrl Pts',(6.03187209968865,3.07246617567722,28.8471214363729));
#190186=CARTESIAN_POINT('Ctrl Pts',(5.94954398337093,3.2289980694472,28.8554196309974));
#190187=CARTESIAN_POINT('Ctrl Pts',(5.86124633355747,3.38202312490012,28.863717825622));
#190188=CARTESIAN_POINT('Ctrl Pts',(5.77288658297748,3.53515580465857,28.8720218564635));
#190189=CARTESIAN_POINT('Ctrl Pts',(5.67854908367685,3.68477641604058,28.8803258873051));
#190190=CARTESIAN_POINT('Ctrl Pts',(5.57855335644909,3.83040878357006,28.8886299181467));
#190191=CARTESIAN_POINT('Ctrl Pts',(5.47852126802292,3.97609410703631,28.8969369685624));
#190192=CARTESIAN_POINT('Ctrl Pts',(5.3728270538298,4.11778801356652,28.9052440189781));
#190193=CARTESIAN_POINT('Ctrl Pts',(5.26183176885043,4.25504587946081,28.9135510693938));
#190194=CARTESIAN_POINT('Ctrl Pts',(5.15071781117833,4.39245049717925,28.9218670014484));
#190195=CARTESIAN_POINT('Ctrl Pts',(5.0342916831421,4.52540933192618,28.9301829335031));
#190196=CARTESIAN_POINT('Ctrl Pts',(4.91295341747405,4.65351240653015,28.9384988655577));
#190197=CARTESIAN_POINT('Ctrl Pts',(4.82148605550475,4.75007922516458,28.9447675917766));
#190198=CARTESIAN_POINT('Ctrl Pts',(4.72722819245259,4.84388749541669,28.9510363179955));
#190199=CARTESIAN_POINT('Ctrl Pts',(4.63036404117561,4.93477637245984,28.9573050442145));
#190200=CARTESIAN_POINT('Ctrl Pts',(4.49979797673741,5.05728818741187,28.965754846341));
#190201=CARTESIAN_POINT('Ctrl Pts',(4.36425593395156,5.1747189922691,28.9742046484675));
#190202=CARTESIAN_POINT('Ctrl Pts',(4.22415975134858,5.28665900121114,28.9826544505941));
#190203=CARTESIAN_POINT('Ctrl Pts',(4.08417659437682,5.39850870012521,28.9910974356596));
#190204=CARTESIAN_POINT('Ctrl Pts',(3.93964687644033,5.50487622392519,28.9995404207252));
#190205=CARTESIAN_POINT('Ctrl Pts',(3.79102756981362,5.60539017062265,29.0079834057908));
#190206=CARTESIAN_POINT('Ctrl Pts',(3.6425351055428,5.70581833152224,29.0164191850084));
#190207=CARTESIAN_POINT('Ctrl Pts',(3.48996028683844,5.8004026930279,29.0248549642261));
#190208=CARTESIAN_POINT('Ctrl Pts',(3.33379134897792,5.88881348333261,29.0332907434438));
#190209=CARTESIAN_POINT('Ctrl Pts',(3.25642392211295,5.93261294465112,29.0374699005836));
#190210=CARTESIAN_POINT('Ctrl Pts',(3.17817486874918,5.974897876672,29.0416490577234));
#190211=CARTESIAN_POINT('Ctrl Pts',(3.09910619832131,6.01563211736941,29.0458282148631));
#190212=CARTESIAN_POINT('Ctrl Pts',(3.09910619832137,6.01563211736939,27.0457199708935));
#190213=CARTESIAN_POINT('Ctrl Pts',(3.07316115263563,6.02899836888404,27.0470975320348));
#190214=CARTESIAN_POINT('Ctrl Pts',(3.04713223696845,6.04219542789079,27.048475093176));
#190215=CARTESIAN_POINT('Ctrl Pts',(3.0210217104256,6.05522227710405,27.0498526543173));
#190216=CARTESIAN_POINT('Ctrl Pts',(2.84958893181414,6.14075210943112,27.0588972491771));
#190217=CARTESIAN_POINT('Ctrl Pts',(2.67447812095438,6.21901965298881,27.067941844037));
#190218=CARTESIAN_POINT('Ctrl Pts',(2.49629646023971,6.28973711553946,27.0769864388968));
#190219=CARTESIAN_POINT('Ctrl Pts',(2.31827830924617,6.36038968368666,27.0860227339171));
#190220=CARTESIAN_POINT('Ctrl Pts',(2.13719515544994,6.42350591570578,27.0950590289375));
#190221=CARTESIAN_POINT('Ctrl Pts',(1.95367442427087,6.47884598087884,27.1040953239578));
#190222=CARTESIAN_POINT('Ctrl Pts',(1.77047844741676,6.53408811746698,27.1131156285455));
#190223=CARTESIAN_POINT('Ctrl Pts',(1.58485373412527,6.58158149665532,27.1221359331332));
#190224=CARTESIAN_POINT('Ctrl Pts',(1.39744296704592,6.62113601686704,27.1311562377209));
#190225=CARTESIAN_POINT('Ctrl Pts',(1.2102682074221,6.66064072584424,27.1401651829873));
#190226=CARTESIAN_POINT('Ctrl Pts',(1.02131211468574,6.69222647833871,27.1491741282536));
#190227=CARTESIAN_POINT('Ctrl Pts',(0.831230156072832,6.71575352642093,
27.1581830735199));
#190228=CARTESIAN_POINT('Ctrl Pts',(0.641579833347911,6.73922714955759,
27.1671715613787));
#190229=CARTESIAN_POINT('Ctrl Pts',(0.450808983602992,6.75467856671836,
27.1761600492375));
#190230=CARTESIAN_POINT('Ctrl Pts',(0.259580348682078,6.76201945002956,
27.1851485370963));
#190231=CARTESIAN_POINT('Ctrl Pts',(0.0918035402349528,6.76846006481325,
27.1930346981116));
#190232=CARTESIAN_POINT('Ctrl Pts',(-0.0763253826688315,6.76865819405494,
27.2009208591268));
#190233=CARTESIAN_POINT('Ctrl Pts',(-0.244353506158314,6.76258681009184,
27.2088070201421));
#190234=CARTESIAN_POINT('Ctrl Pts',(-0.417395179683282,6.75633427081586,
27.2169284849983));
#190235=CARTESIAN_POINT('Ctrl Pts',(-0.590252428843142,6.74343366726387,
27.2250499498544));
#190236=CARTESIAN_POINT('Ctrl Pts',(-0.762373606214561,6.72391816462302,
27.2331714147106));
#190237=CARTESIAN_POINT('Ctrl Pts',(-0.934482508813035,6.70440405372471,
27.2412923003868));
#190238=CARTESIAN_POINT('Ctrl Pts',(-1.10585508032576,6.67827602463097,
27.249413186063));
#190239=CARTESIAN_POINT('Ctrl Pts',(-1.27594518429308,6.64561907474987,
27.2575340717392));
#190240=CARTESIAN_POINT('Ctrl Pts',(-1.44605561889158,6.61295822142942,
27.2656559280935));
#190241=CARTESIAN_POINT('Ctrl Pts',(-1.61488292132075,6.57376696360522,
27.2737777844478));
#190242=CARTESIAN_POINT('Ctrl Pts',(-1.78189157647687,6.52818132481634,
27.281899640802));
#190243=CARTESIAN_POINT('Ctrl Pts',(-1.94902207908151,6.48256242730939,
27.2900274227622));
#190244=CARTESIAN_POINT('Ctrl Pts',(-2.11433093068078,6.43053992756398,
27.2981552047224));
#190245=CARTESIAN_POINT('Ctrl Pts',(-2.27729758842626,6.37229979628611,
27.3062829866826));
#190246=CARTESIAN_POINT('Ctrl Pts',(-2.44033063273094,6.31403594014343,
27.314414079599));
#190247=CARTESIAN_POINT('Ctrl Pts',(-2.60101924174457,6.24954954010989,
27.3225451725155));
#190248=CARTESIAN_POINT('Ctrl Pts',(-2.75886350925092,6.17907445636672,
27.3306762654319));
#190249=CARTESIAN_POINT('Ctrl Pts',(-2.91688005717841,6.10852245201504,
27.3388162330965));
#190250=CARTESIAN_POINT('Ctrl Pts',(-3.07204573492137,6.03196887041107,
27.346956200761));
#190251=CARTESIAN_POINT('Ctrl Pts',(-3.22388519457764,5.94969354271152,
27.3550961684256));
#190252=CARTESIAN_POINT('Ctrl Pts',(-3.30263570347203,5.9070220004098,27.359317907606));
#190253=CARTESIAN_POINT('Ctrl Pts',(-3.38049194906336,5.86281208461277,
27.3635396467864));
#190254=CARTESIAN_POINT('Ctrl Pts',(-3.45739080292563,5.81710734264422,
27.3677613859669));
#190255=CARTESIAN_POINT('Ctrl Pts',(-3.61112896767471,5.72573324800347,
27.3762015954245));
#190256=CARTESIAN_POINT('Ctrl Pts',(-3.76135650917294,5.62819308269307,
27.3846418048821));
#190257=CARTESIAN_POINT('Ctrl Pts',(-3.90756625773005,5.52478189084869,
27.3930820143397));
#190258=CARTESIAN_POINT('Ctrl Pts',(-4.05366523074137,5.42144904830269,
27.4015158290883));
#190259=CARTESIAN_POINT('Ctrl Pts',(-4.19575220767966,5.31225423823208,
27.4099496438368));
#190260=CARTESIAN_POINT('Ctrl Pts',(-4.33334775121705,5.19753655754552,
27.4183834585853));
#190261=CARTESIAN_POINT('Ctrl Pts',(-4.47086019788112,5.08288815730464,
27.4268121799739));
#190262=CARTESIAN_POINT('Ctrl Pts',(-4.60388636334862,4.96272374902026,
27.4352409013624));
#190263=CARTESIAN_POINT('Ctrl Pts',(-4.73197843795805,4.83742380433016,
27.443669622751));
#190264=CARTESIAN_POINT('Ctrl Pts',(-4.86001282459775,4.71218029013694,
27.4520945481527));
#190265=CARTESIAN_POINT('Ctrl Pts',(-4.98311731306697,4.58180608392272,
27.4605194735544));
#190266=CARTESIAN_POINT('Ctrl Pts',(-5.1008793537298,4.44672000677949,27.4689443989562));
#190267=CARTESIAN_POINT('Ctrl Pts',(-5.21860642687796,4.31167404124064,
27.4773668227139));
#190268=CARTESIAN_POINT('Ctrl Pts',(-5.33099399684997,4.17191924601885,
27.4857892464717));
#190269=CARTESIAN_POINT('Ctrl Pts',(-5.4376681125929,4.02790944502112,27.4942116702294));
#190270=CARTESIAN_POINT('Ctrl Pts',(-5.54434390601232,3.88389737916414,
27.5026342264476));
#190271=CARTESIAN_POINT('Ctrl Pts',(-5.64530586187403,3.73563043777246,
27.5110567826658));
#190272=CARTESIAN_POINT('Ctrl Pts',(-5.74022148867819,3.58359404242684,
27.519479338884));
#190273=CARTESIAN_POINT('Ctrl Pts',(-5.83514032175027,3.43155251126289,
27.5279021796178));
#190274=CARTESIAN_POINT('Ctrl Pts',(-5.92401224172111,3.27574155512807,
27.5363250203515));
#190275=CARTESIAN_POINT('Ctrl Pts',(-6.00654904914689,3.11667411196497,
27.5447478610853));
#190276=CARTESIAN_POINT('Ctrl Pts',(-6.08910016773277,2.95757908789926,
27.5531721622659));
#190277=CARTESIAN_POINT('Ctrl Pts',(-6.16531383015456,2.79522674714078,
27.5615964634465));
#190278=CARTESIAN_POINT('Ctrl Pts',(-6.234948446618,2.63015339248795,27.5700207646271));
#190279=CARTESIAN_POINT('Ctrl Pts',(-6.30460486185674,2.46502836243069,
27.5784477029939));
#190280=CARTESIAN_POINT('Ctrl Pts',(-6.36767799538117,2.29718092743717,
27.5868746413607));
#190281=CARTESIAN_POINT('Ctrl Pts',(-6.42397478820149,2.12716640640822,
27.5953015797276));
#190282=CARTESIAN_POINT('Ctrl Pts',(-6.48032219891496,1.95699902095436,
27.6037360949712));
#190283=CARTESIAN_POINT('Ctrl Pts',(-6.52988098962663,1.78466097304688,
27.6121706102149));
#190284=CARTESIAN_POINT('Ctrl Pts',(-6.57250795993592,1.61072285529788,
27.6206051254585));
#190285=CARTESIAN_POINT('Ctrl Pts',(-6.61515551943702,1.43670072394806,
27.6290437146453));
#190286=CARTESIAN_POINT('Ctrl Pts',(-6.65086450963091,1.26107730706265,
27.637482303832));
#190287=CARTESIAN_POINT('Ctrl Pts',(-6.67954296945572,1.08443290211735,
27.6459208930188));
#190288=CARTESIAN_POINT('Ctrl Pts',(-6.70825348531028,0.907591048692114,
27.6543689146391));
#190289=CARTESIAN_POINT('Ctrl Pts',(-6.72991772269395,0.729726257331115,
27.6628169362594));
#190290=CARTESIAN_POINT('Ctrl Pts',(-6.74449552026904,0.551424679417716,
27.6712649578797));
#190291=CARTESIAN_POINT('Ctrl Pts',(-6.75278130646117,0.450080923977191,
27.6760666777919));
#190292=CARTESIAN_POINT('Ctrl Pts',(-6.75877869763147,0.348596103748422,
27.6808683977041));
#190293=CARTESIAN_POINT('Ctrl Pts',(-6.76248782396277,0.247077782803984,
27.6856701176163));
#190294=CARTESIAN_POINT('Ctrl Pts',(-6.76545140137005,0.165965042092728,
27.6895066730142));
#190295=CARTESIAN_POINT('Ctrl Pts',(-6.76695633114201,0.0847788957426476,
27.6933432284121));
#190296=CARTESIAN_POINT('Ctrl Pts',(-6.76699906337201,0.00356038233445201,
27.69717978381));
#190297=CARTESIAN_POINT('',(-6.76699961187957,-0.00229190351974674,27.3028202162279));
#190298=CARTESIAN_POINT('Ctrl Pts',(3.0991061983213,6.01563211736942,26.6512942524228));
#190299=CARTESIAN_POINT('Ctrl Pts',(2.94383276466504,6.09562518398154,26.6594981890752));
#190300=CARTESIAN_POINT('Ctrl Pts',(2.78554342077026,6.16955974932361,26.6677021257276));
#190301=CARTESIAN_POINT('Ctrl Pts',(2.62475652218203,6.23722231440109,26.6759060623801));
#190302=CARTESIAN_POINT('Ctrl Pts',(2.46378057777883,6.30496443399993,26.6841196448426));
#190303=CARTESIAN_POINT('Ctrl Pts',(2.30030154507449,6.36641968763182,26.6923332273051));
#190304=CARTESIAN_POINT('Ctrl Pts',(2.1348554629473,6.4214236079178,26.7005468097676));
#190305=CARTESIAN_POINT('Ctrl Pts',(1.96929468394184,6.47646566013093,26.7087660863648));
#190306=CARTESIAN_POINT('Ctrl Pts',(1.80176448095945,6.52504736574828,26.7169853629619));
#190307=CARTESIAN_POINT('Ctrl Pts',(1.63281263736181,6.56705503945807,26.7252046395591));
#190308=CARTESIAN_POINT('Ctrl Pts',(1.46362873059184,6.60912041265084,26.7334352057129));
#190309=CARTESIAN_POINT('Ctrl Pts',(1.29301963370594,6.64459365085365,26.7416657718666));
#190310=CARTESIAN_POINT('Ctrl Pts',(1.12154069219706,6.67341258096232,26.7498963380204));
#190311=CARTESIAN_POINT('Ctrl Pts',(1.07487975720384,6.68125446645883,26.7521359477875));
#190312=CARTESIAN_POINT('Ctrl Pts',(1.02815442916004,6.68860394334448,26.7543755575546));
#190313=CARTESIAN_POINT('Ctrl Pts',(0.981375910960085,6.69546042639244,
26.7566151673218));
#190314=CARTESIAN_POINT('Ctrl Pts',(0.812833009482774,6.72016432021596,
26.7646844765443));
#190315=CARTESIAN_POINT('Ctrl Pts',(0.643047741566264,6.73854524219892,
26.7727537857668));
#190316=CARTESIAN_POINT('Ctrl Pts',(0.472545764272061,6.7504806866377,26.7808230949893));
#190317=CARTESIAN_POINT('Ctrl Pts',(0.302256449284434,6.76240124433331,
26.7888823395901));
#190318=CARTESIAN_POINT('Ctrl Pts',(0.131252571120187,6.76789229474629,
26.7969415841908));
#190319=CARTESIAN_POINT('Ctrl Pts',(-0.0399295845166925,6.76688219405956,
26.8050008287916));
#190320=CARTESIAN_POINT('Ctrl Pts',(-0.210935795122136,6.76587313157799,
26.8130517899119));
#190321=CARTESIAN_POINT('Ctrl Pts',(-0.382119548577863,6.75837621755593,
26.8211027510321));
#190322=CARTESIAN_POINT('Ctrl Pts',(-0.552939091407244,6.74437153196603,
26.8291537121524));
#190323=CARTESIAN_POINT('Ctrl Pts',(-0.723620491858464,6.73037817201569,
26.8371981624315));
#190324=CARTESIAN_POINT('Ctrl Pts',(-0.893937897912533,6.70988754566047,
26.8452426127106));
#190325=CARTESIAN_POINT('Ctrl Pts',(-1.06334931334904,6.68293178461371,
26.8532870629897));
#190326=CARTESIAN_POINT('Ctrl Pts',(-1.23266080774108,6.65599192242353,
26.8613267685479));
#190327=CARTESIAN_POINT('Ctrl Pts',(-1.40106700770738,6.6225945750113,26.8693664741062));
#190328=CARTESIAN_POINT('Ctrl Pts',(-1.56803090743718,6.58282371580173,
26.8774061796644));
#190329=CARTESIAN_POINT('Ctrl Pts',(-1.7385986336788,6.54219442385881,26.8856194179688));
#190330=CARTESIAN_POINT('Ctrl Pts',(-1.90766069180216,6.49491338734593,
26.8938326562733));
#190331=CARTESIAN_POINT('Ctrl Pts',(-2.07465492144769,6.4411253641668,26.9020458945777));
#190332=CARTESIAN_POINT('Ctrl Pts',(-2.23806820665575,6.38849074564611,
26.9100830121259));
#190333=CARTESIAN_POINT('Ctrl Pts',(-2.39950108146646,6.32962550801559,
26.9181201296741));
#190334=CARTESIAN_POINT('Ctrl Pts',(-2.55844205524812,6.2647157357647,26.9261572472223));
#190335=CARTESIAN_POINT('Ctrl Pts',(-2.71739984397433,6.19979909647256,
26.9341952150464));
#190336=CARTESIAN_POINT('Ctrl Pts',(-2.87386486079827,6.12883679043341,
26.9422331828705));
#190337=CARTESIAN_POINT('Ctrl Pts',(-3.02734586883941,6.05206295327643,
26.9502711506946));
#190338=CARTESIAN_POINT('Ctrl Pts',(-3.18087352444107,5.97526578220823,
26.9583115615023));
#190339=CARTESIAN_POINT('Ctrl Pts',(-3.33141503206904,5.89265373127158,
26.9663519723101));
#190340=CARTESIAN_POINT('Ctrl Pts',(-3.47850415630701,5.80450668313466,
26.9743923831178));
#190341=CARTESIAN_POINT('Ctrl Pts',(-3.63115241984803,5.71302817373379,
26.9827366761056));
#190342=CARTESIAN_POINT('Ctrl Pts',(-3.78008185807882,5.61558833844509,
26.9910809690934));
#190343=CARTESIAN_POINT('Ctrl Pts',(-3.92480572123883,5.51254832636694,
26.9994252620812));
#190344=CARTESIAN_POINT('Ctrl Pts',(-4.06450531092812,5.4130854797113,27.0074798722967));
#190345=CARTESIAN_POINT('Ctrl Pts',(-4.20028618576589,5.30840505205388,
27.0155344825122));
#190346=CARTESIAN_POINT('Ctrl Pts',(-4.33174593792675,5.19887162077071,
27.0235890927278));
#190347=CARTESIAN_POINT('Ctrl Pts',(-4.46330520697713,5.08925527113269,
27.031649800397));
#190348=CARTESIAN_POINT('Ctrl Pts',(-4.59053656432683,4.97477885105254,
27.0397105080663));
#190349=CARTESIAN_POINT('Ctrl Pts',(-4.71307542986726,4.85584276849875,
27.0477712157355));
#190350=CARTESIAN_POINT('Ctrl Pts',(-4.83578706786635,4.73673899319445,
27.0558432885197));
#190351=CARTESIAN_POINT('Ctrl Pts',(-4.95379275822236,4.61316327767268,
27.0639153613038));
#190352=CARTESIAN_POINT('Ctrl Pts',(-5.06676866695437,4.48554838069656,
27.0719874340879));
#190353=CARTESIAN_POINT('Ctrl Pts',(-5.07860203502974,4.47218168982619,
27.0728329223824));
#190354=CARTESIAN_POINT('Ctrl Pts',(-5.09038026136851,4.45877071037642,
27.0736784106768));
#190355=CARTESIAN_POINT('Ctrl Pts',(-5.10210300204977,4.44531595687806,
27.0745238989712));
#190356=CARTESIAN_POINT('Ctrl Pts',(-5.21798439699456,4.3123133044761,27.0828817024604));
#190357=CARTESIAN_POINT('Ctrl Pts',(-5.32881037871687,4.17460609882494,
27.0912395059495));
#190358=CARTESIAN_POINT('Ctrl Pts',(-5.43418447660398,4.03260809827045,
27.0995973094387));
#190359=CARTESIAN_POINT('Ctrl Pts',(-5.54094314081068,3.88874431045931,
27.1080649305533));
#190360=CARTESIAN_POINT('Ctrl Pts',(-5.64210535689717,3.74047639141668,
27.116532551668));
#190361=CARTESIAN_POINT('Ctrl Pts',(-5.7372978182351,3.58827294737661,27.1250001727826));
#190362=CARTESIAN_POINT('Ctrl Pts',(-5.83100808026938,3.43843939519139,
27.1333359483504));
#190363=CARTESIAN_POINT('Ctrl Pts',(-5.91893291945275,3.28479227163124,
27.1416717239182));
#190364=CARTESIAN_POINT('Ctrl Pts',(-6.00075701597266,3.1278114129939,27.150007499486));
#190365=CARTESIAN_POINT('Ctrl Pts',(-6.08251488675048,2.97095760951879,
27.1583365283502));
#190366=CARTESIAN_POINT('Ctrl Pts',(-6.15818169342941,2.81077575102921,
27.1666655572145));
#190367=CARTESIAN_POINT('Ctrl Pts',(-6.2274864770947,2.64777287122643,27.1749945860787));
#190368=CARTESIAN_POINT('Ctrl Pts',(-6.29674637522643,2.48487556092182,
27.1833182206125));
#190369=CARTESIAN_POINT('Ctrl Pts',(-6.35965232603162,2.31916118643877,
27.1916418551463));
#190370=CARTESIAN_POINT('Ctrl Pts',(-6.41598012033015,2.15115970944242,
27.1999654896801));
#190371=CARTESIAN_POINT('Ctrl Pts',(-6.47398342659767,1.97816090405742,
27.2085367168893));
#190372=CARTESIAN_POINT('Ctrl Pts',(-6.52501100444624,1.80273715993301,
27.2171079440984));
#190373=CARTESIAN_POINT('Ctrl Pts',(-6.56887177036432,1.62548843875023,
27.2256791713076));
#190374=CARTESIAN_POINT('Ctrl Pts',(-6.61143244030448,1.45349362375625,
27.2339963350551));
#190375=CARTESIAN_POINT('Ctrl Pts',(-6.64724502646991,1.279780837463,27.2423134988025));
#190376=CARTESIAN_POINT('Ctrl Pts',(-6.67618580650384,1.10491270109302,
27.25063066255));
#190377=CARTESIAN_POINT('Ctrl Pts',(-6.70645266264653,0.922032048904484,
27.25932892149));
#190378=CARTESIAN_POINT('Ctrl Pts',(-6.72920303762109,0.737888063829979,
27.26802718043));
#190379=CARTESIAN_POINT('Ctrl Pts',(-6.74435547311584,0.553134931325414,
27.27672543937));
#190380=CARTESIAN_POINT('Ctrl Pts',(-6.7595079086106,0.368381798820848,
27.2854236983099));
#190381=CARTESIAN_POINT('Ctrl Pts',(-6.76706237481184,0.183019949639337,
27.2941219572499));
#190382=CARTESIAN_POINT('Ctrl Pts',(-6.76699961187985,-0.00229190270927458,
27.3028202161899));
#190383=CARTESIAN_POINT('Ctrl Pts',(-6.76699961187957,-0.00229190351973855,
27.3028202162279));
#190384=CARTESIAN_POINT('Ctrl Pts',(-6.76692935620143,-0.209726528320418,
27.3125568847506));
#190385=CARTESIAN_POINT('Ctrl Pts',(-6.75731700521489,-0.416851375284489,
27.3222935532733));
#190386=CARTESIAN_POINT('Ctrl Pts',(-6.7382722925091,-0.622876803231719,
27.332030221796));
#190387=CARTESIAN_POINT('Ctrl Pts',(-6.7185813253142,-0.835893402940784,
27.3420972899335));
#190388=CARTESIAN_POINT('Ctrl Pts',(-6.68880680709447,-1.04773457373278,
27.3521643580709));
#190389=CARTESIAN_POINT('Ctrl Pts',(-6.64912538009576,-1.25754549808999,
27.3622314262084));
#190390=CARTESIAN_POINT('Ctrl Pts',(-6.60944395309706,-1.4673564224472,
27.3722984943459));
#190391=CARTESIAN_POINT('Ctrl Pts',(-6.55985570281287,-1.67513707154593,
27.3823655624833));
#190392=CARTESIAN_POINT('Ctrl Pts',(-6.50059196810456,-1.88005134616439,
27.3924326306208));
#190393=CARTESIAN_POINT('Ctrl Pts',(-6.45084615562013,-2.05205581282049,
27.4008828993441));
#190394=CARTESIAN_POINT('Ctrl Pts',(-6.39422714905118,-2.22223068762529,
27.4093331680675));
#190395=CARTESIAN_POINT('Ctrl Pts',(-6.33088855698631,-2.39000817551317,
27.4177834367908));
#190396=CARTESIAN_POINT('Ctrl Pts',(-6.26760586337782,-2.55763759407583,
27.4262262478653));
#190397=CARTESIAN_POINT('Ctrl Pts',(-6.19761552091997,-2.72287353407569,
27.4346690589398));
#190398=CARTESIAN_POINT('Ctrl Pts',(-6.12112090541313,-2.88516340287936,
27.4431118700143));
#190399=CARTESIAN_POINT('Ctrl Pts',(-6.04468338406107,-3.04733214155083,
27.4515483795321));
#190400=CARTESIAN_POINT('Ctrl Pts',(-5.96175140807754,-3.20655889344229,
27.4599848890498));
#190401=CARTESIAN_POINT('Ctrl Pts',(-5.87257656555222,-3.36231073545068,
27.4684213985675));
#190402=CARTESIAN_POINT('Ctrl Pts',(-5.78346553242522,-3.5179511286351,
27.4768518713087));
#190403=CARTESIAN_POINT('Ctrl Pts',(-5.68812070747364,-3.67012128457289,
27.4852823440499));
#190404=CARTESIAN_POINT('Ctrl Pts',(-5.58683983253178,-3.81831241330988,
27.4937128167911));
#190405=CARTESIAN_POINT('Ctrl Pts',(-5.4856024979637,-3.96643983508205,
27.502139665295));
#190406=CARTESIAN_POINT('Ctrl Pts',(-5.37843438744359,-4.1105913664876,
27.5105665137988));
#190407=CARTESIAN_POINT('Ctrl Pts',(-5.26567716922619,-4.25028621971392,
27.5189933623026));
#190408=CARTESIAN_POINT('Ctrl Pts',(-5.15295475513509,-4.38993795412807,
27.5274176097392));
#190409=CARTESIAN_POINT('Ctrl Pts',(-5.03464688174096,-4.52513549595337,
27.5358418571758));
#190410=CARTESIAN_POINT('Ctrl Pts',(-4.9111364192475,-4.65542995560462,
27.5442661046125));
#190411=CARTESIAN_POINT('Ctrl Pts',(-4.8763358964991,-4.6921419491924,27.5466397352235));
#190412=CARTESIAN_POINT('Ctrl Pts',(-4.84112258449267,-4.72846489357281,
27.5490133658345));
#190413=CARTESIAN_POINT('Ctrl Pts',(-4.80550560803795,-4.7643892421921,
27.5513869964455));
#190414=CARTESIAN_POINT('Ctrl Pts',(-4.67617844302602,-4.89483249213332,
27.5600057773828));
#190415=CARTESIAN_POINT('Ctrl Pts',(-4.5415841897705,-5.0199592705319,27.56862455832));
#190416=CARTESIAN_POINT('Ctrl Pts',(-4.4021859336116,-5.1393626069691,27.5772433392572));
#190417=CARTESIAN_POINT('Ctrl Pts',(-4.26270394176749,-5.25883766826476,
27.5858672974438));
#190418=CARTESIAN_POINT('Ctrl Pts',(-4.11841241898026,-5.37258222844547,
27.5944912556303));
#190419=CARTESIAN_POINT('Ctrl Pts',(-3.96980693260753,-5.48023009716026,
27.6031152138169));
#190420=CARTESIAN_POINT('Ctrl Pts',(-3.8158328370502,-5.59176691608001,
27.612050726188));
#190421=CARTESIAN_POINT('Ctrl Pts',(-3.65722756505202,-5.69675811833182,
27.6209862385591));
#190422=CARTESIAN_POINT('Ctrl Pts',(-3.49457381291732,-5.79484623316896,
27.6299217509302));
#190423=CARTESIAN_POINT('Ctrl Pts',(-3.33729780225805,-5.88969130862654,
27.6385618328249));
#190424=CARTESIAN_POINT('Ctrl Pts',(-3.17623702193311,-5.97808235164047,
27.6472019147197));
#190425=CARTESIAN_POINT('Ctrl Pts',(-3.01194252884547,-6.05974349316306,
27.6558419966144));
#190426=CARTESIAN_POINT('Ctrl Pts',(-2.8392214488999,-6.14559299601794,
27.6649252242237));
#190427=CARTESIAN_POINT('Ctrl Pts',(-2.66292659147694,-6.22400395746316,
27.674008451833));
#190428=CARTESIAN_POINT('Ctrl Pts',(-2.48372148272282,-6.29471338475877,
27.6830916794423));
#190429=CARTESIAN_POINT('Ctrl Pts',(-2.3045163739687,-6.36542281205437,
27.6921749070516));
#190430=CARTESIAN_POINT('Ctrl Pts',(-2.12240139134993,-6.42843061021735,
27.701258134661));
#190431=CARTESIAN_POINT('Ctrl Pts',(-1.93805838123456,-6.48353443045739,
27.7103413622703));
#190432=CARTESIAN_POINT('Ctrl Pts',(-1.75449941811638,-6.53840388333648,
27.7193859571301));
#190433=CARTESIAN_POINT('Ctrl Pts',(-1.56856207868349,-6.58548795982809,
27.7284305519899));
#190434=CARTESIAN_POINT('Ctrl Pts',(-1.38089389838517,-6.62460723676526,
27.7374751468497));
#190435=CARTESIAN_POINT('Ctrl Pts',(-1.19339793318271,-6.66369061560816,
27.7465114418701));
#190436=CARTESIAN_POINT('Ctrl Pts',(-1.00417453088861,-6.6948237387627,
27.7555477368904));
#190437=CARTESIAN_POINT('Ctrl Pts',(-0.813882946743737,-6.71787790518701,
27.7645840319108));
#190438=CARTESIAN_POINT('Ctrl Pts',(-0.623928098479182,-6.74089127545598,
27.7736043364985));
#190439=CARTESIAN_POINT('Ctrl Pts',(-0.432909078774653,-6.75585420840333,
27.7826246410862));
#190440=CARTESIAN_POINT('Ctrl Pts',(-0.241491647624095,-6.76268961169503,
27.7916449456739));
#190441=CARTESIAN_POINT('Ctrl Pts',(-0.0503152695442017,-6.76951640712409,
27.8006538909402));
#190442=CARTESIAN_POINT('Ctrl Pts',(0.141258281686187,-6.76823609006339,
27.8096628362065));
#190443=CARTESIAN_POINT('Ctrl Pts',(0.332559284423795,-6.75882336818647,
27.8186717814728));
#190444=CARTESIAN_POINT('Ctrl Pts',(0.52342588308228,-6.74943202060828,
27.8276602693316));
#190445=CARTESIAN_POINT('Ctrl Pts',(0.714020931458135,-6.7319451415487,
27.8366487571904));
#190446=CARTESIAN_POINT('Ctrl Pts',(0.903676357486737,-6.70638934456683,
27.8456372450492));
#190447=CARTESIAN_POINT('Ctrl Pts',(1.07007289165117,-6.68396764994602,
27.8535234060645));
#190448=CARTESIAN_POINT('Ctrl Pts',(1.2357459922794,-6.65533554034296,27.8614095670797));
#190449=CARTESIAN_POINT('Ctrl Pts',(1.40024481847694,-6.62054404473896,
27.869295728095));
#190450=CARTESIAN_POINT('Ctrl Pts',(1.56965188907279,-6.58471445562782,
27.8774171929512));
#190451=CARTESIAN_POINT('Ctrl Pts',(1.73773739248944,-6.54236687363886,
27.8855386578074));
#190452=CARTESIAN_POINT('Ctrl Pts',(1.90396353704619,-6.49362855802506,
27.8936601226635));
#190453=CARTESIAN_POINT('Ctrl Pts',(2.07017782723239,-6.44489371817047,
27.9017810083397));
#190454=CARTESIAN_POINT('Ctrl Pts',(2.23453267128481,-6.38976915551758,
27.9099018940159));
#190455=CARTESIAN_POINT('Ctrl Pts',(2.39650459400326,-6.32843224905832,
27.9180227796922));
#190456=CARTESIAN_POINT('Ctrl Pts',(2.55849587699832,-6.2670880110847,27.9261446360464));
#190457=CARTESIAN_POINT('Ctrl Pts',(2.71810332948052,-6.19953008151649,
27.9342664924007));
#190458=CARTESIAN_POINT('Ctrl Pts',(2.87482268923173,-6.12598428870646,
27.942388348755));
#190459=CARTESIAN_POINT('Ctrl Pts',(3.03165638948868,-6.05238483779601,
27.9505161307152));
#190460=CARTESIAN_POINT('Ctrl Pts',(3.18559745668893,-5.9727889539448,27.9586439126753));
#190461=CARTESIAN_POINT('Ctrl Pts',(3.33616494306543,-5.88746910587744,
27.9667716946355));
#190462=CARTESIAN_POINT('Ctrl Pts',(3.48679376503956,-5.80211450167516,
27.974902787552));
#190463=CARTESIAN_POINT('Ctrl Pts',(3.63404595567512,-5.7110314779604,27.9830338804684));
#190464=CARTESIAN_POINT('Ctrl Pts',(3.77746910933932,-5.61453614539859,
27.9911649733849));
#190465=CARTESIAN_POINT('Ctrl Pts',(3.92104880338185,-5.51793549221399,
27.9993049410494));
#190466=CARTESIAN_POINT('Ctrl Pts',(4.06079081773718,-5.41591094698189,
28.007444908714));
#190467=CARTESIAN_POINT('Ctrl Pts',(4.19627482356807,-5.30881969980982,
28.0155848763785));
#190468=CARTESIAN_POINT('Ctrl Pts',(4.26654268694401,-5.25327754869835,
28.019806615559));
#190469=CARTESIAN_POINT('Ctrl Pts',(4.33566576122989,-5.19637313556894,
28.0240283547394));
#190470=CARTESIAN_POINT('Ctrl Pts',(4.40358931946146,-5.13816018683,28.0282500939198));
#190471=CARTESIAN_POINT('Ctrl Pts',(4.53938384254327,-5.02177936378421,
28.0366903033774));
#190472=CARTESIAN_POINT('Ctrl Pts',(4.6706624990829,-4.89992571217488,28.0451305128351));
#190473=CARTESIAN_POINT('Ctrl Pts',(4.79697621810871,-4.77297686595059,
28.0535707222927));
#190474=CARTESIAN_POINT('Ctrl Pts',(4.92319423577882,-4.64612420228494,
28.0620045370412));
#190475=CARTESIAN_POINT('Ctrl Pts',(5.04445458021174,-4.51418427493211,
28.0704383517898));
#190476=CARTESIAN_POINT('Ctrl Pts',(5.16034305538164,-4.37757336326583,
28.0788721665383));
#190477=CARTESIAN_POINT('Ctrl Pts',(5.27616154303811,-4.24104495383284,
28.0873008879268));
#190478=CARTESIAN_POINT('Ctrl Pts',(5.38661441399116,-4.09985143763769,
28.0957296093154));
#190479=CARTESIAN_POINT('Ctrl Pts',(5.49132572560371,-3.95444443320714,
28.1041583307039));
#190480=CARTESIAN_POINT('Ctrl Pts',(5.59598987908404,-3.80910291475547,
28.1125832561057));
#190481=CARTESIAN_POINT('Ctrl Pts',(5.69491743443856,-3.65955196183723,
28.1210081815074));
#190482=CARTESIAN_POINT('Ctrl Pts',(5.78777376227501,-3.50627492885555,
28.1294331069091));
#190483=CARTESIAN_POINT('Ctrl Pts',(5.88060251794135,-3.35304340898564,
28.1378555306669));
#190484=CARTESIAN_POINT('Ctrl Pts',(5.96736346856393,-3.19608830037617,
28.1462779544246));
#190485=CARTESIAN_POINT('Ctrl Pts',(6.04776601329938,-3.03592082379975,
28.1547003781823));
#190486=CARTESIAN_POINT('Ctrl Pts',(6.12816982253537,-2.87575082825006,
28.1631229344005));
#190487=CARTESIAN_POINT('Ctrl Pts',(6.20221487056331,-2.71236865877128,
28.1715454906187));
#190488=CARTESIAN_POINT('Ctrl Pts',(6.2696568198473,-2.54630955724993,28.1799680468369));
#190489=CARTESIAN_POINT('Ctrl Pts',(6.33710104733314,-2.38024484622059,
28.1883908875706));
#190490=CARTESIAN_POINT('Ctrl Pts',(6.39794160564978,-2.21150333184239,
28.1968137283044));
#190491=CARTESIAN_POINT('Ctrl Pts',(6.45198251134582,-2.04063977058366,
28.2052365690381));
#190492=CARTESIAN_POINT('Ctrl Pts',(6.50603278726208,-1.86974658307837,
28.2136608702188));
#190493=CARTESIAN_POINT('Ctrl Pts',(6.55328095939107,-1.69673093315023,
28.2220851713994));
#190494=CARTESIAN_POINT('Ctrl Pts',(6.59358096982342,-1.52216260444884,
28.2305094725801));
#190495=CARTESIAN_POINT('Ctrl Pts',(6.63389359597634,-1.34753962798846,
28.2389364109468));
#190496=CARTESIAN_POINT('Ctrl Pts',(6.66725364889593,-1.17136332857334,
28.2473633493137));
#190497=CARTESIAN_POINT('Ctrl Pts',(6.69356614328442,-0.994213903280681,
28.2557902876804));
#190498=CARTESIAN_POINT('Ctrl Pts',(6.71990229591283,-0.816905198387038,
28.2642248029241));
#190499=CARTESIAN_POINT('Ctrl Pts',(6.73917817934357,-0.638621949562761,
28.2726593181678));
#190500=CARTESIAN_POINT('Ctrl Pts',(6.75135054734373,-0.459950852680545,
28.2810938334114));
#190501=CARTESIAN_POINT('Ctrl Pts',(6.76352879470191,-0.281193456127886,
28.2895324225982));
#190502=CARTESIAN_POINT('Ctrl Pts',(6.76859666922576,-0.102048170990221,
28.297971011785));
#190503=CARTESIAN_POINT('Ctrl Pts',(6.76656306921745,0.0768975311863861,
28.3064096009717));
#190504=CARTESIAN_POINT('Ctrl Pts',(6.76452719610442,0.256043254172507,
28.314857622592));
#190505=CARTESIAN_POINT('Ctrl Pts',(6.75537399924369,0.434988615036042,
28.3233056442123));
#190506=CARTESIAN_POINT('Ctrl Pts',(6.73916441327626,0.613149256568786,
28.3317536658326));
#190507=CARTESIAN_POINT('Ctrl Pts',(6.72995114474939,0.714412906032747,
28.3365553857449));
#190508=CARTESIAN_POINT('Ctrl Pts',(6.71845918276298,0.815423164162881,
28.3413571056571));
#190509=CARTESIAN_POINT('Ctrl Pts',(6.70470709845652,0.916074082106259,
28.3461588255693));
#190510=CARTESIAN_POINT('Ctrl Pts',(6.68110915048584,1.08878645587435,28.3543983574201));
#190511=CARTESIAN_POINT('Ctrl Pts',(6.65080067256821,1.26082572099317,28.362637889271));
#190512=CARTESIAN_POINT('Ctrl Pts',(6.61382766119517,1.43163286774565,28.3708774211218));
#190513=CARTESIAN_POINT('Ctrl Pts',(6.5768956872807,1.60225043050297,28.3791078076681));
#190514=CARTESIAN_POINT('Ctrl Pts',(6.53331398354332,1.77163825316013,28.3873381942145));
#190515=CARTESIAN_POINT('Ctrl Pts',(6.48318023834598,1.93924289276001,28.3955685807608));
#190516=CARTESIAN_POINT('Ctrl Pts',(6.43309319470263,2.10669140205094,28.4037913003786));
#190517=CARTESIAN_POINT('Ctrl Pts',(6.37646636618576,2.27235969742888,28.4120140199964));
#190518=CARTESIAN_POINT('Ctrl Pts',(6.31344840173509,2.43570488331995,28.4202367396142));
#190519=CARTESIAN_POINT('Ctrl Pts',(6.25048627574123,2.59890533360766,28.42845217331));
#190520=CARTESIAN_POINT('Ctrl Pts',(6.18114442833579,2.75978644629152,28.4366676070058));
#190521=CARTESIAN_POINT('Ctrl Pts',(6.10562116455277,2.9178209669144,28.4448830407015));
#190522=CARTESIAN_POINT('Ctrl Pts',(6.03013671386276,3.07577427006547,28.4530942523024));
#190523=CARTESIAN_POINT('Ctrl Pts',(5.9484773266948,3.23088357436767,28.4613054639032));
#190524=CARTESIAN_POINT('Ctrl Pts',(5.86088936719711,3.38264169333317,28.469516675504));
#190525=CARTESIAN_POINT('Ctrl Pts',(5.77333077986805,3.53434892099937,28.4777251335175));
#190526=CARTESIAN_POINT('Ctrl Pts',(5.67984775842618,3.68270689412139,28.4859335915311));
#190527=CARTESIAN_POINT('Ctrl Pts',(5.58073258542937,3.82723304881305,28.4941420495446));
#190528=CARTESIAN_POINT('Ctrl Pts',(5.53657461160154,3.89162260657044,28.4977990968278));
#190529=CARTESIAN_POINT('Ctrl Pts',(5.49129931099631,3.95525193628647,28.5014561441109));
#190530=CARTESIAN_POINT('Ctrl Pts',(5.44493534228971,4.01808015329268,28.5051131913941));
#190531=CARTESIAN_POINT('Ctrl Pts',(5.33263634492837,4.17025750075933,28.5139709909885));
#190532=CARTESIAN_POINT('Ctrl Pts',(5.21406458886683,4.31757487740604,28.5228287905828));
#190533=CARTESIAN_POINT('Ctrl Pts',(5.08966368674469,4.45955295470661,28.5316865901772));
#190534=CARTESIAN_POINT('Ctrl Pts',(4.96502798744218,4.60179900476024,28.5405611081902));
#190535=CARTESIAN_POINT('Ctrl Pts',(4.83454132547222,4.73868542096927,28.5494356262033));
#190536=CARTESIAN_POINT('Ctrl Pts',(4.69868395107327,4.86976982288963,28.5583101442164));
#190537=CARTESIAN_POINT('Ctrl Pts',(4.56245570530148,5.00121206664459,28.5672088884055));
#190538=CARTESIAN_POINT('Ctrl Pts',(4.42082759892887,5.126820423822,28.5761076325947));
#190539=CARTESIAN_POINT('Ctrl Pts',(4.27431492765299,5.24619108489606,28.5850063767839));
#190540=CARTESIAN_POINT('Ctrl Pts',(4.12760021857274,5.36572635552953,28.5939173921488));
#190541=CARTESIAN_POINT('Ctrl Pts',(3.97598769379786,5.47900658847,28.6028284075138));
#190542=CARTESIAN_POINT('Ctrl Pts',(3.82002257712792,5.58567064104508,28.6117394228787));
#190543=CARTESIAN_POINT('Ctrl Pts',(3.66374397081258,5.69254908820232,28.6206683493708));
#190544=CARTESIAN_POINT('Ctrl Pts',(3.50309549256772,5.79278461607391,28.629597275863));
#190545=CARTESIAN_POINT('Ctrl Pts',(3.33865005573199,5.88606021081681,28.6385262023551));
#190546=CARTESIAN_POINT('Ctrl Pts',(3.25965616527438,5.93086657489275,28.6428153492892));
#190547=CARTESIAN_POINT('Ctrl Pts',(3.1797864617139,5.97406762348353,28.6471044962232));
#190548=CARTESIAN_POINT('Ctrl Pts',(3.09910619832131,6.01563211736942,28.6513936431573));
#190549=CARTESIAN_POINT('Origin',(0.,0.,4.30282021618968));
#190550=CARTESIAN_POINT('',(3.09910619832132,6.01563211736941,31.0457552630242));
#190551=CARTESIAN_POINT('',(3.09910619832131,6.01563211736941,30.6515994289918));
#190552=CARTESIAN_POINT('',(3.09910619832133,6.0156321173694,4.30282021618968));
#190553=CARTESIAN_POINT('',(-6.767,7.81740666123965E-13,29.6971797838101));
#190554=CARTESIAN_POINT('Ctrl Pts',(-6.767,7.81740771273666E-13,29.6971797838101));
#190555=CARTESIAN_POINT('Ctrl Pts',(-6.76700000000002,-0.186007249526226,
29.7059292956213));
#190556=CARTESIAN_POINT('Ctrl Pts',(-6.75932637294523,-0.37201435574941,
29.7146788074325));
#190557=CARTESIAN_POINT('Ctrl Pts',(-6.74400518264183,-0.557389537487122,
29.7234283192437));
#190558=CARTESIAN_POINT('Ctrl Pts',(-6.72868405705087,-0.742763936251697,
29.7321777940994));
#190559=CARTESIAN_POINT('Ctrl Pts',(-6.70571545645723,-0.927506130242437,
29.740927268955));
#190560=CARTESIAN_POINT('Ctrl Pts',(-6.67517739404794,-1.11098863990204,
29.7496767438107));
#190561=CARTESIAN_POINT('Ctrl Pts',(-6.64463945808665,-1.29447038982134,
29.7584261824377));
#190562=CARTESIAN_POINT('Ctrl Pts',(-6.60653217008313,-1.47669218313869,
29.7671756210647));
#190563=CARTESIAN_POINT('Ctrl Pts',(-6.56098496092631,-1.65703510599469,
29.7759250596917));
#190564=CARTESIAN_POINT('Ctrl Pts',(-6.51543793658245,-1.83737729708884,
29.7846744628169));
#190565=CARTESIAN_POINT('Ctrl Pts',(-6.46245112167363,-2.01584035511112,
29.7934238659421));
#190566=CARTESIAN_POINT('Ctrl Pts',(-6.4022044837419,-2.19181813760978,
29.8021732690673));
#190567=CARTESIAN_POINT('Ctrl Pts',(-6.34195808526437,-2.36779522067323,
29.8109226374173));
#190568=CARTESIAN_POINT('Ctrl Pts',(-6.27445201433034,-2.54128677684338,
29.8196720057674));
#190569=CARTESIAN_POINT('Ctrl Pts',(-6.1999155507183,-2.71170355384977,
29.8284213741175));
#190570=CARTESIAN_POINT('Ctrl Pts',(-6.12537937716614,-2.88211966767644,
29.8371707084193));
#190571=CARTESIAN_POINT('Ctrl Pts',(-6.04381298052436,-3.04946076371953,
29.8459200427211));
#190572=CARTESIAN_POINT('Ctrl Pts',(-5.95549339335741,-3.21315848374715,
29.8546693770229));
#190573=CARTESIAN_POINT('Ctrl Pts',(-5.86717414255318,-3.3768555803365,
29.8634186780031));
#190574=CARTESIAN_POINT('Ctrl Pts',(-5.77210188876508,-3.53690907646903,
29.8721679789833));
#190575=CARTESIAN_POINT('Ctrl Pts',(-5.67059953346907,-3.69277536969424,
29.8809172799634));
#190576=CARTESIAN_POINT('Ctrl Pts',(-5.56909755631295,-3.84864108225051,
29.8896665483487));
#190577=CARTESIAN_POINT('Ctrl Pts',(-5.46116568196763,-4.00031938297635,
29.898415816734));
#190578=CARTESIAN_POINT('Ctrl Pts',(-5.34717048533519,-4.14729511859963,
29.9071650851193));
#190579=CARTESIAN_POINT('Ctrl Pts',(-5.23317570391761,-4.29427031888008,
29.9159143216363));
#190580=CARTESIAN_POINT('Ctrl Pts',(-5.11311782003448,-4.43654276189623,
29.9246635581533));
#190581=CARTESIAN_POINT('Ctrl Pts',(-4.98740458984698,-4.57362924351912,
29.9334127946704));
#190582=CARTESIAN_POINT('Ctrl Pts',(-4.86169180711681,-4.71071523720332,
29.9421620000458));
#190583=CARTESIAN_POINT('Ctrl Pts',(-4.73032391204102,-4.84261509523306,
29.9509112054213));
#190584=CARTESIAN_POINT('Ctrl Pts',(-4.59374707013521,-4.96888084538402,
29.9596604107967));
#190585=CARTESIAN_POINT('Ctrl Pts',(-4.45717070301378,-5.09514615659522,
29.9684095857571));
#190586=CARTESIAN_POINT('Ctrl Pts',(-4.31538563570984,-5.21577720459574,
29.9771587607176));
#190587=CARTESIAN_POINT('Ctrl Pts',(-4.16887341029465,-5.33036429232921,
29.985907935678));
#190588=CARTESIAN_POINT('Ctrl Pts',(-4.02236168203633,-5.44495099123671,
29.99465708095));
#190589=CARTESIAN_POINT('Ctrl Pts',(-3.87112305348063,-5.55349359438674,
30.0034062262221));
#190590=CARTESIAN_POINT('Ctrl Pts',(-3.71567117017626,-5.65562346298982,
30.0121553714941));
#190591=CARTESIAN_POINT('Ctrl Pts',(-3.56021980145682,-5.75775299351728,
30.0209044878043));
#190592=CARTESIAN_POINT('Ctrl Pts',(-3.40055544538211,-5.85346967463953,
30.0296536041145));
#190593=CARTESIAN_POINT('Ctrl Pts',(-3.23722035986713,-5.94244842986977,
30.0384027204246));
#190594=CARTESIAN_POINT('Ctrl Pts',(-3.07388580147008,-6.03142689794618,
30.0471518084995));
#190595=CARTESIAN_POINT('Ctrl Pts',(-2.90688078896373,-6.1136673465688,
30.0559008965743));
#190596=CARTESIAN_POINT('Ctrl Pts',(-2.73677250721131,-6.18889046952459,
30.0646499846492));
#190597=CARTESIAN_POINT('Ctrl Pts',(-2.56666476031231,-6.2641133559643,
30.0733990452152));
#190598=CARTESIAN_POINT('Ctrl Pts',(-2.39345402574903,-6.33231884500655,
30.0821481057813));
#190599=CARTESIAN_POINT('Ctrl Pts',(-2.21772856065317,-6.39327529762822,
30.0908971663473));
#190600=CARTESIAN_POINT('Ctrl Pts',(-2.04200363348209,-6.45423156365208,
30.099646200131));
#190601=CARTESIAN_POINT('Ctrl Pts',(-1.86376426188944,-6.50793874375755,
30.1083952339147));
#190602=CARTESIAN_POINT('Ctrl Pts',(-1.6836157775279,-6.55421443909636,
30.1171442676984));
#190603=CARTESIAN_POINT('Ctrl Pts',(-1.50346782967444,-6.60048999661949,
30.1258932754262));
#190604=CARTESIAN_POINT('Ctrl Pts',(-1.3214110579464,-6.63933404237781,
30.1346422831541));
#190605=CARTESIAN_POINT('Ctrl Pts',(-1.13806375486686,-6.67061465607618,
30.1433912908819));
#190606=CARTESIAN_POINT('Ctrl Pts',(-0.95471698259975,-6.70189517921342,
30.1521402732803));
#190607=CARTESIAN_POINT('Ctrl Pts',(-0.770079968898975,-6.72561226592264,
30.1608892556787));
#190608=CARTESIAN_POINT('Ctrl Pts',(-0.584779765555192,-6.74168536983129,
30.1696382380771));
#190609=CARTESIAN_POINT('Ctrl Pts',(-0.391489830648283,-6.7584515101387,
30.178764457087));
#190610=CARTESIAN_POINT('Ctrl Pts',(-0.197478578235363,-6.76689983031634,
30.1878906760968));
#190611=CARTESIAN_POINT('Ctrl Pts',(-0.00346287644841733,-6.76699911397118,
30.1970168951067));
#190612=CARTESIAN_POINT('Ctrl Pts',(0.184489834657685,-6.76709529501181,
30.2058579197725));
#190613=CARTESIAN_POINT('Ctrl Pts',(0.37244640425314,-6.75935639738147,
30.2146989444383));
#190614=CARTESIAN_POINT('Ctrl Pts',(0.559755019492074,-6.74380925873156,
30.2235399691041));
#190615=CARTESIAN_POINT('Ctrl Pts',(0.745134705525503,-6.72842222659764,
30.2322899477139));
#190616=CARTESIAN_POINT('Ctrl Pts',(0.929879431232284,-6.70538706057472,
30.2410399263236));
#190617=CARTESIAN_POINT('Ctrl Pts',(1.11336163627195,-6.67478200894066,
30.2497899049333));
#190618=CARTESIAN_POINT('Ctrl Pts',(1.29684196301104,-6.64417727060938,
30.2585397939699));
#190619=CARTESIAN_POINT('Ctrl Pts',(1.47905951217911,-6.60600284890501,
30.2672896830064));
#190620=CARTESIAN_POINT('Ctrl Pts',(1.659395320675,-6.56038841607126,30.2760395720429));
#190621=CARTESIAN_POINT('Ctrl Pts',(1.83972934301221,-6.51477443503138,
30.2847893744151));
#190622=CARTESIAN_POINT('Ctrl Pts',(2.01818138406688,-6.46172066062009,
30.2935391767873));
#190623=CARTESIAN_POINT('Ctrl Pts',(2.19414528354625,-6.40140730423332,
30.3022889791594));
#190624=CARTESIAN_POINT('Ctrl Pts',(2.37010749864422,-6.34109452518484,
30.3110386977757));
#190625=CARTESIAN_POINT('Ctrl Pts',(2.54358134866877,-6.27352239616335,
30.3197884163921));
#190626=CARTESIAN_POINT('Ctrl Pts',(2.71397759435968,-6.19892043966638,
30.3285381350084));
#190627=CARTESIAN_POINT('Ctrl Pts',(2.88437226558535,-6.12431917249321,
30.3372877727771));
#190628=CARTESIAN_POINT('Ctrl Pts',(3.05168912681365,-6.04268832278592,
30.3460374105458));
#190629=CARTESIAN_POINT('Ctrl Pts',(3.21535986274262,-5.95430516123114,
30.3547870483145));
#190630=CARTESIAN_POINT('Ctrl Pts',(3.37902914073255,-5.86592278697203,
30.3635366081436));
#190631=CARTESIAN_POINT('Ctrl Pts',(3.5390521062199,-5.77078835741686,30.3722861679727));
#190632=CARTESIAN_POINT('Ctrl Pts',(3.69488522832119,-5.66922500431355,
30.3810357278017));
#190633=CARTESIAN_POINT('Ctrl Pts',(3.85071701407367,-5.56766252216798,
30.3897852125989));
#190634=CARTESIAN_POINT('Ctrl Pts',(4.00235878822836,-5.45967138329054,
30.398534697396));
#190635=CARTESIAN_POINT('Ctrl Pts',(4.14929549611761,-5.34561838199269,
30.4072841821931));
#190636=CARTESIAN_POINT('Ctrl Pts',(4.29623099276522,-5.23156632086661,
30.4160335948657));
#190637=CARTESIAN_POINT('Ctrl Pts',(4.43846127436456,-5.11145267304592,
30.4247830075383));
#190638=CARTESIAN_POINT('Ctrl Pts',(4.57550326054866,-4.98568540049496,
30.4335324202109));
#190639=CARTESIAN_POINT('Ctrl Pts',(4.71254416258193,-4.8599191228996,30.4422817636661));
#190640=CARTESIAN_POINT('Ctrl Pts',(4.84439664019163,-4.72849950385007,
30.4510311071214));
#190641=CARTESIAN_POINT('Ctrl Pts',(4.97061286795135,-4.59187289860646,
30.4597804505766));
#190642=CARTESIAN_POINT('Ctrl Pts',(5.09682813913057,-4.45524732884258,
30.4685297277214));
#190643=CARTESIAN_POINT('Ctrl Pts',(5.21740705148194,-4.31341506235357,
30.4772790048663));
#190644=CARTESIAN_POINT('Ctrl Pts',(5.33194007546035,-4.16685781275291,
30.4860282820111));
#190645=CARTESIAN_POINT('Ctrl Pts',(5.44647226944804,-4.0203016252141,30.4947774957522));
#190646=CARTESIAN_POINT('Ctrl Pts',(5.55495848628411,-3.86902074887505,
30.5035267094933));
#190647=CARTESIAN_POINT('Ctrl Pts',(5.65703027292067,-3.71352898080238,
30.5122759232344));
#190648=CARTESIAN_POINT('Ctrl Pts',(5.75910135377258,-3.55803828789165,
30.5210250764783));
#190649=CARTESIAN_POINT('Ctrl Pts',(5.85475793592996,-3.39833700106292,
30.5297742297222));
#190650=CARTESIAN_POINT('Ctrl Pts',(5.94367514427625,-3.23496750823137,
30.5385233829661));
#190651=CARTESIAN_POINT('Ctrl Pts',(6.03259176732859,-3.07159909077295,
30.547272478619));
#190652=CARTESIAN_POINT('Ctrl Pts',(6.11476896836134,-2.90456276730992,
30.5560215742719));
#190653=CARTESIAN_POINT('Ctrl Pts',(6.18992765548087,-2.73442583002596,
30.5647706699249));
#190654=CARTESIAN_POINT('Ctrl Pts',(6.26508587283246,-2.56428995615703,
30.5735197108929));
#190655=CARTESIAN_POINT('Ctrl Pts',(6.33322554827342,-2.39105376934722,
30.5822687518609));
#190656=CARTESIAN_POINT('Ctrl Pts',(6.39411526733201,-2.21530561053587,
30.591017792829));
#190657=CARTESIAN_POINT('Ctrl Pts',(6.45500462603,-2.03955849184614,30.599766782018));
#190658=CARTESIAN_POINT('Ctrl Pts',(6.50864402040876,-1.8612997016407,30.608515771207));
#190659=CARTESIAN_POINT('Ctrl Pts',(6.5548512836872,-1.68113463135594,30.617264760396));
#190660=CARTESIAN_POINT('Ctrl Pts',(6.60199809554427,-1.49730620116425,
30.6261916458675));
#190661=CARTESIAN_POINT('Ctrl Pts',(6.64140720707956,-1.31149343245275,
30.6351185313389));
#190662=CARTESIAN_POINT('Ctrl Pts',(6.67293928722951,-1.12435326697124,
30.6440454168103));
#190663=CARTESIAN_POINT('Ctrl Pts',(6.70384625876313,-0.940923067002602,
30.6527953309878));
#190664=CARTESIAN_POINT('Ctrl Pts',(6.7271855457984,-0.756217899517709,
30.6615452451652));
#190665=CARTESIAN_POINT('Ctrl Pts',(6.74287786815361,-0.570865181250576,
30.6702951593427));
#190666=CARTESIAN_POINT('Ctrl Pts',(6.75856988190868,-0.385516108070075,
30.6790449014472));
#190667=CARTESIAN_POINT('Ctrl Pts',(6.76661520773414,-0.19951979522253,
30.6877946435517));
#190668=CARTESIAN_POINT('Ctrl Pts',(6.7669865178958,-0.0135080204518887,
30.6965443856561));
#190669=CARTESIAN_POINT('Ctrl Pts',(6.76735782124893,0.172500343516661,
30.7052939673211));
#190670=CARTESIAN_POINT('Ctrl Pts',(6.76005538995164,0.358523882214559,
30.7140435489861));
#190671=CARTESIAN_POINT('Ctrl Pts',(6.74510402742332,0.543930748567948,
30.722793130651));
#190672=CARTESIAN_POINT('Ctrl Pts',(6.73015291917992,0.729334461618776,
30.7315425635077));
#190673=CARTESIAN_POINT('Ctrl Pts',(6.70755316306547,0.914121237638186,
30.7402919963644));
#190674=CARTESIAN_POINT('Ctrl Pts',(6.67738151874517,1.09766345166468,30.7490414292211));
#190675=CARTESIAN_POINT('Ctrl Pts',(6.64721034747502,1.28120278800011,30.7577907248986));
#190676=CARTESIAN_POINT('Ctrl Pts',(6.60946757205065,1.46349731860674,30.7665400205761));
#190677=CARTESIAN_POINT('Ctrl Pts',(6.56428138111437,1.64392790278506,30.7752893162537));
#190678=CARTESIAN_POINT('Ctrl Pts',(6.51909583859753,1.82435589779401,30.7840384863793));
#190679=CARTESIAN_POINT('Ctrl Pts',(6.46646716392768,2.00291972192611,30.7927876565049));
#190680=CARTESIAN_POINT('Ctrl Pts',(6.40657409872766,2.1790129227501,30.8015368266305));
#190681=CARTESIAN_POINT('Ctrl Pts',(6.34668181341948,2.35510383059322,30.8102858828296));
#190682=CARTESIAN_POINT('Ctrl Pts',(6.27952541913912,2.52872390822924,30.8190349390287));
#190683=CARTESIAN_POINT('Ctrl Pts',(6.20533299175368,2.69928350890627,30.8277839952278));
#190684=CARTESIAN_POINT('Ctrl Pts',(6.12831602991395,2.8763363796595,30.836866131386));
#190685=CARTESIAN_POINT('Ctrl Pts',(6.04371690605112,3.05009086601774,30.8459482675442));
#190686=CARTESIAN_POINT('Ctrl Pts',(5.9518452031647,3.21991112883033,30.8550304037024));
#190687=CARTESIAN_POINT('Ctrl Pts',(5.86333549509103,3.38351691183315,30.8637801840459));
#190688=CARTESIAN_POINT('Ctrl Pts',(5.76807618099186,3.54347103712301,30.8725299643895));
#190689=CARTESIAN_POINT('Ctrl Pts',(5.66639083308823,3.6992301802799,30.8812797447331));
#190690=CARTESIAN_POINT('Ctrl Pts',(5.56470914081996,3.85498372382346,30.890029210518));
#190691=CARTESIAN_POINT('Ctrl Pts',(5.4566020337185,4.00654234702293,30.8987786763029));
#190692=CARTESIAN_POINT('Ctrl Pts',(5.34243669838987,4.15339127986964,30.9075281420878));
#190693=CARTESIAN_POINT('Ctrl Pts',(5.22827486050352,4.30023571401571,30.9162773398338));
#190694=CARTESIAN_POINT('Ctrl Pts',(5.10805534166861,4.44237052028758,30.9250265375798));
#190695=CARTESIAN_POINT('Ctrl Pts',(4.9821864433969,4.57931296629005,30.9337757353259));
#190696=CARTESIAN_POINT('Ctrl Pts',(4.85632073219319,4.71625194483636,30.9425247115375));
#190697=CARTESIAN_POINT('Ctrl Pts',(4.72480612170045,4.84799861524775,30.9512736877491));
#190698=CARTESIAN_POINT('Ctrl Pts',(4.58808925235032,4.97410554898743,30.9600226639608));
#190699=CARTESIAN_POINT('Ctrl Pts',(4.45136349473761,5.10022068121457,30.9687722089625));
#190700=CARTESIAN_POINT('Ctrl Pts',(4.30943501209786,5.22069514872076,30.9775217539642));
#190701=CARTESIAN_POINT('Ctrl Pts',(4.16278587431482,5.33511975166491,30.9862712989659));
#190702=CARTESIAN_POINT('Ctrl Pts',(4.01614535740143,5.44953762808067,30.9950203296196));
#190703=CARTESIAN_POINT('Ctrl Pts',(3.86478496657614,5.55790617532999,31.0037693602733));
#190704=CARTESIAN_POINT('Ctrl Pts',(3.70921874746882,5.65985735539561,31.0125183909271));
#190705=CARTESIAN_POINT('Ctrl Pts',(3.55365041605579,5.76180991977244,31.0212675403767));
#190706=CARTESIAN_POINT('Ctrl Pts',(3.39387638174194,5.85734478553003,31.0300166898263));
#190707=CARTESIAN_POINT('Ctrl Pts',(3.23043927904203,5.94613749121414,31.0387658392759));
#190708=CARTESIAN_POINT('Ctrl Pts',(3.18691767070203,5.96978206944267,31.041095647192));
#190709=CARTESIAN_POINT('Ctrl Pts',(3.14313645919513,5.99294880633486,31.0434254551081));
#190710=CARTESIAN_POINT('Ctrl Pts',(3.09910619832133,6.01563211736941,31.0457552630242));
#190711=CARTESIAN_POINT('Ctrl Pts',(3.09910619832131,6.01563211736941,29.0458282148631));
#190712=CARTESIAN_POINT('Ctrl Pts',(2.93964010377536,6.09778514009208,29.054256760126));
#190713=CARTESIAN_POINT('Ctrl Pts',(2.77683871929303,6.17362780397065,29.0626853053889));
#190714=CARTESIAN_POINT('Ctrl Pts',(2.6112299438694,6.24289733859526,29.0711138506517));
#190715=CARTESIAN_POINT('Ctrl Pts',(2.44567997482292,6.31214227615147,29.0795394030043));
#190716=CARTESIAN_POINT('Ctrl Pts',(2.27732490764698,6.37481860978555,29.0879649553568));
#190717=CARTESIAN_POINT('Ctrl Pts',(2.10671402246393,6.43071108257507,29.0963905077094));
#190718=CARTESIAN_POINT('Ctrl Pts',(1.97260408037893,6.47464577220961,29.1030134751527));
#190719=CARTESIAN_POINT('Ctrl Pts',(1.83710078387265,6.51438972229086,29.1096364425959));
#190720=CARTESIAN_POINT('Ctrl Pts',(1.70047857745579,6.54985966319996,29.1162594100392));
#190721=CARTESIAN_POINT('Ctrl Pts',(1.52268563519071,6.59601837576647,29.1248781909764));
#190722=CARTESIAN_POINT('Ctrl Pts',(1.34307708786584,6.63491687714489,29.1334969719136));
#190723=CARTESIAN_POINT('Ctrl Pts',(1.16225888109226,6.66644157653258,29.1421157528508));
#190724=CARTESIAN_POINT('Ctrl Pts',(0.981332057920183,6.6979852126157,29.1507397110374));
#190725=CARTESIAN_POINT('Ctrl Pts',(0.799194424809612,6.72214615473156,
29.1593636692239));
#190726=CARTESIAN_POINT('Ctrl Pts',(0.61645904406323,6.73886245942093,29.1679876274105));
#190727=CARTESIAN_POINT('Ctrl Pts',(0.427122057498962,6.75618266716312,
29.1769231397816));
#190728=CARTESIAN_POINT('Ctrl Pts',(0.237143689164434,6.76551028319707,
29.1858586521527));
#190729=CARTESIAN_POINT('Ctrl Pts',(0.0472074746267504,6.76683533524641,
29.1947941645239));
#190730=CARTESIAN_POINT('Ctrl Pts',(-0.136448971720794,6.76811657774773,
29.2034342464186));
#190731=CARTESIAN_POINT('Ctrl Pts',(-0.320065704186172,6.7619160130467,
29.2120743283132));
#190732=CARTESIAN_POINT('Ctrl Pts',(-0.503028046335158,6.74827769024069,
29.2207144102079));
#190733=CARTESIAN_POINT('Ctrl Pts',(-0.695374440493255,6.73393986430729,
29.2297976378173));
#190734=CARTESIAN_POINT('Ctrl Pts',(-0.886997163713638,6.71138132769076,
29.2388808654266));
#190735=CARTESIAN_POINT('Ctrl Pts',(-1.07719139734627,6.68071460949225,
29.2479640930359));
#190736=CARTESIAN_POINT('Ctrl Pts',(-1.26738563097888,6.65004789129375,
29.2570473206453));
#190737=CARTESIAN_POINT('Ctrl Pts',(-1.4561510019505,6.6112731025047,29.2661305482546));
#190738=CARTESIAN_POINT('Ctrl Pts',(-1.6427978920141,6.56456427236371,29.2752137758639));
#190739=CARTESIAN_POINT('Ctrl Pts',(-1.8286509362264,6.51805410404351,29.2842583707237));
#190740=CARTESIAN_POINT('Ctrl Pts',(-2.01257532509177,6.46363514011707,
29.2933029655835));
#190741=CARTESIAN_POINT('Ctrl Pts',(-2.19392264690429,6.40148361080464,
29.3023475604433));
#190742=CARTESIAN_POINT('Ctrl Pts',(-2.37510355400318,6.33938911530363,
29.3113838554636));
#190743=CARTESIAN_POINT('Ctrl Pts',(-2.55371189066327,6.26957629836902,
29.320420150484));
#190744=CARTESIAN_POINT('Ctrl Pts',(-2.7291150570561,6.19227098933418,29.3294564455043));
#190745=CARTESIAN_POINT('Ctrl Pts',(-2.90420783379178,6.11510247810556,
29.338476750092));
#190746=CARTESIAN_POINT('Ctrl Pts',(-3.07610654871627,6.0304680462325,29.3474970546796));
#190747=CARTESIAN_POINT('Ctrl Pts',(-3.24419935093474,5.93864122265309,
29.3565173592673));
#190748=CARTESIAN_POINT('Ctrl Pts',(-3.4120804729224,5.84693003711977,29.3655263045337));
#190749=CARTESIAN_POINT('Ctrl Pts',(-3.57616503885175,5.74804464908513,
29.3745352498));
#190750=CARTESIAN_POINT('Ctrl Pts',(-3.73586423127392,5.64230515352441,
29.3835441950664));
#190751=CARTESIAN_POINT('Ctrl Pts',(-3.89520078063752,5.53680576997366,
29.3925326829251));
#190752=CARTESIAN_POINT('Ctrl Pts',(-4.05017163604127,5.42448347752928,
29.4015211707839));
#190753=CARTESIAN_POINT('Ctrl Pts',(-4.20021589273682,5.30570216412503,
29.4105096586427));
#190754=CARTESIAN_POINT('Ctrl Pts',(-4.33185907747665,5.20148790942121,
29.418395819658));
#190755=CARTESIAN_POINT('Ctrl Pts',(-4.45971019984325,5.09230245030685,
29.4262819806734));
#190756=CARTESIAN_POINT('Ctrl Pts',(-4.5834076189865,4.97841978927214,29.4341681416887));
#190757=CARTESIAN_POINT('Ctrl Pts',(-4.71079586789761,4.86113914695132,
29.4422896065449));
#190758=CARTESIAN_POINT('Ctrl Pts',(-4.83372071066561,4.73892811148528,
29.4504110714011));
#190759=CARTESIAN_POINT('Ctrl Pts',(-4.95178464568388,4.61217061943391,
29.4585325362572));
#190760=CARTESIAN_POINT('Ctrl Pts',(-5.06984016100606,4.48542216705718,
29.4666534219335));
#190761=CARTESIAN_POINT('Ctrl Pts',(-5.18303520948358,4.35412817187285,
29.4747743076097));
#190762=CARTESIAN_POINT('Ctrl Pts',(-5.29101018304382,4.21870836191915,
29.4828951932859));
#190763=CARTESIAN_POINT('Ctrl Pts',(-5.39899806270143,4.08327236542524,
29.4910170496402));
#190764=CARTESIAN_POINT('Ctrl Pts',(-5.5017643976717,3.94370985924083,29.4991389059945));
#190765=CARTESIAN_POINT('Ctrl Pts',(-5.59899083141245,3.80047242718051,
29.5072607623488));
#190766=CARTESIAN_POINT('Ctrl Pts',(-5.69628820035554,3.65713049086313,
29.515388544309));
#190767=CARTESIAN_POINT('Ctrl Pts',(-5.78803738953845,3.51010857691508,
29.5235163262691));
#190768=CARTESIAN_POINT('Ctrl Pts',(-5.87396389752997,3.35988647583733,
29.5316441082293));
#190769=CARTESIAN_POINT('Ctrl Pts',(-5.95992540878718,3.20960317985896,
29.5397752011457));
#190770=CARTESIAN_POINT('Ctrl Pts',(-6.040059341546,3.05611742261582,29.5479062940622));
#190771=CARTESIAN_POINT('Ctrl Pts',(-6.11413801439777,2.8999319545286,29.5560373869786));
#190772=CARTESIAN_POINT('Ctrl Pts',(-6.18829754102527,2.74357601652982,
29.5641773546432));
#190773=CARTESIAN_POINT('Ctrl Pts',(-6.25638846331034,2.58451481853252,
29.5723173223077));
#190774=CARTESIAN_POINT('Ctrl Pts',(-6.31823165142553,2.4232700631429,29.5804572899723));
#190775=CARTESIAN_POINT('Ctrl Pts',(-6.35030620270938,2.33964156122346,
29.5846790291527));
#190776=CARTESIAN_POINT('Ctrl Pts',(-6.38070099002848,2.25542595378637,
29.5889007683331));
#190777=CARTESIAN_POINT('Ctrl Pts',(-6.40939637596837,2.17069737543572,
29.5931225075134));
#190778=CARTESIAN_POINT('Ctrl Pts',(-6.47710331149741,1.9707797857622,29.6030837264741));
#190779=CARTESIAN_POINT('Ctrl Pts',(-6.53544742714254,1.7677082918809,29.6130449454347));
#190780=CARTESIAN_POINT('Ctrl Pts',(-6.58419091130636,1.56228007843368,
29.6230061643953));
#190781=CARTESIAN_POINT('Ctrl Pts',(-6.63281384523588,1.35735992097974,
29.6329427477087));
#190782=CARTESIAN_POINT('Ctrl Pts',(-6.67188356067146,1.15009468543861,
29.6428793310221));
#190783=CARTESIAN_POINT('Ctrl Pts',(-6.70121328168156,0.941291428525053,
29.6528159143355));
#190784=CARTESIAN_POINT('Ctrl Pts',(-6.73033525608324,0.733967154941493,
29.6626821154083));
#190785=CARTESIAN_POINT('Ctrl Pts',(-6.74985470567611,0.525126579051215,
29.672548316481));
#190786=CARTESIAN_POINT('Ctrl Pts',(-6.75963765824527,0.315575235454933,
29.6824145175538));
#190787=CARTESIAN_POINT('Ctrl Pts',(-6.76451788513943,0.211040526173875,
29.6873362729725));
#190788=CARTESIAN_POINT('Ctrl Pts',(-6.76697593628995,0.106329183087804,
29.6922580283913));
#190789=CARTESIAN_POINT('Ctrl Pts',(-6.76699982416302,0.00154265278611927,
29.69717978381));
#190790=CARTESIAN_POINT('',(-6.76699936525298,-0.00293098375184019,29.3028202162149));
#190791=CARTESIAN_POINT('Ctrl Pts',(3.09910619832131,6.01563211736942,28.6513936431573));
#190792=CARTESIAN_POINT('Ctrl Pts',(3.01963936879232,6.05657147987517,28.6556182811778));
#190793=CARTESIAN_POINT('Ctrl Pts',(2.93938618624693,6.09592314957077,28.6598429191983));
#190794=CARTESIAN_POINT('Ctrl Pts',(2.85840996112926,6.13365971456821,28.6640675572189));
#190795=CARTESIAN_POINT('Ctrl Pts',(2.70079997522997,6.20710916801571,28.6722902810847));
#190796=CARTESIAN_POINT('Ctrl Pts',(2.54014742829101,6.27457755010999,28.6805130049506));
#190797=CARTESIAN_POINT('Ctrl Pts',(2.37694609925172,6.33580430894548,28.6887357288165));
#190798=CARTESIAN_POINT('Ctrl Pts',(2.2139175132905,6.39696626133089,28.6969497492077));
#190799=CARTESIAN_POINT('Ctrl Pts',(2.04834585048812,6.45189962125721,28.7051637695989));
#190800=CARTESIAN_POINT('Ctrl Pts',(1.88074787242205,6.5003904836848,28.7133777899902));
#190801=CARTESIAN_POINT('Ctrl Pts',(1.71329364220257,6.54883975577143,28.7215847652621));
#190802=CARTESIAN_POINT('Ctrl Pts',(1.54381690065292,6.59085743612007,28.7297917405341));
#190803=CARTESIAN_POINT('Ctrl Pts',(1.37285278805253,6.6262783085482,28.7379987158061));
#190804=CARTESIAN_POINT('Ctrl Pts',(1.20200099546234,6.66167591017001,28.7462002992591));
#190805=CARTESIAN_POINT('Ctrl Pts',(1.02966412823749,6.69048526410618,28.754401882712));
#190806=CARTESIAN_POINT('Ctrl Pts',(0.856390921950913,6.71259142126199,
28.762603466165));
#190807=CARTESIAN_POINT('Ctrl Pts',(0.683196781399244,6.73468749122891,
28.7708013071801));
#190808=CARTESIAN_POINT('Ctrl Pts',(0.509067508093343,6.75008641281681,
28.7789991481951));
#190809=CARTESIAN_POINT('Ctrl Pts',(0.334560516946642,6.75872460309639,
28.7871969892101));
#190810=CARTESIAN_POINT('Ctrl Pts',(0.160068925497279,6.76736203108264,
28.7953941067913));
#190811=CARTESIAN_POINT('Ctrl Pts',(-0.0147999598090707,6.76923988984333,
28.8035912243725));
#190812=CARTESIAN_POINT('Ctrl Pts',(-0.189484763044477,6.76434657040678,
28.8117883419536));
#190813=CARTESIAN_POINT('Ctrl Pts',(-0.364167622716883,6.75945330541386,
28.8199853683327));
#190814=CARTESIAN_POINT('Ctrl Pts',(-0.538666045676,6.74778902125161,28.8281823947118));
#190815=CARTESIAN_POINT('Ctrl Pts',(-0.712419940840349,6.7293942392977,
28.8363794210909));
#190816=CARTESIAN_POINT('Ctrl Pts',(-0.886203496528949,6.71099631727677,
28.844577846737));
#190817=CARTESIAN_POINT('Ctrl Pts',(-1.05924191436472,6.68586564624408,
28.8527762723832));
#190818=CARTESIAN_POINT('Ctrl Pts',(-1.23098144775283,6.65409450453541,
28.8609746980293));
#190819=CARTESIAN_POINT('Ctrl Pts',(-1.40278152559977,6.62231216233875,
28.86917601392));
#190820=CARTESIAN_POINT('Ctrl Pts',(-1.57328145421884,6.58388475138881,
28.8773773298106));
#190821=CARTESIAN_POINT('Ctrl Pts',(-1.74193882837407,6.53895543020464,
28.8855786457013));
#190822=CARTESIAN_POINT('Ctrl Pts',(-1.91078827504614,6.49397494204457,
28.8937893015179));
#190823=CARTESIAN_POINT('Ctrl Pts',(-2.07779062800259,6.44247784306836,
28.9019999573344));
#190824=CARTESIAN_POINT('Ctrl Pts',(-2.24241875863819,6.38465716471195,
28.910210613151));
#190825=CARTESIAN_POINT('Ctrl Pts',(-2.40714390064255,6.32680241403065,
28.9184261073082));
#190826=CARTESIAN_POINT('Ctrl Pts',(-2.56949169834462,6.26261678781179,
28.9266416014653));
#190827=CARTESIAN_POINT('Ctrl Pts',(-2.72895621360771,6.1923409938578,28.9348570956225));
#190828=CARTESIAN_POINT('Ctrl Pts',(-2.88866814100077,6.12195616571626,
28.94308533627));
#190829=CARTESIAN_POINT('Ctrl Pts',(-3.04548752391195,6.04546244421245,
28.9513135769175));
#190830=CARTESIAN_POINT('Ctrl Pts',(-3.19893300132467,5.96314653962452,
28.959541817565));
#190831=CARTESIAN_POINT('Ctrl Pts',(-3.33839044255761,5.88833452417665,
28.9670199746661));
#190832=CARTESIAN_POINT('Ctrl Pts',(-3.47506124340677,5.80871410454857,
28.9744981317673));
#190833=CARTESIAN_POINT('Ctrl Pts',(-3.60860639176604,5.72453045317302,
28.9819762888684));
#190834=CARTESIAN_POINT('Ctrl Pts',(-3.75270835200911,5.63369204134993,
28.9900455980909));
#190835=CARTESIAN_POINT('Ctrl Pts',(-3.8936422053575,5.53724234215498,28.9981149073134));
#190836=CARTESIAN_POINT('Ctrl Pts',(-4.03092895988346,5.43543013204777,
29.006184216536));
#190837=CARTESIAN_POINT('Ctrl Pts',(-4.16804448051318,5.33374490943824,
29.0142434611367));
#190838=CARTESIAN_POINT('Ctrl Pts',(-4.30152165754444,5.22671070372065,
29.0223027057375));
#190839=CARTESIAN_POINT('Ctrl Pts',(-4.43090650081178,5.11462184145259,
29.0303619503382));
#190840=CARTESIAN_POINT('Ctrl Pts',(-4.56015835930497,5.00264818674407,
29.0384129114585));
#190841=CARTESIAN_POINT('Ctrl Pts',(-4.68532597480511,4.88563045647616,
29.0464638725788));
#190842=CARTESIAN_POINT('Ctrl Pts',(-4.80598483996478,4.7639058258984,29.054514833699));
#190843=CARTESIAN_POINT('Ctrl Pts',(-4.9265461278667,4.64227963446672,29.0625592839781));
#190844=CARTESIAN_POINT('Ctrl Pts',(-5.04260566130644,4.51595438255239,
29.0706037342572));
#190845=CARTESIAN_POINT('Ctrl Pts',(-5.15377259831527,4.38530694534085,
29.0786481845363));
#190846=CARTESIAN_POINT('Ctrl Pts',(-5.26487396762636,4.25473656567811,
29.0866878900946));
#190847=CARTESIAN_POINT('Ctrl Pts',(-5.37108824391054,4.11984935903987,
29.0947275956528));
#190848=CARTESIAN_POINT('Ctrl Pts',(-5.47206208945628,3.98105833782116,
29.102767301211));
#190849=CARTESIAN_POINT('Ctrl Pts',(-5.57521540147456,3.83927158661118,
29.1109805395155));
#190850=CARTESIAN_POINT('Ctrl Pts',(-5.67289920651918,3.69341086488444,
29.1191937778199));
#190851=CARTESIAN_POINT('Ctrl Pts',(-5.76478058652902,3.5439517193633,29.1274070161244));
#190852=CARTESIAN_POINT('Ctrl Pts',(-5.85469170614516,3.39769750431736,
29.1354441336726));
#190853=CARTESIAN_POINT('Ctrl Pts',(-5.93904653417511,3.24799796437482,
29.1434812512207));
#190854=CARTESIAN_POINT('Ctrl Pts',(-6.01757751986774,3.09532708972451,
29.1515183687689));
#190855=CARTESIAN_POINT('Ctrl Pts',(-6.09611681363938,2.94264006346631,
29.159556336593));
#190856=CARTESIAN_POINT('Ctrl Pts',(-6.16883086726497,2.786981408797,29.1675943044171));
#190857=CARTESIAN_POINT('Ctrl Pts',(-6.23549876428527,2.62884844762814,
29.1756322722413));
#190858=CARTESIAN_POINT('Ctrl Pts',(-6.30218692371324,2.4706674250284,29.183672683049));
#190859=CARTESIAN_POINT('Ctrl Pts',(-6.36282512373256,2.31001094312603,
29.1917130938567));
#190860=CARTESIAN_POINT('Ctrl Pts',(-6.41724119048436,2.14739481771537,
29.1997535046645));
#190861=CARTESIAN_POINT('Ctrl Pts',(-6.47371387764892,1.97863271993062,
29.2080977976523));
#190862=CARTESIAN_POINT('Ctrl Pts',(-6.52348477802392,1.80776038001368,
29.21644209064));
#190863=CARTESIAN_POINT('Ctrl Pts',(-6.56641898204299,1.63536869001015,
29.2247863836278));
#190864=CARTESIAN_POINT('Ctrl Pts',(-6.60786267041708,1.46896179737004,
29.2328409938434));
#190865=CARTESIAN_POINT('Ctrl Pts',(-6.64293638714389,1.30113965252255,
29.2408956040589));
#190866=CARTESIAN_POINT('Ctrl Pts',(-6.67157152402784,1.13244090343861,
29.2489502142744));
#190867=CARTESIAN_POINT('Ctrl Pts',(-6.70022833811489,0.963614447018662,
29.2570109219437));
#190868=CARTESIAN_POINT('Ctrl Pts',(-6.72243681932683,0.793910432895307,
29.2650716296129));
#190869=CARTESIAN_POINT('Ctrl Pts',(-6.73818039700338,0.623870128664149,
29.2731323372822));
#190870=CARTESIAN_POINT('Ctrl Pts',(-6.75394617218128,0.453590077790773,
29.2812044100664));
#190871=CARTESIAN_POINT('Ctrl Pts',(-6.76322883750484,0.282973160259584,
29.2892764828505));
#190872=CARTESIAN_POINT('Ctrl Pts',(-6.76606381392599,0.112558721924744,
29.2973485556347));
#190873=CARTESIAN_POINT('Ctrl Pts',(-6.76636075616661,0.0947091042783638,
29.2981940439291));
#190874=CARTESIAN_POINT('Ctrl Pts',(-6.76658700763728,0.0768617012250634,
29.2990395322235));
#190875=CARTESIAN_POINT('Ctrl Pts',(-6.76674264167672,0.0590171272931185,
29.2998850205179));
#190876=CARTESIAN_POINT('Ctrl Pts',(-6.7669227412957,0.0383673968275339,
29.3008634190753));
#190877=CARTESIAN_POINT('Ctrl Pts',(-6.76700830886146,0.0177178525793984,
29.3018418176326));
#190878=CARTESIAN_POINT('Ctrl Pts',(-6.76699936525321,-0.00293098322481845,
29.3028202161899));
#190879=CARTESIAN_POINT('Ctrl Pts',(-6.76699936525298,-0.00293098375180045,
29.3028202162149));
#190880=CARTESIAN_POINT('Ctrl Pts',(-6.76692334343068,-0.17844871664729,
29.3111367285007));
#190881=CARTESIAN_POINT('Ctrl Pts',(-6.76001423110666,-0.35419545525724,
29.3194532407865));
#190882=CARTESIAN_POINT('Ctrl Pts',(-6.74624402573338,-0.52960414014304,
29.3277697530723));
#190883=CARTESIAN_POINT('Ctrl Pts',(-6.73249024537216,-0.704803598682164,
29.3360763454759));
#190884=CARTESIAN_POINT('Ctrl Pts',(-6.71189170086085,-0.879665461091391,
29.3443829378796));
#190885=CARTESIAN_POINT('Ctrl Pts',(-6.6844723585507,-1.05362151068196,
29.3526895302832));
#190886=CARTESIAN_POINT('Ctrl Pts',(-6.65708060167097,-1.22740255051303,
29.3609877657787));
#190887=CARTESIAN_POINT('Ctrl Pts',(-6.62288177172376,-1.40027924971875,
29.3692860012741));
#190888=CARTESIAN_POINT('Ctrl Pts',(-6.58195172285144,-1.57168715654644,
29.3775842367696));
#190889=CARTESIAN_POINT('Ctrl Pts',(-6.54105521325882,-1.74295460671968,
29.385875672448));
#190890=CARTESIAN_POINT('Ctrl Pts',(-6.49343855552541,-1.91275532387974,
29.3941671081265));
#190891=CARTESIAN_POINT('Ctrl Pts',(-6.43922893693435,-2.08053351276717,
29.4024585438049));
#190892=CARTESIAN_POINT('Ctrl Pts',(-6.38505362700411,-2.2482055167169,
29.4107447319266));
#190893=CARTESIAN_POINT('Ctrl Pts',(-6.32429377847391,-2.41385721133037,
29.4190309200482));
#190894=CARTESIAN_POINT('Ctrl Pts',(-6.25712688900796,-2.57694627317947,
29.4273171081698));
#190895=CARTESIAN_POINT('Ctrl Pts',(-6.18998725095775,-2.73996916540451,
29.4355999343618));
#190896=CARTESIAN_POINT('Ctrl Pts',(-6.11644588430375,-2.90043117357467,
29.4438827605538));
#190897=CARTESIAN_POINT('Ctrl Pts',(-6.03672914460988,-3.05780807681216,
29.4521655867458));
#190898=CARTESIAN_POINT('Ctrl Pts',(-5.95702895048088,-3.21515231577145,
29.4604466938002));
#190899=CARTESIAN_POINT('Ctrl Pts',(-5.87115609458469,-3.36941241358713,
29.4687278008547));
#190900=CARTESIAN_POINT('Ctrl Pts',(-5.77938388808665,-3.52008677082319,
29.4770089079091));
#190901=CARTESIAN_POINT('Ctrl Pts',(-5.68761521411714,-3.67075532824812,
29.4852896962043));
#190902=CARTESIAN_POINT('Ctrl Pts',(-5.58994782412242,-3.81783812156665,
29.4935704844994));
#190903=CARTESIAN_POINT('Ctrl Pts',(-5.48669963192837,-3.9608605313741,
29.5018512727945));
#190904=CARTESIAN_POINT('Ctrl Pts',(-5.38343795931271,-4.10390161465509,
29.5101331422564));
#190905=CARTESIAN_POINT('Ctrl Pts',(-5.27459423789114,-4.24288097498686,
29.5184150117184));
#190906=CARTESIAN_POINT('Ctrl Pts',(-5.16052821794216,-4.37735508176144,
29.5266968811803));
#190907=CARTESIAN_POINT('Ctrl Pts',(-5.04638099100757,-4.51192492464446,
29.5349846467509));
#190908=CARTESIAN_POINT('Ctrl Pts',(-4.92700426361538,-4.64198283850877,
29.5432724123216));
#190909=CARTESIAN_POINT('Ctrl Pts',(-4.80279697001287,-4.76711970322072,
29.5515601778922));
#190910=CARTESIAN_POINT('Ctrl Pts',(-4.67854263339442,-4.89230396301996,
29.559851082421));
#190911=CARTESIAN_POINT('Ctrl Pts',(-4.54945433598132,-5.01256321634397,
29.5681419869497));
#190912=CARTESIAN_POINT('Ctrl Pts',(-4.4159661242158,-5.12752690775763,
29.5764328914784));
#190913=CARTESIAN_POINT('Ctrl Pts',(-4.28233650304424,-5.24261238481141,
29.5847325788942));
#190914=CARTESIAN_POINT('Ctrl Pts',(-4.14429792605753,-5.3523908706024,
29.5930322663099));
#190915=CARTESIAN_POINT('Ctrl Pts',(-4.00231641433118,-5.45653299445493,
29.6013319537257));
#190916=CARTESIAN_POINT('Ctrl Pts',(-3.90844657275726,-5.52538565384941,
29.6068192198729));
#190917=CARTESIAN_POINT('Ctrl Pts',(-3.81285386559171,-5.59177549299337,
29.6123064860202));
#190918=CARTESIAN_POINT('Ctrl Pts',(-3.71567934690656,-5.65561809097573,
29.6177937521674));
#190919=CARTESIAN_POINT('Ctrl Pts',(-3.56603273347159,-5.75393428240353,
29.6262440208908));
#190920=CARTESIAN_POINT('Ctrl Pts',(-3.41235457220222,-5.84639088124095,
29.6346942896141));
#190921=CARTESIAN_POINT('Ctrl Pts',(-3.25513079771634,-5.93265644460882,
29.6431445583375));
#190922=CARTESIAN_POINT('Ctrl Pts',(-3.09804577854547,-6.01884587569035,
29.651587369412));
#190923=CARTESIAN_POINT('Ctrl Pts',(-2.93742167241164,-6.09885500288081,
29.6600301804865));
#190924=CARTESIAN_POINT('Ctrl Pts',(-2.7737723342264,-6.17239629624348,
29.668472991561));
#190925=CARTESIAN_POINT('Ctrl Pts',(-2.6102451408566,-6.24588269975566,
29.6769095010787));
#190926=CARTESIAN_POINT('Ctrl Pts',(-2.44369751804175,-6.31291075726125,
29.6853460105964));
#190927=CARTESIAN_POINT('Ctrl Pts',(-2.27466715476121,-6.37323923409835,
29.6937825201141));
#190928=CARTESIAN_POINT('Ctrl Pts',(-2.10575774180036,-6.43352454266427,
29.7022129928554));
#190929=CARTESIAN_POINT('Ctrl Pts',(-1.93436944348861,-6.48711972159933,
29.7106434655966));
#190930=CARTESIAN_POINT('Ctrl Pts',(-1.76105931632406,-6.53383188369492,
29.7190739383378));
#190931=CARTESIAN_POINT('Ctrl Pts',(-1.58782369471363,-6.58052396435857,
29.7275007868416));
#190932=CARTESIAN_POINT('Ctrl Pts',(-1.41266821085646,-6.62033884089884,
29.7359276353455));
#190933=CARTESIAN_POINT('Ctrl Pts',(-1.23616508069522,-6.65313346426102,
29.7443544838493));
#190934=CARTESIAN_POINT('Ctrl Pts',(-1.05971643074671,-6.68591796509417,
29.7527787312859));
#190935=CARTESIAN_POINT('Ctrl Pts',(-0.881921289659919,-6.7116864735628,
29.7612029787226));
#190936=CARTESIAN_POINT('Ctrl Pts',(-0.703362429461534,-6.73034696674859,
29.7696272261592));
#190937=CARTESIAN_POINT('Ctrl Pts',(-0.653051374424555,-6.73560477976691,
29.7720008567702));
#190938=CARTESIAN_POINT('Ctrl Pts',(-0.602679739026944,-6.74029860317789,
29.7743744873812));
#190939=CARTESIAN_POINT('Ctrl Pts',(-0.552260663323196,-6.74442711872149,
29.7767481179922));
#190940=CARTESIAN_POINT('Ctrl Pts',(-0.36918627654349,-6.75941798162218,
29.7853668989294));
#190941=CARTESIAN_POINT('Ctrl Pts',(-0.185568004040187,-6.76694484582585,
29.7939856798667));
#190942=CARTESIAN_POINT('Ctrl Pts',(-0.00202229430074478,-6.7669996978222,
29.8026044608039));
#190943=CARTESIAN_POINT('Ctrl Pts',(0.181633670230526,-6.76705458276781,
29.8112284189904));
#190944=CARTESIAN_POINT('Ctrl Pts',(0.365216680836257,-6.75962849794704,
29.819852377177));
#190945=CARTESIAN_POINT('Ctrl Pts',(0.548112133156137,-6.74476553258058,
29.8284763353635));
#190946=CARTESIAN_POINT('Ctrl Pts',(0.73761497413429,-6.72936561898745,
29.8374118477346));
#190947=CARTESIAN_POINT('Ctrl Pts',(0.926379292811044,-6.70598150364335,
29.8463473601057));
#190948=CARTESIAN_POINT('Ctrl Pts',(1.11372996614274,-6.67472056063141,
29.8552828724768));
#190949=CARTESIAN_POINT('Ctrl Pts',(1.29488635576899,-6.64449318289294,
29.8639229543715));
#190950=CARTESIAN_POINT('Ctrl Pts',(1.47472079254162,-6.60690160412118,
29.8725630362662));
#190951=CARTESIAN_POINT('Ctrl Pts',(1.65263525530527,-6.56209461322542,
29.8812031181609));
#190952=CARTESIAN_POINT('Ctrl Pts',(1.83967486673138,-6.51498949295507,
29.8902863457703));
#190953=CARTESIAN_POINT('Ctrl Pts',(2.02459200481753,-6.45990948142009,
29.8993695733796));
#190954=CARTESIAN_POINT('Ctrl Pts',(2.20671158264246,-6.39708628916569,
29.9084528009889));
#190955=CARTESIAN_POINT('Ctrl Pts',(2.3888311604674,-6.33426309691129,29.9175360285983));
#190956=CARTESIAN_POINT('Ctrl Pts',(2.56815282951321,-6.2636968972522,29.9266192562076));
#190957=CARTESIAN_POINT('Ctrl Pts',(2.74402702294552,-6.18567738387194,
29.9357024838169));
#190958=CARTESIAN_POINT('Ctrl Pts',(2.91915318891973,-6.10798970279257,
29.9447470786767));
#190959=CARTESIAN_POINT('Ctrl Pts',(3.09102322236968,-6.02284103247761,
29.9537916735366));
#190960=CARTESIAN_POINT('Ctrl Pts',(3.25902853016055,-5.93051616974438,
29.9628362683964));
#190961=CARTESIAN_POINT('Ctrl Pts',(3.42687966663643,-5.83827602960522,
29.9718725634168));
#190962=CARTESIAN_POINT('Ctrl Pts',(3.5908729497389,-5.7388729590765,29.9809088584371));
#190963=CARTESIAN_POINT('Ctrl Pts',(3.75042386829534,-5.63263790848663,
29.9899451534575));
#190964=CARTESIAN_POINT('Ctrl Pts',(3.90969244898952,-5.52659084914966,
29.9989654580452));
#190965=CARTESIAN_POINT('Ctrl Pts',(4.06453416501961,-5.41373608306452,
30.0079857626329));
#190966=CARTESIAN_POINT('Ctrl Pts',(4.21439312543053,-5.29444799618656,
30.0170060672206));
#190967=CARTESIAN_POINT('Ctrl Pts',(4.36406336759178,-5.17531012948162,
30.0260150124869));
#190968=CARTESIAN_POINT('Ctrl Pts',(4.50876319093296,-5.04975525754166,
30.0350239577532));
#190969=CARTESIAN_POINT('Ctrl Pts',(4.64796738103697,-4.91819969346674,
30.0440329030196));
#190970=CARTESIAN_POINT('Ctrl Pts',(4.78685546789453,-4.78694286422776,
30.0530213908784));
#190971=CARTESIAN_POINT('Ctrl Pts',(4.92027265893366,-4.64971270522507,
30.0620098787372));
#190972=CARTESIAN_POINT('Ctrl Pts',(5.0477287478029,-4.50696388809631,30.070998366596));
#190973=CARTESIAN_POINT('Ctrl Pts',(5.15955392407119,-4.38172144751043,
30.0788845276112));
#190974=CARTESIAN_POINT('Ctrl Pts',(5.26679083365828,-4.25223160546079,
30.0867706886265));
#190975=CARTESIAN_POINT('Ctrl Pts',(5.36913017152967,-4.11882631354732,
30.0946568496417));
#190976=CARTESIAN_POINT('Ctrl Pts',(5.47452306603439,-3.98144053258129,
30.1027783144979));
#190977=CARTESIAN_POINT('Ctrl Pts',(5.5746732893869,-3.83996266533143,30.110899779354));
#190978=CARTESIAN_POINT('Ctrl Pts',(5.66925505609524,-3.69483911814013,
30.1190212442102));
#190979=CARTESIAN_POINT('Ctrl Pts',(5.76383007773165,-3.54972592039354,
30.1271421298864));
#190980=CARTESIAN_POINT('Ctrl Pts',(5.85283723377556,-3.40096786735389,
30.1352630155626));
#190981=CARTESIAN_POINT('Ctrl Pts',(5.93599420789973,-3.24904012960457,
30.1433839012388));
#190982=CARTESIAN_POINT('Ctrl Pts',(6.01916112166023,-3.09709423214613,
30.1515057575931));
#190983=CARTESIAN_POINT('Ctrl Pts',(6.09647628634571,-2.94197821735398,
30.1596276139474));
#190984=CARTESIAN_POINT('Ctrl Pts',(6.16770348824845,-2.78419156687322,
30.1677494703016));
#190985=CARTESIAN_POINT('Ctrl Pts',(6.23898265663644,-2.62628979720448,
30.1758772522618));
#190986=CARTESIAN_POINT('Ctrl Pts',(6.30416484013487,-2.46571383433586,
30.184005034222));
#190987=CARTESIAN_POINT('Ctrl Pts',(6.36306186700887,-2.30298342951433,
30.1921328161821));
#190988=CARTESIAN_POINT('Ctrl Pts',(6.42198288634252,-2.14018673437428,
30.2002639090986));
#190989=CARTESIAN_POINT('Ctrl Pts',(6.47461353434605,-1.97523419651346,
30.208395002015));
#190990=CARTESIAN_POINT('Ctrl Pts',(6.52081570265401,-1.80866015935027,
30.2165260949315));
#190991=CARTESIAN_POINT('Ctrl Pts',(6.56706829869779,-1.64190431358699,
30.224666062596));
#190992=CARTESIAN_POINT('Ctrl Pts',(6.60687831677082,-1.47352378957396,
30.2328060302606));
#190993=CARTESIAN_POINT('Ctrl Pts',(6.64015873062925,-1.30406327762429,
30.2409459979251));
#190994=CARTESIAN_POINT('Ctrl Pts',(6.65741939220892,-1.21617372912516,
30.2451677371056));
#190995=CARTESIAN_POINT('Ctrl Pts',(6.67292450033912,-1.12799378098362,
30.249389476286));
#190996=CARTESIAN_POINT('Ctrl Pts',(6.68666741949639,-1.0395998369784,30.2536112154665));
#190997=CARTESIAN_POINT('Ctrl Pts',(6.71414261663411,-0.862880392620828,
30.2620514249241));
#190998=CARTESIAN_POINT('Ctrl Pts',(6.73462821456756,-0.684940126377725,
30.2704916343817));
#190999=CARTESIAN_POINT('Ctrl Pts',(6.74802864739416,-0.506357950414263,
30.2789318438393));
#191000=CARTESIAN_POINT('Ctrl Pts',(6.76141892740761,-0.327911076906168,
30.2873656585879));
#191001=CARTESIAN_POINT('Ctrl Pts',(6.76773471832173,-0.148823594521152,
30.2957994733364));
#191002=CARTESIAN_POINT('Ctrl Pts',(6.76693207915634,0.0303189063932844,
30.3042332880849));
#191003=CARTESIAN_POINT('Ctrl Pts',(6.7661299247218,0.209353219343611,30.3126620094735));
#191004=CARTESIAN_POINT('Ctrl Pts',(6.75821791231362,0.3884421519357,30.321090730862));
#191005=CARTESIAN_POINT('Ctrl Pts',(6.74320414226847,0.566998144347376,
30.3295194522506));
#191006=CARTESIAN_POINT('Ctrl Pts',(6.7281971338744,0.745473721692369,30.3379443776523));
#191007=CARTESIAN_POINT('Ctrl Pts',(6.70609477293042,0.923416505664779,
30.346369303054));
#191008=CARTESIAN_POINT('Ctrl Pts',(6.67695718231888,1.10024169412013,30.3547942284558));
#191009=CARTESIAN_POINT('Ctrl Pts',(6.64782824363899,1.27701437722366,30.3632166522135));
#191010=CARTESIAN_POINT('Ctrl Pts',(6.61166829537166,1.45266979789972,30.3716390759712));
#191011=CARTESIAN_POINT('Ctrl Pts',(6.56858902929615,1.62663061701489,30.3800614997289));
#191012=CARTESIAN_POINT('Ctrl Pts',(6.52550908570783,1.80059417203284,30.3884840559471));
#191013=CARTESIAN_POINT('Ctrl Pts',(6.47550968056998,1.97286274701657,30.3969066121654));
#191014=CARTESIAN_POINT('Ctrl Pts',(6.41875327162557,2.14287084025054,30.4053291683836));
#191015=CARTESIAN_POINT('Ctrl Pts',(6.36199494543892,2.31288467639009,30.4137520091173));
#191016=CARTESIAN_POINT('Ctrl Pts',(6.29847926580235,2.48063756206188,30.4221748498511));
#191017=CARTESIAN_POINT('Ctrl Pts',(6.22841811407609,2.64558061609335,30.4305976905848));
#191018=CARTESIAN_POINT('Ctrl Pts',(6.15834481435909,2.81055226980729,30.4390219917654));
#191019=CARTESIAN_POINT('Ctrl Pts',(6.08172391024639,2.97271281353646,30.4474462929461));
#191020=CARTESIAN_POINT('Ctrl Pts',(5.99881498229965,3.13153441752397,30.4558705941267));
#191021=CARTESIAN_POINT('Ctrl Pts',(5.91588010011969,3.2904057398356,30.4642975324935));
#191022=CARTESIAN_POINT('Ctrl Pts',(5.82665342388158,3.4459357429023,30.4727244708603));
#191023=CARTESIAN_POINT('Ctrl Pts',(5.73144010436975,3.59762189925819,30.4811514092271));
#191024=CARTESIAN_POINT('Ctrl Pts',(5.63614117611542,3.74944444053551,30.4895859244708));
#191025=CARTESIAN_POINT('Ctrl Pts',(5.53484502651753,3.89741594647505,30.4980204397144));
#191026=CARTESIAN_POINT('Ctrl Pts',(5.4279003371413,4.04106259912679,30.5064549549581));
#191027=CARTESIAN_POINT('Ctrl Pts',(5.32090399256389,4.1847786343424,30.5148935441448));
#191028=CARTESIAN_POINT('Ctrl Pts',(5.20825387249812,4.324165387617,30.5233321333316));
#191029=CARTESIAN_POINT('Ctrl Pts',(5.09033877550769,4.45878236187447,30.5317707225184));
#191030=CARTESIAN_POINT('Ctrl Pts',(4.97229187611655,4.59354980745272,30.5402187441387));
#191031=CARTESIAN_POINT('Ctrl Pts',(4.84896846634489,4.72353657520099,30.548666765759));
#191032=CARTESIAN_POINT('Ctrl Pts',(4.72079484984724,4.84833837367564,30.5571147873793));
#191033=CARTESIAN_POINT('Ctrl Pts',(4.64794302320433,4.91927371306638,30.5619165072915));
#191034=CARTESIAN_POINT('Ctrl Pts',(4.57352492750606,4.98853470115086,30.5667182272037));
#191035=CARTESIAN_POINT('Ctrl Pts',(4.49762357029666,5.05605292890728,30.571519947116));
#191036=CARTESIAN_POINT('Ctrl Pts',(4.36738098180202,5.17191052456671,30.5797594365478));
#191037=CARTESIAN_POINT('Ctrl Pts',(4.23247839139077,5.28289290409624,30.5879989259797));
#191038=CARTESIAN_POINT('Ctrl Pts',(4.09331426468497,5.38860532332129,30.5962384154116));
#191039=CARTESIAN_POINT('Ctrl Pts',(3.95429111441627,5.49421065345253,30.6044695580527));
#191040=CARTESIAN_POINT('Ctrl Pts',(3.81101530141311,5.59455643582094,30.6127007006937));
#191041=CARTESIAN_POINT('Ctrl Pts',(3.66392106719515,5.68928566811015,30.6209318433347));
#191042=CARTESIAN_POINT('Ctrl Pts',(3.5169829921805,5.78391433329337,30.6291542475728));
#191043=CARTESIAN_POINT('Ctrl Pts',(3.36623487045386,5.87293813722831,30.637376651811));
#191044=CARTESIAN_POINT('Ctrl Pts',(3.21214262503794,5.95604136624439,30.6455990560492));
#191045=CARTESIAN_POINT('Ctrl Pts',(3.17465922751093,5.97625647415317,30.6475991803634));
#191046=CARTESIAN_POINT('Ctrl Pts',(3.13697809406508,5.99612144508233,30.6495993046776));
#191047=CARTESIAN_POINT('Ctrl Pts',(3.09910619832131,6.01563211736941,30.6515994289918));
#191048=CARTESIAN_POINT('Origin',(0.,0.,4.30282021618968));
#191049=CARTESIAN_POINT('',(3.09910619832137,6.01563211736938,33.0454119479742));
#191050=CARTESIAN_POINT('',(3.09910619832135,6.0156321173694,32.6513224177368));
#191051=CARTESIAN_POINT('',(3.09910619832133,6.0156321173694,4.30282021618968));
#191052=CARTESIAN_POINT('',(-6.7669999994793,-8.39470370789987E-5,31.6971797838101));
#191053=CARTESIAN_POINT('Ctrl Pts',(-6.7669999994793,-8.39470370789987E-5,
31.6971797838101));
#191054=CARTESIAN_POINT('Ctrl Pts',(-6.76699779048473,-0.178151771749838,
31.7055231531321));
#191055=CARTESIAN_POINT('Ctrl Pts',(-6.75996269808484,-0.356151551338823,
31.7138665224542));
#191056=CARTESIAN_POINT('Ctrl Pts',(-6.745936741221,-0.533503967599661,
31.7222098917762));
#191057=CARTESIAN_POINT('Ctrl Pts',(-6.73189495467664,-0.711056543615564,
31.7305626774163));
#191058=CARTESIAN_POINT('Ctrl Pts',(-6.71084656433386,-0.887959956551547,
31.7389154630564));
#191059=CARTESIAN_POINT('Ctrl Pts',(-6.68288543867111,-1.06364054717637,
31.7472682486965));
#191060=CARTESIAN_POINT('Ctrl Pts',(-6.65490792499826,-1.23942410415982,
31.7556259299026));
#191061=CARTESIAN_POINT('Ctrl Pts',(-6.62000965983928,-1.4139830754286,
31.7639836111087));
#191062=CARTESIAN_POINT('Ctrl Pts',(-6.57833536682154,-1.58675543220273,
31.7723412923148));
#191063=CARTESIAN_POINT('Ctrl Pts',(-6.53660132810523,-1.75977548136477,
31.7807109553798));
#191064=CARTESIAN_POINT('Ctrl Pts',(-6.48807193581272,-1.93100346826878,
31.7890806184449));
#191065=CARTESIAN_POINT('Ctrl Pts',(-6.43294181850615,-2.09989251146692,
31.7974502815099));
#191066=CARTESIAN_POINT('Ctrl Pts',(-6.38676031319846,-2.24136781799481,
31.80446139736));
#191067=CARTESIAN_POINT('Ctrl Pts',(-6.33594791712753,-2.38120208121305,
31.81147251321));
#191068=CARTESIAN_POINT('Ctrl Pts',(-6.28064456195365,-2.51908572430596,
31.8184836290601));
#191069=CARTESIAN_POINT('Ctrl Pts',(-6.21406858298535,-2.68507454168897,
31.8269238385177));
#191070=CARTESIAN_POINT('Ctrl Pts',(-6.1408589613978,-2.84854548522437,
31.8353640479753));
#191071=CARTESIAN_POINT('Ctrl Pts',(-6.06122901080011,-3.00895195685062,
31.8438042574329));
#191072=CARTESIAN_POINT('Ctrl Pts',(-5.98165939168721,-3.16923689681031,
31.8522380721815));
#191073=CARTESIAN_POINT('Ctrl Pts',(-5.89567928807107,-3.32646169556683,
31.86067188693));
#191074=CARTESIAN_POINT('Ctrl Pts',(-5.80354981563181,-3.48010036313322,
31.8691057016786));
#191075=CARTESIAN_POINT('Ctrl Pts',(-5.71147598213936,-3.63364624504236,
31.8775344230671));
#191076=CARTESIAN_POINT('Ctrl Pts',(-5.61326035475892,-3.78361002818852,
31.8859631444556));
#191077=CARTESIAN_POINT('Ctrl Pts',(-5.50920980585384,-3.92949059231397,
31.8943918658442));
#191078=CARTESIAN_POINT('Ctrl Pts',(-5.40520611749779,-4.07530545718649,
31.9028167912459));
#191079=CARTESIAN_POINT('Ctrl Pts',(-5.29537294054972,-4.21704049861424,
31.9112417166476));
#191080=CARTESIAN_POINT('Ctrl Pts',(-5.18006047504566,-4.35422352146393,
31.9196666420493));
#191081=CARTESIAN_POINT('Ctrl Pts',(-5.06478224969517,-4.49136581005519,
31.928089065807));
#191082=CARTESIAN_POINT('Ctrl Pts',(-4.94402819470515,-4.62395852054418,
31.9365114895647));
#191083=CARTESIAN_POINT('Ctrl Pts',(-4.81818904595063,-4.75156219758106,
31.9449339133224));
#191084=CARTESIAN_POINT('Ctrl Pts',(-4.69234791810826,-4.87916788145675,
31.9533564695406));
#191085=CARTESIAN_POINT('Ctrl Pts',(-4.56142176607839,-5.00178413305368,
31.9617790257588));
#191086=CARTESIAN_POINT('Ctrl Pts',(-4.42583893829837,-5.11900758860953,
31.970201581977));
#191087=CARTESIAN_POINT('Ctrl Pts',(-4.29025153050468,-5.23623500399597,
31.9786244227108));
#191088=CARTESIAN_POINT('Ctrl Pts',(-4.15000738554183,-5.34806904181338,
31.9870472634445));
#191089=CARTESIAN_POINT('Ctrl Pts',(-4.00556886865909,-5.45414585782496,
31.9954701041783));
#191090=CARTESIAN_POINT('Ctrl Pts',(-3.86110530740117,-5.56024106662839,
32.0038944053589));
#191091=CARTESIAN_POINT('Ctrl Pts',(-3.71244619311137,-5.66057686596334,
32.0123187065395));
#191092=CARTESIAN_POINT('Ctrl Pts',(-3.56008416335048,-5.75483186112862,
32.0207430077202));
#191093=CARTESIAN_POINT('Ctrl Pts',(-3.40767443740344,-5.84911636235786,
32.029169946087));
#191094=CARTESIAN_POINT('Ctrl Pts',(-3.25155976845531,-5.93731608880691,
32.0375968844538));
#191095=CARTESIAN_POINT('Ctrl Pts',(-3.09225906586156,-6.01915466403689,
32.0460238228206));
#191096=CARTESIAN_POINT('Ctrl Pts',(-2.93281513191226,-6.10106682243301,
32.0544583380643));
#191097=CARTESIAN_POINT('Ctrl Pts',(-2.77017973728863,-6.17660624862224,
32.0628928533079));
#191098=CARTESIAN_POINT('Ctrl Pts',(-2.60489457024093,-6.24554347338399,
32.0713273685516));
#191099=CARTESIAN_POINT('Ctrl Pts',(-2.43952956904178,-6.31451399541578,
32.0797659577384));
#191100=CARTESIAN_POINT('Ctrl Pts',(-2.27151255362936,-6.37687583527864,
32.0882045469251));
#191101=CARTESIAN_POINT('Ctrl Pts',(-2.1014027018023,-6.43244865388431,
32.0966431361119));
#191102=CARTESIAN_POINT('Ctrl Pts',(-1.93110270564717,-6.48808359032818,
32.1050911577322));
#191103=CARTESIAN_POINT('Ctrl Pts',(-1.75870551827341,-6.53691424640581,
32.1135391793525));
#191104=CARTESIAN_POINT('Ctrl Pts',(-1.58478408853412,-6.57881056063549,
32.1219872009728));
#191105=CARTESIAN_POINT('Ctrl Pts',(-1.48592993902001,-6.60262375327748,
32.1267889208851));
#191106=CARTESIAN_POINT('Ctrl Pts',(-1.38658355724041,-6.62419766959716,
32.1315906407974));
#191107=CARTESIAN_POINT('Ctrl Pts',(-1.28685124095519,-6.64351585259282,
32.1363923607096));
#191108=CARTESIAN_POINT('Ctrl Pts',(-1.1157151456392,-6.67666497145037,
32.1446318925605));
#191109=CARTESIAN_POINT('Ctrl Pts',(-0.943060246836166,-6.70324312969394,
32.1528714244113));
#191110=CARTESIAN_POINT('Ctrl Pts',(-0.769430690151189,-6.72311426446505,
32.1611109562621));
#191111=CARTESIAN_POINT('Ctrl Pts',(-0.595993850139201,-6.74296334366536,
32.1693413428085));
#191112=CARTESIAN_POINT('Ctrl Pts',(-0.42158485677799,-6.75612018218729,
32.1775717293548));
#191113=CARTESIAN_POINT('Ctrl Pts',(-0.246759193670351,-6.76249945658698,
32.1858021159011));
#191114=CARTESIAN_POINT('Ctrl Pts',(-0.0720963875388228,-6.76887278844185,
32.1940248355189));
#191115=CARTESIAN_POINT('Ctrl Pts',(0.102981961764185,-6.76848111684952,
32.2022475551367));
#191116=CARTESIAN_POINT('Ctrl Pts',(0.277913984123325,-6.7612907656326,
32.2104702747545));
#191117=CARTESIAN_POINT('Ctrl Pts',(0.45269100410728,-6.75410678558491,
32.2186857084503));
#191118=CARTESIAN_POINT('Ctrl Pts',(0.627321601313725,-6.74013614711203,
32.2269011421461));
#191119=CARTESIAN_POINT('Ctrl Pts',(0.801242761887947,-6.71939722270697,
32.2351165758419));
#191120=CARTESIAN_POINT('Ctrl Pts',(0.975074540490718,-6.69866895649867,
32.2433277874427));
#191121=CARTESIAN_POINT('Ctrl Pts',(1.1481972560462,-6.67117937388351,32.2515389990435));
#191122=CARTESIAN_POINT('Ctrl Pts',(1.32005145620136,-6.63699880616086,
32.2597502106443));
#191123=CARTESIAN_POINT('Ctrl Pts',(1.49184802594091,-6.6028297007145,32.2679586686578));
#191124=CARTESIAN_POINT('Ctrl Pts',(1.66237657899897,-6.56197414933219,
32.2761671266713));
#191125=CARTESIAN_POINT('Ctrl Pts',(1.83108622547783,-6.51455387842217,
32.2843755846849));
#191126=CARTESIAN_POINT('Ctrl Pts',(1.90625005689209,-6.49342711227282,
32.2880326319681));
#191127=CARTESIAN_POINT('Ctrl Pts',(1.98105299213458,-6.4709979944983,32.2916896792512));
#191128=CARTESIAN_POINT('Ctrl Pts',(2.05544710603844,-6.4472805270345,32.2953467265344));
#191129=CARTESIAN_POINT('Ctrl Pts',(2.23566434751522,-6.38982575895074,
32.3042058007103));
#191130=CARTESIAN_POINT('Ctrl Pts',(2.41329414565916,-6.32486711023106,
32.3130648748862));
#191131=CARTESIAN_POINT('Ctrl Pts',(2.58773979349527,-6.25267077025179,
32.3219239490621));
#191132=CARTESIAN_POINT('Ctrl Pts',(2.76251318960721,-6.18033878787476,
32.330799667656));
#191133=CARTESIAN_POINT('Ctrl Pts',(2.93409024044558,-6.10074203822208,
32.3396753862499));
#191134=CARTESIAN_POINT('Ctrl Pts',(3.10189748446334,-6.01419329552019,
32.3485511048438));
#191135=CARTESIAN_POINT('Ctrl Pts',(3.27018360294229,-5.92739756716062,
32.3574521522308));
#191136=CARTESIAN_POINT('Ctrl Pts',(3.4346781545769,-5.83361026468774,32.3663531996178));
#191137=CARTESIAN_POINT('Ctrl Pts',(3.59483275660182,-5.73318990197103,
32.3752542470048));
#191138=CARTESIAN_POINT('Ctrl Pts',(3.75520509100505,-5.63263301639373,
32.3841673954878));
#191139=CARTESIAN_POINT('Ctrl Pts',(3.91122547361042,-5.52542520029555,
32.3930805439708));
#191140=CARTESIAN_POINT('Ctrl Pts',(4.06237637333955,-5.41196703623855,
32.4019936924538));
#191141=CARTESIAN_POINT('Ctrl Pts',(4.21386286939723,-5.298256964033,32.4109266305637));
#191142=CARTESIAN_POINT('Ctrl Pts',(4.36045804925197,-5.17826894262874,
32.4198595686736));
#191143=CARTESIAN_POINT('Ctrl Pts',(4.50167700658102,-5.05244427266841,
32.4287925067834));
#191144=CARTESIAN_POINT('Ctrl Pts',(4.63609697806302,-4.93267743068279,
32.437295368642));
#191145=CARTESIAN_POINT('Ctrl Pts',(4.7656460821748,-4.80762284615651,32.4457982305006));
#191146=CARTESIAN_POINT('Ctrl Pts',(4.8899385936831,-4.67769062145077,32.4543010923592));
#191147=CARTESIAN_POINT('Ctrl Pts',(5.01013612455314,-4.55203918516906,
32.462523816225));
#191148=CARTESIAN_POINT('Ctrl Pts',(5.12564738476965,-4.42158470198206,
32.4707465400909));
#191149=CARTESIAN_POINT('Ctrl Pts',(5.23606697884529,-4.28671104613385,
32.4789692639568));
#191150=CARTESIAN_POINT('Ctrl Pts',(5.34636969752114,-4.15198014948142,
32.487183284348));
#191151=CARTESIAN_POINT('Ctrl Pts',(5.4515912566418,-4.01283966992172,32.4953973047392));
#191152=CARTESIAN_POINT('Ctrl Pts',(5.55136304920776,-3.86971023409902,
32.5036113251304));
#191153=CARTESIAN_POINT('Ctrl Pts',(5.65104926806641,-3.72670355959127,
32.5118183004024));
#191154=CARTESIAN_POINT('Ctrl Pts',(5.74529482553669,-3.5797150352594,32.5200252756744));
#191155=CARTESIAN_POINT('Ctrl Pts',(5.83377131614394,-3.42919833648277,
32.5282322509463));
#191156=CARTESIAN_POINT('Ctrl Pts',(5.92218967946257,-3.27878052417342,
32.5364338343993));
#191157=CARTESIAN_POINT('Ctrl Pts',(6.00484634433252,-3.12483946262162,
32.5446354178523));
#191158=CARTESIAN_POINT('Ctrl Pts',(6.08145613834093,-2.9678578533069,32.5528370013053));
#191159=CARTESIAN_POINT('Ctrl Pts',(6.15803097478276,-2.81094787576107,
32.5610348423204));
#191160=CARTESIAN_POINT('Ctrl Pts',(6.22856428041561,-2.65100043625445,
32.5692326833354));
#191161=CARTESIAN_POINT('Ctrl Pts',(6.29281673627029,-2.48852296025505,
32.5774305243505));
#191162=CARTESIAN_POINT('Ctrl Pts',(6.35706352204614,-2.32605982238614,
32.5856276419316));
#191163=CARTESIAN_POINT('Ctrl Pts',(6.41503042226882,-2.1610674229237,32.5938247595128));
#191164=CARTESIAN_POINT('Ctrl Pts',(6.46652606306023,-1.99407363850053,
32.6020218770939));
#191165=CARTESIAN_POINT('Ctrl Pts',(6.5180211309053,-1.82708171206919,32.610218903473));
#191166=CARTESIAN_POINT('Ctrl Pts',(6.56304497596077,-1.65808878761181,
32.6184159298521));
#191167=CARTESIAN_POINT('Ctrl Pts',(6.60145600313079,-1.48763827549859,
32.6266129562312));
#191168=CARTESIAN_POINT('Ctrl Pts',(6.63987358722549,-1.31715866676256,
32.6348113818773));
#191169=CARTESIAN_POINT('Ctrl Pts',(6.67167602557125,-1.14522132471924,
32.6430098075235));
#191170=CARTESIAN_POINT('Ctrl Pts',(6.69677277402005,-0.972380282165284,
32.6512082331696));
#191171=CARTESIAN_POINT('Ctrl Pts',(6.72187836998941,-0.799478306830294,
32.6594095490603));
#191172=CARTESIAN_POINT('Ctrl Pts',(6.74027351541787,-0.625672351247381,
32.6676108649509));
#191173=CARTESIAN_POINT('Ctrl Pts',(6.75191949241272,-0.451522057021841,
32.6758121808416));
#191174=CARTESIAN_POINT('Ctrl Pts',(6.76357873222588,-0.277173434762984,
32.6840228366582));
#191175=CARTESIAN_POINT('Ctrl Pts',(6.76847342403245,-0.102480048831869,
32.6922334924748));
#191176=CARTESIAN_POINT('Ctrl Pts',(6.76661698681875,0.0719969005999661,
32.7004441482914));
#191177=CARTESIAN_POINT('Ctrl Pts',(6.76475945565157,0.246576665070998,
32.7086596424485));
#191178=CARTESIAN_POINT('Ctrl Pts',(6.75614288306288,0.420939381007314,
32.7168751366057));
#191179=CARTESIAN_POINT('Ctrl Pts',(6.7408326450742,0.594528595697426,32.7250906307628));
#191180=CARTESIAN_POINT('Ctrl Pts',(6.72549865296955,0.768387137248436,
32.7333188714103));
#191181=CARTESIAN_POINT('Ctrl Pts',(6.70345028676967,0.941469423557725,
32.7415471120578));
#191182=CARTESIAN_POINT('Ctrl Pts',(6.67480438259898,1.1132274942874,32.7497753527053));
#191183=CARTESIAN_POINT('Ctrl Pts',(6.64876982905722,1.26932815922007,32.7572535098064));
#191184=CARTESIAN_POINT('Ctrl Pts',(6.6172864561182,1.42433498569818,32.7647316669076));
#191185=CARTESIAN_POINT('Ctrl Pts',(6.58047750411487,1.57784816057762,32.7722098240087));
#191186=CARTESIAN_POINT('Ctrl Pts',(6.54075442868357,1.74351480126009,32.7802800184165));
#191187=CARTESIAN_POINT('Ctrl Pts',(6.49469826418184,1.9079840842533,32.7883502128243));
#191188=CARTESIAN_POINT('Ctrl Pts',(6.4423907154619,2.07072230618457,32.7964204072321));
#191189=CARTESIAN_POINT('Ctrl Pts',(6.39014957552271,2.23325391841677,32.8044803558574));
#191190=CARTESIAN_POINT('Ctrl Pts',(6.33167295723089,2.39405849188848,32.8125403044826));
#191191=CARTESIAN_POINT('Ctrl Pts',(6.26709374653857,2.55261140248516,32.8206002531079));
#191192=CARTESIAN_POINT('Ctrl Pts',(6.20258234835552,2.71099782187504,32.8286517382456));
#191193=CARTESIAN_POINT('Ctrl Pts',(6.13198125093969,2.86713694125061,32.8367032233834));
#191194=CARTESIAN_POINT('Ctrl Pts',(6.05547339459548,3.02051832759649,32.8447547085212));
#191195=CARTESIAN_POINT('Ctrl Pts',(5.97602710307384,3.17979062871556,32.8531154268317));
#191196=CARTESIAN_POINT('Ctrl Pts',(5.89021140791942,3.33608876421771,32.8614761451422));
#191197=CARTESIAN_POINT('Ctrl Pts',(5.79828704848706,3.48886174895871,32.8698368634528));
#191198=CARTESIAN_POINT('Ctrl Pts',(5.70989303947358,3.63576749487417,32.8778764887955));
#191199=CARTESIAN_POINT('Ctrl Pts',(5.61585104634007,3.77941345614814,32.8859161141381));
#191200=CARTESIAN_POINT('Ctrl Pts',(5.51644043469078,3.91933335281763,32.8939557394808));
#191201=CARTESIAN_POINT('Ctrl Pts',(5.4170614940298,4.05920867274284,32.9019928034985));
#191202=CARTESIAN_POINT('Ctrl Pts',(5.31231755445393,4.19535998632222,32.9100298675162));
#191203=CARTESIAN_POINT('Ctrl Pts',(5.20253156485098,4.32734957181983,32.918066931534));
#191204=CARTESIAN_POINT('Ctrl Pts',(5.09275880476625,4.45932325220392,32.926103027063));
#191205=CARTESIAN_POINT('Ctrl Pts',(4.97794544321802,4.58713591610239,32.9341391225921));
#191206=CARTESIAN_POINT('Ctrl Pts',(4.85845491233771,4.71038266649129,32.9421752181211));
#191207=CARTESIAN_POINT('Ctrl Pts',(4.73895511116022,4.83363897859186,32.9502119371054));
#191208=CARTESIAN_POINT('Ctrl Pts',(4.61477767949704,4.95232840523451,32.9582486560897));
#191209=CARTESIAN_POINT('Ctrl Pts',(4.48632300569103,5.06608279527757,32.966285375074));
#191210=CARTESIAN_POINT('Ctrl Pts',(4.35778545910317,5.17991057418591,32.9743272789631));
#191211=CARTESIAN_POINT('Ctrl Pts',(4.22496544038581,5.28879671172445,32.9823691828522));
#191212=CARTESIAN_POINT('Ctrl Pts',(4.08829686519804,5.39241297954931,32.9904110867413));
#191213=CARTESIAN_POINT('Ctrl Pts',(3.9515756999819,5.49606911888419,32.9984560851527));
#191214=CARTESIAN_POINT('Ctrl Pts',(3.81100333320647,5.59445113434709,33.0065010835641));
#191215=CARTESIAN_POINT('Ctrl Pts',(3.66704237855232,5.6872743202611,33.0145460819755));
#191216=CARTESIAN_POINT('Ctrl Pts',(3.52294177556791,5.78018754866583,33.0225988843821));
#191217=CARTESIAN_POINT('Ctrl Pts',(3.37544634346979,5.86753099361946,33.0306516867887));
#191218=CARTESIAN_POINT('Ctrl Pts',(3.22504338389341,5.94906582347223,33.0387044891953));
#191219=CARTESIAN_POINT('Ctrl Pts',(3.18328476783862,5.97170355390324,33.0409403087882));
#191220=CARTESIAN_POINT('Ctrl Pts',(3.14130214153681,5.99389380182556,33.0431761283812));
#191221=CARTESIAN_POINT('Ctrl Pts',(3.09910619832137,6.01563211736938,33.0454119479742));
#191222=CARTESIAN_POINT('Ctrl Pts',(3.09910619832133,6.01563211736941,31.0457552630242));
#191223=CARTESIAN_POINT('Ctrl Pts',(2.93375330764826,6.10081787314653,31.0545047109265));
#191224=CARTESIAN_POINT('Ctrl Pts',(2.76488627843072,6.17918207037038,31.0632541588288));
#191225=CARTESIAN_POINT('Ctrl Pts',(2.59307866646706,6.25045854553996,31.0720036067311));
#191226=CARTESIAN_POINT('Ctrl Pts',(2.42127244185383,6.32173444515035,31.0807529839814));
#191227=CARTESIAN_POINT('Ctrl Pts',(2.24652594672473,6.38592262741835,31.0895023612317));
#191228=CARTESIAN_POINT('Ctrl Pts',(2.06943269687132,6.44280508110558,31.098251738482));
#191229=CARTESIAN_POINT('Ctrl Pts',(1.89234081822088,6.49968709436163,31.1070010479874));
#191230=CARTESIAN_POINT('Ctrl Pts',(1.71290249405599,6.54926340459542,31.1157503574927));
#191231=CARTESIAN_POINT('Ctrl Pts',(1.53172716625068,6.59136563150381,31.1244996669981));
#191232=CARTESIAN_POINT('Ctrl Pts',(1.35055318107347,6.63346754640707,31.1332489116653));
#191233=CARTESIAN_POINT('Ctrl Pts',(1.16764249714436,6.66809542395773,31.1419981563326));
#191234=CARTESIAN_POINT('Ctrl Pts',(0.983616340614552,6.69513165624665,
31.1507474009998));
#191235=CARTESIAN_POINT('Ctrl Pts',(0.799591486713964,6.7221676971596,31.1594965837355));
#191236=CARTESIAN_POINT('Ctrl Pts',(0.61445145952676,6.74161215869371,31.1682457664712));
#191237=CARTESIAN_POINT('Ctrl Pts',(0.428825047910254,6.75339900185712,
31.1769949492069));
#191238=CARTESIAN_POINT('Ctrl Pts',(0.243199888597137,6.7651857655022,31.1857440729174));
#191239=CARTESIAN_POINT('Ctrl Pts',(0.0570886373921277,6.76931499599834,
31.194493196628));
#191240=CARTESIAN_POINT('Ctrl Pts',(-0.128876626810819,6.76577266947847,
31.2032423203385));
#191241=CARTESIAN_POINT('Ctrl Pts',(-0.314840698187879,6.76223036567994,
31.21199138793));
#191242=CARTESIAN_POINT('Ctrl Pts',(-0.500658497951023,6.75101660879225,
31.2207404555216));
#191243=CARTESIAN_POINT('Ctrl Pts',(-0.685698951926038,6.7321694829622,
31.2294895231131));
#191244=CARTESIAN_POINT('Ctrl Pts',(-0.870738280459658,6.71332247176296,
31.2382385374916));
#191245=CARTESIAN_POINT('Ctrl Pts',(-1.0549999876123,6.6868422135619,31.2469875518702));
#191246=CARTESIAN_POINT('Ctrl Pts',(-1.23785829161397,6.65281863948526,
31.2557365662487));
#191247=CARTESIAN_POINT('Ctrl Pts',(-1.43007412917382,6.61705395368866,
31.2649332999479));
#191248=CARTESIAN_POINT('Ctrl Pts',(-1.62073882535771,6.57295372727795,
31.2741300336471));
#191249=CARTESIAN_POINT('Ctrl Pts',(-1.80913696091494,6.52068343478285,
31.2833267673463));
#191250=CARTESIAN_POINT('Ctrl Pts',(-1.9883835618609,6.47095219815205,31.2920767650599));
#191251=CARTESIAN_POINT('Ctrl Pts',(-2.16557827572509,6.41382586850899,
31.3008267627736));
#191252=CARTESIAN_POINT('Ctrl Pts',(-2.34011918621675,6.34949849943287,
31.3095767604873));
#191253=CARTESIAN_POINT('Ctrl Pts',(-2.51465655691071,6.28517243495561,
31.3183265807456));
#191254=CARTESIAN_POINT('Ctrl Pts',(-2.68653996295299,6.21364572242387,
31.3270764010039));
#191255=CARTESIAN_POINT('Ctrl Pts',(-2.85518555379957,6.13516132252236,
31.3358262212622));
#191256=CARTESIAN_POINT('Ctrl Pts',(-3.02382794858655,6.05667841000524,
31.3445758756997));
#191257=CARTESIAN_POINT('Ctrl Pts',(-3.18923239109244,5.971238194921,31.3533255301372));
#191258=CARTESIAN_POINT('Ctrl Pts',(-3.35083705967659,5.87913088810735,
31.3620751845747));
#191259=CARTESIAN_POINT('Ctrl Pts',(-3.51243888042352,5.78702520443132,
31.3708246848236));
#191260=CARTESIAN_POINT('Ctrl Pts',(-3.67024081223635,5.68825280605819,
31.3795741850726));
#191261=CARTESIAN_POINT('Ctrl Pts',(-3.82370687544338,5.58314917682548,
31.3883236853215));
#191262=CARTESIAN_POINT('Ctrl Pts',(-3.97717043817748,5.4780472600807,31.397073043012));
#191263=CARTESIAN_POINT('Ctrl Pts',(-4.1262980372239,5.3666144808429,31.4058224007024));
#191264=CARTESIAN_POINT('Ctrl Pts',(-4.27058317206834,5.24922931204636,
31.4145717583929));
#191265=CARTESIAN_POINT('Ctrl Pts',(-4.41486614774763,5.13184589986852,
31.423320985153));
#191266=CARTESIAN_POINT('Ctrl Pts',(-4.55430658194344,5.00851045723098,
31.4320702119131));
#191267=CARTESIAN_POINT('Ctrl Pts',(-4.68843089001777,4.87964187103185,
31.4408194386731));
#191268=CARTESIAN_POINT('Ctrl Pts',(-4.82255336917799,4.75077504208,31.4495685461291));
#191269=CARTESIAN_POINT('Ctrl Pts',(-4.95135966065125,4.61637541908105,
31.458317653585));
#191270=CARTESIAN_POINT('Ctrl Pts',(-5.07441230869261,4.47689945401826,
31.467066761041));
#191271=CARTESIAN_POINT('Ctrl Pts',(-5.19746344226432,4.33742520555498,
31.4758157608173));
#191272=CARTESIAN_POINT('Ctrl Pts',(-5.3147608845478,4.19287495491321,31.4845647605937));
#191273=CARTESIAN_POINT('Ctrl Pts',(-5.42590627628864,4.04373961586692,
31.4933137603701));
#191274=CARTESIAN_POINT('Ctrl Pts',(-5.53706380672678,3.89458798906719,
31.5020637156647));
#191275=CARTESIAN_POINT('Ctrl Pts',(-5.64206777071874,3.74085050155268,
31.5108136709595));
#191276=CARTESIAN_POINT('Ctrl Pts',(-5.74056148164018,3.58304938223145,
31.5195636262542));
#191277=CARTESIAN_POINT('Ctrl Pts',(-5.83905138951893,3.42525435593267,
31.5283132436953));
#191278=CARTESIAN_POINT('Ctrl Pts',(-5.9310313955766,3.26339625497169,31.5370628611364));
#191279=CARTESIAN_POINT('Ctrl Pts',(-6.01618907820853,3.09802485064992,
31.5458124785775));
#191280=CARTESIAN_POINT('Ctrl Pts',(-6.10134392544993,2.9326589524962,31.5545618046934));
#191281=CARTESIAN_POINT('Ctrl Pts',(-6.17967677261844,2.76378023986007,
31.5633111308092));
#191282=CARTESIAN_POINT('Ctrl Pts',(-6.25092157009239,2.5919622922708,31.5720604569251));
#191283=CARTESIAN_POINT('Ctrl Pts',(-6.32216437407773,2.4201491522904,31.5808095382276));
#191284=CARTESIAN_POINT('Ctrl Pts',(-6.38631941548945,2.24539720662784,
31.58955861953));
#191285=CARTESIAN_POINT('Ctrl Pts',(-6.44316881037564,2.06829994947604,
31.5983077008325));
#191286=CARTESIAN_POINT('Ctrl Pts',(-6.50002334524598,1.89118668024359,
31.6070575731748));
#191287=CARTESIAN_POINT('Ctrl Pts',(-6.54957082411122,1.71172794807603,
31.6158074455172));
#191288=CARTESIAN_POINT('Ctrl Pts',(-6.59164294296109,1.53053334250232,
31.6245573178595));
#191289=CARTESIAN_POINT('Ctrl Pts',(-6.63371214082158,1.34935131693482,
31.6333065827144));
#191290=CARTESIAN_POINT('Ctrl Pts',(-6.66830695239712,1.16643393829637,
31.6420558475694));
#191291=CARTESIAN_POINT('Ctrl Pts',(-6.69530988154008,0.982402458339632,
31.6508051124243));
#191292=CARTESIAN_POINT('Ctrl Pts',(-6.72231419690499,0.798361530945697,
31.6595548264313));
#191293=CARTESIAN_POINT('Ctrl Pts',(-6.7417258082929,0.613206671361114,
31.6683045404383));
#191294=CARTESIAN_POINT('Ctrl Pts',(-6.75347878028188,0.427566795112034,
31.6770542544453));
#191295=CARTESIAN_POINT('Ctrl Pts',(-6.7624899236822,0.285234494204129,
31.6837627642336));
#191296=CARTESIAN_POINT('Ctrl Pts',(-6.76699999999999,0.142617266091207,
31.6904712740219));
#191297=CARTESIAN_POINT('Ctrl Pts',(-6.767,7.38320933005802E-13,31.6971797838101));
#191298=CARTESIAN_POINT('',(-6.76699549529041,0.00780811880521902,31.3028202161435));
#191299=CARTESIAN_POINT('Ctrl Pts',(3.09910619832131,6.01563211736941,30.6515994289918));
#191300=CARTESIAN_POINT('Ctrl Pts',(2.94357060213463,6.0957602436905,30.6598137135304));
#191301=CARTESIAN_POINT('Ctrl Pts',(2.78481548965909,6.1699090339229,30.6680279980691));
#191302=CARTESIAN_POINT('Ctrl Pts',(2.62334051058967,6.23781801317569,30.6762422826077));
#191303=CARTESIAN_POINT('Ctrl Pts',(2.46194222829986,6.30569473727635,30.6844526655563));
#191304=CARTESIAN_POINT('Ctrl Pts',(2.2978269799286,6.36733741584077,30.6926630485049));
#191305=CARTESIAN_POINT('Ctrl Pts',(2.13151676911067,6.42253262062561,30.7008734314535));
#191306=CARTESIAN_POINT('Ctrl Pts',(1.96525728650907,6.47771098967754,30.7090813100575));
#191307=CARTESIAN_POINT('Ctrl Pts',(1.79680451303939,6.52644569168536,30.7172891886614));
#191308=CARTESIAN_POINT('Ctrl Pts',(1.62669815475407,6.56857230403379,30.7254970672654));
#191309=CARTESIAN_POINT('Ctrl Pts',(1.59231407181106,6.57708747623368,30.7271561491572));
#191310=CARTESIAN_POINT('Ctrl Pts',(1.55786247707645,6.58533281996979,30.7288152310489));
#191311=CARTESIAN_POINT('Ctrl Pts',(1.52334789899919,6.59330722616615,30.7304743129407));
#191312=CARTESIAN_POINT('Ctrl Pts',(1.33904885453736,6.63588852149155,30.7393333871166));
#191313=CARTESIAN_POINT('Ctrl Pts',(1.15314461898355,6.670696371689,30.7481924612925));
#191314=CARTESIAN_POINT('Ctrl Pts',(0.966284183446046,6.69765510285667,
30.7570515354684));
#191315=CARTESIAN_POINT('Ctrl Pts',(0.779072674744174,6.72466448405645,
30.7659272540623));
#191316=CARTESIAN_POINT('Ctrl Pts',(0.590901632418583,6.74379523835157,
30.7748029726563));
#191317=CARTESIAN_POINT('Ctrl Pts',(0.402423836541893,6.75502361622688,
30.7836786912502));
#191318=CARTESIAN_POINT('Ctrl Pts',(0.213408178289638,6.76628403672011,
30.7925797386372));
#191319=CARTESIAN_POINT('Ctrl Pts',(0.0240842751173204,6.76959693729915,
30.8014807860242));
#191320=CARTESIAN_POINT('Ctrl Pts',(-0.164893311894069,6.76499070181864,
30.8103818334112));
#191321=CARTESIAN_POINT('Ctrl Pts',(-0.35412781652711,6.76037820409781,
30.8192949818942));
#191322=CARTESIAN_POINT('Ctrl Pts',(-0.543014805549959,6.74782507704769,
30.8282081303772));
#191323=CARTESIAN_POINT('Ctrl Pts',(-0.730904774868618,6.72741162781603,
30.8371212788602));
#191324=CARTESIAN_POINT('Ctrl Pts',(-0.919211911296424,6.70695285514515,
30.8460542169701));
#191325=CARTESIAN_POINT('Ctrl Pts',(-1.10651734152201,6.67859888108208,
30.85498715508));
#191326=CARTESIAN_POINT('Ctrl Pts',(-1.29217883252649,6.64248167967142,
30.8639200931899));
#191327=CARTESIAN_POINT('Ctrl Pts',(-1.46890165216808,6.60810334070451,
30.8724229550484));
#191328=CARTESIAN_POINT('Ctrl Pts',(-1.64413492123316,6.56669173726127,
30.880925816907));
#191329=CARTESIAN_POINT('Ctrl Pts',(-1.81733761904343,6.51840264009593,
30.8894286787655));
#191330=CARTESIAN_POINT('Ctrl Pts',(-1.98483392565318,6.47170449089288,
30.8976514026314));
#191331=CARTESIAN_POINT('Ctrl Pts',(-2.15075201823491,6.41848410030407,
30.9058741264973));
#191332=CARTESIAN_POINT('Ctrl Pts',(-2.31454734880366,6.3588646447417,30.9140968503632));
#191333=CARTESIAN_POINT('Ctrl Pts',(-2.47816930756371,6.29930829435338,
30.9223108707544));
#191334=CARTESIAN_POINT('Ctrl Pts',(-2.63967264426746,6.23336648827075,
30.9305248911456));
#191335=CARTESIAN_POINT('Ctrl Pts',(-2.79852568667736,6.16121278491556,
30.9387389115368));
#191336=CARTESIAN_POINT('Ctrl Pts',(-2.95724248172313,6.08912096738734,
30.9469458868088));
#191337=CARTESIAN_POINT('Ctrl Pts',(-3.11331318487453,6.01082801108859,
30.9551528620807));
#191338=CARTESIAN_POINT('Ctrl Pts',(-3.26622382503544,5.92655641370019,
30.9633598373527));
#191339=CARTESIAN_POINT('Ctrl Pts',(-3.41903400595708,5.84234018106964,
30.9715614208057));
#191340=CARTESIAN_POINT('Ctrl Pts',(-3.56868794618186,5.75215330367483,
30.9797630042587));
#191341=CARTESIAN_POINT('Ctrl Pts',(-3.71469403590035,5.65626530668836,
30.9879645877116));
#191342=CARTESIAN_POINT('Ctrl Pts',(-3.86063350205369,5.56042106404273,
30.9961624287267));
#191343=CARTESIAN_POINT('Ctrl Pts',(-4.00292813464445,5.45888108106069,
31.0043602697417));
#191344=CARTESIAN_POINT('Ctrl Pts',(-4.14111313438697,5.35195954844651,
31.0125581107568));
#191345=CARTESIAN_POINT('Ctrl Pts',(-4.27928593973443,5.24504745132396,
31.0207552283379));
#191346=CARTESIAN_POINT('Ctrl Pts',(-4.41334954586082,5.13275496308821,
31.0289523459191));
#191347=CARTESIAN_POINT('Ctrl Pts',(-4.54286994362221,5.01543833331983,
31.0371494635002));
#191348=CARTESIAN_POINT('Ctrl Pts',(-4.67238890032491,4.89812300882963,
31.0453464898793));
#191349=CARTESIAN_POINT('Ctrl Pts',(-4.79736448266942,4.7757838942429,31.0535435162584));
#191350=CARTESIAN_POINT('Ctrl Pts',(-4.91739755847299,4.64881600538501,
31.0617405426375));
#191351=CARTESIAN_POINT('Ctrl Pts',(-5.03745112442993,4.52182644257186,
31.0699389682836));
#191352=CARTESIAN_POINT('Ctrl Pts',(-5.15256025641228,4.3902067920332,31.0781373939298));
#191353=CARTESIAN_POINT('Ctrl Pts',(-5.26236430002846,4.25438726184934,
31.0863358195759));
#191354=CARTESIAN_POINT('Ctrl Pts',(-5.37220705358104,4.11851985031975,
31.0945371354666));
#191355=CARTESIAN_POINT('Ctrl Pts',(-5.47674076777648,3.97844988862926,
31.1027384513572));
#191356=CARTESIAN_POINT('Ctrl Pts',(-5.57564649180597,3.83463886153726,
31.1109397672479));
#191357=CARTESIAN_POINT('Ctrl Pts',(-5.67466485289878,3.69066405775869,
31.1191504230644));
#191358=CARTESIAN_POINT('Ctrl Pts',(-5.7680422155583,3.5429399729292,31.1273610788811));
#191359=CARTESIAN_POINT('Ctrl Pts',(-5.85550366702557,3.39195604415065,
31.1355717346976));
#191360=CARTESIAN_POINT('Ctrl Pts',(-5.94301665740724,3.2408831442008,31.1437872288548));
#191361=CARTESIAN_POINT('Ctrl Pts',(-6.02460662015879,3.08654688789638,
31.1520027230119));
#191362=CARTESIAN_POINT('Ctrl Pts',(-6.10004574468918,2.92945915020152,
31.1602182171691));
#191363=CARTESIAN_POINT('Ctrl Pts',(-6.17560191440945,2.77212768799103,
31.1684464578166));
#191364=CARTESIAN_POINT('Ctrl Pts',(-6.2449880323563,2.61203654231964,31.1766746984641));
#191365=CARTESIAN_POINT('Ctrl Pts',(-6.3080248742912,2.4497165520369,31.1849029391116));
#191366=CARTESIAN_POINT('Ctrl Pts',(-6.36531529971067,2.30219359543024,
31.1923810962127));
#191367=CARTESIAN_POINT('Ctrl Pts',(-6.41736184690403,2.15283002573584,
31.1998592533139));
#191368=CARTESIAN_POINT('Ctrl Pts',(-6.46406641715259,2.00203255583923,
31.207337410415));
#191369=CARTESIAN_POINT('Ctrl Pts',(-6.52558928020088,1.80339049492085,
31.2171882158659));
#191370=CARTESIAN_POINT('Ctrl Pts',(-6.57800965699778,1.60172401471904,
31.2270390213168));
#191371=CARTESIAN_POINT('Ctrl Pts',(-6.62106237412575,1.3977918435648,31.2368898267678));
#191372=CARTESIAN_POINT('Ctrl Pts',(-6.66381959841371,1.19525936331145,
31.2466730210974));
#191373=CARTESIAN_POINT('Ctrl Pts',(-6.69733723382138,0.990492200673051,
31.2564562154271));
#191374=CARTESIAN_POINT('Ctrl Pts',(-6.72140083822521,0.784257465316973,
31.2662394097567));
#191375=CARTESIAN_POINT('Ctrl Pts',(-6.7451831335258,0.580433661735232,
31.275908236281));
#191376=CARTESIAN_POINT('Ctrl Pts',(-6.75973107202396,0.375176437153415,
31.2855770628053));
#191377=CARTESIAN_POINT('Ctrl Pts',(-6.76488312322251,0.1692493106021,31.2952458893297));
#191378=CARTESIAN_POINT('Ctrl Pts',(-6.76622845433865,0.115476519857375,
31.2977706649343));
#191379=CARTESIAN_POINT('Ctrl Pts',(-6.76693336023889,0.0616581720950804,
31.3002954405389));
#191380=CARTESIAN_POINT('Ctrl Pts',(-6.76699549529041,0.00780811880521902,
31.3028202161435));
#191381=CARTESIAN_POINT('Ctrl Pts',(-6.76699549529156,0.00780811781447526,
31.3028202161899));
#191382=CARTESIAN_POINT('Ctrl Pts',(-6.76719184327957,-0.162359134009222,
31.3107985578972));
#191383=CARTESIAN_POINT('Ctrl Pts',(-6.76096531296404,-0.332675349828753,
31.3187768996044));
#191384=CARTESIAN_POINT('Ctrl Pts',(-6.74830930116178,-0.502603796099331,
31.3267552413117));
#191385=CARTESIAN_POINT('Ctrl Pts',(-6.73518991247414,-0.678753863793646,
31.3350256955097));
#191386=CARTESIAN_POINT('Ctrl Pts',(-6.71516126771013,-0.854486811391087,
31.3432961497078));
#191387=CARTESIAN_POINT('Ctrl Pts',(-6.68827515678769,-1.02920572632327,
31.3515666039058));
#191388=CARTESIAN_POINT('Ctrl Pts',(-6.66235021874996,-1.19767847631315,
31.3595413910829));
#191389=CARTESIAN_POINT('Ctrl Pts',(-6.63004972960425,-1.36520804468051,
31.3675161782601));
#191390=CARTESIAN_POINT('Ctrl Pts',(-6.59147278417489,-1.5312659910942,
31.3754909654373));
#191391=CARTESIAN_POINT('Ctrl Pts',(-6.55289330849773,-1.69733482918813,
31.3834662756778));
#191392=CARTESIAN_POINT('Ctrl Pts',(-6.50803664249827,-1.86193148395629,
31.3914415859184));
#191393=CARTESIAN_POINT('Ctrl Pts',(-6.45705259235887,-2.02453965619635,
31.3994168961589));
#191394=CARTESIAN_POINT('Ctrl Pts',(-6.4060548599749,-2.18719146649134,
31.4073943466795));
#191395=CARTESIAN_POINT('Ctrl Pts',(-6.34892658479085,-2.3478533709865,
31.4153717972001));
#191396=CARTESIAN_POINT('Ctrl Pts',(-6.28586676284999,-2.50602634457378,
31.4233492477207));
#191397=CARTESIAN_POINT('Ctrl Pts',(-6.22277722222699,-2.66427386154194,
31.4313304578351));
#191398=CARTESIAN_POINT('Ctrl Pts',(-6.15375071269929,-2.82002976236166,
31.4393116679495));
#191399=CARTESIAN_POINT('Ctrl Pts',(-6.07903336624391,-2.97281723825957,
31.4472928780639));
#191400=CARTESIAN_POINT('Ctrl Pts',(-6.00422403241851,-3.12579281663631,
31.4552839141499));
#191401=CARTESIAN_POINT('Ctrl Pts',(-5.92371004415084,-3.27579233613148,
31.463274950236));
#191402=CARTESIAN_POINT('Ctrl Pts',(-5.8377826042711,-3.42236515662338,
31.471265986322));
#191403=CARTESIAN_POINT('Ctrl Pts',(-5.75179237700291,-3.56904507823024,
31.4792628614775));
#191404=CARTESIAN_POINT('Ctrl Pts',(-5.66038102722886,-3.71229299987543,
31.487259736633));
#191405=CARTESIAN_POINT('Ctrl Pts',(-5.56388123139021,-3.85168984252156,
31.4952566117885));
#191406=CARTESIAN_POINT('Ctrl Pts',(-5.46724056855824,-3.99129017175469,
31.5032651604998));
#191407=CARTESIAN_POINT('Ctrl Pts',(-5.36549686450026,-4.1270279052731,
31.5112737092112));
#191408=CARTESIAN_POINT('Ctrl Pts',(-5.25902133096911,-4.25851894916671,
31.5192822579225));
#191409=CARTESIAN_POINT('Ctrl Pts',(-5.23259091813481,-4.29115896005807,
31.5212702193032));
#191410=CARTESIAN_POINT('Ctrl Pts',(-5.20586910604315,-4.32353748584664,
31.5232581806838));
#191411=CARTESIAN_POINT('Ctrl Pts',(-5.17886189454373,-4.35564903053987,
31.5252461420645));
#191412=CARTESIAN_POINT('Ctrl Pts',(-5.06565597901967,-4.49025073927117,
31.5335790641112));
#191413=CARTESIAN_POINT('Ctrl Pts',(-4.94705382912415,-4.62060908824771,
31.5419119861579));
#191414=CARTESIAN_POINT('Ctrl Pts',(-4.82340118551416,-4.74627116835739,
31.5502449082046));
#191415=CARTESIAN_POINT('Ctrl Pts',(-4.69989466934291,-4.87178474636167,
31.5585679827582));
#191416=CARTESIAN_POINT('Ctrl Pts',(-4.57134979105569,-4.99261286534171,
31.5668910573118));
#191417=CARTESIAN_POINT('Ctrl Pts',(-4.43815272838792,-5.10833528260458,
31.5752141318654));
#191418=CARTESIAN_POINT('Ctrl Pts',(-4.30508862326199,-5.22394218554734,
31.5835288983114));
#191419=CARTESIAN_POINT('Ctrl Pts',(-4.16738184676328,-5.33445331389551,
31.5918436647574));
#191420=CARTESIAN_POINT('Ctrl Pts',(-4.02545578956299,-5.4394847813257,
31.6001584312033));
#191421=CARTESIAN_POINT('Ctrl Pts',(-3.88364536918663,-5.54443067246674,
31.6084664230428));
#191422=CARTESIAN_POINT('Ctrl Pts',(-3.73762279656343,-5.64390559279126,
31.6167744148823));
#191423=CARTESIAN_POINT('Ctrl Pts',(-3.58784511245682,-5.73756537644842,
31.6250824067218));
#191424=CARTESIAN_POINT('Ctrl Pts',(-3.4381620031427,-5.83116602008979,
31.6333851526089));
#191425=CARTESIAN_POINT('Ctrl Pts',(-3.28472880186222,-5.91895866071897,
31.641687898496));
#191426=CARTESIAN_POINT('Ctrl Pts',(-3.12803233099951,-6.00064186035309,
31.6499906443831));
#191427=CARTESIAN_POINT('Ctrl Pts',(-2.97139989699096,-6.08229167866654,
31.6582899972025));
#191428=CARTESIAN_POINT('Ctrl Pts',(-2.81150715872327,-6.15783687033687,
31.666589350022));
#191429=CARTESIAN_POINT('Ctrl Pts',(-2.64886664316344,-6.22702131895629,
31.6748887028414));
#191430=CARTESIAN_POINT('Ctrl Pts',(-2.48626071851213,-6.29619105320441,
31.6831862905278));
#191431=CARTESIAN_POINT('Ctrl Pts',(-2.32090850079585,-6.35900260342622,
31.6914838782141));
#191432=CARTESIAN_POINT('Ctrl Pts',(-2.15334387794478,-6.41524739533229,
31.6997814659004));
#191433=CARTESIAN_POINT('Ctrl Pts',(-1.98578704818373,-6.47148957140742,
31.7080786676829));
#191434=CARTESIAN_POINT('Ctrl Pts',(-1.81601834817873,-6.52116548721558,
31.7163758694653));
#191435=CARTESIAN_POINT('Ctrl Pts',(-1.64458844236092,-6.56411592335578,
31.7246730712477));
#191436=CARTESIAN_POINT('Ctrl Pts',(-1.47313802326137,-6.60707149893996,
31.7329712658723));
#191437=CARTESIAN_POINT('Ctrl Pts',(-1.30002633985434,-6.64329990729337,
31.7412694604968));
#191438=CARTESIAN_POINT('Ctrl Pts',(-1.12581609449634,-6.67269264400609,
31.7495676551214));
#191439=CARTESIAN_POINT('Ctrl Pts',(-0.951483325042399,-6.70210605297311,
31.757871685963));
#191440=CARTESIAN_POINT('Ctrl Pts',(-0.776050793243537,-6.72467412580284,
31.7661757168045));
#191441=CARTESIAN_POINT('Ctrl Pts',(-0.600089106419969,-6.74033990718243,
31.7744797476461));
#191442=CARTESIAN_POINT('Ctrl Pts',(-0.424063435083924,-6.75601138507133,
31.7827867980618));
#191443=CARTESIAN_POINT('Ctrl Pts',(-0.247508572355687,-6.76477554554829,
31.7910938484776));
#191444=CARTESIAN_POINT('Ctrl Pts',(-0.0709972550978696,-6.76662754921302,
31.7994008988933));
#191445=CARTESIAN_POINT('Ctrl Pts',(0.10570278254808,-6.76848153298223,
31.8077168309479));
#191446=CARTESIAN_POINT('Ctrl Pts',(0.282358833551052,-6.76340859785611,
31.8160327630025));
#191447=CARTESIAN_POINT('Ctrl Pts',(0.458400045588006,-6.75145602060807,
31.8243486950572));
#191448=CARTESIAN_POINT('Ctrl Pts',(0.59110365045948,-6.74244591399742,
31.8306174212761));
#191449=CARTESIAN_POINT('Ctrl Pts',(0.723457918522209,-6.72952755339485,
31.8368861474951));
#191450=CARTESIAN_POINT('Ctrl Pts',(0.855221520991356,-6.71274050966021,
31.843154873714));
#191451=CARTESIAN_POINT('Ctrl Pts',(1.03283939899858,-6.69011150566907,
31.8516051424374));
#191452=CARTESIAN_POINT('Ctrl Pts',(1.20970936416206,-6.66040939559615,
31.8600554111607));
#191453=CARTESIAN_POINT('Ctrl Pts',(1.38524672645127,-6.62369840095819,
31.8685056798841));
#191454=CARTESIAN_POINT('Ctrl Pts',(1.56062917106292,-6.58701980501847,
31.8769484909586));
#191455=CARTESIAN_POINT('Ctrl Pts',(1.73468103386601,-6.54334472104775,
31.8853913020331));
#191456=CARTESIAN_POINT('Ctrl Pts',(1.9068249716965,-6.49278888670459,31.8938341131076));
#191457=CARTESIAN_POINT('Ctrl Pts',(2.07884042450166,-6.4422707862935,31.9022706226254));
#191458=CARTESIAN_POINT('Ctrl Pts',(2.24895047397252,-6.38488226629492,
31.9107071321431));
#191459=CARTESIAN_POINT('Ctrl Pts',(2.41658977724467,-6.32078973297772,
31.9191436416609));
#191460=CARTESIAN_POINT('Ctrl Pts',(2.58410912557434,-6.25674306131705,
31.9275741144021));
#191461=CARTESIAN_POINT('Ctrl Pts',(2.74916094520258,-6.186002063016,31.9360045871433));
#191462=CARTESIAN_POINT('Ctrl Pts',(2.91119662121485,-6.10878246728653,
31.9444350598845));
#191463=CARTESIAN_POINT('Ctrl Pts',(3.07316263853026,-6.03159606805145,
31.9528619083884));
#191464=CARTESIAN_POINT('Ctrl Pts',(3.23211479832979,-5.9479367660304,31.9612887568923));
#191465=CARTESIAN_POINT('Ctrl Pts',(3.38752537980897,-5.85806800926296,
31.9697156053962));
#191466=CARTESIAN_POINT('Ctrl Pts',(3.54288799159001,-5.7682269917723,31.9781398528328));
#191467=CARTESIAN_POINT('Ctrl Pts',(3.69471091835848,-5.67218050755823,
31.9865641002694));
#191468=CARTESIAN_POINT('Ctrl Pts',(3.84249160300592,-5.57023763234829,
31.994988347706));
#191469=CARTESIAN_POINT('Ctrl Pts',(3.88413054576305,-5.5415140305089,31.9973619783169));
#191470=CARTESIAN_POINT('Ctrl Pts',(3.92544874126732,-5.51232258739618,
31.9997356089279));
#191471=CARTESIAN_POINT('Ctrl Pts',(3.96643535015279,-5.48267084668214,
32.0021092395388));
#191472=CARTESIAN_POINT('Ctrl Pts',(4.11525994051487,-5.37500377479484,
32.010728020476));
#191473=CARTESIAN_POINT('Ctrl Pts',(4.25964378853244,-5.26131284237969,
32.0193468014133));
#191474=CARTESIAN_POINT('Ctrl Pts',(4.39911338632861,-5.14199284462984,
32.0279655823505));
#191475=CARTESIAN_POINT('Ctrl Pts',(4.53866676266386,-5.02260117208309,
32.036589540537));
#191476=CARTESIAN_POINT('Ctrl Pts',(4.67329976643146,-4.89757388380107,
32.0452134987235));
#191477=CARTESIAN_POINT('Ctrl Pts',(4.80257417362319,-4.76734415653491,
32.05383745691));
#191478=CARTESIAN_POINT('Ctrl Pts',(4.93651882406666,-4.63240967356224,
32.0627729692812));
#191479=CARTESIAN_POINT('Ctrl Pts',(5.06471023354607,-4.49189011125268,
32.0717084816523));
#191480=CARTESIAN_POINT('Ctrl Pts',(5.18670535870331,-4.34630607780888,
32.0806439940234));
#191481=CARTESIAN_POINT('Ctrl Pts',(5.30466701868792,-4.2055354180784,32.0892840759181));
#191482=CARTESIAN_POINT('Ctrl Pts',(5.41683541664909,-4.06003008503996,
32.0979241578128));
#191483=CARTESIAN_POINT('Ctrl Pts',(5.52285301360676,-3.91029200828976,
32.1065642397075));
#191484=CARTESIAN_POINT('Ctrl Pts',(5.63430820297883,-3.75287393639111,
32.1156474673169));
#191485=CARTESIAN_POINT('Ctrl Pts',(5.73896486183385,-3.59077785566703,
32.1247306949262));
#191486=CARTESIAN_POINT('Ctrl Pts',(5.83646083153779,-3.42461880534538,
32.1338139225356));
#191487=CARTESIAN_POINT('Ctrl Pts',(5.93395680124173,-3.25845975502374,
32.1428971501449));
#191488=CARTESIAN_POINT('Ctrl Pts',(6.0242919297448,-3.0882380934111,32.1519803777542));
#191489=CARTESIAN_POINT('Ctrl Pts',(6.10716115225622,-2.91459631173385,
32.1610636053636));
#191490=CARTESIAN_POINT('Ctrl Pts',(6.18967791570172,-2.74169306263019,
32.1701082002234));
#191491=CARTESIAN_POINT('Ctrl Pts',(6.26486913904146,-2.56523943023071,
32.1791527950832));
#191492=CARTESIAN_POINT('Ctrl Pts',(6.33245769943833,-2.38584754014675,
32.188197389943));
#191493=CARTESIAN_POINT('Ctrl Pts',(6.3999842366925,-2.20662027035845,32.1972336849634));
#191494=CARTESIAN_POINT('Ctrl Pts',(6.4599219560979,-2.02446034851526,32.2062699799837));
#191495=CARTESIAN_POINT('Ctrl Pts',(6.51204204323386,-1.83999930085709,
32.2153062750041));
#191496=CARTESIAN_POINT('Ctrl Pts',(6.56406989978825,-1.65586467148865,
32.2243265795918));
#191497=CARTESIAN_POINT('Ctrl Pts',(6.60830768403376,-1.46943727624787,
32.2333468841795));
#191498=CARTESIAN_POINT('Ctrl Pts',(6.64457657006855,-1.28136302603753,
32.2423671887672));
#191499=CARTESIAN_POINT('Ctrl Pts',(6.6807997824869,-1.09352561881039,32.2513761340335));
#191500=CARTESIAN_POINT('Ctrl Pts',(6.70907407874981,-0.904045728284308,
32.2603850792999));
#191501=CARTESIAN_POINT('Ctrl Pts',(6.72927120261495,-0.713581166831877,
32.2693940245662));
#191502=CARTESIAN_POINT('Ctrl Pts',(6.74942246308742,-0.52354911007812,
32.278382512425));
#191503=CARTESIAN_POINT('Ctrl Pts',(6.7615331374365,-0.332537081736051,
32.2873710002838));
#191504=CARTESIAN_POINT('Ctrl Pts',(6.76552650890326,-0.141209267851879,
32.2963594881426));
#191505=CARTESIAN_POINT('Ctrl Pts',(6.76903014275974,0.0266545564857062,
32.3042456491578));
#191506=CARTESIAN_POINT('Ctrl Pts',(6.76628608516899,0.194761201565154,
32.3121318101731));
#191507=CARTESIAN_POINT('Ctrl Pts',(6.75727523833114,0.362657349900467,
32.3200179711883));
#191508=CARTESIAN_POINT('Ctrl Pts',(6.74799552976617,0.535563110454366,
32.3281394360445));
#191509=CARTESIAN_POINT('Ctrl Pts',(6.73207200223608,0.708168137699135,
32.3362609009007));
#191510=CARTESIAN_POINT('Ctrl Pts',(6.70954746935247,0.879921449054339,
32.3443823657569));
#191511=CARTESIAN_POINT('Ctrl Pts',(6.68702454279963,1.05166251187013,32.352503251433));
#191512=CARTESIAN_POINT('Ctrl Pts',(6.65790159617412,1.22255161670381,32.3606241371092));
#191513=CARTESIAN_POINT('Ctrl Pts',(6.62227317093297,1.39204419812784,32.3687450227854));
#191514=CARTESIAN_POINT('Ctrl Pts',(6.58664048707617,1.56155703876218,32.3768668791397));
#191515=CARTESIAN_POINT('Ctrl Pts',(6.54450085274506,1.72967266550059,32.3849887354939));
#191516=CARTESIAN_POINT('Ctrl Pts',(6.49599964184681,1.89585802557211,32.3931105918482));
#191517=CARTESIAN_POINT('Ctrl Pts',(6.44746304506513,2.06216463242634,32.4012383738083));
#191518=CARTESIAN_POINT('Ctrl Pts',(6.39255570441807,2.2265378079745,32.4093661557685));
#191519=CARTESIAN_POINT('Ctrl Pts',(6.33147267132592,2.38846034345412,32.4174939377287));
#191520=CARTESIAN_POINT('Ctrl Pts',(6.27036475527627,2.55044884015679,32.4256250306451));
#191521=CARTESIAN_POINT('Ctrl Pts',(6.20307627439913,2.7099843697335,32.4337561235616));
#191522=CARTESIAN_POINT('Ctrl Pts',(6.12984980112805,2.8665711949314,32.441887216478));
#191523=CARTESIAN_POINT('Ctrl Pts',(6.05654340422177,3.02332892810471,32.4500271841426));
#191524=CARTESIAN_POINT('Ctrl Pts',(5.97728623760122,3.1771312035923,32.4581671518071));
#191525=CARTESIAN_POINT('Ctrl Pts',(5.8923664078801,3.3275076431597,32.4663071194717));
#191526=CARTESIAN_POINT('Ctrl Pts',(5.84832331248869,3.40549936657975,32.4705288586522));
#191527=CARTESIAN_POINT('Ctrl Pts',(5.80275772824519,3.48257004300769,32.4747505978326));
#191528=CARTESIAN_POINT('Ctrl Pts',(5.75571430051519,3.55865731573651,32.4789723370131));
#191529=CARTESIAN_POINT('Ctrl Pts',(5.6616666918867,3.71076838400895,32.4874122933117));
#191530=CARTESIAN_POINT('Ctrl Pts',(5.56151575697688,3.85926168118158,32.4958522496103));
#191531=CARTESIAN_POINT('Ctrl Pts',(5.45556534188854,4.00363532310132,32.5042922059089));
#191532=CARTESIAN_POINT('Ctrl Pts',(5.34969215428111,4.14790373076912,32.5127260103055));
#191533=CARTESIAN_POINT('Ctrl Pts',(5.2380281087655,4.28805820050605,32.5211598147022));
#191534=CARTESIAN_POINT('Ctrl Pts',(5.12092063759979,4.42362530323315,32.5295936190988));
#191535=CARTESIAN_POINT('Ctrl Pts',(5.00388213697058,4.55911256360934,32.5380224563998));
#191536=CARTESIAN_POINT('Ctrl Pts',(4.88140681907092,4.69001759109137,32.5464512937007));
#191537=CARTESIAN_POINT('Ctrl Pts',(4.75388294872376,4.81589928360566,32.5548801310017));
#191538=CARTESIAN_POINT('Ctrl Pts',(4.62641663704579,4.94172415865764,32.563305163896));
#191539=CARTESIAN_POINT('Ctrl Pts',(4.49390655336497,5.06252998563764,32.5717301967904));
#191540=CARTESIAN_POINT('Ctrl Pts',(4.35677868991053,5.17791159128287,32.5801552296847));
#191541=CARTESIAN_POINT('Ctrl Pts',(4.21969089840114,5.29325947974441,32.5885778005888));
#191542=CARTESIAN_POINT('Ctrl Pts',(4.07798827294214,5.40318609321708,32.597000371493));
#191543=CARTESIAN_POINT('Ctrl Pts',(3.93213113612272,5.50732546054201,32.6054229423971));
#191544=CARTESIAN_POINT('Ctrl Pts',(3.78627698404962,5.61146269681186,32.613845340946));
#191545=CARTESIAN_POINT('Ctrl Pts',(3.63626875842448,5.70981272508494,32.622267739495));
#191546=CARTESIAN_POINT('Ctrl Pts',(3.48259759741858,5.80205161769993,32.6306901380439));
#191547=CARTESIAN_POINT('Ctrl Pts',(3.35711527563958,5.87737056712343,32.6375675646082));
#191548=CARTESIAN_POINT('Ctrl Pts',(3.2291912354976,5.94861549514981,32.6444449911725));
#191549=CARTESIAN_POINT('Ctrl Pts',(3.09910619832134,6.0156321173694,32.6513224177368));
#191550=CARTESIAN_POINT('Origin',(0.,0.,4.30282021618968));
#191551=CARTESIAN_POINT('',(3.09910619832134,6.0156321173694,35.0460577214445));
#191552=CARTESIAN_POINT('',(3.09910619832129,6.01563211736943,34.6512344137135));
#191553=CARTESIAN_POINT('',(3.09910619832133,6.0156321173694,4.30282021618968));
#191554=CARTESIAN_POINT('',(-6.76699957039783,-0.0024112725963184,33.6971797837815));
#191555=CARTESIAN_POINT('Ctrl Pts',(-6.76699957039762,-0.00241127320226596,
33.6971797838101));
#191556=CARTESIAN_POINT('Ctrl Pts',(-6.7669271526358,-0.205644553729062,
33.7067651955258));
#191557=CARTESIAN_POINT('Ctrl Pts',(-6.75769587893337,-0.408730533938623,
33.7163506072415));
#191558=CARTESIAN_POINT('Ctrl Pts',(-6.73936492970196,-0.610941359136269,
33.7259360189573));
#191559=CARTESIAN_POINT('Ctrl Pts',(-6.72206822778545,-0.801743282352738,
33.7349806138171));
#191560=CARTESIAN_POINT('Ctrl Pts',(-6.69665992838825,-0.991859096466692,
33.7440252086769));
#191561=CARTESIAN_POINT('Ctrl Pts',(-6.66321417359887,-1.18062097082473,
33.7530698035367));
#191562=CARTESIAN_POINT('Ctrl Pts',(-6.62979911055412,-1.36920962645055,
33.7621060985571));
#191563=CARTESIAN_POINT('Ctrl Pts',(-6.58836135906894,-1.5564465888405,
33.7711423935774));
#191564=CARTESIAN_POINT('Ctrl Pts',(-6.53902650525747,-1.74167200228408,
33.7801786885978));
#191565=CARTESIAN_POINT('Ctrl Pts',(-6.48977895333856,-1.92656964483361,
33.7891989931855));
#191566=CARTESIAN_POINT('Ctrl Pts',(-6.43266226562066,-2.10946261691137,
33.7982192977732));
#191567=CARTESIAN_POINT('Ctrl Pts',(-6.36785235671145,-2.28970420865327,
33.8072396023609));
#191568=CARTESIAN_POINT('Ctrl Pts',(-6.30312406329269,-2.46971882112366,
33.8162485476272));
#191569=CARTESIAN_POINT('Ctrl Pts',(-6.230721963088,-2.64708849335919,33.8252574928936));
#191570=CARTESIAN_POINT('Ctrl Pts',(-6.1508715314434,-2.82118209332171,
33.8342664381599));
#191571=CARTESIAN_POINT('Ctrl Pts',(-6.07120242322513,-2.99488036357349,
33.8432549260187));
#191572=CARTESIAN_POINT('Ctrl Pts',(-5.98411884353561,-3.16531719513597,
33.8522434138775));
#191573=CARTESIAN_POINT('Ctrl Pts',(-5.8898938408915,-3.33188228228855,
33.8612319017363));
#191574=CARTESIAN_POINT('Ctrl Pts',(-5.80722436920872,-3.47802022199983,
33.8691180627515));
#191575=CARTESIAN_POINT('Ctrl Pts',(-5.71905843551334,-3.62117797452296,
33.8770042237668));
#191576=CARTESIAN_POINT('Ctrl Pts',(-5.62561100294064,-3.76095597469489,
33.884890384782));
#191577=CARTESIAN_POINT('Ctrl Pts',(-5.52937532653589,-3.90490461001544,
33.8930118496382));
#191578=CARTESIAN_POINT('Ctrl Pts',(-5.42757999479772,-4.04520345033654,
33.9011333144944));
#191579=CARTESIAN_POINT('Ctrl Pts',(-5.3205430607239,-4.18140054754178,
33.9092547793505));
#191580=CARTESIAN_POINT('Ctrl Pts',(-5.21351375995882,-4.31758793188949,
33.9173756650267));
#191581=CARTESIAN_POINT('Ctrl Pts',(-5.10124382769221,-4.4496738678554,
33.9254965507029));
#191582=CARTESIAN_POINT('Ctrl Pts',(-4.98409252327873,-4.57723832888316,
33.9336174363792));
#191583=CARTESIAN_POINT('Ctrl Pts',(-4.86692721593431,-4.70481803751185,
33.9417392927334));
#191584=CARTESIAN_POINT('Ctrl Pts',(-4.7448796232044,-4.82787492616167,
33.9498611490877));
#191585=CARTESIAN_POINT('Ctrl Pts',(-4.61834683994616,-4.9460248145313,
33.957983005442));
#191586=CARTESIAN_POINT('Ctrl Pts',(-4.4917217399348,-5.06426090359765,
33.9661107874021));
#191587=CARTESIAN_POINT('Ctrl Pts',(-4.360605181564,-5.17758259180336,33.9742385693623));
#191588=CARTESIAN_POINT('Ctrl Pts',(-4.22542889119776,-5.28564468020991,
33.9823663513225));
#191589=CARTESIAN_POINT('Ctrl Pts',(-4.09019753503495,-5.3937507890949,
33.9904974442389));
#191590=CARTESIAN_POINT('Ctrl Pts',(-3.95090344480812,-5.4965928100976,
33.9986285371554));
#191591=CARTESIAN_POINT('Ctrl Pts',(-3.80800825153753,-5.59386826411045,
34.0067596300718));
#191592=CARTESIAN_POINT('Ctrl Pts',(-3.66495709413552,-5.69124989021592,
34.0148995977364));
#191593=CARTESIAN_POINT('Ctrl Pts',(-3.5182972932805,-5.7830526201265,34.0230395654009));
#191594=CARTESIAN_POINT('Ctrl Pts',(-3.36851669183846,-5.8690190233808,
34.0311795330655));
#191595=CARTESIAN_POINT('Ctrl Pts',(-3.29083399583325,-5.91360491705708,
34.0354012722459));
#191596=CARTESIAN_POINT('Ctrl Pts',(-3.21231220779933,-5.95662166305593,
34.0396230114264));
#191597=CARTESIAN_POINT('Ctrl Pts',(-3.13302154779433,-5.99803842777424,
34.0438447506068));
#191598=CARTESIAN_POINT('Ctrl Pts',(-2.97450162274143,-6.08083988810595,
34.0522849600644));
#191599=CARTESIAN_POINT('Ctrl Pts',(-2.81257972647671,-6.15741467235917,
34.0607251695221));
#191600=CARTESIAN_POINT('Ctrl Pts',(-2.64777336502189,-6.22748626714509,
34.0691653789797));
#191601=CARTESIAN_POINT('Ctrl Pts',(-2.48309186880216,-6.29750477231675,
34.0775991937282));
#191602=CARTESIAN_POINT('Ctrl Pts',(-2.31553056965315,-6.36102977990712,
34.0860330084768));
#191603=CARTESIAN_POINT('Ctrl Pts',(-2.14562988568944,-6.41783151801575,
34.0944668232253));
#191604=CARTESIAN_POINT('Ctrl Pts',(-1.97583180836011,-6.47459895234738,
34.1028955446139));
#191605=CARTESIAN_POINT('Ctrl Pts',(-1.80369747832809,-6.52465110656424,
34.1113242660024));
#191606=CARTESIAN_POINT('Ctrl Pts',(-1.62978590058578,-6.56780685756302,
34.1197529873909));
#191607=CARTESIAN_POINT('Ctrl Pts',(-1.45595264623619,-6.6109431727952,
34.1281779127927));
#191608=CARTESIAN_POINT('Ctrl Pts',(-1.28034406322702,-6.64718919741407,
34.1366028381944));
#191609=CARTESIAN_POINT('Ctrl Pts',(-1.10353326092001,-6.67641395825957,
34.1450277635961));
#191610=CARTESIAN_POINT('Ctrl Pts',(-0.926774959693113,-6.70563004128964,
34.1534501873539));
#191611=CARTESIAN_POINT('Ctrl Pts',(-0.7488154797323,-6.72782896386837,
34.1618726111116));
#191612=CARTESIAN_POINT('Ctrl Pts',(-0.570237433187901,-6.74293098509775,
34.1702950348693));
#191613=CARTESIAN_POINT('Ctrl Pts',(-0.391656578125033,-6.75803324383844,
34.1787175910875));
#191614=CARTESIAN_POINT('Ctrl Pts',(-0.212457468695141,-6.76603834350035,
34.1871401473057));
#191615=CARTESIAN_POINT('Ctrl Pts',(-0.0332278194027092,-6.76691842067109,
34.1955627035239));
#191616=CARTESIAN_POINT('Ctrl Pts',(0.146007884301281,-6.76779852757101,
34.2039855442577));
#191617=CARTESIAN_POINT('Ctrl Pts',(0.325273796352285,-6.76155313026978,
34.2124083849914));
#191618=CARTESIAN_POINT('Ctrl Pts',(0.503982060694046,-6.74820650858423,
34.2208312257252));
#191619=CARTESIAN_POINT('Ctrl Pts',(0.682721311485282,-6.73485757271126,
34.2292555269058));
#191620=CARTESIAN_POINT('Ctrl Pts',(0.860902389161484,-6.71440498246587,
34.2376798280864));
#191621=CARTESIAN_POINT('Ctrl Pts',(1.03794204611007,-6.68692495164383,
34.2461041292671));
#191622=CARTESIAN_POINT('Ctrl Pts',(1.21503712445465,-6.65943631833297,
34.2545310676339));
#191623=CARTESIAN_POINT('Ctrl Pts',(1.3909897401937,-6.62491590957336,34.2629580060007));
#191624=CARTESIAN_POINT('Ctrl Pts',(1.5652259636951,-6.58349122294355,34.2713849443675));
#191625=CARTESIAN_POINT('Ctrl Pts',(1.739618847463,-6.54202929031335,34.2798194596111));
#191626=CARTESIAN_POINT('Ctrl Pts',(1.91229193050123,-6.49365075284648,
34.2882539748548));
#191627=CARTESIAN_POINT('Ctrl Pts',(2.08268448301231,-6.43853355541615,
34.2966884900984));
#191628=CARTESIAN_POINT('Ctrl Pts',(2.25315933658591,-6.3833897359073,34.3051270792852));
#191629=CARTESIAN_POINT('Ctrl Pts',(2.42135114815643,-6.32150087536006,
34.313565668472));
#191630=CARTESIAN_POINT('Ctrl Pts',(2.58671785149581,-6.25309361490398,
34.3220042576587));
#191631=CARTESIAN_POINT('Ctrl Pts',(2.75226939739626,-6.18460989060746,
34.330452279279));
#191632=CARTESIAN_POINT('Ctrl Pts',(2.91498922011784,-6.10959334256098,
34.3389003008993));
#191633=CARTESIAN_POINT('Ctrl Pts',(3.07435748803953,-6.02831776167575,
34.3473483225196));
#191634=CARTESIAN_POINT('Ctrl Pts',(3.16493985392956,-5.982122025839,34.3521500424319));
#191635=CARTESIAN_POINT('Ctrl Pts',(3.25443992877924,-5.93390507819876,
34.3569517623441));
#191636=CARTESIAN_POINT('Ctrl Pts',(3.34276625935181,-5.88372354341527,
34.3617534822563));
#191637=CARTESIAN_POINT('Ctrl Pts',(3.49433020463023,-5.79761432385856,
34.3699930141071));
#191638=CARTESIAN_POINT('Ctrl Pts',(3.64277477392542,-5.70552565776409,
34.3782325459579));
#191639=CARTESIAN_POINT('Ctrl Pts',(3.78759811378457,-5.60770804593602,
34.3864720778088));
#191640=CARTESIAN_POINT('Ctrl Pts',(3.93226070985816,-5.50999900482062,
34.3947024643551));
#191641=CARTESIAN_POINT('Ctrl Pts',(4.07330978728402,-5.40657387672074,
34.4029328509015));
#191642=CARTESIAN_POINT('Ctrl Pts',(4.21026787585194,-5.29772908080143,
34.4111632374478));
#191643=CARTESIAN_POINT('Ctrl Pts',(4.34709838257771,-5.18898567808728,
34.4193859570656));
#191644=CARTESIAN_POINT('Ctrl Pts',(4.47984521295829,-5.07483288212843,
34.4276086766834));
#191645=CARTESIAN_POINT('Ctrl Pts',(4.60805963189971,-4.95561050011563,
34.4358313963012));
#191646=CARTESIAN_POINT('Ctrl Pts',(4.73616044362843,-4.83649375772296,
34.444046829997));
#191647=CARTESIAN_POINT('Ctrl Pts',(4.85973658862605,-4.71231662372661,
34.4522622636928));
#191648=CARTESIAN_POINT('Ctrl Pts',(4.97837231072254,-4.58345918884756,
34.4604776973885));
#191649=CARTESIAN_POINT('Ctrl Pts',(5.09694706327011,-4.45466797668406,
34.4686889089894));
#191650=CARTESIAN_POINT('Ctrl Pts',(5.21058620907145,-4.32120151522181,
34.4769001205902));
#191651=CARTESIAN_POINT('Ctrl Pts',(5.31891048686519,-4.18347705057832,
34.485111332191));
#191652=CARTESIAN_POINT('Ctrl Pts',(5.4271984386734,-4.04579877112076,34.4933197902045));
#191653=CARTESIAN_POINT('Ctrl Pts',(5.53017485320515,-3.90386561242643,
34.501528248218));
#191654=CARTESIAN_POINT('Ctrl Pts',(5.62750039659726,-3.75812829561442,
34.5097367062316));
#191655=CARTESIAN_POINT('Ctrl Pts',(5.67086105135836,-3.69319913868554,
34.5133937535147));
#191656=CARTESIAN_POINT('Ctrl Pts',(5.71310061191423,-3.62751532051784,
34.5170508007979));
#191657=CARTESIAN_POINT('Ctrl Pts',(5.75419177661988,-3.56111864417351,
34.5207078480811));
#191658=CARTESIAN_POINT('Ctrl Pts',(5.8537337425594,-3.40027492649089,34.529566922257));
#191659=CARTESIAN_POINT('Ctrl Pts',(5.94643025790849,-3.23541338678471,
34.5384259964329));
#191660=CARTESIAN_POINT('Ctrl Pts',(6.03200112876272,-3.06712428548393,
34.5472850706088));
#191661=CARTESIAN_POINT('Ctrl Pts',(6.11773277006746,-2.89851900281952,
34.5561607892027));
#191662=CARTESIAN_POINT('Ctrl Pts',(6.19631189493145,-2.72647352027105,
34.5650365077966));
#191663=CARTESIAN_POINT('Ctrl Pts',(6.26750626288204,-2.55159837057764,
34.5739122263905));
#191664=CARTESIAN_POINT('Ctrl Pts',(6.33890379944304,-2.37622417661734,
34.5828132737775));
#191665=CARTESIAN_POINT('Ctrl Pts',(6.40287430870817,-2.19800439778514,
34.5917143211645));
#191666=CARTESIAN_POINT('Ctrl Pts',(6.45923434673109,-2.01756800480415,
34.6006153685515));
#191667=CARTESIAN_POINT('Ctrl Pts',(6.51567100699877,-1.83688630607194,
34.6095285170345));
#191668=CARTESIAN_POINT('Ctrl Pts',(6.56447645711243,-1.65398222284785,
34.6184416655175));
#191669=CARTESIAN_POINT('Ctrl Pts',(6.60551804789054,-1.46949662095304,
34.6273548140005));
#191670=CARTESIAN_POINT('Ctrl Pts',(6.64665076222272,-1.28460141057566,
34.6362877521104));
#191671=CARTESIAN_POINT('Ctrl Pts',(6.67998508175404,-1.09811791216753,
34.6452206902203));
#191672=CARTESIAN_POINT('Ctrl Pts',(6.7054396206955,-0.910696707585425,
34.6541536283302));
#191673=CARTESIAN_POINT('Ctrl Pts',(6.72966865101346,-0.732298895765291,
34.6626564901887));
#191674=CARTESIAN_POINT('Ctrl Pts',(6.74675876246543,-0.553051726812206,
34.6711593520473));
#191675=CARTESIAN_POINT('Ctrl Pts',(6.75668362546571,-0.373517583740801,
34.6796622139058));
#191676=CARTESIAN_POINT('Ctrl Pts',(6.76628150077116,-0.199898429680771,
34.6878849377717));
#191677=CARTESIAN_POINT('Ctrl Pts',(6.76919589212276,-0.0256780814334027,
34.6961076616376));
#191678=CARTESIAN_POINT('Ctrl Pts',(6.7653684706439,0.148588210896766,34.7043303855035));
#191679=CARTESIAN_POINT('Ctrl Pts',(6.76154510036101,0.32267004825996,34.7125444058947));
#191680=CARTESIAN_POINT('Ctrl Pts',(6.75099413508758,0.496797377211207,
34.7207584262859));
#191681=CARTESIAN_POINT('Ctrl Pts',(6.73370909347369,0.670410951931526,
34.7289724466771));
#191682=CARTESIAN_POINT('Ctrl Pts',(6.71643887714313,0.843875619261818,
34.7371794219491));
#191683=CARTESIAN_POINT('Ctrl Pts',(6.69244612277225,1.01682705500566,34.7453863972211));
#191684=CARTESIAN_POINT('Ctrl Pts',(6.66177638078357,1.18870705072113,34.753593372493));
#191685=CARTESIAN_POINT('Ctrl Pts',(6.63112678820333,1.36047412470952,34.761794955946));
#191686=CARTESIAN_POINT('Ctrl Pts',(6.59380900846871,1.5311708089034,34.769996539399));
#191687=CARTESIAN_POINT('Ctrl Pts',(6.54992031077734,1.70024495954743,34.778198122852));
#191688=CARTESIAN_POINT('Ctrl Pts',(6.50605163979526,1.86924196051419,34.786395963867));
#191689=CARTESIAN_POINT('Ctrl Pts',(6.45561811425605,2.03661755643509,34.7945938048821));
#191690=CARTESIAN_POINT('Ctrl Pts',(6.39876791504692,2.20183064048216,34.8027916458971));
#191691=CARTESIAN_POINT('Ctrl Pts',(6.34192273269053,2.36702914498994,34.8109887634783));
#191692=CARTESIAN_POINT('Ctrl Pts',(6.27866211308071,2.53006517600267,34.8191858810594));
#191693=CARTESIAN_POINT('Ctrl Pts',(6.20918395909201,2.69041326976999,34.8273829986406));
#191694=CARTESIAN_POINT('Ctrl Pts',(6.13970657812516,2.85075957948618,34.8355800250197));
#191695=CARTESIAN_POINT('Ctrl Pts',(6.0640119422426,3.00841768184325,34.8437770513988));
#191696=CARTESIAN_POINT('Ctrl Pts',(5.98234587145017,3.16288268425231,34.8519740777779));
#191697=CARTESIAN_POINT('Ctrl Pts',(5.9006658599143,3.31737405449014,34.860172503424));
#191698=CARTESIAN_POINT('Ctrl Pts',(5.81301255034493,3.4686709215932,34.8683709290701));
#191699=CARTESIAN_POINT('Ctrl Pts',(5.71967745242754,3.61629352240551,34.8765693547163));
#191700=CARTESIAN_POINT('Ctrl Pts',(5.62630945047878,3.76396816557697,34.8847706706069));
#191701=CARTESIAN_POINT('Ctrl Pts',(5.52725586175385,3.90796565906952,34.8929719864976));
#191702=CARTESIAN_POINT('Ctrl Pts',(5.4228512141872,4.04783568203903,34.9011733023882));
#191703=CARTESIAN_POINT('Ctrl Pts',(5.31832766720378,4.18786499355118,34.9093839582048));
#191704=CARTESIAN_POINT('Ctrl Pts',(5.20844110159758,4.32375715592714,34.9175946140214));
#191705=CARTESIAN_POINT('Ctrl Pts',(5.09356666560883,4.4550945694787,34.925805269838));
#191706=CARTESIAN_POINT('Ctrl Pts',(4.97862453689802,4.58650937698614,34.9340207639951));
#191707=CARTESIAN_POINT('Ctrl Pts',(4.85868892501422,4.71336382520894,34.9422362581523));
#191708=CARTESIAN_POINT('Ctrl Pts',(4.73417136100773,4.83527770915117,34.9504517523094));
#191709=CARTESIAN_POINT('Ctrl Pts',(4.60946060570938,4.95738074472775,34.9586799929569));
#191710=CARTESIAN_POINT('Ctrl Pts',(4.48015395749285,5.07452765682164,34.9669082336044));
#191711=CARTESIAN_POINT('Ctrl Pts',(4.34669651735882,5.18637815686253,34.9751364742519));
#191712=CARTESIAN_POINT('Ctrl Pts',(4.22540501090053,5.28803240434733,34.9826146313531));
#191713=CARTESIAN_POINT('Ctrl Pts',(4.10068554142758,5.38531227359529,34.9900927884542));
#191714=CARTESIAN_POINT('Ctrl Pts',(3.97289173337,5.47799418354203,34.9975709455553));
#191715=CARTESIAN_POINT('Ctrl Pts',(3.83479376690758,5.57814914007742,35.0056520748702));
#191716=CARTESIAN_POINT('Ctrl Pts',(3.69265246187375,5.67326238485263,35.0137332041851));
#191717=CARTESIAN_POINT('Ctrl Pts',(3.54687864974605,5.7629802050654,35.0218143334999));
#191718=CARTESIAN_POINT('Ctrl Pts',(3.40110483761835,5.85269802527818,35.0298954628148));
#191719=CARTESIAN_POINT('Ctrl Pts',(3.25169878737696,5.93702015617671,35.0379765921297));
#191720=CARTESIAN_POINT('Ctrl Pts',(3.09910619832134,6.0156321173694,35.0460577214446));
#191721=CARTESIAN_POINT('Ctrl Pts',(3.09910619832137,6.01563211736938,33.0454119479742));
#191722=CARTESIAN_POINT('Ctrl Pts',(2.94681999133791,6.09408623802922,33.0534810764109));
#191723=CARTESIAN_POINT('Ctrl Pts',(2.79175421223906,6.16665004262685,33.0615502048476));
#191724=CARTESIAN_POINT('Ctrl Pts',(2.63442150037846,6.23314626479627,33.0696193332843));
#191725=CARTESIAN_POINT('Ctrl Pts',(2.50118950502637,6.28945638783577,33.0764524074089));
#191726=CARTESIAN_POINT('Ctrl Pts',(2.36633229850053,6.34141627804308,33.0832854815335));
#191727=CARTESIAN_POINT('Ctrl Pts',(2.23016766295296,6.38894679858261,33.0901185556582));
#191728=CARTESIAN_POINT('Ctrl Pts',(2.06411512600675,6.44691018596453,33.0984514777049));
#191729=CARTESIAN_POINT('Ctrl Pts',(1.89558818275161,6.49847023352894,33.1067843997516));
#191730=CARTESIAN_POINT('Ctrl Pts',(1.72511532004303,6.54341395087861,33.1151173217983));
#191731=CARTESIAN_POINT('Ctrl Pts',(1.55484391491809,6.58830455565333,33.1234403963519));
#191732=CARTESIAN_POINT('Ctrl Pts',(1.38263150491179,6.62659431812345,33.1317634709055));
#191733=CARTESIAN_POINT('Ctrl Pts',(1.20902467572304,6.65811897862248,33.1400865454592));
#191734=CARTESIAN_POINT('Ctrl Pts',(1.03559114117627,6.68961217115,33.1484013119051));
#191735=CARTESIAN_POINT('Ctrl Pts',(0.860766300803221,6.71435365394648,
33.1567160783511));
#191736=CARTESIAN_POINT('Ctrl Pts',(0.685110183186748,6.73222942544993,
33.1650308447971));
#191737=CARTESIAN_POINT('Ctrl Pts',(0.509597184570617,6.75009063234507,
33.1733388366366));
#191738=CARTESIAN_POINT('Ctrl Pts',(0.333254602950186,6.76109723930545,
33.1816468284761));
#191739=CARTESIAN_POINT('Ctrl Pts',(0.156651128898255,6.76518657716215,
33.1899548203157));
#191740=CARTESIAN_POINT('Ctrl Pts',(-0.0198408316317251,6.76927333286994,
33.1982575662028));
#191741=CARTESIAN_POINT('Ctrl Pts',(-0.196593009420326,6.76645151595209,
33.2065603120898));
#191742=CARTESIAN_POINT('Ctrl Pts',(-0.373032913541262,6.75671040118007,
33.2148630579769));
#191743=CARTESIAN_POINT('Ctrl Pts',(-0.549400712296347,6.74697326729122,
33.2231624107964));
#191744=CARTESIAN_POINT('Ctrl Pts',(-0.725456144818687,6.73032248909197,
33.2314617636158));
#191745=CARTESIAN_POINT('Ctrl Pts',(-0.900627749657548,6.70679943464443,
33.2397611164352));
#191746=CARTESIAN_POINT('Ctrl Pts',(-1.07576209843538,6.68328138315585,
33.2480587041216));
#191747=CARTESIAN_POINT('Ctrl Pts',(-1.2500126494086,6.6528940135678,33.2563562918079));
#191748=CARTESIAN_POINT('Ctrl Pts',(-1.42281383919723,6.61573047962119,
33.2646538794943));
#191749=CARTESIAN_POINT('Ctrl Pts',(-1.59560699235385,6.57856867407499,
33.2729510812767));
#191750=CARTESIAN_POINT('Ctrl Pts',(-1.76695057857995,6.5346314054757,33.2812482830591));
#191751=CARTESIAN_POINT('Ctrl Pts',(-1.9362898001284,6.48406283204587,33.2895454848415));
#191752=CARTESIAN_POINT('Ctrl Pts',(-2.1056492847869,6.43348820758688,33.2978436794661));
#191753=CARTESIAN_POINT('Ctrl Pts',(-2.27300359369002,6.37628079726977,
33.3061418740906));
#191754=CARTESIAN_POINT('Ctrl Pts',(-2.43781346375676,6.31263451467977,
33.3144400687152));
#191755=CARTESIAN_POINT('Ctrl Pts',(-2.60273924652664,6.24894346891717,
33.3227440995567));
#191756=CARTESIAN_POINT('Ctrl Pts',(-2.76511668967857,6.17880462746615,
33.3310481303983));
#191757=CARTESIAN_POINT('Ctrl Pts',(-2.92442604456808,6.10246026696216,
33.3393521612399));
#191758=CARTESIAN_POINT('Ctrl Pts',(-3.08379332872378,6.02608814554743,
33.3476592116556));
#191759=CARTESIAN_POINT('Ctrl Pts',(-3.24008999050089,5.94350616458784,
33.3559662620714));
#191760=CARTESIAN_POINT('Ctrl Pts',(-3.39282105141429,5.85500250325139,
33.3642733124871));
#191761=CARTESIAN_POINT('Ctrl Pts',(-3.54571540760837,5.76640421656413,
33.3725892445417));
#191762=CARTESIAN_POINT('Ctrl Pts',(-3.69503624859151,5.67187178046481,
33.3809051765964));
#191763=CARTESIAN_POINT('Ctrl Pts',(-3.84031681796374,5.57173722798059,
33.389221108651));
#191764=CARTESIAN_POINT('Ctrl Pts',(-3.94983239701644,5.49625367539074,
33.3954898348699));
#191765=CARTESIAN_POINT('Ctrl Pts',(-4.05705269361544,5.41758764516095,
33.4017585610888));
#191766=CARTESIAN_POINT('Ctrl Pts',(-4.16179038218382,5.33589634595372,
33.4080272873078));
#191767=CARTESIAN_POINT('Ctrl Pts',(-4.30297721710928,5.22577613866572,
33.4164775560311));
#191768=CARTESIAN_POINT('Ctrl Pts',(-4.43991059809946,5.10995537588841,
33.4249278247545));
#191769=CARTESIAN_POINT('Ctrl Pts',(-4.57212051848605,4.98878772493267,
33.4333780934778));
#191770=CARTESIAN_POINT('Ctrl Pts',(-4.70421375913251,4.86772700853966,
33.4418209045523));
#191771=CARTESIAN_POINT('Ctrl Pts',(-4.83159160466415,4.74132903239765,
33.4502637156268));
#191772=CARTESIAN_POINT('Ctrl Pts',(-4.95381666139334,4.60998801357463,
33.4587065267013));
#191773=CARTESIAN_POINT('Ctrl Pts',(-5.07595049161931,4.47874502523895,
33.4671430362191));
#191774=CARTESIAN_POINT('Ctrl Pts',(-5.19293897456915,4.34256659076512,
33.4755795457368));
#191775=CARTESIAN_POINT('Ctrl Pts',(-5.30438089851626,4.20188437292792,
33.4840160552546));
#191776=CARTESIAN_POINT('Ctrl Pts',(-5.41574307976984,4.06130282078801,
33.4924465279958));
#191777=CARTESIAN_POINT('Ctrl Pts',(-5.52156641316081,3.9162241727613,33.500877000737));
#191778=CARTESIAN_POINT('Ctrl Pts',(-5.62148924746264,3.76711396703922,
33.5093074734782));
#191779=CARTESIAN_POINT('Ctrl Pts',(-5.7213691252086,3.61806786339078,33.517734321982));
#191780=CARTESIAN_POINT('Ctrl Pts',(-5.81535337643285,3.46499393209991,
33.5261611704858));
#191781=CARTESIAN_POINT('Ctrl Pts',(-5.90312267419187,3.30838808083965,
33.5345880189896));
#191782=CARTESIAN_POINT('Ctrl Pts',(-5.99086488070321,3.15183056821275,
33.5430122664263));
#191783=CARTESIAN_POINT('Ctrl Pts',(-6.07239579744064,2.99174359860373,
33.5514365138629));
#191784=CARTESIAN_POINT('Ctrl Pts',(-6.14744102587402,2.82864947163853,
33.5598607612995));
#191785=CARTESIAN_POINT('Ctrl Pts',(-6.16858589997194,2.78269578673703,
33.5622343919105));
#191786=CARTESIAN_POINT('Ctrl Pts',(-6.18921615777526,2.73650351364091,
33.5646080225215));
#191787=CARTESIAN_POINT('Ctrl Pts',(-6.20932632878607,2.69008467202133,
33.5669816531325));
#191788=CARTESIAN_POINT('Ctrl Pts',(-6.28108308539527,2.52445378214046,
33.5754511999076));
#191789=CARTESIAN_POINT('Ctrl Pts',(-6.34619125863235,2.35599024723317,
33.5839207466827));
#191790=CARTESIAN_POINT('Ctrl Pts',(-6.40444782480402,2.18525446100975,
33.5923902934579));
#191791=CARTESIAN_POINT('Ctrl Pts',(-6.46451278498047,2.0092187130396,33.6011227509848));
#191792=CARTESIAN_POINT('Ctrl Pts',(-6.51729378950696,1.83076772316103,
33.6098552085118));
#191793=CARTESIAN_POINT('Ctrl Pts',(-6.56262398702231,1.65053185517863,
33.6185876660388));
#191794=CARTESIAN_POINT('Ctrl Pts',(-6.60664942458908,1.47548379917879,
33.6270687732196));
#191795=CARTESIAN_POINT('Ctrl Pts',(-6.64364700528507,1.298752522188,33.6355498804005));
#191796=CARTESIAN_POINT('Ctrl Pts',(-6.67351596073093,1.12092538639715,
33.6440309875814));
#191797=CARTESIAN_POINT('Ctrl Pts',(-6.70471273319322,0.935192989328691,
33.6528891202814));
#191798=CARTESIAN_POINT('Ctrl Pts',(-6.72813253998287,0.748265475079885,
33.6617472529814));
#191799=CARTESIAN_POINT('Ctrl Pts',(-6.74372097542174,0.560817622455764,
33.6706053856814));
#191800=CARTESIAN_POINT('Ctrl Pts',(-6.7593094108606,0.373369769831643,
33.6794635183815));
#191801=CARTESIAN_POINT('Ctrl Pts',(-6.76706649355167,0.185401981686163,
33.6883216510815));
#191802=CARTESIAN_POINT('Ctrl Pts',(-6.76699957039783,-0.00241127259631757,
33.6971797837815));
#191803=CARTESIAN_POINT('',(-6.76699870538252,-0.00418585132867157,33.3028202162336));
#191804=CARTESIAN_POINT('Ctrl Pts',(3.09910619832134,6.0156321173694,32.6513224177368));
#191805=CARTESIAN_POINT('Ctrl Pts',(2.93976909702956,6.09771868592969,32.659746362849));
#191806=CARTESIAN_POINT('Ctrl Pts',(2.77718943464024,6.1734601017708,32.6681703079613));
#191807=CARTESIAN_POINT('Ctrl Pts',(2.61190384602355,6.24261542137007,32.6765942530736));
#191808=CARTESIAN_POINT('Ctrl Pts',(2.44657075146376,6.31179061740688,32.6850206193737));
#191809=CARTESIAN_POINT('Ctrl Pts',(2.27853048772618,6.37437581447125,32.6934469856739));
#191810=CARTESIAN_POINT('Ctrl Pts',(2.10833867007918,6.43017861744514,32.701873351974));
#191811=CARTESIAN_POINT('Ctrl Pts',(1.93799498176463,6.48603121604997,32.710307237542));
#191812=CARTESIAN_POINT('Ctrl Pts',(1.76549622016069,6.53508922196037,32.71874112311));
#191813=CARTESIAN_POINT('Ctrl Pts',(1.5914132705117,6.57721010782226,32.7271750086781));
#191814=CARTESIAN_POINT('Ctrl Pts',(1.41725032812322,6.61935034862417,32.7356127696952));
#191815=CARTESIAN_POINT('Ctrl Pts',(1.2415020718237,6.65454704126416,32.7440505307124));
#191816=CARTESIAN_POINT('Ctrl Pts',(1.06474905880451,6.68270891493674,32.7524882917295));
#191817=CARTESIAN_POINT('Ctrl Pts',(0.887791059201659,6.71090344890842,
32.76093583831));
#191818=CARTESIAN_POINT('Ctrl Pts',(0.709826304952664,6.73204681432255,
32.7693833848905));
#191819=CARTESIAN_POINT('Ctrl Pts',(0.531441288722675,6.74609955134378,
32.777830931471));
#191820=CARTESIAN_POINT('Ctrl Pts',(0.397348744821141,6.75666303529429,
32.7841809772015));
#191821=CARTESIAN_POINT('Ctrl Pts',(0.263018840592247,6.76322098232725,
32.7905310229321));
#191822=CARTESIAN_POINT('Ctrl Pts',(0.128700420179844,6.76577602362401,
32.7968810686626));
#191823=CARTESIAN_POINT('Ctrl Pts',(-0.0455850810752542,6.76909132953489,
32.8051206005134));
#191824=CARTESIAN_POINT('Ctrl Pts',(-0.220240240340706,6.76567256978095,
32.8133601323642));
#191825=CARTESIAN_POINT('Ctrl Pts',(-0.394705640901005,6.75547899538152,
32.8215996642151));
#191826=CARTESIAN_POINT('Ctrl Pts',(-0.568977397060637,6.74529673513721,
32.8298300507614));
#191827=CARTESIAN_POINT('Ctrl Pts',(-0.743059461722417,6.72835465355148,
32.8380604373078));
#191828=CARTESIAN_POINT('Ctrl Pts',(-0.916389947831463,6.70466393367434,
32.8462908238541));
#191829=CARTESIAN_POINT('Ctrl Pts',(-1.08955896978082,6.6809952826338,32.854513543472));
#191830=CARTESIAN_POINT('Ctrl Pts',(-1.26197745693309,6.65059056112991,
32.8627362630898));
#191831=CARTESIAN_POINT('Ctrl Pts',(-1.43308608571328,6.61351292967172,
32.8709589827077));
#191832=CARTESIAN_POINT('Ctrl Pts',(-1.60404309991955,6.57646815166654,
32.8791744164035));
#191833=CARTESIAN_POINT('Ctrl Pts',(-1.77369222248841,6.53276232331814,
32.8873898500992));
#191834=CARTESIAN_POINT('Ctrl Pts',(-1.94148192728308,6.48251007913086,
32.895605283795));
#191835=CARTESIAN_POINT('Ctrl Pts',(-2.10918540119871,6.4322836606949,32.9038164953959));
#191836=CARTESIAN_POINT('Ctrl Pts',(-2.27503102038421,6.37551762868008,
32.9120277069967));
#191837=CARTESIAN_POINT('Ctrl Pts',(-2.43847967629493,6.31237719629432,
32.9202389185975));
#191838=CARTESIAN_POINT('Ctrl Pts',(-2.60187352054539,6.24925793772556,
32.928447376611));
#191839=CARTESIAN_POINT('Ctrl Pts',(-2.76287167113866,6.17976866522749,
32.9366558346245));
#191840=CARTESIAN_POINT('Ctrl Pts',(-2.92095226736622,6.10412375790073,
32.9448642926381));
#191841=CARTESIAN_POINT('Ctrl Pts',(-2.99138062479868,6.07042229992112,
32.9485213399212));
#191842=CARTESIAN_POINT('Ctrl Pts',(-3.0612301299238,6.03549965571144,32.9521783872043));
#191843=CARTESIAN_POINT('Ctrl Pts',(-3.13045596805582,5.99937783708142,
32.9558354344874));
#191844=CARTESIAN_POINT('Ctrl Pts',(-3.2981532351189,5.91187394505123,32.9646945086632));
#191845=CARTESIAN_POINT('Ctrl Pts',(-3.46201476408152,5.81742093791027,
32.9735535828391));
#191846=CARTESIAN_POINT('Ctrl Pts',(-3.62149832520691,5.71638337417318,
32.982412657015));
#191847=CARTESIAN_POINT('Ctrl Pts',(-3.78128152385848,5.61515598118074,
32.9912883756089));
#191848=CARTESIAN_POINT('Ctrl Pts',(-3.93667009785948,5.50731944748327,
33.0001640942028));
#191849=CARTESIAN_POINT('Ctrl Pts',(-4.08715270607949,5.39328024092825,
33.0090398127968));
#191850=CARTESIAN_POINT('Ctrl Pts',(-4.23806474914441,5.27891559869957,
33.0179408601838));
#191851=CARTESIAN_POINT('Ctrl Pts',(-4.38404260209493,5.15831301966201,
33.0268419075708));
#191852=CARTESIAN_POINT('Ctrl Pts',(-4.52460747369214,5.03191973395933,
33.0357429549577));
#191853=CARTESIAN_POINT('Ctrl Pts',(-4.6653634451595,4.90535461485181,33.0446561034407));
#191854=CARTESIAN_POINT('Ctrl Pts',(-4.80069154679471,4.77298324132962,
33.0535692519236));
#191855=CARTESIAN_POINT('Ctrl Pts',(-4.93015059524625,4.63528899942529,
33.0624824004066));
#191856=CARTESIAN_POINT('Ctrl Pts',(-5.05989707818596,4.4972890386514,33.0714153385164));
#191857=CARTESIAN_POINT('Ctrl Pts',(-5.18374826544594,4.35394276052935,
33.0803482766263));
#191858=CARTESIAN_POINT('Ctrl Pts',(-5.30130209679829,4.20576807235992,
33.0892812147362));
#191859=CARTESIAN_POINT('Ctrl Pts',(-5.4131962996516,4.06472725365568,33.0977840765948));
#191860=CARTESIAN_POINT('Ctrl Pts',(-5.51938513319482,3.91931215430751,
33.1062869384535));
#191861=CARTESIAN_POINT('Ctrl Pts',(-5.61955890029082,3.7699929398027,33.1147898003121));
#191862=CARTESIAN_POINT('Ctrl Pts',(-5.71636857825428,3.62568824318374,
33.1230071145069));
#191863=CARTESIAN_POINT('Ctrl Pts',(-5.80775482896632,3.47744567269272,
33.1312244287017));
#191864=CARTESIAN_POINT('Ctrl Pts',(-5.89338115962983,3.32571007565604,
33.1394417428965));
#191865=CARTESIAN_POINT('Ctrl Pts',(-5.97891380324206,3.17414049835361,
33.1476500662127));
#191866=CARTESIAN_POINT('Ctrl Pts',(-6.05869889872921,3.01908581222887,
33.155858389529));
#191867=CARTESIAN_POINT('Ctrl Pts',(-6.13244214595523,2.86102120343629,
33.1640667128453));
#191868=CARTESIAN_POINT('Ctrl Pts',(-6.20611811168363,2.70310080884637,
33.1722675470923));
#191869=CARTESIAN_POINT('Ctrl Pts',(-6.2737630546176,2.54217628233276,33.1804683813393));
#191870=CARTESIAN_POINT('Ctrl Pts',(-6.33512766578461,2.37874892710653,
33.1886692155863));
#191871=CARTESIAN_POINT('Ctrl Pts',(-6.39644744104012,2.21544097970014,
33.1968640579127));
#191872=CARTESIAN_POINT('Ctrl Pts',(-6.45149589761738,2.04963417970298,
33.2050589002391));
#191873=CARTESIAN_POINT('Ctrl Pts',(-6.50007108122949,1.88185146570183,
33.2132537425655));
#191874=CARTESIAN_POINT('Ctrl Pts',(-6.54861871409412,1.71416391426809,
33.2214439369624));
#191875=CARTESIAN_POINT('Ctrl Pts',(-6.59070028934588,1.54450302516549,
33.2296341313592));
#191876=CARTESIAN_POINT('Ctrl Pts',(-6.6261631197505,1.37340864656457,33.237824325756));
#191877=CARTESIAN_POINT('Ctrl Pts',(-6.66161398315837,1.20237200407354,
33.2460117563569));
#191878=CARTESIAN_POINT('Ctrl Pts',(-6.690450478747,1.02990318643661,33.2541991869577));
#191879=CARTESIAN_POINT('Ctrl Pts',(-6.7125705924874,0.856554166923097,
33.2623866175585));
#191880=CARTESIAN_POINT('Ctrl Pts',(-6.73469010246755,0.683209878906435,
33.2705738246865));
#191881=CARTESIAN_POINT('Ctrl Pts',(-6.75009354462253,0.508985791705292,
33.2787610318144));
#191882=CARTESIAN_POINT('Ctrl Pts',(-6.75873050626867,0.334441240927599,
33.2869482389424));
#191883=CARTESIAN_POINT('Ctrl Pts',(-6.76431180143616,0.221648722252779,
33.2922388980249));
#191884=CARTESIAN_POINT('Ctrl Pts',(-6.76706854691273,0.108722518485693,
33.2975295571074));
#191885=CARTESIAN_POINT('Ctrl Pts',(-6.7669987053831,-0.00418585039646904,
33.3028202161899));
#191886=CARTESIAN_POINT('Ctrl Pts',(-6.76699870538252,-0.00418585132862214,
33.3028202162336));
#191887=CARTESIAN_POINT('Ctrl Pts',(-6.76687598560987,-0.202579075886211,
33.3121165237244));
#191888=CARTESIAN_POINT('Ctrl Pts',(-6.75802467330528,-0.400624589624038,
33.3214128312153));
#191889=CARTESIAN_POINT('Ctrl Pts',(-6.74056009748527,-0.597610719607133,
33.3307091387062));
#191890=CARTESIAN_POINT('Ctrl Pts',(-6.72296064155559,-0.796118186901281,
33.3400772422135));
#191891=CARTESIAN_POINT('Ctrl Pts',(-6.69661444238275,-0.993549688353143,
33.3494453457209));
#191892=CARTESIAN_POINT('Ctrl Pts',(-6.66168924145868,-1.18919529524538,
33.3588134492283));
#191893=CARTESIAN_POINT('Ctrl Pts',(-6.62663418857151,-1.38556831287409,
33.3682163833622));
#191894=CARTESIAN_POINT('Ctrl Pts',(-6.58293632376023,-1.58014199450794,
33.3776193174961));
#191895=CARTESIAN_POINT('Ctrl Pts',(-6.53081377367392,-1.77221907607129,
33.38702225163));
#191896=CARTESIAN_POINT('Ctrl Pts',(-6.47844794047052,-1.96519268152013,
33.3964690741601));
#191897=CARTESIAN_POINT('Ctrl Pts',(-6.41757868048744,-2.15564619035235,
33.4059158966902));
#191898=CARTESIAN_POINT('Ctrl Pts',(-6.34847464685296,-2.3428953579418,
33.4153627192203));
#191899=CARTESIAN_POINT('Ctrl Pts',(-6.30620383452604,-2.45743533491929,
33.4211413234674));
#191900=CARTESIAN_POINT('Ctrl Pts',(-6.26085269822801,-2.57077678281479,
33.4269199277145));
#191901=CARTESIAN_POINT('Ctrl Pts',(-6.21249120912136,-2.68276759645517,
33.4326985319617));
#191902=CARTESIAN_POINT('Ctrl Pts',(-6.14495867126726,-2.83915285259983,
33.4407678411842));
#191903=CARTESIAN_POINT('Ctrl Pts',(-6.07139345292414,-2.99327311130894,
33.4488371504067));
#191904=CARTESIAN_POINT('Ctrl Pts',(-5.99196749816581,-3.1446167494505,
33.4569064596292));
#191905=CARTESIAN_POINT('Ctrl Pts',(-5.91264060916037,-3.29577162094135,
33.46496570423));
#191906=CARTESIAN_POINT('Ctrl Pts',(-5.8274676997558,-3.4441564364899,33.4730249488308));
#191907=CARTESIAN_POINT('Ctrl Pts',(-5.73666957447558,-3.58927725221752,
33.4810841934315));
#191908=CARTESIAN_POINT('Ctrl Pts',(-5.64596477363654,-3.7342489093696,
33.4891351545518));
#191909=CARTESIAN_POINT('Ctrl Pts',(-5.54964645891247,-3.87596292919723,
33.497186115672));
#191910=CARTESIAN_POINT('Ctrl Pts',(-5.44798231712482,-4.01394789107872,
33.5052370767923));
#191911=CARTESIAN_POINT('Ctrl Pts',(-5.34640039149385,-4.15182126402584,
33.5132815270714));
#191912=CARTESIAN_POINT('Ctrl Pts',(-5.23948146358352,-4.28597128239312,
33.5213259773505));
#191913=CARTESIAN_POINT('Ctrl Pts',(-5.12753763633549,-4.41595366687232,
33.5293704276296));
#191914=CARTESIAN_POINT('Ctrl Pts',(-5.01565983500512,-4.54585938605942,
33.5374101331878));
#191915=CARTESIAN_POINT('Ctrl Pts',(-4.89876327716363,-4.67160208273011,
33.5454498387461));
#191916=CARTESIAN_POINT('Ctrl Pts',(-4.77720155368238,-4.79276896120548,
33.5534895443043));
#191917=CARTESIAN_POINT('Ctrl Pts',(-4.65301598539016,-4.91655116197347,
33.5617027826087));
#191918=CARTESIAN_POINT('Ctrl Pts',(-4.52396180850659,-5.03555744474693,
33.5699160209132));
#191919=CARTESIAN_POINT('Ctrl Pts',(-4.39045754893377,-5.14938554693766,
33.5781292592176));
#191920=CARTESIAN_POINT('Ctrl Pts',(-4.25981609088834,-5.26077277371472,
33.5861663767658));
#191921=CARTESIAN_POINT('Ctrl Pts',(-4.12491377015921,-5.36720140300616,
33.594203494314));
#191922=CARTESIAN_POINT('Ctrl Pts',(-3.98617765391193,-5.46833399779615,
33.6022406118622));
#191923=CARTESIAN_POINT('Ctrl Pts',(-3.84742686026559,-5.56947729177169,
33.6102785796863));
#191924=CARTESIAN_POINT('Ctrl Pts',(-3.70484176537793,-5.6653232154408,
33.6183165475104));
#191925=CARTESIAN_POINT('Ctrl Pts',(-3.55887967978884,-5.7555768107798,
33.6263545153345));
#191926=CARTESIAN_POINT('Ctrl Pts',(-3.41287323186925,-5.84585783693967,
33.6343949261422));
#191927=CARTESIAN_POINT('Ctrl Pts',(-3.26348806786615,-5.93054295519892,
33.6424353369499));
#191928=CARTESIAN_POINT('Ctrl Pts',(-3.11120728679728,-6.00938251558174,
33.6504757477577));
#191929=CARTESIAN_POINT('Ctrl Pts',(-2.95317115107825,-6.0912017666864,
33.6588200407455));
#191930=CARTESIAN_POINT('Ctrl Pts',(-2.79201664149837,-6.16672476394506,
33.6671643337333));
#191931=CARTESIAN_POINT('Ctrl Pts',(-2.62830678136401,-6.23572709978844,
33.6755086267211));
#191932=CARTESIAN_POINT('Ctrl Pts',(-2.47028031779755,-6.30233393154681,
33.6835632369366));
#191933=CARTESIAN_POINT('Ctrl Pts',(-2.3098733223086,-6.36286519375461,
33.6916178471521));
#191934=CARTESIAN_POINT('Ctrl Pts',(-2.1476074221366,-6.41717004296939,
33.6996724573677));
#191935=CARTESIAN_POINT('Ctrl Pts',(-1.98521868438587,-6.47151600172218,
33.7077331650369));
#191936=CARTESIAN_POINT('Ctrl Pts',(-1.82096859603854,-6.5196260581066,
33.7157938727062));
#191937=CARTESIAN_POINT('Ctrl Pts',(-1.65538939645397,-6.5614003799576,
33.7238545803754));
#191938=CARTESIAN_POINT('Ctrl Pts',(-1.48957674011847,-6.60323360109956,
33.7319266531596));
#191939=CARTESIAN_POINT('Ctrl Pts',(-1.32243159560379,-6.63871318802318,
33.7399987259437));
#191940=CARTESIAN_POINT('Ctrl Pts',(-1.15449232025342,-6.66779097471388,
33.7480707987278));
#191941=CARTESIAN_POINT('Ctrl Pts',(-1.13690195712319,-6.67083665194362,
33.7489162870223));
#191942=CARTESIAN_POINT('Ctrl Pts',(-1.11930288207885,-6.67381214233745,
33.7497617753167));
#191943=CARTESIAN_POINT('Ctrl Pts',(-1.10169571360772,-6.67671742360109,
33.7506072636112));
#191944=CARTESIAN_POINT('Ctrl Pts',(-0.928163846523169,-6.70535115212547,
33.7589401856579));
#191945=CARTESIAN_POINT('Ctrl Pts',(-0.753292129788909,-6.72725210630963,
33.7672731077046));
#191946=CARTESIAN_POINT('Ctrl Pts',(-0.577637743217702,-6.74230106399962,
33.7756060297513));
#191947=CARTESIAN_POINT('Ctrl Pts',(-0.402190937534932,-6.75733223747101,
33.7839291043049));
#191948=CARTESIAN_POINT('Ctrl Pts',(-0.225963648258534,-6.76552751565066,
33.7922521788585));
#191949=CARTESIAN_POINT('Ctrl Pts',(-0.0495225306741007,-6.76681878868909,
33.8005752534121));
#191950=CARTESIAN_POINT('Ctrl Pts',(0.126742463076882,-6.7681087727765,
33.8088900198581));
#191951=CARTESIAN_POINT('Ctrl Pts',(0.303220514111993,-6.76250847945381,
33.817204786304));
#191952=CARTESIAN_POINT('Ctrl Pts',(0.479340340565712,-6.7500016176225,
33.82551955275));
#191953=CARTESIAN_POINT('Ctrl Pts',(0.655316670203667,-6.7375049459832,
33.8338275445895));
#191954=CARTESIAN_POINT('Ctrl Pts',(0.830935011259,-6.71811294314075,33.8421355364291));
#191955=CARTESIAN_POINT('Ctrl Pts',(1.00562434957782,-6.69186137539745,
33.8504435282686));
#191956=CARTESIAN_POINT('Ctrl Pts',(1.18020338302623,-6.66562638379901,
33.8587462741557));
#191957=CARTESIAN_POINT('Ctrl Pts',(1.35385423965773,-6.63254051075785,
33.8670490200428));
#191958=CARTESIAN_POINT('Ctrl Pts',(1.52601106752696,-6.59269134889426,
33.8753517659298));
#191959=CARTESIAN_POINT('Ctrl Pts',(1.69809754038708,-6.55285847211318,
33.8836511187493));
#191960=CARTESIAN_POINT('Ctrl Pts',(1.86869086264453,-6.5062678922022,33.8919504715687));
#191961=CARTESIAN_POINT('Ctrl Pts',(2.03723512847489,-6.45305834711789,
33.9002498243881));
#191962=CARTESIAN_POINT('Ctrl Pts',(2.20574354776793,-6.39986011881102,
33.9085474120745));
#191963=CARTESIAN_POINT('Ctrl Pts',(2.37220344727305,-6.34004583454991,
33.9168449997608));
#191964=CARTESIAN_POINT('Ctrl Pts',(2.53607361104077,-6.273804239804,33.9251425874472));
#191965=CARTESIAN_POINT('Ctrl Pts',(2.6999361535403,-6.20756572582001,33.9334397892296));
#191966=CARTESIAN_POINT('Ctrl Pts',(2.86120887784884,-6.13490062754828,
33.941736991012));
#191967=CARTESIAN_POINT('Ctrl Pts',(3.01936991942733,-6.0560460937527,33.9500341927944));
#191968=CARTESIAN_POINT('Ctrl Pts',(3.17754988653657,-5.97718212423333,
33.958332387419));
#191969=CARTESIAN_POINT('Ctrl Pts',(3.33261711791284,-5.89212739916181,
33.9666305820435));
#191970=CARTESIAN_POINT('Ctrl Pts',(3.48407358466363,-5.80116542227931,
33.9749287766681));
#191971=CARTESIAN_POINT('Ctrl Pts',(3.63563657251316,-5.71013947077805,
33.9832328075096));
#191972=CARTESIAN_POINT('Ctrl Pts',(3.78358342271712,-5.61319814502181,
33.9915368383512));
#191973=CARTESIAN_POINT('Ctrl Pts',(3.92744362413891,-5.51066924966566,
33.9998408691928));
#191974=CARTESIAN_POINT('Ctrl Pts',(4.07135613708945,-5.40810307198121,
34.0081479196085));
#191975=CARTESIAN_POINT('Ctrl Pts',(4.2111787604503,-5.29994548298093,34.0164549700243));
#191976=CARTESIAN_POINT('Ctrl Pts',(4.34647325685333,-5.1865652630097,34.02476202044));
#191977=CARTESIAN_POINT('Ctrl Pts',(4.48191240590684,-5.07306382044798,
34.0330779524946));
#191978=CARTESIAN_POINT('Ctrl Pts',(4.61281349292275,-4.9543288195222,34.0413938845493));
#191979=CARTESIAN_POINT('Ctrl Pts',(4.73877360384359,-4.83076740606658,
34.0497098166039));
#191980=CARTESIAN_POINT('Ctrl Pts',(4.83372501093598,-4.73762418807348,
34.0559785428228));
#191981=CARTESIAN_POINT('Ctrl Pts',(4.92586945993759,-4.64173916925834,
34.0622472690418));
#191982=CARTESIAN_POINT('Ctrl Pts',(5.01504935426716,-4.54329934896046,
34.0685159952607));
#191983=CARTESIAN_POINT('Ctrl Pts',(5.13526421857672,-4.41060206636408,
34.0769662639841));
#191984=CARTESIAN_POINT('Ctrl Pts',(5.25031120312685,-4.27301794204137,
34.0854165327074));
#191985=CARTESIAN_POINT('Ctrl Pts',(5.35978790112841,-4.1309759930212,34.0938668014307));
#191986=CARTESIAN_POINT('Ctrl Pts',(5.46916798222985,-3.98905940084,34.1023096125053));
#191987=CARTESIAN_POINT('Ctrl Pts',(5.57298737371688,-3.84269308690014,
34.1107524235798));
#191988=CARTESIAN_POINT('Ctrl Pts',(5.67088275146282,-3.69234042568687,
34.1191952346543));
#191989=CARTESIAN_POINT('Ctrl Pts',(5.76870506192389,-3.54209998489687,
34.127631744172));
#191990=CARTESIAN_POINT('Ctrl Pts',(5.86061199246948,-3.38787940495988,
34.1360682536897));
#191991=CARTESIAN_POINT('Ctrl Pts',(5.94628228554423,-3.23017274779894,
34.1445047632075));
#191992=CARTESIAN_POINT('Ctrl Pts',(6.03189127691449,-3.07257893823715,
34.1529352359487));
#191993=CARTESIAN_POINT('Ctrl Pts',(6.1112723743925,-2.91150431774581,34.1613657086899));
#191994=CARTESIAN_POINT('Ctrl Pts',(6.18414910334081,-2.74746953898474,
34.1697961814311));
#191995=CARTESIAN_POINT('Ctrl Pts',(6.25699450278089,-2.58350527833043,
34.1782230299349));
#191996=CARTESIAN_POINT('Ctrl Pts',(6.32334097365471,-2.41658369877348,
34.1866498784388));
#191997=CARTESIAN_POINT('Ctrl Pts',(6.38295894597132,-2.24724811581737,
34.1950767269426));
#191998=CARTESIAN_POINT('Ctrl Pts',(6.44255851634897,-2.07796480070834,
34.2035009743792));
#191999=CARTESIAN_POINT('Ctrl Pts',(6.49543361990836,-1.90626928053868,
34.2119252218159));
#192000=CARTESIAN_POINT('Ctrl Pts',(6.5414034748861,-1.73272316852638,34.2203494692525));
#192001=CARTESIAN_POINT('Ctrl Pts',(6.55435602118504,-1.683824514138,34.2227230998635));
#192002=CARTESIAN_POINT('Ctrl Pts',(6.56676066383916,-1.6347790406321,34.2250967304745));
#192003=CARTESIAN_POINT('Ctrl Pts',(6.57861407424934,-1.58559952765146,
34.2274703610854));
#192004=CARTESIAN_POINT('Ctrl Pts',(6.62165444759655,-1.40702606006075,
34.2360891420226));
#192005=CARTESIAN_POINT('Ctrl Pts',(6.65740394947293,-1.22676431481958,
34.2447079229599));
#192006=CARTESIAN_POINT('Ctrl Pts',(6.68575961015859,-1.04542213252451,
34.2533267038971));
#192007=CARTESIAN_POINT('Ctrl Pts',(6.71413230391721,-0.863971019083175,
34.2619506620836));
#192008=CARTESIAN_POINT('Ctrl Pts',(6.73510224573738,-0.681438473878653,
34.2705746202702));
#192009=CARTESIAN_POINT('Ctrl Pts',(6.74861822987197,-0.498438549311445,
34.2791985784567));
#192010=CARTESIAN_POINT('Ctrl Pts',(6.76262250039721,-0.308827461859928,
34.2881340908278));
#192011=CARTESIAN_POINT('Ctrl Pts',(6.76862417928981,-0.118714956467937,
34.2970696031989));
#192012=CARTESIAN_POINT('Ctrl Pts',(6.76662525726767,0.071215361455789,
34.3060051155701));
#192013=CARTESIAN_POINT('Ctrl Pts',(6.76469242462695,0.254866106146177,
34.3146451974648));
#192014=CARTESIAN_POINT('Ctrl Pts',(6.75527962541511,0.438346215844395,
34.3232852793595));
#192015=CARTESIAN_POINT('Ctrl Pts',(6.7384416584577,0.621041879072454,34.3319253612542));
#192016=CARTESIAN_POINT('Ctrl Pts',(6.72074008013742,0.813107916473974,
34.3410085888635));
#192017=CARTESIAN_POINT('Ctrl Pts',(6.6948317137539,1.00430653618667,34.3500918164728));
#192018=CARTESIAN_POINT('Ctrl Pts',(6.66084140508571,1.1939349966794,34.3591750440822));
#192019=CARTESIAN_POINT('Ctrl Pts',(6.62685109641752,1.38356345717214,34.3682582716915));
#192020=CARTESIAN_POINT('Ctrl Pts',(6.58477896296765,1.57162138737109,34.3773414993009));
#192021=CARTESIAN_POINT('Ctrl Pts',(6.53481107523681,1.75742232003644,34.3864247269102));
#192022=CARTESIAN_POINT('Ctrl Pts',(6.48505571073819,1.9424330048736,34.39546932177));
#192023=CARTESIAN_POINT('Ctrl Pts',(6.42742651200367,2.12537693045655,34.4045139166298));
#192024=CARTESIAN_POINT('Ctrl Pts',(6.36211102908855,2.30560886829267,34.4135585114896));
#192025=CARTESIAN_POINT('Ctrl Pts',(6.29685548341016,2.48567541495596,34.42259480651));
#192026=CARTESIAN_POINT('Ctrl Pts',(6.2239278166343,2.66303471905864,34.4316311015303));
#192027=CARTESIAN_POINT('Ctrl Pts',(6.14356489363596,2.83705822951941,34.4406673965507));
#192028=CARTESIAN_POINT('Ctrl Pts',(6.06334417913174,3.0107737917319,34.4496877011384));
#192029=CARTESIAN_POINT('Ctrl Pts',(5.97571458140068,3.18116513204231,34.4587080057261));
#192030=CARTESIAN_POINT('Ctrl Pts',(5.88096029452438,3.34762527984059,34.4677283103138));
#192031=CARTESIAN_POINT('Ctrl Pts',(5.78632533226585,3.51387580341852,34.4767372555801));
#192032=CARTESIAN_POINT('Ctrl Pts',(5.68458370354612,3.67620480799962,34.4857462008464));
#192033=CARTESIAN_POINT('Ctrl Pts',(5.57606575828179,3.83402916777082,34.4947551461128));
#192034=CARTESIAN_POINT('Ctrl Pts',(5.46779423429805,3.99149514183217,34.5037436339716));
#192035=CARTESIAN_POINT('Ctrl Pts',(5.35277724324437,4.14447669357504,34.5127321218304));
#192036=CARTESIAN_POINT('Ctrl Pts',(5.23138843283429,4.29241937196351,34.5217206096892));
#192037=CARTESIAN_POINT('Ctrl Pts',(5.12488645837745,4.42221871097652,34.5296067707044));
#192038=CARTESIAN_POINT('Ctrl Pts',(5.01348039957638,4.54813957515049,34.5374929317197));
#192039=CARTESIAN_POINT('Ctrl Pts',(4.89745054546475,4.66982517389324,34.5453790927349));
#192040=CARTESIAN_POINT('Ctrl Pts',(4.77796699932706,4.79513281099226,34.5534999896431));
#192041=CARTESIAN_POINT('Ctrl Pts',(4.65363260093625,4.91589208310284,34.5616208865514));
#192042=CARTESIAN_POINT('Ctrl Pts',(4.5248381008275,5.03171234882319,34.5697417834596));
#192043=CARTESIAN_POINT('Ctrl Pts',(4.39603319210573,5.1475419746352,34.5778633366634));
#192044=CARTESIAN_POINT('Ctrl Pts',(4.26276772961882,5.25843154700934,34.5859848898673));
#192045=CARTESIAN_POINT('Ctrl Pts',(4.12546777413614,5.36402876992324,34.5941064430712));
#192046=CARTESIAN_POINT('Ctrl Pts',(3.98816086652181,5.46963133971283,34.6022284075069));
#192047=CARTESIAN_POINT('Ctrl Pts',(3.84681935301713,5.56994080785572,34.6103503719426));
#192048=CARTESIAN_POINT('Ctrl Pts',(3.70190033812664,5.66464675744021,34.6184723363782));
#192049=CARTESIAN_POINT('Ctrl Pts',(3.55690923914435,5.75939981466181,34.626598340756));
#192050=CARTESIAN_POINT('Ctrl Pts',(3.40833739558179,5.84854359293189,34.6347243451338));
#192051=CARTESIAN_POINT('Ctrl Pts',(3.25666900829462,5.93181219952329,34.6428503495116));
#192052=CARTESIAN_POINT('Ctrl Pts',(3.20450735387843,5.96044986330035,34.6456450375789));
#192053=CARTESIAN_POINT('Ctrl Pts',(3.15197964667623,5.98839301292847,34.6484397256462));
#192054=CARTESIAN_POINT('Ctrl Pts',(3.09910619832129,6.01563211736943,34.6512344137135));
#192055=CARTESIAN_POINT('Origin',(0.,0.,4.30282021618968));
#192056=CARTESIAN_POINT('',(3.09910619832131,6.01563211736941,37.0458284616795));
#192057=CARTESIAN_POINT('',(3.0991061983213,6.01563211736942,36.6515010185242));
#192058=CARTESIAN_POINT('',(3.09910619832133,6.0156321173694,4.30282021618968));
#192059=CARTESIAN_POINT('',(-6.76699950557411,0.00258680493565955,35.6971797838413));
#192060=CARTESIAN_POINT('Ctrl Pts',(-6.76699950557411,0.00258680493565955,
35.6971797838413));
#192061=CARTESIAN_POINT('Ctrl Pts',(-6.76706491533245,-0.168523044232433,
35.7052286768605));
#192062=CARTESIAN_POINT('Ctrl Pts',(-6.76063604028297,-0.339784646345535,
35.7132775698797));
#192063=CARTESIAN_POINT('Ctrl Pts',(-6.74770474594979,-0.510656108831311,
35.7213264628988));
#192064=CARTESIAN_POINT('Ctrl Pts',(-6.7347794102295,-0.681448835432342,
35.7293716470675));
#192065=CARTESIAN_POINT('Ctrl Pts',(-6.71535764621149,-0.851851407750275,
35.7374168312361));
#192066=CARTESIAN_POINT('Ctrl Pts',(-6.68948339477062,-1.02132311786633,
35.7454620154047));
#192067=CARTESIAN_POINT('Ctrl Pts',(-6.66361188957647,-1.19077684055841,
35.7535063456719));
#192068=CARTESIAN_POINT('Ctrl Pts',(-6.63128930707785,-1.35929952639152,
35.7615506759391));
#192069=CARTESIAN_POINT('Ctrl Pts',(-6.59261134108946,-1.52635667697255,
35.7695950062063));
#192070=CARTESIAN_POINT('Ctrl Pts',(-6.55615347216897,-1.6838248256322,
35.7771775956973));
#192071=CARTESIAN_POINT('Ctrl Pts',(-6.51404935939128,-1.83999064974016,
35.7847601851882));
#192072=CARTESIAN_POINT('Ctrl Pts',(-6.46642052635441,-1.99441584839831,
35.7923427746792));
#192073=CARTESIAN_POINT('Ctrl Pts',(-6.41228302112202,-2.16994387348973,
35.8009615556164));
#192074=CARTESIAN_POINT('Ctrl Pts',(-6.35101420069501,-2.34320222199084,
35.8095803365536));
#192075=CARTESIAN_POINT('Ctrl Pts',(-6.2828357778544,-2.51361564056893,
35.8181991174909));
#192076=CARTESIAN_POINT('Ctrl Pts',(-6.2146164006499,-2.68413142545095,
35.8268230756774));
#192077=CARTESIAN_POINT('Ctrl Pts',(-6.13947925076779,-2.85179858749008,
35.8354470338639));
#192078=CARTESIAN_POINT('Ctrl Pts',(-6.05769372457999,-3.01606295345178,
35.8440709920504));
#192079=CARTESIAN_POINT('Ctrl Pts',(-5.97295356638063,-3.18626163049089,
35.8530065044216));
#192080=CARTESIAN_POINT('Ctrl Pts',(-5.88107587592368,-3.35280674405556,
35.8619420167927));
#192081=CARTESIAN_POINT('Ctrl Pts',(-5.78241129609706,-3.51511146377596,
35.8708775291638));
#192082=CARTESIAN_POINT('Ctrl Pts',(-5.68700881503044,-3.67204998190839,
35.8795176110585));
#192083=CARTESIAN_POINT('Ctrl Pts',(-5.58526125217604,-3.82502378651878,
35.8881576929532));
#192084=CARTESIAN_POINT('Ctrl Pts',(-5.4775290364657,-3.97353301920031,
35.8967977748479));
#192085=CARTESIAN_POINT('Ctrl Pts',(-5.36427128635596,-4.12965922019907,
35.9058810024572));
#192086=CARTESIAN_POINT('Ctrl Pts',(-5.24439910264273,-4.28085054005772,
35.9149642300665));
#192087=CARTESIAN_POINT('Ctrl Pts',(-5.11837854143579,-4.42656640146397,
35.9240474576759));
#192088=CARTESIAN_POINT('Ctrl Pts',(-4.99235798022887,-4.57228226287019,
35.9331306852852));
#192089=CARTESIAN_POINT('Ctrl Pts',(-4.86018933197781,-4.71252240670671,
35.9422139128946));
#192090=CARTESIAN_POINT('Ctrl Pts',(-4.72238299435586,-4.84679150104671,
35.9512971405039));
#192091=CARTESIAN_POINT('Ctrl Pts',(-4.58516277413118,-4.98048952257928,
35.9603417353637));
#192092=CARTESIAN_POINT('Ctrl Pts',(-4.44222661118032,-5.1083912730571,
35.9693863302235));
#192093=CARTESIAN_POINT('Ctrl Pts',(-4.29406512608389,-5.23003763781392,
35.9784309250834));
#192094=CARTESIAN_POINT('Ctrl Pts',(-4.146039602472,-5.35157237288282,35.9874672201037));
#192095=CARTESIAN_POINT('Ctrl Pts',(-3.99279851377013,-5.46686303194261,
35.996503515124));
#192096=CARTESIAN_POINT('Ctrl Pts',(-3.83486637478639,-5.5754900132215,
36.0055398101443));
#192097=CARTESIAN_POINT('Ctrl Pts',(-3.67721370910681,-5.68392477053905,
36.014560114732));
#192098=CARTESIAN_POINT('Ctrl Pts',(-3.51488676529724,-5.78571926235838,
36.0235804193198));
#192099=CARTESIAN_POINT('Ctrl Pts',(-3.34843974226654,-5.88049660253367,
36.0326007239075));
#192100=CARTESIAN_POINT('Ctrl Pts',(-3.18220232692764,-5.97515458906028,
36.0416096691738));
#192101=CARTESIAN_POINT('Ctrl Pts',(-3.01185539281924,-6.06281294167381,
36.0506186144402));
#192102=CARTESIAN_POINT('Ctrl Pts',(-2.83798065817008,-6.14313883807395,
36.0596275597065));
#192103=CARTESIAN_POINT('Ctrl Pts',(-2.66450075623476,-6.22328233136801,
36.0686160475653));
#192104=CARTESIAN_POINT('Ctrl Pts',(-2.48750925974602,-6.29612650461054,
36.0776045354241));
#192105=CARTESIAN_POINT('Ctrl Pts',(-2.30761048321135,-6.36138529392561,
36.0865930232829));
#192106=CARTESIAN_POINT('Ctrl Pts',(-2.14977406617603,-6.4186409000168,
36.0944791842982));
#192107=CARTESIAN_POINT('Ctrl Pts',(-1.98970020554991,-6.47005814533542,
36.1023653453134));
#192108=CARTESIAN_POINT('Ctrl Pts',(-1.82781204343855,-6.51547328548441,
36.1102515063287));
#192109=CARTESIAN_POINT('Ctrl Pts',(-1.66109353278753,-6.56224350282395,
36.1183729711848));
#192110=CARTESIAN_POINT('Ctrl Pts',(-1.49252502542138,-6.60262558404109,
36.126494436041));
#192111=CARTESIAN_POINT('Ctrl Pts',(-1.32264204275989,-6.63648303145001,
36.1346159008972));
#192112=CARTESIAN_POINT('Ctrl Pts',(-1.15277117525538,-6.67033806432463,
36.1427367865734));
#192113=CARTESIAN_POINT('Ctrl Pts',(-0.981586378299208,-6.69766931863469,
36.1508576722496));
#192114=CARTESIAN_POINT('Ctrl Pts',(-0.809633717570386,-6.71839134342241,
36.1589785579257));
#192115=CARTESIAN_POINT('Ctrl Pts',(-0.637660503579715,-6.73911584508487,
36.1671004142801));
#192116=CARTESIAN_POINT('Ctrl Pts',(-0.464919606751438,-6.75322950155105,
36.1752222706344));
#192117=CARTESIAN_POINT('Ctrl Pts',(-0.29196252402161,-6.7606986979577,
36.1833441269888));
#192118=CARTESIAN_POINT('Ctrl Pts',(-0.118879253945957,-6.76817334379755,
36.1914719089489));
#192119=CARTESIAN_POINT('Ctrl Pts',(0.0544201508324774,-6.76899383155364,
36.1995996909091));
#192120=CARTESIAN_POINT('Ctrl Pts',(0.227383234888612,-6.76317868050901,
36.2077274728692));
#192121=CARTESIAN_POINT('Ctrl Pts',(0.400416777676826,-6.75736116058797,
36.2158585657857));
#192122=CARTESIAN_POINT('Ctrl Pts',(0.573113361673498,-6.74490264013385,
36.2239896587021));
#192123=CARTESIAN_POINT('Ctrl Pts',(0.744925594969273,-6.72587353865352,
36.2321207516186));
#192124=CARTESIAN_POINT('Ctrl Pts',(0.916925354137106,-6.70682366770422,
36.2402607192831));
#192125=CARTESIAN_POINT('Ctrl Pts',(1.08803847300764,-6.68118894601193,
36.2484006869477));
#192126=CARTESIAN_POINT('Ctrl Pts',(1.25772694295228,-6.64909106096254,
36.2565406546122));
#192127=CARTESIAN_POINT('Ctrl Pts',(1.34573472032298,-6.63244370995266,
36.2607623937926));
#192128=CARTESIAN_POINT('Ctrl Pts',(1.43335949671735,-6.61405865640257,
36.264984132973));
#192129=CARTESIAN_POINT('Ctrl Pts',(1.52052787674695,-6.59395814181705,
36.2692058721534));
#192130=CARTESIAN_POINT('Ctrl Pts',(1.69479714211257,-6.55377267652449,
36.277646081611));
#192131=CARTESIAN_POINT('Ctrl Pts',(1.86760150681647,-6.50664466348891,
36.2860862910686));
#192132=CARTESIAN_POINT('Ctrl Pts',(2.03836801823528,-6.45270058364989,
36.2945265005263));
#192133=CARTESIAN_POINT('Ctrl Pts',(2.20900514872209,-6.39879737444333,
36.3029603152748));
#192134=CARTESIAN_POINT('Ctrl Pts',(2.37760718688367,-6.33808849297188,
36.3113941300233));
#192135=CARTESIAN_POINT('Ctrl Pts',(2.54361417096903,-6.27075082819,36.3198279447718));
#192136=CARTESIAN_POINT('Ctrl Pts',(2.70952089990792,-6.20345383005527,
36.3282566661604));
#192137=CARTESIAN_POINT('Ctrl Pts',(2.87283539097089,-6.12953615472672,
36.3366853875489));
#192138=CARTESIAN_POINT('Ctrl Pts',(3.03301519935228,-6.04922373536457,
36.3451141089374));
#192139=CARTESIAN_POINT('Ctrl Pts',(3.19312286862617,-5.96894748576883,
36.3535390343391));
#192140=CARTESIAN_POINT('Ctrl Pts',(3.35009837246566,-5.88228238367233,
36.3619639597408));
#192141=CARTESIAN_POINT('Ctrl Pts',(3.50342116444249,-5.78950163179323,
36.3703888851426));
#192142=CARTESIAN_POINT('Ctrl Pts',(3.65669842971953,-5.69674842964357,
36.3788113089002));
#192143=CARTESIAN_POINT('Ctrl Pts',(3.80632486108276,-5.59788337156605,
36.3872337326579));
#192144=CARTESIAN_POINT('Ctrl Pts',(3.95180601000119,-5.49322475958508,
36.3956561564156));
#192145=CARTESIAN_POINT('Ctrl Pts',(4.09728944692012,-5.38856450162481,
36.4040787126338));
#192146=CARTESIAN_POINT('Ctrl Pts',(4.23862719660897,-5.27811069700969,
36.412501268852));
#192147=CARTESIAN_POINT('Ctrl Pts',(4.37535467090177,-5.16222437557862,
36.4209238250702));
#192148=CARTESIAN_POINT('Ctrl Pts',(4.51208676387452,-5.04633413948569,
36.4293466658039));
#192149=CARTESIAN_POINT('Ctrl Pts',(4.64420801634832,-4.92501123622479,
36.4377695065377));
#192150=CARTESIAN_POINT('Ctrl Pts',(4.77128764190422,-4.79865639926554,
36.4461923472714));
#192151=CARTESIAN_POINT('Ctrl Pts',(4.89838930195545,-4.67227965348295,
36.4546166484521));
#192152=CARTESIAN_POINT('Ctrl Pts',(5.02044735570816,-4.54086946969294,
36.4630409496327));
#192153=CARTESIAN_POINT('Ctrl Pts',(5.13706829083558,-4.40486303706388,
36.4714652508134));
#192154=CARTESIAN_POINT('Ctrl Pts',(5.25372573357491,-4.26881402828797,
36.4798921891802));
#192155=CARTESIAN_POINT('Ctrl Pts',(5.36494244719491,-4.12816615515036,
36.488319127547));
#192156=CARTESIAN_POINT('Ctrl Pts',(5.47036534831931,-3.98338950592424,
36.4967460659138));
#192157=CARTESIAN_POINT('Ctrl Pts',(5.57588303788324,-3.83848268429237,
36.5051805811575));
#192158=CARTESIAN_POINT('Ctrl Pts',(5.67559630927362,-3.68943993873915,
36.5136150964012));
#192159=CARTESIAN_POINT('Ctrl Pts',(5.76919491301089,-3.53676109677899,
36.5220496116448));
#192160=CARTESIAN_POINT('Ctrl Pts',(5.86283872567579,-3.38400850962989,
36.5304882008316));
#192161=CARTESIAN_POINT('Ctrl Pts',(5.95036181311914,-3.22761661180973,
36.5389267900184));
#192162=CARTESIAN_POINT('Ctrl Pts',(6.03149977166802,-3.06811008674209,
36.5473653792052));
#192163=CARTESIAN_POINT('Ctrl Pts',(6.11272842409734,-2.90842526946731,
36.5558134008255));
#192164=CARTESIAN_POINT('Ctrl Pts',(6.18755754249105,-2.7456191693734,36.5642614224458));
#192165=CARTESIAN_POINT('Ctrl Pts',(6.25577027609986,-2.58023782870215,
36.5727094440661));
#192166=CARTESIAN_POINT('Ctrl Pts',(6.29454129918217,-2.48623772876007,
36.5775111639784));
#192167=CARTESIAN_POINT('Ctrl Pts',(6.33117572478765,-2.39140600253605,
36.5823128838907));
#192168=CARTESIAN_POINT('Ctrl Pts',(6.36564090235695,-2.29584513899352,
36.587114603803));
#192169=CARTESIAN_POINT('Ctrl Pts',(6.42478157143281,-2.13186706587876,
36.5953541356538));
#192170=CARTESIAN_POINT('Ctrl Pts',(6.47766405255244,-1.96537515686491,
36.6035936675047));
#192171=CARTESIAN_POINT('Ctrl Pts',(6.52407000662113,-1.79688607004079,
36.6118331993555));
#192172=CARTESIAN_POINT('Ctrl Pts',(6.57042445332396,-1.62858399432788,
36.6200635859018));
#192173=CARTESIAN_POINT('Ctrl Pts',(6.61031659279737,-1.45828949478854,
36.6282939724482));
#192174=CARTESIAN_POINT('Ctrl Pts',(6.64357647031582,-1.28653825557814,
36.6365243589945));
#192175=CARTESIAN_POINT('Ctrl Pts',(6.67680536495121,-1.11494700939706,
36.6447470786123));
#192176=CARTESIAN_POINT('Ctrl Pts',(6.70341423438039,-0.941902073415117,
36.6529697982301));
#192177=CARTESIAN_POINT('Ctrl Pts',(6.72328316872599,-0.767953405569558,
36.6611925178479));
#192178=CARTESIAN_POINT('Ctrl Pts',(6.74313449776428,-0.594158868776013,
36.6694079515437));
#192179=CARTESIAN_POINT('Ctrl Pts',(6.75625775437691,-0.419462548391257,
36.6776233852395));
#192180=CARTESIAN_POINT('Ctrl Pts',(6.76258427853708,-0.244423557954591,
36.6858388189353));
#192181=CARTESIAN_POINT('Ctrl Pts',(6.76890755135511,-0.069474523966355,
36.6940500305361));
#192182=CARTESIAN_POINT('Ctrl Pts',(6.76844103549978,0.10581647453887,36.702261242137));
#192183=CARTESIAN_POINT('Ctrl Pts',(6.76116795752074,0.280885831246064,
36.7104724537378));
#192184=CARTESIAN_POINT('Ctrl Pts',(6.75389731853075,0.455896479350804,
36.7186809117514));
#192185=CARTESIAN_POINT('Ctrl Pts',(6.73982467920251,0.630685278503534,
36.7268893697649));
#192186=CARTESIAN_POINT('Ctrl Pts',(6.71898536681812,0.804689157677629,
36.7350978277784));
#192187=CARTESIAN_POINT('Ctrl Pts',(6.70970099810832,0.882211685359438,
36.7387548750615));
#192188=CARTESIAN_POINT('Ctrl Pts',(6.69907420526101,0.959578446429873,
36.7424119223446));
#192189=CARTESIAN_POINT('Ctrl Pts',(6.68711143303382,1.03673992987072,36.7460689696277));
#192190=CARTESIAN_POINT('Ctrl Pts',(6.65813201923183,1.22366103107891,36.7549280438036));
#192191=CARTESIAN_POINT('Ctrl Pts',(6.62133949993905,1.40918267875476,36.7637871179795));
#192192=CARTESIAN_POINT('Ctrl Pts',(6.57690487306358,1.59267425755317,36.7726461921554));
#192193=CARTESIAN_POINT('Ctrl Pts',(6.53238676246426,1.77651058011047,36.7815219107493));
#192194=CARTESIAN_POINT('Ctrl Pts',(6.48019791169681,1.9583089595996,36.7903976293432));
#192195=CARTESIAN_POINT('Ctrl Pts',(6.42055893068183,2.13745456504736,36.799273347937));
#192196=CARTESIAN_POINT('Ctrl Pts',(6.36074975686555,2.3171114014369,36.808174395324));
#192197=CARTESIAN_POINT('Ctrl Pts',(6.29344798985411,2.49410006711822,36.817075442711));
#192198=CARTESIAN_POINT('Ctrl Pts',(6.21892329917187,2.66782345724325,36.825976490098));
#192199=CARTESIAN_POINT('Ctrl Pts',(6.14429729115033,2.84178302670024,36.834889638581));
#192200=CARTESIAN_POINT('Ctrl Pts',(6.06242885224265,3.01246821742171,36.843802787064));
#192201=CARTESIAN_POINT('Ctrl Pts',(5.97363397466996,3.17930592058531,36.852715935547));
#192202=CARTESIAN_POINT('Ctrl Pts',(5.8846419481887,3.34651404907056,36.8616488736568));
#192203=CARTESIAN_POINT('Ctrl Pts',(5.78869284534651,3.50985737369966,36.8705818117667));
#192204=CARTESIAN_POINT('Ctrl Pts',(5.68614791999638,3.66878874179488,36.8795147498766));
#192205=CARTESIAN_POINT('Ctrl Pts',(5.58854001945675,3.82006836013483,36.8880176117352));
#192206=CARTESIAN_POINT('Ctrl Pts',(5.4849565601488,3.96735069595758,36.8965204735938));
#192207=CARTESIAN_POINT('Ctrl Pts',(5.37574326378257,4.11019140209995,36.9050233354524));
#192208=CARTESIAN_POINT('Ctrl Pts',(5.27012059960917,4.24833589949314,36.913246646647));
#192209=CARTESIAN_POINT('Ctrl Pts',(5.15902895751334,4.38259021076979,36.9214699578416));
#192210=CARTESIAN_POINT('Ctrl Pts',(5.0427851812063,4.5124945004073,36.9296932690362));
#192211=CARTESIAN_POINT('Ctrl Pts',(4.92666151119018,4.64226456933298,36.9379080836778));
#192212=CARTESIAN_POINT('Ctrl Pts',(4.80539654369622,4.7676933006627,36.9461228983194));
#192213=CARTESIAN_POINT('Ctrl Pts',(4.67934914740928,4.88835151729498,36.954337712961));
#192214=CARTESIAN_POINT('Ctrl Pts',(4.55343102504504,5.00888598713493,36.9625441025074));
#192215=CARTESIAN_POINT('Ctrl Pts',(4.42274050632266,5.12465944592435,36.9707504920537));
#192216=CARTESIAN_POINT('Ctrl Pts',(4.2876751231104,5.23527755125363,36.9789568816001));
#192217=CARTESIAN_POINT('Ctrl Pts',(4.15269036318479,5.3458296263759,36.9871583725849));
#192218=CARTESIAN_POINT('Ctrl Pts',(4.01333621478219,5.45123224877674,36.9953598635698));
#192219=CARTESIAN_POINT('Ctrl Pts',(3.87004562352525,5.55112924294085,37.0035613545546));
#192220=CARTESIAN_POINT('Ctrl Pts',(3.72681512970077,5.65098433935852,37.0117594057563));
#192221=CARTESIAN_POINT('Ctrl Pts',(3.57965177466728,5.74533820145981,37.019957456958));
#192222=CARTESIAN_POINT('Ctrl Pts',(3.42902005282767,5.83387611089795,37.0281555081598));
#192223=CARTESIAN_POINT('Ctrl Pts',(3.32077857961416,5.89749799369786,37.0340464926663));
#192224=CARTESIAN_POINT('Ctrl Pts',(3.21074685607432,5.95811758727905,37.0399374771729));
#192225=CARTESIAN_POINT('Ctrl Pts',(3.09910619832131,6.01563211736941,37.0458284616795));
#192226=CARTESIAN_POINT('Ctrl Pts',(3.09910619832134,6.0156321173694,35.0460577214446));
#192227=CARTESIAN_POINT('Ctrl Pts',(2.94708384676306,6.09395030618239,35.0541086516326));
#192228=CARTESIAN_POINT('Ctrl Pts',(2.79189904270229,6.16660071990929,35.0621595818206));
#192229=CARTESIAN_POINT('Ctrl Pts',(2.63402271304241,6.23331479609178,35.0702105120086));
#192230=CARTESIAN_POINT('Ctrl Pts',(2.47627391386713,6.2999749814948,35.0782549387579));
#192231=CARTESIAN_POINT('Ctrl Pts',(2.31583825840021,6.3607082290828,35.0862993655072));
#192232=CARTESIAN_POINT('Ctrl Pts',(2.15321099490439,6.41529199736246,35.0943437922565));
#192233=CARTESIAN_POINT('Ctrl Pts',(1.9906795021762,6.46984362140459,35.1023834816641));
#192234=CARTESIAN_POINT('Ctrl Pts',(1.82595932353737,6.51825285686615,35.1104231710717));
#192235=CARTESIAN_POINT('Ctrl Pts',(1.65956529319152,6.56034542060357,35.1184628604792));
#192236=CARTESIAN_POINT('Ctrl Pts',(1.48966640925584,6.60332460432857,35.1266718945095));
#192237=CARTESIAN_POINT('Ctrl Pts',(1.31802274300623,6.63971790327552,35.1348809285397));
#192238=CARTESIAN_POINT('Ctrl Pts',(1.14519870426525,6.66939344526541,35.1430899625699));
#192239=CARTESIAN_POINT('Ctrl Pts',(0.975994003012665,6.69844751235866,
35.1511270803273));
#192240=CARTESIAN_POINT('Ctrl Pts',(0.805658264584453,6.72106235791392,
35.1591641980846));
#192241=CARTESIAN_POINT('Ctrl Pts',(0.634730995471674,6.73716598900365,
35.1672013158419));
#192242=CARTESIAN_POINT('Ctrl Pts',(0.463785519346714,6.75327133543704,
35.1752392897055));
#192243=CARTESIAN_POINT('Ctrl Pts',(0.29224875906145,6.76286405125259,35.183277263569));
#192244=CARTESIAN_POINT('Ctrl Pts',(0.120664526296393,6.76592411072528,
35.1913152374326));
#192245=CARTESIAN_POINT('Ctrl Pts',(-0.0509719806591898,6.76898510246389,
35.1993556601143));
#192246=CARTESIAN_POINT('Ctrl Pts',(-0.222655615537248,6.76550946970699,
35.2073960827959));
#192247=CARTESIAN_POINT('Ctrl Pts',(-0.393843536411067,6.75552931078145,
35.2154365054776));
#192248=CARTESIAN_POINT('Ctrl Pts',(-0.571344388912239,6.745181111514,35.2237734364549));
#192249=CARTESIAN_POINT('Ctrl Pts',(-0.74831182610218,6.7278395231367,35.2321103674321));
#192250=CARTESIAN_POINT('Ctrl Pts',(-0.924148767020826,6.70359888838927,
35.2404472984094));
#192251=CARTESIAN_POINT('Ctrl Pts',(-1.09403149957942,6.68017909247874,
35.2485019233828));
#192252=CARTESIAN_POINT('Ctrl Pts',(-1.26285869709422,6.65031998160127,
35.2565565483562));
#192253=CARTESIAN_POINT('Ctrl Pts',(-1.43010484633272,6.61415823279846,
35.2646111733296));
#192254=CARTESIAN_POINT('Ctrl Pts',(-1.60614369396661,6.57609533797752,
35.2730892573088));
#192255=CARTESIAN_POINT('Ctrl Pts',(-1.78043028805679,6.531049369789,35.281567341288));
#192256=CARTESIAN_POINT('Ctrl Pts',(-1.95237352217877,6.47923812109844,
35.2900454252672));
#192257=CARTESIAN_POINT('Ctrl Pts',(-2.12431675630074,6.42742687240789,
35.2985235092464));
#192258=CARTESIAN_POINT('Ctrl Pts',(-2.29391621380858,6.36885058085278,
35.3070015932256));
#192259=CARTESIAN_POINT('Ctrl Pts',(-2.46060943853249,6.30378379951318,
35.3154796772048));
#192260=CARTESIAN_POINT('Ctrl Pts',(-2.6244485383512,6.23983109297434,35.3238125992515));
#192261=CARTESIAN_POINT('Ctrl Pts',(-2.78600320925251,6.16940483780113,
35.3321455212982));
#192262=CARTESIAN_POINT('Ctrl Pts',(-2.9447334664738,6.09268691230964,35.3404784433449));
#192263=CARTESIAN_POINT('Ctrl Pts',(-3.10327614302356,6.01605964880179,
35.3488015178985));
#192264=CARTESIAN_POINT('Ctrl Pts',(-3.25900074439442,5.93315567665279,
35.3571245924521));
#192265=CARTESIAN_POINT('Ctrl Pts',(-3.41138522679582,5.84420566325307,
35.3654476670058));
#192266=CARTESIAN_POINT('Ctrl Pts',(-3.56361759873903,5.75534443991308,
35.3737624334517));
#192267=CARTESIAN_POINT('Ctrl Pts',(-3.71251619570537,5.6604493736353,35.3820771998977));
#192268=CARTESIAN_POINT('Ctrl Pts',(-3.85758144512978,5.55979805336403,
35.3903919663436));
#192269=CARTESIAN_POINT('Ctrl Pts',(-4.00252850001729,5.45922874057722,
35.3986999581832));
#192270=CARTESIAN_POINT('Ctrl Pts',(-4.14364814613331,5.35291271652895,
35.4070079500227));
#192271=CARTESIAN_POINT('Ctrl Pts',(-4.28046761265466,5.24117219875617,
35.4153159418623));
#192272=CARTESIAN_POINT('Ctrl Pts',(-4.41720068664815,5.12950223779844,
35.4236186877493));
#192273=CARTESIAN_POINT('Ctrl Pts',(-4.5496387235486,5.01241482863005,35.4319214336364));
#192274=CARTESIAN_POINT('Ctrl Pts',(-4.67733984520325,4.8902741203816,35.4402241795235));
#192275=CARTESIAN_POINT('Ctrl Pts',(-4.804988779479,4.7681833271483,35.4485235323429));
#192276=CARTESIAN_POINT('Ctrl Pts',(-4.92790440474795,4.64104358985111,
35.4568228851624));
#192277=CARTESIAN_POINT('Ctrl Pts',(-5.04567950172157,4.50925796178338,
35.4651222379818));
#192278=CARTESIAN_POINT('Ctrl Pts',(-5.16342954990833,4.37750036230737,
35.4734198256682));
#192279=CARTESIAN_POINT('Ctrl Pts',(-5.27604101621247,4.24109909984328,
35.4817174133545));
#192280=CARTESIAN_POINT('Ctrl Pts',(-5.38314483868581,4.10049273206652,
35.4900150010409));
#192281=CARTESIAN_POINT('Ctrl Pts',(-5.4902436799781,3.95989290360609,35.4983122028233));
#192282=CARTESIAN_POINT('Ctrl Pts',(-5.59183517720703,3.81508863639148,
35.5066094046057));
#192283=CARTESIAN_POINT('Ctrl Pts',(-5.68759161547871,3.66655023360328,
35.5149066063881));
#192284=CARTESIAN_POINT('Ctrl Pts',(-5.78335951195384,3.51799405672836,
35.5232048010126));
#192285=CARTESIAN_POINT('Ctrl Pts',(-5.87329077019387,3.3657031466418,35.5315029956372));
#192286=CARTESIAN_POINT('Ctrl Pts',(-5.95710183292946,3.21017550176131,
35.5398011902617));
#192287=CARTESIAN_POINT('Ctrl Pts',(-6.0409718409626,3.05453847247494,35.5481052211033));
#192288=CARTESIAN_POINT('Ctrl Pts',(-6.11871288720063,2.89566046627381,
35.5564092519449));
#192289=CARTESIAN_POINT('Ctrl Pts',(-6.19008768987053,2.73406353103095,
35.5647132827864));
#192290=CARTESIAN_POINT('Ctrl Pts',(-6.26148844638324,2.57240783469454,
35.5730203332022));
#192291=CARTESIAN_POINT('Ctrl Pts',(-6.3265182115725,2.40803155994252,35.5813273836179));
#192292=CARTESIAN_POINT('Ctrl Pts',(-6.38498837166966,2.24147551707423,
35.5896344340337));
#192293=CARTESIAN_POINT('Ctrl Pts',(-6.443521046236,2.07474139768638,35.5979503660883));
#192294=CARTESIAN_POINT('Ctrl Pts',(-6.49547999468642,1.90582318462834,
35.6062662981429));
#192295=CARTESIAN_POINT('Ctrl Pts',(-6.54072656130306,1.73527664948983,
35.6145822301976));
#192296=CARTESIAN_POINT('Ctrl Pts',(-6.5748343842871,1.60671504877589,35.6208509564165));
#192297=CARTESIAN_POINT('Ctrl Pts',(-6.60512895506477,1.47722846531531,
35.6271196826355));
#192298=CARTESIAN_POINT('Ctrl Pts',(-6.63157020267617,1.34705814535883,
35.6333884088544));
#192299=CARTESIAN_POINT('Ctrl Pts',(-6.67246149404957,1.14575022828408,
35.6430829707043));
#192300=CARTESIAN_POINT('Ctrl Pts',(-6.70419740181038,0.942504625848324,
35.6527775325543));
#192301=CARTESIAN_POINT('Ctrl Pts',(-6.72662719127631,0.738089174546172,
35.6624720944042));
#192302=CARTESIAN_POINT('Ctrl Pts',(-6.74895889811254,0.534567606133308,
35.6721242631626));
#192303=CARTESIAN_POINT('Ctrl Pts',(-6.7620656592192,0.329886476403177,
35.6817764319209));
#192304=CARTESIAN_POINT('Ctrl Pts',(-6.76584879210263,0.124816354711093,
35.6914286006792));
#192305=CARTESIAN_POINT('Ctrl Pts',(-6.76660017729443,0.0840864471273353,
35.6933456617228));
#192306=CARTESIAN_POINT('Ctrl Pts',(-6.76698392647106,0.0433412329773021,
35.6952627227665));
#192307=CARTESIAN_POINT('Ctrl Pts',(-6.76699950557385,0.00258680559947647,
35.6971797838101));
#192308=CARTESIAN_POINT('',(-6.76699947070562,-0.00267646592832112,35.302820216152));
#192309=CARTESIAN_POINT('Ctrl Pts',(3.09910619832129,6.01563211736943,34.6512344137135));
#192310=CARTESIAN_POINT('Ctrl Pts',(2.94524428385927,6.09489800389497,34.6593669654902));
#192311=CARTESIAN_POINT('Ctrl Pts',(2.78845331533177,6.16819833692683,34.6674995172669));
#192312=CARTESIAN_POINT('Ctrl Pts',(2.62924644675822,6.23533095530697,34.6756320690436));
#192313=CARTESIAN_POINT('Ctrl Pts',(2.46987617618944,6.30253247526081,34.6837729676661));
#192314=CARTESIAN_POINT('Ctrl Pts',(2.30808539730431,6.36355351502733,34.6919138662887));
#192315=CARTESIAN_POINT('Ctrl Pts',(2.14440346720432,6.4182414078813,34.7000547649112));
#192316=CARTESIAN_POINT('Ctrl Pts',(2.11572748325503,6.42782236246036,34.7014809961274));
#192317=CARTESIAN_POINT('Ctrl Pts',(2.08699348323649,6.43720906171219,34.7029072273436));
#192318=CARTESIAN_POINT('Ctrl Pts',(2.05820434701039,6.44640084589436,34.7043334585597));
#192319=CARTESIAN_POINT('Ctrl Pts',(1.88783481849595,6.50079636248869,34.7127736680173));
#192320=CARTESIAN_POINT('Ctrl Pts',(1.71518132090391,6.5484741124627,34.721213877475));
#192321=CARTESIAN_POINT('Ctrl Pts',(1.5408011074484,6.58925040860383,34.7296540869326));
#192322=CARTESIAN_POINT('Ctrl Pts',(1.36655301283911,6.62999581065961,34.7380879016811));
#192323=CARTESIAN_POINT('Ctrl Pts',(1.19058113381837,6.663850106632,34.7465217164297));
#192324=CARTESIAN_POINT('Ctrl Pts',(1.01345728211852,6.6906795871063,34.7549555311782));
#192325=CARTESIAN_POINT('Ctrl Pts',(0.836440399277796,6.71749286468704,
34.7633842525668));
#192326=CARTESIAN_POINT('Ctrl Pts',(0.658273259633997,6.73728973485391,
34.7718129739553));
#192327=CARTESIAN_POINT('Ctrl Pts',(0.479537645247769,6.74998760345456,
34.7802416953438));
#192328=CARTESIAN_POINT('Ctrl Pts',(0.30088252682305,6.76267975340118,34.7886666207456));
#192329=CARTESIAN_POINT('Ctrl Pts',(0.121659776223405,6.76827925290529,
34.7970915461473));
#192330=CARTESIAN_POINT('Ctrl Pts',(-0.0575435276757699,6.76675533342404,
34.8055164715491));
#192331=CARTESIAN_POINT('Ctrl Pts',(-0.236693620080711,6.76523186644578,
34.8139388953068));
#192332=CARTESIAN_POINT('Ctrl Pts',(-0.41582394418443,6.75658920145334,
34.8223613190645));
#192333=CARTESIAN_POINT('Ctrl Pts',(-0.59434684330733,6.74084867281937,
34.8307837428223));
#192334=CARTESIAN_POINT('Ctrl Pts',(-0.772872550081101,6.72510789663223,
34.8392062990405));
#192335=CARTESIAN_POINT('Ctrl Pts',(-0.950790480090896,6.70226905642334,
34.8476288552587));
#192336=CARTESIAN_POINT('Ctrl Pts',(-1.12751684475177,6.67240547065307,
34.8560514114769));
#192337=CARTESIAN_POINT('Ctrl Pts',(-1.30424917926287,6.64254087608519,
34.8644742522106));
#192338=CARTESIAN_POINT('Ctrl Pts',(-1.47978953922511,6.60565111822101,
34.8728970929444));
#192339=CARTESIAN_POINT('Ctrl Pts',(-1.65356293705119,6.56186091084005,
34.8813199336781));
#192340=CARTESIAN_POINT('Ctrl Pts',(-1.82736646566389,6.51806311062032,
34.8897442348588));
#192341=CARTESIAN_POINT('Ctrl Pts',(-1.99940209787068,6.46736255696685,
34.8981685360394));
#192342=CARTESIAN_POINT('Ctrl Pts',(-2.16910829085744,6.40993433839486,
34.90659283722));
#192343=CARTESIAN_POINT('Ctrl Pts',(-2.33886760953542,6.35248814220076,
34.9150197755868));
#192344=CARTESIAN_POINT('Ctrl Pts',(-2.50629571928938,6.28831018905033,
34.9234467139536));
#192345=CARTESIAN_POINT('Ctrl Pts',(-2.67084905039007,6.21762449413202,
34.9318736523204));
#192346=CARTESIAN_POINT('Ctrl Pts',(-2.83555033561984,6.14687524388876,
34.9403081675641));
#192347=CARTESIAN_POINT('Ctrl Pts',(-2.99737137060435,6.06960669187759,
34.9487426828077));
#192348=CARTESIAN_POINT('Ctrl Pts',(-3.15579023964393,5.98609029027863,
34.9571771980514));
#192349=CARTESIAN_POINT('Ctrl Pts',(-3.3142856263542,5.90253354954234,34.9656157872381));
#192350=CARTESIAN_POINT('Ctrl Pts',(-3.46937527873959,5.81272310325608,
34.9740543764249));
#192351=CARTESIAN_POINT('Ctrl Pts',(-3.62056401772094,5.71697517867486,
34.9824929656117));
#192352=CARTESIAN_POINT('Ctrl Pts',(-3.77192175150706,5.62112022957626,
34.990940987232));
#192353=CARTESIAN_POINT('Ctrl Pts',(-3.91936958179618,5.51931472613761,
34.9993890088523));
#192354=CARTESIAN_POINT('Ctrl Pts',(-4.06244231912662,5.41191753482711,
35.0078370304726));
#192355=CARTESIAN_POINT('Ctrl Pts',(-4.14376256694475,5.35087469483328,
35.0126387503848));
#192356=CARTESIAN_POINT('Ctrl Pts',(-4.2236699951816,5.28802614393199,35.017440470297));
#192357=CARTESIAN_POINT('Ctrl Pts',(-4.30208421375348,5.22344334876652,
35.0222421902092));
#192358=CARTESIAN_POINT('Ctrl Pts',(-4.43663942798737,5.11262222477164,
35.0304817220601));
#192359=CARTESIAN_POINT('Ctrl Pts',(-4.56709622751511,4.99644504958966,
35.0387212539109));
#192360=CARTESIAN_POINT('Ctrl Pts',(-4.69300314149685,4.87524466195295,
35.0469607857617));
#192361=CARTESIAN_POINT('Ctrl Pts',(-4.81877030760365,4.75417879827588,
35.055191172308));
#192362=CARTESIAN_POINT('Ctrl Pts',(-4.93999738951996,4.62810106838202,
35.0634215588544));
#192363=CARTESIAN_POINT('Ctrl Pts',(-5.05626481170138,4.49738536862814,
35.0716519454007));
#192364=CARTESIAN_POINT('Ctrl Pts',(-5.1724239262096,4.36679143568583,35.0798746650185));
#192365=CARTESIAN_POINT('Ctrl Pts',(-5.28363234687956,4.23156840150379,
35.0880973846363));
#192366=CARTESIAN_POINT('Ctrl Pts',(-5.38950624703963,4.09212798102904,
35.0963201042541));
#192367=CARTESIAN_POINT('Ctrl Pts',(-5.49528633529622,3.95281111481315,
35.1045355379499));
#192368=CARTESIAN_POINT('Ctrl Pts',(-5.59574110953696,3.80928459269179,
35.1127509716456));
#192369=CARTESIAN_POINT('Ctrl Pts',(-5.69052614062956,3.66199416203954,
35.1209664053414));
#192370=CARTESIAN_POINT('Ctrl Pts',(-5.78526245957638,3.51477942723131,
35.1291776169422));
#192371=CARTESIAN_POINT('Ctrl Pts',(-5.87433464635052,3.36380493489245,
35.1373888285431));
#192372=CARTESIAN_POINT('Ctrl Pts',(-5.95744059692783,3.20954678016635,
35.1456000401439));
#192373=CARTESIAN_POINT('Ctrl Pts',(-6.04051867835514,3.05534035511332,
35.1538084981574));
#192374=CARTESIAN_POINT('Ctrl Pts',(-6.11763434062253,2.89785277426996,
35.1620169561709));
#192375=CARTESIAN_POINT('Ctrl Pts',(-6.18853055543361,2.73758626612288,
35.1702254141845));
#192376=CARTESIAN_POINT('Ctrl Pts',(-6.22011636720662,2.66618403719796,
35.1738824614677));
#192377=CARTESIAN_POINT('Ctrl Pts',(-6.25046829301772,2.59423054496445,
35.1775395087508));
#192378=CARTESIAN_POINT('Ctrl Pts',(-6.27956660306054,2.52177165455691,
35.181196556034));
#192379=CARTESIAN_POINT('Ctrl Pts',(-6.34676898490522,2.35442825853,35.1896424859724));
#192380=CARTESIAN_POINT('Ctrl Pts',(-6.40723500136563,2.18450425283061,
35.1980884159108));
#192381=CARTESIAN_POINT('Ctrl Pts',(-6.46079362546452,2.01256918617895,
35.2065343458492));
#192382=CARTESIAN_POINT('Ctrl Pts',(-6.51443996200314,1.84035254313462,
35.2149941076053));
#192383=CARTESIAN_POINT('Ctrl Pts',(-6.56115619788299,1.66611856781043,
35.2234538693613));
#192384=CARTESIAN_POINT('Ctrl Pts',(-6.60082171080229,1.49045018105308,
35.2319136311174));
#192385=CARTESIAN_POINT('Ctrl Pts',(-6.64052142330933,1.31463033309016,
35.2403806868763));
#192386=CARTESIAN_POINT('Ctrl Pts',(-6.67315822316374,1.13737392599471,
35.2488477426351));
#192387=CARTESIAN_POINT('Ctrl Pts',(-6.69866314743055,0.959271096852089,
35.257314798394));
#192388=CARTESIAN_POINT('Ctrl Pts',(-6.72421360004147,0.780850339814223,
35.2657969685294));
#192389=CARTESIAN_POINT('Ctrl Pts',(-6.74260669113894,0.601580464528102,
35.2742791386648));
#192390=CARTESIAN_POINT('Ctrl Pts',(-6.75382544137001,0.42205557395115,
35.2827613088002));
#192391=CARTESIAN_POINT('Ctrl Pts',(-6.7626689278794,0.280540172037556,
35.2894476112508));
#192392=CARTESIAN_POINT('Ctrl Pts',(-6.7670554533611,0.138866378318778,
35.2961339137014));
#192393=CARTESIAN_POINT('Ctrl Pts',(-6.76699947070562,-0.00267646592831579,
35.302820216152));
#192394=CARTESIAN_POINT('Ctrl Pts',(-6.7669994707053,-0.002676466730765,
35.3028202161899));
#192395=CARTESIAN_POINT('Ctrl Pts',(-6.76689528394057,-0.266095314299261,
35.3152637847462));
#192396=CARTESIAN_POINT('Ctrl Pts',(-6.75140799360082,-0.529171608800042,
35.3277073533025));
#192397=CARTESIAN_POINT('Ctrl Pts',(-6.72066816122544,-0.790511522174531,
35.3401509218588));
#192398=CARTESIAN_POINT('Ctrl Pts',(-6.7003552459903,-0.963205226001814,
35.3483736457246));
#192399=CARTESIAN_POINT('Ctrl Pts',(-6.67335474094204,-1.13534527406606,
35.3565963695905));
#192400=CARTESIAN_POINT('Ctrl Pts',(-6.63970438390436,-1.3063746378284,
35.3648190934564));
#192401=CARTESIAN_POINT('Ctrl Pts',(-6.60608964462966,-1.47722297280297,
35.3730331138476));
#192402=CARTESIAN_POINT('Ctrl Pts',(-6.56583913824034,-1.64696261546586,
35.3812471342388));
#192403=CARTESIAN_POINT('Ctrl Pts',(-6.51904236738862,-1.81504149048779,
35.3894611546301));
#192404=CARTESIAN_POINT('Ctrl Pts',(-6.47228573386492,-1.98297620520089,
35.397668129902));
#192405=CARTESIAN_POINT('Ctrl Pts',(-6.41899411369779,-2.14925264552916,
35.405875105174));
#192406=CARTESIAN_POINT('Ctrl Pts',(-6.35930809291377,-2.31332867950091,
35.414082080446));
#192407=CARTESIAN_POINT('Ctrl Pts',(-6.29966128465423,-2.47729691879288,
35.422283663899));
#192408=CARTESIAN_POINT('Ctrl Pts',(-6.23362856584403,-2.63906729533269,
35.4304852473521));
#192409=CARTESIAN_POINT('Ctrl Pts',(-6.16140043554176,-2.7981125197007,
35.4386868308051));
#192410=CARTESIAN_POINT('Ctrl Pts',(-6.0892052634236,-2.95708517065772,
35.4468846718201));
#192411=CARTESIAN_POINT('Ctrl Pts',(-6.01082045992842,-3.11333482086274,
35.4550825128352));
#192412=CARTESIAN_POINT('Ctrl Pts',(-5.92648478947531,-3.26635378367344,
35.4632803538502));
#192413=CARTESIAN_POINT('Ctrl Pts',(-5.84215656138202,-3.41935924303805,
35.4714774714314));
#192414=CARTESIAN_POINT('Ctrl Pts',(-5.75187867785699,-3.56913426481417,
35.4796745890125));
#192415=CARTESIAN_POINT('Ctrl Pts',(-5.6559362068274,-3.71519509908953,
35.4878717065937));
#192416=CARTESIAN_POINT('Ctrl Pts',(-5.55999480326459,-3.86125430827554,
35.4960687329728));
#192417=CARTESIAN_POINT('Ctrl Pts',(-5.45838913383538,-4.00359911176378,
35.5042657593519));
#192418=CARTESIAN_POINT('Ctrl Pts',(-5.35144794687987,-4.14177424201697,
35.5124627857309));
#192419=CARTESIAN_POINT('Ctrl Pts',(-5.24448850461171,-4.27997295934895,
35.5206612113771));
#192420=CARTESIAN_POINT('Ctrl Pts',(-5.13219194987402,-4.41400030158837,
35.5288596370232));
#192421=CARTESIAN_POINT('Ctrl Pts',(-5.014927735395,-4.54343359242391,35.5370580626694));
#192422=CARTESIAN_POINT('Ctrl Pts',(-4.89762218099701,-4.67291251322233,
35.54525937856));
#192423=CARTESIAN_POINT('Ctrl Pts',(-4.7753457190642,-4.79779389065165,
35.5534606944507));
#192424=CARTESIAN_POINT('Ctrl Pts',(-4.6485051353589,-4.91769143059443,
35.5616620103414));
#192425=CARTESIAN_POINT('Ctrl Pts',(-4.52152010146121,-5.037725513765,35.5698726661579));
#192426=CARTESIAN_POINT('Ctrl Pts',(-4.38996082261079,-5.15276417354653,
35.5780833219745));
#192427=CARTESIAN_POINT('Ctrl Pts',(-4.25426849298258,-5.26246031715354,
35.5862939777911));
#192428=CARTESIAN_POINT('Ctrl Pts',(-4.11849620315205,-5.37222110204029,
35.5945094719483));
#192429=CARTESIAN_POINT('Ctrl Pts',(-3.97858629483901,-5.4766328810103,
35.6027249661054));
#192430=CARTESIAN_POINT('Ctrl Pts',(-3.83500939456544,-5.57539164037782,
35.6109404602626));
#192431=CARTESIAN_POINT('Ctrl Pts',(-3.691209732089,-5.67430362577785,35.6191687009101));
#192432=CARTESIAN_POINT('Ctrl Pts',(-3.54373201107681,-5.76754487250477,
35.6273969415576));
#192433=CARTESIAN_POINT('Ctrl Pts',(-3.39307308681808,-5.85485644807034,
35.6356251822051));
#192434=CARTESIAN_POINT('Ctrl Pts',(-3.25614817752705,-5.934208730872,35.6431033393062));
#192435=CARTESIAN_POINT('Ctrl Pts',(-3.11659609816114,-6.0086636579805,
35.6505814964072));
#192436=CARTESIAN_POINT('Ctrl Pts',(-2.9748035714871,-6.07806159158227,
35.6580596535083));
#192437=CARTESIAN_POINT('Ctrl Pts',(-2.82180227347862,-6.1529454671238,
35.6661289627308));
#192438=CARTESIAN_POINT('Ctrl Pts',(-2.66569108822884,-6.22218558074512,
35.6741982719533));
#192439=CARTESIAN_POINT('Ctrl Pts',(-2.506933350062,-6.28550508538072,35.6822675811759));
#192440=CARTESIAN_POINT('Ctrl Pts',(-2.34837362594366,-6.34874561338434,
35.6903268257766));
#192441=CARTESIAN_POINT('Ctrl Pts',(-2.18717425916129,-6.40608008931937,
35.6983860703774));
#192442=CARTESIAN_POINT('Ctrl Pts',(-2.02382420479174,-6.45727687094948,
35.7064453149781));
#192443=CARTESIAN_POINT('Ctrl Pts',(-1.86064204543636,-6.50842103132757,
35.7144962760984));
#192444=CARTESIAN_POINT('Ctrl Pts',(-1.69531395053249,-6.55343994071516,
35.7225472372186));
#192445=CARTESIAN_POINT('Ctrl Pts',(-1.52834984306422,-6.59214955513037,
35.7305981983389));
#192446=CARTESIAN_POINT('Ctrl Pts',(-1.36152076006945,-6.63082786494135,
35.738642648618));
#192447=CARTESIAN_POINT('Ctrl Pts',(-1.19305865946455,-6.66320695129684,
35.7466870988971));
#192448=CARTESIAN_POINT('Ctrl Pts',(-1.02348955549306,-6.68915227288157,
35.7547315491762));
#192449=CARTESIAN_POINT('Ctrl Pts',(-0.854020465573154,-6.71508229157992,
35.7627712547344));
#192450=CARTESIAN_POINT('Ctrl Pts',(-0.683446039977079,-6.73458604336561,
35.7708109602926));
#192451=CARTESIAN_POINT('Ctrl Pts',(-0.512303335900461,-6.74757988407883,
35.7788506658509));
#192452=CARTESIAN_POINT('Ctrl Pts',(-0.337466608053861,-6.76085418989699,
35.7870639041553));
#192453=CARTESIAN_POINT('Ctrl Pts',(-0.162037179450421,-6.76733427404382,
35.7952771424598));
#192454=CARTESIAN_POINT('Ctrl Pts',(0.01340541338267,-6.76698672193851,
35.8034903807642));
#192455=CARTESIAN_POINT('Ctrl Pts',(0.185085899116309,-6.76664662257441,
35.8115274983124));
#192456=CARTESIAN_POINT('Ctrl Pts',(0.356778601719374,-6.75976874907977,
35.8195646158606));
#192457=CARTESIAN_POINT('Ctrl Pts',(0.527939652872292,-6.74637448730243,
35.8276017334087));
#192458=CARTESIAN_POINT('Ctrl Pts',(0.699118811776092,-6.73297880849736,
35.8356397012329));
#192459=CARTESIAN_POINT('Ctrl Pts',(0.869765834724054,-6.71306539776337,
35.843677669057));
#192460=CARTESIAN_POINT('Ctrl Pts',(1.03934150297878,-6.68670757848628,
35.8517156368811));
#192461=CARTESIAN_POINT('Ctrl Pts',(1.20896871045226,-6.66034174826382,
35.8597560476888));
#192462=CARTESIAN_POINT('Ctrl Pts',(1.37752354611965,-6.62752766817689,
35.8677964584965));
#192463=CARTESIAN_POINT('Ctrl Pts',(1.54447666483523,-6.58838985122916,
35.8758368693043));
#192464=CARTESIAN_POINT('Ctrl Pts',(1.7177396698112,-6.54777284554079,35.8841811622921));
#192465=CARTESIAN_POINT('Ctrl Pts',(1.88927708696084,-6.50034486233937,
35.8925254552799));
#192466=CARTESIAN_POINT('Ctrl Pts',(2.05851527055682,-6.44630156608302,
35.9008697482677));
#192467=CARTESIAN_POINT('Ctrl Pts',(2.22187813478561,-6.39413445177577,
35.9089243584832));
#192468=CARTESIAN_POINT('Ctrl Pts',(2.38309840904916,-6.33580383312127,
35.9169789686987));
#192469=CARTESIAN_POINT('Ctrl Pts',(2.54168173442563,-6.27153433865168,
35.9250335789143));
#192470=CARTESIAN_POINT('Ctrl Pts',(2.70038510961958,-6.20721619126689,
35.9330942865835));
#192471=CARTESIAN_POINT('Ctrl Pts',(2.85644722297175,-6.13695036868298,
35.9411549942527));
#192472=CARTESIAN_POINT('Ctrl Pts',(3.00939882702473,-6.06100715227281,
35.949215701922));
#192473=CARTESIAN_POINT('Ctrl Pts',(3.16256608367581,-5.98495686047742,
35.9572877747061));
#192474=CARTESIAN_POINT('Ctrl Pts',(3.31261375603508,-5.90321338096559,
35.9653598474903));
#192475=CARTESIAN_POINT('Ctrl Pts',(3.45910154803444,-5.81609022285467,
35.9734319202744));
#192476=CARTESIAN_POINT('Ctrl Pts',(3.47444503126758,-5.80696473398323,
35.9742774085689));
#192477=CARTESIAN_POINT('Ctrl Pts',(3.4897494894461,-5.79778026092327,35.9751228968634));
#192478=CARTESIAN_POINT('Ctrl Pts',(3.50501443822637,-5.7885371889472,35.9759683851578));
#192479=CARTESIAN_POINT('Ctrl Pts',(3.65546197140124,-5.69743977370033,
35.9843013072045));
#192480=CARTESIAN_POINT('Ctrl Pts',(3.80254895383336,-5.60035636262105,
35.9926342292513));
#192481=CARTESIAN_POINT('Ctrl Pts',(3.94577458207431,-5.49755872614894,
36.000967151298));
#192482=CARTESIAN_POINT('Ctrl Pts',(4.08883095235525,-5.39488257155445,
36.0092902258516));
#192483=CARTESIAN_POINT('Ctrl Pts',(4.22803477840236,-5.28650584488286,
36.0176133004052));
#192484=CARTESIAN_POINT('Ctrl Pts',(4.36291129740579,-5.17274530698825,
36.0259363749588));
#192485=CARTESIAN_POINT('Ctrl Pts',(4.49765318243103,-5.05909832506239,
36.0342511414048));
#192486=CARTESIAN_POINT('Ctrl Pts',(4.62807610197493,-4.94007846184567,
36.0425659078507));
#192487=CARTESIAN_POINT('Ctrl Pts',(4.75373547682771,-4.81604485198692,
36.0508806742967));
#192488=CARTESIAN_POINT('Ctrl Pts',(4.87929246843091,-4.69211230075628,
36.0591886661362));
#192489=CARTESIAN_POINT('Ctrl Pts',(5.00009340235943,-4.56317438604016,
36.0674966579758));
#192490=CARTESIAN_POINT('Ctrl Pts',(5.11572775623998,-4.4296296147687,36.0758046498153));
#192491=CARTESIAN_POINT('Ctrl Pts',(5.23128909460308,-4.29616916826967,
36.0841073957024));
#192492=CARTESIAN_POINT('Ctrl Pts',(5.34169012728582,-4.15810792466243,
36.0924101415895));
#192493=CARTESIAN_POINT('Ctrl Pts',(5.44655795667186,-4.01588040467025,
36.1007128874766));
#192494=CARTESIAN_POINT('Ctrl Pts',(5.55138292991797,-3.87371100853297,
36.109012240296));
#192495=CARTESIAN_POINT('Ctrl Pts',(5.65067899941118,-3.72737900821017,
36.1173115931154));
#192496=CARTESIAN_POINT('Ctrl Pts',(5.74411408363114,-3.57735130987025,
36.1256109459349));
#192497=CARTESIAN_POINT('Ctrl Pts',(5.83752929577646,-3.42735551990441,
36.1339085336212));
#192498=CARTESIAN_POINT('Ctrl Pts',(5.92508582221167,-3.27366589298205,
36.1422061213076));
#192499=CARTESIAN_POINT('Ctrl Pts',(6.00649526125543,-3.11677777143576,
36.1505037089939));
#192500=CARTESIAN_POINT('Ctrl Pts',(6.08790091411175,-2.95989694643693,
36.1588009107763));
#192501=CARTESIAN_POINT('Ctrl Pts',(6.16315988919264,-2.79981823210372,
36.1670981125587));
#192502=CARTESIAN_POINT('Ctrl Pts',(6.2320299626385,-2.63706115681378,36.1753953143411));
#192503=CARTESIAN_POINT('Ctrl Pts',(6.30090827706874,-2.47428460603254,
36.1836935089657));
#192504=CARTESIAN_POINT('Ctrl Pts',(6.36339603150264,-2.30882937628908,
36.1919917035902));
#192505=CARTESIAN_POINT('Ctrl Pts',(6.41929925439431,-2.14123470981878,
36.2002898982148));
#192506=CARTESIAN_POINT('Ctrl Pts',(6.47524179467439,-1.97352217206561,
36.2085939290563));
#192507=CARTESIAN_POINT('Ctrl Pts',(6.52459043958811,-1.80366752134964,
36.2168979598979));
#192508=CARTESIAN_POINT('Ctrl Pts',(6.56720093130783,-1.63222575884269,
36.2252019907395));
#192509=CARTESIAN_POINT('Ctrl Pts',(6.6098269173751,-1.46072165539234,36.2335090411552));
#192510=CARTESIAN_POINT('Ctrl Pts',(6.64570979000095,-1.28762962925029,
36.241816091571));
#192511=CARTESIAN_POINT('Ctrl Pts',(6.67475645564233,-1.11351482157222,
36.2501231419867));
#192512=CARTESIAN_POINT('Ctrl Pts',(6.70383417707155,-0.939213855779091,
36.2584390740413));
#192513=CARTESIAN_POINT('Ctrl Pts',(6.72606103795095,-0.76388826813644,
36.2667550060959));
#192514=CARTESIAN_POINT('Ctrl Pts',(6.74139572822352,-0.588109373747527,
36.2750709381506));
#192515=CARTESIAN_POINT('Ctrl Pts',(6.75295534347028,-0.455603509493314,
36.2813396643694));
#192516=CARTESIAN_POINT('Ctrl Pts',(6.76059957923247,-0.322840178810183,
36.2876083905883));
#192517=CARTESIAN_POINT('Ctrl Pts',(6.76433032192128,-0.190063925920677,
36.2938771168071));
#192518=CARTESIAN_POINT('Ctrl Pts',(6.76935937840859,-0.0110809909792215,
36.3023273855305));
#192519=CARTESIAN_POINT('Ctrl Pts',(6.76728459495253,0.168253599084478,
36.3107776542538));
#192520=CARTESIAN_POINT('Ctrl Pts',(6.75807926991523,0.347352244187413,
36.3192279229772));
#192521=CARTESIAN_POINT('Ctrl Pts',(6.74888206888957,0.526292828659922,
36.3276707340517));
#192522=CARTESIAN_POINT('Ctrl Pts',(6.73256688619761,0.704997553608084,
36.3361135451262));
#192523=CARTESIAN_POINT('Ctrl Pts',(6.70915905308408,0.88287813452362,36.3445563562007));
#192524=CARTESIAN_POINT('Ctrl Pts',(6.68576869114079,1.06062594868987,36.3529928657185));
#192525=CARTESIAN_POINT('Ctrl Pts',(6.65529627483146,1.23755051737008,36.3614293752362));
#192526=CARTESIAN_POINT('Ctrl Pts',(6.61781904841466,1.41306760009566,36.3698658847539));
#192527=CARTESIAN_POINT('Ctrl Pts',(6.58036863896995,1.58845909090426,36.3782963574951));
#192528=CARTESIAN_POINT('Ctrl Pts',(6.53592348636612,1.76244478115858,36.3867268302363));
#192529=CARTESIAN_POINT('Ctrl Pts',(6.48461214727213,1.93444935303325,36.3951573029776));
#192530=CARTESIAN_POINT('Ctrl Pts',(6.43332286678374,2.10637998060868,36.4035841514814));
#192531=CARTESIAN_POINT('Ctrl Pts',(6.37517337884471,2.2763308704905,36.4120109999852));
#192532=CARTESIAN_POINT('Ctrl Pts',(6.31034260999571,2.44373999117594,36.4204378484891));
#192533=CARTESIAN_POINT('Ctrl Pts',(6.2455318520898,2.61109743864438,36.4288620959257));
#192534=CARTESIAN_POINT('Ctrl Pts',(6.17404404553782,2.77591437265637,36.4372863433624));
#192535=CARTESIAN_POINT('Ctrl Pts',(6.09610707896122,2.93764658899585,36.445710590799));
#192536=CARTESIAN_POINT('Ctrl Pts',(6.07414742369342,2.98321653959202,36.4480842214101));
#192537=CARTESIAN_POINT('Ctrl Pts',(6.05167606520156,3.02854171668513,36.4504578520211));
#192538=CARTESIAN_POINT('Ctrl Pts',(6.02869878558656,3.07361024735849,36.4528314826322));
#192539=CARTESIAN_POINT('Ctrl Pts',(5.94526704241081,3.23725651617065,36.4614502635694));
#192540=CARTESIAN_POINT('Ctrl Pts',(5.85519874817166,3.39744398776223,36.4700690445067));
#192541=CARTESIAN_POINT('Ctrl Pts',(5.75881096500374,3.5536439423995,36.478687825444));
#192542=CARTESIAN_POINT('Ctrl Pts',(5.66236528228048,3.70993772539988,36.4873117836305));
#192543=CARTESIAN_POINT('Ctrl Pts',(5.55959269454276,3.86223895234433,36.4959357418171));
#192544=CARTESIAN_POINT('Ctrl Pts',(5.45085362699419,4.01004784723129,36.5045597000037));
#192545=CARTESIAN_POINT('Ctrl Pts',(5.33818618795038,4.16319657316984,36.5134952123748));
#192546=CARTESIAN_POINT('Ctrl Pts',(5.21911335343159,4.31152204278115,36.5224307247459));
#192547=CARTESIAN_POINT('Ctrl Pts',(5.094081191368,4.4545062370313,36.531366237117));
#192548=CARTESIAN_POINT('Ctrl Pts',(4.9731829065423,4.59276301478131,36.5400063190117));
#192549=CARTESIAN_POINT('Ctrl Pts',(4.84671329108184,4.72602586710489,36.5486464009064));
#192550=CARTESIAN_POINT('Ctrl Pts',(4.71511314186959,4.85386413688813,36.5572864828012));
#192551=CARTESIAN_POINT('Ctrl Pts',(4.57676328323695,4.9882591710748,36.5663697104104));
#192552=CARTESIAN_POINT('Ctrl Pts',(4.43274307541669,5.11665829633533,36.5754529380197));
#192553=CARTESIAN_POINT('Ctrl Pts',(4.28360435989835,5.23860885043537,36.584536165629));
#192554=CARTESIAN_POINT('Ctrl Pts',(4.13446564438004,5.3605594045354,36.5936193932383));
#192555=CARTESIAN_POINT('Ctrl Pts',(3.98020875174013,5.47606118199518,36.6027026208476));
#192556=CARTESIAN_POINT('Ctrl Pts',(3.82142145063258,5.5847136987177,36.6117858484568));
#192557=CARTESIAN_POINT('Ctrl Pts',(3.6633094499645,5.69290413130769,36.6208304463549));
#192558=CARTESIAN_POINT('Ctrl Pts',(3.5005599757691,5.79440407155689,36.6298750442529));
#192559=CARTESIAN_POINT('Ctrl Pts',(3.33373510326058,5.88884532495872,36.6389196421509));
#192560=CARTESIAN_POINT('Ctrl Pts',(3.25638187602201,5.93263577194207,36.6431134342753));
#192561=CARTESIAN_POINT('Ctrl Pts',(3.17815286472116,5.97490921260783,36.6473072263997));
#192562=CARTESIAN_POINT('Ctrl Pts',(3.0991061983213,6.01563211736942,36.6515010185242));
#192563=CARTESIAN_POINT('Origin',(0.,0.,4.30282021618968));
#192564=CARTESIAN_POINT('',(3.09910619832132,6.01563211736941,39.0457552630242));
#192565=CARTESIAN_POINT('',(3.0991061983213,6.01563211736942,38.6513937037315));
#192566=CARTESIAN_POINT('',(3.09910619832133,6.0156321173694,4.30282021618968));
#192567=CARTESIAN_POINT('',(-6.767,4.99256668992643E-13,37.6971797838101));
#192568=CARTESIAN_POINT('Ctrl Pts',(-6.767,4.9925651306646E-13,37.6971797838101));
#192569=CARTESIAN_POINT('Ctrl Pts',(-6.76700000000001,-0.186007249526497,
37.7059292956213));
#192570=CARTESIAN_POINT('Ctrl Pts',(-6.75932637294522,-0.372014355749668,
37.7146788074325));
#192571=CARTESIAN_POINT('Ctrl Pts',(-6.74400518264181,-0.557389537487367,
37.7234283192437));
#192572=CARTESIAN_POINT('Ctrl Pts',(-6.72868405705086,-0.74276393625177,
37.7321777940993));
#192573=CARTESIAN_POINT('Ctrl Pts',(-6.70571545645724,-0.927506130242345,
37.740927268955));
#192574=CARTESIAN_POINT('Ctrl Pts',(-6.67517739404798,-1.11098863990178,
37.7496767438107));
#192575=CARTESIAN_POINT('Ctrl Pts',(-6.64463945808664,-1.29447038982144,
37.7584261824377));
#192576=CARTESIAN_POINT('Ctrl Pts',(-6.60653217008304,-1.47669218313915,
37.7671756210647));
#192577=CARTESIAN_POINT('Ctrl Pts',(-6.5609849609261,-1.65703510599551,
37.7759250596918));
#192578=CARTESIAN_POINT('Ctrl Pts',(-6.51543793658224,-1.83737729708959,
37.7846744628169));
#192579=CARTESIAN_POINT('Ctrl Pts',(-6.46245112167342,-2.01584035511179,
37.7934238659421));
#192580=CARTESIAN_POINT('Ctrl Pts',(-6.40220448374169,-2.19181813761036,
37.8021732690673));
#192581=CARTESIAN_POINT('Ctrl Pts',(-6.34195808526415,-2.3677952206738,
37.8109226374174));
#192582=CARTESIAN_POINT('Ctrl Pts',(-6.27445201433011,-2.54128677684393,
37.8196720057675));
#192583=CARTESIAN_POINT('Ctrl Pts',(-6.19991555071806,-2.71170355385031,
37.8284213741175));
#192584=CARTESIAN_POINT('Ctrl Pts',(-6.12537937716588,-2.88211966767699,
37.8371707084193));
#192585=CARTESIAN_POINT('Ctrl Pts',(-6.04381298052407,-3.04946076372009,
37.8459200427211));
#192586=CARTESIAN_POINT('Ctrl Pts',(-5.9554933933571,-3.21315848374772,
37.8546693770229));
#192587=CARTESIAN_POINT('Ctrl Pts',(-5.86717414255279,-3.37685558033719,
37.8634186780031));
#192588=CARTESIAN_POINT('Ctrl Pts',(-5.77210188876459,-3.53690907646984,
37.8721679789833));
#192589=CARTESIAN_POINT('Ctrl Pts',(-5.67059953346847,-3.69277536969515,
37.8809172799635));
#192590=CARTESIAN_POINT('Ctrl Pts',(-5.5690975563123,-3.84864108225145,
37.8896665483487));
#192591=CARTESIAN_POINT('Ctrl Pts',(-5.46116568196693,-4.00031938297732,
37.898415816734));
#192592=CARTESIAN_POINT('Ctrl Pts',(-5.34717048533442,-4.14729511860062,
37.9071650851193));
#192593=CARTESIAN_POINT('Ctrl Pts',(-5.23317570391682,-4.29427031888104,
37.9159143216363));
#192594=CARTESIAN_POINT('Ctrl Pts',(-5.11311782003368,-4.43654276189715,
37.9246635581534));
#192595=CARTESIAN_POINT('Ctrl Pts',(-4.98740458984616,-4.57362924352002,
37.9334127946704));
#192596=CARTESIAN_POINT('Ctrl Pts',(-4.86169180711615,-4.71071523720399,
37.9421620000458));
#192597=CARTESIAN_POINT('Ctrl Pts',(-4.73032391204053,-4.84261509523353,
37.9509112054213));
#192598=CARTESIAN_POINT('Ctrl Pts',(-4.59374707013491,-4.9688808453843,
37.9596604107967));
#192599=CARTESIAN_POINT('Ctrl Pts',(-4.45717070301345,-5.09514615659551,
37.9684095857571));
#192600=CARTESIAN_POINT('Ctrl Pts',(-4.3153856357095,-5.21577720459602,
37.9771587607176));
#192601=CARTESIAN_POINT('Ctrl Pts',(-4.16887341029428,-5.3303642923295,
37.985907935678));
#192602=CARTESIAN_POINT('Ctrl Pts',(-4.02236168203632,-5.4449509912367,
37.99465708095));
#192603=CARTESIAN_POINT('Ctrl Pts',(-3.87112305348099,-5.55349359438647,
38.0034062262221));
#192604=CARTESIAN_POINT('Ctrl Pts',(-3.71567117017703,-5.65562346298932,
38.0121553714941));
#192605=CARTESIAN_POINT('Ctrl Pts',(-3.56021980145756,-5.75775299351683,
38.0209044878042));
#192606=CARTESIAN_POINT('Ctrl Pts',(-3.40055544538281,-5.85346967463913,
38.0296536041144));
#192607=CARTESIAN_POINT('Ctrl Pts',(-3.2372203598678,-5.94244842986941,
38.0384027204246));
#192608=CARTESIAN_POINT('Ctrl Pts',(-3.0738858014711,-6.03142689794564,
38.0471518084994));
#192609=CARTESIAN_POINT('Ctrl Pts',(-2.90688078896512,-6.11366734656813,
38.0559008965743));
#192610=CARTESIAN_POINT('Ctrl Pts',(-2.73677250721309,-6.18889046952381,
38.0646499846491));
#192611=CARTESIAN_POINT('Ctrl Pts',(-2.56666476031374,-6.26411335596373,
38.0733990452151));
#192612=CARTESIAN_POINT('Ctrl Pts',(-2.3934540257501,-6.33231884500616,
38.0821481057812));
#192613=CARTESIAN_POINT('Ctrl Pts',(-2.21772856065386,-6.39327529762798,
38.0908971663473));
#192614=CARTESIAN_POINT('Ctrl Pts',(-2.04200363348265,-6.45423156365191,
38.099646200131));
#192615=CARTESIAN_POINT('Ctrl Pts',(-1.86376426188986,-6.50793874375743,
38.1083952339147));
#192616=CARTESIAN_POINT('Ctrl Pts',(-1.68361577752817,-6.55421443909629,
38.1171442676984));
#192617=CARTESIAN_POINT('Ctrl Pts',(-1.50346782967488,-6.60048999661938,
38.1258932754262));
#192618=CARTESIAN_POINT('Ctrl Pts',(-1.32141105794702,-6.63933404237768,
38.134642283154));
#192619=CARTESIAN_POINT('Ctrl Pts',(-1.13806375486765,-6.67061465607605,
38.1433912908818));
#192620=CARTESIAN_POINT('Ctrl Pts',(-0.954716982601093,-6.70189517921322,
38.1521402732802));
#192621=CARTESIAN_POINT('Ctrl Pts',(-0.770079968900879,-6.72561226592241,
38.1608892556786));
#192622=CARTESIAN_POINT('Ctrl Pts',(-0.584779765557656,-6.74168536983107,
38.169638238077));
#192623=CARTESIAN_POINT('Ctrl Pts',(-0.391489830650733,-6.75845151013856,
38.1787644570868));
#192624=CARTESIAN_POINT('Ctrl Pts',(-0.197478578237794,-6.76689983031627,
38.1878906760967));
#192625=CARTESIAN_POINT('Ctrl Pts',(-0.00346287645082897,-6.76699911397118,
38.1970168951066));
#192626=CARTESIAN_POINT('Ctrl Pts',(0.184489834655294,-6.76709529501187,
38.2058579197724));
#192627=CARTESIAN_POINT('Ctrl Pts',(0.372446404250773,-6.7593563973816,
38.2146989444382));
#192628=CARTESIAN_POINT('Ctrl Pts',(0.559755019489732,-6.74380925873175,
38.223539969104));
#192629=CARTESIAN_POINT('Ctrl Pts',(0.745134705523219,-6.7284222265979,
38.2322899477137));
#192630=CARTESIAN_POINT('Ctrl Pts',(0.92987943123006,-6.70538706057503,
38.2410399263235));
#192631=CARTESIAN_POINT('Ctrl Pts',(1.11336163626979,-6.67478200894102,
38.2497899049332));
#192632=CARTESIAN_POINT('Ctrl Pts',(1.29684196300894,-6.64417727060979,
38.2585397939698));
#192633=CARTESIAN_POINT('Ctrl Pts',(1.47905951217707,-6.60600284890547,
38.2672896830063));
#192634=CARTESIAN_POINT('Ctrl Pts',(1.65939532067302,-6.56038841607176,
38.2760395720428));
#192635=CARTESIAN_POINT('Ctrl Pts',(1.83972934301021,-6.51477443503195,
38.284789374415));
#192636=CARTESIAN_POINT('Ctrl Pts',(2.01818138406485,-6.46172066062072,
38.2935391767871));
#192637=CARTESIAN_POINT('Ctrl Pts',(2.1941452835442,-6.40140730423403,38.3022889791593));
#192638=CARTESIAN_POINT('Ctrl Pts',(2.3701074986422,-6.3410945251856,38.3110386977756));
#192639=CARTESIAN_POINT('Ctrl Pts',(2.5435813486668,-6.27352239616415,38.3197884163919));
#192640=CARTESIAN_POINT('Ctrl Pts',(2.71397759435775,-6.19892043966723,
38.3285381350083));
#192641=CARTESIAN_POINT('Ctrl Pts',(2.88437226558332,-6.12431917249417,
38.337287772777));
#192642=CARTESIAN_POINT('Ctrl Pts',(3.05168912681152,-6.04268832278699,
38.3460374105457));
#192643=CARTESIAN_POINT('Ctrl Pts',(3.21535986274039,-5.95430516123234,
38.3547870483144));
#192644=CARTESIAN_POINT('Ctrl Pts',(3.37902914073035,-5.8659227869733,38.3635366081435));
#192645=CARTESIAN_POINT('Ctrl Pts',(3.53905210621772,-5.77078835741819,
38.3722861679725));
#192646=CARTESIAN_POINT('Ctrl Pts',(3.69488522831904,-5.66922500431494,
38.3810357278016));
#192647=CARTESIAN_POINT('Ctrl Pts',(3.85071701407155,-5.56766252216945,
38.3897852125987));
#192648=CARTESIAN_POINT('Ctrl Pts',(4.00235878822627,-5.45967138329207,
38.3985346973958));
#192649=CARTESIAN_POINT('Ctrl Pts',(4.14929549611555,-5.34561838199428,
38.407284182193));
#192650=CARTESIAN_POINT('Ctrl Pts',(4.29623099276313,-5.23156632086832,
38.4160335948656));
#192651=CARTESIAN_POINT('Ctrl Pts',(4.43846127436243,-5.11145267304777,
38.4247830075381));
#192652=CARTESIAN_POINT('Ctrl Pts',(4.5755032605465,-4.98568540049694,38.4335324202107));
#192653=CARTESIAN_POINT('Ctrl Pts',(4.7125441625798,-4.85991912290167,38.442281763666));
#192654=CARTESIAN_POINT('Ctrl Pts',(4.84439664018952,-4.72849950385223,
38.4510311071212));
#192655=CARTESIAN_POINT('Ctrl Pts',(4.97061286794928,-4.5918728986087,38.4597804505765));
#192656=CARTESIAN_POINT('Ctrl Pts',(5.09682813912862,-4.45524732884482,
38.4685297277213));
#192657=CARTESIAN_POINT('Ctrl Pts',(5.21740705148011,-4.3134150623558,38.4772790048661));
#192658=CARTESIAN_POINT('Ctrl Pts',(5.33194007545862,-4.16685781275511,
38.4860282820109));
#192659=CARTESIAN_POINT('Ctrl Pts',(5.44647226944641,-4.02030162521631,
38.4947774957521));
#192660=CARTESIAN_POINT('Ctrl Pts',(5.55495848628257,-3.86902074887726,
38.5035267094932));
#192661=CARTESIAN_POINT('Ctrl Pts',(5.65703027291922,-3.71352898080459,
38.5122759232343));
#192662=CARTESIAN_POINT('Ctrl Pts',(5.75910135377133,-3.5580382878937,38.5210250764782));
#192663=CARTESIAN_POINT('Ctrl Pts',(5.85475793592888,-3.39833700106479,
38.5297742297221));
#192664=CARTESIAN_POINT('Ctrl Pts',(5.94367514427534,-3.23496750823305,
38.538523382966));
#192665=CARTESIAN_POINT('Ctrl Pts',(6.03259176732766,-3.07159909077478,
38.5472724786189));
#192666=CARTESIAN_POINT('Ctrl Pts',(6.1147689683604,-2.9045627673119,38.5560215742718));
#192667=CARTESIAN_POINT('Ctrl Pts',(6.18992765547993,-2.73442583002809,
38.5647706699247));
#192668=CARTESIAN_POINT('Ctrl Pts',(6.26508587283156,-2.56428995615922,
38.5735197108928));
#192669=CARTESIAN_POINT('Ctrl Pts',(6.33322554827256,-2.39105376934948,
38.5822687518608));
#192670=CARTESIAN_POINT('Ctrl Pts',(6.39411526733121,-2.21530561053819,
38.5910177928289));
#192671=CARTESIAN_POINT('Ctrl Pts',(6.45500462602929,-2.03955849184841,
38.5997667820179));
#192672=CARTESIAN_POINT('Ctrl Pts',(6.50864402040813,-1.86129970164291,
38.6085157712069));
#192673=CARTESIAN_POINT('Ctrl Pts',(6.55485128368665,-1.68113463135808,
38.6172647603959));
#192674=CARTESIAN_POINT('Ctrl Pts',(6.60199809554379,-1.49730620116635,
38.6261916458674));
#192675=CARTESIAN_POINT('Ctrl Pts',(6.64140720707916,-1.31149343245482,
38.6351185313388));
#192676=CARTESIAN_POINT('Ctrl Pts',(6.67293928722917,-1.12435326697326,
38.6440454168102));
#192677=CARTESIAN_POINT('Ctrl Pts',(6.70384625876285,-0.940923067004551,
38.6527953309877));
#192678=CARTESIAN_POINT('Ctrl Pts',(6.72718554579819,-0.75621789951958,
38.6615452451651));
#192679=CARTESIAN_POINT('Ctrl Pts',(6.74287786815346,-0.570865181252368,
38.6702951593426));
#192680=CARTESIAN_POINT('Ctrl Pts',(6.75856988190857,-0.385516108071883,
38.6790449014471));
#192681=CARTESIAN_POINT('Ctrl Pts',(6.76661520773408,-0.199519795224353,
38.6877946435516));
#192682=CARTESIAN_POINT('Ctrl Pts',(6.76698651789579,-0.0135080204537233,
38.696544385656));
#192683=CARTESIAN_POINT('Ctrl Pts',(6.76735782124898,0.172500343514815,
38.705293967321));
#192684=CARTESIAN_POINT('Ctrl Pts',(6.76005538995174,0.358523882212703,
38.714043548986));
#192685=CARTESIAN_POINT('Ctrl Pts',(6.74510402742347,0.543930748566084,
38.7227931306509));
#192686=CARTESIAN_POINT('Ctrl Pts',(6.73015291918012,0.729334461616904,
38.7315425635076));
#192687=CARTESIAN_POINT('Ctrl Pts',(6.70755316306572,0.914121237636309,
38.7402919963643));
#192688=CARTESIAN_POINT('Ctrl Pts',(6.67738151874548,1.0976634516628,38.749041429221));
#192689=CARTESIAN_POINT('Ctrl Pts',(6.64721034747539,1.28120278799822,38.7577907248985));
#192690=CARTESIAN_POINT('Ctrl Pts',(6.60946757205107,1.46349731860486,38.766540020576));
#192691=CARTESIAN_POINT('Ctrl Pts',(6.56428138111484,1.64392790278318,38.7752893162536));
#192692=CARTESIAN_POINT('Ctrl Pts',(6.51909583859811,1.82435589779195,38.7840384863792));
#192693=CARTESIAN_POINT('Ctrl Pts',(6.46646716392837,2.00291972192387,38.7927876565047));
#192694=CARTESIAN_POINT('Ctrl Pts',(6.40657409872848,2.17901292274768,38.8015368266303));
#192695=CARTESIAN_POINT('Ctrl Pts',(6.34668181342035,2.35510383059088,38.8102858828294));
#192696=CARTESIAN_POINT('Ctrl Pts',(6.27952541914004,2.52872390822696,38.8190349390286));
#192697=CARTESIAN_POINT('Ctrl Pts',(6.20533299175464,2.69928350890407,38.8277839952277));
#192698=CARTESIAN_POINT('Ctrl Pts',(6.12831602991493,2.87633637965741,38.8368661313859));
#192699=CARTESIAN_POINT('Ctrl Pts',(6.04371690605213,3.05009086601576,38.8459482675441));
#192700=CARTESIAN_POINT('Ctrl Pts',(5.95184520316572,3.21991112882844,38.8550304037022));
#192701=CARTESIAN_POINT('Ctrl Pts',(5.86333549509209,3.38351691183131,38.8637801840458));
#192702=CARTESIAN_POINT('Ctrl Pts',(5.76807618099297,3.54347103712121,38.8725299643894));
#192703=CARTESIAN_POINT('Ctrl Pts',(5.66639083308937,3.69923018027816,38.881279744733));
#192704=CARTESIAN_POINT('Ctrl Pts',(5.56470914082117,3.85498372382171,38.8900292105179));
#192705=CARTESIAN_POINT('Ctrl Pts',(5.45660203371979,4.00654234702118,38.8987786763028));
#192706=CARTESIAN_POINT('Ctrl Pts',(5.34243669839123,4.15339127986789,38.9075281420877));
#192707=CARTESIAN_POINT('Ctrl Pts',(5.22827486050489,4.30023571401404,38.9162773398337));
#192708=CARTESIAN_POINT('Ctrl Pts',(5.10805534166999,4.44237052028598,38.9250265375797));
#192709=CARTESIAN_POINT('Ctrl Pts',(4.9821864433983,4.57931296628853,38.9337757353257));
#192710=CARTESIAN_POINT('Ctrl Pts',(4.85632073219463,4.71625194483487,38.9425247115374));
#192711=CARTESIAN_POINT('Ctrl Pts',(4.72480612170194,4.8479986152463,38.951273687749));
#192712=CARTESIAN_POINT('Ctrl Pts',(4.58808925235186,4.97410554898601,38.9600226639607));
#192713=CARTESIAN_POINT('Ctrl Pts',(4.4513634947392,5.10022068121318,38.9687722089624));
#192714=CARTESIAN_POINT('Ctrl Pts',(4.3094350120995,5.22069514871942,38.9775217539641));
#192715=CARTESIAN_POINT('Ctrl Pts',(4.16278587431649,5.3351197516636,38.9862712989658));
#192716=CARTESIAN_POINT('Ctrl Pts',(4.01614535740297,5.44953762807954,38.9950203296195));
#192717=CARTESIAN_POINT('Ctrl Pts',(3.86478496657754,5.55790617532902,39.0037693602732));
#192718=CARTESIAN_POINT('Ctrl Pts',(3.70921874747007,5.6598573553948,39.012518390927));
#192719=CARTESIAN_POINT('Ctrl Pts',(3.55365041605713,5.76180991977162,39.0212675403766));
#192720=CARTESIAN_POINT('Ctrl Pts',(3.39387638174336,5.85734478552921,39.0300166898262));
#192721=CARTESIAN_POINT('Ctrl Pts',(3.23043927904355,5.94613749121332,39.0387658392758));
#192722=CARTESIAN_POINT('Ctrl Pts',(3.18691767070304,5.96978206944214,39.041095647192));
#192723=CARTESIAN_POINT('Ctrl Pts',(3.14313645919564,5.9929488063346,39.0434254551081));
#192724=CARTESIAN_POINT('Ctrl Pts',(3.09910619832132,6.01563211736941,39.0457552630242));
#192725=CARTESIAN_POINT('Ctrl Pts',(3.09910619832131,6.01563211736941,37.0458284616795));
#192726=CARTESIAN_POINT('Ctrl Pts',(2.9437658708396,6.09565964604056,37.054025363067));
#192727=CARTESIAN_POINT('Ctrl Pts',(2.78530975093572,6.16967354755004,37.0622222644545));
#192728=CARTESIAN_POINT('Ctrl Pts',(2.62424690404949,6.23743674810308,37.0704191658421));
#192729=CARTESIAN_POINT('Ctrl Pts',(2.46316479927292,6.30520805093613,37.0786170473131));
#192730=CARTESIAN_POINT('Ctrl Pts',(2.29947567723226,6.36672702439135,37.086814928784));
#192731=CARTESIAN_POINT('Ctrl Pts',(2.13370830002611,6.42180487794512,37.095012810255));
#192732=CARTESIAN_POINT('Ctrl Pts',(1.96789096067751,6.47689933191575,37.1032131625603));
#192733=CARTESIAN_POINT('Ctrl Pts',(1.7999944587886,6.52554868564942,37.1114135148655));
#192734=CARTESIAN_POINT('Ctrl Pts',(1.63056246409196,6.56761410640838,37.1196138671708));
#192735=CARTESIAN_POINT('Ctrl Pts',(1.45266961214355,6.61178013113482,37.128223717165));
#192736=CARTESIAN_POINT('Ctrl Pts',(1.2730844187967,6.64868769951069,37.1368335671593));
#192737=CARTESIAN_POINT('Ctrl Pts',(1.09244692275168,6.678236947052,37.1454434171536));
#192738=CARTESIAN_POINT('Ctrl Pts',(0.920109234862118,6.70642848597189,
37.1536576676474));
#192739=CARTESIAN_POINT('Ctrl Pts',(0.746814140581132,6.72792277328595,
37.1618719181412));
#192740=CARTESIAN_POINT('Ctrl Pts',(0.573121202973082,6.74268648883386,
37.170086168635));
#192741=CARTESIAN_POINT('Ctrl Pts',(0.399304144714054,6.75746075450551,
37.1783062890169));
#192742=CARTESIAN_POINT('Ctrl Pts',(0.225089033396702,6.76549484641998,
37.1865264093989));
#192743=CARTESIAN_POINT('Ctrl Pts',(0.051034827200337,6.76680755204496,
37.1947465297809));
#192744=CARTESIAN_POINT('Ctrl Pts',(-0.123252425226701,6.76812201528961,
37.2029776563207));
#192745=CARTESIAN_POINT('Ctrl Pts',(-0.297377985862902,6.76269713672645,
37.2112087828605));
#192746=CARTESIAN_POINT('Ctrl Pts',(-0.470787829535581,6.75060351520967,
37.2194399094004));
#192747=CARTESIAN_POINT('Ctrl Pts',(-0.495311589767621,6.7488932254814,
37.2206039619676));
#192748=CARTESIAN_POINT('Ctrl Pts',(-0.519821052605789,6.74704964539409,
37.2217680145347));
#192749=CARTESIAN_POINT('Ctrl Pts',(-0.544314668960146,6.74507305676928,
37.2229320671019));
#192750=CARTESIAN_POINT('Ctrl Pts',(-0.714106454926598,6.73137118000788,
37.2310013763244));
#192751=CARTESIAN_POINT('Ctrl Pts',(-0.883691765990604,6.7112287430705,
37.239070685547));
#192752=CARTESIAN_POINT('Ctrl Pts',(-1.05253086097781,6.68464417801646,
37.2471399947695));
#192753=CARTESIAN_POINT('Ctrl Pts',(-1.22115936772438,6.65809277114052,
37.2551992393702));
#192754=CARTESIAN_POINT('Ctrl Pts',(-1.38904314637551,6.62511528112674,
37.263258483971));
#192755=CARTESIAN_POINT('Ctrl Pts',(-1.55564349772948,6.58576209014355,
37.2713177285718));
#192756=CARTESIAN_POINT('Ctrl Pts',(-1.72207261333684,6.54644934729259,
37.279368689692));
#192757=CARTESIAN_POINT('Ctrl Pts',(-1.88722056668069,6.5007740293082,37.2874196508122));
#192758=CARTESIAN_POINT('Ctrl Pts',(-2.05055492328046,6.44883815168363,
37.2954706119324));
#192759=CARTESIAN_POINT('Ctrl Pts',(-2.21375719080067,6.39694427478943,
37.3035150622115));
#192760=CARTESIAN_POINT('Ctrl Pts',(-2.375148426933,6.33880002766862,37.3115595124906));
#192761=CARTESIAN_POINT('Ctrl Pts',(-2.53420762751316,6.27455820760746,
37.3196039627697));
#192762=CARTESIAN_POINT('Ctrl Pts',(-2.69317301291823,6.21035427820321,
37.327643668328));
#192763=CARTESIAN_POINT('Ctrl Pts',(-2.8498087558028,6.14006007465764,37.3356833738862));
#192764=CARTESIAN_POINT('Ctrl Pts',(-3.00361033524864,6.06387779840487,
37.3437230794444));
#192765=CARTESIAN_POINT('Ctrl Pts',(-3.1607316395605,5.98605116844822,37.3519363177489));
#192766=CARTESIAN_POINT('Ctrl Pts',(-3.31489466169615,5.90207951539378,
37.3601495560533));
#192767=CARTESIAN_POINT('Ctrl Pts',(-3.46558399043854,5.81222991675451,
37.3683627943578));
#192768=CARTESIAN_POINT('Ctrl Pts',(-3.61304200924495,5.72430700996031,
37.376399911906));
#192769=CARTESIAN_POINT('Ctrl Pts',(-3.75717347361353,5.63075589959779,
37.3844370294542));
#192770=CARTESIAN_POINT('Ctrl Pts',(-3.89752161580777,5.53187258117098,
37.3924741470024));
#192771=CARTESIAN_POINT('Ctrl Pts',(-4.03788460594328,5.43297880151766,
37.4005121148265));
#192772=CARTESIAN_POINT('Ctrl Pts',(-4.17446317143389,5.3287519056758,37.4085500826506));
#192773=CARTESIAN_POINT('Ctrl Pts',(-4.30683105316518,5.21953017804209,
37.4165880504748));
#192774=CARTESIAN_POINT('Ctrl Pts',(-4.43923916553369,5.11027525459348,
37.4246284612825));
#192775=CARTESIAN_POINT('Ctrl Pts',(-4.5674337587902,4.99602271528344,37.4326688720903));
#192776=CARTESIAN_POINT('Ctrl Pts',(-4.69102319291762,4.87714982377094,
37.4407092828981));
#192777=CARTESIAN_POINT('Ctrl Pts',(-4.81928361060147,4.75378420741122,
37.4490535758858));
#192778=CARTESIAN_POINT('Ctrl Pts',(-4.94258364897058,4.62544247759992,
37.4573978688736));
#192779=CARTESIAN_POINT('Ctrl Pts',(-5.06052989067974,4.49258569484623,
37.4657421618614));
#192780=CARTESIAN_POINT('Ctrl Pts',(-5.1743814781955,4.36434120473315,37.4737967720769));
#192781=CARTESIAN_POINT('Ctrl Pts',(-5.28324458573389,4.23189022616613,
37.4818513822925));
#192782=CARTESIAN_POINT('Ctrl Pts',(-5.38680876038135,4.09567825629391,
37.489905992508));
#192783=CARTESIAN_POINT('Ctrl Pts',(-5.49045133457159,3.95936317203687,
37.4979667001772));
#192784=CARTESIAN_POINT('Ctrl Pts',(-5.58878677562368,3.81928173115245,
37.5060274078465));
#192785=CARTESIAN_POINT('Ctrl Pts',(-5.68154952696108,3.67590587103212,
37.5140881155157));
#192786=CARTESIAN_POINT('Ctrl Pts',(-5.77444306822101,3.5323278595378,37.5221601882999));
#192787=CARTESIAN_POINT('Ctrl Pts',(-5.86174805435501,3.38544647943955,
37.530232261084));
#192788=CARTESIAN_POINT('Ctrl Pts',(-5.94324588931876,3.23575606297751,
37.5383043338682));
#192789=CARTESIAN_POINT('Ctrl Pts',(-5.95178216832952,3.22007712916626,
37.5391498221626));
#192790=CARTESIAN_POINT('Ctrl Pts',(-5.96025478173107,3.2043673930891,37.539995310457));
#192791=CARTESIAN_POINT('Ctrl Pts',(-5.96866350967991,3.18862743327212,
37.5408407987514));
#192792=CARTESIAN_POINT('Ctrl Pts',(-6.05851105501668,3.02044542502301,
37.5498748700551));
#192793=CARTESIAN_POINT('Ctrl Pts',(-6.1413108520305,2.84834316167856,37.5589089413587));
#192794=CARTESIAN_POINT('Ctrl Pts',(-6.21674145466605,2.67290379285088,
37.5679430126624));
#192795=CARTESIAN_POINT('Ctrl Pts',(-6.29202726850127,2.49780117933015,
37.5769597430951));
#192796=CARTESIAN_POINT('Ctrl Pts',(-6.35997201579616,2.31937446278634,
37.5859764735278));
#192797=CARTESIAN_POINT('Ctrl Pts',(-6.42030078831588,2.13822982570877,
37.5949932039605));
#192798=CARTESIAN_POINT('Ctrl Pts',(-6.48043547153938,1.95766796586426,
37.6039809258325));
#192799=CARTESIAN_POINT('Ctrl Pts',(-6.53300299195141,1.7744058617648,37.6129686477044));
#192800=CARTESIAN_POINT('Ctrl Pts',(-6.57777737586843,1.58906695690065,
37.6219563695763));
#192801=CARTESIAN_POINT('Ctrl Pts',(-6.62246057309719,1.40410550984739,
37.6309257872189));
#192802=CARTESIAN_POINT('Ctrl Pts',(-6.65938223385962,1.21707593198739,
37.6398952048615));
#192803=CARTESIAN_POINT('Ctrl Pts',(-6.68836562468187,1.02861765033172,
37.6488646225041));
#192804=CARTESIAN_POINT('Ctrl Pts',(-6.71725025336708,0.840801548286838,
37.6578034764745));
#192805=CARTESIAN_POINT('Ctrl Pts',(-6.73825053371445,0.651566692490344,
37.666742330445));
#192806=CARTESIAN_POINT('Ctrl Pts',(-6.75124057061721,0.461562300943391,
37.6756811844155));
#192807=CARTESIAN_POINT('Ctrl Pts',(-6.76165456777378,0.309237468603303,
37.6828473842137));
#192808=CARTESIAN_POINT('Ctrl Pts',(-6.7669212299791,0.156418407734503,
37.6900135840119));
#192809=CARTESIAN_POINT('Ctrl Pts',(-6.76699912273183,0.00344571424731888,
37.6971797838101));
#192810=CARTESIAN_POINT('',(-6.76699756085807,0.00574554966943631,37.3028202162268));
#192811=CARTESIAN_POINT('Ctrl Pts',(3.0991061983213,6.01563211736942,36.6515010185242));
#192812=CARTESIAN_POINT('Ctrl Pts',(2.92887035067861,6.1033334528754,36.6605328194799));
#192813=CARTESIAN_POINT('Ctrl Pts',(2.75484054269377,6.18384034560604,36.6695646204357));
#192814=CARTESIAN_POINT('Ctrl Pts',(2.57761663267981,6.25685076495616,36.6785964213915));
#192815=CARTESIAN_POINT('Ctrl Pts',(2.40071872169563,6.32972688343304,36.6876116085712));
#192816=CARTESIAN_POINT('Ctrl Pts',(2.22063865975616,6.3951339710474,36.6966267957509));
#192817=CARTESIAN_POINT('Ctrl Pts',(2.03799658225956,6.45281790620953,36.7056419829307));
#192818=CARTESIAN_POINT('Ctrl Pts',(1.85559641772055,6.51042543788594,36.714645229321));
#192819=CARTESIAN_POINT('Ctrl Pts',(1.6706412354187,6.56033015820393,36.7236484757112));
#192820=CARTESIAN_POINT('Ctrl Pts',(1.48376906171766,6.60232673922531,36.7326517221015));
#192821=CARTESIAN_POINT('Ctrl Pts',(1.2973000589344,6.64423271392592,36.741635544267));
#192822=CARTESIAN_POINT('Ctrl Pts',(1.1089225512334,6.67826454966805,36.7506193664325));
#192823=CARTESIAN_POINT('Ctrl Pts',(0.919287431701544,6.70426726927825,
36.7596031885979));
#192824=CARTESIAN_POINT('Ctrl Pts',(0.840925417633422,6.71501224882072,
36.7633155304925));
#192825=CARTESIAN_POINT('Ctrl Pts',(0.762348841543449,6.72438680262534,
36.767027872387));
#192826=CARTESIAN_POINT('Ctrl Pts',(0.683604340953227,6.73238249841985,
36.7707402142816));
#192827=CARTESIAN_POINT('Ctrl Pts',(0.511335538045042,6.74987462717316,
36.7788616791378));
#192828=CARTESIAN_POINT('Ctrl Pts',(0.338339441484207,6.76075602110291,
36.786983143994));
#192829=CARTESIAN_POINT('Ctrl Pts',(0.165167046070349,6.7649840241417,36.7951046088501));
#192830=CARTESIAN_POINT('Ctrl Pts',(-0.00799299960279759,6.76921172566164,
36.8032254945263));
#192831=CARTESIAN_POINT('Ctrl Pts',(-0.181328953008264,6.76678697245923,
36.8113463802025));
#192832=CARTESIAN_POINT('Ctrl Pts',(-0.354288183683026,6.75771920716617,
36.8194672658787));
#192833=CARTESIAN_POINT('Ctrl Pts',(-0.527268087931676,6.74865035801587,
36.827589122233));
#192834=CARTESIAN_POINT('Ctrl Pts',(-0.699870814171343,6.73293693605041,
36.8357109785872));
#192835=CARTESIAN_POINT('Ctrl Pts',(-0.871547268904518,6.71064038360461,
36.8438328349414));
#192836=CARTESIAN_POINT('Ctrl Pts',(-1.04334897665523,6.68832756386999,
36.8519606169016));
#192837=CARTESIAN_POINT('Ctrl Pts',(-1.21422269964026,6.65942206802559,
36.8600883988618));
#192838=CARTESIAN_POINT('Ctrl Pts',(-1.383627338963,6.62403686484867,36.868216180822));
#192839=CARTESIAN_POINT('Ctrl Pts',(-1.55310098743957,6.58863724705513,
36.8763472737384));
#192840=CARTESIAN_POINT('Ctrl Pts',(-1.7211040043136,6.54675274900076,36.8844783666548));
#192841=CARTESIAN_POINT('Ctrl Pts',(-1.887109178007,6.49854660291682,36.8926094595713));
#192842=CARTESIAN_POINT('Ctrl Pts',(-2.0532955394097,6.4502878418391,36.9007494272359));
#192843=CARTESIAN_POINT('Ctrl Pts',(-2.21747935526281,6.39569376690599,
36.9088893949004));
#192844=CARTESIAN_POINT('Ctrl Pts',(-2.3791514486796,6.33497651015738,36.917029362565));
#192845=CARTESIAN_POINT('Ctrl Pts',(-2.46300158657844,6.30348591556178,
36.9212511017454));
#192846=CARTESIAN_POINT('Ctrl Pts',(-2.54617644965186,6.27034902093991,
36.9254728409259));
#192847=CARTESIAN_POINT('Ctrl Pts',(-2.62860754292939,6.23560032276402,
36.9296945801064));
#192848=CARTESIAN_POINT('Ctrl Pts',(-2.79340590288101,6.16612983241687,
36.938134789564));
#192849=CARTESIAN_POINT('Ctrl Pts',(-2.95557068972406,6.09007077653584,
36.9465749990216));
#192850=CARTESIAN_POINT('Ctrl Pts',(-3.1145591219573,6.00764600120818,36.9550152084792));
#192851=CARTESIAN_POINT('Ctrl Pts',(-3.27342709689875,5.92528367485918,
36.9634490232278));
#192852=CARTESIAN_POINT('Ctrl Pts',(-3.42912321954626,5.83656539627821,
36.9718828379763));
#192853=CARTESIAN_POINT('Ctrl Pts',(-3.5811261498254,5.74176144567472,36.9803166527248));
#192854=CARTESIAN_POINT('Ctrl Pts',(-3.73303728230423,5.647014749192,36.9887453741134));
#192855=CARTESIAN_POINT('Ctrl Pts',(-3.88125938678123,5.54618988389685,
36.9971740955019));
#192856=CARTESIAN_POINT('Ctrl Pts',(-4.02529678981785,5.43960244446983,
37.0056028168905));
#192857=CARTESIAN_POINT('Ctrl Pts',(-4.16926932369352,5.33306300811436,
37.0140277422922));
#192858=CARTESIAN_POINT('Ctrl Pts',(-4.30906064625791,5.22076637030717,
37.0224526676939));
#192859=CARTESIAN_POINT('Ctrl Pts',(-4.44420476297629,5.10307094059438,
37.0308775930957));
#192860=CARTESIAN_POINT('Ctrl Pts',(-4.57930875085604,4.98541045861756,
37.0393000168534));
#192861=CARTESIAN_POINT('Ctrl Pts',(-4.70976803352087,4.86235460041507,
37.0477224406111));
#192862=CARTESIAN_POINT('Ctrl Pts',(-4.83515006055934,4.73430173223814,
37.0561448643688));
#192863=CARTESIAN_POINT('Ctrl Pts',(-4.96053405949648,4.60624685015789,
37.064567420587));
#192864=CARTESIAN_POINT('Ctrl Pts',(-5.08084040525924,4.47319503464877,
37.0729899768052));
#192865=CARTESIAN_POINT('Ctrl Pts',(-5.19567329169468,4.33558162718344,
37.0814125330234));
#192866=CARTESIAN_POINT('Ctrl Pts',(-5.3105100572068,4.1979635711111,37.0898353737571));
#192867=CARTESIAN_POINT('Ctrl Pts',(-5.41987278087791,4.05578387184934,
37.0982582144909));
#192868=CARTESIAN_POINT('Ctrl Pts',(-5.52340576530313,3.90951119090561,
37.1066810552246));
#192869=CARTESIAN_POINT('Ctrl Pts',(-5.62695670144184,3.76321314755901,
37.1151053564052));
#192870=CARTESIAN_POINT('Ctrl Pts',(-5.72467569033827,3.61282097988212,
37.1235296575859));
#192871=CARTESIAN_POINT('Ctrl Pts',(-5.81625000737054,3.45883287421671,
37.1319539587665));
#192872=CARTESIAN_POINT('Ctrl Pts',(-5.90785299129355,3.30479656333018,
37.1403808971333));
#192873=CARTESIAN_POINT('Ctrl Pts',(-5.99330729786934,3.14716235671892,
37.1488078355001));
#192874=CARTESIAN_POINT('Ctrl Pts',(-6.07234567358564,2.98645392070358,
37.1572347738669));
#192875=CARTESIAN_POINT('Ctrl Pts',(-6.15145511473691,2.82560098760307,
37.1656692891105));
#192876=CARTESIAN_POINT('Ctrl Pts',(-6.22413695084444,2.66166860156118,
37.1741038043542));
#192877=CARTESIAN_POINT('Ctrl Pts',(-6.29017122704871,2.4952023834568,37.1825383195978));
#192878=CARTESIAN_POINT('Ctrl Pts',(-6.35623739837415,2.32865576074286,
37.1909769087846));
#192879=CARTESIAN_POINT('Ctrl Pts',(-6.41564949081724,2.15957317792961,
37.1994154979714));
#192880=CARTESIAN_POINT('Ctrl Pts',(-6.46823697818444,1.98851688301797,
37.2078540871582));
#192881=CARTESIAN_POINT('Ctrl Pts',(-6.52088324646486,1.81726938586923,
37.2163021087785));
#192882=CARTESIAN_POINT('Ctrl Pts',(-6.56668957669043,1.64404408951035,
37.2247501303988));
#192883=CARTESIAN_POINT('Ctrl Pts',(-6.6055359535606,1.46941613105964,37.2331981520191));
#192884=CARTESIAN_POINT('Ctrl Pts',(-6.6276156107538,1.37016040196483,37.2379998719313));
#192885=CARTESIAN_POINT('Ctrl Pts',(-6.64744772074405,1.27045170198658,
37.2428015918436));
#192886=CARTESIAN_POINT('Ctrl Pts',(-6.66501768919741,1.17039660059555,
37.2476033117559));
#192887=CARTESIAN_POINT('Ctrl Pts',(-6.70147283283432,0.962796734807662,
37.2575661861669));
#192888=CARTESIAN_POINT('Ctrl Pts',(-6.72825461317304,0.753321225376306,
37.2675290605779));
#192889=CARTESIAN_POINT('Ctrl Pts',(-6.74519660546739,0.542781497097296,
37.2774919349889));
#192890=CARTESIAN_POINT('Ctrl Pts',(-6.75955362491231,0.364365469022645,
37.2859346953892));
#192891=CARTESIAN_POINT('Ctrl Pts',(-6.76684520655625,0.18518548270118,
37.2943774557896));
#192892=CARTESIAN_POINT('Ctrl Pts',(-6.7669975608574,0.00574555045427647,
37.3028202161899));
#192893=CARTESIAN_POINT('Ctrl Pts',(-6.76699756085807,0.00574554966948139,
37.3028202162268));
#192894=CARTESIAN_POINT('Ctrl Pts',(-6.76713851673575,-0.160269563827458,
37.3106313305565));
#192895=CARTESIAN_POINT('Ctrl Pts',(-6.76116605585226,-0.326516156793914,
37.3184424448862));
#192896=CARTESIAN_POINT('Ctrl Pts',(-6.749055763498,-0.492478731717873,
37.3262535592158));
#192897=CARTESIAN_POINT('Ctrl Pts',(-6.73695361445242,-0.658329708635924,
37.3340594211277));
#192898=CARTESIAN_POINT('Ctrl Pts',(-6.71872187055446,-0.823896656406961,
37.3418652830396));
#192899=CARTESIAN_POINT('Ctrl Pts',(-6.69438819322006,-0.988663602281313,
37.3496711449514));
#192900=CARTESIAN_POINT('Ctrl Pts',(-6.6700641320408,-1.15336543574001,
37.3574739221516));
#192901=CARTESIAN_POINT('Ctrl Pts',(-6.63964298988069,-1.31726750716917,
37.3652766993517));
#192902=CARTESIAN_POINT('Ctrl Pts',(-6.60320428531312,-1.47985883327513,
37.3730794765519));
#192903=CARTESIAN_POINT('Ctrl Pts',(-6.56676827782901,-1.64243812485955,
37.3808816762139));
#192904=CARTESIAN_POINT('Ctrl Pts',(-6.524315674495,-1.80370647872397,37.3886838758759));
#192905=CARTESIAN_POINT('Ctrl Pts',(-6.47597707366099,-1.96316324879446,
37.3964860755379));
#192906=CARTESIAN_POINT('Ctrl Pts',(-6.45517750550536,-2.03177574273791,
37.3998432762189));
#192907=CARTESIAN_POINT('Ctrl Pts',(-6.43328878854922,-2.10005298722402,
37.4032004768998));
#192908=CARTESIAN_POINT('Ctrl Pts',(-6.410324172489,-2.16795595056801,37.4065576775807));
#192909=CARTESIAN_POINT('Ctrl Pts',(-6.34972450734084,-2.34714017165063,
37.4154167517565));
#192910=CARTESIAN_POINT('Ctrl Pts',(-6.28166738932326,-2.52360603214291,
37.4242758259324));
#192911=CARTESIAN_POINT('Ctrl Pts',(-6.20642940907034,-2.69676157459772,
37.4331349001083));
#192912=CARTESIAN_POINT('Ctrl Pts',(-6.13105007179007,-2.8702424414787,
37.4420106187021));
#192913=CARTESIAN_POINT('Ctrl Pts',(-6.04846301380922,-3.04040032340966,
37.450886337296));
#192914=CARTESIAN_POINT('Ctrl Pts',(-5.95899099669742,-3.2066673200192,
37.4597620558899));
#192915=CARTESIAN_POINT('Ctrl Pts',(-5.86926365172822,-3.37340879565996,
37.4686631032768));
#192916=CARTESIAN_POINT('Ctrl Pts',(-5.77261215341232,-3.53623693664242,
37.4775641506638));
#192917=CARTESIAN_POINT('Ctrl Pts',(-5.66940455709463,-3.69460971795327,
37.4864651980508));
#192918=CARTESIAN_POINT('Ctrl Pts',(-5.56605664863431,-3.85319780923227,
37.4953783465337));
#192919=CARTESIAN_POINT('Ctrl Pts',(-5.45613498466277,-4.00731822777013,
37.5042914950167));
#192920=CARTESIAN_POINT('Ctrl Pts',(-5.34004914288942,-4.15646053169352,
37.5132046434997));
#192921=CARTESIAN_POINT('Ctrl Pts',(-5.22370555880406,-4.30593397231406,
37.5221375816095));
#192922=CARTESIAN_POINT('Ctrl Pts',(-5.10117058197372,-4.45040698533129,
37.5310705197194));
#192923=CARTESIAN_POINT('Ctrl Pts',(-4.97289393103948,-4.58940246117408,
37.5400034578293));
#192924=CARTESIAN_POINT('Ctrl Pts',(-4.85079315868725,-4.72170600067458,
37.548506319688));
#192925=CARTESIAN_POINT('Ctrl Pts',(-4.72349069077873,-4.84904688630267,
37.5570091815467));
#192926=CARTESIAN_POINT('Ctrl Pts',(-4.59140331684061,-4.97104662843802,
37.5655120434054));
#192927=CARTESIAN_POINT('Ctrl Pts',(-4.46366773556069,-5.08902692824291,
37.5737347672712));
#192928=CARTESIAN_POINT('Ctrl Pts',(-4.33121184980721,-5.20223762451192,
37.5819574911371));
#192929=CARTESIAN_POINT('Ctrl Pts',(-4.19442656922371,-5.31028010140616,
37.590180215003));
#192930=CARTESIAN_POINT('Ctrl Pts',(-4.05778607122618,-5.41820821899849,
37.5983942353942));
#192931=CARTESIAN_POINT('Ctrl Pts',(-3.91682558282514,-5.52097879000792,
37.6066082557854));
#192932=CARTESIAN_POINT('Ctrl Pts',(-3.77197211665981,-5.61823062459534,
37.6148222761767));
#192933=CARTESIAN_POINT('Ctrl Pts',(-3.62724289050052,-5.71539904682933,
37.6230292514486));
#192934=CARTESIAN_POINT('Ctrl Pts',(-3.47862763259262,-5.80705796077186,
37.6312362267206));
#192935=CARTESIAN_POINT('Ctrl Pts',(-3.32658569574698,-5.89288695028605,
37.6394432019925));
#192936=CARTESIAN_POINT('Ctrl Pts',(-3.17464364741953,-5.97865955186702,
37.6476447854455));
#192937=CARTESIAN_POINT('Ctrl Pts',(-3.01927971565959,-6.0586096824938,
37.6558463688985));
#192938=CARTESIAN_POINT('Ctrl Pts',(-2.86098151838054,-6.13246066041071,
37.6640479523515));
#192939=CARTESIAN_POINT('Ctrl Pts',(-2.70275555363839,-6.20627793962745,
37.6722457933666));
#192940=CARTESIAN_POINT('Ctrl Pts',(-2.541598315259,-6.2740014593689,37.6804436343817));
#192941=CARTESIAN_POINT('Ctrl Pts',(-2.37802133895028,-6.33540081695682,
37.6886414753967));
#192942=CARTESIAN_POINT('Ctrl Pts',(-2.21445879779948,-6.39679475624295,
37.6968385929779));
#192943=CARTESIAN_POINT('Ctrl Pts',(-2.04847727662655,-6.45186551101317,
37.705035710559));
#192944=CARTESIAN_POINT('Ctrl Pts',(-1.88060792016194,-6.50043097422196,
37.7132328281402));
#192945=CARTESIAN_POINT('Ctrl Pts',(-1.71274043143095,-6.54899589708585,
37.7214298545193));
#192946=CARTESIAN_POINT('Ctrl Pts',(-1.54298549364252,-6.59105557179551,
37.7296268808984));
#192947=CARTESIAN_POINT('Ctrl Pts',(-1.37188891178661,-6.62647793429639,
37.7378239072775));
#192948=CARTESIAN_POINT('Ctrl Pts',(-1.20076312302135,-6.6619063435442,
37.7460223329236));
#192949=CARTESIAN_POINT('Ctrl Pts',(-1.02829558529569,-6.69069511052739,
37.7542207585697));
#192950=CARTESIAN_POINT('Ctrl Pts',(-0.855041831038226,-6.71276340020821,
37.7624191842158));
#192951=CARTESIAN_POINT('Ctrl Pts',(-0.681726998503361,-6.73483946976729,
37.7706205001065));
#192952=CARTESIAN_POINT('Ctrl Pts',(-0.507625753050677,-6.75019029721376,
37.7788218159972));
#192953=CARTESIAN_POINT('Ctrl Pts',(-0.333298328129745,-6.75878696398,37.7870231318878));
#192954=CARTESIAN_POINT('Ctrl Pts',(-0.158772373453413,-6.76739342091064,
37.7952337877044));
#192955=CARTESIAN_POINT('Ctrl Pts',(0.0159799165223041,-6.76923033250532,
37.803444443521));
#192956=CARTESIAN_POINT('Ctrl Pts',(0.190397662384689,-6.76432093636593,
37.8116550993376));
#192957=CARTESIAN_POINT('Ctrl Pts',(0.364918188399296,-6.75940864723833,
37.8198705934948));
#192958=CARTESIAN_POINT('Ctrl Pts',(0.539103419896524,-6.74774214989725,
37.8280860876519));
#192959=CARTESIAN_POINT('Ctrl Pts',(0.712398133414095,-6.72939654794604,
37.8363015818091));
#192960=CARTESIAN_POINT('Ctrl Pts',(0.885961716868385,-6.71102248245584,
37.8445298224566));
#192961=CARTESIAN_POINT('Ctrl Pts',(1.05863166637931,-6.68594865502462,
37.8527580631041));
#192962=CARTESIAN_POINT('Ctrl Pts',(1.22986215007908,-6.65430147286722,
37.8609863037516));
#192963=CARTESIAN_POINT('Ctrl Pts',(1.38548332263012,-6.62553923679303,
37.8684644608527));
#192964=CARTESIAN_POINT('Ctrl Pts',(1.5399154731124,-6.59134815720409,37.8759426179537));
#192965=CARTESIAN_POINT('Ctrl Pts',(1.69276100623654,-6.55185845205504,
37.8834207750548));
#192966=CARTESIAN_POINT('Ctrl Pts',(1.85768905647565,-6.50924706563356,
37.8914900842773));
#192967=CARTESIAN_POINT('Ctrl Pts',(2.02130939409484,-6.46032589831497,
37.8995593934999));
#192968=CARTESIAN_POINT('Ctrl Pts',(2.18309000201918,-6.40518594914183,
37.9076287027224));
#192969=CARTESIAN_POINT('Ctrl Pts',(2.34466882555505,-6.3501147744718,37.9156879473232));
#192970=CARTESIAN_POINT('Ctrl Pts',(2.50441213640657,-6.28884037018999,
37.9237471919239));
#192971=CARTESIAN_POINT('Ctrl Pts',(2.66179785138195,-6.22150473747135,
37.9318064365247));
#192972=CARTESIAN_POINT('Ctrl Pts',(2.81902180163089,-6.15423831389414,
37.939857397645));
#192973=CARTESIAN_POINT('Ctrl Pts',(2.97389263804433,-6.08092320497609,
37.9479083587652));
#192974=CARTESIAN_POINT('Ctrl Pts',(3.12590330240368,-6.00175120644148,
37.9559593198855));
#192975=CARTESIAN_POINT('Ctrl Pts',(3.27779103519237,-5.92264323458667,
37.9640037701646));
#192976=CARTESIAN_POINT('Ctrl Pts',(3.42682287036525,-5.8376879717809,37.9720482204437));
#192977=CARTESIAN_POINT('Ctrl Pts',(3.57251171777222,-5.74712528368576,
37.9800926707228));
#192978=CARTESIAN_POINT('Ctrl Pts',(3.71811463601211,-5.65661601063574,
37.988132376281));
#192979=CARTESIAN_POINT('Ctrl Pts',(3.86037817552832,-5.56050609270054,
37.9961720818393));
#192980=CARTESIAN_POINT('Ctrl Pts',(3.99883995613077,-5.45908124186223,
38.0042117873975));
#192981=CARTESIAN_POINT('Ctrl Pts',(4.14029036024209,-5.35546718984306,
38.012425025702));
#192982=CARTESIAN_POINT('Ctrl Pts',(4.27777266816484,-5.24630634100549,
38.0206382640064));
#192983=CARTESIAN_POINT('Ctrl Pts',(4.41082489430424,-5.1319501899167,38.0288515023109));
#192984=CARTESIAN_POINT('Ctrl Pts',(4.54102401210514,-5.02004623746973,
38.0368886198591));
#192985=CARTESIAN_POINT('Ctrl Pts',(4.66698082876847,-4.90316779802486,
38.0449257374072));
#192986=CARTESIAN_POINT('Ctrl Pts',(4.78829609200327,-4.78168480091549,
38.0529628549554));
#192987=CARTESIAN_POINT('Ctrl Pts',(4.90962418962153,-4.66018895167748,
38.0610008227795));
#192988=CARTESIAN_POINT('Ctrl Pts',(5.02630949196048,-4.53408783912808,
38.0690387906036));
#192989=CARTESIAN_POINT('Ctrl Pts',(5.13799005438748,-4.40378782425032,
38.0770767584278));
#192990=CARTESIAN_POINT('Ctrl Pts',(5.24970455994399,-4.2734482072235,38.0851171692355));
#192991=CARTESIAN_POINT('Ctrl Pts',(5.3564110548689,-4.13890743117581,38.0931575800432));
#192992=CARTESIAN_POINT('Ctrl Pts',(5.4577883843241,-4.00060432334128,38.1011979908509));
#192993=CARTESIAN_POINT('Ctrl Pts',(5.56299720505791,-3.85707413806921,
38.1095422838387));
#192994=CARTESIAN_POINT('Ctrl Pts',(5.66246590187949,-3.70949203405389,
38.1178865768265));
#192995=CARTESIAN_POINT('Ctrl Pts',(5.75588593671061,-3.55837969918572,
38.1262308698143));
#192996=CARTESIAN_POINT('Ctrl Pts',(5.84606277589728,-3.41251342173075,
38.1342854800299));
#192997=CARTESIAN_POINT('Ctrl Pts',(5.93060376618149,-3.26335827140706,
38.1423400902454));
#192998=CARTESIAN_POINT('Ctrl Pts',(6.00927943682381,-3.11140637817796,
38.150394700461));
#192999=CARTESIAN_POINT('Ctrl Pts',(6.08801466606033,-2.95933945521893,
38.1584554081303));
#193000=CARTESIAN_POINT('Ctrl Pts',(6.1608755769082,-2.80447190949692,38.1665161157995));
#193001=CARTESIAN_POINT('Ctrl Pts',(6.22768146353394,-2.64731422176435,
38.1745768234688));
#193002=CARTESIAN_POINT('Ctrl Pts',(6.29458154245726,-2.4899349511079,38.182648896253));
#193003=CARTESIAN_POINT('Ctrl Pts',(6.35540943224122,-2.33025944187843,
38.1907209690371));
#193004=CARTESIAN_POINT('Ctrl Pts',(6.41003453196383,-2.16881218620499,
38.1987930418213));
#193005=CARTESIAN_POINT('Ctrl Pts',(6.4157560961312,-2.15190181281123,38.1996385301157));
#193006=CARTESIAN_POINT('Ctrl Pts',(6.42140965616103,-2.13497200937217,
38.2004840184101));
#193007=CARTESIAN_POINT('Ctrl Pts',(6.42699509465927,-2.11802338354082,
38.2013295067046));
#193008=CARTESIAN_POINT('Ctrl Pts',(6.48204378534905,-1.9509819486917,38.2096624287513));
#193009=CARTESIAN_POINT('Ctrl Pts',(6.53064681609766,-1.78157854108172,
38.217995350798));
#193010=CARTESIAN_POINT('Ctrl Pts',(6.572600477329,-1.61034529384682,38.2263282728447));
#193011=CARTESIAN_POINT('Ctrl Pts',(6.61450455950663,-1.43931440278568,
38.2346513473984));
#193012=CARTESIAN_POINT('Ctrl Pts',(6.64977484370763,-1.26645831488991,
38.242974421952));
#193013=CARTESIAN_POINT('Ctrl Pts',(6.67825666034375,-1.09232640660853,
38.2512974965056));
#193014=CARTESIAN_POINT('Ctrl Pts',(6.70671004638049,-0.918368317103827,
38.2596122629516));
#193015=CARTESIAN_POINT('Ctrl Pts',(6.72838840952356,-0.743137285736674,
38.2679270293975));
#193016=CARTESIAN_POINT('Ctrl Pts',(6.74318756583585,-0.567195250294588,
38.2762417958435));
#193017=CARTESIAN_POINT('Ctrl Pts',(6.75797466426776,-0.391396566809408,
38.2845497876831));
#193018=CARTESIAN_POINT('Ctrl Pts',(6.7658936951739,-0.214888378786781,
38.2928577795226));
#193019=CARTESIAN_POINT('Ctrl Pts',(6.76689195072957,-0.038240386391329,
38.3011657713622));
#193020=CARTESIAN_POINT('Ctrl Pts',(6.76788957595228,0.138296064372749,
38.3094685172494));
#193021=CARTESIAN_POINT('Ctrl Pts',(6.76197513278595,0.314971796623375,
38.3177712631365));
#193022=CARTESIAN_POINT('Ctrl Pts',(6.74914791589627,0.49121421941257,38.3260740090236));
#193023=CARTESIAN_POINT('Ctrl Pts',(6.73632594108143,0.667384617538833,
38.3343733618431));
#193024=CARTESIAN_POINT('Ctrl Pts',(6.71659684684124,0.843121712586421,
38.3426727146625));
#193025=CARTESIAN_POINT('Ctrl Pts',(6.69001199513991,1.01785485452697,38.350972067482));
#193026=CARTESIAN_POINT('Ctrl Pts',(6.66343279759041,1.19255083366045,38.3592696551683));
#193027=CARTESIAN_POINT('Ctrl Pts',(6.63000079975274,1.36624294132703,38.3675672428547));
#193028=CARTESIAN_POINT('Ctrl Pts',(6.58981903812744,1.53836733088464,38.375864830541));
#193029=CARTESIAN_POINT('Ctrl Pts',(6.54963914527426,1.71048371528651,38.3841620323235));
#193030=CARTESIAN_POINT('Ctrl Pts',(6.50271019343199,1.88103218813741,38.3924592341059));
#193031=CARTESIAN_POINT('Ctrl Pts',(6.44918602738049,2.04946055932782,38.4007564358883));
#193032=CARTESIAN_POINT('Ctrl Pts',(6.3956554566342,2.21790908463531,38.4090546305128));
#193033=CARTESIAN_POINT('Ctrl Pts',(6.33552820507133,2.38423667141169,38.4173528251373));
#193034=CARTESIAN_POINT('Ctrl Pts',(6.26900759336808,2.54790753252417,38.4256510197618));
#193035=CARTESIAN_POINT('Ctrl Pts',(6.20244019694276,2.71169350526221,38.4339550506034));
#193036=CARTESIAN_POINT('Ctrl Pts',(6.12947058658925,2.8728186959976,38.4422590814449));
#193037=CARTESIAN_POINT('Ctrl Pts',(6.05035009713727,3.03076767537056,38.4505631122865));
#193038=CARTESIAN_POINT('Ctrl Pts',(5.97120083729755,3.18877408933993,38.4588701627023));
#193039=CARTESIAN_POINT('Ctrl Pts',(5.88589640287763,3.3436016822627,38.467177213118));
#193040=CARTESIAN_POINT('Ctrl Pts',(5.79473359074778,3.49476059441263,38.4754842635338));
#193041=CARTESIAN_POINT('Ctrl Pts',(5.70347331018626,3.64608112095067,38.4838001955884));
#193042=CARTESIAN_POINT('Ctrl Pts',(5.60634232328536,3.79372483537982,38.492116127643));
#193043=CARTESIAN_POINT('Ctrl Pts',(5.50368078018955,3.93723086315397,38.5004320596976));
#193044=CARTESIAN_POINT('Ctrl Pts',(5.42629232840349,4.04540875505498,38.5067007859164));
#193045=CARTESIAN_POINT('Ctrl Pts',(5.34576205238126,4.15123602449831,38.5129695121352));
#193046=CARTESIAN_POINT('Ctrl Pts',(5.26225041479912,4.25452812564995,38.519238238354));
#193047=CARTESIAN_POINT('Ctrl Pts',(5.1496660934682,4.39377903059797,38.5276892795189));
#193048=CARTESIAN_POINT('Ctrl Pts',(5.03145549337433,4.52867658034508,38.5361403206837));
#193049=CARTESIAN_POINT('Ctrl Pts',(4.90798055367651,4.65875690337382,38.5445913618486));
#193050=CARTESIAN_POINT('Ctrl Pts',(4.78461598664243,4.78872094927146,38.5530348487362));
#193051=CARTESIAN_POINT('Ctrl Pts',(4.6559966870466,4.91387611205978,38.5614783356238));
#193052=CARTESIAN_POINT('Ctrl Pts',(4.52252456739381,5.03379186471982,38.5699218225115));
#193053=CARTESIAN_POINT('Ctrl Pts',(4.38917673031639,5.15359595781675,38.5783574472456));
#193054=CARTESIAN_POINT('Ctrl Pts',(4.25098533229574,5.26817015116777,38.5867930719797));
#193055=CARTESIAN_POINT('Ctrl Pts',(4.10838885729898,5.37712097662137,38.5952286967138));
#193056=CARTESIAN_POINT('Ctrl Pts',(3.96587158772197,5.48601128518028,38.6036596358678));
#193057=CARTESIAN_POINT('Ctrl Pts',(3.81895438078495,5.58928425063585,38.6120905750219));
#193058=CARTESIAN_POINT('Ctrl Pts',(3.66810911342265,5.68658636899377,38.620521514176));
#193059=CARTESIAN_POINT('Ctrl Pts',(3.51733768316777,5.78384085902969,38.6289483264776));
#193060=CARTESIAN_POINT('Ctrl Pts',(3.36264230529054,5.8751301513764,38.6373751387792));
#193061=CARTESIAN_POINT('Ctrl Pts',(3.20452439648501,5.96014365534358,38.6458019510809));
#193062=CARTESIAN_POINT('Ctrl Pts',(3.16955046628708,5.97894770085678,38.6476658686311));
#193063=CARTESIAN_POINT('Ctrl Pts',(3.13440919851847,5.99744487709346,38.6495297861813));
#193064=CARTESIAN_POINT('Ctrl Pts',(3.0991061983213,6.01563211736942,38.6513937037315));
#193065=CARTESIAN_POINT('Origin',(0.,0.,4.30282021618968));
#193066=CARTESIAN_POINT('',(3.09910619832129,6.01563211736942,41.0459058825584));
#193067=CARTESIAN_POINT('',(3.09910619832134,6.0156321173694,40.651395695404));
#193068=CARTESIAN_POINT('',(3.09910619832133,6.0156321173694,4.30282021618968));
#193069=CARTESIAN_POINT('',(-6.76699683428592,-0.00454281799175943,39.69717978381));
#193070=CARTESIAN_POINT('Ctrl Pts',(-6.76699342768056,-0.00943131635262364,
39.69717978381));
#193071=CARTESIAN_POINT('Ctrl Pts',(-6.76668020929751,-0.234166301401713,
39.7077500331228));
#193072=CARTESIAN_POINT('Ctrl Pts',(-6.7551688358066,-0.458328916408552,
39.7183202824357));
#193073=CARTESIAN_POINT('Ctrl Pts',(-6.73264806908026,-0.680983830872519,
39.7288905317485));
#193074=CARTESIAN_POINT('Ctrl Pts',(-6.70948849224833,-0.909954436589295,
39.7397606101995));
#193075=CARTESIAN_POINT('Ctrl Pts',(-6.67468607867271,-1.1373308841783,
39.7506306886506));
#193076=CARTESIAN_POINT('Ctrl Pts',(-6.62849165631605,-1.36212604488297,
39.7615007671016));
#193077=CARTESIAN_POINT('Ctrl Pts',(-6.62183218103256,-1.39453294035194,
39.7630678181671));
#193078=CARTESIAN_POINT('Ctrl Pts',(-6.61493602539058,-1.42688623496732,
39.7646348692326));
#193079=CARTESIAN_POINT('Ctrl Pts',(-6.60780401710258,-1.45918301510227,
39.7662019202981));
#193080=CARTESIAN_POINT('Ctrl Pts',(-6.56987898044705,-1.63092378165966,
39.7745348423448));
#193081=CARTESIAN_POINT('Ctrl Pts',(-6.52520557100435,-1.80140561528577,
39.7828677643916));
#193082=CARTESIAN_POINT('Ctrl Pts',(-6.47388023008809,-1.97006694466829,
39.7912006864383));
#193083=CARTESIAN_POINT('Ctrl Pts',(-6.42261554327828,-2.13852895726023,
39.7995237609919));
#193084=CARTESIAN_POINT('Ctrl Pts',(-6.36471468509409,-2.30517442132003,
39.8078468355455));
#193085=CARTESIAN_POINT('Ctrl Pts',(-6.300325068815,-2.46945196901282,39.8161699100991));
#193086=CARTESIAN_POINT('Ctrl Pts',(-6.23599972636393,-2.63356553456907,
39.8244846765451));
#193087=CARTESIAN_POINT('Ctrl Pts',(-6.16519865644741,-2.79531557098695,
39.832799442991));
#193088=CARTESIAN_POINT('Ctrl Pts',(-6.08811909765784,-2.95416567794258,
39.841114209437));
#193089=CARTESIAN_POINT('Ctrl Pts',(-6.01110234083374,-3.11288635889876,
39.8494222012766));
#193090=CARTESIAN_POINT('Ctrl Pts',(-5.92781743946158,-3.26871150671735,
39.8577301931161));
#193091=CARTESIAN_POINT('Ctrl Pts',(-5.83850985964285,-3.42112432087073,
39.8660381849556));
#193092=CARTESIAN_POINT('Ctrl Pts',(-5.74925867170873,-3.57344089631911,
39.8743409308427));
#193093=CARTESIAN_POINT('Ctrl Pts',(-5.65399255952059,-3.72234913273447,
39.8826436767298));
#193094=CARTESIAN_POINT('Ctrl Pts',(-5.55300318273677,-3.86735628724784,
39.8909464226169));
#193095=CARTESIAN_POINT('Ctrl Pts',(-5.45205507709289,-4.01230418195826,
39.8992457754363));
#193096=CARTESIAN_POINT('Ctrl Pts',(-5.34538856584358,-4.15335388636473,
39.9075451282557));
#193097=CARTESIAN_POINT('Ctrl Pts',(-5.23333909169961,-4.2900409032186,
39.9158444810752));
#193098=CARTESIAN_POINT('Ctrl Pts',(-5.12131344859866,-4.42669884903752,
39.9241420687615));
#193099=CARTESIAN_POINT('Ctrl Pts',(-5.00390734386614,-4.55899568693043,
39.9324396564479));
#193100=CARTESIAN_POINT('Ctrl Pts',(-4.88149718358398,-4.68649914612835,
39.9407372441342));
#193101=CARTESIAN_POINT('Ctrl Pts',(-4.75909271634931,-4.8139966753998,
39.9490344459166));
#193102=CARTESIAN_POINT('Ctrl Pts',(-4.63168489837398,-4.93670101938003,
39.9573316476991));
#193103=CARTESIAN_POINT('Ctrl Pts',(-4.49968787701916,-5.05421586493956,
39.9656288494815));
#193104=CARTESIAN_POINT('Ctrl Pts',(-4.36767506091743,-5.17174477231069,
39.973927044106));
#193105=CARTESIAN_POINT('Ctrl Pts',(-4.23107220743187,-5.28408271302187,
39.9822252387306));
#193106=CARTESIAN_POINT('Ctrl Pts',(-4.09032763674328,-5.39087273306412,
39.9905234333551));
#193107=CARTESIAN_POINT('Ctrl Pts',(-3.94948407875723,-5.49773785977248,
39.9988274641967));
#193108=CARTESIAN_POINT('Ctrl Pts',(-3.80449326047922,-5.59904705846489,
40.0071314950383));
#193109=CARTESIAN_POINT('Ctrl Pts',(-3.65583439928966,-5.69448538895047,
40.0154355258798));
#193110=CARTESIAN_POINT('Ctrl Pts',(-3.50712148164643,-5.78995842343991,
40.0237425762956));
#193111=CARTESIAN_POINT('Ctrl Pts',(-3.35473815937241,-5.87955615306873,
40.0320496267113));
#193112=CARTESIAN_POINT('Ctrl Pts',(-3.19918969215561,-5.96300883058254,
40.040356677127));
#193113=CARTESIAN_POINT('Ctrl Pts',(-3.04347491737529,-6.046550733093,40.0486726091817));
#193114=CARTESIAN_POINT('Ctrl Pts',(-2.88458854646557,-6.12393429831167,
40.0569885412363));
#193115=CARTESIAN_POINT('Ctrl Pts',(-2.72305832466099,-6.19493683264765,
40.0653044732909));
#193116=CARTESIAN_POINT('Ctrl Pts',(-2.60129341245105,-6.24846005117306,
40.0715731995099));
#193117=CARTESIAN_POINT('Ctrl Pts',(-2.47802660277811,-6.29835824701142,
40.0778419257288));
#193118=CARTESIAN_POINT('Ctrl Pts',(-2.35349007810612,-6.34455462993708,
40.0841106519477));
#193119=CARTESIAN_POINT('Ctrl Pts',(-2.18561433068993,-6.4068275441042,
40.0925609206711));
#193120=CARTESIAN_POINT('Ctrl Pts',(-2.01512298024384,-6.46248632007681,
40.1010111893944));
#193121=CARTESIAN_POINT('Ctrl Pts',(-1.84256388736499,-6.51131686534901,
40.1094614581177));
#193122=CARTESIAN_POINT('Ctrl Pts',(-1.67015708373984,-6.56010431600838,
40.1179042691923));
#193123=CARTESIAN_POINT('Ctrl Pts',(-1.49568649251017,-6.60207545729679,
40.1263470802668));
#193124=CARTESIAN_POINT('Ctrl Pts',(-1.31971734153615,-6.63706525042874,
40.1347898913413));
#193125=CARTESIAN_POINT('Ctrl Pts',(-1.14387953065585,-6.67202892783142,
40.143226400859));
#193126=CARTESIAN_POINT('Ctrl Pts',(-0.96654571384302,-6.7000215799563,
40.1516629103767));
#193127=CARTESIAN_POINT('Ctrl Pts',(-0.788293969984889,-6.72092862756967,
40.1600994198945));
#193128=CARTESIAN_POINT('Ctrl Pts',(-0.610169774840731,-6.74182071506552,
40.1685298926357));
#193129=CARTESIAN_POINT('Ctrl Pts',(-0.431129291323293,-6.75563727271,40.1769603653769));
#193130=CARTESIAN_POINT('Ctrl Pts',(-0.251758636464925,-6.762315179653,
40.1853908381181));
#193131=CARTESIAN_POINT('Ctrl Pts',(-0.0724650925651713,-6.76899021578189,
40.1938176866219));
#193132=CARTESIAN_POINT('Ctrl Pts',(0.107158008968874,-6.76853270682738,
40.2022445351258));
#193133=CARTESIAN_POINT('Ctrl Pts',(0.286520948093409,-6.76093149989731,
40.2106713836296));
#193134=CARTESIAN_POINT('Ctrl Pts',(0.465828524284084,-6.75333263918836,
40.2190956310662));
#193135=CARTESIAN_POINT('Ctrl Pts',(0.644875767309722,-6.73859449182824,
40.2275198785029));
#193136=CARTESIAN_POINT('Ctrl Pts',(0.823074106626459,-6.71675799884149,
40.2359441259395));
#193137=CARTESIAN_POINT('Ctrl Pts',(0.873283580672546,-6.71060531059489,
40.2383177565505));
#193138=CARTESIAN_POINT('Ctrl Pts',(0.923425681025626,-6.70388940388024,
40.2406913871614));
#193139=CARTESIAN_POINT('Ctrl Pts',(0.973487306479602,-6.69661193919157,
40.2430650177724));
#193140=CARTESIAN_POINT('Ctrl Pts',(1.15526377209883,-6.67018707188496,
40.2516837987096));
#193141=CARTESIAN_POINT('Ctrl Pts',(1.33589730369004,-6.63636620633356,
40.2603025796469));
#193142=CARTESIAN_POINT('Ctrl Pts',(1.51478534096077,-6.59527970375862,
40.2689213605841));
#193143=CARTESIAN_POINT('Ctrl Pts',(1.69378083518798,-6.55416852077135,
40.2775453187706));
#193144=CARTESIAN_POINT('Ctrl Pts',(1.87102844613696,-6.50578305878432,
40.2861692769572));
#193145=CARTESIAN_POINT('Ctrl Pts',(2.04593908903496,-6.45030404275324,
40.2947932351437));
#193146=CARTESIAN_POINT('Ctrl Pts',(2.22716865667085,-6.39282075916574,
40.3037287475148));
#193147=CARTESIAN_POINT('Ctrl Pts',(2.40588891227613,-6.32772194894361,
40.312664259886));
#193148=CARTESIAN_POINT('Ctrl Pts',(2.5814659768532,-6.25526357640902,40.3215997722571));
#193149=CARTESIAN_POINT('Ctrl Pts',(2.75123802279417,-6.18520085961636,
40.3302398541518));
#193150=CARTESIAN_POINT('Ctrl Pts',(2.91807113745933,-6.10825761238182,
40.3388799360465));
#193151=CARTESIAN_POINT('Ctrl Pts',(3.08141586475482,-6.02471287850611,
40.3475200179412));
#193152=CARTESIAN_POINT('Ctrl Pts',(3.2531384658705,-5.93688317473671,40.3566032455505));
#193153=CARTESIAN_POINT('Ctrl Pts',(3.42100510273873,-5.84175721689526,
40.3656864731598));
#193154=CARTESIAN_POINT('Ctrl Pts',(3.58440980035587,-5.73971213416778,
40.3747697007692));
#193155=CARTESIAN_POINT('Ctrl Pts',(3.74781449797301,-5.6376670514403,40.3838529283785));
#193156=CARTESIAN_POINT('Ctrl Pts',(3.90675695553529,-5.52870309084873,
40.3929361559879));
#193157=CARTESIAN_POINT('Ctrl Pts',(4.06066906516457,-5.41324816937257,
40.4020193835972));
#193158=CARTESIAN_POINT('Ctrl Pts',(4.21392655638789,-5.29828430033433,
40.411063978457));
#193159=CARTESIAN_POINT('Ctrl Pts',(4.36233845402035,-5.17677910252117,
40.4201085733168));
#193160=CARTESIAN_POINT('Ctrl Pts',(4.5053754838023,-5.0491465367875,40.4291531681767));
#193161=CARTESIAN_POINT('Ctrl Pts',(4.64828125459441,-4.92163109402313,
40.438189463197));
#193162=CARTESIAN_POINT('Ctrl Pts',(4.78582182752243,-4.78799966758519,
40.4472257582174));
#193163=CARTESIAN_POINT('Ctrl Pts',(4.91750174242367,-4.64870579981786,
40.4562620532377));
#193164=CARTESIAN_POINT('Ctrl Pts',(5.04894863938934,-4.50965842347277,
40.4652823578255));
#193165=CARTESIAN_POINT('Ctrl Pts',(5.17455542446903,-4.36496878737805,
40.4743026624132));
#193166=CARTESIAN_POINT('Ctrl Pts',(5.29386426519827,-4.21512634942973,
40.4833229670009));
#193167=CARTESIAN_POINT('Ctrl Pts',(5.41302285961901,-4.06547260892428,
40.4923319122672));
#193168=CARTESIAN_POINT('Ctrl Pts',(5.52589918957355,-3.91067920183336,
40.5013408575335));
#193169=CARTESIAN_POINT('Ctrl Pts',(5.63207471618558,-3.75126957059914,
40.5103498027998));
#193170=CARTESIAN_POINT('Ctrl Pts',(5.73800914065386,-3.59222192489072,
40.5193382906586));
#193171=CARTESIAN_POINT('Ctrl Pts',(5.83727300280782,-3.42857917657921,
40.5283267785174));
#193172=CARTESIAN_POINT('Ctrl Pts',(5.92949047881157,-3.26089430397291,
40.5373152663762));
#193173=CARTESIAN_POINT('Ctrl Pts',(6.01039862216227,-3.11377390664147,
40.5452014273915));
#193174=CARTESIAN_POINT('Ctrl Pts',(6.08588322532871,-2.96354258947786,
40.5530875884067));
#193175=CARTESIAN_POINT('Ctrl Pts',(6.15571725662143,-2.81059318588322,
40.560973749422));
#193176=CARTESIAN_POINT('Ctrl Pts',(6.22763496535337,-2.65308014453613,
40.5690952142782));
#193177=CARTESIAN_POINT('Ctrl Pts',(6.29352619185559,-2.49275422514349,
40.5772166791343));
#193178=CARTESIAN_POINT('Ctrl Pts',(6.35317349719531,-2.3301234977003,40.5853381439905));
#193179=CARTESIAN_POINT('Ctrl Pts',(6.4128165488043,-2.16750436822152,40.5934590296667));
#193180=CARTESIAN_POINT('Ctrl Pts',(6.4662164401011,-2.00258110188059,40.6015799153428));
#193181=CARTESIAN_POINT('Ctrl Pts',(6.5132045425492,-1.83588005787863,40.609700801019));
#193182=CARTESIAN_POINT('Ctrl Pts',(6.56019826141917,-1.66915908833511,
40.6178226573733));
#193183=CARTESIAN_POINT('Ctrl Pts',(6.60077856718998,-1.50066027077619,
40.6259445137275));
#193184=CARTESIAN_POINT('Ctrl Pts',(6.63482721003681,-1.33092332346952,
40.6340663700818));
#193185=CARTESIAN_POINT('Ctrl Pts',(6.66890069435223,-1.161062538186,40.6421941520419));
#193186=CARTESIAN_POINT('Ctrl Pts',(6.69643292580591,-0.989962178373673,
40.6503219340021));
#193187=CARTESIAN_POINT('Ctrl Pts',(6.71735701744158,-0.818170948047107,
40.6584497159622));
#193188=CARTESIAN_POINT('Ctrl Pts',(6.73828963277449,-0.646309736358405,
40.6665808088787));
#193189=CARTESIAN_POINT('Ctrl Pts',(6.75260871229353,-0.473757457852254,
40.6747119017951));
#193190=CARTESIAN_POINT('Ctrl Pts',(6.76029942933705,-0.3010658162349,40.6828429947116));
#193191=CARTESIAN_POINT('Ctrl Pts',(6.7679985404768,-0.128185688907929,
40.6909829623761));
#193192=CARTESIAN_POINT('Ctrl Pts',(6.76905483703964,0.0448337396062329,
40.6991229300406));
#193193=CARTESIAN_POINT('Ctrl Pts',(6.76350559395359,0.217442131516707,
40.7072628977052));
#193194=CARTESIAN_POINT('Ctrl Pts',(6.76062751655525,0.30696430667064,40.7114846368857));
#193195=CARTESIAN_POINT('Ctrl Pts',(6.75597346216984,0.39637600283174,40.7157063760662));
#193196=CARTESIAN_POINT('Ctrl Pts',(6.7495540892548,0.485601272881148,40.7199281152467));
#193197=CARTESIAN_POINT('Ctrl Pts',(6.73672031396149,0.66398272562659,40.7283683247043));
#193198=CARTESIAN_POINT('Ctrl Pts',(6.71680114117658,0.841987289132607,
40.7368085341619));
#193199=CARTESIAN_POINT('Ctrl Pts',(6.68983319393488,1.01902936038517,40.7452487436196));
#193200=CARTESIAN_POINT('Ctrl Pts',(6.66288567890855,1.19593729603986,40.7536825583681));
#193201=CARTESIAN_POINT('Ctrl Pts',(6.62890008537371,1.3718838646168,40.7621163731167));
#193202=CARTESIAN_POINT('Ctrl Pts',(6.58796484463954,1.54628852604988,40.7705501878652));
#193203=CARTESIAN_POINT('Ctrl Pts',(6.54705432556735,1.72058786080084,40.7789789092538));
#193204=CARTESIAN_POINT('Ctrl Pts',(6.4992026027077,1.89334682102212,40.7874076306423));
#193205=CARTESIAN_POINT('Ctrl Pts',(6.44454926603385,2.06399461182983,40.7958363520309));
#193206=CARTESIAN_POINT('Ctrl Pts',(6.38992054321726,2.23456554913469,40.8042612774326));
#193207=CARTESIAN_POINT('Ctrl Pts',(6.32849641580291,2.40302689573561,40.8126862028343));
#193208=CARTESIAN_POINT('Ctrl Pts',(6.26046655459002,2.56882220460269,40.8211111282361));
#193209=CARTESIAN_POINT('Ctrl Pts',(6.19245689373339,2.73456828326046,40.8295335519938));
#193210=CARTESIAN_POINT('Ctrl Pts',(6.11784553712781,2.89764959468847,40.8379559757516));
#193211=CARTESIAN_POINT('Ctrl Pts',(6.03687073963793,3.05752852364511,40.8463783995093));
#193212=CARTESIAN_POINT('Ctrl Pts',(5.95589466864763,3.21740996703697,40.8548009557275));
#193213=CARTESIAN_POINT('Ctrl Pts',(5.86855510151997,3.37408862689546,40.8632235119457));
#193214=CARTESIAN_POINT('Ctrl Pts',(5.7751371142008,3.52704980290618,40.8716460681639));
#193215=CARTESIAN_POINT('Ctrl Pts',(5.6817159712043,3.68001614597441,40.8800689088977));
#193216=CARTESIAN_POINT('Ctrl Pts',(5.58221617232746,3.8292644700334,40.8884917496314));
#193217=CARTESIAN_POINT('Ctrl Pts',(5.47696723431399,3.97430735024997,40.8969145903652));
#193218=CARTESIAN_POINT('Ctrl Pts',(5.37170004705555,4.1193753796329,40.9053388915458));
#193219=CARTESIAN_POINT('Ctrl Pts',(5.2606819291352,4.26023624141864,40.9137631927264));
#193220=CARTESIAN_POINT('Ctrl Pts',(5.14428416441681,4.39643371788208,40.9221874939071));
#193221=CARTESIAN_POINT('Ctrl Pts',(5.02784996194912,4.53267383029747,40.9306144322739));
#193222=CARTESIAN_POINT('Ctrl Pts',(4.90603297172752,4.66424739337065,40.9390413706407));
#193223=CARTESIAN_POINT('Ctrl Pts',(4.77924321713337,4.79073306201511,40.9474683090075));
#193224=CARTESIAN_POINT('Ctrl Pts',(4.65233946261239,4.9173324571749,40.9559028242512));
#193225=CARTESIAN_POINT('Ctrl Pts',(4.5204542460474,5.03883458120982,40.9643373394948));
#193226=CARTESIAN_POINT('Ctrl Pts',(4.38403357908909,5.15485582508563,40.9727718547385));
#193227=CARTESIAN_POINT('Ctrl Pts',(4.24754701977988,5.27093310821624,40.9812104439253));
#193228=CARTESIAN_POINT('Ctrl Pts',(4.10652090021877,5.38152402168038,40.989649033112));
#193229=CARTESIAN_POINT('Ctrl Pts',(3.96143285981027,5.48628642136149,40.9980876222988));
#193230=CARTESIAN_POINT('Ctrl Pts',(3.81618264379811,5.59116592170342,41.0065356439191));
#193231=CARTESIAN_POINT('Ctrl Pts',(3.66686170979056,5.6902037016385,41.0149836655394));
#193232=CARTESIAN_POINT('Ctrl Pts',(3.51397613290303,5.78310130789595,41.0234316871597));
#193233=CARTESIAN_POINT('Ctrl Pts',(3.42707842456215,5.83590281643894,41.0282334070719));
#193234=CARTESIAN_POINT('Ctrl Pts',(3.33902958718176,5.88672151057191,41.033035126984));
#193235=CARTESIAN_POINT('Ctrl Pts',(3.24992584954597,5.93550932713048,41.0378368468961));
#193236=CARTESIAN_POINT('Ctrl Pts',(3.20001448099601,5.96283777324972,41.0405265254502));
#193237=CARTESIAN_POINT('Ctrl Pts',(3.14973585451903,5.98954895964303,41.0432162040043));
#193238=CARTESIAN_POINT('Ctrl Pts',(3.09910619832129,6.01563211736942,41.0459058825584));
#193239=CARTESIAN_POINT('Ctrl Pts',(3.09910619832132,6.01563211736941,39.0457552630242));
#193240=CARTESIAN_POINT('Ctrl Pts',(2.93375330764821,6.10081787314655,39.0545047109265));
#193241=CARTESIAN_POINT('Ctrl Pts',(2.76488627843062,6.17918207037043,39.0632541588288));
#193242=CARTESIAN_POINT('Ctrl Pts',(2.59307866646691,6.25045854554002,39.0720036067311));
#193243=CARTESIAN_POINT('Ctrl Pts',(2.42127244185369,6.3217344451504,39.0807529839814));
#193244=CARTESIAN_POINT('Ctrl Pts',(2.24652594672461,6.38592262741839,39.0895023612317));
#193245=CARTESIAN_POINT('Ctrl Pts',(2.06943269687121,6.44280508110562,39.098251738482));
#193246=CARTESIAN_POINT('Ctrl Pts',(1.89234081822083,6.49968709436164,39.1070010479874));
#193247=CARTESIAN_POINT('Ctrl Pts',(1.71290249405601,6.54926340459541,39.1157503574927));
#193248=CARTESIAN_POINT('Ctrl Pts',(1.53172716625078,6.59136563150379,39.1244996669981));
#193249=CARTESIAN_POINT('Ctrl Pts',(1.35055318107349,6.63346754640707,39.1332489116653));
#193250=CARTESIAN_POINT('Ctrl Pts',(1.16764249714429,6.66809542395774,39.1419981563325));
#193251=CARTESIAN_POINT('Ctrl Pts',(0.983616340614404,6.69513165624667,
39.1507474009998));
#193252=CARTESIAN_POINT('Ctrl Pts',(0.799591486713889,6.7221676971596,39.1594965837355));
#193253=CARTESIAN_POINT('Ctrl Pts',(0.614451459526761,6.74161215869371,
39.1682457664712));
#193254=CARTESIAN_POINT('Ctrl Pts',(0.428825047910331,6.75339900185712,
39.1769949492069));
#193255=CARTESIAN_POINT('Ctrl Pts',(0.243199888597193,6.7651857655022,39.1857440729174));
#193256=CARTESIAN_POINT('Ctrl Pts',(0.0570886373921646,6.76931499599834,
39.1944931966279));
#193257=CARTESIAN_POINT('Ctrl Pts',(-0.128876626810802,6.76577266947848,
39.2032423203385));
#193258=CARTESIAN_POINT('Ctrl Pts',(-0.314840698187818,6.76223036567995,
39.21199138793));
#193259=CARTESIAN_POINT('Ctrl Pts',(-0.500658497950919,6.75101660879225,
39.2207404555216));
#193260=CARTESIAN_POINT('Ctrl Pts',(-0.68569895192589,6.73216948296222,
39.2294895231131));
#193261=CARTESIAN_POINT('Ctrl Pts',(-0.870738280459308,6.713322471763,39.2382385374916));
#193262=CARTESIAN_POINT('Ctrl Pts',(-1.05499998761175,6.68684221356198,
39.2469875518701));
#193263=CARTESIAN_POINT('Ctrl Pts',(-1.23785829161323,6.6528186394854,39.2557365662486));
#193264=CARTESIAN_POINT('Ctrl Pts',(-1.4300741291731,6.61705395368882,39.2649332999478));
#193265=CARTESIAN_POINT('Ctrl Pts',(-1.62073882535701,6.57295372727812,
39.274130033647));
#193266=CARTESIAN_POINT('Ctrl Pts',(-1.80913696091426,6.52068343478304,
39.2833267673462));
#193267=CARTESIAN_POINT('Ctrl Pts',(-1.98838356186025,6.47095219815225,
39.2920767650599));
#193268=CARTESIAN_POINT('Ctrl Pts',(-2.16557827572447,6.4138258685092,39.3008267627736));
#193269=CARTESIAN_POINT('Ctrl Pts',(-2.34011918621615,6.34949849943309,
39.3095767604872));
#193270=CARTESIAN_POINT('Ctrl Pts',(-2.51465655691014,6.28517243495584,
39.3183265807455));
#193271=CARTESIAN_POINT('Ctrl Pts',(-2.68653996295244,6.21364572242411,
39.3270764010039));
#193272=CARTESIAN_POINT('Ctrl Pts',(-2.85518555379905,6.1351613225226,39.3358262212622));
#193273=CARTESIAN_POINT('Ctrl Pts',(-3.02382794858611,6.05667841000546,
39.3445758756997));
#193274=CARTESIAN_POINT('Ctrl Pts',(-3.18923239109208,5.9712381949212,39.3533255301372));
#193275=CARTESIAN_POINT('Ctrl Pts',(-3.35083705967631,5.87913088810751,
39.3620751845747));
#193276=CARTESIAN_POINT('Ctrl Pts',(-3.51243888042335,5.78702520443143,
39.3708246848236));
#193277=CARTESIAN_POINT('Ctrl Pts',(-3.67024081223627,5.68825280605824,
39.3795741850726));
#193278=CARTESIAN_POINT('Ctrl Pts',(-3.8237068754434,5.58314917682547,39.3883236853215));
#193279=CARTESIAN_POINT('Ctrl Pts',(-3.97717043817747,5.47804726008071,
39.397073043012));
#193280=CARTESIAN_POINT('Ctrl Pts',(-4.12629803722385,5.36661448084293,
39.4058224007024));
#193281=CARTESIAN_POINT('Ctrl Pts',(-4.27058317206826,5.24922931204643,
39.4145717583929));
#193282=CARTESIAN_POINT('Ctrl Pts',(-4.41486614774757,5.13184589986858,
39.423320985153));
#193283=CARTESIAN_POINT('Ctrl Pts',(-4.55430658194339,5.00851045723103,
39.4320702119131));
#193284=CARTESIAN_POINT('Ctrl Pts',(-4.68843089001774,4.87964187103188,
39.4408194386731));
#193285=CARTESIAN_POINT('Ctrl Pts',(-4.82255336917779,4.7507750420802,39.4495685461291));
#193286=CARTESIAN_POINT('Ctrl Pts',(-4.95135966065089,4.61637541908142,
39.458317653585));
#193287=CARTESIAN_POINT('Ctrl Pts',(-5.07441230869211,4.47689945401882,
39.4670667610409));
#193288=CARTESIAN_POINT('Ctrl Pts',(-5.19746344226393,4.33742520555545,
39.4758157608173));
#193289=CARTESIAN_POINT('Ctrl Pts',(-5.31476088454752,4.19287495491357,
39.4845647605937));
#193290=CARTESIAN_POINT('Ctrl Pts',(-5.42590627628846,4.04373961586716,
39.49331376037));
#193291=CARTESIAN_POINT('Ctrl Pts',(-5.53706380672662,3.89458798906743,
39.5020637156647));
#193292=CARTESIAN_POINT('Ctrl Pts',(-5.6420677707186,3.74085050155291,39.5108136709594));
#193293=CARTESIAN_POINT('Ctrl Pts',(-5.74056148164005,3.58304938223166,
39.5195636262541));
#193294=CARTESIAN_POINT('Ctrl Pts',(-5.83905138951876,3.42525435593295,
39.5283132436952));
#193295=CARTESIAN_POINT('Ctrl Pts',(-5.93103139557641,3.26339625497204,
39.5370628611363));
#193296=CARTESIAN_POINT('Ctrl Pts',(-6.01618907820831,3.09802485065034,
39.5458124785775));
#193297=CARTESIAN_POINT('Ctrl Pts',(-6.10134392544966,2.93265895249676,
39.5545618046933));
#193298=CARTESIAN_POINT('Ctrl Pts',(-6.17967677261813,2.76378023986076,
39.5633111308092));
#193299=CARTESIAN_POINT('Ctrl Pts',(-6.25092157009205,2.59196229227162,
39.572060456925));
#193300=CARTESIAN_POINT('Ctrl Pts',(-6.32216437407752,2.42014915229098,
39.5808095382275));
#193301=CARTESIAN_POINT('Ctrl Pts',(-6.38631941548934,2.24539720662817,
39.58955861953));
#193302=CARTESIAN_POINT('Ctrl Pts',(-6.44316881037562,2.0682999494761,39.5983077008325));
#193303=CARTESIAN_POINT('Ctrl Pts',(-6.50002334524594,1.89118668024373,
39.6070575731748));
#193304=CARTESIAN_POINT('Ctrl Pts',(-6.54957082411117,1.71172794807624,
39.6158074455172));
#193305=CARTESIAN_POINT('Ctrl Pts',(-6.59164294296102,1.5305333425026,39.6245573178595));
#193306=CARTESIAN_POINT('Ctrl Pts',(-6.63371214082151,1.34935131693515,
39.6333065827144));
#193307=CARTESIAN_POINT('Ctrl Pts',(-6.66830695239706,1.16643393829675,
39.6420558475693));
#193308=CARTESIAN_POINT('Ctrl Pts',(-6.69530988154002,0.982402458340054,
39.6508051124242));
#193309=CARTESIAN_POINT('Ctrl Pts',(-6.72231419690493,0.798361530946196,
39.6595548264312));
#193310=CARTESIAN_POINT('Ctrl Pts',(-6.74172580829285,0.613206671361688,
39.6683045404383));
#193311=CARTESIAN_POINT('Ctrl Pts',(-6.75347878028184,0.427566795112685,
39.6770542544453));
#193312=CARTESIAN_POINT('Ctrl Pts',(-6.76248992368219,0.285234494204469,
39.6837627642336));
#193313=CARTESIAN_POINT('Ctrl Pts',(-6.76699999999999,0.142617266091236,
39.6904712740218));
#193314=CARTESIAN_POINT('Ctrl Pts',(-6.767,4.55836674798597E-13,39.6971797838101));
#193315=CARTESIAN_POINT('',(-6.76699999743973,-0.000186146809638267,39.3028289722665));
#193316=CARTESIAN_POINT('Ctrl Pts',(3.0991061983213,6.01563211736942,38.6513937037315));
#193317=CARTESIAN_POINT('Ctrl Pts',(2.93955787853499,6.09782750052023,38.6598174895769));
#193318=CARTESIAN_POINT('Ctrl Pts',(2.77670433697083,6.173688756113,38.6682412754222));
#193319=CARTESIAN_POINT('Ctrl Pts',(2.61107769107173,6.2429610195153,38.6766650612676));
#193320=CARTESIAN_POINT('Ctrl Pts',(2.60106628553135,6.24714822452604,38.677174242238));
#193321=CARTESIAN_POINT('Ctrl Pts',(2.59104475479507,6.25131136978227,38.6776834232084));
#193322=CARTESIAN_POINT('Ctrl Pts',(2.58101321895029,6.25545040453554,38.6781926041788));
#193323=CARTESIAN_POINT('Ctrl Pts',(2.41121188124054,6.32551082686845,38.6868113851161));
#193324=CARTESIAN_POINT('Ctrl Pts',(2.23861825503386,6.38862789171524,38.6954301660533));
#193325=CARTESIAN_POINT('Ctrl Pts',(2.06381703439645,6.44460613602841,38.7040489469906));
#193326=CARTESIAN_POINT('Ctrl Pts',(1.88891081173156,6.50061800613165,38.712672905177));
#193327=CARTESIAN_POINT('Ctrl Pts',(1.71179463784775,6.54948240489686,38.7212968633634));
#193328=CARTESIAN_POINT('Ctrl Pts',(1.53306732596922,6.59105405637411,38.7299208215498));
#193329=CARTESIAN_POINT('Ctrl Pts',(1.34788320612202,6.63412754977864,38.738856333921));
#193330=CARTESIAN_POINT('Ctrl Pts',(1.16096972126086,6.66937147171092,38.7477918462921));
#193331=CARTESIAN_POINT('Ctrl Pts',(0.97300260833897,6.69668238190864,38.7567273586633));
#193332=CARTESIAN_POINT('Ctrl Pts',(0.791250160164018,6.72309032483632,
38.7653674405579));
#193333=CARTESIAN_POINT('Ctrl Pts',(0.608512947785567,6.74208144528608,
38.7740075224526));
#193334=CARTESIAN_POINT('Ctrl Pts',(0.425405891550251,6.75361524129369,
38.7826476043473));
#193335=CARTESIAN_POINT('Ctrl Pts',(0.232907360987668,6.76574060024446,
38.7917308319567));
#193336=CARTESIAN_POINT('Ctrl Pts',(0.0400004451269104,6.76962356844915,
38.800814059566));
#193337=CARTESIAN_POINT('Ctrl Pts',(-0.152601268419071,6.76527914079507,
38.8098972871754));
#193338=CARTESIAN_POINT('Ctrl Pts',(-0.345202981965021,6.760934713141,38.8189805147848));
#193339=CARTESIAN_POINT('Ctrl Pts',(-0.537499108441993,6.74836294850892,
38.8280637423941));
#193340=CARTESIAN_POINT('Ctrl Pts',(-0.728782699476038,6.72764184368821,
38.8371469700035));
#193341=CARTESIAN_POINT('Ctrl Pts',(-0.919252723859074,6.7070088697927,
38.8461915648633));
#193342=CARTESIAN_POINT('Ctrl Pts',(-1.10889479605317,6.67827754701845,
38.8552361597231));
#193343=CARTESIAN_POINT('Ctrl Pts',(-1.29704248510996,6.64153369274144,
38.8642807545829));
#193344=CARTESIAN_POINT('Ctrl Pts',(-1.48501751904548,6.60482355673463,
38.8733170496033));
#193345=CARTESIAN_POINT('Ctrl Pts',(-1.67150067443269,6.56011561460289,
38.8823533446236));
#193346=CARTESIAN_POINT('Ctrl Pts',(-1.85583439428491,6.50754698031364,
38.8913896396439));
#193347=CARTESIAN_POINT('Ctrl Pts',(-2.03984192116548,6.45507137034489,
38.9004099442316));
#193348=CARTESIAN_POINT('Ctrl Pts',(-2.22170737933003,6.39476291009423,
38.9094302488193));
#193349=CARTESIAN_POINT('Ctrl Pts',(-2.40078723634419,6.32680880427146,
38.918450553407));
#193350=CARTESIAN_POINT('Ctrl Pts',(-2.57964157706582,6.25894027344446,
38.9274594986733));
#193351=CARTESIAN_POINT('Ctrl Pts',(-2.7557170954925,6.18344539577992,38.9364684439396));
#193352=CARTESIAN_POINT('Ctrl Pts',(-2.92838670191392,6.10056065653426,
38.9454773892059));
#193353=CARTESIAN_POINT('Ctrl Pts',(-3.10066421221319,6.01786413098478,
38.9544658770647));
#193354=CARTESIAN_POINT('Ctrl Pts',(-3.26955103437948,5.92781134255887,
38.9634543649236));
#193355=CARTESIAN_POINT('Ctrl Pts',(-3.43444173433328,5.8306859779506,38.9724428527824));
#193356=CARTESIAN_POINT('Ctrl Pts',(-3.57911062972357,5.74547183781903,
38.9803290137977));
#193357=CARTESIAN_POINT('Ctrl Pts',(-3.72070360944361,5.65481422883725,
38.988215174813));
#193358=CARTESIAN_POINT('Ctrl Pts',(-3.85882493124176,5.55893507337755,
38.9961013358283));
#193359=CARTESIAN_POINT('Ctrl Pts',(-4.00106745693917,5.46019511739701,
39.0042228006845));
#193360=CARTESIAN_POINT('Ctrl Pts',(-4.13956345584402,5.35596022666187,
39.0123442655406));
#193361=CARTESIAN_POINT('Ctrl Pts',(-4.27386661478399,5.24655631429177,
39.0204657303968));
#193362=CARTESIAN_POINT('Ctrl Pts',(-4.40816019593243,5.13716020403053,
39.028586616073));
#193363=CARTESIAN_POINT('Ctrl Pts',(-4.5382612487939,5.02259603766209,39.0367075017493));
#193364=CARTESIAN_POINT('Ctrl Pts',(-4.66375609795499,4.90323036974479,
39.0448283874255));
#193365=CARTESIAN_POINT('Ctrl Pts',(-4.78926594733842,4.78385043421754,
39.0529502437797));
#193366=CARTESIAN_POINT('Ctrl Pts',(-4.91016823220562,4.65966810758013,
39.061072100134));
#193367=CARTESIAN_POINT('Ctrl Pts',(-5.026085780008,4.53108714681162,39.0691939564882));
#193368=CARTESIAN_POINT('Ctrl Pts',(-5.14208789981946,4.40241237496455,
39.0773217384484));
#193369=CARTESIAN_POINT('Ctrl Pts',(-5.25309777343552,4.26933283162074,
39.0854495204086));
#193370=CARTESIAN_POINT('Ctrl Pts',(-5.35877780973219,4.13228621781235,
39.0935773023688));
#193371=CARTESIAN_POINT('Ctrl Pts',(-5.46450089614862,3.99518377630609,
39.1017083952853));
#193372=CARTESIAN_POINT('Ctrl Pts',(-5.56488960531525,3.85411134126507,
39.1098394882018));
#193373=CARTESIAN_POINT('Ctrl Pts',(-5.6596495827113,3.7095357662268,39.1179705811183));
#193374=CARTESIAN_POINT('Ctrl Pts',(-5.75451298666182,3.56480239299146,
39.1261105487829));
#193375=CARTESIAN_POINT('Ctrl Pts',(-5.84373519957199,3.41655855625808,
39.1342505164475));
#193376=CARTESIAN_POINT('Ctrl Pts',(-5.92706736736082,3.26529652907152,
39.142390484112));
#193377=CARTESIAN_POINT('Ctrl Pts',(-5.97028703262615,3.18684550162526,
39.1466122232923));
#193378=CARTESIAN_POINT('Ctrl Pts',(-6.01192310687886,3.10758296979167,
39.1508339624726));
#193379=CARTESIAN_POINT('Ctrl Pts',(-6.05194599004669,3.02757968244566,
39.1550557016529));
#193380=CARTESIAN_POINT('Ctrl Pts',(-6.13730252520239,2.85695720679128,
39.1640593765569));
#193381=CARTESIAN_POINT('Ctrl Pts',(-6.21546903201688,2.68266435945838,
39.1730630514608));
#193382=CARTESIAN_POINT('Ctrl Pts',(-6.2861558532949,2.50530109729075,39.1820667263648));
#193383=CARTESIAN_POINT('Ctrl Pts',(-6.3567693877612,2.32812172213015,39.1910610664222));
#193384=CARTESIAN_POINT('Ctrl Pts',(-6.419918626014,2.14787851373907,39.2000554064796));
#193385=CARTESIAN_POINT('Ctrl Pts',(-6.47536170120775,1.9651920614871,39.209049746537));
#193386=CARTESIAN_POINT('Ctrl Pts',(-6.53070441239066,1.78283631140145,
39.218027804885));
#193387=CARTESIAN_POINT('Ctrl Pts',(-6.57836874168706,1.59804638192057,
39.2270058632329));
#193388=CARTESIAN_POINT('Ctrl Pts',(-6.61816240750102,1.41145858881525,
39.2359839215808));
#193389=CARTESIAN_POINT('Ctrl Pts',(-6.65790533220295,1.2251087147837,39.2449505319595));
#193390=CARTESIAN_POINT('Ctrl Pts',(-6.68979756797501,1.03696579016012,
39.2539171423381));
#193391=CARTESIAN_POINT('Ctrl Pts',(-6.71369709982694,0.847679333106166,
39.2628837527167));
#193392=CARTESIAN_POINT('Ctrl Pts',(-6.73754730394719,0.658783556155203,
39.27183185635));
#193393=CARTESIAN_POINT('Ctrl Pts',(-6.7534376990638,0.468749199963441,
39.2807799599832));
#193394=CARTESIAN_POINT('Ctrl Pts',(-6.76127761090634,0.278233837368261,
39.2897280636165));
#193395=CARTESIAN_POINT('Ctrl Pts',(-6.76509309690497,0.185514848544821,
39.294082878417));
#193396=CARTESIAN_POINT('Ctrl Pts',(-6.76700257553491,0.0926820920658435,
39.2984376932176));
#193397=CARTESIAN_POINT('Ctrl Pts',(-6.76699999739247,-0.000187857213484029,
39.3027925080181));
#193398=CARTESIAN_POINT('Ctrl Pts',(-6.76699999743974,-0.000186146809638268,
39.3028289722665));
#193399=CARTESIAN_POINT('Ctrl Pts',(-6.76699488074755,-0.186193396001483,
39.3115784840652));
#193400=CARTESIAN_POINT('Ctrl Pts',(-6.75931613702926,-0.372200290803175,
39.3203279958639));
#193401=CARTESIAN_POINT('Ctrl Pts',(-6.74398984746996,-0.557575050752965,
39.3290775076626));
#193402=CARTESIAN_POINT('Ctrl Pts',(-6.7286636226442,-0.742949027736605,
39.3378269825061));
#193403=CARTESIAN_POINT('Ctrl Pts',(-6.70568994023064,-0.927690589582378,
39.3465764573496));
#193404=CARTESIAN_POINT('Ctrl Pts',(-6.67514683067657,-1.11117225888182,
39.3553259321931));
#193405=CARTESIAN_POINT('Ctrl Pts',(-6.64460384759053,-1.29465316844967,
39.3640753708081));
#193406=CARTESIAN_POINT('Ctrl Pts',(-6.60649154714446,-1.47687391320333,
39.3728248094232));
#193407=CARTESIAN_POINT('Ctrl Pts',(-6.56093937725161,-1.65721558284652,
39.3815742480382));
#193408=CARTESIAN_POINT('Ctrl Pts',(-6.51538739219062,-1.83755652073779,
39.3903236511517));
#193409=CARTESIAN_POINT('Ctrl Pts',(-6.46239566827804,-2.01601812091156,
39.3990730542651));
#193410=CARTESIAN_POINT('Ctrl Pts',(-6.40214418972864,-2.19199424586922,
39.4078224573786));
#193411=CARTESIAN_POINT('Ctrl Pts',(-6.34189295065092,-2.36796967140345,
39.4165718257172));
#193412=CARTESIAN_POINT('Ctrl Pts',(-6.27438210750929,-2.54145937035588,
39.4253211940558));
#193413=CARTESIAN_POINT('Ctrl Pts',(-6.1998409562901,-2.71187409676552,
39.4340705623944));
#193414=CARTESIAN_POINT('Ctrl Pts',(-6.12530009514714,-2.8822881600078,
39.442819896685));
#193415=CARTESIAN_POINT('Ctrl Pts',(-6.04372909552121,-3.04962701209198,
39.4515692309755));
#193416=CARTESIAN_POINT('Ctrl Pts',(-5.95540500560968,-3.21332230240901,
39.4603185652661));
#193417=CARTESIAN_POINT('Ctrl Pts',(-5.86708125207551,-3.37701696930168,
39.4690678662352));
#193418=CARTESIAN_POINT('Ctrl Pts',(-5.77200459580281,-3.53706784999082,
39.4778171672044));
#193419=CARTESIAN_POINT('Ctrl Pts',(-5.67049795321926,-3.69293135091031,
39.4865664681736));
#193420=CARTESIAN_POINT('Ctrl Pts',(-5.5689916887887,-3.84879427117568,
39.4953157365482));
#193421=CARTESIAN_POINT('Ctrl Pts',(-5.46105564237136,-4.00046960275369,
39.5040650049227));
#193422=CARTESIAN_POINT('Ctrl Pts',(-5.34705640303826,-4.14744220245775,
39.5128142732972));
#193423=CARTESIAN_POINT('Ctrl Pts',(-5.23305757893143,-4.29441426683468,
39.5215635098038));
#193424=CARTESIAN_POINT('Ctrl Pts',(-5.11299578173536,-4.43668340718169,
39.5303127463103));
#193425=CARTESIAN_POINT('Ctrl Pts',(-4.98727878090113,-4.57376643058796,
39.5390619828169));
#193426=CARTESIAN_POINT('Ctrl Pts',(-4.86156222753462,-4.71084896607114,
39.547811188182));
#193427=CARTESIAN_POINT('Ctrl Pts',(-4.73019070449323,-4.84274521035855,
39.5565603935472));
#193428=CARTESIAN_POINT('Ctrl Pts',(-4.5936103896132,-4.96900720350028,
39.5653095989123));
#193429=CARTESIAN_POINT('Ctrl Pts',(-4.45703054952563,-5.09526875771901,
39.5740587738628));
#193430=CARTESIAN_POINT('Ctrl Pts',(-4.3152421642509,-5.2158959054666,39.5828079488132));
#193431=CARTESIAN_POINT('Ctrl Pts',(-4.16872678712792,-5.33047896293402,
39.5915571237636));
#193432=CARTESIAN_POINT('Ctrl Pts',(-4.02221190716869,-5.44506163159212,
39.6003062690258));
#193433=CARTESIAN_POINT('Ctrl Pts',(-3.87097029317856,-5.5536000744864,
39.6090554142881));
#193434=CARTESIAN_POINT('Ctrl Pts',(-3.71551560084441,-5.6557256669575,
39.6178045595503));
#193435=CARTESIAN_POINT('Ctrl Pts',(-3.5600614230999,-5.75785092137014,
39.626553675851));
#193436=CARTESIAN_POINT('Ctrl Pts',(-3.40039443440767,-5.85356321050832,
39.6353027921516));
#193437=CARTESIAN_POINT('Ctrl Pts',(-3.23705690162253,-5.94253747280217,
39.6440519084522));
#193438=CARTESIAN_POINT('Ctrl Pts',(-3.07371989595894,-6.031511447959,39.6528009965178));
#193439=CARTESIAN_POINT('Ctrl Pts',(-2.90671262153579,-6.11374730271696,
39.6615500845833));
#193440=CARTESIAN_POINT('Ctrl Pts',(-2.73660227089706,-6.18896574646532,
39.6702991726489));
#193441=CARTESIAN_POINT('Ctrl Pts',(-2.56649245511316,-6.26418395371457,
39.6790482332058));
#193442=CARTESIAN_POINT('Ctrl Pts',(-2.39327984469725,-6.33238467823092,
39.6877972937628));
#193443=CARTESIAN_POINT('Ctrl Pts',(-2.21755270315058,-6.39333629717299,
39.6965463543198));
#193444=CARTESIAN_POINT('Ctrl Pts',(-2.04182609952928,-6.45428772953361,
39.7052953880947));
#193445=CARTESIAN_POINT('Ctrl Pts',(-1.86358525088945,-6.50799000682964,
39.7140444218696));
#193446=CARTESIAN_POINT('Ctrl Pts',(-1.68343549389886,-6.55426074686395,
39.7227934556445));
#193447=CARTESIAN_POINT('Ctrl Pts',(-1.50328627341453,-6.60053134909878,
39.7315424633637));
#193448=CARTESIAN_POINT('Ctrl Pts',(-1.32122843347438,-6.63937038708123,
39.740291471083));
#193449=CARTESIAN_POINT('Ctrl Pts',(-1.13788027022808,-6.67064595752358,
39.7490404788023));
#193450=CARTESIAN_POINT('Ctrl Pts',(-0.954532637792132,-6.70192143742018,
39.7577894611924));
#193451=CARTESIAN_POINT('Ctrl Pts',(-0.769894971967928,-6.72563344541621,
39.7665384435824));
#193452=CARTESIAN_POINT('Ctrl Pts',(-0.584594326759636,-6.74170145238726,
39.7752874259725));
#193453=CARTESIAN_POINT('Ctrl Pts',(-0.391305862408406,-6.75846210850439,
39.7844135537791));
#193454=CARTESIAN_POINT('Ctrl Pts',(-0.197296323759575,-6.76690509100547,
39.7935396815856));
#193455=CARTESIAN_POINT('Ctrl Pts',(-0.00328255830076272,-6.76699920384294,
39.8026658093922));
#193456=CARTESIAN_POINT('Ctrl Pts',(0.184668276987458,-6.76709037565425,
39.8115067457049));
#193457=CARTESIAN_POINT('Ctrl Pts',(0.372622761917631,-6.75934662538464,
39.8203476820175));
#193458=CARTESIAN_POINT('Ctrl Pts',(0.559929103887351,-6.74379480697774,
39.8291886183301));
#193459=CARTESIAN_POINT('Ctrl Pts',(0.745308392054773,-6.72840298951089,
39.8379385969113));
#193460=CARTESIAN_POINT('Ctrl Pts',(0.930052522471095,-6.70536305459828,
39.8466885754926));
#193461=CARTESIAN_POINT('Ctrl Pts',(1.11353393682208,-6.67475326671672,
39.8554385540738));
#193462=CARTESIAN_POINT('Ctrl Pts',(1.29701347289961,-6.64414379218326,
39.8641884430828));
#193463=CARTESIAN_POINT('Ctrl Pts',(1.47923003601286,-6.60596466692396,
39.8729383320917));
#193464=CARTESIAN_POINT('Ctrl Pts',(1.65956466641403,-6.56034557915893,
39.8816882211007));
#193465=CARTESIAN_POINT('Ctrl Pts',(1.83989751068703,-6.51472694322911,
39.8904380234462));
#193466=CARTESIAN_POINT('Ctrl Pts',(2.01834818164281,-6.46166856255618,
39.8991878257917));
#193467=CARTESIAN_POINT('Ctrl Pts',(2.19431052364624,-6.40135066418138,
39.9079376281372));
#193468=CARTESIAN_POINT('Ctrl Pts',(2.37027118130145,-6.34103334318208,
39.9166873467277));
#193469=CARTESIAN_POINT('Ctrl Pts',(2.54374328651165,-6.27345673648762,
39.9254370653183));
#193470=CARTESIAN_POINT('Ctrl Pts',(2.71413760594672,-6.19885038180354,
39.9341867839088));
#193471=CARTESIAN_POINT('Ctrl Pts',(2.88453035095198,-6.12424471647617,
39.9429364216527));
#193472=CARTESIAN_POINT('Ctrl Pts',(3.05184510452406,-6.04260954810436,
39.9516860593966));
#193473=CARTESIAN_POINT('Ctrl Pts',(3.21551355852316,-5.95422216204214,
39.9604356971404));
#193474=CARTESIAN_POINT('Ctrl Pts',(3.37918055462056,-5.86583556330403,
39.9691852569455));
#193475=CARTESIAN_POINT('Ctrl Pts',(3.53920106394761,-5.77069700343036,
39.9779348167507));
#193476=CARTESIAN_POINT('Ctrl Pts',(3.69503156396635,-5.66912962819624,
39.9866843765558));
#193477=CARTESIAN_POINT('Ctrl Pts',(3.85086072767506,-5.56756312394374,
39.9954338613299));
#193478=CARTESIAN_POINT('Ctrl Pts',(4.00249971386974,-5.45956807115004,
40.004183346104));
#193479=CARTESIAN_POINT('Ctrl Pts',(4.14943347735481,-5.34551127741839,
40.0129328308781));
#193480=CARTESIAN_POINT('Ctrl Pts',(4.29636602963781,-5.2314554238779,40.0216822435285));
#193481=CARTESIAN_POINT('Ctrl Pts',(4.43859321043452,-5.11133810512784,
40.030431656179));
#193482=CARTESIAN_POINT('Ctrl Pts',(4.57563194991217,-4.98556729559867,
40.0391810688295));
#193483=CARTESIAN_POINT('Ctrl Pts',(4.71266960527883,-4.85979748104009,
40.0479304122635));
#193484=CARTESIAN_POINT('Ctrl Pts',(4.84451869032434,-4.72837445898066,
40.0566797556975));
#193485=CARTESIAN_POINT('Ctrl Pts',(4.97073139114703,-4.59174459623633,
40.0654290991316));
#193486=CARTESIAN_POINT('Ctrl Pts',(5.09694313542921,-4.45511576898207,
40.0741783762561));
#193487=CARTESIAN_POINT('Ctrl Pts',(5.21751838651698,-4.31328039051357,
40.0829276533806));
#193488=CARTESIAN_POINT('Ctrl Pts',(5.33204762730209,-4.16672018501149,
40.0916769305051));
#193489=CARTESIAN_POINT('Ctrl Pts',(5.44657603813579,-4.02016104157748,
40.1004261442269));
#193490=CARTESIAN_POINT('Ctrl Pts',(5.55505834989452,-3.86887736542261,
40.1091753579486));
#193491=CARTESIAN_POINT('Ctrl Pts',(5.65712612279487,-3.71338296312027,
40.1179245716703));
#193492=CARTESIAN_POINT('Ctrl Pts',(5.75919318994895,-3.55788963598193,
40.1266737248957));
#193493=CARTESIAN_POINT('Ctrl Pts',(5.85484564975599,-3.39818588051262,
40.1354228781211));
#193494=CARTESIAN_POINT('Ctrl Pts',(5.94375864110141,-3.23481409300941,
40.1441720313465));
#193495=CARTESIAN_POINT('Ctrl Pts',(6.03267104718983,-3.07144338087755,
40.1529211269819));
#193496=CARTESIAN_POINT('Ctrl Pts',(6.11484393661448,-2.90440493671046,
40.1616702226172));
#193497=CARTESIAN_POINT('Ctrl Pts',(6.189998232126,-2.73426605989194,40.1704193182526));
#193498=CARTESIAN_POINT('Ctrl Pts',(6.26515205790492,-2.56412824648274,
40.179168359204));
#193499=CARTESIAN_POINT('Ctrl Pts',(6.3332872617796,-2.39089030130223,40.1879174001553));
#193500=CARTESIAN_POINT('Ctrl Pts',(6.39417244446545,-2.21514057125925,
40.1966664411067));
#193501=CARTESIAN_POINT('Ctrl Pts',(6.45505726682384,-2.03939188132899,
40.20541543028));
#193502=CARTESIAN_POINT('Ctrl Pts',(6.50869206006277,-1.86113170702176,
40.2141644194533));
#193503=CARTESIAN_POINT('Ctrl Pts',(6.55489467302792,-1.68096544447239,
40.2229134086265));
#193504=CARTESIAN_POINT('Ctrl Pts',(6.60203583620101,-1.49713932218074,
40.2318401229344));
#193505=CARTESIAN_POINT('Ctrl Pts',(6.64143954473786,-1.31132913720938,
40.2407668372423));
#193506=CARTESIAN_POINT('Ctrl Pts',(6.67296649201383,-1.12419179700824,
40.2496935515501));
#193507=CARTESIAN_POINT('Ctrl Pts',(6.70386902476921,-0.94076085031058,
40.2584434656754));
#193508=CARTESIAN_POINT('Ctrl Pts',(6.72720384226755,-0.75605511923264,
40.2671933798007));
#193509=CARTESIAN_POINT('Ctrl Pts',(6.74289167951043,-0.570702022415406,
40.2759432939259));
#193510=CARTESIAN_POINT('Ctrl Pts',(6.7585792082475,-0.385352570619957,
40.2846930359816));
#193511=CARTESIAN_POINT('Ctrl Pts',(6.76662003348113,-0.199356064193198,
40.2934427780373));
#193512=CARTESIAN_POINT('Ctrl Pts',(6.76698684276469,-0.0133442815295733,
40.302192520093));
#193513=CARTESIAN_POINT('Ctrl Pts',(6.76735364532241,0.172664090404337,
40.3109421017126));
#193514=CARTESIAN_POINT('Ctrl Pts',(6.76004671294439,0.358687451388182,
40.3196916833322));
#193515=CARTESIAN_POINT('Ctrl Pts',(6.74509086433814,0.544093954958275,
40.3284412649518));
#193516=CARTESIAN_POINT('Ctrl Pts',(6.73013527008728,0.729497305304266,
40.3371906977665));
#193517=CARTESIAN_POINT('Ctrl Pts',(6.70753104296859,0.91428353355598,40.3459401305813));
#193518=CARTESIAN_POINT('Ctrl Pts',(6.67735495783224,1.09782501661842,40.354689563396));
#193519=CARTESIAN_POINT('Ctrl Pts',(6.6471793458039,1.2813636220728,40.363438859035));
#193520=CARTESIAN_POINT('Ctrl Pts',(6.60943215980949,1.46365723860794,40.372188154674));
#193521=CARTESIAN_POINT('Ctrl Pts',(6.56424160347017,1.64408672863429,40.3809374503129));
#193522=CARTESIAN_POINT('Ctrl Pts',(6.51905169559535,1.82451362957721,40.3896866204034));
#193523=CARTESIAN_POINT('Ctrl Pts',(6.46641870073413,2.0030761795682,40.3984357904939));
#193524=CARTESIAN_POINT('Ctrl Pts',(6.40652137518049,2.17916793050821,40.4071849605843));
#193525=CARTESIAN_POINT('Ctrl Pts',(6.34662482955081,2.35525738855497,40.4159340167517));
#193526=CARTESIAN_POINT('Ctrl Pts',(6.27946423478602,2.52887584065665,40.4246830729191));
#193527=CARTESIAN_POINT('Ctrl Pts',(6.20526768101723,2.69943364558626,40.4334321290865));
#193528=CARTESIAN_POINT('Ctrl Pts',(6.12824915677822,2.87647839720717,40.4425139443497));
#193529=CARTESIAN_POINT('Ctrl Pts',(6.04364908642058,3.05022481423258,40.4515957596129));
#193530=CARTESIAN_POINT('Ctrl Pts',(5.95177703455489,3.22003713192023,40.4606775748762));
#193531=CARTESIAN_POINT('Ctrl Pts',(5.86326386375463,3.38364103946599,40.469427355133));
#193532=CARTESIAN_POINT('Ctrl Pts',(5.76800116437186,3.54359314647918,40.4781771353899));
#193533=CARTESIAN_POINT('Ctrl Pts',(5.66631252012015,3.69935013540617,40.4869269156467));
#193534=CARTESIAN_POINT('Ctrl Pts',(5.56462753148356,3.85510152500977,40.4956763813569));
#193535=CARTESIAN_POINT('Ctrl Pts',(5.45651721693046,4.00665785831769,40.504425847067));
#193536=CARTESIAN_POINT('Ctrl Pts',(5.34234877395471,4.15350437310768,40.5131753127771));
#193537=CARTESIAN_POINT('Ctrl Pts',(5.22818382836054,4.30034638947163,40.5219245104603));
#193538=CARTESIAN_POINT('Ctrl Pts',(5.10796130160446,4.44247864979492,40.5306737081435));
#193539=CARTESIAN_POINT('Ctrl Pts',(4.98208950540816,4.5794184303361,40.5394229058267));
#193540=CARTESIAN_POINT('Ctrl Pts',(4.85622089618151,4.71635474367543,40.5481718819874));
#193541=CARTESIAN_POINT('Ctrl Pts',(4.72470349764587,4.84809862936311,40.5569208581481));
#193542=CARTESIAN_POINT('Ctrl Pts',(4.58798395969625,4.97420266832484,40.5656698343089));
#193543=CARTESIAN_POINT('Ctrl Pts',(4.45125553495138,5.10031490407241,40.5744193791547));
#193544=CARTESIAN_POINT('Ctrl Pts',(4.30932450476746,5.2207863651704,40.5831689240005));
#193545=CARTESIAN_POINT('Ctrl Pts',(4.16267294766396,5.33520786200375,40.5919184688463));
#193546=CARTESIAN_POINT('Ctrl Pts',(4.01603001077209,5.44962263311569,40.6006674993919));
#193547=CARTESIAN_POINT('Ctrl Pts',(3.86466732812914,5.55798797530905,40.6094165299374));
#193548=CARTESIAN_POINT('Ctrl Pts',(3.70909895313569,5.6599358614606,40.618165560483));
#193549=CARTESIAN_POINT('Ctrl Pts',(3.55352846818182,5.76188513032251,40.626914709691));
#193550=CARTESIAN_POINT('Ctrl Pts',(3.39375241639409,5.85741661190576,40.6356638588989));
#193551=CARTESIAN_POINT('Ctrl Pts',(3.23031343910922,5.94620585626754,40.6444130081068));
#193552=CARTESIAN_POINT('Ctrl Pts',(3.18683327726978,5.96982672552765,40.6467405705392));
#193553=CARTESIAN_POINT('Ctrl Pts',(3.14309402254946,5.99297066865441,40.6490681329716));
#193554=CARTESIAN_POINT('Ctrl Pts',(3.09910619832134,6.0156321173694,40.651395695404));
#193555=CARTESIAN_POINT('Origin',(0.,0.,4.30282021618968));
#193556=CARTESIAN_POINT('',(3.09910619832137,6.01563211736938,43.0457451347211));
#193557=CARTESIAN_POINT('',(3.09910619832134,6.0156321173694,42.651395695404));
#193558=CARTESIAN_POINT('',(3.09910619832133,6.0156321173694,4.30282021618968));
#193559=CARTESIAN_POINT('',(-6.76699752108395,0.00579220542896902,41.6971797838367));
#193560=CARTESIAN_POINT('Ctrl Pts',(-6.76699752108395,0.00579220542897352,
41.6971797838367));
#193561=CARTESIAN_POINT('Ctrl Pts',(-6.7671419157541,-0.162903188225639,
41.7051597747815));
#193562=CARTESIAN_POINT('Ctrl Pts',(-6.76097415360396,-0.331919362032048,
41.7131397657264));
#193563=CARTESIAN_POINT('Ctrl Pts',(-6.74844880523453,-0.500727194317024,
41.7211197566712));
#193564=CARTESIAN_POINT('Ctrl Pts',(-6.73593791874819,-0.669340119517491,
41.7290905338447));
#193565=CARTESIAN_POINT('Ctrl Pts',(-6.71708407476151,-0.837744806685119,
41.7370613110182));
#193566=CARTESIAN_POINT('Ctrl Pts',(-6.69189373650032,-1.00540898115535,
41.7450320881916));
#193567=CARTESIAN_POINT('Ctrl Pts',(-6.66672676650753,-1.1729176189516,
41.7529954711309));
#193568=CARTESIAN_POINT('Ctrl Pts',(-6.63523505233561,-1.3396867371706,
41.7609588540702));
#193569=CARTESIAN_POINT('Ctrl Pts',(-6.59747704608564,-1.50518624308525,
41.7689222370095));
#193570=CARTESIAN_POINT('Ctrl Pts',(-6.5597455214126,-1.67056967592472,
41.7768800348303));
#193571=CARTESIAN_POINT('Ctrl Pts',(-6.51575653367953,-1.83468489874086,
41.7848378326512));
#193572=CARTESIAN_POINT('Ctrl Pts',(-6.46562006098974,-1.99700932069108,
41.792795630472));
#193573=CARTESIAN_POINT('Ctrl Pts',(-6.41344117349947,-2.16594636981835,
41.8010776059459));
#193574=CARTESIAN_POINT('Ctrl Pts',(-6.35460345110363,-2.33294322299446,
41.8093595814197));
#193575=CARTESIAN_POINT('Ctrl Pts',(-6.28928922096292,-2.49742469257426,
41.8176415568936));
#193576=CARTESIAN_POINT('Ctrl Pts',(-6.22656637487845,-2.65538025414138,
41.825594939668));
#193577=CARTESIAN_POINT('Ctrl Pts',(-6.15787122358108,-2.81101581324948,
41.8335483224424));
#193578=CARTESIAN_POINT('Ctrl Pts',(-6.08341529326123,-2.96383997032825,
41.8415017052167));
#193579=CARTESIAN_POINT('Ctrl Pts',(-6.00895734476367,-3.11666826980785,
41.8494553035729));
#193580=CARTESIAN_POINT('Ctrl Pts',(-5.92873847287648,-3.26668467282175,
41.857408901929));
#193581=CARTESIAN_POINT('Ctrl Pts',(-5.84301703124469,-3.41342071426662,
41.8653625002851));
#193582=CARTESIAN_POINT('Ctrl Pts',(-5.75727574448061,-3.56019072616391,
41.8733179399567));
#193583=CARTESIAN_POINT('Ctrl Pts',(-5.66602954574324,-3.7036785367616,
41.8812733796282));
#193584=CARTESIAN_POINT('Ctrl Pts',(-5.56958099527458,-3.84344331779151,
41.8892288192998));
#193585=CARTESIAN_POINT('Ctrl Pts',(-5.47309038661119,-3.98326904586883,
41.8971877280896));
#193586=CARTESIAN_POINT('Ctrl Pts',(-5.37139312906561,-4.11936820155264,
41.9051466368794));
#193587=CARTESIAN_POINT('Ctrl Pts',(-5.26483288548004,-4.25133198985541,
41.9131055456693));
#193588=CARTESIAN_POINT('Ctrl Pts',(-5.15814568872913,-4.38345299646091,
41.9210739365007));
#193589=CARTESIAN_POINT('Ctrl Pts',(-5.04658418186476,-4.51142850673486,
41.9290423273321));
#193590=CARTESIAN_POINT('Ctrl Pts',(-4.93053021868755,-4.63488519411311,
41.9370107181636));
#193591=CARTESIAN_POINT('Ctrl Pts',(-4.81439468646419,-4.75842865357526,
41.9449847096141));
#193592=CARTESIAN_POINT('Ctrl Pts',(-4.6937606833546,-4.87744670354447,
41.9529587010646));
#193593=CARTESIAN_POINT('Ctrl Pts',(-4.5690435503665,-4.99160595749046,
41.9609326925151));
#193594=CARTESIAN_POINT('Ctrl Pts',(-4.44414673822428,-5.10592967992361,
41.9689181720427));
#193595=CARTESIAN_POINT('Ctrl Pts',(-4.31515534748906,-5.21538039602099,
41.9769036515704));
#193596=CARTESIAN_POINT('Ctrl Pts',(-4.18251456892623,-5.31966736560848,
41.984889131098));
#193597=CARTESIAN_POINT('Ctrl Pts',(-4.14556280272493,-5.34872017847487,
41.9871137680136));
#193598=CARTESIAN_POINT('Ctrl Pts',(-4.10832795919166,-5.3773725065816,
41.9893384049292));
#193599=CARTESIAN_POINT('Ctrl Pts',(-4.07081999675313,-5.40561870224259,
41.9915630418449));
#193600=CARTESIAN_POINT('Ctrl Pts',(-3.93032474337721,-5.51142174133862,
41.9998959638916));
#193601=CARTESIAN_POINT('Ctrl Pts',(-3.78552165961881,-5.61187987212897,
42.0082288859383));
#193602=CARTESIAN_POINT('Ctrl Pts',(-3.63684920453656,-5.70662920325667,
42.016561807985));
#193603=CARTESIAN_POINT('Ctrl Pts',(-3.48835244424243,-5.80126656365214,
42.0248848825387));
#193604=CARTESIAN_POINT('Ctrl Pts',(-3.33599571263826,-5.89020837836998,
42.0332079570923));
#193605=CARTESIAN_POINT('Ctrl Pts',(-3.18024955516211,-5.97313165491028,
42.0415310316459));
#193606=CARTESIAN_POINT('Ctrl Pts',(-3.02465886377403,-6.05597215729022,
42.0498457980919));
#193607=CARTESIAN_POINT('Ctrl Pts',(-2.86568579241507,-6.13280592828548,
42.0581605645379));
#193608=CARTESIAN_POINT('Ctrl Pts',(-2.70382900372628,-6.20335374766009,
42.0664753309839));
#193609=CARTESIAN_POINT('Ctrl Pts',(-2.54210409078569,-6.27384408692196,
42.0747833228234));
#193610=CARTESIAN_POINT('Ctrl Pts',(-2.37750045979973,-6.33805854133451,
42.083091314663));
#193611=CARTESIAN_POINT('Ctrl Pts',(-2.21054066438813,-6.39576414285944,
42.0913993065025));
#193612=CARTESIAN_POINT('Ctrl Pts',(-2.04368629314711,-6.45343330707822,
42.0997020523896));
#193613=CARTESIAN_POINT('Ctrl Pts',(-1.87447905034718,-6.50460169563769,
42.1080047982766));
#193614=CARTESIAN_POINT('Ctrl Pts',(-1.70346093646292,-6.54908465649551,
42.1163075441637));
#193615=CARTESIAN_POINT('Ctrl Pts',(-1.53251271223167,-6.59354943858484,
42.1246068969831));
#193616=CARTESIAN_POINT('Ctrl Pts',(-1.35975542770278,-6.63133414948042,
42.1329062498026));
#193617=CARTESIAN_POINT('Ctrl Pts',(-1.18574597554647,-6.66230406702331,
42.141205602622));
#193618=CARTESIAN_POINT('Ctrl Pts',(-1.01177353228092,-6.69326739778439,
42.1495031903083));
#193619=CARTESIAN_POINT('Ctrl Pts',(-0.836549794271697,-6.71741876178281,
42.1578007779947));
#193620=CARTESIAN_POINT('Ctrl Pts',(-0.66064181556716,-6.73467455720944,
42.166098365681));
#193621=CARTESIAN_POINT('Ctrl Pts',(-0.484742017984839,-6.75192955010413,
42.1743955674634));
#193622=CARTESIAN_POINT('Ctrl Pts',(-0.308158389356044,-6.76228957969436,
42.1826927692459));
#193623=CARTESIAN_POINT('Ctrl Pts',(-0.131463270973249,-6.76572290360646,
42.1909899710283));
#193624=CARTESIAN_POINT('Ctrl Pts',(0.0452529907255948,-6.76915663834968,
42.1992881656528));
#193625=CARTESIAN_POINT('Ctrl Pts',(0.222080420934282,-6.76566200967775,
42.2075863602774));
#193626=CARTESIAN_POINT('Ctrl Pts',(0.398446313981372,-6.75525939804495,
42.2158845549019));
#193627=CARTESIAN_POINT('Ctrl Pts',(0.5749362472169,-6.74484947013414,42.2241885857435));
#193628=CARTESIAN_POINT('Ctrl Pts',(0.750963646941569,-6.72752187160386,
42.2324926165851));
#193629=CARTESIAN_POINT('Ctrl Pts',(0.92595965786807,-6.70334899225759,
42.2407966474267));
#193630=CARTESIAN_POINT('Ctrl Pts',(1.10101930216068,-6.67916732298706,
42.2491036978424));
#193631=CARTESIAN_POINT('Ctrl Pts',(1.27504646657759,-6.64813546666324,
42.2574107482581));
#193632=CARTESIAN_POINT('Ctrl Pts',(1.44748190173852,-6.61037708032904,
42.2657177986739));
#193633=CARTESIAN_POINT('Ctrl Pts',(1.62010169948183,-6.5725783239073,42.2740337307285));
#193634=CARTESIAN_POINT('Ctrl Pts',(1.79112602924616,-6.52803874986931,
42.2823496627831));
#193635=CARTESIAN_POINT('Ctrl Pts',(1.96000915956826,-6.47693238303509,
42.2906655948378));
#193636=CARTESIAN_POINT('Ctrl Pts',(2.08731685039777,-6.4384073181814,42.2969343210566));
#193637=CARTESIAN_POINT('Ctrl Pts',(2.21340809606874,-6.39615173772712,
42.3032030472755));
#193638=CARTESIAN_POINT('Ctrl Pts',(2.33805657735998,-6.35025829719262,
42.3094717734943));
#193639=CARTESIAN_POINT('Ctrl Pts',(2.50608324276164,-6.2883937506138,42.3179220422176));
#193640=CARTESIAN_POINT('Ctrl Pts',(2.67179565761498,-6.21980369679273,
42.326372310941));
#193641=CARTESIAN_POINT('Ctrl Pts',(2.83463840281996,-6.14468177575197,
42.3348225796643));
#193642=CARTESIAN_POINT('Ctrl Pts',(2.99733743377775,-6.06962615235508,
42.3432653907389));
#193643=CARTESIAN_POINT('Ctrl Pts',(3.15717154329149,-5.98805028986467,
42.3517082018134));
#193644=CARTESIAN_POINT('Ctrl Pts',(3.31360401903543,-5.90019638698851,
42.3601510128879));
#193645=CARTESIAN_POINT('Ctrl Pts',(3.46991973649539,-5.81240805662785,
42.3685875224056));
#193646=CARTESIAN_POINT('Ctrl Pts',(3.6228385932091,-5.71835118861923,42.3770240319233));
#193647=CARTESIAN_POINT('Ctrl Pts',(3.7718469286948,-5.61831467136681,42.385460541441));
#193648=CARTESIAN_POINT('Ctrl Pts',(3.92074864069892,-5.51834973562506,
42.3938910141822));
#193649=CARTESIAN_POINT('Ctrl Pts',(4.06574513828252,-5.41241386968859,
42.4023214869235));
#193650=CARTESIAN_POINT('Ctrl Pts',(4.20635011855401,-5.30084028057257,
42.4107519596647));
#193651=CARTESIAN_POINT('Ctrl Pts',(4.34689465312561,-5.18931465664007,
42.4191788081685));
#193652=CARTESIAN_POINT('Ctrl Pts',(4.48305117471774,-5.07215634687458,
42.4276056566723));
#193653=CARTESIAN_POINT('Ctrl Pts',(4.61436443864262,-4.94974037979674,
42.4360325051761));
#193654=CARTESIAN_POINT('Ctrl Pts',(4.74563717085251,-4.8273621981561,42.4444567526128));
#193655=CARTESIAN_POINT('Ctrl Pts',(4.87206938440724,-4.69972982139218,
42.4528810000495));
#193656=CARTESIAN_POINT('Ctrl Pts',(4.99324058506915,-4.56725710461086,
42.4613052474861));
#193657=CARTESIAN_POINT('Ctrl Pts',(5.0273819933344,-4.52993136150579,42.4636788780971));
#193658=CARTESIAN_POINT('Ctrl Pts',(5.06110595313962,-4.49222157277779,
42.4660525087081));
#193659=CARTESIAN_POINT('Ctrl Pts',(5.09440359174525,-4.45413751970156,
42.4684261393191));
#193660=CARTESIAN_POINT('Ctrl Pts',(5.21530911577234,-4.3158522662398,42.4770449202563));
#193661=CARTESIAN_POINT('Ctrl Pts',(5.33053669471643,-4.17269176633671,
42.4856637011936));
#193662=CARTESIAN_POINT('Ctrl Pts',(5.43971335764167,-4.02514690249869,
42.4942824821308));
#193663=CARTESIAN_POINT('Ctrl Pts',(5.54895560232493,-3.8775134093575,42.5029064403173));
#193664=CARTESIAN_POINT('Ctrl Pts',(5.65213949620672,-3.72549054080655,
42.5115303985039));
#193665=CARTESIAN_POINT('Ctrl Pts',(5.74893505733717,-3.56959867583454,
42.5201543566905));
#193666=CARTESIAN_POINT('Ctrl Pts',(5.84922751182715,-3.40807496968036,
42.5290898690616));
#193667=CARTESIAN_POINT('Ctrl Pts',(5.94266126508607,-3.24239781794299,
42.5380253814327));
#193668=CARTESIAN_POINT('Ctrl Pts',(6.02892123533005,-3.07317388674744,
42.5469608938038));
#193669=CARTESIAN_POINT('Ctrl Pts',(6.11232923435509,-2.90954492364616,
42.5556009756985));
#193670=CARTESIAN_POINT('Ctrl Pts',(6.1890301394651,-2.74260025437282,42.5642410575931));
#193671=CARTESIAN_POINT('Ctrl Pts',(6.25878801113481,-2.57290917672489,
42.5728811394877));
#193672=CARTESIAN_POINT('Ctrl Pts',(6.33212373105573,-2.39451472394703,
42.5819643670971));
#193673=CARTESIAN_POINT('Ctrl Pts',(6.39778536647262,-2.21308510877036,
42.5910475947064));
#193674=CARTESIAN_POINT('Ctrl Pts',(6.45555782815182,-2.02930089621716,
42.6001308223158));
#193675=CARTESIAN_POINT('Ctrl Pts',(6.51333028983101,-1.84551668366399,
42.6092140499251));
#193676=CARTESIAN_POINT('Ctrl Pts',(6.56321350990222,-1.65937825700491,
42.6182972775345));
#193677=CARTESIAN_POINT('Ctrl Pts',(6.60505419342663,-1.47158013777615,
42.6273805051438));
#193678=CARTESIAN_POINT('Ctrl Pts',(6.64671692031331,-1.2845807608015,42.6364251000036));
#193679=CARTESIAN_POINT('Ctrl Pts',(6.68044470798201,-1.09576328069521,
42.6454696948635));
#193680=CARTESIAN_POINT('Ctrl Pts',(6.70610468636559,-0.905786363059985,
42.6545142897234));
#193681=CARTESIAN_POINT('Ctrl Pts',(6.73174111768006,-0.715983779149547,
42.6635505847438));
#193682=CARTESIAN_POINT('Ctrl Pts',(6.74932448898829,-0.525024117474134,
42.6725868797642));
#193683=CARTESIAN_POINT('Ctrl Pts',(6.75877335798435,-0.333574122798727,
42.6816231747846));
#193684=CARTESIAN_POINT('Ctrl Pts',(6.76820550646572,-0.142462913902861,
42.6906434793724));
#193685=CARTESIAN_POINT('Ctrl Pts',(6.769531885184,0.0491366580460953,42.6996637839601));
#193686=CARTESIAN_POINT('Ctrl Pts',(6.76272299267066,0.240555034043397,
42.7086840885478));
#193687=CARTESIAN_POINT('Ctrl Pts',(6.75592267463481,0.431732355779322,
42.7176930338142));
#193688=CARTESIAN_POINT('Ctrl Pts',(6.74100753888465,0.622728699902162,
42.7267019790805));
#193689=CARTESIAN_POINT('Ctrl Pts',(6.71800003456061,0.812874243437263,
42.7357109243468));
#193690=CARTESIAN_POINT('Ctrl Pts',(6.69504477540808,1.00258800669779,42.7446994122056));
#193691=CARTESIAN_POINT('Ctrl Pts',(6.66403385639883,1.19145459005036,42.7536879000645));
#193692=CARTESIAN_POINT('Ctrl Pts',(6.62504138342984,1.37880951107905,42.7626763879233));
#193693=CARTESIAN_POINT('Ctrl Pts',(6.59083085491407,1.54318766871784,42.7705625489384));
#193694=CARTESIAN_POINT('Ctrl Pts',(6.5504771695524,1.70640211062867,42.7784487099534));
#193695=CARTESIAN_POINT('Ctrl Pts',(6.50406332209127,1.86800677253244,42.7863348709685));
#193696=CARTESIAN_POINT('Ctrl Pts',(6.45626459844424,2.03443332402401,42.7944563358247));
#193697=CARTESIAN_POINT('Ctrl Pts',(6.40205850140957,2.19907764734956,42.8025778006808));
#193698=CARTESIAN_POINT('Ctrl Pts',(6.3416102525954,2.36141237486741,42.810699265537));
#193699=CARTESIAN_POINT('Ctrl Pts',(6.28116631463095,2.5237355255302,42.8188201512132));
#193700=CARTESIAN_POINT('Ctrl Pts',(6.21448123936187,2.68374906529327,42.8269410368894));
#193701=CARTESIAN_POINT('Ctrl Pts',(6.14176922178484,2.84094347468169,42.8350619225656));
#193702=CARTESIAN_POINT('Ctrl Pts',(6.06904851304248,2.99815667329708,42.8431837789199));
#193703=CARTESIAN_POINT('Ctrl Pts',(5.99029958234779,3.15254973871702,42.8513056352741));
#193704=CARTESIAN_POINT('Ctrl Pts',(5.90578358336553,3.30363576479767,42.8594274916284));
#193705=CARTESIAN_POINT('Ctrl Pts',(5.82120592255594,3.45483202137389,42.8675552735886));
#193706=CARTESIAN_POINT('Ctrl Pts',(5.73085296872741,3.60271609973036,42.8756830555488));
#193707=CARTESIAN_POINT('Ctrl Pts',(5.63503073783105,3.74682766933565,42.8838108375089));
#193708=CARTESIAN_POINT('Ctrl Pts',(5.53916947251942,3.89099794463796,42.8919419304254));
#193709=CARTESIAN_POINT('Ctrl Pts',(5.43783470331295,4.03139235124276,42.9000730233418));
#193710=CARTESIAN_POINT('Ctrl Pts',(5.33137394546845,4.16758213519304,42.9082041162583));
#193711=CARTESIAN_POINT('Ctrl Pts',(5.22479699015606,4.30392056460075,42.9163440839229));
#193712=CARTESIAN_POINT('Ctrl Pts',(5.11308310766669,4.43604492596168,42.9244840515874));
#193713=CARTESIAN_POINT('Ctrl Pts',(4.99661850493419,4.56356138516283,42.932624019252));
#193714=CARTESIAN_POINT('Ctrl Pts',(4.93621492634999,4.62969693436335,42.9368457584325));
#193715=CARTESIAN_POINT('Ctrl Pts',(4.87453403930079,4.69459361999119,42.941067497613));
#193716=CARTESIAN_POINT('Ctrl Pts',(4.81163332987714,4.7582006787036,42.9452892367935));
#193717=CARTESIAN_POINT('Ctrl Pts',(4.68589120127583,4.88535484007718,42.9537287357407));
#193718=CARTESIAN_POINT('Ctrl Pts',(4.55501247853667,5.00761580790413,42.9621682346878));
#193719=CARTESIAN_POINT('Ctrl Pts',(4.4194057018988,5.12456263909657,42.970607733635));
#193720=CARTESIAN_POINT('Ctrl Pts',(4.28389115220958,5.24142993407657,42.9790414928304));
#193721=CARTESIAN_POINT('Ctrl Pts',(4.14365520789653,5.35299007747284,42.9874752520258));
#193722=CARTESIAN_POINT('Ctrl Pts',(3.99914256677247,5.45885956318978,42.9959090112212));
#193723=CARTESIAN_POINT('Ctrl Pts',(3.85472117236771,5.56466220186019,43.0043374452571));
#193724=CARTESIAN_POINT('Ctrl Pts',(3.70602873374957,5.66478115071055,43.0127658792931));
#193725=CARTESIAN_POINT('Ctrl Pts',(3.55354243465342,5.7588736021133,43.021194313329));
#193726=CARTESIAN_POINT('Ctrl Pts',(3.40548551692778,5.8502328810683,43.0293779204597));
#193727=CARTESIAN_POINT('Ctrl Pts',(3.25385232116557,5.93591070836102,43.0375615275904));
#193728=CARTESIAN_POINT('Ctrl Pts',(3.09910619832137,6.01563211736938,43.0457451347211));
#193729=CARTESIAN_POINT('Ctrl Pts',(3.09910619832129,6.01563211736942,41.0459058825584));
#193730=CARTESIAN_POINT('Ctrl Pts',(2.94406710095791,6.09550445966803,41.054142267447));
#193731=CARTESIAN_POINT('Ctrl Pts',(2.78573418535561,6.16948443241409,41.0623786523356));
#193732=CARTESIAN_POINT('Ctrl Pts',(2.62459330575604,6.23729099684956,41.0706150372242));
#193733=CARTESIAN_POINT('Ctrl Pts',(2.4636219004224,6.30502624811012,41.0788427597841));
#193734=CARTESIAN_POINT('Ctrl Pts',(2.29984873717746,6.3666008827864,41.0870704823439));
#193735=CARTESIAN_POINT('Ctrl Pts',(2.13378450708244,6.42177955689348,41.0952982049037));
#193736=CARTESIAN_POINT('Ctrl Pts',(1.96307750522898,6.47850089909751,41.1037559555552));
#193737=CARTESIAN_POINT('Ctrl Pts',(1.78994978312948,6.52846323509716,41.1122137062066));
#193738=CARTESIAN_POINT('Ctrl Pts',(1.61497995666406,6.57146321146009,41.1206714568581));
#193739=CARTESIAN_POINT('Ctrl Pts',(1.44505721225939,6.61322283447926,41.1288852399498));
#193740=CARTESIAN_POINT('Ctrl Pts',(1.27339753524235,6.6484160883722,41.1370990230415));
#193741=CARTESIAN_POINT('Ctrl Pts',(1.10054774648411,6.6769067432239,41.1453128061333));
#193742=CARTESIAN_POINT('Ctrl Pts',(0.919996925079205,6.70666675145296,
41.1538925405646));
#193743=CARTESIAN_POINT('Ctrl Pts',(0.738147891892085,6.72911308957362,
41.1624722749959));
#193744=CARTESIAN_POINT('Ctrl Pts',(0.555637124469811,6.74414978970003,
41.1710520094272));
#193745=CARTESIAN_POINT('Ctrl Pts',(0.373126357047538,6.75918648982644,
41.1796317438585));
#193746=CARTESIAN_POINT('Ctrl Pts',(0.189954295794854,6.76681349632012,
41.1882114782898));
#193747=CARTESIAN_POINT('Ctrl Pts',(0.00676451732140437,6.76699661898138,
41.1967912127211));
#193748=CARTESIAN_POINT('Ctrl Pts',(-0.182389569994082,6.76718570376627,
41.205650286897));
#193749=CARTESIAN_POINT('Ctrl Pts',(-0.371365666416525,6.75943933602207,
41.2145093610729));
#193750=CARTESIAN_POINT('Ctrl Pts',(-0.559514331608083,6.74382923217405,
41.2233684352488));
#193751=CARTESIAN_POINT('Ctrl Pts',(-0.74801649028807,6.72818980008147,
41.2322441538427));
#193752=CARTESIAN_POINT('Ctrl Pts',(-0.93568785266029,6.70465712757872,
41.2411198724367));
#193753=CARTESIAN_POINT('Ctrl Pts',(-1.12188692416418,6.67335438362069,
41.2499955910306));
#193754=CARTESIAN_POINT('Ctrl Pts',(-1.30861735520857,6.64196231047582,
41.2588966384176));
#193755=CARTESIAN_POINT('Ctrl Pts',(-1.49386683033995,6.60275583669487,
41.2677976858046));
#193756=CARTESIAN_POINT('Ctrl Pts',(-1.67700380448391,6.55590933736477,
41.2766987331917));
#193757=CARTESIAN_POINT('Ctrl Pts',(-1.86038975585627,6.50899914957624,
41.2856118816747));
#193758=CARTESIAN_POINT('Ctrl Pts',(-2.04165721980538,6.45442825866837,
41.2945250301577));
#193759=CARTESIAN_POINT('Ctrl Pts',(-2.22019121767212,6.39242050845934,
41.3034381786407));
#193760=CARTESIAN_POINT('Ctrl Pts',(-2.39912160983302,6.33027508408925,
41.3123711167506));
#193761=CARTESIAN_POINT('Ctrl Pts',(-2.57530615082169,6.26065985907395,
41.3213040548605));
#193762=CARTESIAN_POINT('Ctrl Pts',(-2.7481485286805,6.18384739982409,41.3302369929704));
#193763=CARTESIAN_POINT('Ctrl Pts',(-2.91266941129938,6.11073307596171,
41.3387398548289));
#193764=CARTESIAN_POINT('Ctrl Pts',(-3.0741622052832,6.0310983035465,41.3472427166873));
#193765=CARTESIAN_POINT('Ctrl Pts',(-3.23213456965948,5.94521615449027,
41.3557455785458));
#193766=CARTESIAN_POINT('Ctrl Pts',(-3.38490232624872,5.86216350604646,
41.3639683024117));
#193767=CARTESIAN_POINT('Ctrl Pts',(-3.53467012740325,5.77310830317956,
41.3721910262775));
#193768=CARTESIAN_POINT('Ctrl Pts',(-3.68093488888944,5.67829264337058,
41.3804137501434));
#193769=CARTESIAN_POINT('Ctrl Pts',(-3.82704483408053,5.5835773427255,41.3886277705346));
#193770=CARTESIAN_POINT('Ctrl Pts',(-3.96965882461234,5.48311392022527,
41.3968417909258));
#193771=CARTESIAN_POINT('Ctrl Pts',(-4.10829761703015,5.3771906875156,41.405055811317));
#193772=CARTESIAN_POINT('Ctrl Pts',(-4.24681749973279,5.2713583045689,41.413262786589));
#193773=CARTESIAN_POINT('Ctrl Pts',(-4.38136869121096,5.16007565425907,
41.421469761861));
#193774=CARTESIAN_POINT('Ctrl Pts',(-4.51150016803177,5.04367477478964,
41.4296767371329));
#193775=CARTESIAN_POINT('Ctrl Pts',(-4.64154615106915,4.92735036837518,
41.4378783205859));
#193776=CARTESIAN_POINT('Ctrl Pts',(-4.76717793678927,4.80591466894603,
41.4460799040389));
#193777=CARTESIAN_POINT('Ctrl Pts',(-4.88797683485411,4.67974053361184,
41.4542814874919));
#193778=CARTESIAN_POINT('Ctrl Pts',(-5.00872061156571,4.55362397238796,
41.462479328507));
#193779=CARTESIAN_POINT('Ctrl Pts',(-5.12463564651238,4.42277354143135,
41.470677169522));
#193780=CARTESIAN_POINT('Ctrl Pts',(-5.2353393890757,4.28759961764068,41.4788750105371));
#193781=CARTESIAN_POINT('Ctrl Pts',(-5.34603336237893,4.15243762252729,
41.4870721281182));
#193782=CARTESIAN_POINT('Ctrl Pts',(-5.4515167255638,4.01295316642926,41.4952692456993));
#193783=CARTESIAN_POINT('Ctrl Pts',(-5.55144636183972,3.86959071370818,
41.5034663632805));
#193784=CARTESIAN_POINT('Ctrl Pts',(-5.65137488628714,3.72622985605405,
41.5116633896596));
#193785=CARTESIAN_POINT('Ctrl Pts',(-5.74574960082674,3.57899138147709,
41.5198604160387));
#193786=CARTESIAN_POINT('Ctrl Pts',(-5.83427006732313,3.42834971692466,
41.5280574424177));
#193787=CARTESIAN_POINT('Ctrl Pts',(-5.92280564463728,3.27768233720341,
41.5362558680639));
#193788=CARTESIAN_POINT('Ctrl Pts',(-6.00548480111659,3.12361091948588,
41.54445429371));
#193789=CARTESIAN_POINT('Ctrl Pts',(-6.08205248542011,2.96663556315822,
41.5526527193561));
#193790=CARTESIAN_POINT('Ctrl Pts',(-6.15864716262927,2.80960486728333,
41.5608540352468));
#193791=CARTESIAN_POINT('Ctrl Pts',(-6.22912591862728,2.64966851580437,
41.5690553511374));
#193792=CARTESIAN_POINT('Ctrl Pts',(-6.29328135494752,2.48734774156529,
41.5772566670281));
#193793=CARTESIAN_POINT('Ctrl Pts',(-6.35750985357043,2.32484211113605,
41.5854673228447));
#193794=CARTESIAN_POINT('Ctrl Pts',(-6.4154005137618,2.15994696700335,41.5936779786613));
#193795=CARTESIAN_POINT('Ctrl Pts',(-6.46679511988317,1.993200912466,41.6018886344779));
#193796=CARTESIAN_POINT('Ctrl Pts',(-6.51822001160071,1.82635659851869,
41.610104128635));
#193797=CARTESIAN_POINT('Ctrl Pts',(-6.56314112660341,1.6576595462069,41.6183196227921));
#193798=CARTESIAN_POINT('Ctrl Pts',(-6.60145118222209,1.48765966831751,
41.6265351169493));
#193799=CARTESIAN_POINT('Ctrl Pts',(-6.63982067659705,1.31739603248923,
41.6347633575968));
#193800=CARTESIAN_POINT('Ctrl Pts',(-6.67155854847443,1.14582588422684,
41.6429915982443));
#193801=CARTESIAN_POINT('Ctrl Pts',(-6.69660911591914,0.97350672755184,
41.6512198388918));
#193802=CARTESIAN_POINT('Ctrl Pts',(-6.7193760823766,0.816896125071227,
41.658697995993));
#193803=CARTESIAN_POINT('Ctrl Pts',(-6.73662003573352,0.659667103896605,
41.6661761530942));
#193804=CARTESIAN_POINT('Ctrl Pts',(-6.74833653388256,0.502238016747035,
41.6736543101954));
#193805=CARTESIAN_POINT('Ctrl Pts',(-6.7606228126333,0.337153055046718,
41.6814961347336));
#193806=CARTESIAN_POINT('Ctrl Pts',(-6.76685562646407,0.171566789773337,
41.6893379592718));
#193807=CARTESIAN_POINT('Ctrl Pts',(-6.76699752108346,0.00579220599325065,
41.69717978381));
#193808=CARTESIAN_POINT('',(-6.767,9.39225326770929E-10,41.3028202161458));
#193809=CARTESIAN_POINT('Ctrl Pts',(3.09910619832134,6.0156321173694,40.651395695404));
#193810=CARTESIAN_POINT('Ctrl Pts',(2.93375330764826,6.10081787314653,40.6601451433063));
#193811=CARTESIAN_POINT('Ctrl Pts',(2.7648862784307,6.17918207037039,40.6688945912086));
#193812=CARTESIAN_POINT('Ctrl Pts',(2.59307866646702,6.25045854553997,40.6776440391109));
#193813=CARTESIAN_POINT('Ctrl Pts',(2.4212724418538,6.32173444515035,40.6863934163612));
#193814=CARTESIAN_POINT('Ctrl Pts',(2.24652594672472,6.38592262741835,40.6951427936115));
#193815=CARTESIAN_POINT('Ctrl Pts',(2.06943269687133,6.44280508110558,40.7038921708618));
#193816=CARTESIAN_POINT('Ctrl Pts',(1.89234081822086,6.49968709436164,40.7126414803672));
#193817=CARTESIAN_POINT('Ctrl Pts',(1.71290249405596,6.54926340459543,40.7213907898725));
#193818=CARTESIAN_POINT('Ctrl Pts',(1.53172716625063,6.59136563150382,40.7301400993779));
#193819=CARTESIAN_POINT('Ctrl Pts',(1.35055318107334,6.6334675464071,40.7388893440451));
#193820=CARTESIAN_POINT('Ctrl Pts',(1.16764249714415,6.66809542395777,40.7476385887124));
#193821=CARTESIAN_POINT('Ctrl Pts',(0.983616340614261,6.6951316562467,40.7563878333796));
#193822=CARTESIAN_POINT('Ctrl Pts',(0.79959148671378,6.72216769715962,40.7651370161153));
#193823=CARTESIAN_POINT('Ctrl Pts',(0.614451459526685,6.74161215869371,
40.773886198851));
#193824=CARTESIAN_POINT('Ctrl Pts',(0.428825047910289,6.75339900185712,
40.7826353815867));
#193825=CARTESIAN_POINT('Ctrl Pts',(0.24319988859693,6.76518576550222,40.7913845052972));
#193826=CARTESIAN_POINT('Ctrl Pts',(0.0570886373916788,6.76931499599835,
40.8001336290078));
#193827=CARTESIAN_POINT('Ctrl Pts',(-0.12887662681151,6.76577266947846,
40.8088827527183));
#193828=CARTESIAN_POINT('Ctrl Pts',(-0.314840698188363,6.76223036567992,
40.8176318203098));
#193829=CARTESIAN_POINT('Ctrl Pts',(-0.500658497951302,6.75101660879222,
40.8263808879014));
#193830=CARTESIAN_POINT('Ctrl Pts',(-0.685698951926112,6.73216948296219,
40.8351299554929));
#193831=CARTESIAN_POINT('Ctrl Pts',(-0.870738280459781,6.71332247176294,
40.8438789698714));
#193832=CARTESIAN_POINT('Ctrl Pts',(-1.05499998761247,6.68684221356187,
40.85262798425));
#193833=CARTESIAN_POINT('Ctrl Pts',(-1.2378582916142,6.65281863948522,40.8613769986285));
#193834=CARTESIAN_POINT('Ctrl Pts',(-1.4300741291548,6.61705395369219,40.8705737323268));
#193835=CARTESIAN_POINT('Ctrl Pts',(-1.62073882531976,6.57295372728672,
40.879770466025));
#193836=CARTESIAN_POINT('Ctrl Pts',(-1.80913696085859,6.52068343479848,
40.8889671997233));
#193837=CARTESIAN_POINT('Ctrl Pts',(-1.98838356180497,6.47095219816924,
40.897717197437));
#193838=CARTESIAN_POINT('Ctrl Pts',(-2.16557827566964,6.41382586852771,
40.9064671951507));
#193839=CARTESIAN_POINT('Ctrl Pts',(-2.34011918616184,6.34949849945311,
40.9152171928643));
#193840=CARTESIAN_POINT('Ctrl Pts',(-2.51465655685641,6.28517243497734,
40.9239670131226));
#193841=CARTESIAN_POINT('Ctrl Pts',(-2.68653996289935,6.21364572244706,
40.9327168333809));
#193842=CARTESIAN_POINT('Ctrl Pts',(-2.85518555374665,6.13516132254698,
40.9414666536392));
#193843=CARTESIAN_POINT('Ctrl Pts',(-3.02382794853427,6.05667841003134,
40.9502163080767));
#193844=CARTESIAN_POINT('Ctrl Pts',(-3.18923239104086,5.97123819494855,
40.9589659625142));
#193845=CARTESIAN_POINT('Ctrl Pts',(-3.35083705962576,5.87913088813632,
40.9677156169518));
#193846=CARTESIAN_POINT('Ctrl Pts',(-3.51243888037353,5.78702520446166,
40.9764651172007));
#193847=CARTESIAN_POINT('Ctrl Pts',(-3.67024081218725,5.68825280608986,
40.9852146174496));
#193848=CARTESIAN_POINT('Ctrl Pts',(-3.82370687539524,5.58314917685845,
40.9939641176986));
#193849=CARTESIAN_POINT('Ctrl Pts',(-3.97717043813042,5.47804726011487,
41.0027134753891));
#193850=CARTESIAN_POINT('Ctrl Pts',(-4.12629803717796,5.36661448087823,
41.0114628330795));
#193851=CARTESIAN_POINT('Ctrl Pts',(-4.27058317202357,5.24922931208279,
41.02021219077));
#193852=CARTESIAN_POINT('Ctrl Pts',(-4.41486614770382,5.13184589990621,
41.0289614175301));
#193853=CARTESIAN_POINT('Ctrl Pts',(-4.55430658190064,5.00851045726989,
41.0377106442901));
#193854=CARTESIAN_POINT('Ctrl Pts',(-4.68843088997604,4.87964187107194,
41.0464598710502));
#193855=CARTESIAN_POINT('Ctrl Pts',(-4.82255336913684,4.75077504212174,
41.0552089785061));
#193856=CARTESIAN_POINT('Ctrl Pts',(-4.95135966061078,4.61637541912442,
41.063958085962));
#193857=CARTESIAN_POINT('Ctrl Pts',(-5.0744123086529,4.47689945406326,41.0727071934179));
#193858=CARTESIAN_POINT('Ctrl Pts',(-5.19746344222582,4.33742520560111,
41.0814561931943));
#193859=CARTESIAN_POINT('Ctrl Pts',(-5.31476088451055,4.19287495496041,
41.0902051929707));
#193860=CARTESIAN_POINT('Ctrl Pts',(-5.4259062762527,4.04373961591515,41.098954192747));
#193861=CARTESIAN_POINT('Ctrl Pts',(-5.53706380669211,3.89458798911648,
41.1077041480417));
#193862=CARTESIAN_POINT('Ctrl Pts',(-5.6420677706854,3.74085050160297,41.1164541033364));
#193863=CARTESIAN_POINT('Ctrl Pts',(-5.7405614816082,3.58304938228267,41.1252040586311));
#193864=CARTESIAN_POINT('Ctrl Pts',(-5.83905138948832,3.42525435598484,
41.1339536760722));
#193865=CARTESIAN_POINT('Ctrl Pts',(-5.9310313955474,3.26339625502476,41.1427032935133));
#193866=CARTESIAN_POINT('Ctrl Pts',(-6.01618907818077,3.09802485070382,
41.1514529109544));
#193867=CARTESIAN_POINT('Ctrl Pts',(-6.10134392542359,2.93265895255099,
41.1602022370703));
#193868=CARTESIAN_POINT('Ctrl Pts',(-6.17967677259356,2.76378023991569,
41.1689515631862));
#193869=CARTESIAN_POINT('Ctrl Pts',(-6.25092157006901,2.59196229232719,
41.177700889302));
#193870=CARTESIAN_POINT('Ctrl Pts',(-6.32216437405586,2.42014915234754,
41.1864499706045));
#193871=CARTESIAN_POINT('Ctrl Pts',(-6.38631941546912,2.24539720668566,
41.1951990519069));
#193872=CARTESIAN_POINT('Ctrl Pts',(-6.44316881035688,2.06829994953448,
41.2039481332094));
#193873=CARTESIAN_POINT('Ctrl Pts',(-6.50002334522881,1.89118668030262,
41.2126980055517));
#193874=CARTESIAN_POINT('Ctrl Pts',(-6.54957082409566,1.71172794813559,
41.2214478778941));
#193875=CARTESIAN_POINT('Ctrl Pts',(-6.59164294294715,1.53053334256234,
41.2301977502364));
#193876=CARTESIAN_POINT('Ctrl Pts',(-6.63371214080929,1.34935131699523,
41.2389470150913));
#193877=CARTESIAN_POINT('Ctrl Pts',(-6.6683069523865,1.16643393835711,41.2476962799462));
#193878=CARTESIAN_POINT('Ctrl Pts',(-6.69530988153113,0.982402458400636,
41.2564455448012));
#193879=CARTESIAN_POINT('Ctrl Pts',(-6.72231419689771,0.798361531006992,
41.2651952588082));
#193880=CARTESIAN_POINT('Ctrl Pts',(-6.74172580828731,0.613206671422632,
41.2739449728152));
#193881=CARTESIAN_POINT('Ctrl Pts',(-6.75347878027798,0.427566795173706,
41.2826946868222));
#193882=CARTESIAN_POINT('Ctrl Pts',(-6.76248992366113,0.28523449455753,
41.2894031965967));
#193883=CARTESIAN_POINT('Ctrl Pts',(-6.76699999998021,0.142617266737464,
41.2961117063712));
#193884=CARTESIAN_POINT('Ctrl Pts',(-6.767,9.39226155489418E-10,41.3028202161458));
#193885=CARTESIAN_POINT('Ctrl Pts',(-6.767,5.59359546727568E-13,41.3028202161899));
#193886=CARTESIAN_POINT('Ctrl Pts',(-6.76700000000002,-0.186007249526374,
41.3115697280011));
#193887=CARTESIAN_POINT('Ctrl Pts',(-6.75932637294523,-0.372014355749482,
41.3203192398123));
#193888=CARTESIAN_POINT('Ctrl Pts',(-6.74400518264183,-0.557389537487119,
41.3290687516235));
#193889=CARTESIAN_POINT('Ctrl Pts',(-6.72868405705088,-0.742763936251683,
41.3378182264791));
#193890=CARTESIAN_POINT('Ctrl Pts',(-6.70571545645723,-0.927506130242415,
41.3465677013348));
#193891=CARTESIAN_POINT('Ctrl Pts',(-6.67517739404794,-1.11098863990201,
41.3553171761905));
#193892=CARTESIAN_POINT('Ctrl Pts',(-6.64463945808663,-1.29447038982145,
41.3640666148175));
#193893=CARTESIAN_POINT('Ctrl Pts',(-6.60653217008308,-1.47669218313894,
41.3728160534445));
#193894=CARTESIAN_POINT('Ctrl Pts',(-6.56098496092621,-1.65703510599509,
41.3815654920716));
#193895=CARTESIAN_POINT('Ctrl Pts',(-6.51543793658235,-1.8373772970892,
41.3903148951967));
#193896=CARTESIAN_POINT('Ctrl Pts',(-6.46245112167353,-2.01584035511143,
41.3990642983219));
#193897=CARTESIAN_POINT('Ctrl Pts',(-6.4022044837418,-2.19181813761005,
41.4078137014471));
#193898=CARTESIAN_POINT('Ctrl Pts',(-6.34195808526423,-2.36779522067361,
41.4165630697972));
#193899=CARTESIAN_POINT('Ctrl Pts',(-6.27445201433015,-2.54128677684386,
41.4253124381473));
#193900=CARTESIAN_POINT('Ctrl Pts',(-6.19991555071804,-2.71170355385035,
41.4340618064974));
#193901=CARTESIAN_POINT('Ctrl Pts',(-6.12537937716586,-2.88211966767704,
41.4428111407991));
#193902=CARTESIAN_POINT('Ctrl Pts',(-6.04381298052405,-3.04946076372014,
41.4515604751009));
#193903=CARTESIAN_POINT('Ctrl Pts',(-5.95549339335707,-3.21315848374777,
41.4603098094027));
#193904=CARTESIAN_POINT('Ctrl Pts',(-5.86717414255276,-3.37685558033724,
41.4690591103829));
#193905=CARTESIAN_POINT('Ctrl Pts',(-5.77210188876456,-3.53690907646989,
41.4778084113631));
#193906=CARTESIAN_POINT('Ctrl Pts',(-5.67059953346844,-3.6927753696952,
41.4865577123433));
#193907=CARTESIAN_POINT('Ctrl Pts',(-5.56909755631226,-3.84864108225152,
41.4953069807286));
#193908=CARTESIAN_POINT('Ctrl Pts',(-5.46116568196686,-4.00031938297741,
41.5040562491138));
#193909=CARTESIAN_POINT('Ctrl Pts',(-5.34717048533433,-4.14729511860074,
41.5128055174991));
#193910=CARTESIAN_POINT('Ctrl Pts',(-5.2331757039167,-4.29427031888118,
41.5215547540162));
#193911=CARTESIAN_POINT('Ctrl Pts',(-5.11311782003353,-4.43654276189732,
41.5303039905332));
#193912=CARTESIAN_POINT('Ctrl Pts',(-4.98740458984599,-4.5736292435202,
41.5390532270502));
#193913=CARTESIAN_POINT('Ctrl Pts',(-4.86169180711571,-4.71071523720445,
41.5478024324257));
#193914=CARTESIAN_POINT('Ctrl Pts',(-4.7303239120398,-4.84261509523426,
41.5565516378011));
#193915=CARTESIAN_POINT('Ctrl Pts',(-4.59374707013388,-4.96888084538525,
41.5653008431766));
#193916=CARTESIAN_POINT('Ctrl Pts',(-4.45717070301225,-5.09514615659657,
41.574050018137));
#193917=CARTESIAN_POINT('Ctrl Pts',(-4.31538563570812,-5.21577720459717,
41.5827991930975));
#193918=CARTESIAN_POINT('Ctrl Pts',(-4.16887341029271,-5.33036429233073,
41.5915483680579));
#193919=CARTESIAN_POINT('Ctrl Pts',(-4.02236168203444,-5.4449509912381,
41.6002975133299));
#193920=CARTESIAN_POINT('Ctrl Pts',(-3.87112305347878,-5.55349359438802,
41.609046658602));
#193921=CARTESIAN_POINT('Ctrl Pts',(-3.71567117017448,-5.65562346299099,
41.617795803874));
#193922=CARTESIAN_POINT('Ctrl Pts',(-3.56021980145488,-5.75775299351849,
41.6265449201842));
#193923=CARTESIAN_POINT('Ctrl Pts',(-3.40055544538,-5.85346967464076,41.6352940364944));
#193924=CARTESIAN_POINT('Ctrl Pts',(-3.23722035986486,-5.94244842987101,
41.6440431528045));
#193925=CARTESIAN_POINT('Ctrl Pts',(-3.07388580146793,-6.03142689794727,
41.6527922408794));
#193926=CARTESIAN_POINT('Ctrl Pts',(-2.9068807889617,-6.11366734656976,
41.6615413289542));
#193927=CARTESIAN_POINT('Ctrl Pts',(-2.73677250720942,-6.18889046952543,
41.6702904170291));
#193928=CARTESIAN_POINT('Ctrl Pts',(-2.56666476031041,-6.26411335596508,
41.6790394775951));
#193929=CARTESIAN_POINT('Ctrl Pts',(-2.39345402574712,-6.33231884500728,
41.6877885381612));
#193930=CARTESIAN_POINT('Ctrl Pts',(-2.21772856065125,-6.39327529762889,
41.6965375987272));
#193931=CARTESIAN_POINT('Ctrl Pts',(-2.04200363348049,-6.45423156365258,
41.7052866325109));
#193932=CARTESIAN_POINT('Ctrl Pts',(-1.86376426188818,-6.5079387437579,
41.7140356662946));
#193933=CARTESIAN_POINT('Ctrl Pts',(-1.68361577752698,-6.55421443909659,
41.7227847000783));
#193934=CARTESIAN_POINT('Ctrl Pts',(-1.50346782967368,-6.60048999661966,
41.7315337078061));
#193935=CARTESIAN_POINT('Ctrl Pts',(-1.32141105794581,-6.63933404237792,
41.7402827155339));
#193936=CARTESIAN_POINT('Ctrl Pts',(-1.13806375486643,-6.67061465607626,
41.7490317232617));
#193937=CARTESIAN_POINT('Ctrl Pts',(-0.95471698259936,-6.70189517921348,
41.7577807056601));
#193938=CARTESIAN_POINT('Ctrl Pts',(-0.770079968898631,-6.72561226592268,
41.7665296880585));
#193939=CARTESIAN_POINT('Ctrl Pts',(-0.58477976555489,-6.74168536983132,
41.7752786704569));
#193940=CARTESIAN_POINT('Ctrl Pts',(-0.391489830647991,-6.75845151013872,
41.7844048894668));
#193941=CARTESIAN_POINT('Ctrl Pts',(-0.19747857823508,-6.76689983031635,
41.7935311084766));
#193942=CARTESIAN_POINT('Ctrl Pts',(-0.00346287644814537,-6.76699911397118,
41.8026573274865));
#193943=CARTESIAN_POINT('Ctrl Pts',(0.184489834657946,-6.7670952950118,
41.8114983521523));
#193944=CARTESIAN_POINT('Ctrl Pts',(0.37244640425339,-6.75935639738146,
41.8203393768181));
#193945=CARTESIAN_POINT('Ctrl Pts',(0.559755019492312,-6.74380925873153,
41.8291804014839));
#193946=CARTESIAN_POINT('Ctrl Pts',(0.74513470552573,-6.72842222659762,
41.8379303800937));
#193947=CARTESIAN_POINT('Ctrl Pts',(0.929879431232497,-6.70538706057469,
41.8466803587034));
#193948=CARTESIAN_POINT('Ctrl Pts',(1.11336163627216,-6.67478200894062,
41.8554303373131));
#193949=CARTESIAN_POINT('Ctrl Pts',(1.29684196301123,-6.64417727060934,
41.8641802263497));
#193950=CARTESIAN_POINT('Ctrl Pts',(1.47905951217929,-6.60600284890497,
41.8729301153862));
#193951=CARTESIAN_POINT('Ctrl Pts',(1.65939532067517,-6.56038841607121,
41.8816800044227));
#193952=CARTESIAN_POINT('Ctrl Pts',(1.83972934301246,-6.51477443503132,
41.8904298067949));
#193953=CARTESIAN_POINT('Ctrl Pts',(2.0181813840672,-6.46172066061999,41.8991796091671));
#193954=CARTESIAN_POINT('Ctrl Pts',(2.19414528354666,-6.40140730423319,
41.9079294115392));
#193955=CARTESIAN_POINT('Ctrl Pts',(2.37010749864455,-6.34109452518472,
41.9166791301556));
#193956=CARTESIAN_POINT('Ctrl Pts',(2.54358134866903,-6.27352239616324,
41.9254288487719));
#193957=CARTESIAN_POINT('Ctrl Pts',(2.71397759435987,-6.1989204396663,41.9341785673882));
#193958=CARTESIAN_POINT('Ctrl Pts',(2.88437226558544,-6.12431917249317,
41.9429282051569));
#193959=CARTESIAN_POINT('Ctrl Pts',(3.05168912681364,-6.04268832278592,
41.9516778429256));
#193960=CARTESIAN_POINT('Ctrl Pts',(3.21535986274252,-5.9543051612312,41.9604274806943));
#193961=CARTESIAN_POINT('Ctrl Pts',(3.37902914073247,-5.86592278697208,
41.9691770405234));
#193962=CARTESIAN_POINT('Ctrl Pts',(3.53905210621983,-5.7707883574169,41.9779266003525));
#193963=CARTESIAN_POINT('Ctrl Pts',(3.69488522832114,-5.66922500431358,
41.9866761601815));
#193964=CARTESIAN_POINT('Ctrl Pts',(3.85071701407354,-5.56766252216807,
41.9954256449786));
#193965=CARTESIAN_POINT('Ctrl Pts',(4.00235878822814,-5.45967138329069,
42.0041751297758));
#193966=CARTESIAN_POINT('Ctrl Pts',(4.14929549611731,-5.34561838199292,
42.0129246145729));
#193967=CARTESIAN_POINT('Ctrl Pts',(4.29623099276485,-5.23156632086691,
42.0216740272455));
#193968=CARTESIAN_POINT('Ctrl Pts',(4.43846127436411,-5.11145267304631,
42.030423439918));
#193969=CARTESIAN_POINT('Ctrl Pts',(4.57550326054814,-4.98568540049544,
42.0391728525906));
#193970=CARTESIAN_POINT('Ctrl Pts',(4.7125441625814,-4.85991912290012,42.0479221960459));
#193971=CARTESIAN_POINT('Ctrl Pts',(4.84439664019108,-4.72849950385063,
42.0566715395011));
#193972=CARTESIAN_POINT('Ctrl Pts',(4.97061286795079,-4.59187289860706,
42.0654208829564));
#193973=CARTESIAN_POINT('Ctrl Pts',(5.09682813913007,-4.45524732884316,
42.0741701601012));
#193974=CARTESIAN_POINT('Ctrl Pts',(5.21740705148149,-4.31341506235413,
42.082919437246));
#193975=CARTESIAN_POINT('Ctrl Pts',(5.33194007545994,-4.16685781275343,
42.0916687143908));
#193976=CARTESIAN_POINT('Ctrl Pts',(5.44647226944759,-4.0203016252147,42.100417928132));
#193977=CARTESIAN_POINT('Ctrl Pts',(5.55495848628365,-3.86902074887572,
42.1091671418731));
#193978=CARTESIAN_POINT('Ctrl Pts',(5.65703027292018,-3.71352898080312,
42.1179163556142));
#193979=CARTESIAN_POINT('Ctrl Pts',(5.75910135377216,-3.55803828789234,
42.1266655088581));
#193980=CARTESIAN_POINT('Ctrl Pts',(5.8547579359296,-3.39833700106354,42.135414662102));
#193981=CARTESIAN_POINT('Ctrl Pts',(5.94367514427595,-3.23496750823193,
42.1441638153458));
#193982=CARTESIAN_POINT('Ctrl Pts',(6.03259176732825,-3.07159909077361,
42.1529129109988));
#193983=CARTESIAN_POINT('Ctrl Pts',(6.11476896836098,-2.90456276731069,
42.1616620066517));
#193984=CARTESIAN_POINT('Ctrl Pts',(6.18992765548048,-2.73442583002683,
42.1704111023046));
#193985=CARTESIAN_POINT('Ctrl Pts',(6.265085872832,-2.56428995615813,42.1791601432726));
#193986=CARTESIAN_POINT('Ctrl Pts',(6.33322554827291,-2.39105376934855,
42.1879091842407));
#193987=CARTESIAN_POINT('Ctrl Pts',(6.39411526733147,-2.21530561053744,
42.1966582252087));
#193988=CARTESIAN_POINT('Ctrl Pts',(6.45500462602956,-2.03955849184755,
42.2054072143977));
#193989=CARTESIAN_POINT('Ctrl Pts',(6.5086440204084,-1.86129970164195,42.2141562035868));
#193990=CARTESIAN_POINT('Ctrl Pts',(6.55485128368692,-1.68113463135703,
42.2229051927758));
#193991=CARTESIAN_POINT('Ctrl Pts',(6.60199809554403,-1.49730620116532,
42.2318320782472));
#193992=CARTESIAN_POINT('Ctrl Pts',(6.64140720707935,-1.31149343245381,
42.2407589637186));
#193993=CARTESIAN_POINT('Ctrl Pts',(6.67293928722934,-1.12435326697228,
42.2496858491901));
#193994=CARTESIAN_POINT('Ctrl Pts',(6.70384625876298,-0.940923067003626,
42.2584357633675));
#193995=CARTESIAN_POINT('Ctrl Pts',(6.72718554579829,-0.756217899518716,
42.267185677545));
#193996=CARTESIAN_POINT('Ctrl Pts',(6.74287786815353,-0.570865181251564,
42.2759355917224));
#193997=CARTESIAN_POINT('Ctrl Pts',(6.75856988190862,-0.385516108071076,
42.2846853338269));
#193998=CARTESIAN_POINT('Ctrl Pts',(6.76661520773411,-0.199519795223544,
42.2934350759314));
#193999=CARTESIAN_POINT('Ctrl Pts',(6.76698651789579,-0.0135080204529134,
42.3021848180359));
#194000=CARTESIAN_POINT('Ctrl Pts',(6.76735782124896,0.172500343515658,
42.3109343997008));
#194001=CARTESIAN_POINT('Ctrl Pts',(6.7600553899517,0.358523882213577,42.3196839813658));
#194002=CARTESIAN_POINT('Ctrl Pts',(6.7451040274234,0.543930748566989,42.3284335630308));
#194003=CARTESIAN_POINT('Ctrl Pts',(6.73015291918002,0.729334461617808,
42.3371829958875));
#194004=CARTESIAN_POINT('Ctrl Pts',(6.7075531630656,0.914121237637212,42.3459324287441));
#194005=CARTESIAN_POINT('Ctrl Pts',(6.67738151874533,1.0976634516637,42.3546818616008));
#194006=CARTESIAN_POINT('Ctrl Pts',(6.64721034747522,1.28120278799909,42.3634311572784));
#194007=CARTESIAN_POINT('Ctrl Pts',(6.60946757205088,1.46349731860569,42.3721804529559));
#194008=CARTESIAN_POINT('Ctrl Pts',(6.56428138111464,1.64392790278397,42.3809297486334));
#194009=CARTESIAN_POINT('Ctrl Pts',(6.51909583859785,1.82435589779289,42.389678918759));
#194010=CARTESIAN_POINT('Ctrl Pts',(6.46646716392804,2.00291972192496,42.3984280888846));
#194011=CARTESIAN_POINT('Ctrl Pts',(6.40657409872806,2.17901292274891,42.4071772590102));
#194012=CARTESIAN_POINT('Ctrl Pts',(6.34668181341991,2.35510383059207,42.4159263152093));
#194013=CARTESIAN_POINT('Ctrl Pts',(6.27952541913957,2.52872390822811,42.4246753714084));
#194014=CARTESIAN_POINT('Ctrl Pts',(6.20533299175416,2.69928350890518,42.4334244276075));
#194015=CARTESIAN_POINT('Ctrl Pts',(6.12831602991443,2.87633637965847,42.4425065637657));
#194016=CARTESIAN_POINT('Ctrl Pts',(6.04371690605161,3.05009086601678,42.4515886999239));
#194017=CARTESIAN_POINT('Ctrl Pts',(5.95184520316519,3.21991112882942,42.4606708360821));
#194018=CARTESIAN_POINT('Ctrl Pts',(5.86333549509153,3.38351691183227,42.4694206164257));
#194019=CARTESIAN_POINT('Ctrl Pts',(5.76807618099238,3.54347103712216,42.4781703967693));
#194020=CARTESIAN_POINT('Ctrl Pts',(5.66639083308876,3.69923018027909,42.4869201771128));
#194021=CARTESIAN_POINT('Ctrl Pts',(5.56470914082053,3.85498372382262,42.4956696428977));
#194022=CARTESIAN_POINT('Ctrl Pts',(5.45660203371912,4.00654234702208,42.5044191086826));
#194023=CARTESIAN_POINT('Ctrl Pts',(5.34243669839054,4.15339127986877,42.5131685744676));
#194024=CARTESIAN_POINT('Ctrl Pts',(5.22827486050418,4.30023571401491,42.5219177722136));
#194025=CARTESIAN_POINT('Ctrl Pts',(5.10805534166926,4.44237052028683,42.5306669699596));
#194026=CARTESIAN_POINT('Ctrl Pts',(4.98218644339754,4.57931296628936,42.5394161677056));
#194027=CARTESIAN_POINT('Ctrl Pts',(4.85632073219396,4.71625194483556,42.5481651439172));
#194028=CARTESIAN_POINT('Ctrl Pts',(4.72480612170136,4.84799861524685,42.5569141201289));
#194029=CARTESIAN_POINT('Ctrl Pts',(4.58808925235138,4.97410554898645,42.5656630963405));
#194030=CARTESIAN_POINT('Ctrl Pts',(4.45136349473871,5.10022068121361,42.5744126413422));
#194031=CARTESIAN_POINT('Ctrl Pts',(4.309435012099,5.22069514871983,42.5831621863439));
#194032=CARTESIAN_POINT('Ctrl Pts',(4.16278587431598,5.335119751664,42.5919117313456));
#194033=CARTESIAN_POINT('Ctrl Pts',(4.01614535740258,5.44953762807982,42.6006607619993));
#194034=CARTESIAN_POINT('Ctrl Pts',(3.86478496657727,5.5579061753292,42.6094097926531));
#194035=CARTESIAN_POINT('Ctrl Pts',(3.70921874746993,5.65985735539489,42.6181588233068));
#194036=CARTESIAN_POINT('Ctrl Pts',(3.5536504160569,5.76180991977176,42.6269079727564));
#194037=CARTESIAN_POINT('Ctrl Pts',(3.39387638174305,5.85734478552939,42.635657122206));
#194038=CARTESIAN_POINT('Ctrl Pts',(3.23043927904314,5.94613749121354,42.6444062716556));
#194039=CARTESIAN_POINT('Ctrl Pts',(3.18691767070278,5.96978206944228,42.6467360795718));
#194040=CARTESIAN_POINT('Ctrl Pts',(3.14313645919552,5.99294880633466,42.6490658874879));
#194041=CARTESIAN_POINT('Ctrl Pts',(3.09910619832134,6.0156321173694,42.651395695404));
#194042=CARTESIAN_POINT('Origin',(0.,0.,4.30282021618968));
#194043=CARTESIAN_POINT('',(3.09910619832132,6.01563211736941,45.0457774706169));
#194044=CARTESIAN_POINT('',(3.09910619832132,6.01563211736941,44.6516492284231));
#194045=CARTESIAN_POINT('',(3.09910619832133,6.0156321173694,4.30282021618968));
#194046=CARTESIAN_POINT('',(-6.76699922072898,0.00324756113893609,43.6971797837735));
#194047=CARTESIAN_POINT('Ctrl Pts',(-6.76699922072936,0.00324756035794601,
43.6971797838101));
#194048=CARTESIAN_POINT('Ctrl Pts',(-6.76708539128521,-0.176307557950773,
43.7055896024739));
#194049=CARTESIAN_POINT('Ctrl Pts',(-6.76002065673009,-0.355840812135418,
43.7139994211378));
#194050=CARTESIAN_POINT('Ctrl Pts',(-6.74583735173559,-0.534759220517912,
43.7224092398016));
#194051=CARTESIAN_POINT('Ctrl Pts',(-6.73172457194684,-0.712787973240606,
43.7307772414001));
#194052=CARTESIAN_POINT('Ctrl Pts',(-6.71056392607303,-0.890207646468588,
43.7391452429986));
#194053=CARTESIAN_POINT('Ctrl Pts',(-6.6824392701373,-1.06644005969713,
43.7475132445971));
#194054=CARTESIAN_POINT('Ctrl Pts',(-6.65430116369288,-1.24275675540054,
43.7558852481602));
#194055=CARTESIAN_POINT('Ctrl Pts',(-6.61919245918884,-1.41788472534874,
43.7642572517233));
#194056=CARTESIAN_POINT('Ctrl Pts',(-6.57724817004016,-1.59125595354843,
43.7726292552864));
#194057=CARTESIAN_POINT('Ctrl Pts',(-6.53527761298665,-1.76473575669399,
43.7810065018754));
#194058=CARTESIAN_POINT('Ctrl Pts',(-6.48646301442609,-1.93645629632921,
43.7893837484644));
#194059=CARTESIAN_POINT('Ctrl Pts',(-6.43098936457008,-2.10586438138513,
43.7977609950534));
#194060=CARTESIAN_POINT('Ctrl Pts',(-6.37511427176604,-2.27649841211543,
43.8061988647774));
#194061=CARTESIAN_POINT('Ctrl Pts',(-6.31248349073343,-2.4447860605028,
43.8146367345015));
#194062=CARTESIAN_POINT('Ctrl Pts',(-6.24333507747812,-2.61018315647223,
43.8230746042255));
#194063=CARTESIAN_POINT('Ctrl Pts',(-6.17452783411554,-2.77476420321026,
43.8314708425227));
#194064=CARTESIAN_POINT('Ctrl Pts',(-6.09926733108904,-2.93648287925634,
43.8398670808199));
#194065=CARTESIAN_POINT('Ctrl Pts',(-6.01783402746916,-3.09482836645821,
43.8482633191171));
#194066=CARTESIAN_POINT('Ctrl Pts',(-5.93579506250964,-3.25435155044554,
43.8567220045546));
#194067=CARTESIAN_POINT('Ctrl Pts',(-5.84749129217044,-3.41045087005848,
43.865180689992));
#194068=CARTESIAN_POINT('Ctrl Pts',(-5.75325351341666,-3.56263427962496,
43.8736393754295));
#194069=CARTESIAN_POINT('Ctrl Pts',(-5.65901573466289,-3.71481768919144,
43.882098060867));
#194070=CARTESIAN_POINT('Ctrl Pts',(-5.55884418801034,-3.86308493565928,
43.8905567463044));
#194071=CARTESIAN_POINT('Ctrl Pts',(-5.4531104642186,-4.00697832100819,
43.8990154317419));
#194072=CARTESIAN_POINT('Ctrl Pts',(-5.3522439502868,-4.14424790385744,
43.9070847409644));
#194073=CARTESIAN_POINT('Ctrl Pts',(-5.24600592261595,-4.27795795198755,
43.9151540501869));
#194074=CARTESIAN_POINT('Ctrl Pts',(-5.1346786257687,-4.40764839909833,
43.9232233594094));
#194075=CARTESIAN_POINT('Ctrl Pts',(-5.0234901843183,-4.53717708697296,
43.9312826040102));
#194076=CARTESIAN_POINT('Ctrl Pts',(-4.90722534389093,-4.66269586987897,
43.939341848611));
#194077=CARTESIAN_POINT('Ctrl Pts',(-4.78621000370878,-4.78377286254249,
43.9474010932117));
#194078=CARTESIAN_POINT('Ctrl Pts',(-4.66531904592962,-4.90472540943516,
43.955452054332));
#194079=CARTESIAN_POINT('Ctrl Pts',(-4.53968756656092,-5.02124498958605,
43.9635030154522));
#194080=CARTESIAN_POINT('Ctrl Pts',(-4.40968210592735,-5.13293217612157,
43.9715539765725));
#194081=CARTESIAN_POINT('Ctrl Pts',(-4.27978178117675,-5.24452904082819,
43.9795984268516));
#194082=CARTESIAN_POINT('Ctrl Pts',(-4.14551479706261,-5.35130104816285,
43.9876428771306));
#194083=CARTESIAN_POINT('Ctrl Pts',(-4.0072848964897,-5.4528851774419,43.9956873274097));
#194084=CARTESIAN_POINT('Ctrl Pts',(-3.86913652570079,-5.55440939108704,
44.0037270329679));
#194085=CARTESIAN_POINT('Ctrl Pts',(-3.72703019139388,-5.65075159757475,
44.0117667385261));
#194086=CARTESIAN_POINT('Ctrl Pts',(-3.5814030120783,-5.74158875792028,
44.0198064440844));
#194087=CARTESIAN_POINT('Ctrl Pts',(-3.43263254795316,-5.83438658980803,
44.0280196823888));
#194088=CARTESIAN_POINT('Ctrl Pts',(-3.28018782247643,-5.92143876717896,
44.0362329206933));
#194089=CARTESIAN_POINT('Ctrl Pts',(-3.12456687615307,-6.00244707069101,
44.0444461589977));
#194090=CARTESIAN_POINT('Ctrl Pts',(-2.9722829910162,-6.08171827086433,
44.0524832765459));
#194091=CARTESIAN_POINT('Ctrl Pts',(-2.81695807331615,-6.15520200520335,
44.0605203940941));
#194092=CARTESIAN_POINT('Ctrl Pts',(-2.65908395749321,-6.22266514501642,
44.0685575116422));
#194093=CARTESIAN_POINT('Ctrl Pts',(-2.50119313959246,-6.29013542200082,
44.0765954794663));
#194094=CARTESIAN_POINT('Ctrl Pts',(-2.34075293012029,-6.3515836892884,
44.0846334472905));
#194095=CARTESIAN_POINT('Ctrl Pts',(-2.17827511616023,-6.40682499513738,
44.0926714151146));
#194096=CARTESIAN_POINT('Ctrl Pts',(-2.01574792023636,-6.46208309050427,
44.1007118259223));
#194097=CARTESIAN_POINT('Ctrl Pts',(-1.85118224066694,-6.51113034921,44.10875223673));
#194098=CARTESIAN_POINT('Ctrl Pts',(-1.6851048415235,-6.55383175501737,
44.1167926475377));
#194099=CARTESIAN_POINT('Ctrl Pts',(-1.5127506533799,-6.59814703312552,
44.1251369405255));
#194100=CARTESIAN_POINT('Ctrl Pts',(-1.33876867553726,-6.63562730071976,
44.1334812335133));
#194101=CARTESIAN_POINT('Ctrl Pts',(-1.16375790499993,-6.66618005596535,
44.1418255265011));
#194102=CARTESIAN_POINT('Ctrl Pts',(-0.994822856547196,-6.69567213334968,
44.1498801367167));
#194103=CARTESIAN_POINT('Ctrl Pts',(-0.824929623160702,-6.71870964961567,
44.1579347469322));
#194104=CARTESIAN_POINT('Ctrl Pts',(-0.654620370348223,-6.73526251683816,
44.1659893571478));
#194105=CARTESIAN_POINT('Ctrl Pts',(-0.484182191025886,-6.75182791481494,
44.174050064817));
#194106=CARTESIAN_POINT('Ctrl Pts',(-0.313327735545389,-6.76189886758439,
44.1821107724862));
#194107=CARTESIAN_POINT('Ctrl Pts',(-0.142598077855184,-6.76549737921699,
44.1901714801554));
#194108=CARTESIAN_POINT('Ctrl Pts',(0.0283722984240017,-6.76910096453542,
44.1982435529396));
#194109=CARTESIAN_POINT('Ctrl Pts',(0.19921715589738,-6.76621390754684,
44.2063156257237));
#194110=CARTESIAN_POINT('Ctrl Pts',(0.369401038750248,-6.75690993521227,
44.2143876985078));
#194111=CARTESIAN_POINT('Ctrl Pts',(0.387226507463855,-6.75593541479951,
44.2152331868024));
#194112=CARTESIAN_POINT('Ctrl Pts',(0.405044734747265,-6.75489054063013,
44.2160786750969));
#194113=CARTESIAN_POINT('Ctrl Pts',(0.422855112852365,-6.75377542960488,
44.2169241633914));
#194114=CARTESIAN_POINT('Ctrl Pts',(0.598389763461888,-6.74278517307849,
44.2252570854381));
#194115=CARTESIAN_POINT('Ctrl Pts',(0.773721088922039,-6.72493313061228,
44.2335900074848));
#194116=CARTESIAN_POINT('Ctrl Pts',(0.948279363318132,-6.70022799978515,
44.2419229295316));
#194117=CARTESIAN_POINT('Ctrl Pts',(1.12263135216511,-6.67555206443156,
44.2502460040852));
#194118=CARTESIAN_POINT('Ctrl Pts',(1.29621176825503,-6.64403922228022,
44.2585690786388));
#194119=CARTESIAN_POINT('Ctrl Pts',(1.46845310760402,-6.60575010659411,
44.2668921531925));
#194120=CARTESIAN_POINT('Ctrl Pts',(1.64052251534514,-6.56749921117062,
44.2752069196384));
#194121=CARTESIAN_POINT('Ctrl Pts',(1.81125517187407,-6.52248559348524,
44.2835216860844));
#194122=CARTESIAN_POINT('Ctrl Pts',(1.98009067900291,-6.47082142412583,
44.2918364525304));
#194123=CARTESIAN_POINT('Ctrl Pts',(2.14878862434689,-6.41919934908337,
44.3001444443699));
#194124=CARTESIAN_POINT('Ctrl Pts',(2.31559216901612,-6.36093762086397,
44.3084524362095));
#194125=CARTESIAN_POINT('Ctrl Pts',(2.47995284387544,-6.29619908295109,
44.316760428049));
#194126=CARTESIAN_POINT('Ctrl Pts',(2.64420973573751,-6.23150142318323,
44.3250631739361));
#194127=CARTESIAN_POINT('Ctrl Pts',(2.80602650900681,-6.16033523112452,
44.3333659198231));
#194128=CARTESIAN_POINT('Ctrl Pts',(2.96487134177183,-6.0829127008975,44.3416686657101));
#194129=CARTESIAN_POINT('Ctrl Pts',(3.12365125971659,-6.00552181079088,
44.3499680185296));
#194130=CARTESIAN_POINT('Ctrl Pts',(3.27946134495144,-5.92187982926044,
44.358267371349));
#194131=CARTESIAN_POINT('Ctrl Pts',(3.43179093234813,-5.83224656514565,
44.3665667241684));
#194132=CARTESIAN_POINT('Ctrl Pts',(3.58408812179778,-5.74263236452202,
44.3748643118548));
#194133=CARTESIAN_POINT('Ctrl Pts',(3.73290598846745,-5.64702959623125,
44.3831618995411));
#194134=CARTESIAN_POINT('Ctrl Pts',(3.87775939203867,-5.54574351169037,
44.3914594872275));
#194135=CARTESIAN_POINT('Ctrl Pts',(4.0226060587724,-5.44446213775951,44.3997566890099));
#194136=CARTESIAN_POINT('Ctrl Pts',(4.16348834482187,-5.33749817378009,
44.4080538907923));
#194137=CARTESIAN_POINT('Ctrl Pts',(4.29995081804031,-5.22519970550739,
44.4163510925747));
#194138=CARTESIAN_POINT('Ctrl Pts',(4.43642962034128,-5.11288779961398,
44.4246492871992));
#194139=CARTESIAN_POINT('Ctrl Pts',(4.56848728772864,-4.99524033900479,
44.4329474818238));
#194140=CARTESIAN_POINT('Ctrl Pts',(4.69570200726063,-4.87264524247442,
44.4412456764483));
#194141=CARTESIAN_POINT('Ctrl Pts',(4.82300619838821,-4.74996392338316,
44.4495497072899));
#194142=CARTESIAN_POINT('Ctrl Pts',(4.9454603847808,-4.62232825689607,44.4578537381314));
#194143=CARTESIAN_POINT('Ctrl Pts',(5.06267950072881,-4.49016316773682,
44.466157768973));
#194144=CARTESIAN_POINT('Ctrl Pts',(5.17994124077344,-4.35795001971374,
44.4744648193887));
#194145=CARTESIAN_POINT('Ctrl Pts',(5.29196389093938,-4.22120443144269,
44.4827718698045));
#194146=CARTESIAN_POINT('Ctrl Pts',(5.39840302243799,-4.0803840269431,44.4910789202202));
#194147=CARTESIAN_POINT('Ctrl Pts',(5.50495595533231,-3.93941306166431,
44.4993948522748));
#194148=CARTESIAN_POINT('Ctrl Pts',(5.60591323799116,-3.79435885764037,
44.5077107843295));
#194149=CARTESIAN_POINT('Ctrl Pts',(5.70097346544871,-3.64570851087271,
44.5160267163841));
#194150=CARTESIAN_POINT('Ctrl Pts',(5.77263188405087,-3.53365272204359,
44.522295442603));
#194151=CARTESIAN_POINT('Ctrl Pts',(5.84094021461499,-3.41955404417975,
44.5285641688219));
#194152=CARTESIAN_POINT('Ctrl Pts',(5.90578678435719,-3.30363004250052,
44.5348328950408));
#194153=CARTESIAN_POINT('Ctrl Pts',(5.99320022705266,-3.14736401149683,
44.5432831637642));
#194154=CARTESIAN_POINT('Ctrl Pts',(6.07448193940124,-2.98749380427392,
44.5517334324875));
#194155=CARTESIAN_POINT('Ctrl Pts',(6.1493359130113,-2.82452771785825,44.5601837012109));
#194156=CARTESIAN_POINT('Ctrl Pts',(6.22412382544997,-2.66170545454302,
44.5686265122854));
#194157=CARTESIAN_POINT('Ctrl Pts',(6.29249516810258,-2.49579305775209,
44.5770693233599));
#194158=CARTESIAN_POINT('Ctrl Pts',(6.35419972174159,-2.32732354781606,
44.5855121344344));
#194159=CARTESIAN_POINT('Ctrl Pts',(6.41585822025235,-2.15897978038082,
44.5939486439522));
#194160=CARTESIAN_POINT('Ctrl Pts',(6.47085973539428,-1.98808301478628,
44.6023851534699));
#194161=CARTESIAN_POINT('Ctrl Pts',(6.51900192249456,-1.81518674921131,
44.6108216629877));
#194162=CARTESIAN_POINT('Ctrl Pts',(6.56710966126934,-1.64241420021824,
44.6192521357289));
#194163=CARTESIAN_POINT('Ctrl Pts',(6.6083677735055,-1.46764532376163,44.6276826084701));
#194164=CARTESIAN_POINT('Ctrl Pts',(6.64262351808422,-1.29144949455812,
44.6361130812113));
#194165=CARTESIAN_POINT('Ctrl Pts',(6.67686453621108,-1.11532941146462,
44.6445399297151));
#194166=CARTESIAN_POINT('Ctrl Pts',(6.7041091246507,-0.937783923435001,
44.6529667782189));
#194167=CARTESIAN_POINT('Ctrl Pts',(6.72425533318508,-0.759393978203656,
44.6613936267227));
#194168=CARTESIAN_POINT('Ctrl Pts',(6.74439532330438,-0.581059095577448,
44.6698178741593));
#194169=CARTESIAN_POINT('Ctrl Pts',(6.75744126575737,-0.401880604658297,
44.6782421215959));
#194170=CARTESIAN_POINT('Ctrl Pts',(6.76334285848322,-0.222446349945432,
44.6866663690325));
#194171=CARTESIAN_POINT('Ctrl Pts',(6.76500570151503,-0.171888642225172,
44.6890399996436));
#194172=CARTESIAN_POINT('Ctrl Pts',(6.76610167319886,-0.121310658110363,
44.6914136302547));
#194173=CARTESIAN_POINT('Ctrl Pts',(6.76663039405615,-0.0707255981630307,
44.6937872608658));
#194174=CARTESIAN_POINT('Ctrl Pts',(6.76855020804263,0.112951486361858,
44.702406041803));
#194175=CARTESIAN_POINT('Ctrl Pts',(6.76298624196818,0.296639716696282,
44.7110248227403));
#194176=CARTESIAN_POINT('Ctrl Pts',(6.7499743874485,0.479723637930475,44.7196436036775));
#194177=CARTESIAN_POINT('Ctrl Pts',(6.736954716787,0.662917536561891,44.728267561864));
#194178=CARTESIAN_POINT('Ctrl Pts',(6.71647825069517,0.84550609823776,44.7368915200505));
#194179=CARTESIAN_POINT('Ctrl Pts',(6.68863272004142,1.02687941667527,44.745515478237));
#194180=CARTESIAN_POINT('Ctrl Pts',(6.65978122537314,1.21480513426844,44.7544509906081));
#194181=CARTESIAN_POINT('Ctrl Pts',(6.62301836171851,1.40142581027156,44.7633865029792));
#194182=CARTESIAN_POINT('Ctrl Pts',(6.57849929254961,1.58607567849844,44.7723220153503));
#194183=CARTESIAN_POINT('Ctrl Pts',(6.53545213559658,1.76462055841857,44.780962097245));
#194184=CARTESIAN_POINT('Ctrl Pts',(6.48515357156149,1.94132258415672,44.7896021791398));
#194185=CARTESIAN_POINT('Ctrl Pts',(6.42779458480289,2.1155958441013,44.7982422610345));
#194186=CARTESIAN_POINT('Ctrl Pts',(6.36749368273758,2.29880749713741,44.8073254886438));
#194187=CARTESIAN_POINT('Ctrl Pts',(6.29938922163399,2.47933433172568,44.8164087162531));
#194188=CARTESIAN_POINT('Ctrl Pts',(6.22376038338747,2.65651946918833,44.8254919438625));
#194189=CARTESIAN_POINT('Ctrl Pts',(6.14813154514096,2.83370460665094,44.8345751714718));
#194190=CARTESIAN_POINT('Ctrl Pts',(6.06497852743741,3.00754771169249,44.8436583990811));
#194191=CARTESIAN_POINT('Ctrl Pts',(5.97463653142741,3.17742148877562,44.8527416266904));
#194192=CARTESIAN_POINT('Ctrl Pts',(5.88467877765542,3.34657275934829,44.8617862215502));
#194193=CARTESIAN_POINT('Ctrl Pts',(5.78751076787639,3.51194501315713,44.87083081641));
#194194=CARTESIAN_POINT('Ctrl Pts',(5.68345990189301,3.67295147579904,44.8798754112698));
#194195=CARTESIAN_POINT('Ctrl Pts',(5.57950451895655,3.8338101896694,44.8889117062902));
#194196=CARTESIAN_POINT('Ctrl Pts',(5.46867901895975,3.9903109113421,44.8979480013106));
#194197=CARTESIAN_POINT('Ctrl Pts',(5.35135512372724,4.14189417293081,44.906984296331));
#194198=CARTESIAN_POINT('Ctrl Pts',(5.23423884232874,4.29320919604988,44.9160046009187));
#194199=CARTESIAN_POINT('Ctrl Pts',(5.11064727398898,4.43962394765089,44.9250249055064));
#194200=CARTESIAN_POINT('Ctrl Pts',(4.98099342848918,4.58061059961962,44.9340452100941));
#194201=CARTESIAN_POINT('Ctrl Pts',(4.85150285682168,4.72141970628777,44.9430541553604));
#194202=CARTESIAN_POINT('Ctrl Pts',(4.71596540390273,4.85681418032171,44.9520631006267));
#194203=CARTESIAN_POINT('Ctrl Pts',(4.57483371642635,4.9862997770941,44.961072045893));
#194204=CARTESIAN_POINT('Ctrl Pts',(4.43402250913482,5.11549133948817,44.9700605337518));
#194205=CARTESIAN_POINT('Ctrl Pts',(4.28764259918326,5.23880064719497,44.9790490216106));
#194206=CARTESIAN_POINT('Ctrl Pts',(4.13618240226534,5.35577110556365,44.9880375094694));
#194207=CARTESIAN_POINT('Ctrl Pts',(4.00329692485621,5.4583965842002,44.9959236704846));
#194208=CARTESIAN_POINT('Ctrl Pts',(3.86650145993055,5.55614306622334,45.0038098314999));
#194209=CARTESIAN_POINT('Ctrl Pts',(3.72614913619673,5.64872566291021,45.0116959925152));
#194210=CARTESIAN_POINT('Ctrl Pts',(3.58161445003416,5.7440671307268,45.0198171534412));
#194211=CARTESIAN_POINT('Ctrl Pts',(3.43337156207057,5.83388832813256,45.0279383143671));
#194212=CARTESIAN_POINT('Ctrl Pts',(3.28188888549178,5.91789610784826,45.036059475293));
#194213=CARTESIAN_POINT('Ctrl Pts',(3.22146616366386,5.9514047493628,45.0392988070677));
#194214=CARTESIAN_POINT('Ctrl Pts',(3.16052829945035,5.98398895658282,45.0425381388423));
#194215=CARTESIAN_POINT('Ctrl Pts',(3.09910619832133,6.01563211736941,45.0457774706169));
#194216=CARTESIAN_POINT('Ctrl Pts',(3.09910619832137,6.01563211736938,43.0457451347211));
#194217=CARTESIAN_POINT('Ctrl Pts',(2.9398432053638,6.0976805071326,43.0541676123953));
#194218=CARTESIAN_POINT('Ctrl Pts',(2.77728306715381,6.17341931069911,43.0625900900695));
#194219=CARTESIAN_POINT('Ctrl Pts',(2.61195574420795,6.24259370696981,43.0710125677437));
#194220=CARTESIAN_POINT('Ctrl Pts',(2.44662669862841,6.3117688240055,43.0794351331761));
#194221=CARTESIAN_POINT('Ctrl Pts',(2.27853071565575,6.37437926216612,43.0878576986086));
#194222=CARTESIAN_POINT('Ctrl Pts',(2.10821854588746,6.43021800274113,43.0962802640411));
#194223=CARTESIAN_POINT('Ctrl Pts',(1.93790130694559,6.48605840530113,43.1047030801629));
#194224=CARTESIAN_POINT('Ctrl Pts',(1.76536806660186,6.53512660429797,43.1131258962847));
#194225=CARTESIAN_POINT('Ctrl Pts',(1.59118572837604,6.57726515945742,43.1215487124066));
#194226=CARTESIAN_POINT('Ctrl Pts',(1.41697388813736,6.61941085180545,43.129972955137));
#194227=CARTESIAN_POINT('Ctrl Pts',(1.24111271735234,6.65462448186093,43.1383971978675));
#194228=CARTESIAN_POINT('Ctrl Pts',(1.06418068793334,6.68279944809282,43.146821440598));
#194229=CARTESIAN_POINT('Ctrl Pts',(0.887193981831948,6.71098312113538,
43.1552482866425));
#194230=CARTESIAN_POINT('Ctrl Pts',(0.709136086613573,6.73212374129672,
43.1636751326871));
#194231=CARTESIAN_POINT('Ctrl Pts',(0.530592361061849,6.74616637405147,
43.1721019787316));
#194232=CARTESIAN_POINT('Ctrl Pts',(0.35188828729745,6.7602216183447,43.1805363928366));
#194233=CARTESIAN_POINT('Ctrl Pts',(0.172697844219148,6.76716611134562,
43.1889708069416));
#194234=CARTESIAN_POINT('Ctrl Pts',(-0.00639066836027456,6.76699698236655,
43.1974052210466));
#194235=CARTESIAN_POINT('Ctrl Pts',(-0.185565022304428,6.76682777231995,
43.2058436779659));
#194236=CARTESIAN_POINT('Ctrl Pts',(-0.364637014990389,6.75953814839691,
43.2142821348853));
#194237=CARTESIAN_POINT('Ctrl Pts',(-0.54302114782077,6.74517731664776,
43.2227205918047));
#194238=CARTESIAN_POINT('Ctrl Pts',(-0.721605831932116,6.73080033949847,
43.2311685357973));
#194239=CARTESIAN_POINT('Ctrl Pts',(-0.899500779066923,6.70933630365108,
43.23961647979));
#194240=CARTESIAN_POINT('Ctrl Pts',(-1.07612714782113,6.6808861209964,43.2480644237827));
#194241=CARTESIAN_POINT('Ctrl Pts',(-1.18159592783921,6.66389768332968,
43.2531089386694));
#194242=CARTESIAN_POINT('Ctrl Pts',(-1.28661256810347,6.64441922430788,
43.2581534535561));
#194243=CARTESIAN_POINT('Ctrl Pts',(-1.39105602147073,6.62248081500657,
43.2631979684429));
#194244=CARTESIAN_POINT('Ctrl Pts',(-1.56165025698225,6.58664739469695,
43.2714375002937));
#194245=CARTESIAN_POINT('Ctrl Pts',(-1.73109537092469,6.54416838885696,
43.2796770321445));
#194246=CARTESIAN_POINT('Ctrl Pts',(-1.89883704638144,6.49512947301972,
43.2879165639953));
#194247=CARTESIAN_POINT('Ctrl Pts',(-2.06639254030146,6.44614498695186,
43.2961469505415));
#194248=CARTESIAN_POINT('Ctrl Pts',(-2.23224802183424,6.39061518765132,
43.3043773370878));
#194249=CARTESIAN_POINT('Ctrl Pts',(-2.39585840662889,6.32867691507362,
43.3126077236341));
#194250=CARTESIAN_POINT('Ctrl Pts',(-2.55931638192079,6.26679634043078,
43.3208304432519));
#194251=CARTESIAN_POINT('Ctrl Pts',(-2.72053309462844,6.19851930662708,
43.3290531628697));
#194252=CARTESIAN_POINT('Ctrl Pts',(-2.87897760889233,6.1240327340321,43.3372758824875));
#194253=CARTESIAN_POINT('Ctrl Pts',(-3.03728172990059,6.04961216190722,
43.3454913161832));
#194254=CARTESIAN_POINT('Ctrl Pts',(-3.19281822737472,5.96899316803299,
43.353706749879));
#194255=CARTESIAN_POINT('Ctrl Pts',(-3.34507530189061,5.88241108939876,
43.3619221835748));
#194256=CARTESIAN_POINT('Ctrl Pts',(-3.49725412809285,5.79587350722991,
43.3701333951755));
#194257=CARTESIAN_POINT('Ctrl Pts',(-3.64615657927168,5.70337911914984,
43.3783446067763));
#194258=CARTESIAN_POINT('Ctrl Pts',(-3.79129429437053,5.60520977069311,
43.3865558183771));
#194259=CARTESIAN_POINT('Ctrl Pts',(-3.93638333828836,5.50707334281892,
43.3947642763905));
#194260=CARTESIAN_POINT('Ctrl Pts',(-4.07770986661839,5.40326594483289,
43.402972734404));
#194261=CARTESIAN_POINT('Ctrl Pts',(-4.21481334735167,5.29411347129869,
43.4111811924175));
#194262=CARTESIAN_POINT('Ctrl Pts',(-4.27589594178423,5.24548366090626,
43.4148382397009));
#194263=CARTESIAN_POINT('Ctrl Pts',(-4.33614069485268,5.1957934790453,43.4184952869842));
#194264=CARTESIAN_POINT('Ctrl Pts',(-4.39550886582442,5.14507442224687,
43.4221523342676));
#194265=CARTESIAN_POINT('Ctrl Pts',(-4.53932626537561,5.02220921119109,
43.4310114084435));
#194266=CARTESIAN_POINT('Ctrl Pts',(-4.67784794423911,4.89343143470241,
43.4398704826195));
#194267=CARTESIAN_POINT('Ctrl Pts',(-4.81062718086157,4.75921791124927,
43.4487295567954));
#194268=CARTESIAN_POINT('Ctrl Pts',(-4.94365588295502,4.62475222758876,
43.4576052753893));
#194269=CARTESIAN_POINT('Ctrl Pts',(-5.07092039950944,4.48483057181061,
43.4664809939832));
#194270=CARTESIAN_POINT('Ctrl Pts',(-5.19201350524001,4.3399636820376,43.4753567125771));
#194271=CARTESIAN_POINT('Ctrl Pts',(-5.31345217648036,4.19468338309228,
43.4842577599641));
#194272=CARTESIAN_POINT('Ctrl Pts',(-5.42868402661054,4.04442980962973,
43.4931588073511));
#194273=CARTESIAN_POINT('Ctrl Pts',(-5.53734268853429,3.88974612921407,
43.5020598547381));
#194274=CARTESIAN_POINT('Ctrl Pts',(-5.6461490733983,3.73485215421465,43.510973003221));
#194275=CARTESIAN_POINT('Ctrl Pts',(-5.74836427551116,3.5755162572007,43.519886151704));
#194276=CARTESIAN_POINT('Ctrl Pts',(-5.84366668278929,3.41230841227144,
43.5287993001869));
#194277=CARTESIAN_POINT('Ctrl Pts',(-5.93918068747235,3.24873820129669,
43.5377322382968));
#194278=CARTESIAN_POINT('Ctrl Pts',(-6.02775106666007,3.08127907205079,
43.5466651764067));
#194279=CARTESIAN_POINT('Ctrl Pts',(-6.10910207358148,2.91052587251211,
43.5555981145166));
#194280=CARTESIAN_POINT('Ctrl Pts',(-6.1865364367665,2.74799358473288,43.5641009763752));
#194281=CARTESIAN_POINT('Ctrl Pts',(-6.25743014094712,2.58247711366446,
43.5726038382338));
#194282=CARTESIAN_POINT('Ctrl Pts',(-6.321586751586,2.41450407789517,43.5811067000924));
#194283=CARTESIAN_POINT('Ctrl Pts',(-6.3896604380815,2.23627546415156,43.5901287033858));
#194284=CARTESIAN_POINT('Ctrl Pts',(-6.45025510538802,2.05500312572533,
43.5991507066792));
#194285=CARTESIAN_POINT('Ctrl Pts',(-6.50311556953205,1.87130352677213,
43.6081727099725));
#194286=CARTESIAN_POINT('Ctrl Pts',(-6.55579193961244,1.68824368772661,
43.6171632928599));
#194287=CARTESIAN_POINT('Ctrl Pts',(-6.60078777408356,1.50277368155816,
43.6261538757472));
#194288=CARTESIAN_POINT('Ctrl Pts',(-6.63789736808551,1.31552557206748,
43.6351444586345));
#194289=CARTESIAN_POINT('Ctrl Pts',(-6.67492295241124,1.12870135977843,
43.6441146884035));
#194290=CARTESIAN_POINT('Ctrl Pts',(-6.70409785465102,0.940107305172852,
43.6530849181725));
#194291=CARTESIAN_POINT('Ctrl Pts',(-6.72526609179442,0.750389895028057,
43.6620551479416));
#194292=CARTESIAN_POINT('Ctrl Pts',(-6.74636212545597,0.561319598645588,
43.6709947808395));
#194293=CARTESIAN_POINT('Ctrl Pts',(-6.75950593593842,0.371133826403229,
43.6799344137374));
#194294=CARTESIAN_POINT('Ctrl Pts',(-6.76459261047664,0.180487712282064,
43.6888740466354));
#194295=CARTESIAN_POINT('Ctrl Pts',(-6.76616793920673,0.121445149484368,
43.6916426256814));
#194296=CARTESIAN_POINT('Ctrl Pts',(-6.76697085269131,0.0623585310693763,
43.6944112047275));
#194297=CARTESIAN_POINT('Ctrl Pts',(-6.76699922072898,0.00324756113897147,
43.6971797837735));
#194298=CARTESIAN_POINT('',(-6.767,4.1676968679568E-13,43.3028202161899));
#194299=CARTESIAN_POINT('Ctrl Pts',(3.09910619832134,6.0156321173694,42.651395695404));
#194300=CARTESIAN_POINT('Ctrl Pts',(2.93375330764829,6.10081787314652,42.6601451433063));
#194301=CARTESIAN_POINT('Ctrl Pts',(2.76488627843076,6.17918207037036,42.6688945912086));
#194302=CARTESIAN_POINT('Ctrl Pts',(2.5930786664671,6.25045854553994,42.6776440391109));
#194303=CARTESIAN_POINT('Ctrl Pts',(2.42127244185385,6.32173444515034,42.6863934163612));
#194304=CARTESIAN_POINT('Ctrl Pts',(2.24652594672474,6.38592262741835,42.6951427936115));
#194305=CARTESIAN_POINT('Ctrl Pts',(2.06943269687131,6.44280508110559,42.7038921708618));
#194306=CARTESIAN_POINT('Ctrl Pts',(1.89234081822081,6.49968709436165,42.7126414803672));
#194307=CARTESIAN_POINT('Ctrl Pts',(1.71290249405587,6.54926340459545,42.7213907898725));
#194308=CARTESIAN_POINT('Ctrl Pts',(1.53172716625051,6.59136563150385,42.7301400993779));
#194309=CARTESIAN_POINT('Ctrl Pts',(1.35055318107338,6.63346754640709,42.7388893440451));
#194310=CARTESIAN_POINT('Ctrl Pts',(1.16764249714434,6.66809542395773,42.7476385887123));
#194311=CARTESIAN_POINT('Ctrl Pts',(0.983616340614606,6.69513165624665,
42.7563878333796));
#194312=CARTESIAN_POINT('Ctrl Pts',(0.79959148671406,6.72216769715958,42.7651370161153));
#194313=CARTESIAN_POINT('Ctrl Pts',(0.614451459526898,6.74161215869369,
42.773886198851));
#194314=CARTESIAN_POINT('Ctrl Pts',(0.428825047910436,6.75339900185711,
42.7826353815867));
#194315=CARTESIAN_POINT('Ctrl Pts',(0.24319988859717,6.7651857655022,42.7913845052972));
#194316=CARTESIAN_POINT('Ctrl Pts',(0.0570886373920126,6.76931499599834,
42.8001336290077));
#194317=CARTESIAN_POINT('Ctrl Pts',(-0.128876626811083,6.76577266947847,
42.8088827527183));
#194318=CARTESIAN_POINT('Ctrl Pts',(-0.31484069818794,6.76223036567994,
42.8176318203098));
#194319=CARTESIAN_POINT('Ctrl Pts',(-0.500658497950882,6.75101660879225,
42.8263808879014));
#194320=CARTESIAN_POINT('Ctrl Pts',(-0.685698951925696,6.73216948296224,
42.8351299554929));
#194321=CARTESIAN_POINT('Ctrl Pts',(-0.870738280459434,6.71332247176299,
42.8438789698714));
#194322=CARTESIAN_POINT('Ctrl Pts',(-1.05499998761219,6.68684221356192,
42.8526279842499));
#194323=CARTESIAN_POINT('Ctrl Pts',(-1.23785829161398,6.65281863948526,
42.8613769986285));
#194324=CARTESIAN_POINT('Ctrl Pts',(-1.43007412917385,6.61705395368865,
42.8705737323277));
#194325=CARTESIAN_POINT('Ctrl Pts',(-1.62073882535776,6.57295372727794,
42.8797704660269));
#194326=CARTESIAN_POINT('Ctrl Pts',(-1.809136960915,6.52068343478283,42.8889671997261));
#194327=CARTESIAN_POINT('Ctrl Pts',(-1.98838356186096,6.47095219815204,
42.8977171974397));
#194328=CARTESIAN_POINT('Ctrl Pts',(-2.16557827572514,6.41382586850897,
42.9064671951534));
#194329=CARTESIAN_POINT('Ctrl Pts',(-2.34011918621678,6.34949849943286,
42.9152171928671));
#194330=CARTESIAN_POINT('Ctrl Pts',(-2.51465655691076,6.28517243495559,
42.9239670131254));
#194331=CARTESIAN_POINT('Ctrl Pts',(-2.68653996295306,6.21364572242384,
42.9327168333837));
#194332=CARTESIAN_POINT('Ctrl Pts',(-2.85518555379966,6.13516132252231,
42.941466653642));
#194333=CARTESIAN_POINT('Ctrl Pts',(-3.02382794858666,6.05667841000518,
42.9502163080795));
#194334=CARTESIAN_POINT('Ctrl Pts',(-3.18923239109257,5.97123819492094,
42.958965962517));
#194335=CARTESIAN_POINT('Ctrl Pts',(-3.35083705967673,5.87913088810727,
42.9677156169545));
#194336=CARTESIAN_POINT('Ctrl Pts',(-3.51243888042371,5.78702520443121,
42.9764651172035));
#194337=CARTESIAN_POINT('Ctrl Pts',(-3.67024081223657,5.68825280605804,
42.9852146174524));
#194338=CARTESIAN_POINT('Ctrl Pts',(-3.82370687544365,5.5831491768253,42.9939641177013));
#194339=CARTESIAN_POINT('Ctrl Pts',(-3.97717043817782,5.47804726008046,
43.0027134753918));
#194340=CARTESIAN_POINT('Ctrl Pts',(-4.1262980372243,5.3666144808426,43.0114628330823));
#194341=CARTESIAN_POINT('Ctrl Pts',(-4.27058317206879,5.24922931204599,
43.0202121907727));
#194342=CARTESIAN_POINT('Ctrl Pts',(-4.41486614774799,5.13184589986821,
43.0289614175328));
#194343=CARTESIAN_POINT('Ctrl Pts',(-4.5543065819437,5.00851045723074,43.0377106442929));
#194344=CARTESIAN_POINT('Ctrl Pts',(-4.68843089001795,4.87964187103167,
43.0464598710529));
#194345=CARTESIAN_POINT('Ctrl Pts',(-4.82255336917797,4.75077504208001,
43.0552089785089));
#194346=CARTESIAN_POINT('Ctrl Pts',(-4.95135966065106,4.61637541908125,
43.0639580859648));
#194347=CARTESIAN_POINT('Ctrl Pts',(-5.07441230869225,4.47689945401866,
43.0727071934207));
#194348=CARTESIAN_POINT('Ctrl Pts',(-5.19746344226398,4.33742520555538,
43.0814561931971));
#194349=CARTESIAN_POINT('Ctrl Pts',(-5.31476088454749,4.1928749549136,43.0902051929735));
#194350=CARTESIAN_POINT('Ctrl Pts',(-5.42590627628836,4.0437396158673,43.0989541927498));
#194351=CARTESIAN_POINT('Ctrl Pts',(-5.5370638067265,3.89458798906759,43.1077041480445));
#194352=CARTESIAN_POINT('Ctrl Pts',(-5.64206777071846,3.7408505015531,43.1164541033392));
#194353=CARTESIAN_POINT('Ctrl Pts',(-5.74056148163991,3.58304938223188,
43.1252040586339));
#194354=CARTESIAN_POINT('Ctrl Pts',(-5.83905138951862,3.42525435593318,
43.133953676075));
#194355=CARTESIAN_POINT('Ctrl Pts',(-5.93103139557628,3.26339625497228,
43.1427032935161));
#194356=CARTESIAN_POINT('Ctrl Pts',(-6.01618907820819,3.09802485065058,
43.1514529109572));
#194357=CARTESIAN_POINT('Ctrl Pts',(-6.10134392544964,2.93265895249682,
43.1602022370731));
#194358=CARTESIAN_POINT('Ctrl Pts',(-6.17967677261819,2.76378023986065,
43.168951563189));
#194359=CARTESIAN_POINT('Ctrl Pts',(-6.25092157009217,2.59196229227133,
43.1777008893049));
#194360=CARTESIAN_POINT('Ctrl Pts',(-6.32216437407745,2.42014915229113,
43.1864499706073));
#194361=CARTESIAN_POINT('Ctrl Pts',(-6.38631941548912,2.24539720662877,
43.1951990519098));
#194362=CARTESIAN_POINT('Ctrl Pts',(-6.44316881037528,2.06829994947717,
43.2039481332122));
#194363=CARTESIAN_POINT('Ctrl Pts',(-6.50002334524563,1.89118668024481,
43.2126980055546));
#194364=CARTESIAN_POINT('Ctrl Pts',(-6.54957082411088,1.71172794807733,
43.2214478778969));
#194365=CARTESIAN_POINT('Ctrl Pts',(-6.59164294296077,1.5305333425037,43.2301977502393));
#194366=CARTESIAN_POINT('Ctrl Pts',(-6.63371214082125,1.34935131693641,
43.2389470150942));
#194367=CARTESIAN_POINT('Ctrl Pts',(-6.6683069523968,1.16643393829817,43.2476962799491));
#194368=CARTESIAN_POINT('Ctrl Pts',(-6.69530988153979,0.982402458341639,
43.256445544804));
#194369=CARTESIAN_POINT('Ctrl Pts',(-6.72231419690474,0.798361530947818,
43.265195258811));
#194370=CARTESIAN_POINT('Ctrl Pts',(-6.7417258082927,0.613206671363342,
43.273944972818));
#194371=CARTESIAN_POINT('Ctrl Pts',(-6.75347878028173,0.427566795114374,
43.282694686825));
#194372=CARTESIAN_POINT('Ctrl Pts',(-6.76248992368216,0.285234494205584,
43.2894031966133));
#194373=CARTESIAN_POINT('Ctrl Pts',(-6.76699999999999,0.142617266091775,
43.2961117064016));
#194374=CARTESIAN_POINT('Ctrl Pts',(-6.767,4.16769702918876E-13,43.3028202161899));
#194375=CARTESIAN_POINT('Ctrl Pts',(-6.76699999999983,1.53523534223817E-6,
43.3028542630209));
#194376=CARTESIAN_POINT('Ctrl Pts',(-6.76700004292237,-0.189192154842816,
43.3117861533015));
#194377=CARTESIAN_POINT('Ctrl Pts',(-6.7590614542694,-0.378469857747368,
43.320718043582));
#194378=CARTESIAN_POINT('Ctrl Pts',(-6.74318913218751,-0.567176628175301,
43.3296499338625));
#194379=CARTESIAN_POINT('Ctrl Pts',(-6.72733425191513,-0.755676032124229,
43.3385720090493));
#194380=CARTESIAN_POINT('Ctrl Pts',(-6.70356305940782,-0.943605498803956,
43.3474940842361));
#194381=CARTESIAN_POINT('Ctrl Pts',(-6.67193243972188,-1.13031257614295,
43.3564161594229));
#194382=CARTESIAN_POINT('Ctrl Pts',(-6.64035725344944,-1.31669244488702,
43.3653225984607));
#194383=CARTESIAN_POINT('Ctrl Pts',(-6.6009501808069,-1.50185394688418,
43.3742290374985));
#194384=CARTESIAN_POINT('Ctrl Pts',(-6.55381956237659,-1.68515226131347,
43.3831354765363));
#194385=CARTESIAN_POINT('Ctrl Pts',(-6.5067453619389,-1.86823115738388,
43.3920312540672));
#194386=CARTESIAN_POINT('Ctrl Pts',(-6.45196612552911,-2.04945106631216,
43.4009270315981));
#194387=CARTESIAN_POINT('Ctrl Pts',(-6.38964113496009,-2.22817754373972,
43.409822809129));
#194388=CARTESIAN_POINT('Ctrl Pts',(-6.32742899935208,-2.40658039224321,
43.418702478633));
#194389=CARTESIAN_POINT('Ctrl Pts',(-6.25769846414383,-2.58249857695067,
43.427582148137));
#194390=CARTESIAN_POINT('Ctrl Pts',(-6.18065849880635,-2.75531296246594,
43.436461817641));
#194391=CARTESIAN_POINT('Ctrl Pts',(-6.15069230357275,-2.82253248408489,
43.4399157380679));
#194392=CARTESIAN_POINT('Ctrl Pts',(-6.11962074893652,-2.88928255697687,
43.4433696584948));
#194393=CARTESIAN_POINT('Ctrl Pts',(-6.08745817512892,-2.95552735836705,
43.4468235789217));
#194394=CARTESIAN_POINT('Ctrl Pts',(-6.01183187788457,-3.11129378025841,
43.4549450437778));
#194395=CARTESIAN_POINT('Ctrl Pts',(-5.9301986729754,-3.26420576152668,
43.463066508634));
#194396=CARTESIAN_POINT('Ctrl Pts',(-5.8428117574739,-3.41377207304834,
43.4711879734902));
#194397=CARTESIAN_POINT('Ctrl Pts',(-5.75543107394573,-3.56332771829053,
43.4793088591664));
#194398=CARTESIAN_POINT('Ctrl Pts',(-5.66229768186461,-3.70953785285899,
43.4874297448425));
#194399=CARTESIAN_POINT('Ctrl Pts',(-5.56370996621465,-3.85193722844023,
43.4955506305187));
#194400=CARTESIAN_POINT('Ctrl Pts',(-5.46511046651363,-3.99435362481866,
43.503672486873));
#194401=CARTESIAN_POINT('Ctrl Pts',(-5.36105555449261,-4.13295805483247,
43.5117943432272));
#194402=CARTESIAN_POINT('Ctrl Pts',(-5.25188600112966,-4.26731560013298,
43.5199161995814));
#194403=CARTESIAN_POINT('Ctrl Pts',(-5.14263679901109,-4.40177117103644,
43.5280439815416));
#194404=CARTESIAN_POINT('Ctrl Pts',(-5.02826573372788,-4.53197338423848,
43.5361717635017));
#194405=CARTESIAN_POINT('Ctrl Pts',(-4.9091532175445,-4.65752119551511,
43.5442995454619));
#194406=CARTESIAN_POINT('Ctrl Pts',(-4.78999217934918,-4.78312015030373,
43.5524306383783));
#194407=CARTESIAN_POINT('Ctrl Pts',(-4.66608610211582,-4.90406066824777,
43.5605617312947));
#194408=CARTESIAN_POINT('Ctrl Pts',(-4.53785086875385,-5.01997992953657,
43.5686928242112));
#194409=CARTESIAN_POINT('Ctrl Pts',(-4.40947567199396,-5.13602571185449,
43.5768327918757));
#194410=CARTESIAN_POINT('Ctrl Pts',(-4.27676216205594,-5.24703905648351,
43.5849727595403));
#194411=CARTESIAN_POINT('Ctrl Pts',(-4.14015835320787,-5.35269818039119,
43.5931127272048));
#194412=CARTESIAN_POINT('Ctrl Pts',(-4.06930971156866,-5.40749757045778,
43.5973344663853));
#194413=CARTESIAN_POINT('Ctrl Pts',(-3.9974150918705,-5.46085743637847,
43.6015562055658));
#194414=CARTESIAN_POINT('Ctrl Pts',(-3.92453983276044,-5.51273762309405,
43.6057779447463));
#194415=CARTESIAN_POINT('Ctrl Pts',(-3.77884574203878,-5.61645782556472,
43.6142181542039));
#194416=CARTESIAN_POINT('Ctrl Pts',(-3.62892939749098,-5.71447561839207,
43.6226583636615));
#194417=CARTESIAN_POINT('Ctrl Pts',(-3.47526558528633,-5.80644625495875,
43.6310985731191));
#194418=CARTESIAN_POINT('Ctrl Pts',(-3.32171819618477,-5.89834721014274,
43.6395323878677));
#194419=CARTESIAN_POINT('Ctrl Pts',(-3.16442928442298,-5.98420997156264,
43.6479662026162));
#194420=CARTESIAN_POINT('Ctrl Pts',(-3.00390273054915,-6.0637329579558,
43.6564000173647));
#194421=CARTESIAN_POINT('Ctrl Pts',(-2.84347312207337,-6.14320791872712,
43.6648287387533));
#194422=CARTESIAN_POINT('Ctrl Pts',(-2.67981006769599,-6.21635058991948,
43.6732574601418));
#194423=CARTESIAN_POINT('Ctrl Pts',(-2.51344251891016,-6.2829050370139,
43.6816861815304));
#194424=CARTESIAN_POINT('Ctrl Pts',(-2.34714989596315,-6.34942951042767,
43.6901111069321));
#194425=CARTESIAN_POINT('Ctrl Pts',(-2.17815551628463,-6.40937155213659,
43.6985360323338));
#194426=CARTESIAN_POINT('Ctrl Pts',(-2.00700916747056,-6.46252297494478,
43.7069609577356));
#194427=CARTESIAN_POINT('Ctrl Pts',(-1.83591363777016,-6.51565861530587,
43.7153833814933));
#194428=CARTESIAN_POINT('Ctrl Pts',(-1.66266773136378,-6.56200755903514,
43.723805805251));
#194429=CARTESIAN_POINT('Ctrl Pts',(-1.48783766182772,-6.60141106825253,
43.7322282290087));
#194430=CARTESIAN_POINT('Ctrl Pts',(-1.31300484271726,-6.64081519717385,
43.7406507852269));
#194431=CARTESIAN_POINT('Ctrl Pts',(-1.13658813447718,-6.67327359354366,
43.7490733414451));
#194432=CARTESIAN_POINT('Ctrl Pts',(-0.959165905965437,-6.69867821027653,
43.7574958976634));
#194433=CARTESIAN_POINT('Ctrl Pts',(-0.781737684097593,-6.7240836851821,
43.7659187383971));
#194434=CARTESIAN_POINT('Ctrl Pts',(-0.603304204417205,-6.74243485789718,
43.7743415791308));
#194435=CARTESIAN_POINT('Ctrl Pts',(-0.424451113328692,-6.7536753144043,
43.7827644198646));
#194436=CARTESIAN_POINT('Ctrl Pts',(-0.245567010679107,-6.76491771990823,
43.7911887210452));
#194437=CARTESIAN_POINT('Ctrl Pts',(-0.0662634844669385,-6.76904693017065,
43.7996130222259));
#194438=CARTESIAN_POINT('Ctrl Pts',(0.112871275286189,-6.76605860713719,
43.8080373234065));
#194439=CARTESIAN_POINT('Ctrl Pts',(0.292062112296732,-6.76306934862388,
43.8164642617733));
#194440=CARTESIAN_POINT('Ctrl Pts',(0.471083744130887,-6.75295812013209,
43.82489120014));
#194441=CARTESIAN_POINT('Ctrl Pts',(0.649350191357576,-6.73577266013216,
43.8333181385068));
#194442=CARTESIAN_POINT('Ctrl Pts',(0.827776922528825,-6.71857174824345,
43.8417526537504));
#194443=CARTESIAN_POINT('Ctrl Pts',(1.00544677998836,-6.69428392735286,
43.8501871689941));
#194444=CARTESIAN_POINT('Ctrl Pts',(1.18177995471074,-6.66300871518595,
43.8586216842377));
#194445=CARTESIAN_POINT('Ctrl Pts',(1.358198299867,-6.63171839682365,43.8670602734245));
#194446=CARTESIAN_POINT('Ctrl Pts',(1.53327834788571,-6.59343402240147,
43.8754988626113));
#194447=CARTESIAN_POINT('Ctrl Pts',(1.70645211213654,-6.54830590221507,
43.883937451798));
#194448=CARTESIAN_POINT('Ctrl Pts',(1.87981944547621,-6.50312733900029,
43.8923854734183));
#194449=CARTESIAN_POINT('Ctrl Pts',(2.05127591668672,-6.45108983649194,
43.9008334950386));
#194450=CARTESIAN_POINT('Ctrl Pts',(2.22026911063925,-6.39239345443796,
43.9092815166589));
#194451=CARTESIAN_POINT('Ctrl Pts',(2.31632213002314,-6.35903137285744,
43.9140832365712));
#194452=CARTESIAN_POINT('Ctrl Pts',(2.41157970716454,-6.32351896044428,
43.9188849564835));
#194453=CARTESIAN_POINT('Ctrl Pts',(2.50594349886653,-6.28589979084049,
43.9236866763959));
#194454=CARTESIAN_POINT('Ctrl Pts',(2.66786745142743,-6.22134701562412,
43.9319262082467));
#194455=CARTESIAN_POINT('Ctrl Pts',(2.82751985065107,-6.1504440960898,43.9401657400975));
#194456=CARTESIAN_POINT('Ctrl Pts',(2.98436927829437,-6.07337048192952,
43.9484052719484));
#194457=CARTESIAN_POINT('Ctrl Pts',(3.14104461403513,-5.9963824140943,43.9566356584947));
#194458=CARTESIAN_POINT('Ctrl Pts',(3.29492285631175,-5.91323744479937,
43.964866045041));
#194459=CARTESIAN_POINT('Ctrl Pts',(3.44549045535073,-5.82416384746231,
43.9730964315874));
#194460=CARTESIAN_POINT('Ctrl Pts',(3.59591779475377,-5.73517322568185,
43.9813191512051));
#194461=CARTESIAN_POINT('Ctrl Pts',(3.74304032822838,-5.64026515465837,
43.9895418708229));
#194462=CARTESIAN_POINT('Ctrl Pts',(3.88636703173365,-5.53971482069734,
43.9977645904408));
#194463=CARTESIAN_POINT('Ctrl Pts',(4.02956673745311,-5.43925358157673,
44.0059800241365));
#194464=CARTESIAN_POINT('Ctrl Pts',(4.16897702648647,-5.33316024751826,
44.0141954578323));
#194465=CARTESIAN_POINT('Ctrl Pts',(4.30413402933039,-5.2217544233294,44.0224108915281));
#194466=CARTESIAN_POINT('Ctrl Pts',(4.43922157196963,-5.11040585308364,
44.0306221031289));
#194467=CARTESIAN_POINT('Ctrl Pts',(4.57005990778635,-4.9937504559764,44.0388333147297));
#194468=CARTESIAN_POINT('Ctrl Pts',(4.69621623288276,-4.87214963789173,
44.0470445263305));
#194469=CARTESIAN_POINT('Ctrl Pts',(4.8223302521095,-4.75058959801106,44.055252984344));
#194470=CARTESIAN_POINT('Ctrl Pts',(4.94376513239408,-4.62408768760204,
44.0634614423575));
#194471=CARTESIAN_POINT('Ctrl Pts',(5.0601230393961,-4.4930439377078,44.0716699003711));
#194472=CARTESIAN_POINT('Ctrl Pts',(5.11196302773182,-4.43466108568667,
44.0753269476542));
#194473=CARTESIAN_POINT('Ctrl Pts',(5.16279577137245,-4.3753772209428,44.0789839949374));
#194474=CARTESIAN_POINT('Ctrl Pts',(5.2125885036707,-4.31523001604782,44.0826410422206));
#194475=CARTESIAN_POINT('Ctrl Pts',(5.33320972475314,-4.16952543298392,
44.0915001163965));
#194476=CARTESIAN_POINT('Ctrl Pts',(5.44759988295617,-4.01890384442965,
44.1003591905724));
#194477=CARTESIAN_POINT('Ctrl Pts',(5.55540062721881,-3.86391160239165,
44.1092182647483));
#194478=CARTESIAN_POINT('Ctrl Pts',(5.66340390738988,-3.70862816111607,
44.1180939833421));
#194479=CARTESIAN_POINT('Ctrl Pts',(5.7647928845205,-3.54895786881008,44.1269697019359));
#194480=CARTESIAN_POINT('Ctrl Pts',(5.85925393477225,-3.3854737228128,44.1358454205297));
#194481=CARTESIAN_POINT('Ctrl Pts',(5.95398455017322,-3.22152303925221,
44.1447464679167));
#194482=CARTESIAN_POINT('Ctrl Pts',(6.04174754497938,-3.05373694815608,
44.1536475153037));
#194483=CARTESIAN_POINT('Ctrl Pts',(6.12227510881517,-2.88271339053715,
44.1625485626907));
#194484=CARTESIAN_POINT('Ctrl Pts',(6.2029121509786,-2.7114573240457,44.1714617111737));
#194485=CARTESIAN_POINT('Ctrl Pts',(6.27629400830026,-2.53695523627329,
44.1803748596567));
#194486=CARTESIAN_POINT('Ctrl Pts',(6.34220155888343,-2.35982380412112,
44.1892880081397));
#194487=CARTESIAN_POINT('Ctrl Pts',(6.40825544225084,-2.18229909175425,
44.1982209462496));
#194488=CARTESIAN_POINT('Ctrl Pts',(6.46680173505636,-2.0021336021734,44.2071538843595));
#194489=CARTESIAN_POINT('Ctrl Pts',(6.51767076636749,-1.81996065376112,
44.2160868224694));
#194490=CARTESIAN_POINT('Ctrl Pts',(6.5660907084741,-1.64655842084732,44.2245896843281));
#194491=CARTESIAN_POINT('Ctrl Pts',(6.60755518447319,-1.47133765518869,
44.2330925461867));
#194492=CARTESIAN_POINT('Ctrl Pts',(6.64196113402503,-1.29485184252906,
44.2415954080454));
#194493=CARTESIAN_POINT('Ctrl Pts',(6.67523353421345,-1.1241805876189,44.2498181319113));
#194494=CARTESIAN_POINT('Ctrl Pts',(6.70196764817162,-0.951998966731906,
44.2580408557772));
#194495=CARTESIAN_POINT('Ctrl Pts',(6.72202969380216,-0.778849019799167,
44.266263579643));
#194496=CARTESIAN_POINT('Ctrl Pts',(6.74207050443702,-0.605882346219521,
44.2744776000343));
#194497=CARTESIAN_POINT('Ctrl Pts',(6.75545326882495,-0.431949740957379,
44.2826916204255));
#194498=CARTESIAN_POINT('Ctrl Pts',(6.76209501746225,-0.257604298900969,
44.2909056408167));
#194499=CARTESIAN_POINT('Ctrl Pts',(6.76873106950894,-0.0834083919538031,
44.2991126160886));
#194500=CARTESIAN_POINT('Ctrl Pts',(6.76863760704288,0.091199290158767,
44.3073195913606));
#194501=CARTESIAN_POINT('Ctrl Pts',(6.76178334459151,0.265659558090598,
44.3155265666325));
#194502=CARTESIAN_POINT('Ctrl Pts',(6.75493358525376,0.440005209108513,
44.3237281500855));
#194503=CARTESIAN_POINT('Ctrl Pts',(6.74133188731707,0.614203281693499,
44.3319297335385));
#194504=CARTESIAN_POINT('Ctrl Pts',(6.72099902742316,0.787693514875522,
44.3401313169915));
#194505=CARTESIAN_POINT('Ctrl Pts',(6.70067544555053,0.96110458329256,44.3483291580066));
#194506=CARTESIAN_POINT('Ctrl Pts',(6.67362686251875,1.13380810023515,44.3565269990216));
#194507=CARTESIAN_POINT('Ctrl Pts',(6.6399259981915,1.30524776902343,44.3647248400367));
#194508=CARTESIAN_POINT('Ctrl Pts',(6.60622810786051,1.47667230879515,44.3729219576178));
#194509=CARTESIAN_POINT('Ctrl Pts',(6.56587916626638,1.64683286919032,44.381119075199));
#194510=CARTESIAN_POINT('Ctrl Pts',(6.51900328847673,1.81518184346075,44.3893161927801));
#194511=CARTESIAN_POINT('Ctrl Pts',(6.47212793223347,1.98352894466121,44.3975132191592));
#194512=CARTESIAN_POINT('Ctrl Pts',(6.41872587965452,2.15006415391288,44.4057102455383));
#194513=CARTESIAN_POINT('Ctrl Pts',(6.35897152769573,2.31425368314605,44.4139072719174));
#194514=CARTESIAN_POINT('Ctrl Pts',(6.29920697541654,2.47847124022572,44.4221056975635));
#194515=CARTESIAN_POINT('Ctrl Pts',(6.23308808610291,2.64034198233027,44.4303041232096));
#194516=CARTESIAN_POINT('Ctrl Pts',(6.16083795604542,2.79935076032821,44.4385025488557));
#194517=CARTESIAN_POINT('Ctrl Pts',(6.08856235517795,2.95841559472862,44.4467038647464));
#194518=CARTESIAN_POINT('Ctrl Pts',(6.01015135621422,3.11461612869953,44.454905180637));
#194519=CARTESIAN_POINT('Ctrl Pts',(5.92587469883682,3.26746048999611,44.4631064965276));
#194520=CARTESIAN_POINT('Ctrl Pts',(5.8415020644539,3.4204789154353,44.4713171523442));
#194521=CARTESIAN_POINT('Ctrl Pts',(5.75125059964335,3.5701332177307,44.4795278081608));
#194522=CARTESIAN_POINT('Ctrl Pts',(5.6554347609124,3.71595837773565,44.4877384639774));
#194523=CARTESIAN_POINT('Ctrl Pts',(5.55956246022919,3.8618694689742,44.4959539581345));
#194524=CARTESIAN_POINT('Ctrl Pts',(5.45811945770854,4.00394662854382,44.5041694522917));
#194525=CARTESIAN_POINT('Ctrl Pts',(5.35146136878129,4.14175689996908,44.5123849464488));
#194526=CARTESIAN_POINT('Ctrl Pts',(5.24463779786639,4.2797809865664,44.5206131870963));
#194527=CARTESIAN_POINT('Ctrl Pts',(5.13258320123164,4.41352468047039,44.5288414277438));
#194528=CARTESIAN_POINT('Ctrl Pts',(5.01569191202018,4.54258997089715,44.5370696683913));
#194529=CARTESIAN_POINT('Ctrl Pts',(4.90945639194587,4.6598897144839,44.5445478254925));
#194530=CARTESIAN_POINT('Ctrl Pts',(4.79922641205564,4.77332546969481,44.5520259825937));
#194531=CARTESIAN_POINT('Ctrl Pts',(4.68532166476138,4.88262735601619,44.5595041396948));
#194532=CARTESIAN_POINT('Ctrl Pts',(4.56242623825974,5.0005566105555,44.5675725593896));
#194533=CARTESIAN_POINT('Ctrl Pts',(4.43485019286915,5.11405902250298,44.5756409790844));
#194534=CARTESIAN_POINT('Ctrl Pts',(4.30295035589384,5.22272986422934,44.5837093987791));
#194535=CARTESIAN_POINT('Ctrl Pts',(4.17119502834896,5.33128164620703,44.5917689787152));
#194536=CARTESIAN_POINT('Ctrl Pts',(4.03512561300381,5.4350121496199,44.5998285586512));
#194537=CARTESIAN_POINT('Ctrl Pts',(3.89513727967132,5.53355171409058,44.6078881385873));
#194538=CARTESIAN_POINT('Ctrl Pts',(3.7553109589693,5.6319772358145,44.6159383909335));
#194539=CARTESIAN_POINT('Ctrl Pts',(3.61157505317701,5.72522356704627,44.6239886432798));
#194540=CARTESIAN_POINT('Ctrl Pts',(3.46435904289281,5.81296012560957,44.6320388956261));
#194541=CARTESIAN_POINT('Ctrl Pts',(3.34482014189342,5.88420191356374,44.6385756732251));
#194542=CARTESIAN_POINT('Ctrl Pts',(3.22298741040076,5.95181155375775,44.6451124508241));
#194543=CARTESIAN_POINT('Ctrl Pts',(3.09910619832132,6.01563211736941,44.6516492284231));
#194544=CARTESIAN_POINT('Origin',(0.,0.,4.30282021618968));
#194545=CARTESIAN_POINT('',(3.09910619832128,6.01563211736943,47.0456420231655));
#194546=CARTESIAN_POINT('',(3.09910619832134,6.0156321173694,46.651350675134));
#194547=CARTESIAN_POINT('',(3.09910619832133,6.0156321173694,4.30282021618968));
#194548=CARTESIAN_POINT('',(-6.76699829542225,-0.00480309820322907,45.6971797838526));
#194549=CARTESIAN_POINT('Ctrl Pts',(-6.76699829542225,-0.00480309820322772,
45.6971797838526));
#194550=CARTESIAN_POINT('Ctrl Pts',(-6.76685365275678,-0.208587536770219,
45.7067503929135));
#194551=CARTESIAN_POINT('Ctrl Pts',(-6.75749973364958,-0.412056637524916,
45.7163210019745));
#194552=CARTESIAN_POINT('Ctrl Pts',(-6.73904578321651,-0.614451732613529,
45.7258916110354));
#194553=CARTESIAN_POINT('Ctrl Pts',(-6.72051194201249,-0.817723035766192,
45.7355036531401));
#194554=CARTESIAN_POINT('Ctrl Pts',(-6.69279918945737,-1.01991092176919,
45.7451156952449));
#194555=CARTESIAN_POINT('Ctrl Pts',(-6.65606837195544,-1.22026342559893,
45.7547277373496));
#194556=CARTESIAN_POINT('Ctrl Pts',(-6.61915583248788,-1.42160715296503,
45.7643873340502));
#194557=CARTESIAN_POINT('Ctrl Pts',(-6.57313583199955,-1.62109720207672,
45.7740469307509));
#194558=CARTESIAN_POINT('Ctrl Pts',(-6.51822114023457,-1.81798849473783,
45.7837065274516));
#194559=CARTESIAN_POINT('Ctrl Pts',(-6.47508857845154,-1.97263610491821,
45.791293625514));
#194560=CARTESIAN_POINT('Ctrl Pts',(-6.42646963323295,-2.1256808188579,
45.7988807235765));
#194561=CARTESIAN_POINT('Ctrl Pts',(-6.37248835238679,-2.27676990464447,
45.8064678216389));
#194562=CARTESIAN_POINT('Ctrl Pts',(-6.31398467118079,-2.44051681042375,
45.8146905455048));
#194563=CARTESIAN_POINT('Ctrl Pts',(-6.24908764947539,-2.6022251899042,
45.8229132693707));
#194564=CARTESIAN_POINT('Ctrl Pts',(-6.17795891737632,-2.76136064562572,
45.8311359932366));
#194565=CARTESIAN_POINT('Ctrl Pts',(-6.10690547263056,-2.92032766185836,
45.8393500136278));
#194566=CARTESIAN_POINT('Ctrl Pts',(-6.02963359751848,-3.07672685262557,
45.847564034019));
#194567=CARTESIAN_POINT('Ctrl Pts',(-5.94635425970498,-3.2300402502273,
45.8557780544103));
#194568=CARTESIAN_POINT('Ctrl Pts',(-5.86314635011295,-3.38322215178686,
45.8639850296822));
#194569=CARTESIAN_POINT('Ctrl Pts',(-5.77394140985738,-3.53332321781279,
45.8721920049542));
#194570=CARTESIAN_POINT('Ctrl Pts',(-5.67899796155401,-3.67984662080709,
45.8803989802261));
#194571=CARTESIAN_POINT('Ctrl Pts',(-5.58411688920132,-3.82627376084992,
45.8886005636791));
#194572=CARTESIAN_POINT('Ctrl Pts',(-5.48350501272984,-3.9691276197129,
45.8968021471321));
#194573=CARTESIAN_POINT('Ctrl Pts',(-5.3774661710349,-4.1079370223234,45.9050037305851));
#194574=CARTESIAN_POINT('Ctrl Pts',(-5.27147571557976,-4.24668308526578,
45.9132015716002));
#194575=CARTESIAN_POINT('Ctrl Pts',(-5.16006344573274,-4.38138808419242,
45.9213994126153));
#194576=CARTESIAN_POINT('Ctrl Pts',(-5.0435758439615,-4.51161076625722,
45.9295972536303));
#194577=CARTESIAN_POINT('Ctrl Pts',(-4.92709852185783,-4.64182195657645,
45.9377943712115));
#194578=CARTESIAN_POINT('Ctrl Pts',(-4.80554699253968,-4.76755134503546,
45.9459914887926));
#194579=CARTESIAN_POINT('Ctrl Pts',(-4.67930749869746,-4.88839138496845,
45.9541886063738));
#194580=CARTESIAN_POINT('Ctrl Pts',(-4.55306940941025,-5.00923008042137,
45.9623856327529));
#194581=CARTESIAN_POINT('Ctrl Pts',(-4.4221437179604,-5.12517928679488,
45.970582659132));
#194582=CARTESIAN_POINT('Ctrl Pts',(-4.2869528520441,-5.23586900565235,
45.9787796855111));
#194583=CARTESIAN_POINT('Ctrl Pts',(-4.1517389084755,-5.34657761971275,
45.9869781111572));
#194584=CARTESIAN_POINT('Ctrl Pts',(-4.01225861753204,-5.4520247302093,
45.9951765368034));
#194585=CARTESIAN_POINT('Ctrl Pts',(-3.86896677065171,-5.55188122419716,
46.0033749624495));
#194586=CARTESIAN_POINT('Ctrl Pts',(-3.72562440816134,-5.65177292124659,
46.0115762783402));
#194587=CARTESIAN_POINT('Ctrl Pts',(-3.578468107264,-5.74606987070758,46.0197775942309));
#194588=CARTESIAN_POINT('Ctrl Pts',(-3.42798088785504,-5.83448678398542,
46.0279789101215));
#194589=CARTESIAN_POINT('Ctrl Pts',(-3.27732228869389,-5.923004389327,46.0361895659381));
#194590=CARTESIAN_POINT('Ctrl Pts',(-3.12332550227137,-6.00562839835296,
46.0444002217547));
#194591=CARTESIAN_POINT('Ctrl Pts',(-2.96649829484811,-6.08211943870418,
46.0526108775713));
#194592=CARTESIAN_POINT('Ctrl Pts',(-2.80957867295087,-6.15865555337238,
46.0608263717285));
#194593=CARTESIAN_POINT('Ctrl Pts',(-2.64982563317626,-6.22905135093668,
46.0690418658856));
#194594=CARTESIAN_POINT('Ctrl Pts',(-2.4877659695276,-6.29311603904301,
46.0772573600428));
#194595=CARTESIAN_POINT('Ctrl Pts',(-2.3254548673288,-6.35728012469177,
46.0854856006903));
#194596=CARTESIAN_POINT('Ctrl Pts',(-2.1608303278032,-6.41509335217598,
46.0937138413378));
#194597=CARTESIAN_POINT('Ctrl Pts',(-1.99443460187551,-6.46641474225414,
46.1019420819853));
#194598=CARTESIAN_POINT('Ctrl Pts',(-1.84320745226529,-6.51305769231962,
46.1094202390864));
#194599=CARTESIAN_POINT('Ctrl Pts',(-1.69051766979617,-6.55433903623512,
46.1168983961874));
#194600=CARTESIAN_POINT('Ctrl Pts',(-1.53677791905916,-6.59018987795437,
46.1243765532884));
#194601=CARTESIAN_POINT('Ctrl Pts',(-1.3708849628497,-6.62887474694168,
46.132445862511));
#194602=CARTESIAN_POINT('Ctrl Pts',(-1.20322623801096,-6.66136239813277,
46.1405151717335));
#194603=CARTESIAN_POINT('Ctrl Pts',(-1.03431534275473,-6.68748688011739,
46.148584480956));
#194604=CARTESIAN_POINT('Ctrl Pts',(-0.865615125293458,-6.71357877777255,
46.1566437255568));
#194605=CARTESIAN_POINT('Ctrl Pts',(-0.69566620906036,-6.73332324163065,
46.1647029701575));
#194606=CARTESIAN_POINT('Ctrl Pts',(-0.524997028932897,-6.74660411759958,
46.1727622147583));
#194607=CARTESIAN_POINT('Ctrl Pts',(-0.354503266588588,-6.75987134317294,
46.1808131758786));
#194608=CARTESIAN_POINT('Ctrl Pts',(-0.183291082436059,-6.76668817269795,
46.1888641369989));
#194609=CARTESIAN_POINT('Ctrl Pts',(-0.0118986770931029,-6.76698953904049,
46.1969150981191));
#194610=CARTESIAN_POINT('Ctrl Pts',(0.159355122595911,-6.76729066166699,
46.2049595483982));
#194611=CARTESIAN_POINT('Ctrl Pts',(0.33078848215301,-6.761086807667,46.2130039986773));
#194612=CARTESIAN_POINT('Ctrl Pts',(0.501858614646054,-6.74836475977,46.2210484489564));
#194613=CARTESIAN_POINT('Ctrl Pts',(0.672827847761438,-6.73565021550145,
46.2290881545147));
#194614=CARTESIAN_POINT('Ctrl Pts',(0.843433909124399,-6.71642515822177,
46.2371278600729));
#194615=CARTESIAN_POINT('Ctrl Pts',(1.01313465791234,-6.69072844800451,
46.2451675656311));
#194616=CARTESIAN_POINT('Ctrl Pts',(1.1864983066362,-6.66447708803538,46.2533808039356));
#194617=CARTESIAN_POINT('Ctrl Pts',(1.3589167182694,-6.63147152425315,46.26159404224));
#194618=CARTESIAN_POINT('Ctrl Pts',(1.52981761192682,-6.59180908963833,
46.2698072805445));
#194619=CARTESIAN_POINT('Ctrl Pts',(1.69705378851112,-6.55299715731278,
46.2778443980927));
#194620=CARTESIAN_POINT('Ctrl Pts',(1.86283649359637,-6.50781105363439,
46.2858815156409));
#194621=CARTESIAN_POINT('Ctrl Pts',(2.02664048997135,-6.45639352304433,
46.293918633189));
#194622=CARTESIAN_POINT('Ctrl Pts',(2.19046181576765,-6.40497055280644,
46.3019566010132));
#194623=CARTESIAN_POINT('Ctrl Pts',(2.35230365951027,-6.34731495479433,
46.3099945688373));
#194624=CARTESIAN_POINT('Ctrl Pts',(2.51165695655697,-6.28361904737859,
46.3180325366614));
#194625=CARTESIAN_POINT('Ctrl Pts',(2.67105868593177,-6.21990378083351,
46.3260729474691));
#194626=CARTESIAN_POINT('Ctrl Pts',(2.827970016382,-6.15014468927429,46.3341133582769));
#194627=CARTESIAN_POINT('Ctrl Pts',(2.98190297929009,-6.07458176520005,
46.3421537690846));
#194628=CARTESIAN_POINT('Ctrl Pts',(3.14165374000358,-5.9961629887759,46.3504980620724));
#194629=CARTESIAN_POINT('Ctrl Pts',(3.29819620377378,-5.91149330051802,
46.3588423550602));
#194630=CARTESIAN_POINT('Ctrl Pts',(3.45101517644059,-5.82089196360633,
46.367186648048));
#194631=CARTESIAN_POINT('Ctrl Pts',(3.59852884358654,-5.73343596764627,
46.3752412582635));
#194632=CARTESIAN_POINT('Ctrl Pts',(3.74257294618498,-5.64045352622386,
46.3832958684791));
#194633=CARTESIAN_POINT('Ctrl Pts',(3.88271605159257,-5.54227435830322,
46.3913504786946));
#194634=CARTESIAN_POINT('Ctrl Pts',(4.02296524731073,-5.44402086736551,
46.3994111863639));
#194635=CARTESIAN_POINT('Ctrl Pts',(4.15930727032309,-5.34056304113514,
46.4074718940331));
#194636=CARTESIAN_POINT('Ctrl Pts',(4.29134539317149,-5.23226946138154,
46.4155326017024));
#194637=CARTESIAN_POINT('Ctrl Pts',(4.42356968186232,-5.12382319416866,
46.4236046744865));
#194638=CARTESIAN_POINT('Ctrl Pts',(4.55147768624772,-5.01052781545749,
46.4316767472706));
#194639=CARTESIAN_POINT('Ctrl Pts',(4.67471058271867,-4.89278754574711,
46.4397488200548));
#194640=CARTESIAN_POINT('Ctrl Pts',(4.68761829232993,-4.88045514705736,
46.4405943083492));
#194641=CARTESIAN_POINT('Ctrl Pts',(4.70047474908031,-4.86807401199892,
46.4414397966437));
#194642=CARTESIAN_POINT('Ctrl Pts',(4.71327956730438,-4.85564462460249,
46.4422852849381));
#194643=CARTESIAN_POINT('Ctrl Pts',(4.83948066645951,-4.73314367817709,
46.4506182069848));
#194644=CARTESIAN_POINT('Ctrl Pts',(4.96106501573664,-4.60556227232716,
46.4589511290316));
#194645=CARTESIAN_POINT('Ctrl Pts',(5.07760546832762,-4.47327751296625,
46.4672840510783));
#194646=CARTESIAN_POINT('Ctrl Pts',(5.19400819836504,-4.34114908211145,
46.4756071256319));
#194647=CARTESIAN_POINT('Ctrl Pts',(5.3053786777772,-4.20432862901411,46.4839302001855));
#194648=CARTESIAN_POINT('Ctrl Pts',(5.41132522199788,-4.06323126855581,
46.4922532747391));
#194649=CARTESIAN_POINT('Ctrl Pts',(5.51716601019195,-3.92227475173064,
46.5005680411851));
#194650=CARTESIAN_POINT('Ctrl Pts',(5.61759344235832,-3.77705010970675,
46.5088828076311));
#194651=CARTESIAN_POINT('Ctrl Pts',(5.71225474723509,-3.62800698768487,
46.517197574077));
#194652=CARTESIAN_POINT('Ctrl Pts',(5.80683892510071,-3.47908530124374,
46.5255055659166));
#194653=CARTESIAN_POINT('Ctrl Pts',(5.89566615120226,-3.32635162652708,
46.5338135577561));
#194654=CARTESIAN_POINT('Ctrl Pts',(5.97842566951192,-3.17028634576137,
46.5421215495957));
#194655=CARTESIAN_POINT('Ctrl Pts',(6.0611329306087,-3.01431960999408,46.5504242954828));
#194656=CARTESIAN_POINT('Ctrl Pts',(6.13777995680726,-2.85502576711637,
46.5587270413698));
#194657=CARTESIAN_POINT('Ctrl Pts',(6.20810073168352,-2.69291186362839,
46.5670297872569));
#194658=CARTESIAN_POINT('Ctrl Pts',(6.27839276870008,-2.53086421092651,
46.5753291400764));
#194659=CARTESIAN_POINT('Ctrl Pts',(6.34236356763179,-2.36599911268145,
46.5836284928958));
#194660=CARTESIAN_POINT('Ctrl Pts',(6.39979414854143,-2.19884602832825,
46.5919278457153));
#194661=CARTESIAN_POINT('Ctrl Pts',(6.45721251493014,-2.0317284946314,46.6002254334016));
#194662=CARTESIAN_POINT('Ctrl Pts',(6.50809332149035,-1.86232427311155,
46.608523021088));
#194663=CARTESIAN_POINT('Ctrl Pts',(6.55226653045999,-1.69118074545975,
46.6168206087743));
#194664=CARTESIAN_POINT('Ctrl Pts',(6.59643768502351,-1.5200451773454,46.6251178105567));
#194665=CARTESIAN_POINT('Ctrl Pts',(6.63390177686028,-1.34717080117684,
46.6334150123391));
#194666=CARTESIAN_POINT('Ctrl Pts',(6.66453919218751,-1.17311821902,46.6417122141216));
#194667=CARTESIAN_POINT('Ctrl Pts',(6.69518027358403,-0.999044809752956,
46.6500104087461));
#194668=CARTESIAN_POINT('Ctrl Pts',(6.71899299102571,-0.823793256288492,
46.6583086033706));
#194669=CARTESIAN_POINT('Ctrl Pts',(6.73590917402292,-0.647932557689332,
46.6666067979952));
#194670=CARTESIAN_POINT('Ctrl Pts',(6.75283725436887,-0.471948174210463,
46.6749108288368));
#194671=CARTESIAN_POINT('Ctrl Pts',(6.7628590748388,-0.295354136261364,
46.6832148596784));
#194672=CARTESIAN_POINT('Ctrl Pts',(6.76595844600158,-0.118723658046192,
46.6915188905199));
#194673=CARTESIAN_POINT('Ctrl Pts',(6.76905894418103,0.0579710478721898,
46.6998259409357));
#194674=CARTESIAN_POINT('Ctrl Pts',(6.76523197725446,0.234701872535052,
46.7081329913514));
#194675=CARTESIAN_POINT('Ctrl Pts',(6.75451349107595,0.41089718771603,46.7164400417672));
#194676=CARTESIAN_POINT('Ctrl Pts',(6.74378354502675,0.587280885425717,
46.7247559738218));
#194677=CARTESIAN_POINT('Ctrl Pts',(6.72614738650391,0.763127582691777,
46.7330719058764));
#194678=CARTESIAN_POINT('Ctrl Pts',(6.70169281114588,0.937871241181677,
46.7413878379311));
#194679=CARTESIAN_POINT('Ctrl Pts',(6.68325843280916,1.0695967226257,46.7476565641499));
#194680=CARTESIAN_POINT('Ctrl Pts',(6.66095058571782,1.20069552610051,46.7539252903687));
#194681=CARTESIAN_POINT('Ctrl Pts',(6.63482592046043,1.33092975216068,46.7601940165876));
#194682=CARTESIAN_POINT('Ctrl Pts',(6.59960976425492,1.5064860244823,46.7686442853109));
#194683=CARTESIAN_POINT('Ctrl Pts',(6.5573916916043,1.68079274914121,46.7770945540343));
#194684=CARTESIAN_POINT('Ctrl Pts',(6.50827738500053,1.85327129149801,46.7855448227576));
#194685=CARTESIAN_POINT('Ctrl Pts',(6.45920642343859,2.02559761568969,46.7939876338321));
#194686=CARTESIAN_POINT('Ctrl Pts',(6.40325144912586,2.19609865602286,46.8024304449066));
#194687=CARTESIAN_POINT('Ctrl Pts',(6.34056900696767,2.36420677350374,46.8108732559812));
#194688=CARTESIAN_POINT('Ctrl Pts',(6.27793334981569,2.53218941821985,46.8193097654989));
#194689=CARTESIAN_POINT('Ctrl Pts',(6.20858034987719,2.69778239076973,46.8277462750166));
#194690=CARTESIAN_POINT('Ctrl Pts',(6.1327162378131,2.86043362909605,46.8361827845343));
#194691=CARTESIAN_POINT('Ctrl Pts',(6.05690641060337,3.02296848170923,46.8446132572755));
#194692=CARTESIAN_POINT('Ctrl Pts',(5.97459490431643,3.18256549902456,46.8530437300167));
#194693=CARTESIAN_POINT('Ctrl Pts',(5.88603595655578,3.33869281577873,46.861474202758));
#194694=CARTESIAN_POINT('Ctrl Pts',(5.79751508004677,3.49475301382253,46.8699010512618));
#194695=CARTESIAN_POINT('Ctrl Pts',(5.70275227951128,3.64734619700503,46.8783278997656));
#194696=CARTESIAN_POINT('Ctrl Pts',(5.60204790286209,3.79596473825014,46.8867547482694));
#194697=CARTESIAN_POINT('Ctrl Pts',(5.50137461005746,3.94453740625928,46.8951789957061));
#194698=CARTESIAN_POINT('Ctrl Pts',(5.39476358425948,4.08913760474125,46.9036032431427));
#194699=CARTESIAN_POINT('Ctrl Pts',(5.28255889390558,4.22928605469281,46.9120274905793));
#194700=CARTESIAN_POINT('Ctrl Pts',(5.2509439051809,4.26877452572753,46.9144011211904));
#194701=CARTESIAN_POINT('Ctrl Pts',(5.21888509609938,4.30790975782307,46.9167747518014));
#194702=CARTESIAN_POINT('Ctrl Pts',(5.18639076284462,4.34668147614706,46.9191483824124));
#194703=CARTESIAN_POINT('Ctrl Pts',(5.068419892342,4.48744243054804,46.9277658624892));
#194704=CARTESIAN_POINT('Ctrl Pts',(4.94475829942727,4.62334654014516,46.9363833425661));
#194705=CARTESIAN_POINT('Ctrl Pts',(4.81583329022593,4.75394980208581,46.9450008226429));
#194706=CARTESIAN_POINT('Ctrl Pts',(4.68676484770896,4.88469836445349,46.9536278899499));
#194707=CARTESIAN_POINT('Ctrl Pts',(4.55242149739686,5.01013407351309,46.9622549572569));
#194708=CARTESIAN_POINT('Ctrl Pts',(4.41326701618101,5.12985021651595,46.9708820245639));
#194709=CARTESIAN_POINT('Ctrl Pts',(4.27403925901451,5.24962939963158,46.9795136347111));
#194710=CARTESIAN_POINT('Ctrl Pts',(4.12999554990547,5.36368281264469,46.9881452448582));
#194711=CARTESIAN_POINT('Ctrl Pts',(3.98163189657912,5.47164476552926,46.9967768550053));
#194712=CARTESIAN_POINT('Ctrl Pts',(3.83309584268652,5.57973217165925,47.0054184951998));
#194713=CARTESIAN_POINT('Ctrl Pts',(3.68023005886038,5.68171379226426,47.0140601353944));
#194714=CARTESIAN_POINT('Ctrl Pts',(3.52356004295536,5.77726696835869,47.0227017755889));
#194715=CARTESIAN_POINT('Ctrl Pts',(3.38492706465539,5.86181933986048,47.0303485247811));
#194716=CARTESIAN_POINT('Ctrl Pts',(3.24331589469917,5.9413388169842,47.0379952739733));
#194717=CARTESIAN_POINT('Ctrl Pts',(3.09910619832128,6.01563211736943,47.0456420231655));
#194718=CARTESIAN_POINT('Ctrl Pts',(3.09910619832133,6.01563211736941,45.0457774706169));
#194719=CARTESIAN_POINT('Ctrl Pts',(2.94511943075718,6.09496232515249,45.0538985576503));
#194720=CARTESIAN_POINT('Ctrl Pts',(2.78808765733465,6.16837455272572,45.0620196446837));
#194721=CARTESIAN_POINT('Ctrl Pts',(2.62851387184196,6.23563980883553,45.0701407317171));
#194722=CARTESIAN_POINT('Ctrl Pts',(2.4639351078096,6.30501481725996,45.0785165339357));
#194723=CARTESIAN_POINT('Ctrl Pts',(2.29665264882922,6.36785079448704,45.0868923361543));
#194724=CARTESIAN_POINT('Ctrl Pts',(2.12723915740466,6.42395069775635,45.0952681383728));
#194725=CARTESIAN_POINT('Ctrl Pts',(1.96281692221674,6.47839778701591,45.1033971729066));
#194726=CARTESIAN_POINT('Ctrl Pts',(1.79638781576152,6.52650003863257,45.1115262074403));
#194727=CARTESIAN_POINT('Ctrl Pts',(1.62848901668219,6.56812854034888,45.119655241974));
#194728=CARTESIAN_POINT('Ctrl Pts',(1.45294502964758,6.61165257509855,45.128154428035));
#194729=CARTESIAN_POINT('Ctrl Pts',(1.27579481701683,6.64809938942929,45.136653614096));
#194730=CARTESIAN_POINT('Ctrl Pts',(1.0976615919955,6.67738182444721,45.145152800157));
#194731=CARTESIAN_POINT('Ctrl Pts',(0.919528366974146,6.70666425946513,
45.153651986218));
#194732=CARTESIAN_POINT('Ctrl Pts',(0.740412585283084,6.72878231212951,
45.162151172279));
#194733=CARTESIAN_POINT('Ctrl Pts',(0.560940188315077,6.7437107815455,45.17065035834));
#194734=CARTESIAN_POINT('Ctrl Pts',(0.382713166174243,6.7585356609926,45.1790905677976));
#194735=CARTESIAN_POINT('Ctrl Pts',(0.203766007222725,6.76630176532737,
45.1875307772553));
#194736=CARTESIAN_POINT('Ctrl Pts',(0.0246829581155314,6.76695498371156,
45.1959709867129));
#194737=CARTESIAN_POINT('Ctrl Pts',(-0.154264409050907,6.76760770718604,
45.2044048014615));
#194738=CARTESIAN_POINT('Ctrl Pts',(-0.333347128852056,6.76115828623688,
45.21283861621));
#194739=CARTESIAN_POINT('Ctrl Pts',(-0.511977968558169,6.74760457938305,
45.2212724309585));
#194740=CARTESIAN_POINT('Ctrl Pts',(-0.69050092930322,6.73405905790087,
45.2297011523471));
#194741=CARTESIAN_POINT('Ctrl Pts',(-0.868572222323422,6.71341782926739,
45.2381298737356));
#194742=CARTESIAN_POINT('Ctrl Pts',(-1.04560635521803,6.68573080148518,
45.2465585951242));
#194743=CARTESIAN_POINT('Ctrl Pts',(-1.22256075843316,6.65805624292466,
45.2549835205258));
#194744=CARTESIAN_POINT('Ctrl Pts',(-1.39847860393442,6.62334226360043,
45.2634084459275));
#194745=CARTESIAN_POINT('Ctrl Pts',(-1.57278085347228,6.5816904657505,45.2718333713291));
#194746=CARTESIAN_POINT('Ctrl Pts',(-1.74703134680747,6.54005103572081,
45.2802557950869));
#194747=CARTESIAN_POINT('Ctrl Pts',(-1.91966687684997,6.49147797282548,
45.2886782188446));
#194748=CARTESIAN_POINT('Ctrl Pts',(-2.09011952060141,6.43612378606883,
45.2971006426024));
#194749=CARTESIAN_POINT('Ctrl Pts',(-2.26057484508011,6.38076872875086,
45.3055231988206));
#194750=CARTESIAN_POINT('Ctrl Pts',(-2.4288468955218,6.3186324311385,45.3139457550388));
#194751=CARTESIAN_POINT('Ctrl Pts',(-2.5943831703266,6.24991719669358,45.322368311257));
#194752=CARTESIAN_POINT('Ctrl Pts',(-2.75992503697877,6.18119964103476,
45.3307911519907));
#194753=CARTESIAN_POINT('Ctrl Pts',(-2.92273063557426,6.10590283315499,
45.3392139927244));
#194754=CARTESIAN_POINT('Ctrl Pts',(-3.08226756133981,6.02427719152367,
45.3476368334582));
#194755=CARTESIAN_POINT('Ctrl Pts',(-3.24183214941292,5.94263739672002,
45.3560611346388));
#194756=CARTESIAN_POINT('Ctrl Pts',(-3.39812663775679,5.85466673227387,
45.3644854358195));
#194757=CARTESIAN_POINT('Ctrl Pts',(-3.55064301529474,5.76066169618896,
45.3729097370002));
#194758=CARTESIAN_POINT('Ctrl Pts',(-3.70320713733692,5.6666272322884,45.381336675367));
#194759=CARTESIAN_POINT('Ctrl Pts',(-3.85199050670598,5.56655480548695,
45.3897636137339));
#194760=CARTESIAN_POINT('Ctrl Pts',(-3.99651359455045,5.4607845671271,45.3981905521007));
#194761=CARTESIAN_POINT('Ctrl Pts',(-4.14116662681661,5.35491922802825,
45.4066250673444));
#194762=CARTESIAN_POINT('Ctrl Pts',(-4.28155145412046,5.2433460378963,45.415059582588));
#194763=CARTESIAN_POINT('Ctrl Pts',(-4.4172202832284,5.12644652458558,45.4234940978317));
#194764=CARTESIAN_POINT('Ctrl Pts',(-4.55295464154302,5.00949054780852,
45.4319326870184));
#194765=CARTESIAN_POINT('Ctrl Pts',(-4.68396821151621,4.88720334070131,
45.4403712762052));
#194766=CARTESIAN_POINT('Ctrl Pts',(-4.80984929216416,4.76000407422808,
45.448809865392));
#194767=CARTESIAN_POINT('Ctrl Pts',(-4.93587107938033,4.63266262775311,
45.4572578870122));
#194768=CARTESIAN_POINT('Ctrl Pts',(-5.05674868504748,4.50039839360241,
45.4657059086325));
#194769=CARTESIAN_POINT('Ctrl Pts',(-5.17210919192994,4.36366537520395,
45.4741539302528));
#194770=CARTESIAN_POINT('Ctrl Pts',(-5.2376782526968,4.28594852188482,45.478955650165));
#194771=CARTESIAN_POINT('Ctrl Pts',(-5.30146570808013,4.20678857005627,
45.4837573700773));
#194772=CARTESIAN_POINT('Ctrl Pts',(-5.36340923190965,4.12627318667418,
45.4885590899895));
#194773=CARTESIAN_POINT('Ctrl Pts',(-5.4697014869505,3.98811246968441,45.4967986218403));
#194774=CARTESIAN_POINT('Ctrl Pts',(-5.57079909755088,3.84565059511103,
45.5050381536911));
#194775=CARTESIAN_POINT('Ctrl Pts',(-5.66633668219299,3.69931312597813,
45.5132776855419));
#194776=CARTESIAN_POINT('Ctrl Pts',(-5.76176822679321,3.55313808120856,
45.5215080720881));
#194777=CARTESIAN_POINT('Ctrl Pts',(-5.8516518405613,3.40309630255716,45.5297384586344));
#194778=CARTESIAN_POINT('Ctrl Pts',(-5.93566242842176,3.2496462170246,45.5379688451807));
#194779=CARTESIAN_POINT('Ctrl Pts',(-6.01959475711712,3.09633907627895,
45.5461915647984));
#194780=CARTESIAN_POINT('Ctrl Pts',(-6.09766478549532,2.93963026201029,
45.5544142844161));
#194781=CARTESIAN_POINT('Ctrl Pts',(-6.16959073445617,2.78000704483148,
45.5626370040338));
#194782=CARTESIAN_POINT('Ctrl Pts',(-6.24145295184508,2.62052526532145,
45.5708524377296));
#194783=CARTESIAN_POINT('Ctrl Pts',(-6.30718179475897,2.45813455305886,
45.5790678714254));
#194784=CARTESIAN_POINT('Ctrl Pts',(-6.36654150727517,2.29334651462496,
45.5872833051211));
#194785=CARTESIAN_POINT('Ctrl Pts',(-6.42587071350849,2.12864316444681,
45.5954945167219));
#194786=CARTESIAN_POINT('Ctrl Pts',(-6.47883718796481,1.96154527583867,
45.6037057283227));
#194787=CARTESIAN_POINT('Ctrl Pts',(-6.52525322510156,1.79258454425495,
45.6119169399235));
#194788=CARTESIAN_POINT('Ctrl Pts',(-6.57165369686032,1.62368047277868,
45.620125397937));
#194789=CARTESIAN_POINT('Ctrl Pts',(-6.61150801304833,1.45291514559708,
45.6283338559505));
#194790=CARTESIAN_POINT('Ctrl Pts',(-6.64467825451656,1.2808356233158,45.6365423139639));
#194791=CARTESIAN_POINT('Ctrl Pts',(-6.65945632139012,1.20417043864179,
45.6401993612473));
#194792=CARTESIAN_POINT('Ctrl Pts',(-6.67290833592412,1.12724457985017,
45.6438564085308));
#194793=CARTESIAN_POINT('Ctrl Pts',(-6.68502535051625,1.05010716736681,
45.6475134558142));
#194794=CARTESIAN_POINT('Ctrl Pts',(-6.7124521958382,0.87550674375319,45.6557911771468));
#194795=CARTESIAN_POINT('Ctrl Pts',(-6.73302212569519,0.699906920301995,
45.6640688984795));
#194796=CARTESIAN_POINT('Ctrl Pts',(-6.74668992367073,0.523893189342903,
45.6723466198121));
#194797=CARTESIAN_POINT('Ctrl Pts',(-6.76035772164626,0.34787945838381,
45.6806243411448));
#194798=CARTESIAN_POINT('Ctrl Pts',(-6.76712339837554,0.171452226019733,
45.6889020624775));
#194799=CARTESIAN_POINT('Ctrl Pts',(-6.76699829542289,-0.00480309729881822,
45.6971797838101));
#194800=CARTESIAN_POINT('',(-6.76699984541771,0.00144641512400706,45.302820216223));
#194801=CARTESIAN_POINT('Ctrl Pts',(3.09910619832132,6.01563211736941,44.6516492284231));
#194802=CARTESIAN_POINT('Ctrl Pts',(2.94672804361013,6.09413360724455,44.6596896898585));
#194803=CARTESIAN_POINT('Ctrl Pts',(2.79125002559318,6.16690088091477,44.6677301512939));
#194804=CARTESIAN_POINT('Ctrl Pts',(2.63315364174409,6.23368196966847,44.6757706127293));
#194805=CARTESIAN_POINT('Ctrl Pts',(2.46795317318091,6.30346387665885,44.6841723735049));
#194806=CARTESIAN_POINT('Ctrl Pts',(2.29989393689133,6.36670894231337,44.6925741342806));
#194807=CARTESIAN_POINT('Ctrl Pts',(2.12955192278888,6.42318438223178,44.7009758950562));
#194808=CARTESIAN_POINT('Ctrl Pts',(1.96660263550652,6.4772088267128,44.7090130251648));
#194809=CARTESIAN_POINT('Ctrl Pts',(1.8015649237697,6.52503873154561,44.7170501552734));
#194810=CARTESIAN_POINT('Ctrl Pts',(1.63496094949383,6.56652051650113,44.725087285382));
#194811=CARTESIAN_POINT('Ctrl Pts',(1.46834476877123,6.60800534067106,44.7331250043409));
#194812=CARTESIAN_POINT('Ctrl Pts',(1.30016245949996,6.64314102821417,44.7411627232999));
#194813=CARTESIAN_POINT('Ctrl Pts',(1.13094842483701,6.67182468747184,44.7492004422588));
#194814=CARTESIAN_POINT('Ctrl Pts',(0.96168846654374,6.70051613129518,44.7572403426043));
#194815=CARTESIAN_POINT('Ctrl Pts',(0.791396593721691,6.72275199893374,
44.7652802429499));
#194816=CARTESIAN_POINT('Ctrl Pts',(0.620614262965681,6.73848105559432,
44.7733201432954));
#194817=CARTESIAN_POINT('Ctrl Pts',(0.449751734246481,6.75421749848919,
44.7813638191114));
#194818=CARTESIAN_POINT('Ctrl Pts',(0.278398660528421,6.76344101428454,
44.7894074949273));
#194819=CARTESIAN_POINT('Ctrl Pts',(0.107098292709033,6.76615244845243,
44.7974511707433));
#194820=CARTESIAN_POINT('Ctrl Pts',(-0.0644124969663495,6.7688672132904,
44.8055047272455));
#194821=CARTESIAN_POINT('Ctrl Pts',(-0.235870078372894,6.76505392147229,
44.8135582837477));
#194822=CARTESIAN_POINT('Ctrl Pts',(-0.406733773147633,6.75476547614949,
44.8216118402499));
#194823=CARTESIAN_POINT('Ctrl Pts',(-0.577720687258337,6.74446961125519,
44.8296712046207));
#194824=CARTESIAN_POINT('Ctrl Pts',(-0.748112492369287,6.72768933119816,
44.8377305689915));
#194825=CARTESIAN_POINT('Ctrl Pts',(-0.917377468442388,6.70452888579013,
44.8457899333623));
#194826=CARTESIAN_POINT('Ctrl Pts',(-1.08689056063974,6.68133449077195,
44.8538611115076));
#194827=CARTESIAN_POINT('Ctrl Pts',(-1.25527316209345,6.65174132884393,
44.8619322896528));
#194828=CARTESIAN_POINT('Ctrl Pts',(-1.4220067907132,6.61590399621741,44.8700034677981));
#194829=CARTESIAN_POINT('Ctrl Pts',(-1.47302770806174,6.60493768065729,
44.8724732689802));
#194830=CARTESIAN_POINT('Ctrl Pts',(-1.52389435012713,6.59338702136638,
44.8749430701622));
#194831=CARTESIAN_POINT('Ctrl Pts',(-1.57459222930149,6.58125735034145,
44.8774128713443));
#194832=CARTESIAN_POINT('Ctrl Pts',(-1.74564303215994,6.54033275939186,
44.885745793391));
#194833=CARTESIAN_POINT('Ctrl Pts',(-1.9153170023392,6.4926828595889,44.8940787154377));
#194834=CARTESIAN_POINT('Ctrl Pts',(-2.08305434218415,6.43841390464358,
44.9024116374844));
#194835=CARTESIAN_POINT('Ctrl Pts',(-2.25059345717093,6.38420908244238,
44.910734712038));
#194836=CARTESIAN_POINT('Ctrl Pts',(-2.41620017272148,6.32340089356206,
44.9190577865916));
#194837=CARTESIAN_POINT('Ctrl Pts',(-2.57932578507492,6.25614637731948,
44.9273808611453));
#194838=CARTESIAN_POINT('Ctrl Pts',(-2.74228856515526,6.18895899465328,
44.9356956275913));
#194839=CARTESIAN_POINT('Ctrl Pts',(-2.9027748566236,6.11533823648511,44.9440103940372));
#194840=CARTESIAN_POINT('Ctrl Pts',(-3.06025179285158,6.03549069789265,
44.9523251604832));
#194841=CARTESIAN_POINT('Ctrl Pts',(-3.2176004218958,5.95570821652731,44.9606331523227));
#194842=CARTESIAN_POINT('Ctrl Pts',(-3.37194427237067,5.86970922054559,
44.9689411441623));
#194843=CARTESIAN_POINT('Ctrl Pts',(-3.52277091839561,5.77774818216458,
44.9772491360018));
#194844=CARTESIAN_POINT('Ctrl Pts',(-3.67350232727717,5.68584521115317,
44.9855518818889));
#194845=CARTESIAN_POINT('Ctrl Pts',(-3.82072066142304,5.58798788084392,
44.993854627776));
#194846=CARTESIAN_POINT('Ctrl Pts',(-3.96393835728736,5.48447642894251,
45.0021573736631));
#194847=CARTESIAN_POINT('Ctrl Pts',(-4.10709752464305,5.38100727887307,
45.0104567264826));
#194848=CARTESIAN_POINT('Ctrl Pts',(-4.2462590299019,5.27188881485649,45.018756079302));
#194849=CARTESIAN_POINT('Ctrl Pts',(-4.38096431699064,5.15746455666491,
45.0270554321214));
#194850=CARTESIAN_POINT('Ctrl Pts',(-4.51564095452497,5.04306463459318,
45.0353530198077));
#194851=CARTESIAN_POINT('Ctrl Pts',(-4.64586299704453,4.92336139158402,
45.0436506074941));
#194852=CARTESIAN_POINT('Ctrl Pts',(-4.77120482685568,4.79873874056393,
45.0519481951804));
#194853=CARTESIAN_POINT('Ctrl Pts',(-4.8965408272736,4.67412188548952,45.0602453969629));
#194854=CARTESIAN_POINT('Ctrl Pts',(-5.01699682069101,4.54458632372077,
45.0685425987453));
#194855=CARTESIAN_POINT('Ctrl Pts',(-5.13218380199773,4.4105530744468,45.0768398005277));
#194856=CARTESIAN_POINT('Ctrl Pts',(-5.24738456656427,4.27650378677094,
45.0851379951523));
#194857=CARTESIAN_POINT('Ctrl Pts',(-5.35731483641111,4.13795600340657,
45.0934361897769));
#194858=CARTESIAN_POINT('Ctrl Pts',(-5.46162555752576,3.99536422236839,
45.1017343844014));
#194859=CARTESIAN_POINT('Ctrl Pts',(-5.56600964158644,3.85267215486853,
45.110038415243));
#194860=CARTESIAN_POINT('Ctrl Pts',(-5.6647660737933,3.70593068757857,45.1183424460846));
#194861=CARTESIAN_POINT('Ctrl Pts',(-5.7575883482012,3.55562447576481,45.1266464769261));
#194862=CARTESIAN_POINT('Ctrl Pts',(-5.8504443753428,3.40526360847561,45.1349535273418));
#194863=CARTESIAN_POINT('Ctrl Pts',(-5.93736176738236,3.25133571294381,
45.1432605777576));
#194864=CARTESIAN_POINT('Ctrl Pts',(-6.01807966011595,3.09435069190592,
45.1515676281733));
#194865=CARTESIAN_POINT('Ctrl Pts',(-6.09888385389992,2.93719782738564,
45.1598835602279));
#194866=CARTESIAN_POINT('Ctrl Pts',(-6.17347515234348,2.77698161964319,
45.1681994922826));
#194867=CARTESIAN_POINT('Ctrl Pts',(-6.24164013118477,2.61423363010726,
45.1765154243372));
#194868=CARTESIAN_POINT('Ctrl Pts',(-6.2930243401069,2.49155073871459,45.1827841505562));
#194869=CARTESIAN_POINT('Ctrl Pts',(-6.34075779911307,2.3674296155873,45.1890528767751));
#194870=CARTESIAN_POINT('Ctrl Pts',(-6.38476779279172,2.24210375141953,
45.1953216029941));
#194871=CARTESIAN_POINT('Ctrl Pts',(-6.44765953403174,2.06300893315002,
45.2042798207604));
#194872=CARTESIAN_POINT('Ctrl Pts',(-6.50304972991107,1.88115764106677,
45.2132380385267));
#194873=CARTESIAN_POINT('Ctrl Pts',(-6.55071587795956,1.6971772112094,45.222196256293));
#194874=CARTESIAN_POINT('Ctrl Pts',(-6.59785592799697,1.5152273993522,45.2310556009441));
#194875=CARTESIAN_POINT('Ctrl Pts',(-6.63744147068533,1.33119547085567,
45.2399149455952));
#194876=CARTESIAN_POINT('Ctrl Pts',(-6.66930629363198,1.14570614108542,
45.2487742902462));
#194877=CARTESIAN_POINT('Ctrl Pts',(-6.70170454897727,0.957111631089739,
45.2577819445702));
#194878=CARTESIAN_POINT('Ctrl Pts',(-6.72612117866493,0.76701074401207,
45.2667895988941));
#194879=CARTESIAN_POINT('Ctrl Pts',(-6.74243476752652,0.576075000021326,
45.2757972532181));
#194880=CARTESIAN_POINT('Ctrl Pts',(-6.75874835638812,0.385139256030517,
45.284804907542));
#194881=CARTESIAN_POINT('Ctrl Pts',(-6.76695882283989,0.193368939904135,
45.2938125618659));
#194882=CARTESIAN_POINT('Ctrl Pts',(-6.76699984541756,0.00144641582902397,
45.3028202161899));
#194883=CARTESIAN_POINT('Ctrl Pts',(-6.76699984541771,0.00144641512391758,
45.302820216223));
#194884=CARTESIAN_POINT('Ctrl Pts',(-6.76703626799262,-0.168955259133196,
45.3108178151777));
#194885=CARTESIAN_POINT('Ctrl Pts',(-6.7606319637346,-0.339423633244816,
45.3188154141325));
#194886=CARTESIAN_POINT('Ctrl Pts',(-6.74779807270397,-0.509421407100884,
45.3268130130872));
#194887=CARTESIAN_POINT('Ctrl Pts',(-6.73496479099209,-0.679411109918256,
45.3348102323374));
#194888=CARTESIAN_POINT('Ctrl Pts',(-6.71570255732075,-0.848929879388188,
45.3428074515876));
#194889=CARTESIAN_POINT('Ctrl Pts',(-6.6900745042534,-1.01744391862089,
45.3508046708377));
#194890=CARTESIAN_POINT('Ctrl Pts',(-6.68636643998395,-1.04182582879324,
45.3519617701647));
#194891=CARTESIAN_POINT('Ctrl Pts',(-6.68252519855856,-1.06618671696161,
45.3531188694917));
#194892=CARTESIAN_POINT('Ctrl Pts',(-6.67855106060485,-1.09052497949101,
45.3542759688187));
#194893=CARTESIAN_POINT('Ctrl Pts',(-6.64894925924002,-1.27181119082858,
45.362894749756));
#194894=CARTESIAN_POINT('Ctrl Pts',(-6.61197259282066,-1.4518252175661,
45.3715135306932));
#194895=CARTESIAN_POINT('Ctrl Pts',(-6.56776194705422,-1.62996687292307,
45.3801323116304));
#194896=CARTESIAN_POINT('Ctrl Pts',(-6.52352474422171,-1.80821553688913,
45.388756269817));
#194897=CARTESIAN_POINT('Ctrl Pts',(-6.47204496319458,-1.98458928965325,
45.3973802280035));
#194898=CARTESIAN_POINT('Ctrl Pts',(-6.41351360988914,-2.15850229922666,
45.40600418619));
#194899=CARTESIAN_POINT('Ctrl Pts',(-6.35286771849596,-2.3386981924501,
45.4149396985611));
#194900=CARTESIAN_POINT('Ctrl Pts',(-6.28465137807912,-2.51625189068267,
45.4238752109322));
#194901=CARTESIAN_POINT('Ctrl Pts',(-6.20913160627264,-2.69053409121427,
45.4328107233033));
#194902=CARTESIAN_POINT('Ctrl Pts',(-6.13610870775519,-2.85905408456685,
45.4414508051981));
#194903=CARTESIAN_POINT('Ctrl Pts',(-6.05625776194166,-3.02451519146708,
45.4500908870928));
#194904=CARTESIAN_POINT('Ctrl Pts',(-5.96986738505975,-3.18637292305843,
45.4587309689875));
#194905=CARTESIAN_POINT('Ctrl Pts',(-5.87904608660028,-3.35653226116301,
45.4678141965968));
#194906=CARTESIAN_POINT('Ctrl Pts',(-5.78099712840625,-3.52270854534843,
45.4768974242061));
#194907=CARTESIAN_POINT('Ctrl Pts',(-5.67610818611867,-3.68430249293901,
45.4859806518155));
#194908=CARTESIAN_POINT('Ctrl Pts',(-5.5712192438311,-3.84589644052959,
45.4950638794248));
#194909=CARTESIAN_POINT('Ctrl Pts',(-5.45949056969796,-4.00290775509036,
45.5041471070341));
#194910=CARTESIAN_POINT('Ctrl Pts',(-5.34135995672453,-4.15477590402896,
45.5132303346434));
#194911=CARTESIAN_POINT('Ctrl Pts',(-5.22373177643027,-4.30599812792723,
45.5222749295032));
#194912=CARTESIAN_POINT('Ctrl Pts',(-5.09964806402658,-4.4522610308465,
45.531319524363));
#194913=CARTESIAN_POINT('Ctrl Pts',(-4.96953197896536,-4.59304266364255,
45.5403641192228));
#194914=CARTESIAN_POINT('Ctrl Pts',(-4.83953529589338,-4.73369510713048,
45.5494004142432));
#194915=CARTESIAN_POINT('Ctrl Pts',(-4.70351745344857,-4.86887614821844,
45.5584367092635));
#194916=CARTESIAN_POINT('Ctrl Pts',(-4.56194059478497,-4.99809833933397,
45.5674730042838));
#194917=CARTESIAN_POINT('Ctrl Pts',(-4.42061426747501,-5.12709186164892,
45.5764933088715));
#194918=CARTESIAN_POINT('Ctrl Pts',(-4.27374874289041,-5.25014743015173,
45.5855136134592));
#194919=CARTESIAN_POINT('Ctrl Pts',(-4.12184141577506,-5.36681584770723,
45.5945339180468));
#194920=CARTESIAN_POINT('Ctrl Pts',(-3.97012538642979,-5.48333734405397,
45.6035428633131));
#194921=CARTESIAN_POINT('Ctrl Pts',(-3.81338041342187,-5.59348759679608,
45.6125518085794));
#194922=CARTESIAN_POINT('Ctrl Pts',(-3.65213718322292,-5.69685729107906,
45.6215607538457));
#194923=CARTESIAN_POINT('Ctrl Pts',(-3.49126010226394,-5.79999225467007,
45.6305492417045));
#194924=CARTESIAN_POINT('Ctrl Pts',(-3.32590535321974,-5.89637726581379,
45.6395377295633));
#194925=CARTESIAN_POINT('Ctrl Pts',(-3.15663240641742,-5.98564623501551,
45.6485262174221));
#194926=CARTESIAN_POINT('Ctrl Pts',(-3.00811869254229,-6.06396746945018,
45.6564123784374));
#194927=CARTESIAN_POINT('Ctrl Pts',(-2.85658944393715,-6.13681155493424,
45.6642985394528));
#194928=CARTESIAN_POINT('Ctrl Pts',(-2.70244140676999,-6.20395836889441,
45.6721847004682));
#194929=CARTESIAN_POINT('Ctrl Pts',(-2.54369396754584,-6.27310868027126,
45.6803061653244));
#194930=CARTESIAN_POINT('Ctrl Pts',(-2.38223954086875,-6.33618420853312,
45.6884276301806));
#194931=CARTESIAN_POINT('Ctrl Pts',(-2.21858992398726,-6.39297643896661,
45.6965490950367));
#194932=CARTESIAN_POINT('Ctrl Pts',(-2.0549519777318,-6.44976461927829,
45.7046699807129));
#194933=CARTESIAN_POINT('Ctrl Pts',(-1.88911949904313,-6.50027027424077,
45.7127908663891));
#194934=CARTESIAN_POINT('Ctrl Pts',(-1.72162171742235,-6.54433401211305,
45.7209117520654));
#194935=CARTESIAN_POINT('Ctrl Pts',(-1.55410391502806,-6.58840301686175,
45.7290336084196));
#194936=CARTESIAN_POINT('Ctrl Pts',(-1.38492076778149,-6.62602847928742,
45.7371554647738));
#194937=CARTESIAN_POINT('Ctrl Pts',(-1.21461398060706,-6.65710161242217,
45.745277321128));
#194938=CARTESIAN_POINT('Ctrl Pts',(-1.044182939707,-6.68819741613055,45.7534051030882));
#194939=CARTESIAN_POINT('Ctrl Pts',(-0.872626982137431,-6.71273127679588,
45.7615328850484));
#194940=CARTESIAN_POINT('Ctrl Pts',(-0.700495898374002,-6.73064591969903,
45.7696606670085));
#194941=CARTESIAN_POINT('Ctrl Pts',(-0.528294694804394,-6.74856786036189,
45.777791759925));
#194942=CARTESIAN_POINT('Ctrl Pts',(-0.355518263194503,-6.75986518465779,
45.7859228528414));
#194943=CARTESIAN_POINT('Ctrl Pts',(-0.182718482227967,-6.76453272268324,
45.7940539457579));
#194944=CARTESIAN_POINT('Ctrl Pts',(-0.00973009752258797,-6.76920535513137,
45.8021939134224));
#194945=CARTESIAN_POINT('Ctrl Pts',(0.163281321721688,-6.76723375250431,
45.810333881087));
#194946=CARTESIAN_POINT('Ctrl Pts',(0.335766174274341,-6.75866481460748,
45.8184738487515));
#194947=CARTESIAN_POINT('Ctrl Pts',(0.425224276575121,-6.75422059291706,
45.822695587932));
#194948=CARTESIAN_POINT('Ctrl Pts',(0.514540838255739,-6.74800259950535,
45.8269173271125));
#194949=CARTESIAN_POINT('Ctrl Pts',(0.603640110343529,-6.74002282022728,
45.831139066293));
#194950=CARTESIAN_POINT('Ctrl Pts',(0.781769664727358,-6.72406944043441,
45.8395792757506));
#194951=CARTESIAN_POINT('Ctrl Pts',(0.959398397327153,-6.70103834344931,
45.8480194852082));
#194952=CARTESIAN_POINT('Ctrl Pts',(1.13594143568155,-6.67097639440448,
45.8564596946658));
#194953=CARTESIAN_POINT('Ctrl Pts',(1.31235071652922,-6.64093722173978,
45.8648935094144));
#194954=CARTESIAN_POINT('Ctrl Pts',(1.48767561530768,-6.6038778716359,45.8733273241629));
#194955=CARTESIAN_POINT('Ctrl Pts',(1.66133722834225,-6.5598969209679,45.8817611389114));
#194956=CARTESIAN_POINT('Ctrl Pts',(1.83489396343796,-6.51594253133071,
45.8901898603));
#194957=CARTESIAN_POINT('Ctrl Pts',(2.00678909292398,-6.46507495642847,
45.8986185816885));
#194958=CARTESIAN_POINT('Ctrl Pts',(2.17645435206196,-6.40744375343167,
45.9070473030771));
#194959=CARTESIAN_POINT('Ctrl Pts',(2.34604320019309,-6.34983850541393,
45.9154722284788));
#194960=CARTESIAN_POINT('Ctrl Pts',(2.51340386510166,-6.28547580994081,
45.9238971538806));
#194961=CARTESIAN_POINT('Ctrl Pts',(2.67798330409106,-6.21455504626112,
45.9323220792823));
#194962=CARTESIAN_POINT('Ctrl Pts',(2.84251387390282,-6.14365534134442,
45.94074450304));
#194963=CARTESIAN_POINT('Ctrl Pts',(3.00426455876845,-6.06620158341942,
45.9491669267977));
#194964=CARTESIAN_POINT('Ctrl Pts',(3.1627019950883,-5.98244139881575,45.9575893505553));
#194965=CARTESIAN_POINT('Ctrl Pts',(3.32114192317398,-5.89867989690494,
45.9660119067736));
#194966=CARTESIAN_POINT('Ctrl Pts',(3.47626820074634,-5.8086119200891,45.9744344629918));
#194967=CARTESIAN_POINT('Ctrl Pts',(3.62757119496527,-5.71253150761186,
45.98285701921));
#194968=CARTESIAN_POINT('Ctrl Pts',(3.77887930022777,-5.61644784952024,
45.9912798599437));
#194969=CARTESIAN_POINT('Ctrl Pts',(3.9263635829329,-5.51435152947949,45.9997027006775));
#194970=CARTESIAN_POINT('Ctrl Pts',(4.06954245923275,-5.40658054342131,
46.0081255414112));
#194971=CARTESIAN_POINT('Ctrl Pts',(4.2127461614971,-5.29879087081702,46.0165498425919));
#194972=CARTESIAN_POINT('Ctrl Pts',(4.35164270251472,-5.18532477110903,
46.0249741437725));
#194973=CARTESIAN_POINT('Ctrl Pts',(4.48578243166701,-5.06656145484762,
46.0333984449532));
#194974=CARTESIAN_POINT('Ctrl Pts',(4.6199641526039,-4.94776096031229,46.04182538332));
#194975=CARTESIAN_POINT('Ctrl Pts',(4.74938584317514,-4.82366016411711,
46.0502523216868));
#194976=CARTESIAN_POINT('Ctrl Pts',(4.87363339797939,-4.69467640014728,
46.0586792600536));
#194977=CARTESIAN_POINT('Ctrl Pts',(4.9979926669528,-4.56557666356095,46.0671137752973));
#194978=CARTESIAN_POINT('Ctrl Pts',(5.11716827269483,-4.43158542694702,
46.0755482905409));
#194979=CARTESIAN_POINT('Ctrl Pts',(5.23078446985143,-4.2931553465908,46.0839828057846));
#194980=CARTESIAN_POINT('Ctrl Pts',(5.34445554460447,-4.15465840332,46.0924213949713));
#194981=CARTESIAN_POINT('Ctrl Pts',(5.45256165018521,-4.01171860314079,
46.1008599841581));
#194982=CARTESIAN_POINT('Ctrl Pts',(5.55476905327486,-3.86481949963771,
46.1092985733449));
#194983=CARTESIAN_POINT('Ctrl Pts',(5.65709070111746,-3.71775619617181,
46.1177465949651));
#194984=CARTESIAN_POINT('Ctrl Pts',(5.75350028792251,-3.56672502468919,
46.1261946165854));
#194985=CARTESIAN_POINT('Ctrl Pts',(5.84370826213485,-3.41223720556717,
46.1346426382057));
#194986=CARTESIAN_POINT('Ctrl Pts',(5.89498102698885,-3.32442880845135,
46.139444358118));
#194987=CARTESIAN_POINT('Ctrl Pts',(5.944251136978,-3.23550415664104,46.1442460780302));
#194988=CARTESIAN_POINT('Ctrl Pts',(5.99147222024434,-3.14556030526206,
46.1490477979425));
#194989=CARTESIAN_POINT('Ctrl Pts',(6.07250144033901,-2.99122076822851,
46.1572873297933));
#194990=CARTESIAN_POINT('Ctrl Pts',(6.14767546819983,-2.83353443999638,
46.1655268616441));
#194991=CARTESIAN_POINT('Ctrl Pts',(6.21670730001626,-2.67298322963773,
46.1737663934949));
#194992=CARTESIAN_POINT('Ctrl Pts',(6.28566251132403,-2.51261021990161,
46.1819967800412));
#194993=CARTESIAN_POINT('Ctrl Pts',(6.34848896184637,-2.3493789836758,46.1902271665875));
#194994=CARTESIAN_POINT('Ctrl Pts',(6.40494497246148,-2.18379689983762,
46.1984575531339));
#194995=CARTESIAN_POINT('Ctrl Pts',(6.46134839208383,-2.01836906221835,
46.2066802727516));
#194996=CARTESIAN_POINT('Ctrl Pts',(6.51139307590824,-1.85059507310794,
46.2149029923694));
#194997=CARTESIAN_POINT('Ctrl Pts',(6.55488496484103,-1.68100330091912,
46.2231257119872));
#194998=CARTESIAN_POINT('Ctrl Pts',(6.59833831682685,-1.51156179925877,
46.231341145683));
#194999=CARTESIAN_POINT('Ctrl Pts',(6.63525035824642,-1.34030606820669,
46.2395565793787));
#195000=CARTESIAN_POINT('Ctrl Pts',(6.6654765442675,-1.16778056064477,46.2477720130745));
#195001=CARTESIAN_POINT('Ctrl Pts',(6.69568719637607,-0.995343717796904,
46.2559832246753));
#195002=CARTESIAN_POINT('Ctrl Pts',(6.71921877493554,-0.821638747792825,
46.2641944362761));
#195003=CARTESIAN_POINT('Ctrl Pts',(6.73597751835221,-0.647221656199521,
46.2724056478769));
#195004=CARTESIAN_POINT('Ctrl Pts',(6.7527306418111,-0.472863054474237,
46.2806141058905));
#195005=CARTESIAN_POINT('Ctrl Pts',(6.76271542062078,-0.297793160777767,
46.288822563904));
#195006=CARTESIAN_POINT('Ctrl Pts',(6.76588977680415,-0.122574581937041,
46.2970310219175));
#195007=CARTESIAN_POINT('Ctrl Pts',(6.76730402179845,-0.0445108790260286,
46.3006880692007));
#195008=CARTESIAN_POINT('Ctrl Pts',(6.7673671566835,0.0335822734222091,
46.304345116484));
#195009=CARTESIAN_POINT('Ctrl Pts',(6.76607878852531,0.111654948246415,
46.3080021637673));
#195010=CARTESIAN_POINT('Ctrl Pts',(6.76295775994808,0.300783379958654,
46.3168612379432));
#195011=CARTESIAN_POINT('Ctrl Pts',(6.75190560870376,0.489594982317368,
46.3257203121191));
#195012=CARTESIAN_POINT('Ctrl Pts',(6.73300540505689,0.677441669426068,
46.334579386295));
#195013=CARTESIAN_POINT('Ctrl Pts',(6.71406969172986,0.865641282667262,
46.343455104889));
#195014=CARTESIAN_POINT('Ctrl Pts',(6.68725648509868,1.05287209978896,46.3523308234829));
#195015=CARTESIAN_POINT('Ctrl Pts',(6.65270016103237,1.23849487984404,46.3612065420769));
#195016=CARTESIAN_POINT('Ctrl Pts',(6.61804522298096,1.42464737486621,46.3701075894639));
#195017=CARTESIAN_POINT('Ctrl Pts',(6.57560299673479,1.60918239336955,46.3790086368509));
#195018=CARTESIAN_POINT('Ctrl Pts',(6.52555888234382,1.79147153844647,46.3879096842379));
#195019=CARTESIAN_POINT('Ctrl Pts',(6.47544673229294,1.97400850811634,46.3968228327209));
#195020=CARTESIAN_POINT('Ctrl Pts',(6.41771212445246,2.15429325699545,46.4057359812039));
#195021=CARTESIAN_POINT('Ctrl Pts',(6.35258963012617,2.33171481772825,46.4146491296869));
#195022=CARTESIAN_POINT('Ctrl Pts',(6.28732254605501,2.50953030284104,46.4235820677968));
#195023=CARTESIAN_POINT('Ctrl Pts',(6.21463485592987,2.68446964016014,46.4325150059067));
#195024=CARTESIAN_POINT('Ctrl Pts',(6.13480951953011,2.85594137878962,46.4414479440166));
#195025=CARTESIAN_POINT('Ctrl Pts',(6.05882737347025,3.01915761159616,46.4499508058751));
#195026=CARTESIAN_POINT('Ctrl Pts',(5.97637876706631,3.17923211546311,46.4584536677335));
#195027=CARTESIAN_POINT('Ctrl Pts',(5.88774534609079,3.33567740340493,46.4669565295919));
#195028=CARTESIAN_POINT('Ctrl Pts',(5.80203966925059,3.48695498181656,46.4751785244403));
#195029=CARTESIAN_POINT('Ctrl Pts',(5.71038591012282,3.63512857379914,46.4834005192887));
#195030=CARTESIAN_POINT('Ctrl Pts',(5.61303486396487,3.77969954042842,46.4916225141371));
#195031=CARTESIAN_POINT('Ctrl Pts',(5.51578170093818,3.92412514591923,46.4998362420522));
#195032=CARTESIAN_POINT('Ctrl Pts',(5.41284285425992,4.06495504278447,46.5080499699674));
#195033=CARTESIAN_POINT('Ctrl Pts',(5.30451494138021,4.20171515415718,46.5162636978825));
#195034=CARTESIAN_POINT('Ctrl Pts',(5.19627624328738,4.33836263505576,46.5244706612809));
#195035=CARTESIAN_POINT('Ctrl Pts',(5.08265753808488,4.47094672502422,46.5326776246792));
#195036=CARTESIAN_POINT('Ctrl Pts',(4.96399869897026,4.59902227833499,46.5408845880776));
#195037=CARTESIAN_POINT('Ctrl Pts',(4.84541600183957,4.72701564706688,46.5490862851639));
#195038=CARTESIAN_POINT('Ctrl Pts',(4.72179985522649,4.8505059790308,46.5572879822502));
#195039=CARTESIAN_POINT('Ctrl Pts',(4.59353039710216,4.96908115157103,46.5654896793365));
#195040=CARTESIAN_POINT('Ctrl Pts',(4.46531758487443,5.08760395937018,46.5736877544188));
#195041=CARTESIAN_POINT('Ctrl Pts',(4.33245581749533,5.20121568852132,46.5818858295011));
#195042=CARTESIAN_POINT('Ctrl Pts',(4.19536213566963,5.30954099245778,46.5900839045835));
#195043=CARTESIAN_POINT('Ctrl Pts',(4.05830407533218,5.4178381498853,46.5982798495338));
#195044=CARTESIAN_POINT('Ctrl Pts',(3.91701657320311,5.52085139744787,46.6064757944842));
#195045=CARTESIAN_POINT('Ctrl Pts',(3.7719498318142,5.61824558614848,46.6146717394345));
#195046=CARTESIAN_POINT('Ctrl Pts',(3.62687458965975,5.71564548205086,46.622868164659));
#195047=CARTESIAN_POINT('Ctrl Pts',(3.47801996180599,5.80742545870113,46.6310645898836));
#195048=CARTESIAN_POINT('Ctrl Pts',(3.32586544744336,5.89329347865032,46.6392610151081));
#195049=CARTESIAN_POINT('Ctrl Pts',(3.25105656024912,5.93551168719234,46.6432909017834));
#195050=CARTESIAN_POINT('Ctrl Pts',(3.17545039875157,5.9763014568265,46.6473207884587));
#195051=CARTESIAN_POINT('Ctrl Pts',(3.09910619832134,6.0156321173694,46.651350675134));
#195052=CARTESIAN_POINT('Origin',(0.,0.,4.30282021618968));
#195053=CARTESIAN_POINT('',(3.09910619832136,6.01563211736939,49.0458451349191));
#195054=CARTESIAN_POINT('',(3.09910619832125,6.01563211736945,48.651281539311));
#195055=CARTESIAN_POINT('',(3.09910619832133,6.0156321173694,4.30282021618968));
#195056=CARTESIAN_POINT('',(-6.76699996850575,0.000652873004102149,47.6971797837837));
#195057=CARTESIAN_POINT('Ctrl Pts',(-6.76699996850581,0.000652872448132562,
47.69717978381));
#195058=CARTESIAN_POINT('Ctrl Pts',(-6.76701135541745,-0.117372066373527,
47.7027599263854));
#195059=CARTESIAN_POINT('Ctrl Pts',(-6.76393518322527,-0.235386287105458,
47.7083400689607));
#195060=CARTESIAN_POINT('Ctrl Pts',(-6.75777199804277,-0.353279807615802,
47.7139202115361));
#195061=CARTESIAN_POINT('Ctrl Pts',(-6.74867155662429,-0.527359126223625,
47.7221597433869));
#195062=CARTESIAN_POINT('Ctrl Pts',(-6.73282781940791,-0.701327768706293,
47.7303992752377));
#195063=CARTESIAN_POINT('Ctrl Pts',(-6.71023996551987,-0.874624836795691,
47.7386388070885));
#195064=CARTESIAN_POINT('Ctrl Pts',(-6.68767718257104,-1.04772955725079,
47.7468691936348));
#195065=CARTESIAN_POINT('Ctrl Pts',(-6.6583852334291,-1.22016383771851,
47.7550995801811));
#195066=CARTESIAN_POINT('Ctrl Pts',(-6.62241527335144,-1.39136801288573,
47.7633299667274));
#195067=CARTESIAN_POINT('Ctrl Pts',(-6.5864788207051,-1.562412704636,47.7715526863452));
#195068=CARTESIAN_POINT('Ctrl Pts',(-6.54387681875919,-1.73222922689334,
47.779775405963));
#195069=CARTESIAN_POINT('Ctrl Pts',(-6.49471208585917,-1.90026417158111,
47.7879981255808));
#195070=CARTESIAN_POINT('Ctrl Pts',(-6.44559091645483,-2.06815022520093,
47.7962135592766));
#195071=CARTESIAN_POINT('Ctrl Pts',(-6.38991870560588,-2.2342575072782,
47.8044289929724));
#195072=CARTESIAN_POINT('Ctrl Pts',(-6.32784905995541,-2.39804405181002,
47.8126444266682));
#195073=CARTESIAN_POINT('Ctrl Pts',(-6.26581131328305,-2.56174642277614,
47.820855638269));
#195074=CARTESIAN_POINT('Ctrl Pts',(-6.19738280553783,-2.72313009952606,
47.8290668498698));
#195075=CARTESIAN_POINT('Ctrl Pts',(-6.12276670973295,-2.88166910282668,
47.8372780614705));
#195076=CARTESIAN_POINT('Ctrl Pts',(-6.04817563604925,-3.04015494089387,
47.8454865194841));
#195077=CARTESIAN_POINT('Ctrl Pts',(-5.96740125923448,-3.19579768417759,
47.8536949774976));
#195078=CARTESIAN_POINT('Ctrl Pts',(-5.88069456558192,-3.34809205762554,
47.8619034355111));
#195079=CARTESIAN_POINT('Ctrl Pts',(-5.84206484024985,-3.4159425264658,
47.8655604827944));
#195080=CARTESIAN_POINT('Ctrl Pts',(-5.80225823542211,-3.48312867576308,
47.8692175300776));
#195081=CARTESIAN_POINT('Ctrl Pts',(-5.76129989740476,-3.54960737155026,
47.8728745773609));
#195082=CARTESIAN_POINT('Ctrl Pts',(-5.66207969965679,-3.71064977857462,
47.8817336515368));
#195083=CARTESIAN_POINT('Ctrl Pts',(-5.55620108325363,-3.86737147401267,
47.8905927257127));
#195084=CARTESIAN_POINT('Ctrl Pts',(-5.44406628293178,-4.01925755669445,
47.8994517998886));
#195085=CARTESIAN_POINT('Ctrl Pts',(-5.33172080388054,-4.1714290027676,
47.9083275184826));
#195086=CARTESIAN_POINT('Ctrl Pts',(-5.21309580497063,-4.31874647139722,
47.9172032370765));
#195087=CARTESIAN_POINT('Ctrl Pts',(-5.08863312498752,-4.46072885516254,
47.9260789556705));
#195088=CARTESIAN_POINT('Ctrl Pts',(-4.96381526368203,-4.60311641653475,
47.9349800030575));
#195089=CARTESIAN_POINT('Ctrl Pts',(-4.83312655610622,-4.7401382298894,
47.9438810504445));
#195090=CARTESIAN_POINT('Ctrl Pts',(-4.69704718270191,-4.87134855696778,
47.9527820978315));
#195091=CARTESIAN_POINT('Ctrl Pts',(-4.56078280752294,-5.00273726628556,
47.9616952463145));
#195092=CARTESIAN_POINT('Ctrl Pts',(-4.41911331812032,-5.12829853178341,
47.9706083947976));
#195093=CARTESIAN_POINT('Ctrl Pts',(-4.27255228179476,-5.24762670159858,
47.9795215432806));
#195094=CARTESIAN_POINT('Ctrl Pts',(-4.12566583989226,-5.36721981258036,
47.9884544813905));
#195095=CARTESIAN_POINT('Ctrl Pts',(-3.97386632979164,-5.48055198264083,
47.9973874195004));
#195096=CARTESIAN_POINT('Ctrl Pts',(-3.81769896731011,-5.58725904133676,
48.0063203576103));
#195097=CARTESIAN_POINT('Ctrl Pts',(-3.66905028155447,-5.6888286893346,
48.0148232194687));
#195098=CARTESIAN_POINT('Ctrl Pts',(-3.51644457724239,-5.78439603991769,
48.0233260813272));
#195099=CARTESIAN_POINT('Ctrl Pts',(-3.36037287420605,-5.87368565266309,
48.0318289431856));
#195100=CARTESIAN_POINT('Ctrl Pts',(-3.20944315916262,-5.9600335014135,
48.0400516670515));
#195101=CARTESIAN_POINT('Ctrl Pts',(-3.05498229824922,-6.04067509035055,
48.0482743909173));
#195102=CARTESIAN_POINT('Ctrl Pts',(-2.89746060097193,-6.11530956418523,
48.0564971147832));
#195103=CARTESIAN_POINT('Ctrl Pts',(-2.74010563507517,-6.1898650399576,
48.0647111351744));
#195104=CARTESIAN_POINT('Ctrl Pts',(-2.57969660576254,-6.25842590978019,
48.0729251555656));
#195105=CARTESIAN_POINT('Ctrl Pts',(-2.41673061829624,-6.32073588426138,
48.0811391759568));
#195106=CARTESIAN_POINT('Ctrl Pts',(-2.253904405844,-6.38299241582669,48.0893461512288));
#195107=CARTESIAN_POINT('Ctrl Pts',(-2.08852593613141,-6.43900860227001,
48.0975531265008));
#195108=CARTESIAN_POINT('Ctrl Pts',(-1.92111469273606,-6.48857513922384,
48.1057601017727));
#195109=CARTESIAN_POINT('Ctrl Pts',(-1.75381343518607,-6.53810911195224,
48.1139616852258));
#195110=CARTESIAN_POINT('Ctrl Pts',(-1.58448240682351,-6.58120177389115,
48.1221632686788));
#195111=CARTESIAN_POINT('Ctrl Pts',(-1.41365883454757,-6.61769277766093,
48.1303648521318));
#195112=CARTESIAN_POINT('Ctrl Pts',(-1.24291321022215,-6.65416713033907,
48.1385626931469));
#195113=CARTESIAN_POINT('Ctrl Pts',(-1.07067674890226,-6.68404575146301,
48.1467605341619));
#195114=CARTESIAN_POINT('Ctrl Pts',(-0.897499613741063,-6.7072187561861,
48.154958375177));
#195115=CARTESIAN_POINT('Ctrl Pts',(-0.724337760921886,-6.73038971596382,
48.1631554927581));
#195116=CARTESIAN_POINT('Ctrl Pts',(-0.550235753757301,-6.74685618198163,
48.1713526103393));
#195117=CARTESIAN_POINT('Ctrl Pts',(-0.375752040519851,-6.75655973140512,
48.1795497279205));
#195118=CARTESIAN_POINT('Ctrl Pts',(-0.20127026860789,-6.76626317286582,
48.1877467542996));
#195119=CARTESIAN_POINT('Ctrl Pts',(-0.0264071573010266,-6.76920382660556,
48.1959437806787));
#195120=CARTESIAN_POINT('Ctrl Pts',(0.148275774513133,-6.76537532548583,
48.2041408070578));
#195121=CARTESIAN_POINT('Ctrl Pts',(0.322988525441801,-6.76154617082479,
48.2123392327039));
#195122=CARTESIAN_POINT('Ctrl Pts',(0.497520676842875,-6.75094556702153,
48.2205376583501));
#195123=CARTESIAN_POINT('Ctrl Pts',(0.671312712364482,-6.73361925284003,
48.2287360839962));
#195124=CARTESIAN_POINT('Ctrl Pts',(0.845166015927335,-6.71628683049983,
48.2369373998869));
#195125=CARTESIAN_POINT('Ctrl Pts',(1.0182783270149,-6.69222401018458,48.2451387157775));
#195126=CARTESIAN_POINT('Ctrl Pts',(1.19009718442701,-6.66152817990128,
48.2533400316682));
#195127=CARTESIAN_POINT('Ctrl Pts',(1.36211171475564,-6.63079739220571,
48.2615506874848));
#195128=CARTESIAN_POINT('Ctrl Pts',(1.53282949495643,-6.59341856639132,
48.2697613433014));
#195129=CARTESIAN_POINT('Ctrl Pts',(1.70170912459192,-6.54954006440762,
48.277971999118));
#195130=CARTESIAN_POINT('Ctrl Pts',(1.87068827090139,-6.50563570588583,
48.2861874932751));
#195131=CARTESIAN_POINT('Ctrl Pts',(2.03782676451964,-6.45522413992352,
48.2944029874323));
#195132=CARTESIAN_POINT('Ctrl Pts',(2.20260034230712,-6.39850300711569,
48.3026184815894));
#195133=CARTESIAN_POINT('Ctrl Pts',(2.36762956933301,-6.34169387042643,
48.3108467222369));
#195134=CARTESIAN_POINT('Ctrl Pts',(2.5302862137073,-6.27855573355922,48.3190749628844));
#195135=CARTESIAN_POINT('Ctrl Pts',(2.69006666413196,-6.20933413036583,
48.3273032035319));
#195136=CARTESIAN_POINT('Ctrl Pts',(2.83528158444731,-6.14642274436639,
48.334781360633));
#195137=CARTESIAN_POINT('Ctrl Pts',(2.97812091338683,-6.07848714887653,
48.3422595177342));
#195138=CARTESIAN_POINT('Ctrl Pts',(3.11822635877642,-6.00574336576514,
48.3497376748353));
#195139=CARTESIAN_POINT('Ctrl Pts',(3.26940721086617,-5.92724914960935,
48.3578069840578));
#195140=CARTESIAN_POINT('Ctrl Pts',(3.41789934746328,-5.84289880365092,
48.3658762932804));
#195141=CARTESIAN_POINT('Ctrl Pts',(3.56320468417953,-5.75290025801257,
48.3739456025029));
#195142=CARTESIAN_POINT('Ctrl Pts',(3.70832878564812,-5.66301396502148,
48.3820048471037));
#195143=CARTESIAN_POINT('Ctrl Pts',(3.85027368283433,-5.56749368369514,
48.3900640917044));
#195144=CARTESIAN_POINT('Ctrl Pts',(3.98856240410905,-5.46659482205585,
48.3981233363052));
#195145=CARTESIAN_POINT('Ctrl Pts',(4.12670898899514,-5.3657996666312,48.4061742974255));
#195146=CARTESIAN_POINT('Ctrl Pts',(4.26120657738466,-5.2596371502495,48.4142252585457));
#195147=CARTESIAN_POINT('Ctrl Pts',(4.39160400129685,-5.14840784085658,
48.422276219666));
#195148=CARTESIAN_POINT('Ctrl Pts',(4.521895972344,-5.03726848300565,48.4303206699451));
#195149=CARTESIAN_POINT('Ctrl Pts',(4.64809409604339,-4.92107072851637,
48.4383651202242));
#195150=CARTESIAN_POINT('Ctrl Pts',(4.76977743883564,-4.80015751657948,
48.4464095705034));
#195151=CARTESIAN_POINT('Ctrl Pts',(4.89138901121838,-4.67931562081898,
48.4544492760616));
#195152=CARTESIAN_POINT('Ctrl Pts',(5.00849083967173,-4.55376406656954,
48.4624889816199));
#195153=CARTESIAN_POINT('Ctrl Pts',(5.1206963478992,-4.42388493437745,48.4705286871782));
#195154=CARTESIAN_POINT('Ctrl Pts',(5.23532375203256,-4.29120243055518,
48.4787419254826));
#195155=CARTESIAN_POINT('Ctrl Pts',(5.34484076078907,-4.15400366706386,
48.4869551637871));
#195156=CARTESIAN_POINT('Ctrl Pts',(5.44887592694491,-4.01273474487915,
48.4951684020915));
#195157=CARTESIAN_POINT('Ctrl Pts',(5.55068021272667,-3.87449512593499,
48.5032055196397));
#195158=CARTESIAN_POINT('Ctrl Pts',(5.64723515239597,-3.73235845615392,
48.5112426371879));
#195159=CARTESIAN_POINT('Ctrl Pts',(5.7382345678756,-3.58677474118985,48.519279754736));
#195160=CARTESIAN_POINT('Ctrl Pts',(5.82924361051464,-3.44117562439465,
48.5273177225601));
#195161=CARTESIAN_POINT('Ctrl Pts',(5.91469576054597,-3.29212905307198,
48.5353556903843));
#195162=CARTESIAN_POINT('Ctrl Pts',(5.99432936412382,-3.14011217544898,
48.5433936582083));
#195163=CARTESIAN_POINT('Ctrl Pts',(6.07398717078326,-2.98804909525914,
48.5514340690161));
#195164=CARTESIAN_POINT('Ctrl Pts',(6.14782273767134,-2.83301424259315,
48.5594744798238));
#195165=CARTESIAN_POINT('Ctrl Pts',(6.21562143990875,-2.67550726325806,
48.5675148906316));
#195166=CARTESIAN_POINT('Ctrl Pts',(6.28598255070105,-2.51204740845511,
48.5758591836193));
#195167=CARTESIAN_POINT('Ctrl Pts',(6.34984138638855,-2.34592532028708,
48.5842034766071));
#195168=CARTESIAN_POINT('Ctrl Pts',(6.40701419024083,-2.17771856906548,
48.5925477695949));
#195169=CARTESIAN_POINT('Ctrl Pts',(6.46220216729716,-2.01535132972001,
48.6006023798104));
#195170=CARTESIAN_POINT('Ctrl Pts',(6.51116052038201,-1.85104211643753,
48.6086569900259));
#195171=CARTESIAN_POINT('Ctrl Pts',(6.55377592327011,-1.6853219714835,48.6167116002415));
#195172=CARTESIAN_POINT('Ctrl Pts',(6.59642358662007,-1.51947637403921,
48.6247723079107));
#195173=CARTESIAN_POINT('Ctrl Pts',(6.63271866035056,-1.35221808076157,
48.63283301558));
#195174=CARTESIAN_POINT('Ctrl Pts',(6.66259945556137,-1.18408508763237,
48.6408937232492));
#195175=CARTESIAN_POINT('Ctrl Pts',(6.69252238090336,-1.01571503705519,
48.6489657960334));
#195176=CARTESIAN_POINT('Ctrl Pts',(6.71601293305232,-0.846468192526026,
48.6570378688175));
#195177=CARTESIAN_POINT('Ctrl Pts',(6.73306139370834,-0.676884974389522,
48.6651099416017));
#195178=CARTESIAN_POINT('Ctrl Pts',(6.73484709043169,-0.659122420744859,
48.665955429896));
#195179=CARTESIAN_POINT('Ctrl Pts',(6.73656215819896,-0.641356173871092,
48.6668009181904));
#195180=CARTESIAN_POINT('Ctrl Pts',(6.73820661880235,-0.623586852273408,
48.6676464064847));
#195181=CARTESIAN_POINT('Ctrl Pts',(6.75441401293016,-0.448456844340352,
48.6759793285314));
#195182=CARTESIAN_POINT('Ctrl Pts',(6.76381033163896,-0.27246969054077,
48.6843122505782));
#195183=CARTESIAN_POINT('Ctrl Pts',(6.76631632073985,-0.0961896443986176,
48.6926451726249));
#195184=CARTESIAN_POINT('Ctrl Pts',(6.76881934836934,0.0798820814776233,
48.7009682471785));
#195185=CARTESIAN_POINT('Ctrl Pts',(6.7644482623793,0.256245665240132,48.7092913217321));
#195186=CARTESIAN_POINT('Ctrl Pts',(6.75317546575908,0.43233104060391,48.7176143962857));
#195187=CARTESIAN_POINT('Ctrl Pts',(6.74191392166429,0.608240647236013,
48.7259291627317));
#195188=CARTESIAN_POINT('Ctrl Pts',(6.72376441472939,0.783872253675042,
48.7342439291776));
#195189=CARTESIAN_POINT('Ctrl Pts',(6.69875136458474,0.958654867756931,
48.7425586956236));
#195190=CARTESIAN_POINT('Ctrl Pts',(6.67375869427519,1.13329507454214,48.7508666874632));
#195191=CARTESIAN_POINT('Ctrl Pts',(6.64191367274921,1.30708732435082,48.7591746793027));
#195192=CARTESIAN_POINT('Ctrl Pts',(6.60329262589929,1.47946459800295,48.7674826711423));
#195193=CARTESIAN_POINT('Ctrl Pts',(6.56469596570982,1.65173302670177,48.7757854170294));
#195194=CARTESIAN_POINT('Ctrl Pts',(6.51933188282585,1.82258792124106,48.7840881629165));
#195195=CARTESIAN_POINT('Ctrl Pts',(6.46732803046758,1.99147110105278,48.7923909088036));
#195196=CARTESIAN_POINT('Ctrl Pts',(6.41534543042666,2.1602852636904,48.800690261623));
#195197=CARTESIAN_POINT('Ctrl Pts',(6.35672856991603,2.32712898517587,48.8089896144425));
#195198=CARTESIAN_POINT('Ctrl Pts',(6.29165540966437,2.49145764684875,48.8172889672619));
#195199=CARTESIAN_POINT('Ctrl Pts',(6.22659608938186,2.655751358573,48.8255865549483));
#195200=CARTESIAN_POINT('Ctrl Pts',(6.15508333299288,2.81753075286874,48.8338841426346));
#195201=CARTESIAN_POINT('Ctrl Pts',(6.07734393609153,2.97626942370001,48.842181730321));
#195202=CARTESIAN_POINT('Ctrl Pts',(5.99960815469194,3.13500071191746,48.8504789321034));
#195203=CARTESIAN_POINT('Ctrl Pts',(5.91564646300443,3.29069124612387,48.8587761338857));
#195204=CARTESIAN_POINT('Ctrl Pts',(5.82573255948691,3.442837368412,48.8670733356681));
#195205=CARTESIAN_POINT('Ctrl Pts',(5.73580789688236,3.59500169648709,48.8753715302927));
#195206=CARTESIAN_POINT('Ctrl Pts',(5.63992978073161,3.74362046834022,48.8836697249172));
#195207=CARTESIAN_POINT('Ctrl Pts',(5.53841645000472,3.88821710123254,48.8919679195418));
#195208=CARTESIAN_POINT('Ctrl Pts',(5.43683172376906,4.03291543062223,48.9002719503834));
#195209=CARTESIAN_POINT('Ctrl Pts',(5.3296040636254,4.17358568342901,48.9085759812249));
#195210=CARTESIAN_POINT('Ctrl Pts',(5.21709393807584,4.30978187862128,48.9168800120665));
#195211=CARTESIAN_POINT('Ctrl Pts',(5.1045429007476,4.44602759849913,48.9251870624823));
#195212=CARTESIAN_POINT('Ctrl Pts',(4.98670579675691,4.57779575468685,48.933494112898));
#195213=CARTESIAN_POINT('Ctrl Pts',(4.8639816687714,4.70467547508388,48.9418011633138));
#195214=CARTESIAN_POINT('Ctrl Pts',(4.74112632798099,4.83169085131545,48.9501170953684));
#195215=CARTESIAN_POINT('Ctrl Pts',(4.61337377080325,4.9538071039659,48.958433027423));
#195216=CARTESIAN_POINT('Ctrl Pts',(4.48115879339748,5.07065132585119,48.9667489594777));
#195217=CARTESIAN_POINT('Ctrl Pts',(4.3814923350924,5.15873098215957,48.9730176856966));
#195218=CARTESIAN_POINT('Ctrl Pts',(4.27929085903611,5.24381561418234,48.9792864119154));
#195219=CARTESIAN_POINT('Ctrl Pts',(4.17475210936812,5.32576133762361,48.9855551381343));
#195220=CARTESIAN_POINT('Ctrl Pts',(4.03381449903641,5.4362393610876,48.9940065429571));
#195221=CARTESIAN_POINT('Ctrl Pts',(3.88836913319198,5.5412132432926,49.0024579477799));
#195222=CARTESIAN_POINT('Ctrl Pts',(3.73887277406846,5.64031199308421,49.0109093526026));
#195223=CARTESIAN_POINT('Ctrl Pts',(3.58953094653658,5.73930830635079,49.0193520213662));
#195224=CARTESIAN_POINT('Ctrl Pts',(3.4361467509964,5.83244141481807,49.0277946901299));
#195225=CARTESIAN_POINT('Ctrl Pts',(3.27920823040502,5.91938192564426,49.0362373588935));
#195226=CARTESIAN_POINT('Ctrl Pts',(3.21967610070156,5.95236142454285,49.039439950902));
#195227=CARTESIAN_POINT('Ctrl Pts',(3.15963283954846,5.98445027557277,49.0426425429105));
#195228=CARTESIAN_POINT('Ctrl Pts',(3.09910619832136,6.01563211736939,49.0458451349191));
#195229=CARTESIAN_POINT('Ctrl Pts',(3.09910619832128,6.01563211736943,47.0456420231655));
#195230=CARTESIAN_POINT('Ctrl Pts',(2.93589454944422,6.09971475786413,47.0542963548475));
#195231=CARTESIAN_POINT('Ctrl Pts',(2.7693543383796,6.17710224807514,47.0629506865295));
#195232=CARTESIAN_POINT('Ctrl Pts',(2.60005473004366,6.24755987572569,47.0716050182115));
#195233=CARTESIAN_POINT('Ctrl Pts',(2.55768430450257,6.26519322819185,47.07377092822));
#195234=CARTESIAN_POINT('Ctrl Pts',(2.51514113168975,6.2823927721951,47.0759368382285));
#195235=CARTESIAN_POINT('Ctrl Pts',(2.47243429729718,6.29915531206753,47.0781027482371));
#195236=CARTESIAN_POINT('Ctrl Pts',(2.2940953943415,6.36915377985658,47.0871473430969));
#195237=CARTESIAN_POINT('Ctrl Pts',(2.11273661928173,6.43159254316305,47.0961919379567));
#195238=CARTESIAN_POINT('Ctrl Pts',(1.92898827293668,6.48623875931751,47.1052365328165));
#195239=CARTESIAN_POINT('Ctrl Pts',(1.74540854462305,6.54083482896684,47.1142728278369));
#195240=CARTESIAN_POINT('Ctrl Pts',(1.55944385080278,6.5876525604937,47.1233091228572));
#195241=CARTESIAN_POINT('Ctrl Pts',(1.37174040463728,6.62650867820194,47.1323454178775));
#195242=CARTESIAN_POINT('Ctrl Pts',(1.1843691144388,6.66529603696293,47.1413657224652));
#195243=CARTESIAN_POINT('Ctrl Pts',(0.995265448640978,6.69614986708242,
47.1503860270529));
#195244=CARTESIAN_POINT('Ctrl Pts',(0.805086409902682,6.71893777859194,
47.1594063316406));
#195245=CARTESIAN_POINT('Ctrl Pts',(0.615146864720306,6.7416969931536,47.1684152769069));
#195246=CARTESIAN_POINT('Ctrl Pts',(0.424134884659359,6.75641053168001,
47.1774242221732));
#195247=CARTESIAN_POINT('Ctrl Pts',(0.232715743612232,6.76299729281884,
47.1864331674395));
#195248=CARTESIAN_POINT('Ctrl Pts',(0.04173127491135,6.76956909681754,47.1954216552983));
#195249=CARTESIAN_POINT('Ctrl Pts',(-0.149658271927432,6.76805095142059,
47.2044101431571));
#195250=CARTESIAN_POINT('Ctrl Pts',(-0.340784934590754,6.75841361773279,
47.2133986310159));
#195251=CARTESIAN_POINT('Ctrl Pts',(-0.508472276417358,6.74995818380283,
47.2212847920312));
#195252=CARTESIAN_POINT('Ctrl Pts',(-0.675957051506147,6.73525362376994,
47.2291709530465));
#195253=CARTESIAN_POINT('Ctrl Pts',(-0.842785732964303,6.71431315983339,
47.2370571140618));
#195254=CARTESIAN_POINT('Ctrl Pts',(-1.01459217602766,6.69274788344573,
47.245178578918));
#195255=CARTESIAN_POINT('Ctrl Pts',(-1.18562567720486,6.66457705395441,
47.2533000437742));
#195256=CARTESIAN_POINT('Ctrl Pts',(-1.35533969976107,6.62988260063869,
47.2614215086304));
#195257=CARTESIAN_POINT('Ctrl Pts',(-1.52504161920968,6.59519062154811,
47.2695423943066));
#195258=CARTESIAN_POINT('Ctrl Pts',(-1.69342388870087,6.55397601864855,
47.2776632799828));
#195259=CARTESIAN_POINT('Ctrl Pts',(-1.85995005486183,6.50637186098516,
47.285784165659));
#195260=CARTESIAN_POINT('Ctrl Pts',(-2.02649612566183,6.45876201326358,
47.2939060220133));
#195261=CARTESIAN_POINT('Ctrl Pts',(-2.19118529961601,6.40476119180939,
47.3020278783675));
#195262=CARTESIAN_POINT('Ctrl Pts',(-2.35349622554594,6.34455234956266,
47.3101497347218));
#195263=CARTESIAN_POINT('Ctrl Pts',(-2.51592557151901,6.28429957968964,
47.318277516682));
#195264=CARTESIAN_POINT('Ctrl Pts',(-2.67597286024064,6.21782987027496,
47.3264052986422));
#195265=CARTESIAN_POINT('Ctrl Pts',(-2.8331360808695,6.14537459779918,47.3345330806024));
#195266=CARTESIAN_POINT('Ctrl Pts',(-2.99036332395316,6.07288980973834,
47.3426641735188));
#195267=CARTESIAN_POINT('Ctrl Pts',(-3.14470383092736,5.99441476425881,
47.3507952664353));
#195268=CARTESIAN_POINT('Ctrl Pts',(-3.2956803909903,5.91022670973306,47.3589263593518));
#195269=CARTESIAN_POINT('Ctrl Pts',(-3.44682173565884,5.82594676746422,
47.3670663270163));
#195270=CARTESIAN_POINT('Ctrl Pts',(-3.59459148762991,5.73594155201354,
47.3752062946809));
#195271=CARTESIAN_POINT('Ctrl Pts',(-3.73854097234446,5.64053192510261,
47.3833462623454));
#195272=CARTESIAN_POINT('Ctrl Pts',(-3.81319939909274,5.59104836733972,
47.3875680015258));
#195273=CARTESIAN_POINT('Ctrl Pts',(-3.88683073018327,5.54011175266949,
47.3917897407062));
#195274=CARTESIAN_POINT('Ctrl Pts',(-3.95937594541187,5.48777105233936,
47.3960114798866));
#195275=CARTESIAN_POINT('Ctrl Pts',(-4.10320066113873,5.38400285312451,
47.4043813004955));
#195276=CARTESIAN_POINT('Ctrl Pts',(-4.24306674454081,5.27448811926054,
47.4127511211043));
#195277=CARTESIAN_POINT('Ctrl Pts',(-4.37849989789952,5.15955692323419,
47.4211209417132));
#195278=CARTESIAN_POINT('Ctrl Pts',(-4.51382446214451,5.04471787803212,
47.4294840514733));
#195279=CARTESIAN_POINT('Ctrl Pts',(-4.64472292002328,4.92447124588934,
47.4378471612335));
#195280=CARTESIAN_POINT('Ctrl Pts',(-4.77075213347198,4.7991887940539,47.4462102709936));
#195281=CARTESIAN_POINT('Ctrl Pts',(-4.89670197423966,4.6739852445921,47.4545681137016));
#195282=CARTESIAN_POINT('Ctrl Pts',(-5.01778844097024,4.54375243716413,
47.4629259564095));
#195283=CARTESIAN_POINT('Ctrl Pts',(-5.13360329946691,4.40890078859827,
47.4712837991175));
#195284=CARTESIAN_POINT('Ctrl Pts',(-5.24936512419065,4.27411089110479,
47.4796378146142));
#195285=CARTESIAN_POINT('Ctrl Pts',(-5.35985993037371,4.1347066276499,47.4879918301109));
#195286=CARTESIAN_POINT('Ctrl Pts',(-5.46471782846359,3.99113368045625,
47.4963458456076));
#195287=CARTESIAN_POINT('Ctrl Pts',(-5.56975227083553,3.847319006284,47.5047139263649));
#195288=CARTESIAN_POINT('Ctrl Pts',(-5.66913058203875,3.69932185952979,
47.5130820071223));
#195289=CARTESIAN_POINT('Ctrl Pts',(-5.76252242132577,3.54762235077493,
47.5214500878796));
#195290=CARTESIAN_POINT('Ctrl Pts',(-5.85573510001801,3.39621385860593,
47.5298021155178));
#195291=CARTESIAN_POINT('Ctrl Pts',(-5.94298408360168,3.24111749420683,
47.5381541431559));
#195292=CARTESIAN_POINT('Ctrl Pts',(-6.02398508524712,3.08283841495467,
47.5465061707941));
#195293=CARTESIAN_POINT('Ctrl Pts',(-6.1049927121405,2.92454638971268,47.5548588815628));
#195294=CARTESIAN_POINT('Ctrl Pts',(-6.17975118257862,2.76307143517032,
47.5632115923314));
#195295=CARTESIAN_POINT('Ctrl Pts',(-6.24802278409988,2.59894214813812,
47.5715643031001));
#195296=CARTESIAN_POINT('Ctrl Pts',(-6.31631061892291,2.4347738352125,47.5799189999372));
#195297=CARTESIAN_POINT('Ctrl Pts',(-6.37810837926626,2.26795024759497,
47.5882736967743));
#195298=CARTESIAN_POINT('Ctrl Pts',(-6.43322689711854,2.09901898280853,
47.5966283936114));
#195299=CARTESIAN_POINT('Ctrl Pts',(-6.48850761428414,1.92959059770366,
47.6050076761258));
#195300=CARTESIAN_POINT('Ctrl Pts',(-6.53706961132309,1.7580424404529,47.6133869586401));
#195301=CARTESIAN_POINT('Ctrl Pts',(-6.57877280228418,1.58494082410858,
47.6217662411545));
#195302=CARTESIAN_POINT('Ctrl Pts',(-6.62040978814003,1.41211401193305,
47.6301322212987));
#195303=CARTESIAN_POINT('Ctrl Pts',(-6.655209693143,1.23773901200889,47.638498201443));
#195304=CARTESIAN_POINT('Ctrl Pts',(-6.68308464123356,1.06238819558019,
47.6468641815872));
#195305=CARTESIAN_POINT('Ctrl Pts',(-6.71102607338273,0.886619152939204,
47.6552501152867));
#195306=CARTESIAN_POINT('Ctrl Pts',(-6.73200944340711,0.709869976767763,
47.6636360489861));
#195307=CARTESIAN_POINT('Ctrl Pts',(-6.74599863286547,0.532720794954758,
47.6720219826855));
#195308=CARTESIAN_POINT('Ctrl Pts',(-6.75998782232383,0.355571613141753,
47.6804079163849));
#195309=CARTESIAN_POINT('Ctrl Pts',(-6.76698285604561,0.178022769645797,
47.6887938500843));
#195310=CARTESIAN_POINT('Ctrl Pts',(-6.76699996850575,0.000652873004196812,
47.6971797837837));
#195311=CARTESIAN_POINT('',(-6.76699998394344,-0.000466164701145535,47.302820216223));
#195312=CARTESIAN_POINT('Ctrl Pts',(3.09910619832134,6.0156321173694,46.651350675134));
#195313=CARTESIAN_POINT('Ctrl Pts',(2.94376773000356,6.09565868824486,46.6595503343105));
#195314=CARTESIAN_POINT('Ctrl Pts',(2.78537251701673,6.16964140625866,46.6677499934871));
#195315=CARTESIAN_POINT('Ctrl Pts',(2.62443560179651,6.23735735484372,46.6759496526637));
#195316=CARTESIAN_POINT('Ctrl Pts',(2.4634275737236,6.30510322493106,46.6841529350062));
#195317=CARTESIAN_POINT('Ctrl Pts',(2.29987593656179,6.36657667055195,46.6923562173487));
#195318=CARTESIAN_POINT('Ctrl Pts',(2.13431370578073,6.42160369419637,46.7005594996913));
#195319=CARTESIAN_POINT('Ctrl Pts',(1.96855810439084,6.47669498738473,46.7087723631665));
#195320=CARTESIAN_POINT('Ctrl Pts',(1.80078755988934,6.5253247082003,46.7169852266417));
#195321=CARTESIAN_POINT('Ctrl Pts',(1.63154910437626,6.56736907140211,46.7251980901169));
#195322=CARTESIAN_POINT('Ctrl Pts',(1.46219735665508,6.6094415800909,46.7334164514764));
#195323=CARTESIAN_POINT('Ctrl Pts',(1.29137608955599,6.64491987211678,46.7416348128359));
#195324=CARTESIAN_POINT('Ctrl Pts',(1.11964027288898,6.67373168919197,46.7498531741954));
#195325=CARTESIAN_POINT('Ctrl Pts',(0.94766179720174,6.70258421674583,46.7580831479229));
#195326=CARTESIAN_POINT('Ctrl Pts',(0.774766545646292,6.72475141133308,
46.7663131216504));
#195327=CARTESIAN_POINT('Ctrl Pts',(0.601513306138231,6.74021295973196,
46.774543095378));
#195328=CARTESIAN_POINT('Ctrl Pts',(0.529080969826472,6.74667700090492,
46.7779838173325));
#195329=CARTESIAN_POINT('Ctrl Pts',(0.456586049233609,6.75196962851049,
46.7814245392871));
#195330=CARTESIAN_POINT('Ctrl Pts',(0.384069221555972,6.75609205332886,
46.7848652612416));
#195331=CARTESIAN_POINT('Ctrl Pts',(0.21400005755518,6.76576011748679,46.7929345704641));
#195332=CARTESIAN_POINT('Ctrl Pts',(0.0432538459028244,6.7690199795768,
46.8010038796867));
#195333=CARTESIAN_POINT('Ctrl Pts',(-0.127634967030817,6.76579620703957,
46.8090731889092));
#195334=CARTESIAN_POINT('Ctrl Pts',(-0.298310635167999,6.76257645542291,
46.8171324335099));
#195335=CARTESIAN_POINT('Ctrl Pts',(-0.469128182337606,6.75288916681211,
46.8251916781107));
#195336=CARTESIAN_POINT('Ctrl Pts',(-0.639547083441763,6.73671051241339,
46.8332509227114));
#195337=CARTESIAN_POINT('Ctrl Pts',(-0.809790824006049,6.72054848681478,
46.8413018838317));
#195338=CARTESIAN_POINT('Ctrl Pts',(-0.979636365564611,6.69790840775643,
46.849352844952));
#195339=CARTESIAN_POINT('Ctrl Pts',(-1.14854232124391,6.66881845129343,
46.8574038060722));
#195340=CARTESIAN_POINT('Ctrl Pts',(-1.31731168206985,6.63975201998275,
46.8654482563513));
#195341=CARTESIAN_POINT('Ctrl Pts',(-1.48514260350749,6.60424615591976,
46.8734927066304));
#195342=CARTESIAN_POINT('Ctrl Pts',(-1.6514980704397,6.56238090355429,46.8815371569095));
#195343=CARTESIAN_POINT('Ctrl Pts',(-1.81775541876575,6.52054034385618,
46.8895768624678));
#195344=CARTESIAN_POINT('Ctrl Pts',(-1.98253868403992,6.47234795351275,
46.8976165680261));
#195345=CARTESIAN_POINT('Ctrl Pts',(-2.14532041684306,6.41793497233155,
46.9056562735843));
#195346=CARTESIAN_POINT('Ctrl Pts',(-2.3116157063202,6.36234751604255,46.9138695118888));
#195347=CARTESIAN_POINT('Ctrl Pts',(-2.47582168400813,6.3002679477279,46.9220827501932));
#195348=CARTESIAN_POINT('Ctrl Pts',(-2.6373912325011,6.23189028198719,46.9302959884977));
#195349=CARTESIAN_POINT('Ctrl Pts',(-2.7954961608265,6.16497887422606,46.9383331060458));
#195350=CARTESIAN_POINT('Ctrl Pts',(-2.95107622949768,6.09203690069045,
46.946370223594));
#195351=CARTESIAN_POINT('Ctrl Pts',(-3.1036384543481,6.01329504886395,46.9544073411422));
#195352=CARTESIAN_POINT('Ctrl Pts',(-3.25621681931218,5.93454486665004,
46.9624453089663));
#195353=CARTESIAN_POINT('Ctrl Pts',(-3.40577637266506,5.84999375566314,
46.9704832767905));
#195354=CARTESIAN_POINT('Ctrl Pts',(-3.55184856323456,5.75991847024319,
46.9785212446146));
#195355=CARTESIAN_POINT('Ctrl Pts',(-3.69796514959805,5.66981580819665,
46.9865616554223));
#195356=CARTESIAN_POINT('Ctrl Pts',(-3.840591945594,5.57418582575094,46.99460206623));
#195357=CARTESIAN_POINT('Ctrl Pts',(-3.97928935785062,5.47334862826193,
47.0026424770377));
#195358=CARTESIAN_POINT('Ctrl Pts',(-4.12322875002765,5.36870035343654,
47.0109867700255));
#195359=CARTESIAN_POINT('Ctrl Pts',(-4.26293557804433,5.2584438285581,47.0193310630133));
#195360=CARTESIAN_POINT('Ctrl Pts',(-4.397957017878,5.1429819238354,47.027675356001));
#195361=CARTESIAN_POINT('Ctrl Pts',(-4.52829101623976,5.03152842637964,
47.0357299662166));
#195362=CARTESIAN_POINT('Ctrl Pts',(-4.65425926856358,4.91522521355805,
47.0437845764321));
#195363=CARTESIAN_POINT('Ctrl Pts',(-4.77549326467682,4.79447109481602,
47.0518391866476));
#195364=CARTESIAN_POINT('Ctrl Pts',(-4.89681903663767,4.67362556350033,
47.0598998943169));
#195365=CARTESIAN_POINT('Ctrl Pts',(-5.01340316372495,4.54832268899797,
47.0679606019861));
#195366=CARTESIAN_POINT('Ctrl Pts',(-5.12491799040585,4.4189936175123,47.0760213096553));
#195367=CARTESIAN_POINT('Ctrl Pts',(-5.23659004631182,4.28948219978359,
47.0840933824395));
#195368=CARTESIAN_POINT('Ctrl Pts',(-5.34317831071259,4.15593354829151,
47.0921654552236));
#195369=CARTESIAN_POINT('Ctrl Pts',(-5.44439858121225,4.01880742122511,
47.1002375280078));
#195370=CARTESIAN_POINT('Ctrl Pts',(-5.45500063549913,4.00444450126718,
47.1010830163022));
#195371=CARTESIAN_POINT('Ctrl Pts',(-5.46554383960578,3.99004235446042,
47.1019285045966));
#195372=CARTESIAN_POINT('Ctrl Pts',(-5.47602789656972,3.97560152379363,
47.102773992891));
#195373=CARTESIAN_POINT('Ctrl Pts',(-5.58175609229637,3.8299705932821,47.1113004585698));
#195374=CARTESIAN_POINT('Ctrl Pts',(-5.68178758471567,3.67995942872403,
47.1198269242485));
#195375=CARTESIAN_POINT('Ctrl Pts',(-5.77575621167564,3.52603590215561,
47.1283533899272));
#195376=CARTESIAN_POINT('Ctrl Pts',(-5.8696048493169,3.37230892181418,47.1368689680912));
#195377=CARTESIAN_POINT('Ctrl Pts',(-5.95740588438657,3.21467981033767,
47.1453845462552));
#195378=CARTESIAN_POINT('Ctrl Pts',(-6.03883491479121,3.05364730640241,
47.1539001244192));
#195379=CARTESIAN_POINT('Ctrl Pts',(-6.12016969913281,2.89280118169139,
47.1624058466423));
#195380=CARTESIAN_POINT('Ctrl Pts',(-6.19514703415947,2.72855980311904,
47.1709115688653));
#195381=CARTESIAN_POINT('Ctrl Pts',(-6.26348690843292,2.56144895476944,
47.1794172910883));
#195382=CARTESIAN_POINT('Ctrl Pts',(-6.33175582951311,2.3945116075924,47.1879141823301));
#195383=CARTESIAN_POINT('Ctrl Pts',(-6.39340090554652,2.22471102761238,
47.1964110735718));
#195384=CARTESIAN_POINT('Ctrl Pts',(-6.44818878959137,2.05259599867782,
47.2049079648135));
#195385=CARTESIAN_POINT('Ctrl Pts',(-6.5029109822524,1.88068733789604,47.2133946681724));
#195386=CARTESIAN_POINT('Ctrl Pts',(-6.55079228728986,1.70647007132983,
47.2218813715313));
#195387=CARTESIAN_POINT('Ctrl Pts',(-6.5916480686147,1.53051126736398,47.2303680748902));
#195388=CARTESIAN_POINT('Ctrl Pts',(-6.6324745582664,1.35467861758255,47.2388486936821));
#195389=CARTESIAN_POINT('Ctrl Pts',(-6.66628549112995,1.17710723318183,
47.2473293124739));
#195390=CARTESIAN_POINT('Ctrl Pts',(-6.69294621220899,0.998378685909012,
47.2558099312658));
#195391=CARTESIAN_POINT('Ctrl Pts',(-6.71958695073797,0.819784097959,47.2642841937258));
#195392=CARTESIAN_POINT('Ctrl Pts',(-6.73908811962763,0.640034396317557,
47.2727584561858));
#195393=CARTESIAN_POINT('Ctrl Pts',(-6.75136621022658,0.459720888595186,
47.2812327186459));
#195394=CARTESIAN_POINT('Ctrl Pts',(-6.76179202415042,0.306609534324127,
47.2884285511605));
#195395=CARTESIAN_POINT('Ctrl Pts',(-6.7670105622296,0.15309194578801,47.2956243836752));
#195396=CARTESIAN_POINT('Ctrl Pts',(-6.76699998394349,-0.000466163995218723,
47.3028202161899));
#195397=CARTESIAN_POINT('Ctrl Pts',(-6.76699998394344,-0.000466164701054033,
47.302820216223));
#195398=CARTESIAN_POINT('Ctrl Pts',(-6.76698667745886,-0.193627467444925,
47.3118718800187));
#195399=CARTESIAN_POINT('Ctrl Pts',(-6.75869855779439,-0.386573833465984,
47.3209235438144));
#195400=CARTESIAN_POINT('Ctrl Pts',(-6.74221614043191,-0.578628132481847,
47.3299752076101));
#195401=CARTESIAN_POINT('Ctrl Pts',(-6.72567262469657,-0.771394354082396,
47.3390604248536));
#195402=CARTESIAN_POINT('Ctrl Pts',(-6.70087401106703,-0.96326166573528,
47.3481456420971));
#195403=CARTESIAN_POINT('Ctrl Pts',(-6.66795266219676,-1.15355810200577,
47.3572308593406));
#195404=CARTESIAN_POINT('Ctrl Pts',(-6.63497125451219,-1.34420169836295,
47.3663326508555));
#195405=CARTESIAN_POINT('Ctrl Pts',(-6.5938375346171,-1.53326847497989,
47.3754344423705));
#195406=CARTESIAN_POINT('Ctrl Pts',(-6.54473447929962,-1.72009871677959,
47.3845362338855));
#195407=CARTESIAN_POINT('Ctrl Pts',(-6.49551953809281,-1.90735466870306,
47.393658764681));
#195408=CARTESIAN_POINT('Ctrl Pts',(-6.43829899304615,-2.09236367814682,
47.4027812954766));
#195409=CARTESIAN_POINT('Ctrl Pts',(-6.3733058150232,-2.2744805974533,47.4119038262721));
#195410=CARTESIAN_POINT('Ctrl Pts',(-6.35245748865429,-2.33289954366425,
47.4148301256949));
#195411=CARTESIAN_POINT('Ctrl Pts',(-6.33080974255341,-2.39102105881993,
47.4177564251177));
#195412=CARTESIAN_POINT('Ctrl Pts',(-6.30837130107367,-2.44882431541956,
47.4206827245405));
#195413=CARTESIAN_POINT('Ctrl Pts',(-6.24357586053917,-2.61574265861571,
47.4291329932639));
#195414=CARTESIAN_POINT('Ctrl Pts',(-6.17209644062764,-2.78022941324602,
47.4375832619872));
#195415=CARTESIAN_POINT('Ctrl Pts',(-6.09413637121529,-2.9417326338454,
47.4460335307106));
#195416=CARTESIAN_POINT('Ctrl Pts',(-6.01624510420906,-3.10309332237344,
47.4544763417851));
#195417=CARTESIAN_POINT('Ctrl Pts',(-5.93188473095685,-3.26147542783308,
47.4629191528596));
#195418=CARTESIAN_POINT('Ctrl Pts',(-5.84130680522698,-3.4163465584172,
47.4713619639341));
#195419=CARTESIAN_POINT('Ctrl Pts',(-5.75079648517205,-3.57110209607701,
47.4797984734518));
#195420=CARTESIAN_POINT('Ctrl Pts',(-5.65407803039699,-3.72235159744624,
47.4882349829696));
#195421=CARTESIAN_POINT('Ctrl Pts',(-5.55144927382354,-3.86958653607387,
47.4966714924873));
#195422=CARTESIAN_POINT('Ctrl Pts',(-5.44889395364787,-4.01671612018018,
47.5051019652286));
#195423=CARTESIAN_POINT('Ctrl Pts',(-5.34043695652181,-4.15983660011802,
47.5135324379698));
#195424=CARTESIAN_POINT('Ctrl Pts',(-5.22641994845009,-4.29846757838685,
47.521962910711));
#195425=CARTESIAN_POINT('Ctrl Pts',(-5.11245195598136,-4.43703895957357,
47.5303897592148));
#195426=CARTESIAN_POINT('Ctrl Pts',(-4.99292892781845,-4.57112443103792,
47.5388166077186));
#195427=CARTESIAN_POINT('Ctrl Pts',(-4.86823380156747,-4.70027538057888,
47.5472434562224));
#195428=CARTESIAN_POINT('Ctrl Pts',(-4.74357716424851,-4.82938646583431,
47.5556677036591));
#195429=CARTESIAN_POINT('Ctrl Pts',(-4.61375184256928,-4.95356582834526,
47.5640919510957));
#195430=CARTESIAN_POINT('Ctrl Pts',(-4.47917898666345,-5.07240028048188,
47.5725161985324));
#195431=CARTESIAN_POINT('Ctrl Pts',(-4.44126150470596,-5.1058832824178,
47.5748898291433));
#195432=CARTESIAN_POINT('Ctrl Pts',(-4.40296734103366,-5.1389421792453,
47.5772634597543));
#195433=CARTESIAN_POINT('Ctrl Pts',(-4.36430643069116,-5.17156827074997,
47.5796370903653));
#195434=CARTESIAN_POINT('Ctrl Pts',(-4.22392657734108,-5.29003537098732,
47.5882558713025));
#195435=CARTESIAN_POINT('Ctrl Pts',(-4.07877158475177,-5.40274008166171,
47.5968746522398));
#195436=CARTESIAN_POINT('Ctrl Pts',(-3.92933878703287,-5.5093180791019,
47.605493433177));
#195437=CARTESIAN_POINT('Ctrl Pts',(-3.77981622594112,-5.61596009729702,
47.6141173913635));
#195438=CARTESIAN_POINT('Ctrl Pts',(-3.62601097911667,-5.71646788091598,
47.62274134955));
#195439=CARTESIAN_POINT('Ctrl Pts',(-3.46844912035301,-5.81052060486171,
47.6313653077365));
#195440=CARTESIAN_POINT('Ctrl Pts',(-3.3051950892284,-5.90797113281861,
47.6403008201077));
#195441=CARTESIAN_POINT('Ctrl Pts',(-3.13790827172861,-5.99849132695656,
47.6492363324788));
#195442=CARTESIAN_POINT('Ctrl Pts',(-2.96720075482661,-6.08177677003657,
47.6581718448499));
#195443=CARTESIAN_POINT('Ctrl Pts',(-2.80213725708672,-6.16230858723531,
47.6668119267446));
#195444=CARTESIAN_POINT('Ctrl Pts',(-2.63387593106464,-6.23607631465909,
47.6754520086393));
#195445=CARTESIAN_POINT('Ctrl Pts',(-2.46299011618518,-6.30285401128521,
47.6840920905341));
#195446=CARTESIAN_POINT('Ctrl Pts',(-2.28333964866977,-6.37305670439317,
47.6931753181434));
#195447=CARTESIAN_POINT('Ctrl Pts',(-2.10078877544895,-6.43553337455878,
47.7022585457527));
#195448=CARTESIAN_POINT('Ctrl Pts',(-1.91602172126667,-6.49008087496869,
47.711341773362));
#195449=CARTESIAN_POINT('Ctrl Pts',(-1.73125466708438,-6.5446283753786,
47.7204250009714));
#195450=CARTESIAN_POINT('Ctrl Pts',(-1.54427181634025,-6.59124664487992,
47.7295082285807));
#195451=CARTESIAN_POINT('Ctrl Pts',(-1.35577026679151,-6.62979456572254,
47.73859145619));
#195452=CARTESIAN_POINT('Ctrl Pts',(-1.16807045132442,-6.66817853469319,
47.7476360510498));
#195453=CARTESIAN_POINT('Ctrl Pts',(-0.978691667858135,-6.69859696376709,
47.7566806459097));
#195454=CARTESIAN_POINT('Ctrl Pts',(-0.788294806283688,-6.72092852948059,
47.7657252407695));
#195455=CARTESIAN_POINT('Ctrl Pts',(-0.598072663799427,-6.74323960246742,
47.7747615357898));
#195456=CARTESIAN_POINT('Ctrl Pts',(-0.406834544506014,-6.75747860040878,
47.7837978308102));
#195457=CARTESIAN_POINT('Ctrl Pts',(-0.215248516264292,-6.76357576110788,
47.7928341258306));
#195458=CARTESIAN_POINT('Ctrl Pts',(-0.024001514523603,-6.76966213240298,
47.8018544304183));
#195459=CARTESIAN_POINT('Ctrl Pts',(0.167591929322728,-6.76763542907804,
47.810874735006));
#195460=CARTESIAN_POINT('Ctrl Pts',(0.358861842538853,-6.7574778710677,
47.8198950395937));
#195461=CARTESIAN_POINT('Ctrl Pts',(0.549890888454496,-6.74733310452851,
47.82890398486));
#195462=CARTESIAN_POINT('Ctrl Pts',(0.740596979969487,-6.72907792986837,
47.8379129301263));
#195463=CARTESIAN_POINT('Ctrl Pts',(0.930310789523399,-6.70274651429519,
47.8469218753927));
#195464=CARTESIAN_POINT('Ctrl Pts',(1.11959379917794,-6.67647489179246,
47.8559103632515));
#195465=CARTESIAN_POINT('Ctrl Pts',(1.30788878937756,-6.64216366811312,
47.8648988511102));
#195466=CARTESIAN_POINT('Ctrl Pts',(1.49453267626538,-6.59989856585501,
47.873887338969));
#195467=CARTESIAN_POINT('Ctrl Pts',(1.65828699930971,-6.56281675554726,
47.8817734999843));
#195468=CARTESIAN_POINT('Ctrl Pts',(1.82077028321809,-6.51961309340796,
47.8896596609996));
#195469=CARTESIAN_POINT('Ctrl Pts',(1.98153798437442,-6.47037836733536,
47.8975458220148));
#195470=CARTESIAN_POINT('Ctrl Pts',(2.14710260224417,-6.41967459692935,
47.905667286871));
#195471=CARTESIAN_POINT('Ctrl Pts',(2.31077313961764,-6.36259562220991,
47.9137887517272));
#195472=CARTESIAN_POINT('Ctrl Pts',(2.4720252008872,-6.29931586810652,47.9219102165833));
#195473=CARTESIAN_POINT('Ctrl Pts',(2.63326576251149,-6.23604062678095,
47.9300311022595));
#195474=CARTESIAN_POINT('Ctrl Pts',(2.7920878506949,-6.16656562065507,47.9381519879358));
#195475=CARTESIAN_POINT('Ctrl Pts',(2.94798577226883,-6.09111392821548,
47.946272873612));
#195476=CARTESIAN_POINT('Ctrl Pts',(3.10390232810235,-6.01565321714107,
47.9543947299662));
#195477=CARTESIAN_POINT('Ctrl Pts',(3.25689369226613,-5.93421455785329,
47.9625165863205));
#195478=CARTESIAN_POINT('Ctrl Pts',(3.40647760320885,-5.84706758459627,
47.9706384426747));
#195479=CARTESIAN_POINT('Ctrl Pts',(3.55617064872238,-5.75985702998573,
47.9787662246349));
#195480=CARTESIAN_POINT('Ctrl Pts',(3.70245095899338,-5.66693002786138,
47.9868940065951));
#195481=CARTESIAN_POINT('Ctrl Pts',(3.84486362907688,-5.56860060282669,
47.9950217885552));
#195482=CARTESIAN_POINT('Ctrl Pts',(3.98733431278901,-5.47023112203893,
48.0031528814717));
#195483=CARTESIAN_POINT('Ctrl Pts',(4.12593392291485,-5.3664550509581,48.0112839743882));
#195484=CARTESIAN_POINT('Ctrl Pts',(4.26023985246192,-5.25762735456739,
48.0194150673046));
#195485=CARTESIAN_POINT('Ctrl Pts',(4.39469237131809,-5.14868087729426,
48.0275550349692));
#195486=CARTESIAN_POINT('Ctrl Pts',(4.52484157423164,-5.03467200313603,
48.0356950026337));
#195487=CARTESIAN_POINT('Ctrl Pts',(4.65030044578834,-4.91599377175162,
48.0438349702983));
#195488=CARTESIAN_POINT('Ctrl Pts',(4.71536884107114,-4.85444210963824,
48.0480567094787));
#195489=CARTESIAN_POINT('Ctrl Pts',(4.77917621034294,-4.79163501402767,
48.0522784486592));
#195490=CARTESIAN_POINT('Ctrl Pts',(4.84167280400669,-4.72763085053624,
48.0565001878396));
#195491=CARTESIAN_POINT('Ctrl Pts',(4.96661760006426,-4.59967208213843,
48.0649403972972));
#195492=CARTESIAN_POINT('Ctrl Pts',(5.08657922504885,-4.4666622832349,48.0733806067548));
#195493=CARTESIAN_POINT('Ctrl Pts',(5.20114384654871,-4.32901740438965,
48.0818208162125));
#195494=CARTESIAN_POINT('Ctrl Pts',(5.31562166837496,-4.19147681193231,
48.090254630961));
#195495=CARTESIAN_POINT('Ctrl Pts',(5.4247104253514,-4.04930839538647,48.0986884457095));
#195496=CARTESIAN_POINT('Ctrl Pts',(5.52803444804585,-3.90296350754378,
48.107122260458));
#195497=CARTESIAN_POINT('Ctrl Pts',(5.63129607116677,-3.75670700048953,
48.1155509818466));
#195498=CARTESIAN_POINT('Ctrl Pts',(5.7287997089068,-3.60627932236902,48.1239797032351));
#195499=CARTESIAN_POINT('Ctrl Pts',(5.82021092691212,-3.45216363549771,
48.1324084246236));
#195500=CARTESIAN_POINT('Ctrl Pts',(5.91158097665924,-3.29811735667639,
48.1408333500254));
#195501=CARTESIAN_POINT('Ctrl Pts',(5.9968639076614,-3.14038666718715,48.1492582754271));
#195502=CARTESIAN_POINT('Ctrl Pts',(6.07576924908423,-2.97948267856729,
48.1576832008288));
#195503=CARTESIAN_POINT('Ctrl Pts',(6.15465116085465,-2.81862646775885,
48.1661056245865));
#195504=CARTESIAN_POINT('Ctrl Pts',(6.22715911286567,-2.65459913599151,
48.1745280483442));
#195505=CARTESIAN_POINT('Ctrl Pts',(6.29304895945054,-2.48793564907907,
48.182950472102));
#195506=CARTESIAN_POINT('Ctrl Pts',(6.35893984229296,-2.32126954102991,
48.1913730283201));
#195507=CARTESIAN_POINT('Ctrl Pts',(6.41821228298509,-2.15196750260328,
48.1997955845383));
#195508=CARTESIAN_POINT('Ctrl Pts',(6.47067034617133,-1.98058432569255,
48.2082181407565));
#195509=CARTESIAN_POINT('Ctrl Pts',(6.5231301814009,-1.80919535942558,48.2166409814903));
#195510=CARTESIAN_POINT('Ctrl Pts',(6.56877508235097,-1.63572543342071,
48.225063822224));
#195511=CARTESIAN_POINT('Ctrl Pts',(6.60745900709423,-1.46074449154169,
48.2334866629578));
#195512=CARTESIAN_POINT('Ctrl Pts',(6.64614963929158,-1.28573320949829,
48.2419109641384));
#195513=CARTESIAN_POINT('Ctrl Pts',(6.67787681693145,-1.10921071493016,
48.250335265319));
#195514=CARTESIAN_POINT('Ctrl Pts',(6.702545559052,-0.931757494647768,48.2587595664996));
#195515=CARTESIAN_POINT('Ctrl Pts',(6.72722202360128,-0.754248723505163,
48.2671865048664));
#195516=CARTESIAN_POINT('Ctrl Pts',(6.74483560136085,-0.575808976013488,
48.2756134432332));
#195517=CARTESIAN_POINT('Ctrl Pts',(6.75534310595481,-0.397024584665557,
48.2840403816));
#195518=CARTESIAN_POINT('Ctrl Pts',(6.76586005811618,-0.218079443676738,
48.2924748968437));
#195519=CARTESIAN_POINT('Ctrl Pts',(6.76925815078355,-0.0387893729546224,
48.3009094120873));
#195520=CARTESIAN_POINT('Ctrl Pts',(6.76554630902837,0.140257407621158,
48.3093439273309));
#195521=CARTESIAN_POINT('Ctrl Pts',(6.76183267442182,0.319390669325824,
48.3177825165177));
#195522=CARTESIAN_POINT('Ctrl Pts',(6.75100227138573,0.498280073453796,
48.3262211057045));
#195523=CARTESIAN_POINT('Ctrl Pts',(6.7331160330511,0.676341249274491,48.3346596948913));
#195524=CARTESIAN_POINT('Ctrl Pts',(6.71520980194868,0.854601457204353,
48.3431077165115));
#195525=CARTESIAN_POINT('Ctrl Pts',(6.69023201777036,1.03203125595538,48.3515557381318));
#195526=CARTESIAN_POINT('Ctrl Pts',(6.65829516914972,1.20805398905742,48.3600037597521));
#195527=CARTESIAN_POINT('Ctrl Pts',(6.640142776927,1.30810248568076,48.3648054796644));
#195528=CARTESIAN_POINT('Ctrl Pts',(6.61974311859267,1.40769661893139,48.3696071995767));
#195529=CARTESIAN_POINT('Ctrl Pts',(6.59712408284742,1.50673250297279,48.374408919489));
#195530=CARTESIAN_POINT('Ctrl Pts',(6.5583108515756,1.67667355239676,48.3826484513398));
#195531=CARTESIAN_POINT('Ctrl Pts',(6.51287316133395,1.84534936240476,48.3908879831907));
#195532=CARTESIAN_POINT('Ctrl Pts',(6.46090637475389,2.01220720023176,48.3991275150415));
#195533=CARTESIAN_POINT('Ctrl Pts',(6.40899726767496,2.17887983752052,48.4073579015879));
#195534=CARTESIAN_POINT('Ctrl Pts',(6.35057359883229,2.34373818363682,48.4155882881342));
#195535=CARTESIAN_POINT('Ctrl Pts',(6.28578172588067,2.50623963231464,48.4238186746805));
#195536=CARTESIAN_POINT('Ctrl Pts',(6.22105020910515,2.66858970450639,48.4320413942983));
#195537=CARTESIAN_POINT('Ctrl Pts',(6.14996243340196,2.82858692306636,48.4402641139162));
#195538=CARTESIAN_POINT('Ctrl Pts',(6.07271458158104,2.98570370443101,48.448486833534));
#195539=CARTESIAN_POINT('Ctrl Pts',(5.99553517692233,3.14268126900754,48.4567022672298));
#195540=CARTESIAN_POINT('Ctrl Pts',(5.91220673142729,3.29678316513945,48.4649177009256));
#195541=CARTESIAN_POINT('Ctrl Pts',(5.82297350223552,3.44750179003042,48.4731331346213));
#195542=CARTESIAN_POINT('Ctrl Pts',(5.73378613199442,3.59814295725181,48.4813443462222));
#195543=CARTESIAN_POINT('Ctrl Pts',(5.63870020260684,3.74540401057651,48.489555557823));
#195544=CARTESIAN_POINT('Ctrl Pts',(5.53800606247838,3.88880159585864,48.4977667694238));
#195545=CARTESIAN_POINT('Ctrl Pts',(5.43734568960834,4.03215109350317,48.5059752274374));
#195546=CARTESIAN_POINT('Ctrl Pts',(5.33108105679396,4.1716394130846,48.5141836854509));
#195547=CARTESIAN_POINT('Ctrl Pts',(5.21954606773301,4.30681179607525,48.5223921434645));
#195548=CARTESIAN_POINT('Ctrl Pts',(5.16985479465303,4.36703404429181,48.5260491907476));
#195549=CARTESIAN_POINT('Ctrl Pts',(5.11911797420273,4.42640002356778,48.5297062380307));
#195550=CARTESIAN_POINT('Ctrl Pts',(5.06736777603006,4.48487155027345,48.5333632853138));
#195551=CARTESIAN_POINT('Ctrl Pts',(4.94206285740536,4.62645110270861,48.5422182468095));
#195552=CARTESIAN_POINT('Ctrl Pts',(4.81094435462351,4.76263729323991,48.5510732083052));
#195553=CARTESIAN_POINT('Ctrl Pts',(4.67449614862399,4.89299241328857,48.559928169801));
#195554=CARTESIAN_POINT('Ctrl Pts',(4.53765432310214,5.02372357580485,48.5688086756832));
#195555=CARTESIAN_POINT('Ctrl Pts',(4.39545221729934,5.14858982823487,48.5776891815655));
#195556=CARTESIAN_POINT('Ctrl Pts',(4.24840844994112,5.26719229214853,48.5865696874478));
#195557=CARTESIAN_POINT('Ctrl Pts',(4.10114695216991,5.38597037291365,48.5954633428586));
#195558=CARTESIAN_POINT('Ctrl Pts',(3.94902967639376,5.49846597893295,48.6043569982693));
#195559=CARTESIAN_POINT('Ctrl Pts',(3.7926047418606,5.60432317697833,48.6132506536801));
#195560=CARTESIAN_POINT('Ctrl Pts',(3.63584600571122,5.71040626806245,48.6221632876288));
#195561=CARTESIAN_POINT('Ctrl Pts',(3.47476144378922,5.80982247761136,48.6310759215775));
#195562=CARTESIAN_POINT('Ctrl Pts',(3.30992645411757,5.90226023387081,48.6399885555262));
#195563=CARTESIAN_POINT('Ctrl Pts',(3.24030697252026,5.94130211862853,48.6437528834545));
#195564=CARTESIAN_POINT('Ctrl Pts',(3.17001873308238,5.97909971782621,48.6475172113827));
#195565=CARTESIAN_POINT('Ctrl Pts',(3.09910619832125,6.01563211736945,48.651281539311));
#195566=CARTESIAN_POINT('Origin',(0.,0.,4.30282021618968));
#195567=CARTESIAN_POINT('',(3.0991061983214,6.01563211736937,51.0457552630242));
#195568=CARTESIAN_POINT('',(3.0991061983213,6.01563211736942,50.6516279712835));
#195569=CARTESIAN_POINT('',(3.09910619832133,6.0156321173694,4.30282021618968));
#195570=CARTESIAN_POINT('',(-6.767,4.15111738386043E-13,49.6971797838101));
#195571=CARTESIAN_POINT('Ctrl Pts',(-6.767,4.15112265940911E-13,49.6971797838101));
#195572=CARTESIAN_POINT('Ctrl Pts',(-6.76700000000001,-0.186007249526577,
49.7059292956213));
#195573=CARTESIAN_POINT('Ctrl Pts',(-6.75932637294521,-0.372014355749744,
49.7146788074325));
#195574=CARTESIAN_POINT('Ctrl Pts',(-6.74400518264181,-0.557389537487439,
49.7234283192437));
#195575=CARTESIAN_POINT('Ctrl Pts',(-6.72868405705085,-0.742763936251934,
49.7321777940993));
#195576=CARTESIAN_POINT('Ctrl Pts',(-6.70571545645721,-0.927506130242599,
49.740927268955));
#195577=CARTESIAN_POINT('Ctrl Pts',(-6.67517739404792,-1.11098863990213,
49.7496767438107));
#195578=CARTESIAN_POINT('Ctrl Pts',(-6.6446394580866,-1.29447038982159,
49.7584261824377));
#195579=CARTESIAN_POINT('Ctrl Pts',(-6.60653217008304,-1.47669218313911,
49.7671756210647));
#195580=CARTESIAN_POINT('Ctrl Pts',(-6.56098496092616,-1.65703510599528,
49.7759250596918));
#195581=CARTESIAN_POINT('Ctrl Pts',(-6.51543793658228,-1.83737729708945,
49.7846744628169));
#195582=CARTESIAN_POINT('Ctrl Pts',(-6.46245112167343,-2.01584035511174,
49.7934238659421));
#195583=CARTESIAN_POINT('Ctrl Pts',(-6.40220448374168,-2.1918181376104,
49.8021732690673));
#195584=CARTESIAN_POINT('Ctrl Pts',(-6.34195808526413,-2.36779522067386,
49.8109226374174));
#195585=CARTESIAN_POINT('Ctrl Pts',(-6.27445201433008,-2.54128677684402,
49.8196720057675));
#195586=CARTESIAN_POINT('Ctrl Pts',(-6.19991555071801,-2.71170355385042,
49.8284213741176));
#195587=CARTESIAN_POINT('Ctrl Pts',(-6.12537937716591,-2.88211966767692,
49.8371707084193));
#195588=CARTESIAN_POINT('Ctrl Pts',(-6.04381298052419,-3.04946076371985,
49.8459200427211));
#195589=CARTESIAN_POINT('Ctrl Pts',(-5.95549339335732,-3.21315848374731,
49.8546693770229));
#195590=CARTESIAN_POINT('Ctrl Pts',(-5.86717414255319,-3.37685558033647,
49.8634186780031));
#195591=CARTESIAN_POINT('Ctrl Pts',(-5.7721018887652,-3.53690907646883,
49.8721679789832));
#195592=CARTESIAN_POINT('Ctrl Pts',(-5.67059953346931,-3.69277536969386,
49.8809172799634));
#195593=CARTESIAN_POINT('Ctrl Pts',(-5.56909755631316,-3.84864108225021,
49.8896665483487));
#195594=CARTESIAN_POINT('Ctrl Pts',(-5.4611656819678,-4.00031938297612,
49.898415816734));
#195595=CARTESIAN_POINT('Ctrl Pts',(-5.34717048533531,-4.14729511859947,
49.9071650851192));
#195596=CARTESIAN_POINT('Ctrl Pts',(-5.23317570391759,-4.29427031888012,
49.9159143216363));
#195597=CARTESIAN_POINT('Ctrl Pts',(-5.1131178200343,-4.43654276189644,
49.9246635581533));
#195598=CARTESIAN_POINT('Ctrl Pts',(-4.98740458984663,-4.57362924351951,
49.9334127946704));
#195599=CARTESIAN_POINT('Ctrl Pts',(-4.86169180711654,-4.71071523720358,
49.9421620000458));
#195600=CARTESIAN_POINT('Ctrl Pts',(-4.73032391204085,-4.84261509523323,
49.9509112054212));
#195601=CARTESIAN_POINT('Ctrl Pts',(-4.59374707013515,-4.96888084538408,
49.9596604107967));
#195602=CARTESIAN_POINT('Ctrl Pts',(-4.45717070301353,-5.09514615659545,
49.9684095857571));
#195603=CARTESIAN_POINT('Ctrl Pts',(-4.31538563570941,-5.21577720459611,
49.9771587607176));
#195604=CARTESIAN_POINT('Ctrl Pts',(-4.16887341029401,-5.33036429232971,
49.985907935678));
#195605=CARTESIAN_POINT('Ctrl Pts',(-4.02236168203572,-5.44495099123716,
49.9946570809501));
#195606=CARTESIAN_POINT('Ctrl Pts',(-3.87112305348004,-5.55349359438715,
50.0034062262221));
#195607=CARTESIAN_POINT('Ctrl Pts',(-3.7156711701757,-5.65562346299019,
50.0121553714941));
#195608=CARTESIAN_POINT('Ctrl Pts',(-3.56021980145608,-5.75775299351775,
50.0209044878043));
#195609=CARTESIAN_POINT('Ctrl Pts',(-3.40055544538117,-5.85346967464008,
50.0296536041145));
#195610=CARTESIAN_POINT('Ctrl Pts',(-3.23722035986599,-5.94244842987039,
50.0384027204247));
#195611=CARTESIAN_POINT('Ctrl Pts',(-3.07388580146917,-6.03142689794664,
50.0471518084995));
#195612=CARTESIAN_POINT('Ctrl Pts',(-2.90688078896305,-6.11366734656912,
50.0559008965744));
#195613=CARTESIAN_POINT('Ctrl Pts',(-2.73677250721087,-6.18889046952479,
50.0646499846492));
#195614=CARTESIAN_POINT('Ctrl Pts',(-2.56666476031186,-6.26411335596449,
50.0733990452152));
#195615=CARTESIAN_POINT('Ctrl Pts',(-2.39345402574855,-6.33231884500673,
50.0821481057813));
#195616=CARTESIAN_POINT('Ctrl Pts',(-2.21772856065267,-6.39327529762839,
50.0908971663473));
#195617=CARTESIAN_POINT('Ctrl Pts',(-2.04200363348157,-6.45423156365225,
50.099646200131));
#195618=CARTESIAN_POINT('Ctrl Pts',(-1.8637642618889,-6.5079387437577,50.1083952339147));
#195619=CARTESIAN_POINT('Ctrl Pts',(-1.68361577752734,-6.5542144390965,
50.1171442676984));
#195620=CARTESIAN_POINT('Ctrl Pts',(-1.50346782967389,-6.60048999661961,
50.1258932754263));
#195621=CARTESIAN_POINT('Ctrl Pts',(-1.32141105794587,-6.63933404237792,
50.1346422831541));
#195622=CARTESIAN_POINT('Ctrl Pts',(-1.13806375486633,-6.67061465607627,
50.1433912908819));
#195623=CARTESIAN_POINT('Ctrl Pts',(-0.954716982599113,-6.70189517921352,
50.1521402732803));
#195624=CARTESIAN_POINT('Ctrl Pts',(-0.770079968898227,-6.72561226592273,
50.1608892556787));
#195625=CARTESIAN_POINT('Ctrl Pts',(-0.58477976555433,-6.74168536983136,
50.1696382380771));
#195626=CARTESIAN_POINT('Ctrl Pts',(-0.391489830647433,-6.75845151013875,
50.178764457087));
#195627=CARTESIAN_POINT('Ctrl Pts',(-0.197478578234526,-6.76689983031636,
50.1878906760968));
#195628=CARTESIAN_POINT('Ctrl Pts',(-0.00346287644759543,-6.76699911397118,
50.1970168951067));
#195629=CARTESIAN_POINT('Ctrl Pts',(0.184489834658524,-6.76709529501178,
50.2058579197725));
#195630=CARTESIAN_POINT('Ctrl Pts',(0.372446404253995,-6.75935639738143,
50.2146989444383));
#195631=CARTESIAN_POINT('Ctrl Pts',(0.559755019492944,-6.74380925873148,
50.2235399691041));
#195632=CARTESIAN_POINT('Ctrl Pts',(0.745134705526356,-6.72842222659755,
50.2322899477139));
#195633=CARTESIAN_POINT('Ctrl Pts',(0.929879431233118,-6.7053870605746,
50.2410399263236));
#195634=CARTESIAN_POINT('Ctrl Pts',(1.11336163627277,-6.67478200894052,
50.2497899049334));
#195635=CARTESIAN_POINT('Ctrl Pts',(1.29684196301187,-6.64417727060922,
50.2585397939699));
#195636=CARTESIAN_POINT('Ctrl Pts',(1.47905951217995,-6.60600284890482,
50.2672896830064));
#195637=CARTESIAN_POINT('Ctrl Pts',(1.65939532067585,-6.56038841607104,
50.276039572043));
#195638=CARTESIAN_POINT('Ctrl Pts',(1.83972934301301,-6.51477443503116,
50.2847893744151));
#195639=CARTESIAN_POINT('Ctrl Pts',(2.01818138406762,-6.46172066061986,
50.2935391767873));
#195640=CARTESIAN_POINT('Ctrl Pts',(2.19414528354694,-6.40140730423309,
50.3022889791594));
#195641=CARTESIAN_POINT('Ctrl Pts',(2.37010749864485,-6.3410945251846,50.3110386977758));
#195642=CARTESIAN_POINT('Ctrl Pts',(2.54358134866937,-6.2735223961631,50.3197884163921));
#195643=CARTESIAN_POINT('Ctrl Pts',(2.71397759436023,-6.19892043966614,
50.3285381350084));
#195644=CARTESIAN_POINT('Ctrl Pts',(2.88437226558593,-6.12431917249294,
50.3372877727771));
#195645=CARTESIAN_POINT('Ctrl Pts',(3.05168912681427,-6.04268832278561,
50.3460374105458));
#195646=CARTESIAN_POINT('Ctrl Pts',(3.21535986274326,-5.95430516123079,
50.3547870483145));
#195647=CARTESIAN_POINT('Ctrl Pts',(3.37902914073314,-5.86592278697169,
50.3635366081436));
#195648=CARTESIAN_POINT('Ctrl Pts',(3.53905210622044,-5.77078835741652,
50.3722861679727));
#195649=CARTESIAN_POINT('Ctrl Pts',(3.69488522832168,-5.66922500431322,
50.3810357278018));
#195650=CARTESIAN_POINT('Ctrl Pts',(3.85071701407415,-5.56766252216765,
50.3897852125989));
#195651=CARTESIAN_POINT('Ctrl Pts',(4.00235878822881,-5.45967138329021,
50.398534697396));
#195652=CARTESIAN_POINT('Ctrl Pts',(4.14929549611804,-5.34561838199236,
50.4072841821931));
#195653=CARTESIAN_POINT('Ctrl Pts',(4.29623099276555,-5.23156632086633,
50.4160335948657));
#195654=CARTESIAN_POINT('Ctrl Pts',(4.4384612743648,-5.11145267304571,50.4247830075383));
#195655=CARTESIAN_POINT('Ctrl Pts',(4.57550326054881,-4.98568540049482,
50.4335324202109));
#195656=CARTESIAN_POINT('Ctrl Pts',(4.71254416258202,-4.85991912289951,
50.4422817636661));
#195657=CARTESIAN_POINT('Ctrl Pts',(4.84439664019166,-4.72849950385004,
50.4510311071214));
#195658=CARTESIAN_POINT('Ctrl Pts',(4.97061286795133,-4.59187289860648,
50.4597804505766));
#195659=CARTESIAN_POINT('Ctrl Pts',(5.09682813913056,-4.45524732884259,
50.4685297277214));
#195660=CARTESIAN_POINT('Ctrl Pts',(5.21740705148195,-4.31341506235357,
50.4772790048663));
#195661=CARTESIAN_POINT('Ctrl Pts',(5.33194007546036,-4.16685781275289,
50.4860282820111));
#195662=CARTESIAN_POINT('Ctrl Pts',(5.4464722694481,-4.02030162521402,50.4947774957522));
#195663=CARTESIAN_POINT('Ctrl Pts',(5.55495848628422,-3.86902074887491,
50.5035267094933));
#195664=CARTESIAN_POINT('Ctrl Pts',(5.65703027292081,-3.71352898080216,
50.5122759232344));
#195665=CARTESIAN_POINT('Ctrl Pts',(5.75910135377274,-3.55803828789139,
50.5210250764783));
#195666=CARTESIAN_POINT('Ctrl Pts',(5.85475793593014,-3.39833700106261,
50.5297742297222));
#195667=CARTESIAN_POINT('Ctrl Pts',(5.94367514427645,-3.23496750823101,
50.5385233829661));
#195668=CARTESIAN_POINT('Ctrl Pts',(6.03259176732873,-3.07159909077266,
50.547272478619));
#195669=CARTESIAN_POINT('Ctrl Pts',(6.11476896836145,-2.9045627673097,50.5560215742719));
#195670=CARTESIAN_POINT('Ctrl Pts',(6.18992765548094,-2.7344258300258,50.5647706699249));
#195671=CARTESIAN_POINT('Ctrl Pts',(6.26508587283255,-2.5642899561568,50.5735197108929));
#195672=CARTESIAN_POINT('Ctrl Pts',(6.33322554827353,-2.39105376934691,
50.5822687518609));
#195673=CARTESIAN_POINT('Ctrl Pts',(6.39411526733215,-2.21530561053548,
50.591017792829));
#195674=CARTESIAN_POINT('Ctrl Pts',(6.45500462603017,-2.03955849184561,
50.599766782018));
#195675=CARTESIAN_POINT('Ctrl Pts',(6.50864402040895,-1.86129970164003,
50.608515771207));
#195676=CARTESIAN_POINT('Ctrl Pts',(6.55485128368741,-1.68113463135513,
50.6172647603961));
#195677=CARTESIAN_POINT('Ctrl Pts',(6.60199809554445,-1.49730620116344,
50.6261916458675));
#195678=CARTESIAN_POINT('Ctrl Pts',(6.64140720707972,-1.31149343245196,
50.6351185313389));
#195679=CARTESIAN_POINT('Ctrl Pts',(6.67293928722964,-1.12435326697046,
50.6440454168103));
#195680=CARTESIAN_POINT('Ctrl Pts',(6.70384625876323,-0.940923067001829,
50.6527953309878));
#195681=CARTESIAN_POINT('Ctrl Pts',(6.72718554579849,-0.756217899516949,
50.6615452451653));
#195682=CARTESIAN_POINT('Ctrl Pts',(6.74287786815367,-0.57086518124983,
50.6702951593427));
#195683=CARTESIAN_POINT('Ctrl Pts',(6.75856988190872,-0.385516108069375,
50.6790449014472));
#195684=CARTESIAN_POINT('Ctrl Pts',(6.76661520773416,-0.199519795221876,
50.6877946435517));
#195685=CARTESIAN_POINT('Ctrl Pts',(6.7669865178958,-0.0135080204512824,
50.6965443856562));
#195686=CARTESIAN_POINT('Ctrl Pts',(6.76735782124892,0.172500343517284,
50.7052939673211));
#195687=CARTESIAN_POINT('Ctrl Pts',(6.76005538995161,0.358523882215196,
50.7140435489861));
#195688=CARTESIAN_POINT('Ctrl Pts',(6.74510402742327,0.5439307485686,50.7227931306511));
#195689=CARTESIAN_POINT('Ctrl Pts',(6.73015291917986,0.729334461619347,
50.7315425635077));
#195690=CARTESIAN_POINT('Ctrl Pts',(6.7075531630654,0.914121237638676,50.7402919963644));
#195691=CARTESIAN_POINT('Ctrl Pts',(6.6773815187451,1.09766345166509,50.7490414292211));
#195692=CARTESIAN_POINT('Ctrl Pts',(6.64721034747495,1.28120278800047,50.7577907248986));
#195693=CARTESIAN_POINT('Ctrl Pts',(6.60946757205058,1.46349731860706,50.7665400205762));
#195694=CARTESIAN_POINT('Ctrl Pts',(6.5642813811143,1.64392790278533,50.7752893162537));
#195695=CARTESIAN_POINT('Ctrl Pts',(6.51909583859747,1.82435589779423,50.7840384863793));
#195696=CARTESIAN_POINT('Ctrl Pts',(6.46646716392763,2.00291972192628,50.7927876565049));
#195697=CARTESIAN_POINT('Ctrl Pts',(6.40657409872762,2.17901292275022,50.8015368266305));
#195698=CARTESIAN_POINT('Ctrl Pts',(6.34668181341944,2.35510383059333,50.8102858828296));
#195699=CARTESIAN_POINT('Ctrl Pts',(6.27952541913908,2.52872390822933,50.8190349390287));
#195700=CARTESIAN_POINT('Ctrl Pts',(6.20533299175365,2.69928350890634,50.8277839952278));
#195701=CARTESIAN_POINT('Ctrl Pts',(6.12831602991392,2.87633637965956,50.836866131386));
#195702=CARTESIAN_POINT('Ctrl Pts',(6.0437169060511,3.05009086601779,50.8459482675442));
#195703=CARTESIAN_POINT('Ctrl Pts',(5.95184520316468,3.21991112883036,50.8550304037024));
#195704=CARTESIAN_POINT('Ctrl Pts',(5.863335495091,3.38351691183319,50.8637801840459));
#195705=CARTESIAN_POINT('Ctrl Pts',(5.76807618099183,3.54347103712307,50.8725299643895));
#195706=CARTESIAN_POINT('Ctrl Pts',(5.66639083308818,3.69923018027997,50.8812797447331));
#195707=CARTESIAN_POINT('Ctrl Pts',(5.5647091408199,3.85498372382354,50.890029210518));
#195708=CARTESIAN_POINT('Ctrl Pts',(5.45660203371843,4.00654234702303,50.8987786763029));
#195709=CARTESIAN_POINT('Ctrl Pts',(5.34243669838979,4.15339127986974,50.9075281420878));
#195710=CARTESIAN_POINT('Ctrl Pts',(5.22827486050342,4.30023571401583,50.9162773398338));
#195711=CARTESIAN_POINT('Ctrl Pts',(5.1080553416685,4.4423705202877,50.9250265375798));
#195712=CARTESIAN_POINT('Ctrl Pts',(4.98218644339678,4.57931296629018,50.9337757353259));
#195713=CARTESIAN_POINT('Ctrl Pts',(4.85632073219318,4.71625194483636,50.9425247115375));
#195714=CARTESIAN_POINT('Ctrl Pts',(4.72480612170057,4.84799861524763,50.9512736877491));
#195715=CARTESIAN_POINT('Ctrl Pts',(4.58808925235057,4.9741055489872,50.9600226639607));
#195716=CARTESIAN_POINT('Ctrl Pts',(4.45136349473788,5.10022068121433,50.9687722089624));
#195717=CARTESIAN_POINT('Ctrl Pts',(4.30943501209815,5.22069514872053,50.9775217539641));
#195718=CARTESIAN_POINT('Ctrl Pts',(4.16278587431512,5.33511975166467,50.9862712989658));
#195719=CARTESIAN_POINT('Ctrl Pts',(4.01614535740155,5.44953762808059,50.9950203296196));
#195720=CARTESIAN_POINT('Ctrl Pts',(3.86478496657606,5.55790617533005,51.0037693602733));
#195721=CARTESIAN_POINT('Ctrl Pts',(3.70921874746854,5.6598573553958,51.0125183909271));
#195722=CARTESIAN_POINT('Ctrl Pts',(3.5536504160555,5.76180991977263,51.0212675403767));
#195723=CARTESIAN_POINT('Ctrl Pts',(3.39387638174163,5.85734478553022,51.0300166898263));
#195724=CARTESIAN_POINT('Ctrl Pts',(3.2304392790417,5.94613749121432,51.0387658392759));
#195725=CARTESIAN_POINT('Ctrl Pts',(3.18691767070183,5.96978206944278,51.041095647192));
#195726=CARTESIAN_POINT('Ctrl Pts',(3.14313645919507,5.99294880633489,51.0434254551081));
#195727=CARTESIAN_POINT('Ctrl Pts',(3.0991061983214,6.01563211736937,51.0457552630242));
#195728=CARTESIAN_POINT('Ctrl Pts',(3.09910619832136,6.01563211736939,49.0458451349191));
#195729=CARTESIAN_POINT('Ctrl Pts',(2.93972393993817,6.09774194975618,49.0542783857431));
#195730=CARTESIAN_POINT('Ctrl Pts',(2.77698811596646,6.17355927733608,49.0627116365671));
#195731=CARTESIAN_POINT('Ctrl Pts',(2.61142360477587,6.2428163321068,49.071144887391));
#195732=CARTESIAN_POINT('Ctrl Pts',(2.44594307296802,6.31203825758159,49.0795738606123));
#195733=CARTESIAN_POINT('Ctrl Pts',(2.27763701902433,6.37470641533421,49.0880028338337));
#195734=CARTESIAN_POINT('Ctrl Pts',(2.10705228741077,6.43060025643929,49.096431807055));
#195735=CARTESIAN_POINT('Ctrl Pts',(1.93652970878945,6.48647373247746,49.1048577091579));
#195736=CARTESIAN_POINT('Ctrl Pts',(1.76373042213216,6.53557770896233,49.1132836112607));
#195737=CARTESIAN_POINT('Ctrl Pts',(1.58921888533647,6.57774067096674,49.1217095133636));
#195738=CARTESIAN_POINT('Ctrl Pts',(1.43181293445047,6.61577082787403,49.1293095102288));
#195739=CARTESIAN_POINT('Ctrl Pts',(1.27301434684598,6.64815456842155,49.1369095070939));
#195740=CARTESIAN_POINT('Ctrl Pts',(1.11324685211149,6.67480115406174,49.1445095039591));
#195741=CARTESIAN_POINT('Ctrl Pts',(0.932062430270227,6.70501973025763,
49.1531282848963));
#195742=CARTESIAN_POINT('Ctrl Pts',(0.74971304937296,6.72784574542047,49.1617470658335));
#195743=CARTESIAN_POINT('Ctrl Pts',(0.566812338184386,6.74321976308662,
49.1703658467708));
#195744=CARTESIAN_POINT('Ctrl Pts',(0.383801759648514,6.75860301583188,
49.1789898049574));
#195745=CARTESIAN_POINT('Ctrl Pts',(0.200239492989446,6.76652531212785,
49.187613763144));
#195746=CARTESIAN_POINT('Ctrl Pts',(0.0167416779525153,6.7669792903643,
49.1962377213307));
#195747=CARTESIAN_POINT('Ctrl Pts',(-0.173385287049673,6.76744966928547,
49.2051732337018));
#195748=CARTESIAN_POINT('Ctrl Pts',(-0.363442695548515,6.75990206500124,
49.2141087460728));
#195749=CARTESIAN_POINT('Ctrl Pts',(-0.552748818302166,6.74438712885504,
49.2230442584439));
#195750=CARTESIAN_POINT('Ctrl Pts',(-0.735796005282449,6.72938515545645,
49.2316843403386));
#195751=CARTESIAN_POINT('Ctrl Pts',(-0.918140493494802,6.70693434116502,
49.2403244222333));
#195752=CARTESIAN_POINT('Ctrl Pts',(-1.09917392994075,6.67713304283647,
49.248964504128));
#195753=CARTESIAN_POINT('Ctrl Pts',(-1.28949248573411,6.64580325000922,
49.2580477317373));
#195754=CARTESIAN_POINT('Ctrl Pts',(-1.47836158572741,6.60634924265721,
49.2671309593466));
#195755=CARTESIAN_POINT('Ctrl Pts',(-1.66508915912587,6.55894557777098,
49.2762141869559));
#195756=CARTESIAN_POINT('Ctrl Pts',(-1.85181673252427,6.51154191288477,
49.2852974145652));
#195757=CARTESIAN_POINT('Ctrl Pts',(-2.03640241756047,6.45618873408586,
49.2943806421744));
#195758=CARTESIAN_POINT('Ctrl Pts',(-2.21817473501047,6.39312050918495,
49.3034638697837));
#195759=CARTESIAN_POINT('Ctrl Pts',(-2.39917393912359,6.33032052582097,
49.3125084646435));
#195760=CARTESIAN_POINT('Ctrl Pts',(-2.57755109173786,6.25981381777489,
49.3215530595033));
#195761=CARTESIAN_POINT('Ctrl Pts',(-2.75267595307432,6.18183339288325,
49.3305976543631));
#195762=CARTESIAN_POINT('Ctrl Pts',(-2.92764010978414,6.10392452730633,
49.3396339493834));
#195763=CARTESIAN_POINT('Ctrl Pts',(-3.09935771662874,6.0185557342239,49.3486702444037));
#195764=CARTESIAN_POINT('Ctrl Pts',(-3.26721867963455,5.92600802391012,
49.357706539424));
#195765=CARTESIAN_POINT('Ctrl Pts',(-3.43478259950343,5.8336240840269,49.3667268440117));
#195766=CARTESIAN_POINT('Ctrl Pts',(-3.59850329539956,5.73408670920529,
49.3757471485994));
#195767=CARTESIAN_POINT('Ctrl Pts',(-3.75779556841933,5.62772258253443,
49.3847674531871));
#195768=CARTESIAN_POINT('Ctrl Pts',(-3.91688724376425,5.52149240081956,
49.3937763984534));
#195769=CARTESIAN_POINT('Ctrl Pts',(-4.07156142823421,5.40845275555742,
49.4027853437196));
#195770=CARTESIAN_POINT('Ctrl Pts',(-4.22125999304436,5.28897467106084,
49.4117942889859));
#195771=CARTESIAN_POINT('Ctrl Pts',(-4.37061862410423,5.16976789600128,
49.4207827768446));
#195772=CARTESIAN_POINT('Ctrl Pts',(-4.51502400285251,5.04415201327701,
49.4297712647034));
#195773=CARTESIAN_POINT('Ctrl Pts',(-4.65394968488556,4.91253919379313,
49.4387597525621));
#195774=CARTESIAN_POINT('Ctrl Pts',(-4.77583785060568,4.79706705849472,
49.4466459135776));
#195775=CARTESIAN_POINT('Ctrl Pts',(-4.89350826159656,4.67697938905811,
49.454532074593));
#195776=CARTESIAN_POINT('Ctrl Pts',(-5.00662498621481,4.55258116318749,
49.4624182356085));
#195777=CARTESIAN_POINT('Ctrl Pts',(-5.12311683843922,4.42447119718552,
49.4705397004647));
#195778=CARTESIAN_POINT('Ctrl Pts',(-5.23472585164597,4.2918458514551,49.4786611653208));
#195779=CARTESIAN_POINT('Ctrl Pts',(-5.34109011845018,4.15512278357618,
49.486782630177));
#195780=CARTESIAN_POINT('Ctrl Pts',(-5.44744679991717,4.01840946606368,
49.4949035158532));
#195781=CARTESIAN_POINT('Ctrl Pts',(-5.54855925514299,3.87759929750489,
49.5030244015295));
#195782=CARTESIAN_POINT('Ctrl Pts',(-5.64410649347399,3.7331422274439,49.5111452872057));
#195783=CARTESIAN_POINT('Ctrl Pts',(-5.73966515243256,3.58866789063165,
49.51926714356));
#195784=CARTESIAN_POINT('Ctrl Pts',(-5.82965706891732,3.44054609040245,
49.5273889999143));
#195785=CARTESIAN_POINT('Ctrl Pts',(-5.91380516494978,3.28925485042028,
49.5355108562687));
#195786=CARTESIAN_POINT('Ctrl Pts',(-5.9980146543913,3.1378532302225,49.5436386382288));
#195787=CARTESIAN_POINT('Ctrl Pts',(-6.07637162967551,2.98327787215715,
49.551766420189));
#195788=CARTESIAN_POINT('Ctrl Pts',(-6.14864519539981,2.82603100851474,
49.5598942021491));
#195789=CARTESIAN_POINT('Ctrl Pts',(-6.2209482026883,2.66872008834513,49.5680252950656));
#195790=CARTESIAN_POINT('Ctrl Pts',(-6.28716272081908,2.50873583148082,
49.576156387982));
#195791=CARTESIAN_POINT('Ctrl Pts',(-6.347106525167,2.3465991899305,49.5842874808984));
#195792=CARTESIAN_POINT('Ctrl Pts',(-6.4071157556725,2.18428558301114,49.5924274485629));
#195793=CARTESIAN_POINT('Ctrl Pts',(-6.46084048863694,2.0198152468596,49.6005674162275));
#195794=CARTESIAN_POINT('Ctrl Pts',(-6.50814853973555,1.85372370776716,
49.608707383892));
#195795=CARTESIAN_POINT('Ctrl Pts',(-6.53268454050372,1.76758145425806,
49.6129291230724));
#195796=CARTESIAN_POINT('Ctrl Pts',(-6.55549535098424,1.68100328982057,
49.6171508622528));
#195797=CARTESIAN_POINT('Ctrl Pts',(-6.57656798188356,1.59406479782472,
49.6213726014332));
#195798=CARTESIAN_POINT('Ctrl Pts',(-6.63298328035275,1.3613145068032,49.6326749716525));
#195799=CARTESIAN_POINT('Ctrl Pts',(-6.67701699606666,1.12565713650379,
49.6439773418719));
#195800=CARTESIAN_POINT('Ctrl Pts',(-6.70845565815198,0.888207004368171,
49.6552797120912));
#195801=CARTESIAN_POINT('Ctrl Pts',(-6.73942658159803,0.654289611679238,
49.6664139277227));
#195802=CARTESIAN_POINT('Ctrl Pts',(-6.75817455604823,0.418631866523409,
49.6775481433541));
#195803=CARTESIAN_POINT('Ctrl Pts',(-6.76454365156374,0.182313428163557,
49.6886823589856));
#195804=CARTESIAN_POINT('Ctrl Pts',(-6.7661639096982,0.1221954928707,49.6915148339271));
#195805=CARTESIAN_POINT('Ctrl Pts',(-6.76698329674138,0.0620348961955091,
49.6943473088686));
#195806=CARTESIAN_POINT('Ctrl Pts',(-6.76699974721993,0.00184962846154336,
49.6971797838101));
#195807=CARTESIAN_POINT('',(-6.76699653643252,-0.00684659844694554,49.302820216166));
#195808=CARTESIAN_POINT('Ctrl Pts',(3.09910619832125,6.01563211736945,48.651281539311));
#195809=CARTESIAN_POINT('Ctrl Pts',(2.93077649148675,6.10235145585861,48.6602171699259));
#195810=CARTESIAN_POINT('Ctrl Pts',(2.75892788574672,6.18193830383501,48.6691528005408));
#195811=CARTESIAN_POINT('Ctrl Pts',(2.58416789816994,6.25414784555562,48.6780884311557));
#195812=CARTESIAN_POINT('Ctrl Pts',(2.4914045027765,6.29247699837079,48.6828315044834));
#195813=CARTESIAN_POINT('Ctrl Pts',(2.39782110739142,6.32872840195926,48.687574577811));
#195814=CARTESIAN_POINT('Ctrl Pts',(2.30351033261469,6.36287114025872,48.6923176511387));
#195815=CARTESIAN_POINT('Ctrl Pts',(2.14001054988095,6.42206194117319,48.7005403750046));
#195816=CARTESIAN_POINT('Ctrl Pts',(1.97401030601349,6.47502553674889,48.7087630988705));
#195817=CARTESIAN_POINT('Ctrl Pts',(1.80602453028676,6.52154616605621,48.7169858227363));
#195818=CARTESIAN_POINT('Ctrl Pts',(1.63821656181282,6.56801755485339,48.7251998431276));
#195819=CARTESIAN_POINT('Ctrl Pts',(1.46842758931484,6.60805946257521,48.7334138635188));
#195820=CARTESIAN_POINT('Ctrl Pts',(1.297191299762,6.64150462860802,48.74162788391));
#195821=CARTESIAN_POINT('Ctrl Pts',(1.12610187861514,6.67492110890934,48.749834859182));
#195822=CARTESIAN_POINT('Ctrl Pts',(0.953567962756425,6.70175204751753,
48.7580418344539));
#195823=CARTESIAN_POINT('Ctrl Pts',(0.78013723004385,6.72188031002483,48.7662488097259));
#195824=CARTESIAN_POINT('Ctrl Pts',(0.60682043786161,6.74199534866536,48.7744503931789));
#195825=CARTESIAN_POINT('Ctrl Pts',(0.43260835747718,6.75541644128931,48.7826519766319));
#195826=CARTESIAN_POINT('Ctrl Pts',(0.258057753170527,6.76207772774231,
48.7908535600849));
#195827=CARTESIAN_POINT('Ctrl Pts',(0.0835867974835264,6.76873597460531,
48.7990514011));
#195828=CARTESIAN_POINT('Ctrl Pts',(-0.091222016658833,6.76864054681347,
48.807249242115));
#195829=CARTESIAN_POINT('Ctrl Pts',(-0.265807832575272,6.76177751749802,
48.8154470831301));
#195830=CARTESIAN_POINT('Ctrl Pts',(-0.440378241837691,6.75491509382351,
48.8236442007112));
#195831=CARTESIAN_POINT('Ctrl Pts',(-0.614725333558899,6.74128626371388,
48.8318413182924));
#195832=CARTESIAN_POINT('Ctrl Pts',(-0.78828891228321,6.72092922078275,
48.8400384358735));
#195833=CARTESIAN_POINT('Ctrl Pts',(-0.961850559919425,6.70057240434639,
48.8482354622526));
#195834=CARTESIAN_POINT('Ctrl Pts',(-1.13462835540743,6.67348756492386,
48.8564324886317));
#195835=CARTESIAN_POINT('Ctrl Pts',(-1.30606800359344,6.63976470742672,
48.8646295150108));
#195836=CARTESIAN_POINT('Ctrl Pts',(-1.477536917252,6.60603609329528,48.872827940657));
#195837=CARTESIAN_POINT('Ctrl Pts',(-1.64766687641729,6.56566727280108,
48.8810263663031));
#195838=CARTESIAN_POINT('Ctrl Pts',(-1.81591449286919,6.51879924177664,
48.8892247919493));
#195839=CARTESIAN_POINT('Ctrl Pts',(-1.98422142275158,6.47191468805928,
48.8974261078399));
#195840=CARTESIAN_POINT('Ctrl Pts',(-2.15064434257303,6.41852645593345,
48.9056274237306));
#195841=CARTESIAN_POINT('Ctrl Pts',(-2.31465567054109,6.35882521593667,
48.9138287396212));
#195842=CARTESIAN_POINT('Ctrl Pts',(-2.47885377995708,6.2990559862212,48.9220393954378));
#195843=CARTESIAN_POINT('Ctrl Pts',(-2.64063447316435,6.23295950824151,
48.9302500512544));
#195844=CARTESIAN_POINT('Ctrl Pts',(-2.79948980530397,6.16077477513982,
48.938460707071));
#195845=CARTESIAN_POINT('Ctrl Pts',(-2.95843874704228,6.08854750532372,
48.9466762012282));
#195846=CARTESIAN_POINT('Ctrl Pts',(-3.11445857133242,6.01022498965705,
48.9548916953853));
#195847=CARTESIAN_POINT('Ctrl Pts',(-3.26706666612296,5.92609183181532,
48.9631071895425));
#195848=CARTESIAN_POINT('Ctrl Pts',(-3.41991153518071,5.84182813983106,
48.97133543019));
#195849=CARTESIAN_POINT('Ctrl Pts',(-3.56933378942484,5.75173597467379,
48.9795636708375));
#195850=CARTESIAN_POINT('Ctrl Pts',(-3.71487937457066,5.65614358307757,
48.987791911485));
#195851=CARTESIAN_POINT('Ctrl Pts',(-3.84715707495859,5.569265360545,48.9952700685861));
#195852=CARTESIAN_POINT('Ctrl Pts',(-3.97623291515218,5.47784464897183,
49.0027482256872));
#195853=CARTESIAN_POINT('Ctrl Pts',(-4.10179094787334,5.38215570379976,
49.0102263827882));
#195854=CARTESIAN_POINT('Ctrl Pts',(-4.23590552294086,5.27994573807888,
49.0182141621454));
#195855=CARTESIAN_POINT('Ctrl Pts',(-4.36646292588354,5.17251694764452,
49.0262019415026));
#195856=CARTESIAN_POINT('Ctrl Pts',(-4.49301282143286,5.06015066835365,
49.0341897208598));
#195857=CARTESIAN_POINT('Ctrl Pts',(-4.61940527170978,4.94792418798854,
49.0421675623337));
#195858=CARTESIAN_POINT('Ctrl Pts',(-4.74179985130257,4.83077268635996,
49.0501454038076));
#195859=CARTESIAN_POINT('Ctrl Pts',(-4.85977478472476,4.70902092177912,
49.0581232452815));
#195860=CARTESIAN_POINT('Ctrl Pts',(-4.97762971433009,4.58739300279864,
49.0660929717143));
#195861=CARTESIAN_POINT('Ctrl Pts',(-5.09107367901489,4.46117440049268,
49.0740626981471));
#195862=CARTESIAN_POINT('Ctrl Pts',(-5.1997177893047,4.33073018226584,49.08203242458));
#195863=CARTESIAN_POINT('Ctrl Pts',(-5.30827596765968,4.20038913874426,
49.0899958473668));
#195864=CARTESIAN_POINT('Ctrl Pts',(-5.41204160340074,4.06582942009886,
49.0979592701536));
#195865=CARTESIAN_POINT('Ctrl Pts',(-5.51066267351968,3.92745285123539,
49.1059226929404));
#195866=CARTESIAN_POINT('Ctrl Pts',(-5.61226389954651,3.78489478496254,
49.1141267564082));
#195867=CARTESIAN_POINT('Ctrl Pts',(-5.70840444721114,3.63828584246661,
49.1223308198759));
#195868=CARTESIAN_POINT('Ctrl Pts',(-5.79874377347859,3.48810258586861,
49.1305348833436));
#195869=CARTESIAN_POINT('Ctrl Pts',(-5.88636446989879,3.34243887464265,
49.1384920575248));
#195870=CARTESIAN_POINT('Ctrl Pts',(-5.96852785293425,3.19341322025949,
49.1464492317059));
#195871=CARTESIAN_POINT('Ctrl Pts',(-6.0449672588425,3.0414897401639,49.1544064058871));
#195872=CARTESIAN_POINT('Ctrl Pts',(-6.12140210458061,2.88957532341604,
49.1623631053645));
#195873=CARTESIAN_POINT('Ctrl Pts',(-6.19211348109745,2.7347637646725,49.170319804842));
#195874=CARTESIAN_POINT('Ctrl Pts',(-6.25688109669869,2.57754300483516,
49.1782765043194));
#195875=CARTESIAN_POINT('Ctrl Pts',(-6.32165806836643,2.42029953352586,
49.1862343531894));
#195876=CARTESIAN_POINT('Ctrl Pts',(-6.38048942633366,2.260646520787,49.1941922020593));
#195877=CARTESIAN_POINT('Ctrl Pts',(-6.43320345590825,2.09909082578392,
49.2021500509292));
#195878=CARTESIAN_POINT('Ctrl Pts',(-6.48593586589165,1.93747879929292,
49.2101106745541));
#195879=CARTESIAN_POINT('Ctrl Pts',(-6.53254658668755,1.77396313228821,
49.218071298179));
#195880=CARTESIAN_POINT('Ctrl Pts',(-6.57291415283513,1.60906449201382,
49.2260319218039));
#195881=CARTESIAN_POINT('Ctrl Pts',(-6.61332397791934,1.44399322698504,
49.2340008790373));
#195882=CARTESIAN_POINT('Ctrl Pts',(-6.64747751440874,1.27753646868631,
49.2419698362706));
#195883=CARTESIAN_POINT('Ctrl Pts',(-6.67530457567069,1.11022422151113,
49.2499387935039));
#195884=CARTESIAN_POINT('Ctrl Pts',(-6.70314910520335,0.942806945076842,
49.2579127532023));
#195885=CARTESIAN_POINT('Ctrl Pts',(-6.72465920715327,0.774533486416592,
49.2658867129007));
#195886=CARTESIAN_POINT('Ctrl Pts',(-6.73981672788629,0.605936856862318,
49.2738606725991));
#195887=CARTESIAN_POINT('Ctrl Pts',(-6.75499391063842,0.437121527283789,
49.2818449759514));
#195888=CARTESIAN_POINT('Ctrl Pts',(-6.76380205298423,0.267982567572156,
49.2898292793037));
#195889=CARTESIAN_POINT('Ctrl Pts',(-6.76627503343266,0.0990513601414978,
49.2978135826559));
#195890=CARTESIAN_POINT('Ctrl Pts',(-6.76679193541882,0.0637413856120705,
49.2994824604926));
#195891=CARTESIAN_POINT('Ctrl Pts',(-6.76703223858502,0.0284404633191816,
49.3011513383293));
#195892=CARTESIAN_POINT('Ctrl Pts',(-6.76699653643252,-0.0068465984469402,
49.302820216166));
#195893=CARTESIAN_POINT('Ctrl Pts',(-6.76699653643201,-0.00684659895290697,
49.3028202161899));
#195894=CARTESIAN_POINT('Ctrl Pts',(-6.76681601664308,-0.185267563115419,
49.3112585156058));
#195895=CARTESIAN_POINT('Ctrl Pts',(-6.75957966634908,-0.36344495759579,
49.3196968150218));
#195896=CARTESIAN_POINT('Ctrl Pts',(-6.74534153478688,-0.540977429361874,
49.3281351144377));
#195897=CARTESIAN_POINT('Ctrl Pts',(-6.73128120881953,-0.716292878015842,
49.3364680364845));
#195898=CARTESIAN_POINT('Ctrl Pts',(-6.7103637057022,-0.891284955468209,
49.3448009585312));
#195899=CARTESIAN_POINT('Ctrl Pts',(-6.68260769154779,-1.06538417524681,
49.3531338805779));
#195900=CARTESIAN_POINT('Ctrl Pts',(-6.65488447827121,-1.23927765196715,
49.3614569551315));
#195901=CARTESIAN_POINT('Ctrl Pts',(-6.62033890717343,-1.41228003226213,
49.3697800296851));
#195902=CARTESIAN_POINT('Ctrl Pts',(-6.57904153321619,-1.58382496009386,
49.3781031042387));
#195903=CARTESIAN_POINT('Ctrl Pts',(-6.5377853823702,-1.75519865147726,
49.3864178706847));
#195904=CARTESIAN_POINT('Ctrl Pts',(-6.48979093716717,-1.92511745270927,
49.3947326371306));
#195905=CARTESIAN_POINT('Ctrl Pts',(-6.43518015765482,-2.09302301433256,
49.4030474035766));
#195906=CARTESIAN_POINT('Ctrl Pts',(-6.38061387326331,-2.26079177186109,
49.4113553954161));
#195907=CARTESIAN_POINT('Ctrl Pts',(-6.31944210328963,-2.42655022880255,
49.4196633872557));
#195908=CARTESIAN_POINT('Ctrl Pts',(-6.25183726416639,-2.58975284967129,
49.4279713790952));
#195909=CARTESIAN_POINT('Ctrl Pts',(-6.18427511306904,-2.75285241877931,
49.4362741249823));
#195910=CARTESIAN_POINT('Ctrl Pts',(-6.11028812081249,-2.91339904746005,
49.4445768708694));
#195911=CARTESIAN_POINT('Ctrl Pts',(-6.03009775559501,-3.07086470850933,
49.4528796167565));
#195912=CARTESIAN_POINT('Ctrl Pts',(-5.94994016162442,-3.22826601836078,
49.461178969576));
#195913=CARTESIAN_POINT('Ctrl Pts',(-5.86358440374889,-3.38258855986731,
49.4694783223954));
#195914=CARTESIAN_POINT('Ctrl Pts',(-5.77129918736136,-3.53332629259769,
49.4777776752149));
#195915=CARTESIAN_POINT('Ctrl Pts',(-5.67903359849096,-3.68403196594145,
49.4860752629012));
#195916=CARTESIAN_POINT('Ctrl Pts',(-5.58084124504725,-3.83115405289675,
49.4943728505875));
#195917=CARTESIAN_POINT('Ctrl Pts',(-5.47703582137325,-3.97421282915174,
49.5026704382739));
#195918=CARTESIAN_POINT('Ctrl Pts',(-5.3732352254783,-4.11726495203411,
49.5109676400563));
#195919=CARTESIAN_POINT('Ctrl Pts',(-5.26382228400117,-4.25625385932584,
49.5192648418387));
#195920=CARTESIAN_POINT('Ctrl Pts',(-5.14915299918866,-4.39073027991318,
49.5275620436212));
#195921=CARTESIAN_POINT('Ctrl Pts',(-5.0344699930639,-4.52522279193214,
49.5358602382457));
#195922=CARTESIAN_POINT('Ctrl Pts',(-4.91452961647778,-4.65520147698483,
49.5441584328702));
#195923=CARTESIAN_POINT('Ctrl Pts',(-4.78972711030074,-4.78025137506912,
49.5524566274948));
#195924=CARTESIAN_POINT('Ctrl Pts',(-4.66483682906601,-4.9053892222047,
49.5607606583364));
#195925=CARTESIAN_POINT('Ctrl Pts',(-4.53507783128464,-5.02559110912605,
49.569064689178));
#195926=CARTESIAN_POINT('Ctrl Pts',(-4.40088171503481,-5.14047946501806,
49.5773687200195));
#195927=CARTESIAN_POINT('Ctrl Pts',(-4.26663680138383,-5.25540959747817,
49.5856757704353));
#195928=CARTESIAN_POINT('Ctrl Pts',(-4.12795182248836,-5.36502212728453,
49.593982820851));
#195929=CARTESIAN_POINT('Ctrl Pts',(-3.9852903595932,-5.46898068653872,
49.6022898712667));
#195930=CARTESIAN_POINT('Ctrl Pts',(-3.84247636751682,-5.57305039503813,
49.6106058033214));
#195931=CARTESIAN_POINT('Ctrl Pts',(-3.6956776825091,-5.67145385588585,
49.618921735376));
#195932=CARTESIAN_POINT('Ctrl Pts',(-3.54538660039247,-5.76389823416041,
49.6272376674306));
#195933=CARTESIAN_POINT('Ctrl Pts',(-3.43209399040731,-5.83358477008577,
49.6335063936495));
#195934=CARTESIAN_POINT('Ctrl Pts',(-3.3168174287625,-5.89988598161268,
49.6397751198684));
#195935=CARTESIAN_POINT('Ctrl Pts',(-3.19977640156996,-5.96269402031968,
49.6460438460873));
#195936=CARTESIAN_POINT('Ctrl Pts',(-3.04200461558026,-6.04735951479634,
49.6544941148106));
#195937=CARTESIAN_POINT('Ctrl Pts',(-2.88073650691223,-6.12583114690814,
49.6629443835339));
#195938=CARTESIAN_POINT('Ctrl Pts',(-2.71648547473006,-6.19782184848682,
49.6713946522573));
#195939=CARTESIAN_POINT('Ctrl Pts',(-2.55237939965628,-6.26974901582896,
49.6798374633318));
#195940=CARTESIAN_POINT('Ctrl Pts',(-2.38529595045556,-6.33520652042679,
49.6882802744063));
#195941=CARTESIAN_POINT('Ctrl Pts',(-2.21577244452717,-6.39395350890778,
49.6967230854808));
#195942=CARTESIAN_POINT('Ctrl Pts',(-2.04637546778268,-6.45265664973195,
49.7051595949985));
#195943=CARTESIAN_POINT('Ctrl Pts',(-1.87454237707326,-6.50465915059237,
49.7135961045163));
#195944=CARTESIAN_POINT('Ctrl Pts',(-1.70083012673447,-6.54976838369056,
49.722032614034));
#195945=CARTESIAN_POINT('Ctrl Pts',(-1.52724217685827,-6.59484533870513,
49.7304630867752));
#195946=CARTESIAN_POINT('Ctrl Pts',(-1.35177806961323,-6.63303878149209,
49.7388935595164));
#195947=CARTESIAN_POINT('Ctrl Pts',(-1.17500976540876,-6.66420595804137,
49.7473240322576));
#195948=CARTESIAN_POINT('Ctrl Pts',(-0.998317453419157,-6.69535973590592,
49.7557508807615));
#195949=CARTESIAN_POINT('Ctrl Pts',(-0.820322388132919,-6.71949321167944,
49.7641777292653));
#195950=CARTESIAN_POINT('Ctrl Pts',(-0.641607212394431,-6.7365146169962,
49.7726045777691));
#195951=CARTESIAN_POINT('Ctrl Pts',(-0.462947199648441,-6.753530768413,
49.7810288252058));
#195952=CARTESIAN_POINT('Ctrl Pts',(-0.28356784941739,-6.76343919580401,
49.7894530726424));
#195953=CARTESIAN_POINT('Ctrl Pts',(-0.104057796442262,-6.76619989174127,
49.797877320079));
#195954=CARTESIAN_POINT('Ctrl Pts',(-0.0534787316738465,-6.76697775023055,
49.80025095069));
#195955=CARTESIAN_POINT('Ctrl Pts',(-0.00288931352831388,-6.76718846934994,
49.802624581301));
#195956=CARTESIAN_POINT('Ctrl Pts',(0.0476972528130159,-6.76683190068101,
49.804998211912));
#195957=CARTESIAN_POINT('Ctrl Pts',(0.231379807142229,-6.7655371805875,
49.8136169928492));
#195958=CARTESIAN_POINT('Ctrl Pts',(0.414942543859155,-6.756759631352,49.8222357737864));
#195959=CARTESIAN_POINT('Ctrl Pts',(0.597770730378398,-6.74054590919036,
49.8308545547236));
#195960=CARTESIAN_POINT('Ctrl Pts',(0.780708740677443,-6.72432244754442,
49.8394785129101));
#195961=CARTESIAN_POINT('Ctrl Pts',(0.962911017213911,-6.70065392533793,
49.8481024710966));
#195962=CARTESIAN_POINT('Ctrl Pts',(1.14376928233591,-6.66963873300382,
49.8567264292831));
#195963=CARTESIAN_POINT('Ctrl Pts',(1.3311613394948,-6.63750306759342,49.8656619416542));
#195964=CARTESIAN_POINT('Ctrl Pts',(1.51711011063208,-6.59748008208997,
49.8745974540253));
#195965=CARTESIAN_POINT('Ctrl Pts',(1.70095264677661,-6.54973656671959,
49.8835329663965));
#195966=CARTESIAN_POINT('Ctrl Pts',(1.87871688703933,-6.50357157185346,
49.8921730482912));
#195967=CARTESIAN_POINT('Ctrl Pts',(2.05451165998388,-6.45018852914267,
49.9008131301858));
#195968=CARTESIAN_POINT('Ctrl Pts',(2.22775448583029,-6.38978864680695,
49.9094532120805));
#195969=CARTESIAN_POINT('Ctrl Pts',(2.40988285429204,-6.32629088306787,
49.9185364396899));
#195970=CARTESIAN_POINT('Ctrl Pts',(2.58919025776469,-6.25503773795242,
49.9276196672992));
#195971=CARTESIAN_POINT('Ctrl Pts',(2.76502480367359,-6.17631984559332,
49.9367028949086));
#195972=CARTESIAN_POINT('Ctrl Pts',(2.94085934958255,-6.09760195323419,
49.945786122518));
#195973=CARTESIAN_POINT('Ctrl Pts',(3.11322070614304,-6.0114195171545,49.9548693501273));
#195974=CARTESIAN_POINT('Ctrl Pts',(3.28148753969462,-5.91811866447682,
49.9639525777367));
#195975=CARTESIAN_POINT('Ctrl Pts',(3.44903870138265,-5.82521463863482,
49.9729971725966));
#195976=CARTESIAN_POINT('Ctrl Pts',(3.61268524976751,-5.72516759141924,
49.9820417674564));
#195977=CARTESIAN_POINT('Ctrl Pts',(3.77184622959922,-5.6183151407035,49.9910863623163));
#195978=CARTESIAN_POINT('Ctrl Pts',(3.93086115417876,-5.51156074393069,
50.0001226573367));
#195979=CARTESIAN_POINT('Ctrl Pts',(4.08539853090776,-5.3980135443738,50.0091589523571));
#195980=CARTESIAN_POINT('Ctrl Pts',(4.23490548248072,-5.27805499729349,
50.0181952473775));
#195981=CARTESIAN_POINT('Ctrl Pts',(4.38414786977883,-5.15830872626915,
50.0272155519652));
#195982=CARTESIAN_POINT('Ctrl Pts',(4.52837742223618,-5.03217391168751,
50.036235856553));
#195983=CARTESIAN_POINT('Ctrl Pts',(4.66707361998934,-4.90007273676623,
50.0452561611407));
#195984=CARTESIAN_POINT('Ctrl Pts',(4.80559515682386,-4.76813791761344,
50.0542651064071));
#195985=CARTESIAN_POINT('Ctrl Pts',(4.93859707330936,-4.63025189600761,
50.0632740516734));
#195986=CARTESIAN_POINT('Ctrl Pts',(5.06559312154925,-4.48687589831867,
50.0722829969398));
#195987=CARTESIAN_POINT('Ctrl Pts',(5.19230078864845,-4.343825477168,50.0812714847986));
#195988=CARTESIAN_POINT('Ctrl Pts',(5.31302965279278,-4.19531014204271,
50.0902599726574));
#195989=CARTESIAN_POINT('Ctrl Pts',(5.42733173623316,-4.04182622398296,
50.0992484605163));
#195990=CARTESIAN_POINT('Ctrl Pts',(5.52761608311355,-3.90716520980037,
50.1071346215313));
#195991=CARTESIAN_POINT('Ctrl Pts',(5.62295375801983,-3.76868018637237,
50.1150207825464));
#195992=CARTESIAN_POINT('Ctrl Pts',(5.71306609539626,-3.62672921371775,
50.1229069435614));
#195993=CARTESIAN_POINT('Ctrl Pts',(5.80586716548787,-3.48054276970326,
50.1310284084176));
#195994=CARTESIAN_POINT('Ctrl Pts',(5.89308350086692,-3.33074502271687,
50.1391498732738));
#195995=CARTESIAN_POINT('Ctrl Pts',(5.97443016494423,-3.17780949778373,
50.1472713381299));
#195996=CARTESIAN_POINT('Ctrl Pts',(6.05577102780719,-3.02488487940432,
50.1553922238061));
#195997=CARTESIAN_POINT('Ctrl Pts',(6.13124288118561,-2.86882325209378,
50.1635131094824));
#195998=CARTESIAN_POINT('Ctrl Pts',(6.20060663605718,-2.7101229390719,50.1716339951586));
#195999=CARTESIAN_POINT('Ctrl Pts',(6.26997868188088,-2.55140365682464,
50.1797558515128));
#196000=CARTESIAN_POINT('Ctrl Pts',(6.33324102986522,-2.39004539684763,
50.1878777078671));
#196001=CARTESIAN_POINT('Ctrl Pts',(6.39020266694267,-2.22656661148926,
50.1959995642213));
#196002=CARTESIAN_POINT('Ctrl Pts',(6.44720586252584,-2.06296855403155,
50.2041273461815));
#196003=CARTESIAN_POINT('Ctrl Pts',(6.49789904528797,-1.89724722734643,
50.2122551281417));
#196004=CARTESIAN_POINT('Ctrl Pts',(6.54214085162684,-1.7299370154648,50.2203829101018));
#196005=CARTESIAN_POINT('Ctrl Pts',(6.58640068043322,-1.56255864762147,
50.2285140030183));
#196006=CARTESIAN_POINT('Ctrl Pts',(6.62420381447888,-1.39359046152614,
50.2366450959348));
#196007=CARTESIAN_POINT('Ctrl Pts',(6.65546004985548,-1.22357693864249,
50.2447761888512));
#196008=CARTESIAN_POINT('Ctrl Pts',(6.68675040010672,-1.05337785310386,
50.2529161565158));
#196009=CARTESIAN_POINT('Ctrl Pts',(6.71147952713835,-0.882131513925039,
50.2610561241803));
#196010=CARTESIAN_POINT('Ctrl Pts',(6.72960902520342,-0.710388181138124,
50.2691960918449));
#196011=CARTESIAN_POINT('Ctrl Pts',(6.73901176676927,-0.621314663048547,
50.2734178310254));
#196012=CARTESIAN_POINT('Ctrl Pts',(6.74664012502561,-0.532107489665762,
50.2776395702059));
#196013=CARTESIAN_POINT('Ctrl Pts',(6.75249426252371,-0.442843352196272,
50.2818613093864));
#196014=CARTESIAN_POINT('Ctrl Pts',(6.76419800464635,-0.264384194705872,
50.290301518844));
#196015=CARTESIAN_POINT('Ctrl Pts',(6.76883145057379,-0.0853285350571334,
50.2987417283017));
#196016=CARTESIAN_POINT('Ctrl Pts',(6.76635072172373,0.0937385226508884,
50.3071819377593));
#196017=CARTESIAN_POINT('Ctrl Pts',(6.7638718723933,0.272669910533722,50.3156157525078));
#196018=CARTESIAN_POINT('Ctrl Pts',(6.75428959757382,0.451612347007539,
50.3240495672564));
#196019=CARTESIAN_POINT('Ctrl Pts',(6.73761203233686,0.62997865178875,50.3324833820049));
#196020=CARTESIAN_POINT('Ctrl Pts',(6.72094453903604,0.808237237367194,
50.3409121033935));
#196021=CARTESIAN_POINT('Ctrl Pts',(6.69719032904113,0.985920053713816,
50.349340824782));
#196022=CARTESIAN_POINT('Ctrl Pts',(6.66640954848244,1.16244257144261,50.3577695461705));
#196023=CARTESIAN_POINT('Ctrl Pts',(6.63564263045777,1.33888558990717,50.3661944715723));
#196024=CARTESIAN_POINT('Ctrl Pts',(6.5978555087356,1.5141690236913,50.374619396974));
#196025=CARTESIAN_POINT('Ctrl Pts',(6.55315990282209,1.68771570119044,50.3830443223758));
#196026=CARTESIAN_POINT('Ctrl Pts',(6.50847756853883,1.86121084683793,50.3914667461335));
#196027=CARTESIAN_POINT('Ctrl Pts',(6.45689092401229,2.03296994202092,50.3998891698912));
#196028=CARTESIAN_POINT('Ctrl Pts',(6.3985623932095,2.20242781952215,50.4083115936489));
#196029=CARTESIAN_POINT('Ctrl Pts',(6.34023294506684,2.37188836210795,50.4167341498671));
#196030=CARTESIAN_POINT('Ctrl Pts',(6.27516150101785,2.53904729728787,50.4251567060854));
#196031=CARTESIAN_POINT('Ctrl Pts',(6.20356000199686,2.70335574825526,50.4335792623036));
#196032=CARTESIAN_POINT('Ctrl Pts',(6.13195608426367,2.86766974959325,50.4420021030373));
#196033=CARTESIAN_POINT('Ctrl Pts',(6.05382180483552,3.02913276885523,50.4504249437711));
#196034=CARTESIAN_POINT('Ctrl Pts',(5.96941686060406,3.18721686496792,50.4588477845048));
#196035=CARTESIAN_POINT('Ctrl Pts',(5.88499728129378,3.34532837147972,50.4672720856855));
#196036=CARTESIAN_POINT('Ctrl Pts',(5.79430502657094,3.50005949253455,50.4756963868661));
#196037=CARTESIAN_POINT('Ctrl Pts',(5.69764543893034,3.65090748338496,50.4841206880467));
#196038=CARTESIAN_POINT('Ctrl Pts',(5.60095559247987,3.80180269645911,50.4925476264135));
#196039=CARTESIAN_POINT('Ctrl Pts',(5.49829486863055,3.94881207502123,50.5009745647804));
#196040=CARTESIAN_POINT('Ctrl Pts',(5.39001175810941,4.09146211609522,50.5094015031472));
#196041=CARTESIAN_POINT('Ctrl Pts',(5.28163128746083,4.23424041748709,50.5178360183908));
#196042=CARTESIAN_POINT('Ctrl Pts',(5.16761853085843,4.3726512834815,50.5262705336345));
#196043=CARTESIAN_POINT('Ctrl Pts',(5.04836279385075,4.50625366592511,50.5347050488782));
#196044=CARTESIAN_POINT('Ctrl Pts',(4.92904945530045,4.63992057946399,50.5431436380649));
#196045=CARTESIAN_POINT('Ctrl Pts',(4.80448831376961,4.7687741341678,50.5515822272517));
#196046=CARTESIAN_POINT('Ctrl Pts',(4.67510568055939,4.8924100273384,50.5600208164385));
#196047=CARTESIAN_POINT('Ctrl Pts',(4.54557842683734,5.01618411746565,50.5684688380588));
#196048=CARTESIAN_POINT('Ctrl Pts',(4.41121915937598,5.13472866788723,50.5769168596791));
#196049=CARTESIAN_POINT('Ctrl Pts',(4.27248833791398,5.24767876326181,50.5853648812994));
#196050=CARTESIAN_POINT('Ctrl Pts',(4.19363596539665,5.31187778480934,50.5901666012115));
#196051=CARTESIAN_POINT('Ctrl Pts',(4.11337189238453,5.37427022041562,50.5949683211236));
#196052=CARTESIAN_POINT('Ctrl Pts',(4.03178486308043,5.4347952875739,50.5997700410358));
#196053=CARTESIAN_POINT('Ctrl Pts',(3.88493003633055,5.54373905384864,50.6084130294104));
#196054=CARTESIAN_POINT('Ctrl Pts',(3.73344294290708,5.64688470195427,50.617056017785));
#196055=CARTESIAN_POINT('Ctrl Pts',(3.57782307109196,5.74382025066611,50.6256990061597));
#196056=CARTESIAN_POINT('Ctrl Pts',(3.4222031992769,5.84075579937792,50.6343419945343));
#196057=CARTESIAN_POINT('Ctrl Pts',(3.26245088247718,5.93148094036033,50.6429849829089));
#196058=CARTESIAN_POINT('Ctrl Pts',(3.0991061983213,6.01563211736942,50.6516279712835));
#196059=CARTESIAN_POINT('Origin',(0.,0.,4.30282021618968));
#196060=CARTESIAN_POINT('',(3.09910619832131,6.01563211736941,53.0454129677962));
#196061=CARTESIAN_POINT('',(3.09910619832128,6.01563211736943,52.6513490741792));
#196062=CARTESIAN_POINT('',(3.09910619832133,6.0156321173694,4.30282021618968));
#196063=CARTESIAN_POINT('',(-6.76699999999835,4.72499786567897E-6,51.6972805685448));
#196064=CARTESIAN_POINT('Ctrl Pts',(-6.76699999999835,4.72499786567896E-6,
51.6972805685448));
#196065=CARTESIAN_POINT('Ctrl Pts',(-6.7670001215516,-0.17408018574719,
51.705442029816));
#196066=CARTESIAN_POINT('Ctrl Pts',(-6.76027824898233,-0.348190866565372,
51.7136034910872));
#196067=CARTESIAN_POINT('Ctrl Pts',(-6.74685446399381,-0.521769912592487,
51.7217649523584));
#196068=CARTESIAN_POINT('Ctrl Pts',(-6.733429900442,-0.695359025994333,
51.7299268869845));
#196069=CARTESIAN_POINT('Ctrl Pts',(-6.71330267886051,-0.868416082426914,
51.7380888216106));
#196070=CARTESIAN_POINT('Ctrl Pts',(-6.68654482128806,-1.04038807802948,
51.7462507562368));
#196071=CARTESIAN_POINT('Ctrl Pts',(-6.65909310961529,-1.21681945435655,
51.7546243367987));
#196072=CARTESIAN_POINT('Ctrl Pts',(-6.62466227160216,-1.39210833402499,
51.7629979173606));
#196073=CARTESIAN_POINT('Ctrl Pts',(-6.58338601740211,-1.56566840227246,
51.7713714979226));
#196074=CARTESIAN_POINT('Ctrl Pts',(-6.54310963007841,-1.73502418971343,
51.7795422387162));
#196075=CARTESIAN_POINT('Ctrl Pts',(-6.49631578017444,-1.90273361408968,
51.7877129795098));
#196076=CARTESIAN_POINT('Ctrl Pts',(-6.44317926085405,-2.068267393859,51.7958837203034));
#196077=CARTESIAN_POINT('Ctrl Pts',(-6.38806405939049,-2.23996527203577,
51.8043587207495));
#196078=CARTESIAN_POINT('Ctrl Pts',(-6.32612486716165,-2.40932194435085,
51.8128337211956));
#196079=CARTESIAN_POINT('Ctrl Pts',(-6.25761121042792,-2.57576997015005,
51.8213087216417));
#196080=CARTESIAN_POINT('Ctrl Pts',(-6.1890975536942,-2.74221799594926,
51.8297837220878));
#196081=CARTESIAN_POINT('Ctrl Pts',(-6.11400965808697,-2.90575700593975,
51.8382587225339));
#196082=CARTESIAN_POINT('Ctrl Pts',(-6.03264948575606,-3.06584885178758,
51.84673372298));
#196083=CARTESIAN_POINT('Ctrl Pts',(-5.95162330760453,-3.22528349960904,
51.8551739324376));
#196084=CARTESIAN_POINT('Ctrl Pts',(-5.86421276379904,-3.38162221811784,
51.8636141418953));
#196085=CARTESIAN_POINT('Ctrl Pts',(-5.77067877548236,-3.53433946731173,
51.8720543513529));
#196086=CARTESIAN_POINT('Ctrl Pts',(-5.67721565301913,-3.68694101056392,
51.8804881661014));
#196087=CARTESIAN_POINT('Ctrl Pts',(-5.57763850795933,-3.83592627071905,
51.8889219808499));
#196088=CARTESIAN_POINT('Ctrl Pts',(-5.47225404880864,-3.98079447162215,
51.8973557955985));
#196089=CARTESIAN_POINT('Ctrl Pts',(-5.36693323357255,-4.12557518353985,
51.905784516987));
#196090=CARTESIAN_POINT('Ctrl Pts',(-5.25581229195834,-4.26624352415761,
51.9142132383756));
#196091=CARTESIAN_POINT('Ctrl Pts',(-5.13924130477004,-4.4023275447592,
51.9226419597641));
#196092=CARTESIAN_POINT('Ctrl Pts',(-5.02272281687667,-4.53835027811165,
51.9310668851659));
#196093=CARTESIAN_POINT('Ctrl Pts',(-4.90075939399643,-4.66979255520143,
51.9394918105676));
#196094=CARTESIAN_POINT('Ctrl Pts',(-4.77374171033594,-4.79621507889282,
51.9479167359693));
#196095=CARTESIAN_POINT('Ctrl Pts',(-4.64676174250258,-4.92260006348012,
51.956339159727));
#196096=CARTESIAN_POINT('Ctrl Pts',(-4.51473074288339,-5.0439680321168,
51.9647615834848));
#196097=CARTESIAN_POINT('Ctrl Pts',(-4.37807686013395,-5.15991589144238,
51.9731840072425));
#196098=CARTESIAN_POINT('Ctrl Pts',(-4.24142082821196,-5.27586557429432,
51.9816065634607));
#196099=CARTESIAN_POINT('Ctrl Pts',(-4.10014201781241,-5.38639475674505,
51.9900291196789));
#196100=CARTESIAN_POINT('Ctrl Pts',(-3.95470284318514,-5.49113962872038,
51.9984516758971));
#196101=CARTESIAN_POINT('Ctrl Pts',(-3.80925875559516,-5.59588803899721,
52.0068745166308));
#196102=CARTESIAN_POINT('Ctrl Pts',(-3.65965429414324,-5.69485155411564,
52.0152973573646));
#196103=CARTESIAN_POINT('Ctrl Pts',(-3.50638225324372,-5.78770874302928,
52.0237201980983));
#196104=CARTESIAN_POINT('Ctrl Pts',(-3.35308363631337,-5.880582032567,52.032144499279));
#196105=CARTESIAN_POINT('Ctrl Pts',(-3.19611645737286,-5.96734671216084,
52.0405688004596));
#196106=CARTESIAN_POINT('Ctrl Pts',(-3.03599990153993,-6.04772631638118,
52.0489931016403));
#196107=CARTESIAN_POINT('Ctrl Pts',(-2.8758332220041,-6.1281310830426,52.0574200400071));
#196108=CARTESIAN_POINT('Ctrl Pts',(-2.71251549795603,-6.20214663963946,
52.0658469783739));
#196109=CARTESIAN_POINT('Ctrl Pts',(-2.54658809276887,-6.26954369039469,
52.0742739167407));
#196110=CARTESIAN_POINT('Ctrl Pts',(-2.38051149798803,-6.33700133957009,
52.0827084319844));
#196111=CARTESIAN_POINT('Ctrl Pts',(-2.21182084286592,-6.39782846647733,
52.091142947228));
#196112=CARTESIAN_POINT('Ctrl Pts',(-2.04107602245292,-6.45184451692443,
52.0995774624717));
#196113=CARTESIAN_POINT('Ctrl Pts',(-1.87024873082868,-6.50588665758671,
52.1080160516584));
#196114=CARTESIAN_POINT('Ctrl Pts',(-1.6973656153603,-6.55311106785541,
52.1164546408452));
#196115=CARTESIAN_POINT('Ctrl Pts',(-1.52299963722095,-6.59338768047389,
52.124893230032));
#196116=CARTESIAN_POINT('Ctrl Pts',(-1.34843875736749,-6.63370931323289,
52.1333412516523));
#196117=CARTESIAN_POINT('Ctrl Pts',(-1.1723920296516,-6.66706756330533,
52.1417892732726));
#196118=CARTESIAN_POINT('Ctrl Pts',(-0.995441675805299,-6.69338366374362,
52.1502372948929));
#196119=CARTESIAN_POINT('Ctrl Pts',(-0.894865934439944,-6.7083413129028,
52.1550390148051));
#196120=CARTESIAN_POINT('Ctrl Pts',(-0.793998373723847,-6.72102487048139,
52.1598407347173));
#196121=CARTESIAN_POINT('Ctrl Pts',(-0.692946331705399,-6.73142736582488,
52.1646424546295));
#196122=CARTESIAN_POINT('Ctrl Pts',(-0.519545647361508,-6.74927757226717,
52.1728819864803));
#196123=CARTESIAN_POINT('Ctrl Pts',(-0.345214546491155,-6.76044806221027,
52.1811215183311));
#196124=CARTESIAN_POINT('Ctrl Pts',(-0.17050709286497,-6.76485153800752,
52.1893610501819));
#196125=CARTESIAN_POINT('Ctrl Pts',(0.00400644769779515,-6.7692501262544,
52.1975914367282));
#196126=CARTESIAN_POINT('Ctrl Pts',(0.178895156596411,-6.76689664695487,
52.2058218232745));
#196127=CARTESIAN_POINT('Ctrl Pts',(0.353598173914164,-6.7577553471108,
52.2140522098208));
#196128=CARTESIAN_POINT('Ctrl Pts',(0.528138448504477,-6.74862256274683,
52.2222749294386));
#196129=CARTESIAN_POINT('Ctrl Pts',(0.702493022673535,-6.73271456893072,
52.2304976490563));
#196130=CARTESIAN_POINT('Ctrl Pts',(0.876099252822407,-6.71004762272251,
52.2387203686741));
#196131=CARTESIAN_POINT('Ctrl Pts',(1.04955165534421,-6.68740076106165,
52.2469358023699));
#196132=CARTESIAN_POINT('Ctrl Pts',(1.22225668387424,-6.65800692939003,
52.2551512360656));
#196133=CARTESIAN_POINT('Ctrl Pts',(1.39365516884833,-6.62193432996299,
52.2633666697614));
#196134=CARTESIAN_POINT('Ctrl Pts',(1.56496556831073,-6.58588026905091,
52.2715778813622));
#196135=CARTESIAN_POINT('Ctrl Pts',(1.73497041406748,-6.54315434936632,
52.279789092963));
#196136=CARTESIAN_POINT('Ctrl Pts',(1.90311868934679,-6.49387621180593,
52.2880003045638));
#196137=CARTESIAN_POINT('Ctrl Pts',(2.07121057697315,-6.44461459941367,
52.2962087625773));
#196138=CARTESIAN_POINT('Ctrl Pts',(2.23744679320222,-6.38880524624889,
52.3044172205909));
#196139=CARTESIAN_POINT('Ctrl Pts',(2.40128940536313,-6.32661822711714,
52.3126256786044));
#196140=CARTESIAN_POINT('Ctrl Pts',(2.47428486671498,-6.29891255219076,
52.3162827258877));
#196141=CARTESIAN_POINT('Ctrl Pts',(2.54680541987644,-6.26994163894168,
52.3199397731709));
#196142=CARTESIAN_POINT('Ctrl Pts',(2.61880456934592,-6.23972368198888,
52.3235968204542));
#196143=CARTESIAN_POINT('Ctrl Pts',(2.79322008994097,-6.16652169651994,
52.3324558946301));
#196144=CARTESIAN_POINT('Ctrl Pts',(2.96439325302043,-6.0860746986052,52.341314968806));
#196145=CARTESIAN_POINT('Ctrl Pts',(3.13175329346485,-5.99870071839495,
52.3501740429818));
#196146=CARTESIAN_POINT('Ctrl Pts',(3.29942776975585,-5.91116258005375,
52.3590497615758));
#196147=CARTESIAN_POINT('Ctrl Pts',(3.46327457659115,-5.81667157085099,
52.3679254801698));
#196148=CARTESIAN_POINT('Ctrl Pts',(3.62275023178512,-5.7155900621109,52.3768011987638));
#196149=CARTESIAN_POINT('Ctrl Pts',(3.78268098543869,-5.61422009530575,
52.3857022461508));
#196150=CARTESIAN_POINT('Ctrl Pts',(3.9382154048476,-5.50622213235346,52.3946032935378));
#196151=CARTESIAN_POINT('Ctrl Pts',(4.0888390419843,-5.39200188137439,52.4035043409248));
#196152=CARTESIAN_POINT('Ctrl Pts',(4.23966745402118,-5.27762634639781,
52.4124174894078));
#196153=CARTESIAN_POINT('Ctrl Pts',(4.385571544924,-5.15701178724975,52.4213306378908));
#196154=CARTESIAN_POINT('Ctrl Pts',(4.52607132563768,-5.0306030806694,52.4302437863738));
#196155=CARTESIAN_POINT('Ctrl Pts',(4.66688305428365,-4.90391371219448,
52.4391767244837));
#196156=CARTESIAN_POINT('Ctrl Pts',(4.80226627894018,-4.77140463884942,
52.4481096625936));
#196157=CARTESIAN_POINT('Ctrl Pts',(4.93177711590503,-4.63355840354208,
52.4570426007034));
#196158=CARTESIAN_POINT('Ctrl Pts',(5.05505265440609,-4.50234877440141,
52.4655454625619));
#196159=CARTESIAN_POINT('Ctrl Pts',(5.17300782307301,-4.36630393741194,
52.4740483244205));
#196160=CARTESIAN_POINT('Ctrl Pts',(5.28529476372081,-4.22586656918855,
52.482551186279));
#196161=CARTESIAN_POINT('Ctrl Pts',(5.39388226308922,-4.0900560951897,52.4907739101448));
#196162=CARTESIAN_POINT('Ctrl Pts',(5.49737622324671,-3.94987683983684,
52.4989966340107));
#196163=CARTESIAN_POINT('Ctrl Pts',(5.59540686847251,-3.80574709830418,
52.5072193578766));
#196164=CARTESIAN_POINT('Ctrl Pts',(5.69333375158116,-3.66176991322049,
52.5154333782678));
#196165=CARTESIAN_POINT('Ctrl Pts',(5.78580863496937,-3.51385086272946,
52.523647398659));
#196166=CARTESIAN_POINT('Ctrl Pts',(5.87250164412075,-3.36244158905386,
52.5318614190502));
#196167=CARTESIAN_POINT('Ctrl Pts',(5.95912029716409,-3.21116217826367,
52.5400683943222));
#196168=CARTESIAN_POINT('Ctrl Pts',(6.03996677517237,-3.05639881573309,
52.5482753695941));
#196169=CARTESIAN_POINT('Ctrl Pts',(6.11475417616781,-2.89863249913444,
52.5564823448661));
#196170=CARTESIAN_POINT('Ctrl Pts',(6.18949244333358,-2.74096983185672,
52.5646839283191));
#196171=CARTESIAN_POINT('Ctrl Pts',(6.25817940944029,-2.58030846323823,
52.5728855117721));
#196172=CARTESIAN_POINT('Ctrl Pts',(6.32057380811288,-2.41715447090115,
52.5810870952251));
#196173=CARTESIAN_POINT('Ctrl Pts',(6.38293973579966,-2.25407492683349,
52.5892849362402));
#196174=CARTESIAN_POINT('Ctrl Pts',(6.4390186885944,-2.08850535939524,52.5974827772553));
#196175=CARTESIAN_POINT('Ctrl Pts',(6.48861726448096,-1.92097240872421,
52.6056806182703));
#196176=CARTESIAN_POINT('Ctrl Pts',(6.53821146344788,-1.75345424231358,
52.6138777358515));
#196177=CARTESIAN_POINT('Ctrl Pts',(6.58132631461898,-1.58397337905668,
52.6220748534326));
#196178=CARTESIAN_POINT('Ctrl Pts',(6.61781798503562,-1.41307258020921,
52.6302719710138));
#196179=CARTESIAN_POINT('Ctrl Pts',(6.65430924944177,-1.2421736828235,52.6384689973929));
#196180=CARTESIAN_POINT('Ctrl Pts',(6.68417740388642,-1.06985523201138,
52.646666023772));
#196181=CARTESIAN_POINT('Ctrl Pts',(6.70732957509223,-0.896671049545541,
52.6548630501511));
#196182=CARTESIAN_POINT('Ctrl Pts',(6.73048569847149,-0.723457303807981,
52.6630614757972));
#196183=CARTESIAN_POINT('Ctrl Pts',(6.74692350700062,-0.549377887665944,
52.6712599014433));
#196184=CARTESIAN_POINT('Ctrl Pts',(6.75660191893404,-0.374992678670986,
52.6794583270895));
#196185=CARTESIAN_POINT('Ctrl Pts',(6.7662837428612,-0.200545992520039,
52.6876596429801));
#196186=CARTESIAN_POINT('Ctrl Pts',(6.76920140349111,-0.0257936568339158,
52.6958609588707));
#196187=CARTESIAN_POINT('Ctrl Pts',(6.76536593848992,0.148703457661181,
52.7040622747613));
#196188=CARTESIAN_POINT('Ctrl Pts',(6.76152610553612,0.32339929516018,52.7122729305779));
#196189=CARTESIAN_POINT('Ctrl Pts',(6.75091779023594,0.497838971674598,
52.7204835863945));
#196190=CARTESIAN_POINT('Ctrl Pts',(6.73360410007997,0.671464685137079,
52.7286942422111));
#196191=CARTESIAN_POINT('Ctrl Pts',(6.71628020738587,0.845192712025799,
52.7369097363683));
#196192=CARTESIAN_POINT('Ctrl Pts',(6.69224311282282,1.01810546492956,52.7451252305254));
#196193=CARTESIAN_POINT('Ctrl Pts',(6.66160725564259,1.18965447570712,52.7533407246825));
#196194=CARTESIAN_POINT('Ctrl Pts',(6.63092386636619,1.36146964793175,52.76156896533));
#196195=CARTESIAN_POINT('Ctrl Pts',(6.59362133137818,1.53191649938276,52.7697972059776));
#196196=CARTESIAN_POINT('Ctrl Pts',(6.54986459478902,1.7004595819746,52.7780254466251));
#196197=CARTESIAN_POINT('Ctrl Pts',(6.51009670703936,1.85363833596687,52.7855036037262));
#196198=CARTESIAN_POINT('Ctrl Pts',(6.46499839601889,2.00524460684536,52.7929817608273));
#196199=CARTESIAN_POINT('Ctrl Pts',(6.414727853989,2.15489107828162,52.8004599179285));
#196200=CARTESIAN_POINT('Ctrl Pts',(6.36047336360953,2.31639705607734,52.8085307201541));
#196201=CARTESIAN_POINT('Ctrl Pts',(6.30001590092302,2.47614879841058,52.8166015223798));
#196202=CARTESIAN_POINT('Ctrl Pts',(6.23348418439502,2.6336218260975,52.8246723246055));
#196203=CARTESIAN_POINT('Ctrl Pts',(6.16703787316329,2.79089270913393,52.8327327665204));
#196204=CARTESIAN_POINT('Ctrl Pts',(6.09453296829489,2.94589035882531,52.8407932084354));
#196205=CARTESIAN_POINT('Ctrl Pts',(6.01614837033181,3.09810390176861,52.8488536503503));
#196206=CARTESIAN_POINT('Ctrl Pts',(5.93650414798612,3.25276348506982,52.8570436219106));
#196207=CARTESIAN_POINT('Ctrl Pts',(5.85078971948395,3.40454833549116,52.8652335934708));
#196208=CARTESIAN_POINT('Ctrl Pts',(5.75924492905679,3.55294059155704,52.8734235650311));
#196209=CARTESIAN_POINT('Ctrl Pts',(5.66933258222671,3.69868668952763,52.881467491507));
#196210=CARTESIAN_POINT('Ctrl Pts',(5.57379625129872,3.84115982554122,52.889511417983));
#196211=CARTESIAN_POINT('Ctrl Pts',(5.47291062215085,3.97989174751631,52.897555344459));
#196212=CARTESIAN_POINT('Ctrl Pts',(5.372079588008,4.11854859368486,52.9055949179046));
#196213=CARTESIAN_POINT('Ctrl Pts',(5.26590523497039,4.25346795360913,52.9136344913502));
#196214=CARTESIAN_POINT('Ctrl Pts',(5.15470620529812,4.38420949967735,52.9216740647958));
#196215=CARTESIAN_POINT('Ctrl Pts',(5.04354531918934,4.51490619869539,52.9297108805017));
#196216=CARTESIAN_POINT('Ctrl Pts',(4.92736342893566,4.64142765250874,52.9377476962076));
#196217=CARTESIAN_POINT('Ctrl Pts',(4.8065201043854,4.7633657728689,52.9457845119135));
#196218=CARTESIAN_POINT('Ctrl Pts',(4.68168382729436,4.88933302044253,52.954086883237));
#196219=CARTESIAN_POINT('Ctrl Pts',(4.55187304049737,5.01040852287378,52.9623892545606));
#196220=CARTESIAN_POINT('Ctrl Pts',(4.41752628628522,5.12618284008473,52.9706916258842));
#196221=CARTESIAN_POINT('Ctrl Pts',(4.28745632268326,5.23827160109707,52.9787296997639));
#196222=CARTESIAN_POINT('Ctrl Pts',(4.15313507913528,5.34539129234802,52.9867677736437));
#196223=CARTESIAN_POINT('Ctrl Pts',(4.01499456498667,5.44721099675123,52.9948058475235));
#196224=CARTESIAN_POINT('Ctrl Pts',(3.87004081697411,5.55405255489759,53.003240367569));
#196225=CARTESIAN_POINT('Ctrl Pts',(3.72088187097125,5.65505778981958,53.0116748876144));
#196226=CARTESIAN_POINT('Ctrl Pts',(3.56805102046256,5.74989573082644,53.0201094076599));
#196227=CARTESIAN_POINT('Ctrl Pts',(3.41522016995381,5.84473367183333,53.0285439277053));
#196228=CARTESIAN_POINT('Ctrl Pts',(3.25871784107602,5.9334041117776,53.0369784477508));
#196229=CARTESIAN_POINT('Ctrl Pts',(3.09910619832131,6.01563211736941,53.0454129677962));
#196230=CARTESIAN_POINT('Ctrl Pts',(3.0991061983214,6.01563211736937,51.0457552630242));
#196231=CARTESIAN_POINT('Ctrl Pts',(2.93375330764836,6.10081787314649,51.0545047109265));
#196232=CARTESIAN_POINT('Ctrl Pts',(2.76488627843083,6.17918207037033,51.0632541588288));
#196233=CARTESIAN_POINT('Ctrl Pts',(2.59307866646718,6.2504585455399,51.0720036067311));
#196234=CARTESIAN_POINT('Ctrl Pts',(2.4212724418539,6.32173444515032,51.0807529839814));
#196235=CARTESIAN_POINT('Ctrl Pts',(2.24652594672477,6.38592262741834,51.0895023612317));
#196236=CARTESIAN_POINT('Ctrl Pts',(2.06943269687131,6.44280508110559,51.098251738482));
#196237=CARTESIAN_POINT('Ctrl Pts',(1.89234081822085,6.49968709436164,51.1070010479874));
#196238=CARTESIAN_POINT('Ctrl Pts',(1.71290249405594,6.54926340459543,51.1157503574927));
#196239=CARTESIAN_POINT('Ctrl Pts',(1.53172716625062,6.59136563150383,51.1244996669981));
#196240=CARTESIAN_POINT('Ctrl Pts',(1.35055318107333,6.6334675464071,51.1332489116653));
#196241=CARTESIAN_POINT('Ctrl Pts',(1.16764249714414,6.66809542395777,51.1419981563326));
#196242=CARTESIAN_POINT('Ctrl Pts',(0.983616340614252,6.6951316562467,51.1507474009998));
#196243=CARTESIAN_POINT('Ctrl Pts',(0.799591486713773,6.72216769715962,
51.1594965837355));
#196244=CARTESIAN_POINT('Ctrl Pts',(0.614451459526678,6.74161215869371,
51.1682457664712));
#196245=CARTESIAN_POINT('Ctrl Pts',(0.428825047910284,6.75339900185712,
51.1769949492069));
#196246=CARTESIAN_POINT('Ctrl Pts',(0.243199888596927,6.76518576550222,
51.1857440729174));
#196247=CARTESIAN_POINT('Ctrl Pts',(0.0570886373916771,6.76931499599835,
51.194493196628));
#196248=CARTESIAN_POINT('Ctrl Pts',(-0.12887662681151,6.76577266947846,
51.2032423203385));
#196249=CARTESIAN_POINT('Ctrl Pts',(-0.314840698188554,6.76223036567991,
51.21199138793));
#196250=CARTESIAN_POINT('Ctrl Pts',(-0.500658497951682,6.7510166087922,
51.2207404555216));
#196251=CARTESIAN_POINT('Ctrl Pts',(-0.68569895192668,6.73216948296214,
51.2294895231131));
#196252=CARTESIAN_POINT('Ctrl Pts',(-0.870738280460442,6.71332247176286,
51.2382385374917));
#196253=CARTESIAN_POINT('Ctrl Pts',(-1.05499998761322,6.68684221356176,
51.2469875518702));
#196254=CARTESIAN_POINT('Ctrl Pts',(-1.23785829161503,6.65281863948507,
51.2557365662487));
#196255=CARTESIAN_POINT('Ctrl Pts',(-1.43007412917486,6.61705395368843,
51.2649332999479));
#196256=CARTESIAN_POINT('Ctrl Pts',(-1.62073882535873,6.5729537272777,51.2741300336471));
#196257=CARTESIAN_POINT('Ctrl Pts',(-1.80913696091594,6.52068343478257,
51.2833267673463));
#196258=CARTESIAN_POINT('Ctrl Pts',(-1.98838356186194,6.47095219815174,
51.29207676506));
#196259=CARTESIAN_POINT('Ctrl Pts',(-2.16557827572617,6.41382586850863,
51.3008267627737));
#196260=CARTESIAN_POINT('Ctrl Pts',(-2.34011918621786,6.34949849943246,
51.3095767604873));
#196261=CARTESIAN_POINT('Ctrl Pts',(-2.51465655691185,6.28517243495516,
51.3183265807457));
#196262=CARTESIAN_POINT('Ctrl Pts',(-2.68653996295416,6.21364572242336,
51.3270764010039));
#196263=CARTESIAN_POINT('Ctrl Pts',(-2.85518555380077,6.1351613225218,51.3358262212623));
#196264=CARTESIAN_POINT('Ctrl Pts',(-3.02382794858787,6.05667841000458,
51.3445758756998));
#196265=CARTESIAN_POINT('Ctrl Pts',(-3.18923239109387,5.97123819492025,
51.3533255301373));
#196266=CARTESIAN_POINT('Ctrl Pts',(-3.35083705967812,5.87913088810648,
51.3620751845748));
#196267=CARTESIAN_POINT('Ctrl Pts',(-3.51243888042504,5.7870252044304,51.3708246848237));
#196268=CARTESIAN_POINT('Ctrl Pts',(-3.67024081223785,5.68825280605722,
51.3795741850727));
#196269=CARTESIAN_POINT('Ctrl Pts',(-3.82370687544488,5.58314917682446,
51.3883236853216));
#196270=CARTESIAN_POINT('Ctrl Pts',(-3.97717043817909,5.47804726007953,
51.3970730430121));
#196271=CARTESIAN_POINT('Ctrl Pts',(-4.12629803722562,5.36661448084158,
51.4058224007025));
#196272=CARTESIAN_POINT('Ctrl Pts',(-4.27058317207016,5.24922931204488,
51.414571758393));
#196273=CARTESIAN_POINT('Ctrl Pts',(-4.41486614774942,5.13184589986699,
51.4233209851531));
#196274=CARTESIAN_POINT('Ctrl Pts',(-4.55430658194519,5.00851045722939,
51.4320702119132));
#196275=CARTESIAN_POINT('Ctrl Pts',(-4.68843089001949,4.8796418710302,51.4408194386733));
#196276=CARTESIAN_POINT('Ctrl Pts',(-4.82255336917937,4.75077504207858,
51.4495685461292));
#196277=CARTESIAN_POINT('Ctrl Pts',(-4.95135966065233,4.61637541907988,
51.4583176535851));
#196278=CARTESIAN_POINT('Ctrl Pts',(-5.0744123086934,4.47689945401736,51.467066761041));
#196279=CARTESIAN_POINT('Ctrl Pts',(-5.19746344226513,4.33742520555401,
51.4758157608174));
#196280=CARTESIAN_POINT('Ctrl Pts',(-5.31476088454863,4.19287495491215,
51.4845647605937));
#196281=CARTESIAN_POINT('Ctrl Pts',(-5.4259062762895,4.04373961586577,51.4933137603701));
#196282=CARTESIAN_POINT('Ctrl Pts',(-5.5370638067276,3.89458798906604,51.5020637156648));
#196283=CARTESIAN_POINT('Ctrl Pts',(-5.64206777071952,3.74085050155152,
51.5108136709595));
#196284=CARTESIAN_POINT('Ctrl Pts',(-5.74056148164091,3.58304938223027,
51.5195636262542));
#196285=CARTESIAN_POINT('Ctrl Pts',(-5.83905138951962,3.42525435593149,
51.5283132436953));
#196286=CARTESIAN_POINT('Ctrl Pts',(-5.93103139557725,3.26339625497051,
51.5370628611364));
#196287=CARTESIAN_POINT('Ctrl Pts',(-6.01618907820914,3.09802485064874,
51.5458124785775));
#196288=CARTESIAN_POINT('Ctrl Pts',(-6.1013439254504,2.93265895249521,51.5545618046934));
#196289=CARTESIAN_POINT('Ctrl Pts',(-6.17967677261879,2.76378023985929,
51.5633111308093));
#196290=CARTESIAN_POINT('Ctrl Pts',(-6.25092157009263,2.59196229227023,
51.5720604569251));
#196291=CARTESIAN_POINT('Ctrl Pts',(-6.32216437407792,2.4201491522899,51.5808095382276));
#196292=CARTESIAN_POINT('Ctrl Pts',(-6.3863194154896,2.24539720662741,51.58955861953));
#196293=CARTESIAN_POINT('Ctrl Pts',(-6.44316881037575,2.06829994947569,
51.5983077008325));
#196294=CARTESIAN_POINT('Ctrl Pts',(-6.50002334524603,1.8911866802434,51.6070575731748));
#196295=CARTESIAN_POINT('Ctrl Pts',(-6.54957082411122,1.71172794807601,
51.6158074455172));
#196296=CARTESIAN_POINT('Ctrl Pts',(-6.59164294296105,1.53053334250247,
51.6245573178595));
#196297=CARTESIAN_POINT('Ctrl Pts',(-6.63371214082145,1.34935131693539,
51.6333065827144));
#196298=CARTESIAN_POINT('Ctrl Pts',(-6.66830695239694,1.16643393829737,
51.6420558475693));
#196299=CARTESIAN_POINT('Ctrl Pts',(-6.69530988153987,0.982402458341065,
51.6508051124242));
#196300=CARTESIAN_POINT('Ctrl Pts',(-6.72231419690482,0.798361530947119,
51.6595548264312));
#196301=CARTESIAN_POINT('Ctrl Pts',(-6.74172580829277,0.613206671362522,
51.6683045404383));
#196302=CARTESIAN_POINT('Ctrl Pts',(-6.75347878028179,0.427566795113429,
51.6770542544453));
#196303=CARTESIAN_POINT('Ctrl Pts',(-6.76248992368217,0.285234494205065,
51.6837627642336));
#196304=CARTESIAN_POINT('Ctrl Pts',(-6.76699999999999,0.142617266091684,
51.6904712740218));
#196305=CARTESIAN_POINT('Ctrl Pts',(-6.767,7.53346691421078E-13,51.6971797838101));
#196306=CARTESIAN_POINT('',(-6.76699439492168,0.00870971288474031,51.3028202162293));
#196307=CARTESIAN_POINT('Ctrl Pts',(3.0991061983213,6.01563211736942,50.6516279712835));
#196308=CARTESIAN_POINT('Ctrl Pts',(2.94371706945757,6.09568478731625,50.6598500107166));
#196309=CARTESIAN_POINT('Ctrl Pts',(2.78507754112672,6.16978840847455,50.6680720501497));
#196310=CARTESIAN_POINT('Ctrl Pts',(2.62368229321237,6.23767426404136,50.6762940895828));
#196311=CARTESIAN_POINT('Ctrl Pts',(2.46242609187697,6.30550163402016,50.6845090454959));
#196312=CARTESIAN_POINT('Ctrl Pts',(2.29841922974917,6.36712177758301,50.692724001409));
#196313=CARTESIAN_POINT('Ctrl Pts',(2.13217947892454,6.42231264184897,50.7009389573222));
#196314=CARTESIAN_POINT('Ctrl Pts',(1.96602252369755,6.47747601834158,50.709149821782));
#196315=CARTESIAN_POINT('Ctrl Pts',(1.79763523168352,6.52621638114251,50.7173606862418));
#196316=CARTESIAN_POINT('Ctrl Pts',(1.62755415300313,6.56836025801282,50.7255715507016));
#196317=CARTESIAN_POINT('Ctrl Pts',(1.45752805383191,6.61049051167658,50.7337797609608));
#196318=CARTESIAN_POINT('Ctrl Pts',(1.28580960394632,6.64602844217198,50.74198797122));
#196319=CARTESIAN_POINT('Ctrl Pts',(1.11294935553933,6.67485076477404,50.7501961814792));
#196320=CARTESIAN_POINT('Ctrl Pts',(1.05308282713589,6.68483277284479,50.753038923273));
#196321=CARTESIAN_POINT('Ctrl Pts',(0.993079451021887,6.69400973202146,
50.7558816650668));
#196322=CARTESIAN_POINT('Ctrl Pts',(0.932962387151618,6.70237794996376,
50.7587244068605));
#196323=CARTESIAN_POINT('Ctrl Pts',(0.745614549499311,6.72845652791753,
50.7675834810364));
#196324=CARTESIAN_POINT('Ctrl Pts',(0.557356828514955,6.74664998063951,
50.7764425552123));
#196325=CARTESIAN_POINT('Ctrl Pts',(0.368842368325365,6.75694045462354,
50.7853016293882));
#196326=CARTESIAN_POINT('Ctrl Pts',(0.17997372739156,6.76725026233788,50.7941773479821));
#196327=CARTESIAN_POINT('Ctrl Pts',(-0.00915235787142143,6.76962740410089,
50.8030530665761));
#196328=CARTESIAN_POINT('Ctrl Pts',(-0.197883571541753,6.76410608226349,
50.81192878517));
#196329=CARTESIAN_POINT('Ctrl Pts',(-0.38715337077011,6.75856900413361,
50.820829832557));
#196330=CARTESIAN_POINT('Ctrl Pts',(-0.5760257826646,6.7450883643955,50.829730879944));
#196331=CARTESIAN_POINT('Ctrl Pts',(-0.763851338084534,6.72375045144497,
50.838631927331));
#196332=CARTESIAN_POINT('Ctrl Pts',(-0.951932244923655,6.70238352930908,
50.847545075814));
#196333=CARTESIAN_POINT('Ctrl Pts',(-1.13896319552895,6.67313803159433,
50.856458224297));
#196334=CARTESIAN_POINT('Ctrl Pts',(-1.3243043600039,6.63615151741389,50.86537137278));
#196335=CARTESIAN_POINT('Ctrl Pts',(-1.51005703254404,6.5990828830583,50.8743043108899));
#196336=CARTESIAN_POINT('Ctrl Pts',(-1.69411215942273,6.55423890568354,
50.8832372489998));
#196337=CARTESIAN_POINT('Ctrl Pts',(-1.87584173263627,6.50180796348986,
50.8921701871096));
#196338=CARTESIAN_POINT('Ctrl Pts',(-2.04882193664544,6.45190130869131,
50.9006730489682));
#196339=CARTESIAN_POINT('Ctrl Pts',(-2.21969506740445,6.3951210949578,50.9091759108267));
#196340=CARTESIAN_POINT('Ctrl Pts',(-2.38793604009994,6.33167043270509,
50.9176787726853));
#196341=CARTESIAN_POINT('Ctrl Pts',(-2.55063409216944,6.27031023616295,
50.9259014965511));
#196342=CARTESIAN_POINT('Ctrl Pts',(-2.71118205042307,6.20259335111222,
50.934124220417));
#196343=CARTESIAN_POINT('Ctrl Pts',(-2.86904842766212,6.12869073454759,
50.9423469442829));
#196344=CARTESIAN_POINT('Ctrl Pts',(-3.02674770868881,6.05486634139905,
50.9505609646741));
#196345=CARTESIAN_POINT('Ctrl Pts',(-3.18177073860635,5.97486940551333,
50.9587749850653));
#196346=CARTESIAN_POINT('Ctrl Pts',(-3.33360332083826,5.88891992637836,
50.9669890054566));
#196347=CARTESIAN_POINT('Ctrl Pts',(-3.48530567711517,5.80304416563004,
50.9751959807285));
#196348=CARTESIAN_POINT('Ctrl Pts',(-3.63382272513363,5.71122620531731,
50.9834029560005));
#196349=CARTESIAN_POINT('Ctrl Pts',(-3.77866223746558,5.61373322265599,
50.9916099312724));
#196350=CARTESIAN_POINT('Ctrl Pts',(-3.92340659312845,5.51630429093864,
50.9998115147254));
#196351=CARTESIAN_POINT('Ctrl Pts',(-4.06447792909981,5.41320796294226,
51.0080130981784));
#196352=CARTESIAN_POINT('Ctrl Pts',(-4.20141045945692,5.3047562763209,51.0162146816314));
#196353=CARTESIAN_POINT('Ctrl Pts',(-4.33828050657513,5.19635407693699,
51.0244125226465));
#196354=CARTESIAN_POINT('Ctrl Pts',(-4.47101522993291,5.08260160960884,
51.0326103636615));
#196355=CARTESIAN_POINT('Ctrl Pts',(-4.59917950748939,4.96385302541178,
51.0408082046765));
#196356=CARTESIAN_POINT('Ctrl Pts',(-4.72733247494833,4.84511492040671,
51.0490053222577));
#196357=CARTESIAN_POINT('Ctrl Pts',(-4.85091553121046,4.721381814058,51.0572024398388));
#196358=CARTESIAN_POINT('Ctrl Pts',(-4.96952795103427,4.59304702173722,
51.06539955742));
#196359=CARTESIAN_POINT('Ctrl Pts',(-5.0881390511629,4.46471365728383,51.0735965837991));
#196360=CARTESIAN_POINT('Ctrl Pts',(-5.20177938066244,4.3317789716239,51.0817936101782));
#196361=CARTESIAN_POINT('Ctrl Pts',(-5.31008638998706,4.19467180252212,
51.0899906365573));
#196362=CARTESIAN_POINT('Ctrl Pts',(-5.41841188777574,4.05754122864734,
51.0981890622034));
#196363=CARTESIAN_POINT('Ctrl Pts',(-5.52140202912524,3.91623703388157,
51.1063874878495));
#196364=CARTESIAN_POINT('Ctrl Pts',(-5.61873571006714,3.7712196993037,51.1145859134956));
#196365=CARTESIAN_POINT('Ctrl Pts',(-5.71610370468702,3.62615124081814,
51.1227872293863));
#196366=CARTESIAN_POINT('Ctrl Pts',(-5.80781106676032,3.47736733270664,
51.1309885452769));
#196367=CARTESIAN_POINT('Ctrl Pts',(-5.8935810039394,3.32535591328277,51.1391898611676));
#196368=CARTESIAN_POINT('Ctrl Pts',(-5.97944861871954,3.17317137829798,
51.1474005169842));
#196369=CARTESIAN_POINT('Ctrl Pts',(-6.0593651233506,3.0177523016584,51.1556111728008));
#196370=CARTESIAN_POINT('Ctrl Pts',(-6.13310006773624,2.85961056074664,
51.1638218286174));
#196371=CARTESIAN_POINT('Ctrl Pts',(-6.20687846233823,2.70137563073829,
51.1720373227745));
#196372=CARTESIAN_POINT('Ctrl Pts',(-6.27446789694731,2.54041516863319,
51.1802528169316));
#196373=CARTESIAN_POINT('Ctrl Pts',(-6.33568682700757,2.37725922652174,
51.1884683110888));
#196374=CARTESIAN_POINT('Ctrl Pts',(-6.39700073936435,2.21385014496376,
51.1966965517363));
#196375=CARTESIAN_POINT('Ctrl Pts',(-6.45192428225839,2.04823911658065,
51.2049247923838));
#196376=CARTESIAN_POINT('Ctrl Pts',(-6.50032598710557,1.88097077631737,
51.2131530330313));
#196377=CARTESIAN_POINT('Ctrl Pts',(-6.54431540942763,1.72895055958778,
51.2206311901325));
#196378=CARTESIAN_POINT('Ctrl Pts',(-6.58291845139467,1.57556175889647,
51.2281093472336));
#196379=CARTESIAN_POINT('Ctrl Pts',(-6.61607344889597,1.42121818128458,
51.2355875043348));
#196380=CARTESIAN_POINT('Ctrl Pts',(-6.66575370129441,1.18994602113622,
51.2467929563106));
#196381=CARTESIAN_POINT('Ctrl Pts',(-6.70334113414235,0.955893976418295,
51.2579984082865));
#196382=CARTESIAN_POINT('Ctrl Pts',(-6.72857472823353,0.720118828095116,
51.2692038602624));
#196383=CARTESIAN_POINT('Ctrl Pts',(-6.75380832232471,0.484343679771937,
51.2804093122382));
#196384=CARTESIAN_POINT('Ctrl Pts',(-6.76668789431658,0.246844735791887,
51.2916147642141));
#196385=CARTESIAN_POINT('Ctrl Pts',(-6.76699439492061,0.00870971372223031,
51.3028202161899));
#196386=CARTESIAN_POINT('Ctrl Pts',(-6.76699439492168,0.00870971288473129,
51.3028202162293));
#196387=CARTESIAN_POINT('Ctrl Pts',(-6.76721129645552,-0.159811509704027,
51.3107499883821));
#196388=CARTESIAN_POINT('Ctrl Pts',(-6.76112905601941,-0.32857630920491,
51.318679760535));
#196389=CARTESIAN_POINT('Ctrl Pts',(-6.74872017415013,-0.497056345919674,
51.3266095326878));
#196390=CARTESIAN_POINT('Ctrl Pts',(-6.73632102486479,-0.665404239697082,
51.33453308533));
#196391=CARTESIAN_POINT('Ctrl Pts',(-6.71760513327507,-0.833467434534488,
51.3424566379721));
#196392=CARTESIAN_POINT('Ctrl Pts',(-6.69259704942585,-1.00071661024312,
51.3503801906143));
#196393=CARTESIAN_POINT('Ctrl Pts',(-6.66760286110771,-1.16787285535639,
51.3582993406012));
#196394=CARTESIAN_POINT('Ctrl Pts',(-6.63632349363579,-1.33421560290597,
51.3662184905881));
#196395=CARTESIAN_POINT('Ctrl Pts',(-6.5988353961203,-1.49921993546972,
51.374137640575));
#196396=CARTESIAN_POINT('Ctrl Pts',(-6.56135387818638,-1.66419530792246,
51.3820554006623));
#196397=CARTESIAN_POINT('Ctrl Pts',(-6.51766587443334,-1.82783235690557,
51.3899731607495));
#196398=CARTESIAN_POINT('Ctrl Pts',(-6.46789907706397,-1.98961567367042,
51.3978909208368));
#196399=CARTESIAN_POINT('Ctrl Pts',(-6.41813475745096,-2.15139093567463,
51.4058082867198));
#196400=CARTESIAN_POINT('Ctrl Pts',(-6.36229235824538,-2.31131228174197,
51.4137256526029));
#196401=CARTESIAN_POINT('Ctrl Pts',(-6.30054953263265,-2.46887921673833,
51.421643018486));
#196402=CARTESIAN_POINT('Ctrl Pts',(-6.2387970222584,-2.62647086712754,
51.4295616262591));
#196403=CARTESIAN_POINT('Ctrl Pts',(-6.17114238463177,-2.78170701433539,
51.4374802340322));
#196404=CARTESIAN_POINT('Ctrl Pts',(-6.09781141086639,-2.93410718916465,
51.4453988418053));
#196405=CARTESIAN_POINT('Ctrl Pts',(-6.02445376858468,-3.08656278786656,
51.4533203293645));
#196406=CARTESIAN_POINT('Ctrl Pts',(-5.94541585065988,-3.2361800172617,
51.4612418169238));
#196407=CARTESIAN_POINT('Ctrl Pts',(-5.86096922732225,-3.38250332097126,
51.469163304483));
#196408=CARTESIAN_POINT('Ctrl Pts',(-5.77642537651826,-3.52899509375073,
51.4770939124325));
#196409=CARTESIAN_POINT('Ctrl Pts',(-5.68646058178355,-3.67218503831081,
51.4850245203821));
#196410=CARTESIAN_POINT('Ctrl Pts',(-5.59138988576118,-3.8116463825239,
51.4929551283316));
#196411=CARTESIAN_POINT('Ctrl Pts',(-5.49625815209595,-3.95119726422939,
51.5008908279197));
#196412=CARTESIAN_POINT('Ctrl Pts',(-5.39601422114059,-4.08701447504856,
51.5088265275077));
#196413=CARTESIAN_POINT('Ctrl Pts',(-5.29101265159158,-4.21870526591961,
51.5167622270957));
#196414=CARTESIAN_POINT('Ctrl Pts',(-5.18585329922107,-4.35059394473307,
51.52470985143));
#196415=CARTESIAN_POINT('Ctrl Pts',(-5.07592228849749,-4.47834353926268,
51.5326574757643));
#196416=CARTESIAN_POINT('Ctrl Pts',(-4.96161065321741,-4.60159849681386,
51.5406051000986));
#196417=CARTESIAN_POINT('Ctrl Pts',(-4.89980573467658,-4.66823880506016,
51.5449021453938));
#196418=CARTESIAN_POINT('Ctrl Pts',(-4.83672082785942,-4.73356591591269,
51.5491991906891));
#196419=CARTESIAN_POINT('Ctrl Pts',(-4.77242149879536,-4.79752874278371,
51.5534962359843));
#196420=CARTESIAN_POINT('Ctrl Pts',(-4.6477308660626,-4.92156682327407,
51.561829158031));
#196421=CARTESIAN_POINT('Ctrl Pts',(-4.51804134224386,-5.04089995580397,
51.5701620800777));
#196422=CARTESIAN_POINT('Ctrl Pts',(-4.38373745032378,-5.15510765810267,
51.5784950021244));
#196423=CARTESIAN_POINT('Ctrl Pts',(-4.24959227303486,-5.26918039459295,
51.5868180766781));
#196424=CARTESIAN_POINT('Ctrl Pts',(-4.11084385337876,-5.37813954342007,
51.5951411512317));
#196425=CARTESIAN_POINT('Ctrl Pts',(-3.96791409691977,-5.48160074425941,
51.6034642257853));
#196426=CARTESIAN_POINT('Ctrl Pts',(-3.82512701319462,-5.58495866994643,
51.6117789922312));
#196427=CARTESIAN_POINT('Ctrl Pts',(-3.67816718835495,-5.68282937887212,
51.6200937586772));
#196428=CARTESIAN_POINT('Ctrl Pts',(-3.52749037203691,-5.77486802231765,
51.6284085251232));
#196429=CARTESIAN_POINT('Ctrl Pts',(-3.37693632238244,-5.86683167561239,
51.6367165169627));
#196430=CARTESIAN_POINT('Ctrl Pts',(-3.2226716114118,-5.95297255114884,
51.6450245088022));
#196431=CARTESIAN_POINT('Ctrl Pts',(-3.0651819858386,-6.03298834688834,
51.6533325006417));
#196432=CARTESIAN_POINT('Ctrl Pts',(-2.90779180464315,-6.11295361789653,
51.6616352465288));
#196433=CARTESIAN_POINT('Ctrl Pts',(-2.74718107632359,-6.18680135958582,
51.6699379924159));
#196434=CARTESIAN_POINT('Ctrl Pts',(-2.58386142486764,-6.25427446927947,
51.678240738303));
#196435=CARTESIAN_POINT('Ctrl Pts',(-2.42060851694903,-6.32172000486323,
51.6865400911224));
#196436=CARTESIAN_POINT('Ctrl Pts',(-2.25464921283202,-6.38279596668328,
51.6948394439418));
#196437=CARTESIAN_POINT('Ctrl Pts',(-2.08651672289654,-6.4372926735603,
51.7031387967613));
#196438=CARTESIAN_POINT('Ctrl Pts',(-1.91841999192032,-6.49177778990225,
51.7114363844476));
#196439=CARTESIAN_POINT('Ctrl Pts',(-1.74815132669517,-6.53968633180688,
51.719733972134));
#196440=CARTESIAN_POINT('Ctrl Pts',(-1.57626100065361,-6.58085786640454,
51.7280315598203));
#196441=CARTESIAN_POINT('Ctrl Pts',(-1.40437866888195,-6.62202748619776,
51.7363287616027));
#196442=CARTESIAN_POINT('Ctrl Pts',(-1.23087516493557,-6.65646064218201,
51.7446259633851));
#196443=CARTESIAN_POINT('Ctrl Pts',(-1.05631309820776,-6.68404754909439,
51.7529231651675));
#196444=CARTESIAN_POINT('Ctrl Pts',(-0.88173014340526,-6.71163775705254,
51.761221359792));
#196445=CARTESIAN_POINT('Ctrl Pts',(-0.706088717132015,-6.73238002983325,
51.7695195544165));
#196446=CARTESIAN_POINT('Ctrl Pts',(-0.529958924265151,-6.74621616453192,
51.7778177490411));
#196447=CARTESIAN_POINT('Ctrl Pts',(-0.353705257260737,-6.76006203034549,
51.7861217798826));
#196448=CARTESIAN_POINT('Ctrl Pts',(-0.176962884594447,-6.76699202522156,
51.7944258107242));
#196449=CARTESIAN_POINT('Ctrl Pts',(-0.00030521600168854,-6.76699999311683,
51.8027298415658));
#196450=CARTESIAN_POINT('Ctrl Pts',(0.176416690181065,-6.76700796390945,
51.8110368919815));
#196451=CARTESIAN_POINT('Ctrl Pts',(0.353053483044433,-6.76008889831693,
51.8193439423972));
#196452=CARTESIAN_POINT('Ctrl Pts',(0.529034250924517,-6.74628873984421,
51.8276509928129));
#196453=CARTESIAN_POINT('Ctrl Pts',(0.705203171946611,-6.73247382667296,
51.8359669248676));
#196454=CARTESIAN_POINT('Ctrl Pts',(0.880714320129311,-6.71176315574064,
51.8442828569222));
#196455=CARTESIAN_POINT('Ctrl Pts',(1.05500328018712,-6.68425441457717,
51.8525987889768));
#196456=CARTESIAN_POINT('Ctrl Pts',(1.18638600029699,-6.66351774118342,
51.8588675151958));
#196457=CARTESIAN_POINT('Ctrl Pts',(1.31707435499131,-6.63891915865807,
51.8651362414147));
#196458=CARTESIAN_POINT('Ctrl Pts',(1.44683147260502,-6.61051947201425,
51.8714049676337));
#196459=CARTESIAN_POINT('Ctrl Pts',(1.62174460077588,-6.57223657762437,
51.879855236357));
#196460=CARTESIAN_POINT('Ctrl Pts',(1.79528584323523,-6.52697470531072,
51.8883055050804));
#196461=CARTESIAN_POINT('Ctrl Pts',(1.96687850332887,-6.4748496471457,51.8967557738037));
#196462=CARTESIAN_POINT('Ctrl Pts',(2.13831972707799,-6.42277059111307,
51.9051985848782));
#196463=CARTESIAN_POINT('Ctrl Pts',(2.30781548032498,-6.36384051783906,
51.9136413959527));
#196464=CARTESIAN_POINT('Ctrl Pts',(2.4748009504396,-6.29822588160374,51.9220842070271));
#196465=CARTESIAN_POINT('Ctrl Pts',(2.64166178571239,-6.23266021890968,
51.9305207165448));
#196466=CARTESIAN_POINT('Ctrl Pts',(2.80601576522364,-6.16042005987778,
51.9389572260625));
#196467=CARTESIAN_POINT('Ctrl Pts',(2.96731452036559,-6.0817212643484,51.9473937355802));
#196468=CARTESIAN_POINT('Ctrl Pts',(3.12849785756989,-6.00307878204146,
51.9558242083215));
#196469=CARTESIAN_POINT('Ctrl Pts',(3.28663003380628,-5.91798702661201,
51.9642546810627));
#196470=CARTESIAN_POINT('Ctrl Pts',(3.44118371426143,-5.8267095040599,51.9726851538039));
#196471=CARTESIAN_POINT('Ctrl Pts',(3.59567095250719,-5.73547122146796,
51.9811120023077));
#196472=CARTESIAN_POINT('Ctrl Pts',(3.74658247681241,-5.63805264135766,
51.9895388508115));
#196473=CARTESIAN_POINT('Ctrl Pts',(3.89341599374254,-5.53476294882354,
51.9979656993153));
#196474=CARTESIAN_POINT('Ctrl Pts',(4.04020418841084,-5.43150513812803,
52.0063899467519));
#196475=CARTESIAN_POINT('Ctrl Pts',(4.18291661503389,-5.32238001952461,
52.0148141941886));
#196476=CARTESIAN_POINT('Ctrl Pts',(4.32108008899238,-5.20773999586323,
52.0232384416253));
#196477=CARTESIAN_POINT('Ctrl Pts',(4.36000926974064,-5.17543882338809,
52.0256120722364));
#196478=CARTESIAN_POINT('Ctrl Pts',(4.39857749904668,-5.14270007998872,
52.0279857028475));
#196479=CARTESIAN_POINT('Ctrl Pts',(4.4367746488298,-5.10953224038182,52.0303593334587));
#196480=CARTESIAN_POINT('Ctrl Pts',(4.57547056253417,-4.98909802353581,
52.038978114396));
#196481=CARTESIAN_POINT('Ctrl Pts',(4.70920929362458,-4.86305725438358,
52.0475968953332));
#196482=CARTESIAN_POINT('Ctrl Pts',(4.83755419002768,-4.73184514312817,
52.0562156762705));
#196483=CARTESIAN_POINT('Ctrl Pts',(4.96597618242891,-4.60055421355612,
52.064839634457));
#196484=CARTESIAN_POINT('Ctrl Pts',(5.08899766130541,-4.4640859599079,52.0734635926436));
#196485=CARTESIAN_POINT('Ctrl Pts',(5.20622052148926,-4.32291069554116,
52.0820875508301));
#196486=CARTESIAN_POINT('Ctrl Pts',(5.32767824365046,-4.17663525055887,
52.0910230632012));
#196487=CARTESIAN_POINT('Ctrl Pts',(5.44291034106364,-4.02530663931312,
52.0999585755723));
#196488=CARTESIAN_POINT('Ctrl Pts',(5.5515216575626,-3.86948268966453,52.1088940879434));
#196489=CARTESIAN_POINT('Ctrl Pts',(5.65654201121118,-3.71881067107087,
52.1175341698381));
#196490=CARTESIAN_POINT('Ctrl Pts',(5.75537225130303,-3.5639360925001,52.1261742517328));
#196491=CARTESIAN_POINT('Ctrl Pts',(5.84770073397215,-3.40539059814019,
52.1348143336276));
#196492=CARTESIAN_POINT('Ctrl Pts',(5.94476470085616,-3.23871338034912,
52.1438975612369));
#196493=CARTESIAN_POINT('Ctrl Pts',(6.03464226453751,-3.06797914483941,
52.1529807888462));
#196494=CARTESIAN_POINT('Ctrl Pts',(6.11702720501719,-2.89383260972013,
52.1620640164555));
#196495=CARTESIAN_POINT('Ctrl Pts',(6.19941214549684,-2.71968607460092,
52.1711472440648));
#196496=CARTESIAN_POINT('Ctrl Pts',(6.27430434308154,-2.54212761024528,
52.1802304716741));
#196497=CARTESIAN_POINT('Ctrl Pts',(6.34145688008563,-2.36182421827169,
52.1893136992833));
#196498=CARTESIAN_POINT('Ctrl Pts',(6.40832380417191,-2.18228769200666,
52.1983582941431));
#196499=CARTESIAN_POINT('Ctrl Pts',(6.4675793353938,-1.99986404640702,52.2074028890029));
#196500=CARTESIAN_POINT('Ctrl Pts',(6.51900169662694,-1.81518756038461,
52.2164474838627));
#196501=CARTESIAN_POINT('Ctrl Pts',(6.57037686974953,-1.63068054410709,
52.2254837788831));
#196502=CARTESIAN_POINT('Ctrl Pts',(6.61393316033545,-1.44392504383055,
52.2345200739034));
#196503=CARTESIAN_POINT('Ctrl Pts',(6.64949862910018,-1.25557038098021,
52.2435563689238));
#196504=CARTESIAN_POINT('Ctrl Pts',(6.68500116197888,-1.06754902647664,
52.2525766735114));
#196505=CARTESIAN_POINT('Ctrl Pts',(6.71254106550225,-0.877934393694752,
52.2615969780991));
#196506=CARTESIAN_POINT('Ctrl Pts',(6.73199746713134,-0.687385701434986,
52.2706172826868));
#196507=CARTESIAN_POINT('Ctrl Pts',(6.75142936720212,-0.497076968237626,
52.2796262279531));
#196508=CARTESIAN_POINT('Ctrl Pts',(6.76279805626797,-0.305836758941343,
52.2886351732194));
#196509=CARTESIAN_POINT('Ctrl Pts',(6.7660340872941,-0.11433166479313,52.2976441184858));
#196510=CARTESIAN_POINT('Ctrl Pts',(6.76926276997881,0.076738561826771,
52.3066326063445));
#196511=CARTESIAN_POINT('Ctrl Pts',(6.76439565342507,0.268072235237285,
52.3156210942033));
#196512=CARTESIAN_POINT('Ctrl Pts',(6.75141519215947,0.459000983744335,
52.324609582062));
#196513=CARTESIAN_POINT('Ctrl Pts',(6.74002662389274,0.626514683139328,
52.3324957430774));
#196514=CARTESIAN_POINT('Ctrl Pts',(6.72239343122672,0.793716490812133,
52.3403819040927));
#196515=CARTESIAN_POINT('Ctrl Pts',(6.69853677078782,0.960153180697496,
52.3482680651081));
#196516=CARTESIAN_POINT('Ctrl Pts',(6.67396828569565,1.13155593611291,52.3563895299643));
#196517=CARTESIAN_POINT('Ctrl Pts',(6.64280878500894,1.30207027473601,52.3645109948204));
#196518=CARTESIAN_POINT('Ctrl Pts',(6.6051497495303,1.47115117723498,52.3726324596766));
#196519=CARTESIAN_POINT('Ctrl Pts',(6.5674933996951,1.64022002177731,52.3807533453528));
#196520=CARTESIAN_POINT('Ctrl Pts',(6.52333851792854,1.80785527638499,52.388874231029));
#196521=CARTESIAN_POINT('Ctrl Pts',(6.47282754051543,1.97352289845976,52.3969951167052));
#196522=CARTESIAN_POINT('Ctrl Pts',(6.42231052559608,2.13921032255288,52.4051169730595));
#196523=CARTESIAN_POINT('Ctrl Pts',(6.36543601016475,2.30292929588791,52.4132388294138));
#196524=CARTESIAN_POINT('Ctrl Pts',(6.30239604248319,2.46416174868702,52.4213606857681));
#196525=CARTESIAN_POINT('Ctrl Pts',(6.23931008162123,2.62551183468867,52.4294884677282));
#196526=CARTESIAN_POINT('Ctrl Pts',(6.17004981778485,2.78437143543766,52.4376162496884));
#196527=CARTESIAN_POINT('Ctrl Pts',(6.09485537691689,2.94024266591507,52.4457440316486));
#196528=CARTESIAN_POINT('Ctrl Pts',(6.01963030462878,3.09617739253786,52.453875124565));
#196529=CARTESIAN_POINT('Ctrl Pts',(5.93846640835912,3.24912099913245,52.4620062174814));
#196530=CARTESIAN_POINT('Ctrl Pts',(5.85164924493249,3.39860119965275,52.4701373103979));
#196531=CARTESIAN_POINT('Ctrl Pts',(5.7647373242001,3.54824455156507,52.4782772780624));
#196532=CARTESIAN_POINT('Ctrl Pts',(5.67216000784978,3.69441663817258,52.486417245727));
#196533=CARTESIAN_POINT('Ctrl Pts',(5.5742459600096,3.83667446851002,52.4945572133915));
#196534=CARTESIAN_POINT('Ctrl Pts',(5.52346350126786,3.91045553015699,52.498778952572));
#196535=CARTESIAN_POINT('Ctrl Pts',(5.47124618168525,3.983184225787,52.5030006917524));
#196536=CARTESIAN_POINT('Ctrl Pts',(5.41764399782902,4.05480240120122,52.5072224309329));
#196537=CARTESIAN_POINT('Ctrl Pts',(5.31047721113774,4.19798853981865,52.5156629493907));
#196538=CARTESIAN_POINT('Ctrl Pts',(5.1975510084198,4.33702963227614,52.5241034678485));
#196539=CARTESIAN_POINT('Ctrl Pts',(5.079212594634,4.47145260720847,52.5325439863063));
#196540=CARTESIAN_POINT('Ctrl Pts',(4.96096191138293,4.60577592726885,52.5409782473607));
#196541=CARTESIAN_POINT('Ctrl Pts',(4.83730723448576,4.73548770469269,52.5494125084151));
#196542=CARTESIAN_POINT('Ctrl Pts',(4.70863665742514,4.86014709945618,52.5578467694695));
#196543=CARTESIAN_POINT('Ctrl Pts',(4.58005485344859,4.98472048855166,52.5662752115139));
#196544=CARTESIAN_POINT('Ctrl Pts',(4.4464642901457,5.10424821561085,52.5747036535584));
#196545=CARTESIAN_POINT('Ctrl Pts',(4.30829074449172,5.21832538856356,52.5831320956028));
#196546=CARTESIAN_POINT('Ctrl Pts',(4.17017545649127,5.33235446353639,52.5915569839912));
#196547=CARTESIAN_POINT('Ctrl Pts',(4.02748129480552,5.44093735359852,52.5999818723796));
#196548=CARTESIAN_POINT('Ctrl Pts',(3.8806684656216,5.54370825891209,52.608406760768));
#196549=CARTESIAN_POINT('Ctrl Pts',(3.73389156471692,5.64645401395913,52.6168295874037));
#196550=CARTESIAN_POINT('Ctrl Pts',(3.58299827789504,5.74339042764865,52.6252524140394));
#196551=CARTESIAN_POINT('Ctrl Pts',(3.42847960027908,5.83419374296656,52.6336752406752));
#196552=CARTESIAN_POINT('Ctrl Pts',(3.32040276338655,5.897705386027,52.6395665185098));
#196553=CARTESIAN_POINT('Ctrl Pts',(3.21055297173536,5.95821747173756,52.6454577963445));
#196554=CARTESIAN_POINT('Ctrl Pts',(3.09910619832128,6.01563211736943,52.6513490741792));
#196555=CARTESIAN_POINT('Origin',(0.,0.,4.30282021618968));
#196556=CARTESIAN_POINT('',(3.09910619832139,6.01563211736937,55.0459882871872));
#196557=CARTESIAN_POINT('',(3.09910619832136,6.01563211736939,54.6512861468277));
#196558=CARTESIAN_POINT('',(3.09910619832133,6.0156321173694,4.30282021618968));
#196559=CARTESIAN_POINT('',(-6.7669990509716,-0.00358387352824917,53.6971797838396));
#196560=CARTESIAN_POINT('Ctrl Pts',(-6.7669990509716,-0.00358387352833798,
53.6971797838396));
#196561=CARTESIAN_POINT('Ctrl Pts',(-6.76689217047806,-0.20539350566186,
53.706683992129));
#196562=CARTESIAN_POINT('Ctrl Pts',(-6.75775334083001,-0.407019112576732,
53.7161882004184));
#196563=CARTESIAN_POINT('Ctrl Pts',(-6.73965675319555,-0.607713624255395,
53.7256924087078));
#196564=CARTESIAN_POINT('Ctrl Pts',(-6.7215721742797,-0.808274957018417,
53.7351903100976));
#196565=CARTESIAN_POINT('Ctrl Pts',(-6.69454179296501,-1.00790630788709,
53.7446882114873));
#196566=CARTESIAN_POINT('Ctrl Pts',(-6.6586905907916,-1.20587255383953,
53.754186112877));
#196567=CARTESIAN_POINT('Ctrl Pts',(-6.62455045966254,-1.39439046080544,
53.7632307077369));
#196568=CARTESIAN_POINT('Ctrl Pts',(-6.58239146852269,-1.58150599709402,
53.7722753025967));
#196569=CARTESIAN_POINT('Ctrl Pts',(-6.53234666004299,-1.76656053194482,
53.7813198974565));
#196570=CARTESIAN_POINT('Ctrl Pts',(-6.48234777555245,-1.95144525013112,
53.7903561924769));
#196571=CARTESIAN_POINT('Ctrl Pts',(-6.42447758343751,-2.13427251340943,
53.7993924874972));
#196572=CARTESIAN_POINT('Ctrl Pts',(-6.35891966107565,-2.31439619425575,
53.8084287825176));
#196573=CARTESIAN_POINT('Ctrl Pts',(-6.29347774859843,-2.49420113212362,
53.8174490871053));
#196574=CARTESIAN_POINT('Ctrl Pts',(-6.22037535266763,-2.67131181774264,
53.826469391693));
#196575=CARTESIAN_POINT('Ctrl Pts',(-6.13984501590862,-2.84509967850374,
53.8354896962807));
#196576=CARTESIAN_POINT('Ctrl Pts',(-6.05941609146528,-3.01866868721349,
53.844498641547));
#196577=CARTESIAN_POINT('Ctrl Pts',(-5.97157799337865,-3.18892300659289,
53.8535075868134));
#196578=CARTESIAN_POINT('Ctrl Pts',(-5.87661124923286,-3.35525397330661,
53.8625165320797));
#196579=CARTESIAN_POINT('Ctrl Pts',(-5.78186015445875,-3.52120723760687,
53.8715050199385));
#196580=CARTESIAN_POINT('Ctrl Pts',(-5.68001284330018,-3.68325472636994,
53.8804935077973));
#196581=CARTESIAN_POINT('Ctrl Pts',(-5.57139538336093,-3.84081273720349,
53.8894819956561));
#196582=CARTESIAN_POINT('Ctrl Pts',(-5.476098511228,-3.97904820708394,53.8973681566713));
#196583=CARTESIAN_POINT('Ctrl Pts',(-5.37559095502018,-4.11382804651479,
53.9052543176866));
#196584=CARTESIAN_POINT('Ctrl Pts',(-5.27012224682619,-4.24477331591543,
53.9131404787018));
#196585=CARTESIAN_POINT('Ctrl Pts',(-5.16150660920894,-4.37962567328717,
53.921261943558));
#196586=CARTESIAN_POINT('Ctrl Pts',(-5.04767669280879,-4.51034982672275,
53.9293834084142));
#196587=CARTESIAN_POINT('Ctrl Pts',(-4.92898935674534,-4.63652379710179,
53.9375048732703));
#196588=CARTESIAN_POINT('Ctrl Pts',(-4.81031048483593,-4.76268876941956,
53.9456257589465));
#196589=CARTESIAN_POINT('Ctrl Pts',(-4.68677513415301,-4.88430393830359,
53.9537466446227));
#196590=CARTESIAN_POINT('Ctrl Pts',(-4.55877837866638,-5.00098277283615,
53.9618675302989));
#196591=CARTESIAN_POINT('Ctrl Pts',(-4.43076632390726,-5.11767555382599,
53.9699893866532));
#196592=CARTESIAN_POINT('Ctrl Pts',(-4.29829207391614,-5.22943057977352,
53.9781112430074));
#196593=CARTESIAN_POINT('Ctrl Pts',(-4.16178521206458,-5.33590037844042,
53.9862330993617));
#196594=CARTESIAN_POINT('Ctrl Pts',(-4.02517875649533,-5.44244785615529,
53.9943608813218));
#196595=CARTESIAN_POINT('Ctrl Pts',(-3.88453410184469,-5.54370217959386,
54.002488663282));
#196596=CARTESIAN_POINT('Ctrl Pts',(-3.74031187162378,-5.63935777398368,
54.0106164452422));
#196597=CARTESIAN_POINT('Ctrl Pts',(-3.59603089062665,-5.7350523349074,
54.0187475381586));
#196598=CARTESIAN_POINT('Ctrl Pts',(-3.44816974160194,-5.82514343027827,
54.0268786310751));
#196599=CARTESIAN_POINT('Ctrl Pts',(-3.2972150485986,-5.90937068758552,
54.0350097239916));
#196600=CARTESIAN_POINT('Ctrl Pts',(-3.1460955948567,-5.99368987542401,
54.0431496916561));
#196601=CARTESIAN_POINT('Ctrl Pts',(-2.99187617918848,-6.07213227618284,
54.0512896593206));
#196602=CARTESIAN_POINT('Ctrl Pts',(-2.83506554149222,-6.14448471195457,
54.0594296269852));
#196603=CARTESIAN_POINT('Ctrl Pts',(-2.75373676472572,-6.18200981346452,
54.0636513661657));
#196604=CARTESIAN_POINT('Ctrl Pts',(-2.67171127792406,-6.21789757109083,
54.0678731053461));
#196605=CARTESIAN_POINT('Ctrl Pts',(-2.58906175767844,-6.25212349645519,
54.0720948445266));
#196606=CARTESIAN_POINT('Ctrl Pts',(-2.42382671291955,-6.32054884596341,
54.0805350539842));
#196607=CARTESIAN_POINT('Ctrl Pts',(-2.25575498027963,-6.3824704961414,
54.0889752634419));
#196608=CARTESIAN_POINT('Ctrl Pts',(-2.08538653745964,-6.43765889041833,
54.0974154728995));
#196609=CARTESIAN_POINT('Ctrl Pts',(-1.91514717397523,-6.49280547131041,
54.105849287648));
#196610=CARTESIAN_POINT('Ctrl Pts',(-1.74261488519324,-6.54122886327688,
54.1142831023966));
#196611=CARTESIAN_POINT('Ctrl Pts',(-1.56834832785497,-6.58274809806015,
54.1227169171451));
#196612=CARTESIAN_POINT('Ctrl Pts',(-1.39418701379491,-6.624242258495,54.1311456385336));
#196613=CARTESIAN_POINT('Ctrl Pts',(-1.21829384283528,-6.65884049728079,
54.1395743599222));
#196614=CARTESIAN_POINT('Ctrl Pts',(-1.04124167351343,-6.686411950915,54.1480030813107));
#196615=CARTESIAN_POINT('Ctrl Pts',(-0.864269241991779,-6.71397098737822,
54.1564280067125));
#196616=CARTESIAN_POINT('Ctrl Pts',(-0.686139181822217,-6.73450949732994,
54.1648529321142));
#196617=CARTESIAN_POINT('Ctrl Pts',(-0.507433955419252,-6.74794781995886,
54.1732778575159));
#196618=CARTESIAN_POINT('Ctrl Pts',(-0.328781792614159,-6.7613821522974,
54.1817002812736));
#196619=CARTESIAN_POINT('Ctrl Pts',(-0.149555136351088,-6.76772047671474,
54.1901227050314));
#196620=CARTESIAN_POINT('Ctrl Pts',(0.0296586264785453,-6.76693500529416,
54.1985451287891));
#196621=CARTESIAN_POINT('Ctrl Pts',(0.208875207824346,-6.76614952152037,
54.2069676850073));
#196622=CARTESIAN_POINT('Ctrl Pts',(0.388078561905396,-6.75824001286657,
54.2153902412255));
#196623=CARTESIAN_POINT('Ctrl Pts',(0.56668081765754,-6.74323081696741,
54.2238127974437));
#196624=CARTESIAN_POINT('Ctrl Pts',(0.745289106627769,-6.72822111405477,
54.2322356381774));
#196625=CARTESIAN_POINT('Ctrl Pts',(0.923295924362521,-6.70611127346617,
54.2406584789112));
#196626=CARTESIAN_POINT('Ctrl Pts',(1.10011788045682,-6.6769775833905,54.2490813196449));
#196627=CARTESIAN_POINT('Ctrl Pts',(1.27697049593126,-6.64783884178787,
54.2575056208255));
#196628=CARTESIAN_POINT('Ctrl Pts',(1.45263751104816,-6.61167387684255,
54.2659299220062));
#196629=CARTESIAN_POINT('Ctrl Pts',(1.62654472881587,-6.56861029786068,
54.2743542231868));
#196630=CARTESIAN_POINT('Ctrl Pts',(1.80050638738515,-6.52553323803661,
54.2827811615536));
#196631=CARTESIAN_POINT('Ctrl Pts',(1.97270682661158,-6.47555333871034,
54.2912080999204));
#196632=CARTESIAN_POINT('Ctrl Pts',(2.14258567628876,-6.41884846524377,
54.2996350382872));
#196633=CARTESIAN_POINT('Ctrl Pts',(2.31261726840537,-6.36209260696821,
54.3080695535309));
#196634=CARTESIAN_POINT('Ctrl Pts',(2.48032278330943,-6.29859979820912,
54.3165040687745));
#196635=CARTESIAN_POINT('Ctrl Pts',(2.64515947001497,-6.2285969831247,54.3249385840182));
#196636=CARTESIAN_POINT('Ctrl Pts',(2.8100757742525,-6.15856035608082,54.333377173205));
#196637=CARTESIAN_POINT('Ctrl Pts',(2.97212018312097,-6.08200758935251,
54.3418157623917));
#196638=CARTESIAN_POINT('Ctrl Pts',(3.13077285188469,-5.99921247747584,
54.3502543515785));
#196639=CARTESIAN_POINT('Ctrl Pts',(3.28960285843758,-5.91632481939614,
54.3587023731988));
#196640=CARTESIAN_POINT('Ctrl Pts',(3.4450332575324,-5.82718103540334,54.3671503948191));
#196641=CARTESIAN_POINT('Ctrl Pts',(3.59657053059673,-5.73209991350841,
54.3755984164394));
#196642=CARTESIAN_POINT('Ctrl Pts',(3.68270188468435,-5.6780573297178,54.3804001363516));
#196643=CARTESIAN_POINT('Ctrl Pts',(3.76757605959588,-5.62209741664671,
54.3852018562638));
#196644=CARTESIAN_POINT('Ctrl Pts',(3.85110698088934,-5.56428468194659,
54.3900035761761));
#196645=CARTESIAN_POINT('Ctrl Pts',(3.99444222307462,-5.465080672206,54.3982431080269));
#196646=CARTESIAN_POINT('Ctrl Pts',(4.13414038505795,-5.36019723159368,
54.4064826398777));
#196647=CARTESIAN_POINT('Ctrl Pts',(4.26972379138673,-5.24992835620318,
54.4147221717285));
#196648=CARTESIAN_POINT('Ctrl Pts',(4.4051567096104,-5.13978187155767,54.4229525582748));
#196649=CARTESIAN_POINT('Ctrl Pts',(4.53648369234045,-5.02426207683795,
54.4311829448211));
#196650=CARTESIAN_POINT('Ctrl Pts',(4.6632554213212,-4.90370654459649,54.4394133313674));
#196651=CARTESIAN_POINT('Ctrl Pts',(4.78990905745408,-4.78326331457134,
54.4476360509852));
#196652=CARTESIAN_POINT('Ctrl Pts',(4.91201563424525,-4.65779393302532,
54.455858770603));
#196653=CARTESIAN_POINT('Ctrl Pts',(5.02915830110851,-4.52767664287009,
54.4640814902208));
#196654=CARTESIAN_POINT('Ctrl Pts',(5.14619717112908,-4.39767464600858,
54.4722969239166));
#196655=CARTESIAN_POINT('Ctrl Pts',(5.25828066038809,-4.26303321235824,
54.4805123576123));
#196656=CARTESIAN_POINT('Ctrl Pts',(5.36502833791073,-4.124167786768,54.4887277913081));
#196657=CARTESIAN_POINT('Ctrl Pts',(5.47172115541633,-3.98537372722328,
54.4969390029089));
#196658=CARTESIAN_POINT('Ctrl Pts',(5.57308340612662,-3.84236028056674,
54.5051502145097));
#196659=CARTESIAN_POINT('Ctrl Pts',(5.66877430356654,-3.69557666612719,
54.5133614261105));
#196660=CARTESIAN_POINT('Ctrl Pts',(5.76443311155956,-3.54884227481258,
54.521569884124));
#196661=CARTESIAN_POINT('Ctrl Pts',(5.85442416079166,-3.39834053214902,
54.5297783421375));
#196662=CARTESIAN_POINT('Ctrl Pts',(5.93844940206025,-3.24455046180056,
54.537986800151));
#196663=CARTESIAN_POINT('Ctrl Pts',(5.9758844818036,-3.17603362733142,54.5416438474343));
#196664=CARTESIAN_POINT('Ctrl Pts',(6.01213599114525,-3.10686446862793,
54.5453008947176));
#196665=CARTESIAN_POINT('Ctrl Pts',(6.04718044105717,-3.03708704407623,
54.5489579420008));
#196666=CARTESIAN_POINT('Ctrl Pts',(6.13207444356175,-2.86805357744901,
54.5578170161767));
#196667=CARTESIAN_POINT('Ctrl Pts',(6.20979382233589,-2.69562484029854,
54.5666760903526));
#196668=CARTESIAN_POINT('Ctrl Pts',(6.28011180328,-2.52041360461001,54.5755351645285));
#196669=CARTESIAN_POINT('Ctrl Pts',(6.35056189756314,-2.34487318226009,
54.5844108831225));
#196670=CARTESIAN_POINT('Ctrl Pts',(6.41358270765095,-2.16654005458681,
54.5932866017164));
#196671=CARTESIAN_POINT('Ctrl Pts',(6.46899702095665,-1.98604293580326,
54.6021623203104));
#196672=CARTESIAN_POINT('Ctrl Pts',(6.52456947105544,-1.80503072924141,
54.6110633676974));
#196673=CARTESIAN_POINT('Ctrl Pts',(6.57249190950509,-1.62184242307575,
54.6199644150844));
#196674=CARTESIAN_POINT('Ctrl Pts',(6.61263736242461,-1.43712077191382,
54.6288654624714));
#196675=CARTESIAN_POINT('Ctrl Pts',(6.65283739363802,-1.25214798913337,
54.6377786109544));
#196676=CARTESIAN_POINT('Ctrl Pts',(6.68523927058451,-1.06563795189312,
54.6466917594375));
#196677=CARTESIAN_POINT('Ctrl Pts',(6.70976766854178,-0.878240760948553,
54.6556049079205));
#196678=CARTESIAN_POINT('Ctrl Pts',(6.73435052624963,-0.690427496997583,
54.6645378460304));
#196679=CARTESIAN_POINT('Ctrl Pts',(6.7510249054307,-0.501723397634979,
54.6734707841403));
#196680=CARTESIAN_POINT('Ctrl Pts',(6.75976740416614,-0.312783697741695,
54.6824037222502));
#196681=CARTESIAN_POINT('Ctrl Pts',(6.76808899535266,-0.132940498561066,
54.6909065841087));
#196682=CARTESIAN_POINT('Ctrl Pts',(6.76922448270502,0.0471159652347299,
54.6994094459671));
#196683=CARTESIAN_POINT('Ctrl Pts',(6.76319748642104,0.226823190322631,
54.7079123078255));
#196684=CARTESIAN_POINT('Ctrl Pts',(6.75736905747454,0.400609723986583,
54.7161350316914));
#196685=CARTESIAN_POINT('Ctrl Pts',(6.74483016277144,0.574402702958768,
54.7243577555573));
#196686=CARTESIAN_POINT('Ctrl Pts',(6.72557191694189,0.747643892533494,
54.7325804794232));
#196687=CARTESIAN_POINT('Ctrl Pts',(6.70633405531315,0.920701712177786,
54.7407944998144));
#196688=CARTESIAN_POINT('Ctrl Pts',(6.68039104454674,1.0932085518923,54.7490085202056));
#196689=CARTESIAN_POINT('Ctrl Pts',(6.64778599689748,1.26460679242751,54.7572225405969));
#196690=CARTESIAN_POINT('Ctrl Pts',(6.61520891441485,1.43585802565241,54.7654295158688));
#196691=CARTESIAN_POINT('Ctrl Pts',(6.57598124161398,1.60600220296919,54.7736364911408));
#196692=CARTESIAN_POINT('Ctrl Pts',(6.53019782579279,1.77448735019755,54.7818434664128));
#196693=CARTESIAN_POINT('Ctrl Pts',(6.48444448876211,1.9428618060466,54.7900450498658));
#196694=CARTESIAN_POINT('Ctrl Pts',(6.43214408145211,2.10957905792641,54.7982466333188));
#196695=CARTESIAN_POINT('Ctrl Pts',(6.37344242884872,2.27409775650718,54.8064482167718));
#196696=CARTESIAN_POINT('Ctrl Pts',(6.31476756220602,2.43854138409422,54.8146460577868));
#196697=CARTESIAN_POINT('Ctrl Pts',(6.24969738978208,2.60078811986705,54.8228438988019));
#196698=CARTESIAN_POINT('Ctrl Pts',(6.17842746963303,2.76031212048275,54.8310417398169));
#196699=CARTESIAN_POINT('Ctrl Pts',(6.10716383883211,2.91982204360303,54.8392388573981));
#196700=CARTESIAN_POINT('Ctrl Pts',(6.02970168845473,3.07660937938224,54.8474359749792));
#196701=CARTESIAN_POINT('Ctrl Pts',(5.94628471634663,3.23016827303818,54.8556330925604));
#196702=CARTESIAN_POINT('Ctrl Pts',(5.86286867234528,3.38372545818037,54.8638301189395));
#196703=CARTESIAN_POINT('Ctrl Pts',(5.77349810891769,3.53405395691857,54.8720271453186));
#196704=CARTESIAN_POINT('Ctrl Pts',(5.67846262915169,3.68067265174828,54.8802241716977));
#196705=CARTESIAN_POINT('Ctrl Pts',(5.58341092642758,3.82731637500895,54.8884225973438));
#196706=CARTESIAN_POINT('Ctrl Pts',(5.48269257594397,3.97024873156114,54.89662102299));
#196707=CARTESIAN_POINT('Ctrl Pts',(5.37664046332861,4.10901768408187,54.9048194486361));
#196708=CARTESIAN_POINT('Ctrl Pts',(5.27055096346976,4.24783555772722,54.9130207645268));
#196709=CARTESIAN_POINT('Ctrl Pts',(5.15912417356631,4.38248681863195,54.9212220804174));
#196710=CARTESIAN_POINT('Ctrl Pts',(5.04273321860242,4.51255256878009,54.9294233963081));
#196711=CARTESIAN_POINT('Ctrl Pts',(4.926209713824,4.64276644204537,54.9376340521247));
#196712=CARTESIAN_POINT('Ctrl Pts',(4.80471098912698,4.76838410399211,54.9458447079413));
#196713=CARTESIAN_POINT('Ctrl Pts',(4.67864772972981,4.88902284931193,54.9540553637579));
#196714=CARTESIAN_POINT('Ctrl Pts',(4.55251018430802,5.00973268412164,54.962270857915));
#196715=CARTESIAN_POINT('Ctrl Pts',(4.42180301076258,5.12545751644231,54.9704863520722));
#196716=CARTESIAN_POINT('Ctrl Pts',(4.28696981949483,5.23585511323036,54.9787018462293));
#196717=CARTESIAN_POINT('Ctrl Pts',(4.15192743204966,5.34642399392132,54.9869300868768));
#196718=CARTESIAN_POINT('Ctrl Pts',(4.01274652002538,5.45164890548821,54.9951583275243));
#196719=CARTESIAN_POINT('Ctrl Pts',(3.86990059370619,5.55123034964615,55.0033865681719));
#196720=CARTESIAN_POINT('Ctrl Pts',(3.74007645218726,5.64173398410144,55.010864725273));
#196721=CARTESIAN_POINT('Ctrl Pts',(3.60722555703865,5.72757662318511,55.0183428823742));
#196722=CARTESIAN_POINT('Ctrl Pts',(3.47171995776768,5.80856690887155,55.0258210394753));
#196723=CARTESIAN_POINT('Ctrl Pts',(3.34990852972529,5.88137233100985,55.0325434553793));
#196724=CARTESIAN_POINT('Ctrl Pts',(3.2256199413191,5.95045533836307,55.0392658712833));
#196725=CARTESIAN_POINT('Ctrl Pts',(3.09910619832139,6.01563211736937,55.0459882871872));
#196726=CARTESIAN_POINT('Ctrl Pts',(3.09910619832131,6.01563211736941,53.0454129677962));
#196727=CARTESIAN_POINT('Ctrl Pts',(2.94667468855627,6.09416109446034,53.0534680607862));
#196728=CARTESIAN_POINT('Ctrl Pts',(2.79140784790711,6.16681448736431,53.0615231537762));
#196729=CARTESIAN_POINT('Ctrl Pts',(2.63381441570988,6.23340281255743,53.0695782467662));
#196730=CARTESIAN_POINT('Ctrl Pts',(2.47472154848197,6.30062469757621,53.0777099805681));
#196731=CARTESIAN_POINT('Ctrl Pts',(2.31325796192262,6.36166538924136,53.0858417143701));
#196732=CARTESIAN_POINT('Ctrl Pts',(2.14996064585907,6.41638201958528,53.093973448172));
#196733=CARTESIAN_POINT('Ctrl Pts',(1.98666332979558,6.47109864992918,53.102105181974));
#196734=CARTESIAN_POINT('Ctrl Pts',(1.82153267172137,6.51949118168162,53.1102369157759));
#196735=CARTESIAN_POINT('Ctrl Pts',(1.65511355105797,6.56146996740092,53.1183686495779));
#196736=CARTESIAN_POINT('Ctrl Pts',(1.48457703408077,6.60448735551693,53.1267015716246));
#196737=CARTESIAN_POINT('Ctrl Pts',(1.31214340187037,6.64090728948818,53.1350344936713));
#196738=CARTESIAN_POINT('Ctrl Pts',(1.13835793945825,6.67056445899988,53.143367415718));
#196739=CARTESIAN_POINT('Ctrl Pts',(0.964777849319081,6.70018658092919,
53.1516904902716));
#196740=CARTESIAN_POINT('Ctrl Pts',(0.789849451455171,6.72306180095026,
53.1600135648252));
#196741=CARTESIAN_POINT('Ctrl Pts',(0.614131739318328,6.73907495185815,
53.1683366393788));
#196742=CARTESIAN_POINT('Ctrl Pts',(0.43858942891076,6.75507211841063,53.1766514058248));
#196743=CARTESIAN_POINT('Ctrl Pts',(0.262259718327668,6.76422083133051,
53.1849661722708));
#196744=CARTESIAN_POINT('Ctrl Pts',(0.0857105364293527,6.76645717520957,
53.1932809387167));
#196745=CARTESIAN_POINT('Ctrl Pts',(-0.090694798828944,6.76869169698699,
53.2015889305563));
#196746=CARTESIAN_POINT('Ctrl Pts',(-0.267318902673587,6.76402506751749,
53.2098969223959));
#196747=CARTESIAN_POINT('Ctrl Pts',(-0.443589768131856,6.75244526950117,
53.2182049142354));
#196748=CARTESIAN_POINT('Ctrl Pts',(-0.619749330088323,6.74087278336857,
53.2265076601225));
#196749=CARTESIAN_POINT('Ctrl Pts',(-0.795555751944949,6.72239585078345,
53.2348104060096));
#196750=CARTESIAN_POINT('Ctrl Pts',(-0.970437845322777,6.69705453078929,
53.2431131518967));
#196751=CARTESIAN_POINT('Ctrl Pts',(-1.1452484699622,6.67172356698502,53.2514125047161));
#196752=CARTESIAN_POINT('Ctrl Pts',(-1.31913517501728,6.6395338552691,53.2597118575355));
#196753=CARTESIAN_POINT('Ctrl Pts',(-1.49153241476046,6.60057725170449,
53.268011210355));
#196754=CARTESIAN_POINT('Ctrl Pts',(-1.66389298850354,6.56162893355578,
53.2763087980413));
#196755=CARTESIAN_POINT('Ctrl Pts',(-1.83476438888806,6.51591666741649,
53.2846063857276));
#196756=CARTESIAN_POINT('Ctrl Pts',(-2.00359153500685,6.46358336844578,
53.292903973414));
#196757=CARTESIAN_POINT('Ctrl Pts',(-2.17241082931851,6.41125250339035,
53.3012011751964));
#196758=CARTESIAN_POINT('Ctrl Pts',(-2.33918572658764,6.35230132228487,
53.3094983769789));
#196759=CARTESIAN_POINT('Ctrl Pts',(-2.50337638989166,6.28692258983145,
53.3177955787613));
#196760=CARTESIAN_POINT('Ctrl Pts',(-2.66758670022945,6.22153603416727,
53.3260937733858));
#196761=CARTESIAN_POINT('Ctrl Pts',(-2.82921183744743,6.14972052384547,
53.3343919680103));
#196762=CARTESIAN_POINT('Ctrl Pts',(-2.98773184815719,6.07171700621062,
53.3426901626349));
#196763=CARTESIAN_POINT('Ctrl Pts',(-3.14636334783892,5.99365862779225,
53.3509941934764));
#196764=CARTESIAN_POINT('Ctrl Pts',(-3.3018850446668,5.90940369950656,53.359298224318));
#196765=CARTESIAN_POINT('Ctrl Pts',(-3.45380070948755,5.81923961176572,
53.3676022551596));
#196766=CARTESIAN_POINT('Ctrl Pts',(-3.60577161502542,5.72904273788087,
53.3759093055753));
#196767=CARTESIAN_POINT('Ctrl Pts',(-3.75413357969917,5.63293260574036,
53.3842163559911));
#196768=CARTESIAN_POINT('Ctrl Pts',(-3.89841911554349,5.53124013215528,
53.3925234064068));
#196769=CARTESIAN_POINT('Ctrl Pts',(-4.04285891697658,5.42943893215338,
53.4008393384614));
#196770=CARTESIAN_POINT('Ctrl Pts',(-4.18321330120341,5.32204367222528,
53.409155270516));
#196771=CARTESIAN_POINT('Ctrl Pts',(-4.31904677820479,5.20942644901326,
53.4174712025706));
#196772=CARTESIAN_POINT('Ctrl Pts',(-4.42144093836636,5.12453319408754,
53.4237399287896));
#196773=CARTESIAN_POINT('Ctrl Pts',(-4.52126677450329,5.0366734265332,53.4300086550086));
#196774=CARTESIAN_POINT('Ctrl Pts',(-4.61835163230513,4.94602033966547,
53.4362773812276));
#196775=CARTESIAN_POINT('Ctrl Pts',(-4.74922241988468,4.82381960575584,
53.444727649951));
#196776=CARTESIAN_POINT('Ctrl Pts',(-4.87535123190647,4.69631775205162,
53.4531779186743));
#196777=CARTESIAN_POINT('Ctrl Pts',(-4.99630125840441,4.56390871241598,
53.4616281873977));
#196778=CARTESIAN_POINT('Ctrl Pts',(-5.11714454240011,4.43161652825049,
53.4700709984723));
#196779=CARTESIAN_POINT('Ctrl Pts',(-5.23281792802177,4.29442603381313,
53.4785138095468));
#196780=CARTESIAN_POINT('Ctrl Pts',(-5.34292068400844,4.15276866251839,
53.4869566206213));
#196781=CARTESIAN_POINT('Ctrl Pts',(-5.45294126135242,4.01121702164244,
53.4953931301392));
#196782=CARTESIAN_POINT('Ctrl Pts',(-5.55739929461045,3.86520541098306,
53.5038296396571));
#196783=CARTESIAN_POINT('Ctrl Pts',(-5.65593341103666,3.71519935534006,
53.5122661491749));
#196784=CARTESIAN_POINT('Ctrl Pts',(-5.7543970209993,3.56530063710344,53.5206966219162));
#196785=CARTESIAN_POINT('Ctrl Pts',(-5.84694498765805,3.41141345157195,
53.5291270946574));
#196786=CARTESIAN_POINT('Ctrl Pts',(-5.93325834557572,3.25403355923938,
53.5375575673987));
#196787=CARTESIAN_POINT('Ctrl Pts',(-6.01953459761426,3.09672132409688,
53.5459844159025));
#196788=CARTESIAN_POINT('Ctrl Pts',(-6.09958142491096,2.93591966565151,
53.5544112644063));
#196789=CARTESIAN_POINT('Ctrl Pts',(-6.17312471149832,2.77215084298976,
53.5628381129101));
#196790=CARTESIAN_POINT('Ctrl Pts',(-6.24664529789971,2.60843256991455,
53.5712623603468));
#196791=CARTESIAN_POINT('Ctrl Pts',(-6.31366621116775,2.44174926118961,
53.5796866077834));
#196792=CARTESIAN_POINT('Ctrl Pts',(-6.37396042614228,2.27264548180577,
53.5881108552201));
#196793=CARTESIAN_POINT('Ctrl Pts',(-6.39094902902823,2.22499850679036,
53.5904844858308));
#196794=CARTESIAN_POINT('Ctrl Pts',(-6.40740389402233,2.17715949500775,
53.5928581164416));
#196795=CARTESIAN_POINT('Ctrl Pts',(-6.42332063750646,2.12914090369416,
53.5952317470523));
#196796=CARTESIAN_POINT('Ctrl Pts',(-6.48028965164174,1.95727334736727,
53.6037274167821));
#196797=CARTESIAN_POINT('Ctrl Pts',(-6.53034517602241,1.78315182404982,
53.6122230865119));
#196798=CARTESIAN_POINT('Ctrl Pts',(-6.57333051505658,1.60736272814384,
53.6207187562417));
#196799=CARTESIAN_POINT('Ctrl Pts',(-6.61586491693437,1.43341774552887,
53.6291253022555));
#196800=CARTESIAN_POINT('Ctrl Pts',(-6.65147672476766,1.25784034745439,
53.6375318482693));
#196801=CARTESIAN_POINT('Ctrl Pts',(-6.68006557790762,1.08120898759385,
53.6459383942831));
#196802=CARTESIAN_POINT('Ctrl Pts',(-6.70910906690362,0.901768737530553,
53.6544786258709));
#196803=CARTESIAN_POINT('Ctrl Pts',(-6.73090428977837,0.721241075837371,
53.6630188574587));
#196804=CARTESIAN_POINT('Ctrl Pts',(-6.74540079315193,0.540238039891024,
53.6715590890465));
#196805=CARTESIAN_POINT('Ctrl Pts',(-6.7598972965255,0.359235003944613,
53.6800993206344));
#196806=CARTESIAN_POINT('Ctrl Pts',(-6.76709509095542,0.177756954509467,
53.6886395522222));
#196807=CARTESIAN_POINT('Ctrl Pts',(-6.76699905097193,-0.00358387290036924,
53.69717978381));
#196808=CARTESIAN_POINT('',(-6.76699985266004,-0.00141212569560718,53.3028202162272));
#196809=CARTESIAN_POINT('Ctrl Pts',(3.09910619832128,6.01563211736943,52.6513490741792));
#196810=CARTESIAN_POINT('Ctrl Pts',(2.93977317202945,6.09771658658964,52.6597717058748));
#196811=CARTESIAN_POINT('Ctrl Pts',(2.77717512720734,6.17346787802227,52.6681943375703));
#196812=CARTESIAN_POINT('Ctrl Pts',(2.61184631544113,6.24263949179484,52.6766169692659));
#196813=CARTESIAN_POINT('Ctrl Pts',(2.44649577225569,6.31182019773545,52.6850407080628));
#196814=CARTESIAN_POINT('Ctrl Pts',(2.27841405421461,6.37441937296258,52.6934644468596));
#196815=CARTESIAN_POINT('Ctrl Pts',(2.10815503505992,6.43023882512551,52.7018881856565));
#196816=CARTESIAN_POINT('Ctrl Pts',(1.93784986185947,6.48607340890122,52.7103142079719));
#196817=CARTESIAN_POINT('Ctrl Pts',(1.76536652769217,6.53512450156946,52.7187402302873));
#196818=CARTESIAN_POINT('Ctrl Pts',(1.59127404266256,6.57724379365311,52.7271662526027));
#196819=CARTESIAN_POINT('Ctrl Pts',(1.41702699399713,6.61940048029128,52.7355997557501));
#196820=CARTESIAN_POINT('Ctrl Pts',(1.2411682639919,6.65461298874775,52.7440332588976));
#196821=CARTESIAN_POINT('Ctrl Pts',(1.06427821797474,6.68278391650849,52.752466762045));
#196822=CARTESIAN_POINT('Ctrl Pts',(0.887309538935354,6.71096736710609,
52.7609040141419));
#196823=CARTESIAN_POINT('Ctrl Pts',(0.709308960135584,6.73210294950367,
52.7693412662388));
#196824=CARTESIAN_POINT('Ctrl Pts',(0.530862494699656,6.74614512234367,
52.7777785183357));
#196825=CARTESIAN_POINT('Ctrl Pts',(0.352204183006753,6.76020396562737,
52.7862257868836));
#196826=CARTESIAN_POINT('Ctrl Pts',(0.173099260154818,6.76715254952147,
52.7946730554315));
#196827=CARTESIAN_POINT('Ctrl Pts',(-0.00586430683023251,6.7669974589847,
52.8031203239794));
#196828=CARTESIAN_POINT('Ctrl Pts',(-0.161304619336367,6.76686275379354,
52.8104572701804));
#196829=CARTESIAN_POINT('Ctrl Pts',(-0.316638166327703,6.76136991059821,
52.8177942163814));
#196830=CARTESIAN_POINT('Ctrl Pts',(-0.471482715514754,6.75055501784637,
52.8251311625824));
#196831=CARTESIAN_POINT('Ctrl Pts',(-0.645376125660536,6.7384096850539,
52.8333706944332));
#196832=CARTESIAN_POINT('Ctrl Pts',(-0.81904087294918,6.71952402580645,
52.841610226284));
#196833=CARTESIAN_POINT('Ctrl Pts',(-0.991916130636073,6.69390703474316,
52.8498497581348));
#196834=CARTESIAN_POINT('Ctrl Pts',(-1.16459950886949,6.66831847674954,
52.8580801446811));
#196835=CARTESIAN_POINT('Ctrl Pts',(-1.33649479335783,6.63601351527784,
52.8663105312274));
#196836=CARTESIAN_POINT('Ctrl Pts',(-1.5070432996742,6.59705309156347,52.8745409177737));
#196837=CARTESIAN_POINT('Ctrl Pts',(-1.6774329333536,6.55812896101511,52.8827636373914));
#196838=CARTESIAN_POINT('Ctrl Pts',(-1.84647794244342,6.51256179407665,
52.8909863570092));
#196839=CARTESIAN_POINT('Ctrl Pts',(-2.01362680286849,6.46046407766266,
52.8992090766269));
#196840=CARTESIAN_POINT('Ctrl Pts',(-2.18062755736146,6.40841252357864,
52.9074245103227));
#196841=CARTESIAN_POINT('Ctrl Pts',(-2.34573517334649,6.34984205863469,
52.9156399440185));
#196842=CARTESIAN_POINT('Ctrl Pts',(-2.50841045583513,6.28491575003651,
52.9238553777143));
#196843=CARTESIAN_POINT('Ctrl Pts',(-2.67100213586083,6.22002280851921,
52.9320665893151));
#196844=CARTESIAN_POINT('Ctrl Pts',(-2.83116364219281,6.14878066029734,
52.9402778009159));
#196845=CARTESIAN_POINT('Ctrl Pts',(-2.98837263154654,6.07140165159773,
52.9484890125168));
#196846=CARTESIAN_POINT('Ctrl Pts',(-3.14552890168,5.99404859154788,52.9566974705303));
#196847=CARTESIAN_POINT('Ctrl Pts',(-3.29973430824302,5.91056292766706,
52.9649059285438));
#196848=CARTESIAN_POINT('Ctrl Pts',(-3.45048804566559,5.82120444982985,
52.9731143865574));
#196849=CARTESIAN_POINT('Ctrl Pts',(-3.51765212751514,5.78139329673992,
52.9767714338406));
#196850=CARTESIAN_POINT('Ctrl Pts',(-3.58413139685294,5.74041706956382,
52.9804284811239));
#196851=CARTESIAN_POINT('Ctrl Pts',(-3.6498831663623,5.6983016655759,52.9840855284071));
#196852=CARTESIAN_POINT('Ctrl Pts',(-3.80916461890021,5.59627851438966,
52.992944602583));
#196853=CARTESIAN_POINT('Ctrl Pts',(-3.96400950308699,5.48767357401941,
53.0018036767588));
#196854=CARTESIAN_POINT('Ctrl Pts',(-4.11391003546707,5.37289802807417,
53.0106627509346));
#196855=CARTESIAN_POINT('Ctrl Pts',(-4.26409220079215,5.25790684196739,
53.0195384695287));
#196856=CARTESIAN_POINT('Ctrl Pts',(-4.40931124407007,5.13672203928987,
53.0284141881227));
#196857=CARTESIAN_POINT('Ctrl Pts',(-4.54909386346712,5.00979381026463,
53.0372899067167));
#196858=CARTESIAN_POINT('Ctrl Pts',(-4.68927538296318,4.88250336393839,
53.0461909541037));
#196859=CARTESIAN_POINT('Ctrl Pts',(-4.8239892397493,4.74943686773294,53.0550920014907));
#196860=CARTESIAN_POINT('Ctrl Pts',(-4.95279816669417,4.61108222871712,
53.0639930488777));
#196861=CARTESIAN_POINT('Ctrl Pts',(-5.08178221114188,4.47253949467199,
53.0729061973607));
#196862=CARTESIAN_POINT('Ctrl Pts',(-5.20484511780985,4.32869445088134,
53.0818193458437));
#196863=CARTESIAN_POINT('Ctrl Pts',(-5.32159028407468,4.18006768467234,
53.0907324943267));
#196864=CARTESIAN_POINT('Ctrl Pts',(-5.43859465653232,4.0311109264007,53.0996654324366));
#196865=CARTESIAN_POINT('Ctrl Pts',(-5.54925307100242,3.87735141500615,
53.1085983705465));
#196866=CARTESIAN_POINT('Ctrl Pts',(-5.65321095375947,3.71934065558587,
53.1175313086564));
#196867=CARTESIAN_POINT('Ctrl Pts',(-5.75216378487853,3.56893732322435,
53.1260341705149));
#196868=CARTESIAN_POINT('Ctrl Pts',(-5.84504599221339,3.41468261487707,
53.1345370323734));
#196869=CARTESIAN_POINT('Ctrl Pts',(-5.93159077007427,3.25707229523228,
53.1430398942319));
#196870=CARTESIAN_POINT('Ctrl Pts',(-6.01739283086702,3.10081456874688,
53.1514697855336));
#196871=CARTESIAN_POINT('Ctrl Pts',(-6.09712353024838,2.94096957357786,
53.1598996768353));
#196872=CARTESIAN_POINT('Ctrl Pts',(-6.17047859025867,2.77803581099298,
53.168329568137));
#196873=CARTESIAN_POINT('Ctrl Pts',(-6.24373763717159,2.61531530943206,
53.176748425708));
#196874=CARTESIAN_POINT('Ctrl Pts',(-6.31063753670765,2.44951439765333,
53.185167283279));
#196875=CARTESIAN_POINT('Ctrl Pts',(-6.37091904262016,2.28115750275595,
53.19358614085));
#196876=CARTESIAN_POINT('Ctrl Pts',(-6.43113017293803,2.11299715597746,
53.2019951698327));
#196877=CARTESIAN_POINT('Ctrl Pts',(-6.48473819541337,1.94228708465093,
53.2104041988154));
#196878=CARTESIAN_POINT('Ctrl Pts',(-6.53153112594885,1.76957343751577,
53.218813227798));
#196879=CARTESIAN_POINT('Ctrl Pts',(-6.57826208234867,1.597088538161,53.227211119579));
#196880=CARTESIAN_POINT('Ctrl Pts',(-6.61819586128774,1.42260567571939,
53.2356090113601));
#196881=CARTESIAN_POINT('Ctrl Pts',(-6.65116970784568,1.24668781875657,
53.2440069031411));
#196882=CARTESIAN_POINT('Ctrl Pts',(-6.68411777619893,1.07090749038074,
53.2523982296409));
#196883=CARTESIAN_POINT('Ctrl Pts',(-6.71011669236257,0.893694729319301,
53.2607895561408));
#196884=CARTESIAN_POINT('Ctrl Pts',(-6.72905411009238,0.715625449134423,
53.2691808826406));
#196885=CARTESIAN_POINT('Ctrl Pts',(-6.74797629764367,0.537699378914352,
53.2775654605224));
#196886=CARTESIAN_POINT('Ctrl Pts',(-6.7598482762806,0.358918494063914,
53.2859500384041));
#196887=CARTESIAN_POINT('Ctrl Pts',(-6.76460915079576,0.17986672001878,
53.2943346162858));
#196888=CARTESIAN_POINT('Ctrl Pts',(-6.76621522951548,0.119463690468786,
53.2971631495872));
#196889=CARTESIAN_POINT('Ctrl Pts',(-6.76701246558696,0.0590298895209724,
53.2999916828885));
#196890=CARTESIAN_POINT('Ctrl Pts',(-6.76699985266021,-0.00141212489864533,
53.3028202161899));
#196891=CARTESIAN_POINT('Ctrl Pts',(-6.76699985266004,-0.00141212569551268,
53.3028202162272));
#196892=CARTESIAN_POINT('Ctrl Pts',(-6.76696059829612,-0.189521637263152,
53.3116232652798));
#196893=CARTESIAN_POINT('Ctrl Pts',(-6.75907349606841,-0.37741475106076,
53.3204263143324));
#196894=CARTESIAN_POINT('Ctrl Pts',(-6.74341788589126,-0.564450366499948,
53.329229363385));
#196895=CARTESIAN_POINT('Ctrl Pts',(-6.72772898176318,-0.751883740603923,
53.3380511334123));
#196896=CARTESIAN_POINT('Ctrl Pts',(-6.7042385751046,-0.938455706213667,
53.3468729034397));
#196897=CARTESIAN_POINT('Ctrl Pts',(-6.67307728490789,-1.1235339557158,
53.3556946734671));
#196898=CARTESIAN_POINT('Ctrl Pts',(-6.64181218264434,-1.30922878288483,
53.3645458327198));
#196899=CARTESIAN_POINT('Ctrl Pts',(-6.60282509282124,-1.49341966888789,
53.3733969919725));
#196900=CARTESIAN_POINT('Ctrl Pts',(-6.5562977086742,-1.67548481199724,
53.3822481512252));
#196901=CARTESIAN_POINT('Ctrl Pts',(-6.50969360393261,-1.85785016854612,
53.391113905457));
#196902=CARTESIAN_POINT('Ctrl Pts',(-6.4555244405932,-2.03808252365794,
53.3999796596888));
#196903=CARTESIAN_POINT('Ctrl Pts',(-6.39402102355469,-2.21557761099464,
53.4088454139206));
#196904=CARTESIAN_POINT('Ctrl Pts',(-6.33234674120663,-2.39356580512929,
53.4177357984887));
#196905=CARTESIAN_POINT('Ctrl Pts',(-6.26329752910282,-2.56880126419075,
53.4266261830567));
#196906=CARTESIAN_POINT('Ctrl Pts',(-6.18715265651196,-2.74069899934616,
53.4355165676248));
#196907=CARTESIAN_POINT('Ctrl Pts',(-6.11454534236484,-2.90461066447783,
53.4439939203769));
#196908=CARTESIAN_POINT('Ctrl Pts',(-6.03548680304529,-3.06548754111755,
53.4524712731291));
#196909=CARTESIAN_POINT('Ctrl Pts',(-5.95025661522847,-3.22284582518771,
53.4609486258813));
#196910=CARTESIAN_POINT('Ctrl Pts',(-5.86912884330557,-3.37262992524929,
53.4690179351038));
#196911=CARTESIAN_POINT('Ctrl Pts',(-5.78219288923522,-3.51962324273108,
53.4770872443263));
#196912=CARTESIAN_POINT('Ctrl Pts',(-5.68966536748213,-3.66333140816859,
53.4851565535488));
#196913=CARTESIAN_POINT('Ctrl Pts',(-5.59725325269687,-3.80686033046512,
53.4932157981496));
#196914=CARTESIAN_POINT('Ctrl Pts',(-5.49926364647894,-3.94711194384287,
53.5012750427503));
#196915=CARTESIAN_POINT('Ctrl Pts',(-5.39596026446172,-4.08361381919865,
53.5093342873511));
#196916=CARTESIAN_POINT('Ctrl Pts',(-5.29276306008153,-4.21997539472793,
53.5173852484714));
#196917=CARTESIAN_POINT('Ctrl Pts',(-5.18426317190447,-4.35259460688288,
53.5254362095916));
#196918=CARTESIAN_POINT('Ctrl Pts',(-5.07076901702374,-4.48102561652933,
53.5334871707119));
#196919=CARTESIAN_POINT('Ctrl Pts',(-4.95736664527389,-4.60935276355679,
53.541531620991));
#196920=CARTESIAN_POINT('Ctrl Pts',(-4.83897829136152,-4.73349817116958,
53.5495760712701));
#196921=CARTESIAN_POINT('Ctrl Pts',(-4.71595420805213,-4.85304697149692,
53.5576205215492));
#196922=CARTESIAN_POINT('Ctrl Pts',(-4.59300268593878,-4.97252526039509,
53.5656602271075));
#196923=CARTESIAN_POINT('Ctrl Pts',(-4.46542114435501,-5.08741207969262,
53.5736999326657));
#196924=CARTESIAN_POINT('Ctrl Pts',(-4.33359837019655,-5.19732759847115,
53.5817396382239));
#196925=CARTESIAN_POINT('Ctrl Pts',(-4.19893027193389,-5.3096155849587,
53.5899528765284));
#196926=CARTESIAN_POINT('Ctrl Pts',(-4.05983603445047,-5.41671492673835,
53.5981661148328));
#196927=CARTESIAN_POINT('Ctrl Pts',(-3.91676819051835,-5.51826203996726,
53.6063793531373));
#196928=CARTESIAN_POINT('Ctrl Pts',(-3.77676822504537,-5.61763162543941,
53.6144164706855));
#196929=CARTESIAN_POINT('Ctrl Pts',(-3.63296366592209,-5.71168447253263,
53.6224535882337));
#196930=CARTESIAN_POINT('Ctrl Pts',(-3.48580980782958,-5.80012232488584,
53.6304907057818));
#196931=CARTESIAN_POINT('Ctrl Pts',(-3.33864038179446,-5.88856953340156,
53.6385286736059));
#196932=CARTESIAN_POINT('Ctrl Pts',(-3.18812127145481,-5.97140037180547,
53.6465666414301));
#196933=CARTESIAN_POINT('Ctrl Pts',(-3.03473413076102,-6.04836157612904,
53.6546046092542));
#196934=CARTESIAN_POINT('Ctrl Pts',(-2.88130037103585,-6.12534617131043,
53.6626450200619));
#196935=CARTESIAN_POINT('Ctrl Pts',(-2.72499717963609,-6.19645741400195,
53.6706854308697));
#196936=CARTESIAN_POINT('Ctrl Pts',(-2.56632788166806,-6.26148945569448,
53.6787258416774));
#196937=CARTESIAN_POINT('Ctrl Pts',(-2.40166177914262,-6.32897934177779,
53.6870701346652));
#196938=CARTESIAN_POINT('Ctrl Pts',(-2.23444763687034,-6.38992136092001,
53.6954144276531));
#196939=CARTESIAN_POINT('Ctrl Pts',(-2.0652661523553,-6.44414189166685,
53.7037587206409));
#196940=CARTESIAN_POINT('Ctrl Pts',(-1.9019580188266,-6.49648008754321,
53.7118133308564));
#196941=CARTESIAN_POINT('Ctrl Pts',(-1.7368172234552,-6.5425556299749,53.7198679410719));
#196942=CARTESIAN_POINT('Ctrl Pts',(-1.57037671033177,-6.58226450301472,
53.7279225512875));
#196943=CARTESIAN_POINT('Ctrl Pts',(-1.40381019938871,-6.62200343623237,
53.7359832589568));
#196944=CARTESIAN_POINT('Ctrl Pts',(-1.23594237548614,-6.65536603123967,
53.744043966626));
#196945=CARTESIAN_POINT('Ctrl Pts',(-1.06731223174368,-6.68230002319339,
53.7521046742953));
#196946=CARTESIAN_POINT('Ctrl Pts',(-0.898444329601532,-6.70927199046209,
53.7601767470794));
#196947=CARTESIAN_POINT('Ctrl Pts',(-0.728812330485791,-6.72979722612918,
53.7682488198635));
#196948=CARTESIAN_POINT('Ctrl Pts',(-0.558956742052996,-6.74387547041859,
53.7763208926477));
#196949=CARTESIAN_POINT('Ctrl Pts',(-0.54116565968643,-6.7453500595448,
53.7771663809422));
#196950=CARTESIAN_POINT('Ctrl Pts',(-0.523372120621158,-6.74675396590074,
53.7780118692366));
#196951=CARTESIAN_POINT('Ctrl Pts',(-0.505576742886304,-6.74808722209876,
53.7788573575311));
#196952=CARTESIAN_POINT('Ctrl Pts',(-0.33018993218177,-6.76122746311562,
53.7871902795778));
#196953=CARTESIAN_POINT('Ctrl Pts',(-0.154065296644953,-6.76754267212398,
53.7955232016245));
#196954=CARTESIAN_POINT('Ctrl Pts',(0.0222316097009473,-6.76696348117308,
53.8038561236712));
#196955=CARTESIAN_POINT('Ctrl Pts',(0.198320175856137,-6.76638497468543,
53.8121791982249));
#196956=CARTESIAN_POINT('Ctrl Pts',(0.374580262292695,-6.75892829984617,
53.8205022727785));
#196957=CARTESIAN_POINT('Ctrl Pts',(0.550441407086462,-6.74457583969257,
53.8288253473321));
#196958=CARTESIAN_POINT('Ctrl Pts',(0.72612700697635,-6.73023770618992,
53.8371401137781));
#196959=CARTESIAN_POINT('Ctrl Pts',(0.901414113975392,-6.70901752941434,
53.845454880224));
#196960=CARTESIAN_POINT('Ctrl Pts',(1.07573225068254,-6.68094971728133,
53.85376964667));
#196961=CARTESIAN_POINT('Ctrl Pts',(1.24990835853327,-6.65290477390618,
53.8620776385095));
#196962=CARTESIAN_POINT('Ctrl Pts',(1.42311672716742,-6.61802336733466,
53.8703856303491));
#196963=CARTESIAN_POINT('Ctrl Pts',(1.59479175988844,-6.57639173427131,
53.8786936221886));
#196964=CARTESIAN_POINT('Ctrl Pts',(1.76635839107584,-6.53478638885619,
53.8869963680757));
#196965=CARTESIAN_POINT('Ctrl Pts',(1.93639327866725,-6.48643939302725,
53.8952991139628));
#196966=CARTESIAN_POINT('Ctrl Pts',(2.10434056142242,-6.43148814828671,
53.9036018598499));
#196967=CARTESIAN_POINT('Ctrl Pts',(2.2722192094751,-6.37655936036876,53.9119012126693));
#196968=CARTESIAN_POINT('Ctrl Pts',(2.43801162247627,-6.3150318094134,53.9202005654887));
#196969=CARTESIAN_POINT('Ctrl Pts',(2.60117637936824,-6.24709295940254,
53.9284999183082));
#196970=CARTESIAN_POINT('Ctrl Pts',(2.76430643385417,-6.17916855884512,
53.9367975059945));
#196971=CARTESIAN_POINT('Ctrl Pts',(2.92480962461324,-6.10483570943703,
53.9450950936809));
#196972=CARTESIAN_POINT('Ctrl Pts',(3.08216359500454,-6.02433038383758,
53.9533926813672));
#196973=CARTESIAN_POINT('Ctrl Pts',(3.23951024718267,-5.94382880237712,
53.9616898831496));
#196974=CARTESIAN_POINT('Ctrl Pts',(3.39370766122959,-5.85715547537241,
53.9699870849321));
#196975=CARTESIAN_POINT('Ctrl Pts',(3.54425704592219,-5.76459287308574,
53.9782842867145));
#196976=CARTESIAN_POINT('Ctrl Pts',(3.69482444533538,-5.67201919476963,
53.986582481339));
#196977=CARTESIAN_POINT('Ctrl Pts',(3.8417426495365,-5.57355501967024,53.9948806759636));
#196978=CARTESIAN_POINT('Ctrl Pts',(3.98454071775745,-5.46952687794228,
54.0031788705881));
#196979=CARTESIAN_POINT('Ctrl Pts',(4.12743921752462,-5.3654255720094,54.0114829014297));
#196980=CARTESIAN_POINT('Ctrl Pts',(4.26621150951494,-5.25575268520299,
54.0197869322713));
#196981=CARTESIAN_POINT('Ctrl Pts',(4.4004179889734,-5.14087643523158,54.0280909631128));
#196982=CARTESIAN_POINT('Ctrl Pts',(4.5346732696016,-5.0259584130939,54.0363980135286));
#196983=CARTESIAN_POINT('Ctrl Pts',(4.66435916913934,-4.90583348844042,
54.0447050639443));
#196984=CARTESIAN_POINT('Ctrl Pts',(4.7890718614116,-4.78090783285305,54.0530121143601));
#196985=CARTESIAN_POINT('Ctrl Pts',(4.91391789259978,-4.65584861065604,
54.0613280464147));
#196986=CARTESIAN_POINT('Ctrl Pts',(5.03377985200776,-4.52597865372332,
54.0696439784693));
#196987=CARTESIAN_POINT('Ctrl Pts',(5.1482924982285,-4.39173921729013,54.077959910524));
#196988=CARTESIAN_POINT('Ctrl Pts',(5.23461456327614,-4.29054667876992,
54.0842286367428));
#196989=CARTESIAN_POINT('Ctrl Pts',(5.31789770134732,-4.18687192182626,
54.0904973629616));
#196990=CARTESIAN_POINT('Ctrl Pts',(5.39800151058386,-4.08091517820873,
54.0967660891804));
#196991=CARTESIAN_POINT('Ctrl Pts',(5.50598177486445,-3.93808505206145,
54.1052163579038));
#196992=CARTESIAN_POINT('Ctrl Pts',(5.60838135925249,-3.79084536638939,
54.1136666266271));
#196993=CARTESIAN_POINT('Ctrl Pts',(5.7048374661404,-3.63965911658232,54.1221168953505));
#196994=CARTESIAN_POINT('Ctrl Pts',(5.80120844724159,-3.48860629376989,
54.130559706425));
#196995=CARTESIAN_POINT('Ctrl Pts',(5.89164622820041,-3.33361412725735,
54.1390025174995));
#196996=CARTESIAN_POINT('Ctrl Pts',(5.975829985486,-3.17517637062358,54.147445328574));
#196997=CARTESIAN_POINT('Ctrl Pts',(6.05995090958461,-3.0168568689776,54.1558818380917));
#196998=CARTESIAN_POINT('Ctrl Pts',(6.13782696010525,-2.85509719565438,
54.1643183476095));
#196999=CARTESIAN_POINT('Ctrl Pts',(6.20918193447105,-2.69041794237223,
54.1727548571272));
#197000=CARTESIAN_POINT('Ctrl Pts',(6.28048585051319,-2.52585652595691,
54.1811853298684));
#197001=CARTESIAN_POINT('Ctrl Pts',(6.3452778663386,-2.35838000017359,54.1896158026096));
#197002=CARTESIAN_POINT('Ctrl Pts',(6.40332874287388,-2.1885314735423,54.1980462753508));
#197003=CARTESIAN_POINT('Ctrl Pts',(6.46135466349469,-2.0187559643322,54.2064731238546));
#197004=CARTESIAN_POINT('Ctrl Pts',(6.51264511504258,-1.84661080030151,
54.2148999723585));
#197005=CARTESIAN_POINT('Ctrl Pts',(6.55701958718149,-1.67265750628106,
54.2233268208623));
#197006=CARTESIAN_POINT('Ctrl Pts',(6.60138036250554,-1.49875790543027,
54.2317510682989));
#197007=CARTESIAN_POINT('Ctrl Pts',(6.63882933368537,-1.32305160850205,
54.2401753157356));
#197008=CARTESIAN_POINT('Ctrl Pts',(6.669236208392,-1.14611404173981,54.2485995631722));
#197009=CARTESIAN_POINT('Ctrl Pts',(6.67780370229957,-1.0962598051607,54.2509731937832));
#197010=CARTESIAN_POINT('Ctrl Pts',(6.68581243581901,-1.04630789009901,
54.2533468243942));
#197011=CARTESIAN_POINT('Ctrl Pts',(6.69326022616024,-0.996271320926859,
54.2557204550053));
#197012=CARTESIAN_POINT('Ctrl Pts',(6.72030355510934,-0.814585836023446,
54.2643392359425));
#197013=CARTESIAN_POINT('Ctrl Pts',(6.73993506892834,-0.631864935886169,
54.2729580168797));
#197014=CARTESIAN_POINT('Ctrl Pts',(6.75210607839452,-0.44872319541984,
54.2815767978169));
#197015=CARTESIAN_POINT('Ctrl Pts',(6.76428439891208,-0.265471442823568,
54.2902007560035));
#197016=CARTESIAN_POINT('Ctrl Pts',(6.76899325123443,-0.0817986488975172,
54.29882471419));
#197017=CARTESIAN_POINT('Ctrl Pts',(6.76623605695892,0.101679012136382,
54.3074486723765));
#197018=CARTESIAN_POINT('Ctrl Pts',(6.7633792546617,0.291785095043078,54.3163841847476));
#197019=CARTESIAN_POINT('Ctrl Pts',(6.75250691412112,0.481681322143884,
54.3253196971188));
#197020=CARTESIAN_POINT('Ctrl Pts',(6.7336816087822,0.670686954956127,54.3342552094899));
#197021=CARTESIAN_POINT('Ctrl Pts',(6.71547871530889,0.85344358694677,54.3428952913846));
#197022=CARTESIAN_POINT('Ctrl Pts',(6.68984041836846,1.03536727747079,54.3515353732793));
#197023=CARTESIAN_POINT('Ctrl Pts',(6.65687570557249,1.21585148787129,54.360175455174));
#197024=CARTESIAN_POINT('Ctrl Pts',(6.62222024824564,1.40559264807541,54.3692586827833));
#197025=CARTESIAN_POINT('Ctrl Pts',(6.57946718504263,1.59374240549075,54.3783419103926));
#197026=CARTESIAN_POINT('Ctrl Pts',(6.52880315705344,1.77961184994062,54.387425138002));
#197027=CARTESIAN_POINT('Ctrl Pts',(6.47813912906425,1.96548129439049,54.3965083656113));
#197028=CARTESIAN_POINT('Ctrl Pts',(6.4195642862191,2.14907006667625,54.4055915932206));
#197029=CARTESIAN_POINT('Ctrl Pts',(6.35332481091391,2.32971089344274,54.41467482083));
#197030=CARTESIAN_POINT('Ctrl Pts',(6.287367065096,2.5095834193241,54.4237194156898));
#197031=CARTESIAN_POINT('Ctrl Pts',(6.21374965904559,2.68669943209794,54.4327640105496));
#197032=CARTESIAN_POINT('Ctrl Pts',(6.13271659374217,2.86043286599063,54.4418086054094));
#197033=CARTESIAN_POINT('Ctrl Pts',(6.05175788903143,3.03400687211068,54.4508449004298));
#197034=CARTESIAN_POINT('Ctrl Pts',(5.96339721182486,3.20420428118829,54.4598811954501));
#197035=CARTESIAN_POINT('Ctrl Pts',(5.86792620564945,3.37042001018455,54.4689174904705));
#197036=CARTESIAN_POINT('Ctrl Pts',(5.77262414290605,3.53634160741416,54.4779377950582));
#197037=CARTESIAN_POINT('Ctrl Pts',(5.67023699474511,3.69829538829857,54.4869580996459));
#197038=CARTESIAN_POINT('Ctrl Pts',(5.56110163486589,3.85570196030398,54.4959784042336));
#197039=CARTESIAN_POINT('Ctrl Pts',(5.45210370977234,4.01291030930898,54.5049873494999));
#197040=CARTESIAN_POINT('Ctrl Pts',(5.33637466731163,4.16558268229743,54.5139962947663));
#197041=CARTESIAN_POINT('Ctrl Pts',(5.21429524190593,4.31316752865423,54.5230052400326));
#197042=CARTESIAN_POINT('Ctrl Pts',(5.09249303303122,4.46041724106853,54.5319937278914));
#197043=CARTESIAN_POINT('Ctrl Pts',(4.96436937687443,4.6026023040594,54.5409822157502));
#197044=CARTESIAN_POINT('Ctrl Pts',(4.83034559369141,4.73920356658226,54.549970703609));
#197045=CARTESIAN_POINT('Ctrl Pts',(4.71275816957089,4.85905237408636,54.5578568646242));
#197046=CARTESIAN_POINT('Ctrl Pts',(4.59062972628005,4.97460330359925,54.5657430256395));
#197047=CARTESIAN_POINT('Ctrl Pts',(4.46427107342755,5.0855258118466,54.5736291866548));
#197048=CARTESIAN_POINT('Ctrl Pts',(4.33414306896021,5.19975720259742,54.5817505964091));
#197049=CARTESIAN_POINT('Ctrl Pts',(4.19958588311641,5.30902755291757,54.5898720061635));
#197050=CARTESIAN_POINT('Ctrl Pts',(4.06102343394452,5.41298232668032,54.5979934159179));
#197051=CARTESIAN_POINT('Ctrl Pts',(3.92247874117177,5.51692377892294,54.6061137849358));
#197052=CARTESIAN_POINT('Ctrl Pts',(3.77993010237479,5.61555079450149,54.6142341539537));
#197053=CARTESIAN_POINT('Ctrl Pts',(3.63383292729056,5.7085503638436,54.6223545229715));
#197054=CARTESIAN_POINT('Ctrl Pts',(3.4877063293019,5.80156866262,54.6304765273725));
#197055=CARTESIAN_POINT('Ctrl Pts',(3.33803007852441,5.88895705803541,54.6385985317734));
#197056=CARTESIAN_POINT('Ctrl Pts',(3.18528699900472,5.97044686216798,54.6467205361743));
#197057=CARTESIAN_POINT('Ctrl Pts',(3.15666658312933,5.98571611096938,54.6482424063921));
#197058=CARTESIAN_POINT('Ctrl Pts',(3.12793856017337,6.00077839134618,54.6497642766099));
#197059=CARTESIAN_POINT('Ctrl Pts',(3.09910619832136,6.01563211736939,54.6512861468277));
#197060=CARTESIAN_POINT('Origin',(0.,0.,4.30282021618968));
#197061=CARTESIAN_POINT('',(3.09910619832134,6.0156321173694,57.0459010634246));
#197062=CARTESIAN_POINT('',(3.09910619832132,6.01563211736941,56.6514148629243));
#197063=CARTESIAN_POINT('',(3.09910619832133,6.0156321173694,4.30282021618968));
#197064=CARTESIAN_POINT('',(-6.76699969835165,0.00202052189306006,55.6971797838405));
#197065=CARTESIAN_POINT('Ctrl Pts',(-6.76699969835165,0.0020205218929699,
55.6971797838405));
#197066=CARTESIAN_POINT('Ctrl Pts',(-6.76705147928238,-0.171400782706949,
55.7053523960128));
#197067=CARTESIAN_POINT('Ctrl Pts',(-6.76043245233308,-0.3450005055368,
55.713525008185));
#197068=CARTESIAN_POINT('Ctrl Pts',(-6.7471277734586,-0.518223705192626,
55.7216976203573));
#197069=CARTESIAN_POINT('Ctrl Pts',(-6.73371132132619,-0.692902161420724,
55.7299388910441));
#197070=CARTESIAN_POINT('Ctrl Pts',(-6.71349632062296,-0.867197368685377,
55.7381801617309));
#197071=CARTESIAN_POINT('Ctrl Pts',(-6.68652127016635,-1.04053942914863,
55.7464214324177));
#197072=CARTESIAN_POINT('Ctrl Pts',(-6.65980533644719,-1.21221640174707,
55.7545835391684));
#197073=CARTESIAN_POINT('Ctrl Pts',(-6.6264587095387,-1.38295809180124,
55.762745645919));
#197074=CARTESIAN_POINT('Ctrl Pts',(-6.58657088360599,-1.55221551185195,
55.7709077526696));
#197075=CARTESIAN_POINT('Ctrl Pts',(-6.54610275210948,-1.72393536298964,
55.7791886053245));
#197076=CARTESIAN_POINT('Ctrl Pts',(-6.49890164906467,-1.89412704152559,
55.7874694579794));
#197077=CARTESIAN_POINT('Ctrl Pts',(-6.44511484732756,-2.06222782561915,
55.7957503106343));
#197078=CARTESIAN_POINT('Ctrl Pts',(-6.39132804559047,-2.23032860971264,
55.8040311632892));
#197079=CARTESIAN_POINT('Ctrl Pts',(-6.33095565914911,-2.39633812586347,
55.8123120159441));
#197080=CARTESIAN_POINT('Ctrl Pts',(-6.26419778537996,-2.55970996514075,
55.820592868599));
#197081=CARTESIAN_POINT('Ctrl Pts',(-6.19471563011998,-2.72974874649895,
55.8292116495363));
#197082=CARTESIAN_POINT('Ctrl Pts',(-6.11833139665957,-2.89689470834243,
55.8378304304735));
#197083=CARTESIAN_POINT('Ctrl Pts',(-6.03531691208284,-3.06059451262772,
55.8464492114108));
#197084=CARTESIAN_POINT('Ctrl Pts',(-5.95225256121027,-3.22439265038952,
55.8550731695973));
#197085=CARTESIAN_POINT('Ctrl Pts',(-5.86255014843089,-3.3847402280458,
55.8636971277838));
#197086=CARTESIAN_POINT('Ctrl Pts',(-5.76652712834069,-3.54110913106486,
55.8723210859703));
#197087=CARTESIAN_POINT('Ctrl Pts',(-5.66703512416222,-3.70312710902409,
55.8812565983414));
#197088=CARTESIAN_POINT('Ctrl Pts',(-5.56075750837659,-3.86087327613705,
55.8901921107126));
#197089=CARTESIAN_POINT('Ctrl Pts',(-5.44809555685882,-4.01379419045561,
55.8991276230837));
#197090=CARTESIAN_POINT('Ctrl Pts',(-5.33915849235693,-4.16165915535622,
55.9077677049784));
#197091=CARTESIAN_POINT('Ctrl Pts',(-5.2242527262714,-4.30501262187923,
55.9164077868731));
#197092=CARTESIAN_POINT('Ctrl Pts',(-5.10378157334828,-4.44338864511654,
55.9250478687678));
#197093=CARTESIAN_POINT('Ctrl Pts',(-4.97713151196047,-4.58886190915005,
55.9341310963771));
#197094=CARTESIAN_POINT('Ctrl Pts',(-4.84433044693398,-4.72883345181669,
55.9432143239864));
#197095=CARTESIAN_POINT('Ctrl Pts',(-4.70589051354589,-4.86280613170202,
55.9522975515957));
#197096=CARTESIAN_POINT('Ctrl Pts',(-4.56745058015781,-4.99677881158735,
55.9613807792051));
#197097=CARTESIAN_POINT('Ctrl Pts',(-4.42337209068111,-5.12475239633751,
55.9704640068144));
#197098=CARTESIAN_POINT('Ctrl Pts',(-4.27420733716871,-5.24627874201258,
55.9795472344237));
#197099=CARTESIAN_POINT('Ctrl Pts',(-4.12567701062539,-5.36728821229094,
55.9885918292835));
#197100=CARTESIAN_POINT('Ctrl Pts',(-3.97196698339277,-5.48201759816239,
55.9976364241433));
#197101=CARTESIAN_POINT('Ctrl Pts',(-3.81360663819394,-5.59005307748711,
56.0066810190031));
#197102=CARTESIAN_POINT('Ctrl Pts',(-3.65539161353856,-5.69798941725421,
56.0157173140235));
#197103=CARTESIAN_POINT('Ctrl Pts',(-3.49253498714845,-5.79924398047969,
56.0247536090438));
#197104=CARTESIAN_POINT('Ctrl Pts',(-3.32559640039692,-5.89344530658146,
56.0337899040641));
#197105=CARTESIAN_POINT('Ctrl Pts',(-3.15895322456582,-5.98747993604951,
56.0428102086518));
#197106=CARTESIAN_POINT('Ctrl Pts',(-2.98824271939455,-6.07448613511232,
56.0518305132395));
#197107=CARTESIAN_POINT('Ctrl Pts',(-2.81405030747951,-6.15413762171228,
56.0608508178272));
#197108=CARTESIAN_POINT('Ctrl Pts',(-2.64007725707004,-6.23368880273733,
56.0698597630935));
#197109=CARTESIAN_POINT('Ctrl Pts',(-2.46263126614196,-6.30590365609888,
56.0788687083598));
#197110=CARTESIAN_POINT('Ctrl Pts',(-2.28232126275601,-6.37050222930436,
56.087877653626));
#197111=CARTESIAN_POINT('Ctrl Pts',(-2.10242070521609,-6.43495411282561,
56.0968661414848));
#197112=CARTESIAN_POINT('Ctrl Pts',(-1.91966934043858,-6.4918241583365,
56.1058546293436));
#197113=CARTESIAN_POINT('Ctrl Pts',(-1.73469445945225,-6.54088099053527,
56.1148431172023));
#197114=CARTESIAN_POINT('Ctrl Pts',(-1.57240445937941,-6.58392160912446,
56.1227292782177));
#197115=CARTESIAN_POINT('Ctrl Pts',(-1.40840329791828,-6.62094853192503,
56.1306154392331));
#197116=CARTESIAN_POINT('Ctrl Pts',(-1.2431269650968,-6.65183616369565,
56.1385016002484));
#197117=CARTESIAN_POINT('Ctrl Pts',(-1.07291918897449,-6.68364540718268,
56.1466230651046));
#197118=CARTESIAN_POINT('Ctrl Pts',(-0.901434902148291,-6.70892768419305,
56.1547445299608));
#197119=CARTESIAN_POINT('Ctrl Pts',(-0.729219616686332,-6.72759449956965,
56.1628659948169));
#197120=CARTESIAN_POINT('Ctrl Pts',(-0.557016612709089,-6.74625998372756,
56.1709868804931));
#197121=CARTESIAN_POINT('Ctrl Pts',(-0.384083077987967,-6.75831090650958,
56.1791077661693));
#197122=CARTESIAN_POINT('Ctrl Pts',(-0.210970502884236,-6.76371055315888,
56.1872286518455));
#197123=CARTESIAN_POINT('Ctrl Pts',(-0.0378372358778278,-6.76911084522035,
56.1953505081997));
#197124=CARTESIAN_POINT('Ctrl Pts',(0.135474748084897,-6.76785826787115,
56.203472364554));
#197125=CARTESIAN_POINT('Ctrl Pts',(0.308413143192804,-6.75996821982958,
56.2115942209082));
#197126=CARTESIAN_POINT('Ctrl Pts',(0.481477712014817,-6.75207241530655,
56.2197220028684));
#197127=CARTESIAN_POINT('Ctrl Pts',(0.654167781411757,-6.73752948477339,
56.2278497848286));
#197128=CARTESIAN_POINT('Ctrl Pts',(0.825934711704664,-6.71640684086375,
56.2359775667887));
#197129=CARTESIAN_POINT('Ctrl Pts',(0.997771613460076,-6.69527559237414,
56.2441086597052));
#197130=CARTESIAN_POINT('Ctrl Pts',(1.16868426532264,-6.66755934643257,
56.2522397526216));
#197131=CARTESIAN_POINT('Ctrl Pts',(1.3381336713158,-6.63337676283286,56.260370845538));
#197132=CARTESIAN_POINT('Ctrl Pts',(1.50776802425461,-6.59915687037158,
56.2685108132026));
#197133=CARTESIAN_POINT('Ctrl Pts',(1.67593558595926,-6.55845662963263,
56.2766507808671));
#197134=CARTESIAN_POINT('Ctrl Pts',(1.8421112508722,-6.51144493483666,56.2847907485317));
#197135=CARTESIAN_POINT('Ctrl Pts',(1.92829713567188,-6.48706263725991,
56.2890124877122));
#197136=CARTESIAN_POINT('Ctrl Pts',(2.01394750765826,-6.46098342309908,
56.2932342268927));
#197137=CARTESIAN_POINT('Ctrl Pts',(2.0989912316564,-6.43323595163659,56.2974559660732));
#197138=CARTESIAN_POINT('Ctrl Pts',(2.26901283008087,-6.37776249364934,
56.3058961755308));
#197139=CARTESIAN_POINT('Ctrl Pts',(2.43695994872582,-6.31550365160833,
56.3143363849885));
#197140=CARTESIAN_POINT('Ctrl Pts',(2.60227310043975,-6.24663619164168,
56.3227765944461));
#197141=CARTESIAN_POINT('Ctrl Pts',(2.76746100294989,-6.17782090897877,
56.3312104091947));
#197142=CARTESIAN_POINT('Ctrl Pts',(2.93001860993022,-6.10240711730429,
56.3396442239432));
#197143=CARTESIAN_POINT('Ctrl Pts',(3.08940384182834,-6.02062064093863,
56.3480780386918));
#197144=CARTESIAN_POINT('Ctrl Pts',(3.24869281759735,-5.93888355716433,
56.3565067600803));
#197145=CARTESIAN_POINT('Ctrl Pts',(3.40481294187678,-5.85078161330139,
56.3649354814689));
#197146=CARTESIAN_POINT('Ctrl Pts',(3.55724393009326,-5.75658793225768,
56.3733642028574));
#197147=CARTESIAN_POINT('Ctrl Pts',(3.70960626898648,-5.66243667259123,
56.3817891282592));
#197148=CARTESIAN_POINT('Ctrl Pts',(3.85828250134583,-5.56219932097617,
56.390214053661));
#197149=CARTESIAN_POINT('Ctrl Pts',(4.00277834447115,-5.45619414290152,
56.3986389790627));
#197150=CARTESIAN_POINT('Ctrl Pts',(4.14723128191518,-5.35022044133364,
56.4070614028204));
#197151=CARTESIAN_POINT('Ctrl Pts',(4.28750603694678,-5.23848252577955,
56.4154838265782));
#197152=CARTESIAN_POINT('Ctrl Pts',(4.42313831937298,-5.12134127037971,
56.4239062503359));
#197153=CARTESIAN_POINT('Ctrl Pts',(4.55877273490465,-5.00419817268502,
56.4323288065541));
#197154=CARTESIAN_POINT('Ctrl Pts',(4.68976427528127,-4.88165177824237,
56.4407513627723));
#197155=CARTESIAN_POINT('Ctrl Pts',(4.81568218028241,-4.75410287420355,
56.4491739189905));
#197156=CARTESIAN_POINT('Ctrl Pts',(4.94160433881428,-4.62654966153854,
56.4575967597243));
#197157=CARTESIAN_POINT('Ctrl Pts',(5.06245228576555,-4.49399383960433,
56.466019600458));
#197158=CARTESIAN_POINT('Ctrl Pts',(5.17783244871321,-4.35687274694277,
56.4744424411918));
#197159=CARTESIAN_POINT('Ctrl Pts',(5.29323261757138,-4.21972787868374,
56.4828667423724));
#197160=CARTESIAN_POINT('Ctrl Pts',(5.40316289750295,-4.07801641674895,
56.4912910435531));
#197161=CARTESIAN_POINT('Ctrl Pts',(5.50727007468458,-3.9322087081542,56.4997153447337));
#197162=CARTESIAN_POINT('Ctrl Pts',(5.61140984210758,-3.78635535517118,
56.5081422831005));
#197163=CARTESIAN_POINT('Ctrl Pts',(5.70972267867272,-3.63640347031142,
56.5165692214673));
#197164=CARTESIAN_POINT('Ctrl Pts',(5.80189855636353,-3.48285258684126,
56.5249961598341));
#197165=CARTESIAN_POINT('Ctrl Pts',(5.89415731175491,-3.32916364182546,
56.5334306750778));
#197166=CARTESIAN_POINT('Ctrl Pts',(5.98026791079522,-3.1718695185201,56.5418651903215));
#197167=CARTESIAN_POINT('Ctrl Pts',(6.05996562668506,-3.01149557585522,
56.5502997055651));
#197168=CARTESIAN_POINT('Ctrl Pts',(6.13970183725431,-2.85104417120237,
56.5587382947519));
#197169=CARTESIAN_POINT('Ctrl Pts',(6.21301884605309,-2.68751028248184,
56.5671768839387));
#197170=CARTESIAN_POINT('Ctrl Pts',(6.27969979472655,-2.5214399632177,56.5756154731255));
#197171=CARTESIAN_POINT('Ctrl Pts',(6.3464552776145,-2.35518401490897,56.5840634947458));
#197172=CARTESIAN_POINT('Ctrl Pts',(6.40655976202181,-2.18638628346224,
56.5925115163661));
#197173=CARTESIAN_POINT('Ctrl Pts',(6.45984564847592,-2.01560988235987,
56.6009595379864));
#197174=CARTESIAN_POINT('Ctrl Pts',(6.49013249118527,-1.9185433166547,56.6057612578985));
#197175=CARTESIAN_POINT('Ctrl Pts',(6.51821743525438,-1.82083777252419,
56.6105629778105));
#197176=CARTESIAN_POINT('Ctrl Pts',(6.54407704261625,-1.72259822950766,
56.6153646977226));
#197177=CARTESIAN_POINT('Ctrl Pts',(6.58845094663599,-1.55402366486885,
56.6236042295735));
#197178=CARTESIAN_POINT('Ctrl Pts',(6.62636848229945,-1.38349984522596,
56.6318437614243));
#197179=CARTESIAN_POINT('Ctrl Pts',(6.6576579632165,-1.21156074747406,56.6400832932751));
#197180=CARTESIAN_POINT('Ctrl Pts',(6.68891271499639,-1.03981249010473,
56.6483136798214));
#197181=CARTESIAN_POINT('Ctrl Pts',(6.71355399724992,-0.866652429542697,
56.6565440663677));
#197182=CARTESIAN_POINT('Ctrl Pts',(6.73146000388173,-0.692629205376576,
56.664774452914));
#197183=CARTESIAN_POINT('Ctrl Pts',(6.74934933036471,-0.518768090682325,
56.6729971725319));
#197184=CARTESIAN_POINT('Ctrl Pts',(6.76051584013589,-0.344045765660869,
56.6812198921497));
#197185=CARTESIAN_POINT('Ctrl Pts',(6.76488884012532,-0.169020651838755,
56.6894426117675));
#197186=CARTESIAN_POINT('Ctrl Pts',(6.7692579653217,0.00584937712268896,
56.6976580454633));
#197187=CARTESIAN_POINT('Ctrl Pts',(6.76684556938897,0.181021305712984,
56.7058734791591));
#197188=CARTESIAN_POINT('Ctrl Pts',(6.75763281889859,0.35593213530774,56.7140889128549));
#197189=CARTESIAN_POINT('Ctrl Pts',(6.74842480304663,0.530753074317118,
56.7223001244557));
#197190=CARTESIAN_POINT('Ctrl Pts',(6.73242341162174,0.705312827026527,
56.7305113360565));
#197191=CARTESIAN_POINT('Ctrl Pts',(6.70966189177258,0.879048518623898,
56.7387225476572));
#197192=CARTESIAN_POINT('Ctrl Pts',(6.68690800488117,1.05272594885721,56.7469310056707));
#197193=CARTESIAN_POINT('Ctrl Pts',(6.65739855175781,1.2255795159683,56.7551394636843));
#197194=CARTESIAN_POINT('Ctrl Pts',(6.62121862778495,1.39705149621392,56.7633479216978));
#197195=CARTESIAN_POINT('Ctrl Pts',(6.60509968163741,1.47344600764146,56.7670049689811));
#197196=CARTESIAN_POINT('Ctrl Pts',(6.58765740095151,1.54956638132596,56.7706620162643));
#197197=CARTESIAN_POINT('Ctrl Pts',(6.56890259347102,1.62536387233434,56.7743190635476));
#197198=CARTESIAN_POINT('Ctrl Pts',(6.52346970246536,1.8089807476912,56.7831781377235));
#197199=CARTESIAN_POINT('Ctrl Pts',(6.47037849510245,1.99051117195333,56.7920372118994));
#197200=CARTESIAN_POINT('Ctrl Pts',(6.4098551901401,2.16934216790115,56.8008962860752));
#197201=CARTESIAN_POINT('Ctrl Pts',(6.34921817406361,2.3485091513137,56.8097720046692));
#197202=CARTESIAN_POINT('Ctrl Pts',(6.28112123841151,2.5249663253962,56.8186477232632));
#197203=CARTESIAN_POINT('Ctrl Pts',(6.20583861966574,2.6981208324805,56.8275234418573));
#197204=CARTESIAN_POINT('Ctrl Pts',(6.13034116559747,2.87176947360253,56.8364244892443));
#197205=CARTESIAN_POINT('Ctrl Pts',(6.04761709727592,3.04209634800314,56.8453255366313));
#197206=CARTESIAN_POINT('Ctrl Pts',(5.95798794656755,3.20853060271456,56.8542265840183));
#197207=CARTESIAN_POINT('Ctrl Pts',(5.86823694379943,3.37519112707807,56.8631397325013));
#197208=CARTESIAN_POINT('Ctrl Pts',(5.77156223505374,3.53794823540166,56.8720528809843));
#197209=CARTESIAN_POINT('Ctrl Pts',(5.66832936572089,3.69625908205935,56.8809660294673));
#197210=CARTESIAN_POINT('Ctrl Pts',(5.56486729118965,3.85492142208588,56.8898989675772));
#197211=CARTESIAN_POINT('Ctrl Pts',(5.45481807376652,4.00911753676417,56.8988319056871));
#197212=CARTESIAN_POINT('Ctrl Pts',(5.33859004174419,4.1583344461683,56.907764843797));
#197213=CARTESIAN_POINT('Ctrl Pts',(5.22795780762323,4.30036730836828,56.9162677056554));
#197214=CARTESIAN_POINT('Ctrl Pts',(5.11172782731296,4.43788898361679,56.9247705675139));
#197215=CARTESIAN_POINT('Ctrl Pts',(4.9902838460473,4.57048751621524,56.9332734293723));
#197216=CARTESIAN_POINT('Ctrl Pts',(4.87281800056972,4.69874252381987,56.9414977633143));
#197217=CARTESIAN_POINT('Ctrl Pts',(4.75024823342919,4.82263683442815,56.9497220972564));
#197218=CARTESIAN_POINT('Ctrl Pts',(4.62293103387865,4.94174034688203,56.9579464311984));
#197219=CARTESIAN_POINT('Ctrl Pts',(4.49578303534043,5.06068557408499,56.9661598352297));
#197220=CARTESIAN_POINT('Ctrl Pts',(4.36390043775118,5.17485244816821,56.974373239261));
#197221=CARTESIAN_POINT('Ctrl Pts',(4.22767853481257,5.28384549417231,56.9825866432922));
#197222=CARTESIAN_POINT('Ctrl Pts',(4.09156113004649,5.39275492972993,56.9907937466796));
#197223=CARTESIAN_POINT('Ctrl Pts',(3.95111132471011,5.49649821510977,56.9990008500669));
#197224=CARTESIAN_POINT('Ctrl Pts',(3.80676015048628,5.59471770124907,57.0072079534542));
#197225=CARTESIAN_POINT('Ctrl Pts',(3.66250955706071,5.6928687501597,57.0154093383081));
#197226=CARTESIAN_POINT('Ctrl Pts',(3.51436330622302,5.78550346700239,57.023610723162));
#197227=CARTESIAN_POINT('Ctrl Pts',(3.36278419189374,5.87230546538151,57.0318121080159));
#197228=CARTESIAN_POINT('Ctrl Pts',(3.27598619290921,5.92201046465206,57.0365084264855));
#197229=CARTESIAN_POINT('Ctrl Pts',(3.18806313841968,5.96980368254101,57.041204744955));
#197230=CARTESIAN_POINT('Ctrl Pts',(3.09910619832134,6.0156321173694,57.0459010634246));
#197231=CARTESIAN_POINT('Ctrl Pts',(3.09910619832139,6.01563211736937,55.0459882871872));
#197232=CARTESIAN_POINT('Ctrl Pts',(2.947404464696,6.09378513168305,55.054049088509));
#197233=CARTESIAN_POINT('Ctrl Pts',(2.79250277190683,6.16632044368588,55.0621098898309));
#197234=CARTESIAN_POINT('Ctrl Pts',(2.63486444203576,6.23295903821737,55.0701706911527));
#197235=CARTESIAN_POINT('Ctrl Pts',(2.47739390984294,6.29952669948375,55.0782229121771));
#197236=CARTESIAN_POINT('Ctrl Pts',(2.31719287792394,6.36020998984401,55.0862751332016));
#197237=CARTESIAN_POINT('Ctrl Pts',(2.15475029648333,6.41477514491389,55.094327354226));
#197238=CARTESIAN_POINT('Ctrl Pts',(1.99244502452738,6.46929417714297,55.1023727688681));
#197239=CARTESIAN_POINT('Ctrl Pts',(1.82790232583838,6.51770524871838,55.1104181835102));
#197240=CARTESIAN_POINT('Ctrl Pts',(1.66163211870152,6.55982223098306,55.1184635981523));
#197241=CARTESIAN_POINT('Ctrl Pts',(1.4954660560798,6.6019128329793,55.1265039734923));
#197242=CARTESIAN_POINT('Ctrl Pts',(1.32757499961367,6.6377171020729,55.1345443488323));
#197243=CARTESIAN_POINT('Ctrl Pts',(1.15848495344206,6.66709844029983,55.1425847241723));
#197244=CARTESIAN_POINT('Ctrl Pts',(0.982230612909521,6.69772465698377,
55.1509657677953));
#197245=CARTESIAN_POINT('Ctrl Pts',(0.804673857516982,6.72137163588897,
55.1593468114183));
#197246=CARTESIAN_POINT('Ctrl Pts',(0.626423866829409,6.73794346511356,
55.1677278550413));
#197247=CARTESIAN_POINT('Ctrl Pts',(0.455488382986473,6.75383526760814,
55.1757649816705));
#197248=CARTESIAN_POINT('Ctrl Pts',(0.283915829244434,6.7632209944559,55.1838021082997));
#197249=CARTESIAN_POINT('Ctrl Pts',(0.112249562627997,6.76606894996569,
55.1918392349289));
#197250=CARTESIAN_POINT('Ctrl Pts',(-0.0594298949380122,6.76891712431427,
55.1998769791362));
#197251=CARTESIAN_POINT('Ctrl Pts',(-0.231202706125807,6.76522652047594,
55.2079147233436));
#197252=CARTESIAN_POINT('Ctrl Pts',(-0.402525040730363,6.75501758632685,
55.2159524675509));
#197253=CARTESIAN_POINT('Ctrl Pts',(-0.573894483692988,6.74480584503574,
55.22399242189));
#197254=CARTESIAN_POINT('Ctrl Pts',(-0.744812830711291,6.72807222796632,
55.2320323762291));
#197255=CARTESIAN_POINT('Ctrl Pts',(-0.914741050811109,6.70488909751392,
55.2400723305681));
#197256=CARTESIAN_POINT('Ctrl Pts',(-1.08474967562401,6.68169499753008,
55.2481160891619));
#197257=CARTESIAN_POINT('Ctrl Pts',(-1.25376687149422,6.65204536028967,
55.2561598477556));
#197258=CARTESIAN_POINT('Ctrl Pts',(-1.42126362542262,6.61606368674385,
55.2642036063493));
#197259=CARTESIAN_POINT('Ctrl Pts',(-1.58896631887206,6.58003777324446,
55.2722572548529));
#197260=CARTESIAN_POINT('Ctrl Pts',(-1.75514447369032,6.53766436007929,
55.2803109033565));
#197261=CARTESIAN_POINT('Ctrl Pts',(-1.91928334731617,6.48911707651471,
55.28836455186));
#197262=CARTESIAN_POINT('Ctrl Pts',(-2.08354111776461,6.44053462688841,
55.2964240341627));
#197263=CARTESIAN_POINT('Ctrl Pts',(-2.24575631385013,6.38576952076682,
55.3044835164654));
#197264=CARTESIAN_POINT('Ctrl Pts',(-2.40543451991011,6.32504338091248,
55.3125429987681));
#197265=CARTESIAN_POINT('Ctrl Pts',(-2.56534597916378,6.26422853411179,
55.3206142541238));
#197266=CARTESIAN_POINT('Ctrl Pts',(-2.72271271096822,6.19743541973706,
55.3286855094795));
#197267=CARTESIAN_POINT('Ctrl Pts',(-2.87706458077591,6.12493170558209,
55.3367567648352));
#197268=CARTESIAN_POINT('Ctrl Pts',(-2.92151436012792,6.10405230774645,
55.339081100265));
#197269=CARTESIAN_POINT('Ctrl Pts',(-2.96571429885978,6.08269960050195,
55.3414054356949));
#197270=CARTESIAN_POINT('Ctrl Pts',(-3.0096536315685,6.06088063056736,55.3437297711247));
#197271=CARTESIAN_POINT('Ctrl Pts',(-3.16717953318606,5.98265793806318,
55.3520626931714));
#197272=CARTESIAN_POINT('Ctrl Pts',(-3.32185622138896,5.8981896526874,55.3603956152181));
#197273=CARTESIAN_POINT('Ctrl Pts',(-3.47316195721547,5.80770479784839,
55.3687285372648));
#197274=CARTESIAN_POINT('Ctrl Pts',(-3.62428888635416,5.71732687416505,
55.3770516118184));
#197275=CARTESIAN_POINT('Ctrl Pts',(-3.7720525027817,5.62094672200501,55.385374686372));
#197276=CARTESIAN_POINT('Ctrl Pts',(-3.91595326226002,5.51884037165374,
55.3936977609256));
#197277=CARTESIAN_POINT('Ctrl Pts',(-4.05971037974752,5.41683594404069,
55.4020125273716));
#197278=CARTESIAN_POINT('Ctrl Pts',(-4.19961204049332,5.30911690624783,
55.4103272938175));
#197279=CARTESIAN_POINT('Ctrl Pts',(-4.33518524188114,5.19600403373361,
55.4186420602635));
#197280=CARTESIAN_POINT('Ctrl Pts',(-4.47064798254955,5.08298332197937,
55.426950052103));
#197281=CARTESIAN_POINT('Ctrl Pts',(-4.60178902506593,4.96457775430237,
55.4352580439425));
#197282=CARTESIAN_POINT('Ctrl Pts',(-4.72816601867455,4.84115018356705,
55.4435660357821));
#197283=CARTESIAN_POINT('Ctrl Pts',(-4.85446321349336,4.71780054925428,
55.4518687816692));
#197284=CARTESIAN_POINT('Ctrl Pts',(-4.97600210613736,4.58943547386822,
55.4601715275563));
#197285=CARTESIAN_POINT('Ctrl Pts',(-5.09237483349377,4.45645683870037,
55.4684742734434));
#197286=CARTESIAN_POINT('Ctrl Pts',(-5.20870000302462,4.32353254766347,
55.4767736262628));
#197287=CARTESIAN_POINT('Ctrl Pts',(-5.31986298531551,4.18599871508608,
55.4850729790822));
#197288=CARTESIAN_POINT('Ctrl Pts',(-5.42549388793494,4.04429290135873,
55.4933723319017));
#197289=CARTESIAN_POINT('Ctrl Pts',(-5.53110232463386,3.90261722608016,
55.501669919588));
#197290=CARTESIAN_POINT('Ctrl Pts',(-5.63118081787038,3.75677161614816,
55.5099675072743));
#197291=CARTESIAN_POINT('Ctrl Pts',(-5.72540062926587,3.60722561456891,
55.5182650949607));
#197292=CARTESIAN_POINT('Ctrl Pts',(-5.81961605868946,3.45768656807019,
55.5265622967431));
#197293=CARTESIAN_POINT('Ctrl Pts',(-5.90797316393929,3.3044477672898,55.5348594985255));
#197294=CARTESIAN_POINT('Ctrl Pts',(-5.990187204686,3.14800671105004,55.5431567003079));
#197295=CARTESIAN_POINT('Ctrl Pts',(-6.07241108315444,2.99154693509328,
55.5514548949324));
#197296=CARTESIAN_POINT('Ctrl Pts',(-6.14849027108658,2.8318844483687,55.5597530895569));
#197297=CARTESIAN_POINT('Ctrl Pts',(-6.2181864667203,2.66954042207578,55.5680512841815));
#197298=CARTESIAN_POINT('Ctrl Pts',(-6.28793168050111,2.50708221733614,
55.576355315023));
#197299=CARTESIAN_POINT('Ctrl Pts',(-6.35128479419908,2.341939024593,55.5846593458646));
#197300=CARTESIAN_POINT('Ctrl Pts',(-6.40805573101609,2.174651868275,55.5929633767062));
#197301=CARTESIAN_POINT('Ctrl Pts',(-6.46484731130831,2.00730388174247,
55.6012704271219));
#197302=CARTESIAN_POINT('Ctrl Pts',(-6.51505183945978,1.83781070956437,
55.6095774775377));
#197303=CARTESIAN_POINT('Ctrl Pts',(-6.55852937811859,1.66672775112055,
55.6178845279534));
#197304=CARTESIAN_POINT('Ctrl Pts',(-6.60205340160396,1.49546187612038,
55.626200460008));
#197305=CARTESIAN_POINT('Ctrl Pts',(-6.63883598675889,1.32260315792511,
55.6345163920627));
#197306=CARTESIAN_POINT('Ctrl Pts',(-6.66878828373765,1.14871747034836,
55.6428323241173));
#197307=CARTESIAN_POINT('Ctrl Pts',(-6.69136696140792,1.01763874559964,
55.6491010503363));
#197308=CARTESIAN_POINT('Ctrl Pts',(-6.71006541001522,0.885976661707472,
55.6553697765552));
#197309=CARTESIAN_POINT('Ctrl Pts',(-6.72486509888574,0.753975067086791,
55.6616385027742));
#197310=CARTESIAN_POINT('Ctrl Pts',(-6.75028615237594,0.527239246691952,
55.672406136197));
#197311=CARTESIAN_POINT('Ctrl Pts',(-6.76424264559793,0.299157940462259,
55.6831737696197));
#197312=CARTESIAN_POINT('Ctrl Pts',(-6.76663034842965,0.0707299633175301,
55.6939414030424));
#197313=CARTESIAN_POINT('Ctrl Pts',(-6.76686971674843,0.0478299524261698,
55.6950208632983));
#197314=CARTESIAN_POINT('Ctrl Pts',(-6.76699285898682,0.0249264676522418,
55.6961003235541));
#197315=CARTESIAN_POINT('Ctrl Pts',(-6.76699969835146,0.00202052254068524,
55.69717978381));
#197316=CARTESIAN_POINT('',(-6.76699843275197,-0.00460555451873011,55.3028202161608));
#197317=CARTESIAN_POINT('Ctrl Pts',(3.09910619832136,6.01563211736939,54.6512861468277));
#197318=CARTESIAN_POINT('Ctrl Pts',(2.94511279802101,6.09496574217557,54.6594144427633));
#197319=CARTESIAN_POINT('Ctrl Pts',(2.78814145528455,6.16834620428235,54.6675427386989));
#197320=CARTESIAN_POINT('Ctrl Pts',(2.62870208357314,6.23556046845977,54.6756710346345));
#197321=CARTESIAN_POINT('Ctrl Pts',(2.46919265465219,6.30280426639501,54.6838029021204));
#197322=CARTESIAN_POINT('Ctrl Pts',(2.30721337762719,6.36387633741049,54.6919347696062));
#197323=CARTESIAN_POINT('Ctrl Pts',(2.1432911071522,6.41861295218853,54.7000666370921));
#197324=CARTESIAN_POINT('Ctrl Pts',(1.97919583167376,6.47340733647037,54.7082070870223));
#197325=CARTESIAN_POINT('Ctrl Pts',(1.81315381883384,6.52185281089454,54.7163475369525));
#197326=CARTESIAN_POINT('Ctrl Pts',(1.64570456140892,6.56383618751702,54.7244879868827));
#197327=CARTESIAN_POINT('Ctrl Pts',(1.59019589955145,6.57775348456813,54.7271865087483));
#197328=CARTESIAN_POINT('Ctrl Pts',(1.53453266244973,6.59096108701847,54.7298850306139));
#197329=CARTESIAN_POINT('Ctrl Pts',(1.47873466302612,6.6034561251185,54.7325835524796));
#197330=CARTESIAN_POINT('Ctrl Pts',(1.30421437899526,6.64253705312163,54.7410237619372));
#197331=CARTESIAN_POINT('Ctrl Pts',(1.1280145363046,6.67472421685401,54.7494639713948));
#197332=CARTESIAN_POINT('Ctrl Pts',(0.950706475874524,6.69988404352868,
54.7579041808524));
#197333=CARTESIAN_POINT('Ctrl Pts',(0.773532752568601,6.7250248079072,54.766337995601));
#197334=CARTESIAN_POINT('Ctrl Pts',(0.595252814277275,6.74314880207744,
54.7747718103495));
#197335=CARTESIAN_POINT('Ctrl Pts',(0.416448073417482,6.75417352472876,
54.783205625098));
#197336=CARTESIAN_POINT('Ctrl Pts',(0.237751316541259,6.76519158931573,
54.7916343464866));
#197337=CARTESIAN_POINT('Ctrl Pts',(0.058530720978724,6.76911890946073,
54.8000630678751));
#197338=CARTESIAN_POINT('Ctrl Pts',(-0.120626900306542,6.76592478164829,
54.8084917892637));
#197339=CARTESIAN_POINT('Ctrl Pts',(-0.299703835573495,6.76273209235381,
54.8169167146654));
#197340=CARTESIAN_POINT('Ctrl Pts',(-0.478717520236171,6.75242435590935,
54.8253416400671));
#197341=CARTESIAN_POINT('Ctrl Pts',(-0.657080458865021,6.73502295991467,
54.8337665654688));
#197342=CARTESIAN_POINT('Ctrl Pts',(-0.835390435531868,6.71762673098037,
54.8421889892265));
#197343=CARTESIAN_POINT('Ctrl Pts',(-1.01304971995069,6.6931410753592,54.8506114129842));
#197344=CARTESIAN_POINT('Ctrl Pts',(-1.18947485924251,6.66163932971682,
54.859033836742));
#197345=CARTESIAN_POINT('Ctrl Pts',(-1.36590277319424,6.63013708864261,
54.8674563929602));
#197346=CARTESIAN_POINT('Ctrl Pts',(-1.54109617385986,6.59161858913544,
54.8758789491784));
#197347=CARTESIAN_POINT('Ctrl Pts',(-1.71448006877979,6.5462086045097,54.8843015053966));
#197348=CARTESIAN_POINT('Ctrl Pts',(-1.88786982064052,6.50079708592609,
54.8927243461303));
#197349=CARTESIAN_POINT('Ctrl Pts',(-2.05944962214071,6.44849370240205,
54.9011471868641));
#197350=CARTESIAN_POINT('Ctrl Pts',(-2.22865780254383,6.38947364022738,
54.9095700275978));
#197351=CARTESIAN_POINT('Ctrl Pts',(-2.39789532216493,6.33044334449032,
54.9179943287784));
#197352=CARTESIAN_POINT('Ctrl Pts',(-2.56476008589129,6.26469415806114,
54.9264186299591));
#197353=CARTESIAN_POINT('Ctrl Pts',(-2.72870827975019,6.19245025204263,
54.9348429311397));
#197354=CARTESIAN_POINT('Ctrl Pts',(-2.89270779678703,6.12018373042369,
54.9432698695065));
#197355=CARTESIAN_POINT('Ctrl Pts',(-3.0537886185245,6.04141857013837,54.9516968078733));
#197356=CARTESIAN_POINT('Ctrl Pts',(-3.2114291698959,5.95642608337766,54.9601237462401));
#197357=CARTESIAN_POINT('Ctrl Pts',(-3.36921145993829,5.87135717768786,
54.9685582614837));
#197358=CARTESIAN_POINT('Ctrl Pts',(-3.52354700495028,5.78004991598772,
54.9769927767274));
#197359=CARTESIAN_POINT('Ctrl Pts',(-3.67394000319246,5.68282094148163,
54.985427291971));
#197360=CARTESIAN_POINT('Ctrl Pts',(-3.8244056425414,5.58554500454777,54.9938658811578));
#197361=CARTESIAN_POINT('Ctrl Pts',(-3.97092466174838,5.48234183817236,
55.0023044703446));
#197362=CARTESIAN_POINT('Ctrl Pts',(-4.11303185905277,5.37357031464342,
55.0107430595314));
#197363=CARTESIAN_POINT('Ctrl Pts',(-4.25529790005259,5.26467720916027,
55.0191910811517));
#197364=CARTESIAN_POINT('Ctrl Pts',(-4.39314200545948,5.15020351876856,
55.027639102772));
#197365=CARTESIAN_POINT('Ctrl Pts',(-4.52613262437603,5.03054792905892,
55.0360871243923));
#197366=CARTESIAN_POINT('Ctrl Pts',(-4.60172235788968,4.96253761214141,
55.0408888443045));
#197367=CARTESIAN_POINT('Ctrl Pts',(-4.67574478522353,4.89285391469649,
55.0456905642168));
#197368=CARTESIAN_POINT('Ctrl Pts',(-4.74812616704887,4.82157514737516,
55.0504922841291));
#197369=CARTESIAN_POINT('Ctrl Pts',(-4.87232930922572,4.69926404127934,
55.0587318159799));
#197370=CARTESIAN_POINT('Ctrl Pts',(-4.99197543961657,4.57198122209799,
55.0669713478307));
#197371=CARTESIAN_POINT('Ctrl Pts',(-5.10664436501536,4.44009823418997,
55.0752108796815));
#197372=CARTESIAN_POINT('Ctrl Pts',(-5.22118601592096,4.30836162718147,
55.0834412662278));
#197373=CARTESIAN_POINT('Ctrl Pts',(-5.33076123027508,4.17203528429697,
55.0916716527742));
#197374=CARTESIAN_POINT('Ctrl Pts',(-5.43498522373034,4.03152881892625,
55.0999020393205));
#197375=CARTESIAN_POINT('Ctrl Pts',(-5.53911212843965,3.89115324084999,
55.1081247589383));
#197376=CARTESIAN_POINT('Ctrl Pts',(-5.63789752891919,3.74660557932165,
55.116347478556));
#197377=CARTESIAN_POINT('Ctrl Pts',(-5.73099560100306,3.59832994891847,
55.1245701981738));
#197378=CARTESIAN_POINT('Ctrl Pts',(-5.82401118148764,3.45018570140663,
55.1327856318696));
#197379=CARTESIAN_POINT('Ctrl Pts',(-5.91134928901013,3.29832036897575,
55.1410010655654));
#197380=CARTESIAN_POINT('Ctrl Pts',(-5.99270635831043,3.14320847273383,
55.1492164992612));
#197381=CARTESIAN_POINT('Ctrl Pts',(-6.0740216163948,2.98817629196154,55.157427710862));
#197382=CARTESIAN_POINT('Ctrl Pts',(-6.14936179306817,2.82990118471906,
55.1656389224628));
#197383=CARTESIAN_POINT('Ctrl Pts',(-6.2184681714375,2.66888414900661,55.1738501340636));
#197384=CARTESIAN_POINT('Ctrl Pts',(-6.28755137534065,2.5079211095234,55.1820585920771));
#197385=CARTESIAN_POINT('Ctrl Pts',(-6.35040480512318,2.3442182999833,55.1902670500907));
#197386=CARTESIAN_POINT('Ctrl Pts',(-6.40681695851238,2.17829875364198,
55.1984755081042));
#197387=CARTESIAN_POINT('Ctrl Pts',(-6.43194980465131,2.10437797276225,
55.2021325553874));
#197388=CARTESIAN_POINT('Ctrl Pts',(-6.45580476048543,2.03001746222543,
55.2057896026706));
#197389=CARTESIAN_POINT('Ctrl Pts',(-6.47836623906171,1.95526465538182,
55.2094466499538));
#197390=CARTESIAN_POINT('Ctrl Pts',(-6.52931529549927,1.78645546311793,
55.2177051117296));
#197391=CARTESIAN_POINT('Ctrl Pts',(-6.57363637656756,1.61573891659319,
55.2259635735053));
#197392=CARTESIAN_POINT('Ctrl Pts',(-6.61120997214735,1.44367299073559,
55.2342220352811));
#197393=CARTESIAN_POINT('Ctrl Pts',(-6.64880347265179,1.27151591152317,
55.2424848720456));
#197394=CARTESIAN_POINT('Ctrl Pts',(-6.67964229747292,1.09800837206614,
55.2507477088102));
#197395=CARTESIAN_POINT('Ctrl Pts',(-6.70365853353092,0.923716009289684,
55.2590105455747));
#197396=CARTESIAN_POINT('Ctrl Pts',(-6.7277071374903,0.749188743841748,
55.2672845185841));
#197397=CARTESIAN_POINT('Ctrl Pts',(-6.74491474196548,0.573874889902926,
55.2755584915935));
#197398=CARTESIAN_POINT('Ctrl Pts',(-6.7552654380163,0.398343899090347,
55.2838324646029));
#197399=CARTESIAN_POINT('Ctrl Pts',(-6.76318329661703,0.264069879403348,
55.2901617151222));
#197400=CARTESIAN_POINT('Ctrl Pts',(-6.76708981864431,0.129668871660295,
55.2964909656416));
#197401=CARTESIAN_POINT('Ctrl Pts',(-6.76699843275197,-0.00460555451873829,
55.3028202161609));
#197402=CARTESIAN_POINT('Ctrl Pts',(-6.76699843275155,-0.00460555513501829,
55.3028202161899));
#197403=CARTESIAN_POINT('Ctrl Pts',(-6.7668369231588,-0.241913573155351,
55.31400612805));
#197404=CARTESIAN_POINT('Ctrl Pts',(-6.75418850557821,-0.478814946071242,
55.32519203991));
#197405=CARTESIAN_POINT('Ctrl Pts',(-6.72920402485982,-0.714214387848929,
55.33637795177));
#197406=CARTESIAN_POINT('Ctrl Pts',(-6.7053621412692,-0.938848477763353,
55.3470523064395));
#197407=CARTESIAN_POINT('Ctrl Pts',(-6.6702870947623,-1.1621154726341,55.357726661109));
#197408=CARTESIAN_POINT('Ctrl Pts',(-6.62415141723983,-1.38307881246136,
55.3684010157785));
#197409=CARTESIAN_POINT('Ctrl Pts',(-6.58861194451494,-1.55329243043991,
55.3766237396444));
#197410=CARTESIAN_POINT('Ctrl Pts',(-6.54646027510188,-1.72236182502713,
55.3848464635103));
#197411=CARTESIAN_POINT('Ctrl Pts',(-6.49778336986864,-1.88973550484151,
55.3930691873761));
#197412=CARTESIAN_POINT('Ctrl Pts',(-6.44915798749064,-2.05693202528564,
55.4012832077674));
#197413=CARTESIAN_POINT('Ctrl Pts',(-6.39402122217541,-2.22243606350356,
55.4094972281586));
#197414=CARTESIAN_POINT('Ctrl Pts',(-6.33251115686558,-2.38570564994363,
55.4177112485498));
#197415=CARTESIAN_POINT('Ctrl Pts',(-6.27105384839404,-2.54883520097445,
55.4259182238217));
#197416=CARTESIAN_POINT('Ctrl Pts',(-6.20323425237369,-2.70973378326702,
55.4341251990937));
#197417=CARTESIAN_POINT('Ctrl Pts',(-6.1292404527537,-2.86787385920784,
55.4423321743657));
#197418=CARTESIAN_POINT('Ctrl Pts',(-6.05529526558349,-3.0259100402745,
55.4505337578186));
#197419=CARTESIAN_POINT('Ctrl Pts',(-5.97518410601595,-3.1811910010899,
55.4587353412716));
#197420=CARTESIAN_POINT('Ctrl Pts',(-5.88914345903629,-3.33320841215939,
55.4669369247246));
#197421=CARTESIAN_POINT('Ctrl Pts',(-5.80314207298519,-3.48515645665709,
55.4751347657396));
#197422=CARTESIAN_POINT('Ctrl Pts',(-5.71121676619947,-3.63384360667496,
55.4833326067547));
#197423=CARTESIAN_POINT('Ctrl Pts',(-5.61365036159667,-3.77878533628806,
55.4915304477697));
#197424=CARTESIAN_POINT('Ctrl Pts',(-5.51609256692457,-3.92371427524588,
55.4997275653508));
#197425=CARTESIAN_POINT('Ctrl Pts',(-5.41289485905208,-4.06489815000376,
55.507924682932));
#197426=CARTESIAN_POINT('Ctrl Pts',(-5.3043840605631,-4.20188038121555,
55.5161218005132));
#197427=CARTESIAN_POINT('Ctrl Pts',(-5.19587446937759,-4.33886108834747,
55.5243188268922));
#197428=CARTESIAN_POINT('Ctrl Pts',(-5.08205212728753,-4.47163996310305,
55.5325158532713));
#197429=CARTESIAN_POINT('Ctrl Pts',(-4.96328484087391,-4.59979266797442,
55.5407128796504));
#197430=CARTESIAN_POINT('Ctrl Pts',(-4.84449728038244,-4.72796724905426,
55.5489113052965));
#197431=CARTESIAN_POINT('Ctrl Pts',(-4.72076333774359,-4.8515138237245,
55.5571097309427));
#197432=CARTESIAN_POINT('Ctrl Pts',(-4.59248847504029,-4.97004412521882,
55.5653081565888));
#197433=CARTESIAN_POINT('Ctrl Pts',(-4.46416839076231,-5.08861621297405,
55.5735094724795));
#197434=CARTESIAN_POINT('Ctrl Pts',(-4.33130446091504,-5.20216826146719,
55.5817107883702));
#197435=CARTESIAN_POINT('Ctrl Pts',(-4.19433610899009,-5.31035155190519,
55.5899121042608));
#197436=CARTESIAN_POINT('Ctrl Pts',(-4.05721177304013,-5.41865804500166,
55.5981227600774));
#197437=CARTESIAN_POINT('Ctrl Pts',(-3.91597395857713,-5.5215833424832,
55.606333415894));
#197438=CARTESIAN_POINT('Ctrl Pts',(-3.77109288751936,-5.6188208223524,
55.6145440717106));
#197439=CARTESIAN_POINT('Ctrl Pts',(-3.62612644155663,-5.7161156019126,
55.6227595658677));
#197440=CARTESIAN_POINT('Ctrl Pts',(-3.47751276448229,-5.80771569480692,
55.6309750600249));
#197441=CARTESIAN_POINT('Ctrl Pts',(-3.32574757645875,-5.89335999729176,
55.639190554182));
#197442=CARTESIAN_POINT('Ctrl Pts',(-3.17374692195308,-5.97913717848801,
55.6474187948295));
#197443=CARTESIAN_POINT('Ctrl Pts',(-3.01858530398695,-6.0589399390686,
55.655647035477));
#197444=CARTESIAN_POINT('Ctrl Pts',(-2.86078057254186,-6.13255440381633,
55.6638752761245));
#197445=CARTESIAN_POINT('Ctrl Pts',(-2.71736126535138,-6.19945819964448,
55.6713534332258));
#197446=CARTESIAN_POINT('Ctrl Pts',(-2.57175919926442,-6.2612510582797,
55.678831590327));
#197447=CARTESIAN_POINT('Ctrl Pts',(-2.42437372432431,-6.31780824691648,
55.6863097474282));
#197448=CARTESIAN_POINT('Ctrl Pts',(-2.26533735264849,-6.37883631007286,
55.6943790566507));
#197449=CARTESIAN_POINT('Ctrl Pts',(-2.10370356158937,-6.43396718238844,
55.7024483658733));
#197450=CARTESIAN_POINT('Ctrl Pts',(-1.93995839993024,-6.48296617348418,
55.7105176750958));
#197451=CARTESIAN_POINT('Ctrl Pts',(-1.77641747299214,-6.53190404952055,
55.7185769196965));
#197452=CARTESIAN_POINT('Ctrl Pts',(-1.61077076827496,-6.5747251564444,
55.7266361642973));
#197453=CARTESIAN_POINT('Ctrl Pts',(-1.44352584780147,-6.61124210165753,
55.7346954088981));
#197454=CARTESIAN_POINT('Ctrl Pts',(-1.27645282557682,-6.64772151389855,
55.7427463700183));
#197455=CARTESIAN_POINT('Ctrl Pts',(-1.10778521803332,-6.67790957996122,
55.7507973311386));
#197456=CARTESIAN_POINT('Ctrl Pts',(-0.938047253761767,-6.70166817663408,
55.7588482922589));
#197457=CARTESIAN_POINT('Ctrl Pts',(-0.768446557191717,-6.72540755964447,
55.766892742538));
#197458=CARTESIAN_POINT('Ctrl Pts',(-0.597777594383516,-6.74272777059752,
55.7749371928171));
#197459=CARTESIAN_POINT('Ctrl Pts',(-0.426576234246035,-6.75354142034951,
55.7829816430962));
#197460=CARTESIAN_POINT('Ctrl Pts',(-0.255475850885913,-6.76434869207096,
55.7910213486544));
#197461=CARTESIAN_POINT('Ctrl Pts',(-0.0838440667595212,-6.76865701875375,
55.7990610542127));
#197462=CARTESIAN_POINT('Ctrl Pts',(0.0877767609437413,-6.76643068687164,
55.8071007597709));
#197463=CARTESIAN_POINT('Ctrl Pts',(0.263101932459457,-6.76415630080612,
55.8153139980754));
#197464=CARTESIAN_POINT('Ctrl Pts',(0.43841527417324,-6.75506189990469,
55.8235272363798));
#197465=CARTESIAN_POINT('Ctrl Pts',(0.613136568790696,-6.73916556763607,
55.8317404746843));
#197466=CARTESIAN_POINT('Ctrl Pts',(0.784111223483176,-6.72361010871817,
55.8397775922324));
#197467=CARTESIAN_POINT('Ctrl Pts',(0.954518579036146,-6.70154152370596,
55.8478147097806));
#197468=CARTESIAN_POINT('Ctrl Pts',(1.12381880315425,-6.67302931940786,
55.8558518273288));
#197469=CARTESIAN_POINT('Ctrl Pts',(1.29313693815969,-6.64451409869983,
55.8638897951529));
#197470=CARTESIAN_POINT('Ctrl Pts',(1.46134734003895,-6.60955396329149,
55.871927762977));
#197471=CARTESIAN_POINT('Ctrl Pts',(1.62791941120203,-6.56826974100727,
55.8799657308011));
#197472=CARTESIAN_POINT('Ctrl Pts',(1.79454210869888,-6.52697297118849,
55.8880061416089));
#197473=CARTESIAN_POINT('Ctrl Pts',(1.95952512189877,-6.47934837844146,
55.8960465524166));
#197474=CARTESIAN_POINT('Ctrl Pts',(2.12235222507528,-6.4255669036061,55.9040869632243));
#197475=CARTESIAN_POINT('Ctrl Pts',(2.29133327439528,-6.36975279235335,
55.9124312562121));
#197476=CARTESIAN_POINT('Ctrl Pts',(2.45799184433616,-6.30730745515342,
55.9207755491999));
#197477=CARTESIAN_POINT('Ctrl Pts',(2.62177388937024,-6.2384766307983,55.9291198421877));
#197478=CARTESIAN_POINT('Ctrl Pts',(2.77987003184592,-6.17203535628801,
55.9371744524032));
#197479=CARTESIAN_POINT('Ctrl Pts',(2.93528572203134,-6.09964474121615,
55.9452290626188));
#197480=CARTESIAN_POINT('Ctrl Pts',(3.08754845635011,-6.02157234696139,
55.9532836728343));
#197481=CARTESIAN_POINT('Ctrl Pts',(3.23992645570963,-5.94344085080131,
55.9613443805036));
#197482=CARTESIAN_POINT('Ctrl Pts',(3.38914642329934,-5.85961919297991,
55.9694050881728));
#197483=CARTESIAN_POINT('Ctrl Pts',(3.53476491456139,-5.7704181823145,55.9774657958421));
#197484=CARTESIAN_POINT('Ctrl Pts',(3.68058871917186,-5.68109140356825,
55.9855378686262));
#197485=CARTESIAN_POINT('Ctrl Pts',(3.82280060830583,-5.5863703445995,55.9936099414104));
#197486=CARTESIAN_POINT('Ctrl Pts',(3.96098980629043,-5.48660630576528,
56.0016820141945));
#197487=CARTESIAN_POINT('Ctrl Pts',(3.97546407484964,-5.47615678068157,
56.0025275024889));
#197488=CARTESIAN_POINT('Ctrl Pts',(3.98989424395179,-5.46565196249461,
56.0033729907833));
#197489=CARTESIAN_POINT('Ctrl Pts',(4.00427986530766,-5.45509227788969,
56.0042184790777));
#197490=CARTESIAN_POINT('Ctrl Pts',(4.14606096641492,-5.35101865648716,
56.0125514011244));
#197491=CARTESIAN_POINT('Ctrl Pts',(4.28396418126854,-5.24128045693582,
56.0208843231711));
#197492=CARTESIAN_POINT('Ctrl Pts',(4.417514765497,-5.12619276818733,56.0292172452178));
#197493=CARTESIAN_POINT('Ctrl Pts',(4.55090752532126,-5.01124108517787,
56.0375403197714));
#197494=CARTESIAN_POINT('Ctrl Pts',(4.67995763994972,-4.89095273169111,
56.045863394325));
#197495=CARTESIAN_POINT('Ctrl Pts',(4.80422029083322,-4.76568530194204,
56.0541864688786));
#197496=CARTESIAN_POINT('Ctrl Pts',(4.92835890252025,-4.64054291436146,
56.0625012353246));
#197497=CARTESIAN_POINT('Ctrl Pts',(5.04771932795627,-4.51043159808899,
56.0708160017705));
#197498=CARTESIAN_POINT('Ctrl Pts',(5.16189056914938,-4.37574847907494,
56.0791307682165));
#197499=CARTESIAN_POINT('Ctrl Pts',(5.27596878725769,-4.24117509556933,
56.087438760056));
#197500=CARTESIAN_POINT('Ctrl Pts',(5.38486602170394,-4.10203759588203,
56.0957467518955));
#197501=CARTESIAN_POINT('Ctrl Pts',(5.48820868701037,-3.95876930469861,
56.1040547437351));
#197502=CARTESIAN_POINT('Ctrl Pts',(5.59148609819536,-3.81559147805318,
56.1123574896221));
#197503=CARTESIAN_POINT('Ctrl Pts',(5.68921572698593,-3.66828833938926,
56.1206602355092));
#197504=CARTESIAN_POINT('Ctrl Pts',(5.7810646566209,-3.51732575061917,56.1289629813963));
#197505=CARTESIAN_POINT('Ctrl Pts',(5.87287605052535,-3.36642485544827,
56.1372623342157));
#197506=CARTESIAN_POINT('Ctrl Pts',(5.95881135337727,-3.21186778683285,
56.1455616870352));
#197507=CARTESIAN_POINT('Ctrl Pts',(6.0385811743165,-3.05414904698352,56.1538610398546));
#197508=CARTESIAN_POINT('Ctrl Pts',(6.11833402955332,-2.89646385126372,
56.1621586275409));
#197509=CARTESIAN_POINT('Ctrl Pts',(6.19192385834307,-2.73561863422694,
56.1704562152273));
#197510=CARTESIAN_POINT('Ctrl Pts',(6.25910729815888,-2.5721323508199,56.1787538029136));
#197511=CARTESIAN_POINT('Ctrl Pts',(6.32628761340949,-2.40865367082751,
56.187051004696));
#197512=CARTESIAN_POINT('Ctrl Pts',(6.3870620013392,-2.24253449106635,56.1953482064784));
#197513=CARTESIAN_POINT('Ctrl Pts',(6.44123523920145,-2.07431376442173,
56.2036454082608));
#197514=CARTESIAN_POINT('Ctrl Pts',(6.49541495942661,-1.90607290850588,
56.2119436028854));
#197515=CARTESIAN_POINT('Ctrl Pts',(6.54299184956379,-1.73573033593956,
56.2202417975099));
#197516=CARTESIAN_POINT('Ctrl Pts',(6.58382049658707,-1.56384035909041,
56.2285399921345));
#197517=CARTESIAN_POINT('Ctrl Pts',(6.6246778588738,-1.39182949001658,56.236844022976));
#197518=CARTESIAN_POINT('Ctrl Pts',(6.65877741387089,-1.21826938090844,
56.2451480538176));
#197519=CARTESIAN_POINT('Ctrl Pts',(6.68602466338608,-1.04372563473027,
56.2534520846592));
#197520=CARTESIAN_POINT('Ctrl Pts',(6.71328182075112,-0.869118419642034,
56.2617591350749));
#197521=CARTESIAN_POINT('Ctrl Pts',(6.73368166003576,-0.693527199420231,
56.2700661854906));
#197522=CARTESIAN_POINT('Ctrl Pts',(6.74718154470948,-0.517523142218622,
56.2783732359064));
#197523=CARTESIAN_POINT('Ctrl Pts',(6.76069586303831,-0.341330906975363,
56.286689167961));
#197524=CARTESIAN_POINT('Ctrl Pts',(6.76729546774921,-0.164725300483295,
56.2950051000156));
#197525=CARTESIAN_POINT('Ctrl Pts',(6.76698984921282,0.0117209492236127,
56.3033210320702));
#197526=CARTESIAN_POINT('Ctrl Pts',(6.76675946746853,0.14472988009398,56.3095897582892));
#197527=CARTESIAN_POINT('Ctrl Pts',(6.76260629585194,0.277648229017697,
56.3158584845082));
#197528=CARTESIAN_POINT('Ctrl Pts',(6.75455388823963,0.410232581430221,
56.3221272107271));
#197529=CARTESIAN_POINT('Ctrl Pts',(6.74369920966265,0.588956833736392,
56.3305774794505));
#197530=CARTESIAN_POINT('Ctrl Pts',(6.72573748134582,0.767401716643068,
56.3390277481738));
#197531=CARTESIAN_POINT('Ctrl Pts',(6.7006941879843,0.944979576029759,56.3474780168972));
#197532=CARTESIAN_POINT('Ctrl Pts',(6.6756729961788,1.12240071693104,56.3559208279717));
#197533=CARTESIAN_POINT('Ctrl Pts',(6.64358274223863,1.29895603264581,56.3643636390462));
#197534=CARTESIAN_POINT('Ctrl Pts',(6.60450079961785,1.47406179919539,56.3728064501208));
#197535=CARTESIAN_POINT('Ctrl Pts',(6.56544802703039,1.64903687006553,56.3812429596385));
#197536=CARTESIAN_POINT('Ctrl Pts',(6.51941404047306,1.82256422594958,56.3896794691562));
#197537=CARTESIAN_POINT('Ctrl Pts',(6.46652756365981,1.99406877224131,56.398115978674));
#197538=CARTESIAN_POINT('Ctrl Pts',(6.4136789299665,2.16545059780162,56.4065464514152));
#197539=CARTESIAN_POINT('Ctrl Pts',(6.35398768396143,2.33481218480885,56.4149769241564));
#197540=CARTESIAN_POINT('Ctrl Pts',(6.28763286896952,2.50159187419814,56.4234073968976));
#197541=CARTESIAN_POINT('Ctrl Pts',(6.22130657973267,2.66829986545113,56.4318342454015));
#197542=CARTESIAN_POINT('Ctrl Pts',(6.14832255464118,2.83242786428337,56.4402610939053));
#197543=CARTESIAN_POINT('Ctrl Pts',(6.06890883103224,2.99343191013574,56.4486879424092));
#197544=CARTESIAN_POINT('Ctrl Pts',(5.98951961960386,3.15438625978872,56.4571121898458));
#197545=CARTESIAN_POINT('Ctrl Pts',(5.9037048139639,3.31221828238127,56.4655364372824));
#197546=CARTESIAN_POINT('Ctrl Pts',(5.81173964072859,3.46640611417415,56.4739606847191));
#197547=CARTESIAN_POINT('Ctrl Pts',(5.78582737355267,3.50985034585596,56.47633431533));
#197548=CARTESIAN_POINT('Ctrl Pts',(5.75942711228635,3.55300541318139,56.478707945941));
#197549=CARTESIAN_POINT('Ctrl Pts',(5.73254566861582,3.59586000245198,56.481081576552));
#197550=CARTESIAN_POINT('Ctrl Pts',(5.63493769490564,3.75146733047175,56.4897003574892));
#197551=CARTESIAN_POINT('Ctrl Pts',(5.53102585618159,3.90304125123259,56.4983191384264));
#197552=CARTESIAN_POINT('Ctrl Pts',(5.42117282916198,4.05008322832456,56.5069379193637));
#197553=CARTESIAN_POINT('Ctrl Pts',(5.3112538140971,4.19721353263796,56.5155618775502));
#197554=CARTESIAN_POINT('Ctrl Pts',(5.19538667047351,4.33980621669734,56.5241858357367));
#197555=CARTESIAN_POINT('Ctrl Pts',(5.07397470201981,4.47739541734511,56.5328097939232));
#197556=CARTESIAN_POINT('Ctrl Pts',(4.94817653339984,4.6199552463621,56.5417453062943));
#197557=CARTESIAN_POINT('Ctrl Pts',(4.81642568281949,4.75714306734963,56.5506808186655));
#197558=CARTESIAN_POINT('Ctrl Pts',(4.67921237661769,4.88848243675968,56.5596163310366));
#197559=CARTESIAN_POINT('Ctrl Pts',(4.5465356868671,5.01547939681854,56.5682564129313));
#197560=CARTESIAN_POINT('Ctrl Pts',(4.40875222440379,5.13700827781193,56.576896494826));
#197561=CARTESIAN_POINT('Ctrl Pts',(4.26633922204371,5.25267918708648,56.5855365767207));
#197562=CARTESIAN_POINT('Ctrl Pts',(4.11662192413715,5.37428280259902,56.59461980433));
#197563=CARTESIAN_POINT('Ctrl Pts',(3.96178803430437,5.48941152268209,56.6037030319393));
#197564=CARTESIAN_POINT('Ctrl Pts',(3.80242734332519,5.59766337847614,56.6127862595487));
#197565=CARTESIAN_POINT('Ctrl Pts',(3.64306665234607,5.70591523427016,56.621869487158));
#197566=CARTESIAN_POINT('Ctrl Pts',(3.47917950770841,5.80729005040436,56.6309527147673));
#197567=CARTESIAN_POINT('Ctrl Pts',(3.31138686120923,5.90144101515985,56.6400359423767));
#197568=CARTESIAN_POINT('Ctrl Pts',(3.24132002024662,5.94075656808565,56.6438289158925));
#197569=CARTESIAN_POINT('Ctrl Pts',(3.17054541902039,5.97882838214224,56.6476218894084));
#197570=CARTESIAN_POINT('Ctrl Pts',(3.09910619832132,6.01563211736941,56.6514148629243));
#197571=CARTESIAN_POINT('Origin',(0.,0.,4.30282021618968));
#197572=CARTESIAN_POINT('',(3.09910619832129,6.01563211736943,59.0457552630241));
#197573=CARTESIAN_POINT('',(3.0991061983213,6.01563211736942,58.6514477063419));
#197574=CARTESIAN_POINT('',(3.09910619832133,6.0156321173694,4.30282021618968));
#197575=CARTESIAN_POINT('',(-6.76799881069709,0.0013588597829734,57.6954514518074));
#197576=CARTESIAN_POINT('Ctrl Pts',(-6.767,1.1904414001692E-12,57.69717978381));
#197577=CARTESIAN_POINT('Ctrl Pts',(-6.76700000000003,-0.186007249525739,
57.7059292956212));
#197578=CARTESIAN_POINT('Ctrl Pts',(-6.75932637294526,-0.372014355748844,
57.7146788074324));
#197579=CARTESIAN_POINT('Ctrl Pts',(-6.74400518264189,-0.557389537486478,
57.7234283192436));
#197580=CARTESIAN_POINT('Ctrl Pts',(-6.72868405705096,-0.742763936250848,
57.7321777940992));
#197581=CARTESIAN_POINT('Ctrl Pts',(-6.70571545645737,-0.927506130241391,
57.7409272689549));
#197582=CARTESIAN_POINT('Ctrl Pts',(-6.67517739404815,-1.1109886399008,
57.7496767438106));
#197583=CARTESIAN_POINT('Ctrl Pts',(-6.64463945808684,-1.2944703898204,
57.7584261824376));
#197584=CARTESIAN_POINT('Ctrl Pts',(-6.60653217008328,-1.47669218313805,
57.7671756210646));
#197585=CARTESIAN_POINT('Ctrl Pts',(-6.56098496092639,-1.65703510599435,
57.7759250596917));
#197586=CARTESIAN_POINT('Ctrl Pts',(-6.51543793658254,-1.83737729708852,
57.7846744628168));
#197587=CARTESIAN_POINT('Ctrl Pts',(-6.46245112167372,-2.01584035511082,
57.793423865942));
#197588=CARTESIAN_POINT('Ctrl Pts',(-6.40220448374199,-2.1918181376095,
57.8021732690672));
#197589=CARTESIAN_POINT('Ctrl Pts',(-6.3419580852644,-2.36779522067315,
57.8109226374173));
#197590=CARTESIAN_POINT('Ctrl Pts',(-6.2744520143303,-2.54128677684349,
57.8196720057674));
#197591=CARTESIAN_POINT('Ctrl Pts',(-6.19991555071816,-2.71170355385007,
57.8284213741175));
#197592=CARTESIAN_POINT('Ctrl Pts',(-6.12537937716599,-2.88211966767675,
57.8371707084193));
#197593=CARTESIAN_POINT('Ctrl Pts',(-6.04381298052419,-3.04946076371986,
57.845920042721));
#197594=CARTESIAN_POINT('Ctrl Pts',(-5.95549339335722,-3.21315848374749,
57.8546693770228));
#197595=CARTESIAN_POINT('Ctrl Pts',(-5.867174142553,-3.37685558033682,57.863418678003));
#197596=CARTESIAN_POINT('Ctrl Pts',(-5.77210188876489,-3.53690907646934,
57.8721679789832));
#197597=CARTESIAN_POINT('Ctrl Pts',(-5.67059953346888,-3.69277536969452,
57.8809172799634));
#197598=CARTESIAN_POINT('Ctrl Pts',(-5.56909755631268,-3.84864108225091,
57.8896665483486));
#197599=CARTESIAN_POINT('Ctrl Pts',(-5.46116568196727,-4.00031938297686,
57.8984158167339));
#197600=CARTESIAN_POINT('Ctrl Pts',(-5.34717048533471,-4.14729511860024,
57.9071650851192));
#197601=CARTESIAN_POINT('Ctrl Pts',(-5.23317570391704,-4.29427031888077,
57.9159143216363));
#197602=CARTESIAN_POINT('Ctrl Pts',(-5.11311782003383,-4.43654276189698,
57.9246635581533));
#197603=CARTESIAN_POINT('Ctrl Pts',(-4.98740458984623,-4.57362924351994,
57.9334127946703));
#197604=CARTESIAN_POINT('Ctrl Pts',(-4.86169180711613,-4.71071523720401,
57.9421620000458));
#197605=CARTESIAN_POINT('Ctrl Pts',(-4.73032391204042,-4.84261509523364,
57.9509112054212));
#197606=CARTESIAN_POINT('Ctrl Pts',(-4.59374707013471,-4.96888084538448,
57.9596604107967));
#197607=CARTESIAN_POINT('Ctrl Pts',(-4.45717070301289,-5.09514615659601,
57.9684095857571));
#197608=CARTESIAN_POINT('Ctrl Pts',(-4.31538563570856,-5.21577720459682,
57.9771587607176));
#197609=CARTESIAN_POINT('Ctrl Pts',(-4.16887341029293,-5.33036429233055,
57.985907935678));
#197610=CARTESIAN_POINT('Ctrl Pts',(-4.02236168203482,-5.44495099123782,
57.9946570809501));
#197611=CARTESIAN_POINT('Ctrl Pts',(-3.87112305347933,-5.55349359438764,
58.0034062262221));
#197612=CARTESIAN_POINT('Ctrl Pts',(-3.7156711701752,-5.65562346299052,
58.0121553714941));
#197613=CARTESIAN_POINT('Ctrl Pts',(-3.56021980145573,-5.75775299351796,
58.0209044878043));
#197614=CARTESIAN_POINT('Ctrl Pts',(-3.40055544538098,-5.85346967464019,
58.0296536041144));
#197615=CARTESIAN_POINT('Ctrl Pts',(-3.23722035986597,-5.94244842987041,
58.0384027204246));
#197616=CARTESIAN_POINT('Ctrl Pts',(-3.07388580146891,-6.03142689794677,
58.0471518084995));
#197617=CARTESIAN_POINT('Ctrl Pts',(-2.90688078896256,-6.11366734656935,
58.0559008965743));
#197618=CARTESIAN_POINT('Ctrl Pts',(-2.73677250721014,-6.18889046952511,
58.0646499846492));
#197619=CARTESIAN_POINT('Ctrl Pts',(-2.566664760311,-6.26411335596484,58.0733990452152));
#197620=CARTESIAN_POINT('Ctrl Pts',(-2.39345402574757,-6.33231884500711,
58.0821481057813));
#197621=CARTESIAN_POINT('Ctrl Pts',(-2.21772856065155,-6.39327529762878,
58.0908971663473));
#197622=CARTESIAN_POINT('Ctrl Pts',(-2.04200363348044,-6.4542315636526,
58.099646200131));
#197623=CARTESIAN_POINT('Ctrl Pts',(-1.86376426188776,-6.50793874375803,
58.1083952339147));
#197624=CARTESIAN_POINT('Ctrl Pts',(-1.68361577752619,-6.55421443909679,
58.1171442676984));
#197625=CARTESIAN_POINT('Ctrl Pts',(-1.50346782967279,-6.60048999661986,
58.1258932754262));
#197626=CARTESIAN_POINT('Ctrl Pts',(-1.32141105794483,-6.63933404237812,
58.1346422831541));
#197627=CARTESIAN_POINT('Ctrl Pts',(-1.13806375486535,-6.67061465607644,
58.1433912908819));
#197628=CARTESIAN_POINT('Ctrl Pts',(-0.954716982598694,-6.70189517921356,
58.1521402732803));
#197629=CARTESIAN_POINT('Ctrl Pts',(-0.770079968898376,-6.7256122659227,
58.1608892556786));
#197630=CARTESIAN_POINT('Ctrl Pts',(-0.584779765555054,-6.7416853698313,
58.169638238077));
#197631=CARTESIAN_POINT('Ctrl Pts',(-0.391489830648159,-6.75845151013871,
58.1787644570869));
#197632=CARTESIAN_POINT('Ctrl Pts',(-0.197478578235256,-6.76689983031634,
58.1878906760967));
#197633=CARTESIAN_POINT('Ctrl Pts',(-0.00346287644832417,-6.76699911397118,
58.1970168951066));
#197634=CARTESIAN_POINT('Ctrl Pts',(0.184489834657796,-6.7670952950118,
58.2058579197724));
#197635=CARTESIAN_POINT('Ctrl Pts',(0.372446404253271,-6.75935639738147,
58.2146989444382));
#197636=CARTESIAN_POINT('Ctrl Pts',(0.559755019492222,-6.74380925873154,
58.223539969104));
#197637=CARTESIAN_POINT('Ctrl Pts',(0.7451347055257,-6.72842222659762,58.2322899477138));
#197638=CARTESIAN_POINT('Ctrl Pts',(0.929879431232527,-6.70538706057469,
58.2410399263235));
#197639=CARTESIAN_POINT('Ctrl Pts',(1.11336163627224,-6.67478200894061,
58.2497899049333));
#197640=CARTESIAN_POINT('Ctrl Pts',(1.29684196301129,-6.64417727060933,
58.2585397939698));
#197641=CARTESIAN_POINT('Ctrl Pts',(1.47905951217931,-6.60600284890497,
58.2672896830063));
#197642=CARTESIAN_POINT('Ctrl Pts',(1.65939532067515,-6.56038841607122,
58.2760395720429));
#197643=CARTESIAN_POINT('Ctrl Pts',(1.83972934301232,-6.51477443503135,
58.284789374415));
#197644=CARTESIAN_POINT('Ctrl Pts',(2.01818138406693,-6.46172066062007,
58.2935391767872));
#197645=CARTESIAN_POINT('Ctrl Pts',(2.19414528354626,-6.40140730423332,
58.3022889791593));
#197646=CARTESIAN_POINT('Ctrl Pts',(2.37010749864418,-6.34109452518486,
58.3110386977757));
#197647=CARTESIAN_POINT('Ctrl Pts',(2.5435813486687,-6.27352239616337,58.319788416392));
#197648=CARTESIAN_POINT('Ctrl Pts',(2.71397759435957,-6.19892043966643,
58.3285381350083));
#197649=CARTESIAN_POINT('Ctrl Pts',(2.88437226558517,-6.1243191724933,58.337287772777));
#197650=CARTESIAN_POINT('Ctrl Pts',(3.0516891268134,-6.04268832278604,58.3460374105457));
#197651=CARTESIAN_POINT('Ctrl Pts',(3.2153598627423,-5.95430516123131,58.3547870483144));
#197652=CARTESIAN_POINT('Ctrl Pts',(3.37902914073225,-5.8659227869722,58.3635366081435));
#197653=CARTESIAN_POINT('Ctrl Pts',(3.53905210621962,-5.77078835741703,
58.3722861679726));
#197654=CARTESIAN_POINT('Ctrl Pts',(3.69488522832093,-5.66922500431372,
58.3810357278016));
#197655=CARTESIAN_POINT('Ctrl Pts',(3.8507170140734,-5.56766252216817,58.3897852125988));
#197656=CARTESIAN_POINT('Ctrl Pts',(4.00235878822809,-5.45967138329074,
58.3985346973959));
#197657=CARTESIAN_POINT('Ctrl Pts',(4.14929549611733,-5.34561838199291,
58.407284182193));
#197658=CARTESIAN_POINT('Ctrl Pts',(4.29623099276496,-5.23156632086682,
58.4160335948656));
#197659=CARTESIAN_POINT('Ctrl Pts',(4.43846127436432,-5.11145267304613,
58.4247830075382));
#197660=CARTESIAN_POINT('Ctrl Pts',(4.57550326054843,-4.98568540049517,
58.4335324202108));
#197661=CARTESIAN_POINT('Ctrl Pts',(4.71254416258175,-4.85991912289978,
58.442281763666));
#197662=CARTESIAN_POINT('Ctrl Pts',(4.84439664019148,-4.72849950385022,
58.4510311071213));
#197663=CARTESIAN_POINT('Ctrl Pts',(4.97061286795124,-4.59187289860657,
58.4597804505765));
#197664=CARTESIAN_POINT('Ctrl Pts',(5.09682813913048,-4.45524732884269,
58.4685297277214));
#197665=CARTESIAN_POINT('Ctrl Pts',(5.21740705148187,-4.31341506235366,
58.4772790048662));
#197666=CARTESIAN_POINT('Ctrl Pts',(5.33194007546028,-4.16685781275299,
58.486028282011));
#197667=CARTESIAN_POINT('Ctrl Pts',(5.44647226944806,-4.02030162521407,
58.4947774957521));
#197668=CARTESIAN_POINT('Ctrl Pts',(5.55495848628422,-3.8690207488749,58.5035267094933));
#197669=CARTESIAN_POINT('Ctrl Pts',(5.65703027292085,-3.7135289808021,58.5122759232344));
#197670=CARTESIAN_POINT('Ctrl Pts',(5.75910135377282,-3.55803828789128,
58.5210250764783));
#197671=CARTESIAN_POINT('Ctrl Pts',(5.85475793593024,-3.39833700106244,
58.5297742297221));
#197672=CARTESIAN_POINT('Ctrl Pts',(5.94367514427657,-3.23496750823078,
58.538523382966));
#197673=CARTESIAN_POINT('Ctrl Pts',(6.03259176732892,-3.07159909077231,
58.547272478619));
#197674=CARTESIAN_POINT('Ctrl Pts',(6.11476896836168,-2.90456276730922,
58.5560215742719));
#197675=CARTESIAN_POINT('Ctrl Pts',(6.1899276554812,-2.73442583002521,58.5647706699248));
#197676=CARTESIAN_POINT('Ctrl Pts',(6.26508587283272,-2.56428995615637,
58.5735197108929));
#197677=CARTESIAN_POINT('Ctrl Pts',(6.33322554827363,-2.39105376934665,
58.5822687518609));
#197678=CARTESIAN_POINT('Ctrl Pts',(6.39411526733217,-2.21530561053541,
58.5910177928289));
#197679=CARTESIAN_POINT('Ctrl Pts',(6.4550046260302,-2.03955849184554,58.599766782018));
#197680=CARTESIAN_POINT('Ctrl Pts',(6.50864402040897,-1.86129970163995,
58.608515771207));
#197681=CARTESIAN_POINT('Ctrl Pts',(6.55485128368743,-1.68113463135505,
58.617264760396));
#197682=CARTESIAN_POINT('Ctrl Pts',(6.60199809554447,-1.49730620116336,
58.6261916458674));
#197683=CARTESIAN_POINT('Ctrl Pts',(6.64140720707974,-1.31149343245187,
58.6351185313388));
#197684=CARTESIAN_POINT('Ctrl Pts',(6.67293928722966,-1.12435326697037,
58.6440454168103));
#197685=CARTESIAN_POINT('Ctrl Pts',(6.70384625876325,-0.940923067001745,
58.6527953309877));
#197686=CARTESIAN_POINT('Ctrl Pts',(6.7271855457985,-0.756217899516862,
58.6615452451652));
#197687=CARTESIAN_POINT('Ctrl Pts',(6.74287786815368,-0.570865181249742,
58.6702951593427));
#197688=CARTESIAN_POINT('Ctrl Pts',(6.75856988190873,-0.385516108069222,
58.6790449014471));
#197689=CARTESIAN_POINT('Ctrl Pts',(6.76661520773417,-0.199519795221659,
58.6877946435516));
#197690=CARTESIAN_POINT('Ctrl Pts',(6.7669865178958,-0.0135080204510007,
58.6965443856561));
#197691=CARTESIAN_POINT('Ctrl Pts',(6.76735782124891,0.172500343517631,
58.7052939673211));
#197692=CARTESIAN_POINT('Ctrl Pts',(6.76005538995159,0.358523882215608,
58.7140435489861));
#197693=CARTESIAN_POINT('Ctrl Pts',(6.74510402742323,0.543930748569076,
58.722793130651));
#197694=CARTESIAN_POINT('Ctrl Pts',(6.7301529191798,0.729334461619886,58.7315425635077));
#197695=CARTESIAN_POINT('Ctrl Pts',(6.70755316306532,0.914121237639279,
58.7402919963644));
#197696=CARTESIAN_POINT('Ctrl Pts',(6.677381518745,1.09766345166576,58.7490414292211));
#197697=CARTESIAN_POINT('Ctrl Pts',(6.64721034747483,1.28120278800113,58.7577907248986));
#197698=CARTESIAN_POINT('Ctrl Pts',(6.60946757205044,1.46349731860771,58.7665400205761));
#197699=CARTESIAN_POINT('Ctrl Pts',(6.56428138111414,1.64392790278598,58.7752893162536));
#197700=CARTESIAN_POINT('Ctrl Pts',(6.51909583859729,1.82435589779488,58.7840384863792));
#197701=CARTESIAN_POINT('Ctrl Pts',(6.46646716392743,2.00291972192693,58.7927876565048));
#197702=CARTESIAN_POINT('Ctrl Pts',(6.4065740987274,2.17901292275086,58.8015368266304));
#197703=CARTESIAN_POINT('Ctrl Pts',(6.34668181341923,2.3551038305939,58.8102858828295));
#197704=CARTESIAN_POINT('Ctrl Pts',(6.27952541913887,2.52872390822984,58.8190349390287));
#197705=CARTESIAN_POINT('Ctrl Pts',(6.20533299175345,2.69928350890679,58.8277839952278));
#197706=CARTESIAN_POINT('Ctrl Pts',(6.12831602991371,2.87633637966001,58.836866131386));
#197707=CARTESIAN_POINT('Ctrl Pts',(6.04371690605088,3.05009086601823,58.8459482675441));
#197708=CARTESIAN_POINT('Ctrl Pts',(5.95184520316445,3.21991112883079,58.8550304037023));
#197709=CARTESIAN_POINT('Ctrl Pts',(5.86333549509076,3.38351691183362,58.8637801840459));
#197710=CARTESIAN_POINT('Ctrl Pts',(5.76807618099157,3.54347103712348,58.8725299643895));
#197711=CARTESIAN_POINT('Ctrl Pts',(5.66639083308792,3.69923018028039,58.881279744733));
#197712=CARTESIAN_POINT('Ctrl Pts',(5.56470914081962,3.85498372382395,58.8900292105179));
#197713=CARTESIAN_POINT('Ctrl Pts',(5.45660203371814,4.00654234702343,58.8987786763029));
#197714=CARTESIAN_POINT('Ctrl Pts',(5.34243669838949,4.15339127987014,58.9075281420878));
#197715=CARTESIAN_POINT('Ctrl Pts',(5.22827486050311,4.30023571401621,58.9162773398338));
#197716=CARTESIAN_POINT('Ctrl Pts',(5.10805534166817,4.44237052028808,58.9250265375798));
#197717=CARTESIAN_POINT('Ctrl Pts',(4.98218644339644,4.57931296629055,58.9337757353258));
#197718=CARTESIAN_POINT('Ctrl Pts',(4.8563207321927,4.71625194483686,58.9425247115375));
#197719=CARTESIAN_POINT('Ctrl Pts',(4.72480612169994,4.84799861524825,58.9512736877491));
#197720=CARTESIAN_POINT('Ctrl Pts',(4.58808925234978,4.97410554898793,58.9600226639607));
#197721=CARTESIAN_POINT('Ctrl Pts',(4.45136349473707,5.10022068121504,58.9687722089624));
#197722=CARTESIAN_POINT('Ctrl Pts',(4.30943501209732,5.22069514872121,58.9775217539641));
#197723=CARTESIAN_POINT('Ctrl Pts',(4.16278587431427,5.33511975166534,58.9862712989658));
#197724=CARTESIAN_POINT('Ctrl Pts',(4.01614535740073,5.44953762808119,58.9950203296196));
#197725=CARTESIAN_POINT('Ctrl Pts',(3.86478496657528,5.55790617533059,59.0037693602733));
#197726=CARTESIAN_POINT('Ctrl Pts',(3.7092187474678,5.65985735539629,59.012518390927));
#197727=CARTESIAN_POINT('Ctrl Pts',(3.55365041605485,5.76180991977303,59.0212675403766));
#197728=CARTESIAN_POINT('Ctrl Pts',(3.39387638174108,5.85734478553053,59.0300166898263));
#197729=CARTESIAN_POINT('Ctrl Pts',(3.23043927904125,5.94613749121457,59.0387658392759));
#197730=CARTESIAN_POINT('Ctrl Pts',(3.1869176707015,5.96978206944296,59.041095647192));
#197731=CARTESIAN_POINT('Ctrl Pts',(3.14313645919485,5.99294880633501,59.0434254551081));
#197732=CARTESIAN_POINT('Ctrl Pts',(3.09910619832129,6.01563211736943,59.0457552630241));
#197733=CARTESIAN_POINT('Ctrl Pts',(3.09910619832134,6.0156321173694,57.0459010634246));
#197734=CARTESIAN_POINT('Ctrl Pts',(2.93708941130078,6.09909919432674,57.0544544424911));
#197735=CARTESIAN_POINT('Ctrl Pts',(2.77164155858761,6.17604560811617,57.0630078215577));
#197736=CARTESIAN_POINT('Ctrl Pts',(2.60333644578525,6.24619310860994,57.0715612006242));
#197737=CARTESIAN_POINT('Ctrl Pts',(2.44204607508404,6.31341695089267,57.0797580857777));
#197738=CARTESIAN_POINT('Ctrl Pts',(2.27813215886749,6.37439700936649,57.0879549709313));
#197739=CARTESIAN_POINT('Ctrl Pts',(2.1121209293986,6.42893725117895,57.0961518560848));
#197740=CARTESIAN_POINT('Ctrl Pts',(1.94609294049766,6.48348299902543,57.1043495687434));
#197741=CARTESIAN_POINT('Ctrl Pts',(1.77796755733578,6.53158752260565,57.112547281402));
#197742=CARTESIAN_POINT('Ctrl Pts',(1.60828684773392,6.57310447318511,57.1207449940607));
#197743=CARTESIAN_POINT('Ctrl Pts',(1.43855815497868,6.61463316413395,57.1289450249092));
#197744=CARTESIAN_POINT('Ctrl Pts',(1.26727360808535,6.64957048589982,57.1371450557577));
#197745=CARTESIAN_POINT('Ctrl Pts',(1.09498620479806,6.67782106763141,57.1453450866062));
#197746=CARTESIAN_POINT('Ctrl Pts',(0.92261875341179,6.7060847751361,57.1535489273495));
#197747=CARTESIAN_POINT('Ctrl Pts',(0.749247871090595,6.72765549585866,
57.1617527680928));
#197748=CARTESIAN_POINT('Ctrl Pts',(0.575432475817302,6.74248963408731,
57.1699566088361));
#197749=CARTESIAN_POINT('Ctrl Pts',(0.401412906582284,6.75734119738216,
57.1781700863015));
#197750=CARTESIAN_POINT('Ctrl Pts',(0.226948139060304,6.76544034478136,
57.186383563767));
#197751=CARTESIAN_POINT('Ctrl Pts',(0.0525988345949597,6.76679557564726,
57.1945970412324));
#197752=CARTESIAN_POINT('Ctrl Pts',(-0.12187074230351,6.76815174140024,
57.2028161846506));
#197753=CARTESIAN_POINT('Ctrl Pts',(-0.296224340113023,6.76275472968003,
57.2110353280687));
#197754=CARTESIAN_POINT('Ctrl Pts',(-0.469905747545066,6.75066497379511,
57.2192544714869));
#197755=CARTESIAN_POINT('Ctrl Pts',(-0.643826689135678,6.73855854422275,
57.2274849504051));
#197756=CARTESIAN_POINT('Ctrl Pts',(-0.817073234136335,6.71974097753192,
57.2357154293233));
#197757=CARTESIAN_POINT('Ctrl Pts',(-0.989097810834744,6.69432405255392,
57.2439459082416));
#197758=CARTESIAN_POINT('Ctrl Pts',(-1.03951258960042,6.68687518289667,
57.2463579925016));
#197759=CARTESIAN_POINT('Ctrl Pts',(-1.08982250582229,6.67885983380128,
57.2487700767617));
#197760=CARTESIAN_POINT('Ctrl Pts',(-1.14001402095487,6.67028163063797,
57.2511821610217));
#197761=CARTESIAN_POINT('Ctrl Pts',(-1.30792310384148,6.64158438525373,
57.2592514702443));
#197762=CARTESIAN_POINT('Ctrl Pts',(-1.47505567297142,6.60649022861081,
57.2673207794668));
#197763=CARTESIAN_POINT('Ctrl Pts',(-1.64087397246921,6.56504543826417,
57.2753900886893));
#197764=CARTESIAN_POINT('Ctrl Pts',(-1.8064854514793,6.52365234083548,57.2834493332901));
#197765=CARTESIAN_POINT('Ctrl Pts',(-1.97078556511015,6.47592445964785,
57.2915085778908));
#197766=CARTESIAN_POINT('Ctrl Pts',(-2.13324219989485,6.42195972555012,
57.2995678224915));
#197767=CARTESIAN_POINT('Ctrl Pts',(-2.29553185794315,6.36805045767076,
57.3076187836118));
#197768=CARTESIAN_POINT('Ctrl Pts',(-2.45598145665742,6.30791721029896,
57.3156697447321));
#197769=CARTESIAN_POINT('Ctrl Pts',(-2.61406969909475,6.24170878912776,
57.3237207058524));
#197770=CARTESIAN_POINT('Ctrl Pts',(-2.77203009500253,6.17555391094459,
57.3317651561315));
#197771=CARTESIAN_POINT('Ctrl Pts',(-2.92763259301981,6.10333378089565,
57.3398096064106));
#197772=CARTESIAN_POINT('Ctrl Pts',(-3.08037178251789,6.02524677349132,
57.3478540566897));
#197773=CARTESIAN_POINT('Ctrl Pts',(-3.23302088446625,5.94720582281405,
57.355893762248));
#197774=CARTESIAN_POINT('Ctrl Pts',(-3.38280970842921,5.86330505275075,
57.3639334678062));
#197775=CARTESIAN_POINT('Ctrl Pts',(-3.52925364102936,5.77379058654546,
57.3719731733645));
#197776=CARTESIAN_POINT('Ctrl Pts',(-3.67885848762091,5.68234399844453,
57.3801864116689));
#197777=CARTESIAN_POINT('Ctrl Pts',(-3.82497203811319,5.58503877621496,
57.3883996499734));
#197778=CARTESIAN_POINT('Ctrl Pts',(-3.9671045819061,5.48218662909424,57.3966128882778));
#197779=CARTESIAN_POINT('Ctrl Pts',(-4.10618930336944,5.38153999425293,
57.404650005826));
#197780=CARTESIAN_POINT('Ctrl Pts',(-4.24146171358088,5.27558215213335,
57.4126871233742));
#197781=CARTESIAN_POINT('Ctrl Pts',(-4.37249307772857,5.1646484183549,57.4207242409224));
#197782=CARTESIAN_POINT('Ctrl Pts',(-4.50353830416122,5.05370294849295,
57.4287622087465));
#197783=CARTESIAN_POINT('Ctrl Pts',(-4.63034130590809,4.93778078013822,
57.4368001765706));
#197784=CARTESIAN_POINT('Ctrl Pts',(-4.75250748493224,4.81725664726959,
57.4448381443947));
#197785=CARTESIAN_POINT('Ctrl Pts',(-4.87471079398519,4.69669588344007,
57.4528785552024));
#197786=CARTESIAN_POINT('Ctrl Pts',(-4.99227420935914,4.57153063329252,
57.4609189660102));
#197787=CARTESIAN_POINT('Ctrl Pts',(-5.10484107074446,4.44217138823353,
57.4689593768179));
#197788=CARTESIAN_POINT('Ctrl Pts',(-5.22166232460481,4.30792309330691,
57.4773036698057));
#197789=CARTESIAN_POINT('Ctrl Pts',(-5.33310166985868,4.16915792692092,
57.4856479627935));
#197790=CARTESIAN_POINT('Ctrl Pts',(-5.4388081030987,4.02637000506262,57.4939922557813));
#197791=CARTESIAN_POINT('Ctrl Pts',(-5.54084480270537,3.88853914800367,
57.5020468659968));
#197792=CARTESIAN_POINT('Ctrl Pts',(-5.63753981844651,3.74696050612187,
57.5101014762123));
#197793=CARTESIAN_POINT('Ctrl Pts',(-5.72862340538127,3.60210533984195,
57.5181560864279));
#197794=CARTESIAN_POINT('Ctrl Pts',(-5.81977594387776,3.4571405161553,57.5262167940971));
#197795=CARTESIAN_POINT('Ctrl Pts',(-5.90530841004553,3.30889455068405,
57.5342775017664));
#197796=CARTESIAN_POINT('Ctrl Pts',(-5.98499812208102,3.15786106070021,
57.5423382094356));
#197797=CARTESIAN_POINT('Ctrl Pts',(-6.06480019183685,3.00661462254282,
57.5504102822198));
#197798=CARTESIAN_POINT('Ctrl Pts',(-6.13874291127432,2.8525731519391,57.558482355004));
#197799=CARTESIAN_POINT('Ctrl Pts',(-6.2066523592396,2.69624841057822,57.5665544277882));
#197800=CARTESIAN_POINT('Ctrl Pts',(-6.2137653579533,2.67987458164076,57.5673999160825));
#197801=CARTESIAN_POINT('Ctrl Pts',(-6.22081221150533,2.66347571459303,
57.5682454043769));
#197802=CARTESIAN_POINT('Ctrl Pts',(-6.2277927521944,2.64705240516974,57.5690908926713));
#197803=CARTESIAN_POINT('Ctrl Pts',(-6.30728184109723,2.46003624682668,
57.5787186704022));
#197804=CARTESIAN_POINT('Ctrl Pts',(-6.37837738907553,2.26935700482112,
57.5883464481332));
#197805=CARTESIAN_POINT('Ctrl Pts',(-6.44078272410078,2.0757184059802,57.5979742258642));
#197806=CARTESIAN_POINT('Ctrl Pts',(-6.50285624708936,1.88310939247571,
57.6075508122582));
#197807=CARTESIAN_POINT('Ctrl Pts',(-6.5563316696614,1.68757250775811,57.6171273986522));
#197808=CARTESIAN_POINT('Ctrl Pts',(-6.60096333987442,1.48982280343468,
57.6267039850461));
#197809=CARTESIAN_POINT('Ctrl Pts',(-6.6454136680469,1.29287657195301,57.6362416610047));
#197810=CARTESIAN_POINT('Ctrl Pts',(-6.68109188231582,1.09373556062145,
57.6457793369633));
#197811=CARTESIAN_POINT('Ctrl Pts',(-6.70780239938444,0.893127074280214,
57.6553170129219));
#197812=CARTESIAN_POINT('Ctrl Pts',(-6.73431424062455,0.694010736411043,
57.6647837465746));
#197813=CARTESIAN_POINT('Ctrl Pts',(-6.75199122402378,0.493448781645467,
57.6742504802273));
#197814=CARTESIAN_POINT('Ctrl Pts',(-6.76068966814693,0.29217154380841,
57.68371721388));
#197815=CARTESIAN_POINT('Ctrl Pts',(-6.76481299855797,0.19675993409133,
57.68820473719));
#197816=CARTESIAN_POINT('Ctrl Pts',(-6.76691950451404,0.101187865534849,
57.6926922605));
#197817=CARTESIAN_POINT('Ctrl Pts',(-6.76699773672647,0.00553454053396756,
57.69717978381));
#197818=CARTESIAN_POINT('',(-6.76699833040872,0.00475355083741498,57.3028202162319));
#197819=CARTESIAN_POINT('Ctrl Pts',(3.09910619832132,6.01563211736941,56.6514148629243));
#197820=CARTESIAN_POINT('Ctrl Pts',(2.9288158558623,6.10336152726886,56.6604562095772));
#197821=CARTESIAN_POINT('Ctrl Pts',(2.75474742236709,6.18388246268263,56.6694975562302));
#197822=CARTESIAN_POINT('Ctrl Pts',(2.57750328655722,6.2568974586281,56.6785389028831));
#197823=CARTESIAN_POINT('Ctrl Pts',(2.40043744629085,6.32983900645453,56.6875711545564));
#197824=CARTESIAN_POINT('Ctrl Pts',(2.22020250089245,6.39528959756098,56.6966034062296));
#197825=CARTESIAN_POINT('Ctrl Pts',(2.03742186377874,6.45299939167798,56.7056356579029));
#197826=CARTESIAN_POINT('Ctrl Pts',(1.8549763315794,6.51060338227049,56.7146513500983));
#197827=CARTESIAN_POINT('Ctrl Pts',(1.66999465320859,6.56049484068034,56.7236670422936));
#197828=CARTESIAN_POINT('Ctrl Pts',(1.48311635673492,6.60247339050945,56.732682734489));
#197829=CARTESIAN_POINT('Ctrl Pts',(1.29648441379771,6.64439660184072,56.7416865416891));
#197830=CARTESIAN_POINT('Ctrl Pts',(1.10796107345928,6.67842766797474,56.7506903488893));
#197831=CARTESIAN_POINT('Ctrl Pts',(0.918199525888249,6.70441635272293,
56.7596941560894));
#197832=CARTESIAN_POINT('Ctrl Pts',(0.728849668397189,6.73034865469053,
56.7686784294158));
#197833=CARTESIAN_POINT('Ctrl Pts',(0.538267200699625,6.74827336726381,
56.7776627027423));
#197834=CARTESIAN_POINT('Ctrl Pts',(0.347113800198479,6.75809152125893,
56.7866469760687));
#197835=CARTESIAN_POINT('Ctrl Pts',(0.259573056317174,6.7625878498726,56.7907614201129));
#197836=CARTESIAN_POINT('Ctrl Pts',(0.171912726692458,6.76538470783889,
56.7948758641572));
#197837=CARTESIAN_POINT('Ctrl Pts',(0.0841970533280191,6.76647617717013,
56.7989903082014));
#197838=CARTESIAN_POINT('Ctrl Pts',(-0.0889441416684437,6.76863061886869,
56.8071117730576));
#197839=CARTESIAN_POINT('Ctrl Pts',(-0.262223833179623,6.76413588094265,
56.8152332379138));
#197840=CARTESIAN_POINT('Ctrl Pts',(-0.435089414198062,6.75299831198356,
56.82335470277));
#197841=CARTESIAN_POINT('Ctrl Pts',(-0.607942667356204,6.74186153729707,
56.8314755884462));
#197842=CARTESIAN_POINT('Ctrl Pts',(-0.780381503416446,6.72408289872817,
56.8395964741224));
#197843=CARTESIAN_POINT('Ctrl Pts',(-0.951856303852425,6.69972078349661,
56.8477173597986));
#197844=CARTESIAN_POINT('Ctrl Pts',(-1.12335160043043,6.67535575629564,
56.8558392161529));
#197845=CARTESIAN_POINT('Ctrl Pts',(-1.29388226956476,6.64440573820314,
56.8639610725071));
#197846=CARTESIAN_POINT('Ctrl Pts',(-1.46290682470662,6.60698059799079,
56.8720829288614));
#197847=CARTESIAN_POINT('Ctrl Pts',(-1.63205469807292,6.56952815285914,
56.8802107108216));
#197848=CARTESIAN_POINT('Ctrl Pts',(-1.79969390486481,6.52559122939987,
56.8883384927817));
#197849=CARTESIAN_POINT('Ctrl Pts',(-1.96529548865556,6.47533031144127,
56.8964662747419));
#197850=CARTESIAN_POINT('Ctrl Pts',(-2.13096453237613,6.4250489190529,56.9045973676583));
#197851=CARTESIAN_POINT('Ctrl Pts',(-2.29459395275117,6.36843851679601,
56.9127284605748));
#197852=CARTESIAN_POINT('Ctrl Pts',(-2.45567308105799,6.30570842324375,
56.9208595534912));
#197853=CARTESIAN_POINT('Ctrl Pts',(-2.61692802050191,6.24290986241585,
56.9289995211558));
#197854=CARTESIAN_POINT('Ctrl Pts',(-2.77562677276144,6.17397841504057,
56.9371394888204));
#197855=CARTESIAN_POINT('Ctrl Pts',(-2.93128096700278,6.09917050855994,
56.9452794564849));
#197856=CARTESIAN_POINT('Ctrl Pts',(-3.01200996219032,6.06037189377348,
56.9495011956653));
#197857=CARTESIAN_POINT('Ctrl Pts',(-3.09192042237868,6.01999331053127,
56.9537229348457));
#197858=CARTESIAN_POINT('Ctrl Pts',(-3.17094717972885,5.9780751905082,56.9579446740261));
#197859=CARTESIAN_POINT('Ctrl Pts',(-3.32893950381451,5.89427140776661,
56.9663848834837));
#197860=CARTESIAN_POINT('Ctrl Pts',(-3.48372465004122,5.80413841391356,
56.9748250929413));
#197861=CARTESIAN_POINT('Ctrl Pts',(-3.63478172484608,5.70794628677644,
56.9832653023989));
#197862=CARTESIAN_POINT('Ctrl Pts',(-3.78572435153768,5.61182703942649,
56.9916991171475));
#197863=CARTESIAN_POINT('Ctrl Pts',(-3.93294425710903,5.5096579885086,57.000132931896));
#197864=CARTESIAN_POINT('Ctrl Pts',(-4.07594610930425,5.40175455884915,
57.0085667466445));
#197865=CARTESIAN_POINT('Ctrl Pts',(-4.21886159964126,5.29391629436448,
57.0169954680331));
#197866=CARTESIAN_POINT('Ctrl Pts',(-4.35756384961711,5.18035075571406,
57.0254241894216));
#197867=CARTESIAN_POINT('Ctrl Pts',(-4.49158710898992,5.0614162289181,57.0338529108102));
#197868=CARTESIAN_POINT('Ctrl Pts',(-4.62555000920494,4.94253526586851,
57.0422778362119));
#197869=CARTESIAN_POINT('Ctrl Pts',(-4.754837871411,4.81829035686463,57.0507027616137));
#197870=CARTESIAN_POINT('Ctrl Pts',(-4.87901830230743,4.68907980373006,
57.0591276870154));
#197871=CARTESIAN_POINT('Ctrl Pts',(-5.00316185985319,4.5599076175588,57.0675501107731));
#197872=CARTESIAN_POINT('Ctrl Pts',(-5.12220077962333,4.42577296785309,
57.0759725345309));
#197873=CARTESIAN_POINT('Ctrl Pts',(-5.23573952232929,4.28711099160251,
57.0843949582886));
#197874=CARTESIAN_POINT('Ctrl Pts',(-5.34928005067248,4.14844683459864,
57.0928175145069));
#197875=CARTESIAN_POINT('Ctrl Pts',(-5.45732001275269,4.00525546253049,
57.101240070725));
#197876=CARTESIAN_POINT('Ctrl Pts',(-5.5595037461799,3.85800558530073,57.1096626269433));
#197877=CARTESIAN_POINT('Ctrl Pts',(-5.66169093139295,3.71075073394229,
57.118085467677));
#197878=CARTESIAN_POINT('Ctrl Pts',(-5.75802130319094,3.5594373780211,57.1265083084108));
#197879=CARTESIAN_POINT('Ctrl Pts',(-5.84818210335718,3.40456386134447,
57.1349311491445));
#197880=CARTESIAN_POINT('Ctrl Pts',(-5.93835853661733,3.24966349095508,
57.1433554503251));
#197881=CARTESIAN_POINT('Ctrl Pts',(-6.02236309766209,3.09120201736223,
57.1517797515058));
#197882=CARTESIAN_POINT('Ctrl Pts',(-6.0999284488278,2.92970338416388,57.1602040526864));
#197883=CARTESIAN_POINT('Ctrl Pts',(-6.17751808144624,2.76815419461056,
57.1686309910532));
#197884=CARTESIAN_POINT('Ctrl Pts',(-6.24866434094537,2.60356625044192,
57.17705792942));
#197885=CARTESIAN_POINT('Ctrl Pts',(-6.31314744019751,2.43648484467433,
57.1854848677868));
#197886=CARTESIAN_POINT('Ctrl Pts',(-6.37768851786137,2.26925321172088,
57.1939193830305));
#197887=CARTESIAN_POINT('Ctrl Pts',(-6.43555434405825,2.09952394891718,
57.2023538982741));
#197888=CARTESIAN_POINT('Ctrl Pts',(-6.48657419007526,1.92786002517027,
57.2107884135178));
#197889=CARTESIAN_POINT('Ctrl Pts',(-6.53761867911499,1.75611318627751,
57.2192270027045));
#197890=CARTESIAN_POINT('Ctrl Pts',(-6.58181050603663,1.58243014458215,
57.2276655918913));
#197891=CARTESIAN_POINT('Ctrl Pts',(-6.61902964998118,1.4073860496218,57.2361041810781));
#197892=CARTESIAN_POINT('Ctrl Pts',(-6.65629039650801,1.23214629496615,
57.2445522026984));
#197893=CARTESIAN_POINT('Ctrl Pts',(-6.6865628251688,1.05554277504005,57.2530002243187));
#197894=CARTESIAN_POINT('Ctrl Pts',(-6.70977836961247,0.878159000796931,
57.261448245939));
#197895=CARTESIAN_POINT('Ctrl Pts',(-6.72297371250336,0.777336910231834,
57.2662499658513));
#197896=CARTESIAN_POINT('Ctrl Pts',(-6.73389020537125,0.67626284025593,
57.2710516857635));
#197897=CARTESIAN_POINT('Ctrl Pts',(-6.74252275698126,0.57504423446365,
57.2758534056758));
#197898=CARTESIAN_POINT('Ctrl Pts',(-6.75868310423,0.385560534680092,57.2848423425139));
#197899=CARTESIAN_POINT('Ctrl Pts',(-6.76686449420557,0.195278323762471,
57.2938312793519));
#197900=CARTESIAN_POINT('Ctrl Pts',(-6.7669983304081,0.00475355172657754,
57.3028202161899));
#197901=CARTESIAN_POINT('Ctrl Pts',(-6.76699833040872,0.00475355083741949,
57.3028202162319));
#197902=CARTESIAN_POINT('Ctrl Pts',(-6.76711724571589,-0.164530361876449,
57.3108070117694));
#197903=CARTESIAN_POINT('Ctrl Pts',(-6.76087979991684,-0.334076059823817,
57.3187938073069));
#197904=CARTESIAN_POINT('Ctrl Pts',(-6.74825359655539,-0.503351166262,57.3267806028444));
#197905=CARTESIAN_POINT('Ctrl Pts',(-6.73563867023757,-0.672475085307733,
57.334760265007));
#197906=CARTESIAN_POINT('Ctrl Pts',(-6.71664636501254,-0.841328517593721,
57.3427399271696));
#197907=CARTESIAN_POINT('Ctrl Pts',(-6.69129630022003,-1.00937744311123,
57.3507195893322));
#197908=CARTESIAN_POINT('Ctrl Pts',(-6.66596532811808,-1.17729980066293,
57.3586932415212));
#197909=CARTESIAN_POINT('Ctrl Pts',(-6.63428618501412,-1.34441848357119,
57.3666668937102));
#197910=CARTESIAN_POINT('Ctrl Pts',(-6.59633041995841,-1.5102032945042,
57.3746405458993));
#197911=CARTESIAN_POINT('Ctrl Pts',(-6.55839134800311,-1.67591519260062,
57.3826106912435));
#197912=CARTESIAN_POINT('Ctrl Pts',(-6.51418123128944,-1.84029401639184,
57.3905808365877));
#197913=CARTESIAN_POINT('Ctrl Pts',(-6.46382293043131,-2.00281854495867,
57.3985509819319));
#197914=CARTESIAN_POINT('Ctrl Pts',(-6.41347226683219,-2.16531842531661,
57.4065199185367));
#197915=CARTESIAN_POINT('Ctrl Pts',(-6.35697538289133,-2.32596420604132,
57.4144888551415));
#197916=CARTESIAN_POINT('Ctrl Pts',(-6.29450531389351,-2.48424875029986,
57.4224577917463));
#197917=CARTESIAN_POINT('Ctrl Pts',(-6.26223400319354,-2.56601670395697,
57.4265744516643));
#197918=CARTESIAN_POINT('Ctrl Pts',(-6.22836947764888,-2.64715478973649,
57.4306911115824));
#197919=CARTESIAN_POINT('Ctrl Pts',(-6.19294068818362,-2.72759502724284,
57.4348077715005));
#197920=CARTESIAN_POINT('Ctrl Pts',(-6.11669774364076,-2.90070284886974,
57.4436668456763));
#197921=CARTESIAN_POINT('Ctrl Pts',(-6.03326763538907,-3.07044202604806,
57.4525259198522));
#197922=CARTESIAN_POINT('Ctrl Pts',(-5.94297833293132,-3.23624744639666,
57.4613849940281));
#197923=CARTESIAN_POINT('Ctrl Pts',(-5.8525193950385,-3.40236438177365,
57.4702607126221));
#197924=CARTESIAN_POINT('Ctrl Pts',(-5.75517563289851,-3.56453256269319,
57.4791364312161));
#197925=CARTESIAN_POINT('Ctrl Pts',(-5.65131887296307,-3.72221493147446,
57.4880121498101));
#197926=CARTESIAN_POINT('Ctrl Pts',(-5.54716573518003,-3.88034728118229,
57.4969131971971));
#197927=CARTESIAN_POINT('Ctrl Pts',(-5.43646254941413,-4.03396798383621,
57.5058142445841));
#197928=CARTESIAN_POINT('Ctrl Pts',(-5.31962396419665,-4.18256976983586,
57.514715291971));
#197929=CARTESIAN_POINT('Ctrl Pts',(-5.20262653531977,-4.33137358200209,
57.523628440454));
#197930=CARTESIAN_POINT('Ctrl Pts',(-5.07947721033135,-4.47514464785269,
57.5325415889371));
#197931=CARTESIAN_POINT('Ctrl Pts',(-4.9506291973722,-4.61341083691078,
57.5414547374201));
#197932=CARTESIAN_POINT('Ctrl Pts',(-4.82149510659183,-4.75198401471636,
57.55038767553));
#197933=CARTESIAN_POINT('Ctrl Pts',(-4.68663719769362,-4.88502767839387,
57.5593206136398));
#197934=CARTESIAN_POINT('Ctrl Pts',(-4.54654570739704,-5.01210645642623,
57.5682535517497));
#197935=CARTESIAN_POINT('Ctrl Pts',(-4.41319892105528,-5.1330670274572,
57.5767564136082));
#197936=CARTESIAN_POINT('Ctrl Pts',(-4.27511077058095,-5.24862343007156,
57.5852592754667));
#197937=CARTESIAN_POINT('Ctrl Pts',(-4.13272995211554,-5.35843560592895,
57.5937621373252));
#197938=CARTESIAN_POINT('Ctrl Pts',(-3.99504005740441,-5.46462987489557,
57.6019848611911));
#197939=CARTESIAN_POINT('Ctrl Pts',(-3.85307118423185,-5.56565493352219,
57.6102075850569));
#197940=CARTESIAN_POINT('Ctrl Pts',(-3.70724803457597,-5.66114838262809,
57.6184303089228));
#197941=CARTESIAN_POINT('Ctrl Pts',(-3.56157923378442,-5.75654075515284,
57.626644329314));
#197942=CARTESIAN_POINT('Ctrl Pts',(-3.41206457795247,-5.84641298249386,
57.6348583497052));
#197943=CARTESIAN_POINT('Ctrl Pts',(-3.25916141275307,-5.93044314411844,
57.6430723700964));
#197944=CARTESIAN_POINT('Ctrl Pts',(-3.10638939174153,-6.01440123354434,
57.6512793453684));
#197945=CARTESIAN_POINT('Ctrl Pts',(-2.95023496211614,-6.09252706471693,
57.6594863206403));
#197946=CARTESIAN_POINT('Ctrl Pts',(-2.79118406851032,-6.16454219676483,
57.6676932959123));
#197947=CARTESIAN_POINT('Ctrl Pts',(-2.63223766816786,-6.23651001630799,
57.6758948793652));
#197948=CARTESIAN_POINT('Ctrl Pts',(-2.47039891984656,-6.30237498590982,
57.6840964628182));
#197949=CARTESIAN_POINT('Ctrl Pts',(-2.30617804569328,-6.36190473219792,
57.6922980462711));
#197950=CARTESIAN_POINT('Ctrl Pts',(-2.14203210663384,-6.4214073146608,
57.7004958872862));
#197951=CARTESIAN_POINT('Ctrl Pts',(-1.97550654382605,-6.47458031100016,
57.7086937283012));
#197952=CARTESIAN_POINT('Ctrl Pts',(-1.8071313011859,-6.52123956470502,
57.7168915693163));
#197953=CARTESIAN_POINT('Ctrl Pts',(-1.63877091713554,-6.56789470087634,
57.7250886868974));
#197954=CARTESIAN_POINT('Ctrl Pts',(-1.46856152152535,-6.60803713537928,
57.7332858044786));
#197955=CARTESIAN_POINT('Ctrl Pts',(-1.2970483094915,-6.64153255528009,
57.7414829220597));
#197956=CARTESIAN_POINT('Ctrl Pts',(-1.12553700573313,-6.67502760250705,
57.7496799484388));
#197957=CARTESIAN_POINT('Ctrl Pts',(-0.95272226641788,-6.70187571260162,
57.7578769748179));
#197958=CARTESIAN_POINT('Ctrl Pts',(-0.779159453741085,-6.72199371806058,
57.766074001197));
#197959=CARTESIAN_POINT('Ctrl Pts',(-0.60556701315866,-6.74211515774809,
57.7742724268432));
#197960=CARTESIAN_POINT('Ctrl Pts',(-0.431226601256352,-6.75550416261753,
57.7824708524893));
#197961=CARTESIAN_POINT('Ctrl Pts',(-0.256698728759893,-6.76212945473932,
57.7906692781354));
#197962=CARTESIAN_POINT('Ctrl Pts',(-0.0821093288132859,-6.76875708251859,
57.7988705940261));
#197963=CARTESIAN_POINT('Ctrl Pts',(0.0926673050172221,-6.76861623408654,
57.8070719099167));
#197964=CARTESIAN_POINT('Ctrl Pts',(0.267070581042112,-6.76172776032442,
57.8152732258074));
#197965=CARTESIAN_POINT('Ctrl Pts',(0.441672473204208,-6.75483144174377,
57.823483881624));
#197966=CARTESIAN_POINT('Ctrl Pts',(0.61589979917764,-6.74117215991515,
57.8316945374406));
#197967=CARTESIAN_POINT('Ctrl Pts',(0.789195946652915,-6.72082277387126,
57.8399051932572));
#197968=CARTESIAN_POINT('Ctrl Pts',(0.962594213349496,-6.70046139642718,
57.8481206874143));
#197969=CARTESIAN_POINT('Ctrl Pts',(1.13505985384755,-6.67340211189372,
57.8563361815715));
#197970=CARTESIAN_POINT('Ctrl Pts',(1.30604648660982,-6.63976893986637,
57.8645516757286));
#197971=CARTESIAN_POINT('Ctrl Pts',(1.47729840827921,-6.60608358535372,
57.8727799163761));
#197972=CARTESIAN_POINT('Ctrl Pts',(1.64706638757443,-6.56580404349757,
57.8810081570236));
#197973=CARTESIAN_POINT('Ctrl Pts',(1.81481794482534,-6.51910460317519,
57.8892363976711));
#197974=CARTESIAN_POINT('Ctrl Pts',(1.96727732865149,-6.47666226753757,
57.8967145547723));
#197975=CARTESIAN_POINT('Ctrl Pts',(2.11807119090478,-6.42891784237976,
57.9041927118735));
#197976=CARTESIAN_POINT('Ctrl Pts',(2.26681504283588,-6.37603627354589,
57.9116708689747));
#197977=CARTESIAN_POINT('Ctrl Pts',(2.42731717189511,-6.31897438980659,
57.9197401781972));
#197978=CARTESIAN_POINT('Ctrl Pts',(2.58595747511384,-6.25574346628744,
57.9278094874198));
#197979=CARTESIAN_POINT('Ctrl Pts',(2.74221409488188,-6.18648129859221,
57.9358787966423));
#197980=CARTESIAN_POINT('Ctrl Pts',(2.89827582017616,-6.11730551964482,
57.9439380412431));
#197981=CARTESIAN_POINT('Ctrl Pts',(3.05195944088801,-6.04211361378504,
57.9519972858438));
#197982=CARTESIAN_POINT('Ctrl Pts',(3.2027575147074,-5.96109329754075,57.9600565304446));
#197983=CARTESIAN_POINT('Ctrl Pts',(3.35340059473218,-5.88015625587642,
57.9681074915649));
#197984=CARTESIAN_POINT('Ctrl Pts',(3.50116370400768,-5.79340290029704,
57.9761584526852));
#197985=CARTESIAN_POINT('Ctrl Pts',(3.64555877954429,-5.70106921418146,
57.9842094138054));
#197986=CARTESIAN_POINT('Ctrl Pts',(3.78983708226455,-5.60881019864956,
57.9922538640845));
#197987=CARTESIAN_POINT('Ctrl Pts',(3.93075245962766,-5.51098003460954,
58.0002983143636));
#197988=CARTESIAN_POINT('Ctrl Pts',(4.06784099874613,-5.40786081634135,
58.0083427646427));
#197989=CARTESIAN_POINT('Ctrl Pts',(4.20484868127066,-5.30480241912218,
58.016382470201));
#197990=CARTESIAN_POINT('Ctrl Pts',(4.33803372136174,-5.19646140151004,
58.0244221757592));
#197991=CARTESIAN_POINT('Ctrl Pts',(4.46696088237514,-5.08316333352868,
58.0324618813175));
#197992=CARTESIAN_POINT('Ctrl Pts',(4.59867086723058,-4.96741978732257,
58.0406751196219));
#197993=CARTESIAN_POINT('Ctrl Pts',(4.72593673940524,-4.84650298249286,
58.0488883579264));
#197994=CARTESIAN_POINT('Ctrl Pts',(4.84832948585928,-4.72080397777195,
58.0571015962308));
#197995=CARTESIAN_POINT('Ctrl Pts',(4.96809770076211,-4.59780040242414,
58.065138713779));
#197996=CARTESIAN_POINT('Ctrl Pts',(5.08319940323806,-4.47021792965405,
58.0731758313272));
#197997=CARTESIAN_POINT('Ctrl Pts',(5.19326970059408,-4.33846042011351,
58.0812129488753));
#197998=CARTESIAN_POINT('Ctrl Pts',(5.30335164268751,-4.20668897146643,
58.0892509166994));
#197999=CARTESIAN_POINT('Ctrl Pts',(5.40840088015366,-4.07074189324922,
58.0972888845236));
#198000=CARTESIAN_POINT('Ctrl Pts',(5.50809291020161,-3.93105602765806,
58.1053268523476));
#198001=CARTESIAN_POINT('Ctrl Pts',(5.60781523969898,-3.7913277072707,58.1133672631554));
#198002=CARTESIAN_POINT('Ctrl Pts',(5.70217690391183,-3.64785864159494,
58.1214076739631));
#198003=CARTESIAN_POINT('Ctrl Pts',(5.79089690691449,-3.50111439594426,
58.1294480847709));
#198004=CARTESIAN_POINT('Ctrl Pts',(5.88297002564342,-3.34882404545615,
58.1377923777587));
#198005=CARTESIAN_POINT('Ctrl Pts',(5.96896647493851,-3.19300649258926,
58.1461366707464));
#198006=CARTESIAN_POINT('Ctrl Pts',(6.04862517023485,-3.03420871892517,
58.1544809637342));
#198007=CARTESIAN_POINT('Ctrl Pts',(6.12551841233805,-2.88092381248301,
58.1625355739498));
#198008=CARTESIAN_POINT('Ctrl Pts',(6.19650648129406,-2.72486250410686,
58.1705901841653));
#198009=CARTESIAN_POINT('Ctrl Pts',(6.26140442885749,-2.56653532574244,
58.1786447943808));
#198010=CARTESIAN_POINT('Ctrl Pts',(6.32635150508414,-2.40808829146705,
58.1867055020501));
#198011=CARTESIAN_POINT('Ctrl Pts',(6.3851991527014,-2.24737232020921,58.1947662097193));
#198012=CARTESIAN_POINT('Ctrl Pts',(6.43781262294535,-2.08491190025995,
58.2028269173886));
#198013=CARTESIAN_POINT('Ctrl Pts',(6.49050027502996,-1.92222242085252,
58.2108989901727));
#198014=CARTESIAN_POINT('Ctrl Pts',(6.53693611201876,-1.75778394157787,
58.2189710629568));
#198015=CARTESIAN_POINT('Ctrl Pts',(6.5770365347422,-1.59213046596888,58.2270431357409));
#198016=CARTESIAN_POINT('Ctrl Pts',(6.581236749349,-1.57477952299459,58.2278886240354));
#198017=CARTESIAN_POINT('Ctrl Pts',(6.58536750530445,-1.55741525391307,
58.2287341123298));
#198018=CARTESIAN_POINT('Ctrl Pts',(6.5894287395351,-1.54003827439088,58.2295796006243));
#198019=CARTESIAN_POINT('Ctrl Pts',(6.62945525259258,-1.36877509225432,
58.237912522671));
#198020=CARTESIAN_POINT('Ctrl Pts',(6.66285212335729,-1.19573053691983,
58.2462454447177));
#198021=CARTESIAN_POINT('Ctrl Pts',(6.68946360899263,-1.02145270275391,
58.2545783667644));
#198022=CARTESIAN_POINT('Ctrl Pts',(6.71604364630531,-0.847380822725198,
58.262901441318));
#198023=CARTESIAN_POINT('Ctrl Pts',(6.73585422025224,-0.672078908217391,
58.2712245158716));
#198024=CARTESIAN_POINT('Ctrl Pts',(6.74878996331768,-0.496107882443526,
58.2795475904253));
#198025=CARTESIAN_POINT('Ctrl Pts',(6.76171279390168,-0.320312511256482,
58.2878623568712));
#198026=CARTESIAN_POINT('Ctrl Pts',(6.76777444049541,-0.143849704344839,
58.2961771233172));
#198027=CARTESIAN_POINT('Ctrl Pts',(6.76692093589621,0.0327115779142395,
58.3044918897632));
#198028=CARTESIAN_POINT('Ctrl Pts',(6.76606812670532,0.209129003673223,
58.3127998816027));
#198029=CARTESIAN_POINT('Ctrl Pts',(6.75831139469508,0.385644398463105,
58.3211078734423));
#198030=CARTESIAN_POINT('Ctrl Pts',(6.74364873418873,0.561685632604875,
58.3294158652818));
#198031=CARTESIAN_POINT('Ctrl Pts',(6.72899533219164,0.737615708243444,
58.3377186111689));
#198032=CARTESIAN_POINT('Ctrl Pts',(6.70744472073708,0.913071874136868,
58.346021357056));
#198033=CARTESIAN_POINT('Ctrl Pts',(6.6790469481925,1.08748373037968,58.3543241029432));
#198034=CARTESIAN_POINT('Ctrl Pts',(6.65066078091265,1.26182431005451,58.3626234557626));
#198035=CARTESIAN_POINT('Ctrl Pts',(6.61543308402124,1.43512108759843,58.370922808582));
#198036=CARTESIAN_POINT('Ctrl Pts',(6.57346559623067,1.60681021131051,58.3792221614015));
#198037=CARTESIAN_POINT('Ctrl Pts',(6.53150703422064,1.77846281962653,58.3875197490878));
#198038=CARTESIAN_POINT('Ctrl Pts',(6.48281161960978,1.94850811753511,58.3958173367742));
#198039=CARTESIAN_POINT('Ctrl Pts',(6.42753195926004,2.11639361005716,58.4041149244605));
#198040=CARTESIAN_POINT('Ctrl Pts',(6.37225486985472,2.2842712945669,58.412412126243));
#198041=CARTESIAN_POINT('Ctrl Pts',(6.3103942538806,2.44998904347843,58.4207093280254));
#198042=CARTESIAN_POINT('Ctrl Pts',(6.2421522933486,2.61301047580045,58.4290065298079));
#198043=CARTESIAN_POINT('Ctrl Pts',(6.17390216699228,2.77605141524631,58.4373047244324));
#198044=CARTESIAN_POINT('Ctrl Pts',(6.09926930941793,2.93639507453469,58.445602919057));
#198045=CARTESIAN_POINT('Ctrl Pts',(6.01850372995083,3.09352579633143,58.4539011136815));
#198046=CARTESIAN_POINT('Ctrl Pts',(5.93768134711018,3.25076702999653,58.4622051445231));
#198047=CARTESIAN_POINT('Ctrl Pts',(5.85071778296393,3.4047905010508,58.4705091753646));
#198048=CARTESIAN_POINT('Ctrl Pts',(5.75790906763323,3.55510508548862,58.4788132062062));
#198049=CARTESIAN_POINT('Ctrl Pts',(5.66506660449923,3.70547432844651,58.4871202566219));
#198050=CARTESIAN_POINT('Ctrl Pts',(5.56637494291118,3.8521317046498,58.4954273070377));
#198051=CARTESIAN_POINT('Ctrl Pts',(5.46217312977042,3.99461558856594,58.5037343574534));
#198052=CARTESIAN_POINT('Ctrl Pts',(5.35785990730502,4.13725181180134,58.5120502895081));
#198053=CARTESIAN_POINT('Ctrl Pts',(5.24802497389089,4.27570535068261,58.5203662215627));
#198054=CARTESIAN_POINT('Ctrl Pts',(5.13304799000972,4.40954729334625,58.5286821536173));
#198055=CARTESIAN_POINT('Ctrl Pts',(5.04637589737093,4.51044019261978,58.5349508798361));
#198056=CARTESIAN_POINT('Ctrl Pts',(4.95678269050299,4.60871324893425,58.541219606055));
#198057=CARTESIAN_POINT('Ctrl Pts',(4.86444455754876,4.70419686519753,58.5474883322738));
#198058=CARTESIAN_POINT('Ctrl Pts',(4.73683470814911,4.83615372312458,58.5561516134461));
#198059=CARTESIAN_POINT('Ctrl Pts',(4.60374100709286,4.96302963095883,58.5648148946185));
#198060=CARTESIAN_POINT('Ctrl Pts',(4.46559664161901,5.08436187090977,58.5734781757908));
#198061=CARTESIAN_POINT('Ctrl Pts',(4.3309786271445,5.20259691566106,58.581920313161));
#198062=CARTESIAN_POINT('Ctrl Pts',(4.19156490220754,5.31556759914414,58.5903624505313));
#198063=CARTESIAN_POINT('Ctrl Pts',(4.04779465364802,5.42288183919754,58.5988045879015));
#198064=CARTESIAN_POINT('Ctrl Pts',(3.89837526115711,5.53441276242443,58.6075784409749));
#198065=CARTESIAN_POINT('Ctrl Pts',(3.74425028870485,5.63983344997825,58.6163522940483));
#198066=CARTESIAN_POINT('Ctrl Pts',(3.58595203971155,5.73874872850246,58.6251261471217));
#198067=CARTESIAN_POINT('Ctrl Pts',(3.42765379071826,5.83766400702666,58.6339000001951));
#198068=CARTESIAN_POINT('Ctrl Pts',(3.26518258774288,5.93007363277307,58.6426738532685));
#198069=CARTESIAN_POINT('Ctrl Pts',(3.0991061983213,6.01563211736942,58.6514477063419));
#198070=CARTESIAN_POINT('Origin',(0.,0.,4.30282021618968));
#198071=CARTESIAN_POINT('',(3.09910619832126,6.01563211736944,61.0457854935189));
#198072=CARTESIAN_POINT('',(3.09910619832132,6.01563211736941,60.6513956954041));
#198073=CARTESIAN_POINT('',(3.09910619832133,6.0156321173694,4.30282021618968));
#198074=CARTESIAN_POINT('',(-6.76699745956572,-0.00415705027770917,59.69717978381));
#198075=CARTESIAN_POINT('Ctrl Pts',(-6.76699494557931,-0.00827082245302645,
59.69717978381));
#198076=CARTESIAN_POINT('Ctrl Pts',(-6.76674793991816,-0.210365120819723,
59.7066512595226));
#198077=CARTESIAN_POINT('Ctrl Pts',(-6.75744417315915,-0.412020284934577,
59.7161227352352));
#198078=CARTESIAN_POINT('Ctrl Pts',(-6.73922359742326,-0.612498411372184,
59.7255942109478));
#198079=CARTESIAN_POINT('Ctrl Pts',(-6.72088520849356,-0.814272817834613,
59.7351269286771));
#198080=CARTESIAN_POINT('Ctrl Pts',(-6.69351444453166,-1.01485482244309,
59.7446596464064));
#198081=CARTESIAN_POINT('Ctrl Pts',(-6.65730215415095,-1.21351432967937,
59.7541923641357));
#198082=CARTESIAN_POINT('Ctrl Pts',(-6.62079334179662,-1.41380054730992,
59.7638031399013));
#198083=CARTESIAN_POINT('Ctrl Pts',(-6.57529770100836,-1.61213256130308,
59.7734139156668));
#198084=CARTESIAN_POINT('Ctrl Pts',(-6.52105806976313,-1.80778611864821,
59.7830246914324));
#198085=CARTESIAN_POINT('Ctrl Pts',(-6.49956088822673,-1.88533089437641,
59.7868337990276));
#198086=CARTESIAN_POINT('Ctrl Pts',(-6.47669068445561,-1.96245519968619,
59.7906429066228));
#198087=CARTESIAN_POINT('Ctrl Pts',(-6.45246456311846,-2.03911501924253,
59.794452014218));
#198088=CARTESIAN_POINT('Ctrl Pts',(-6.3994667478689,-2.20681842076402,
59.8027849362647));
#198089=CARTESIAN_POINT('Ctrl Pts',(-6.33985870359495,-2.37266971007358,
59.8111178583114));
#198090=CARTESIAN_POINT('Ctrl Pts',(-6.27378626625729,-2.53611807401024,
59.8194507803581));
#198091=CARTESIAN_POINT('Ctrl Pts',(-6.20779191051785,-2.69937328161732,
59.8277738549118));
#198092=CARTESIAN_POINT('Ctrl Pts',(-6.13534850917667,-2.8602309008722,
59.8360969294654));
#198093=CARTESIAN_POINT('Ctrl Pts',(-6.05665176517554,-3.01815479977354,
59.844420004019));
#198094=CARTESIAN_POINT('Ctrl Pts',(-5.97803357640252,-3.17592105876156,
59.852734770465));
#198095=CARTESIAN_POINT('Ctrl Pts',(-5.89317463545723,-3.33075912231229,
59.8610495369109));
#198096=CARTESIAN_POINT('Ctrl Pts',(-5.80231894786804,-3.48215218323547,
59.8693643033569));
#198097=CARTESIAN_POINT('Ctrl Pts',(-5.7115372865945,-3.63342189392255,
59.8776722951964));
#198098=CARTESIAN_POINT('Ctrl Pts',(-5.61476879262656,-3.7812518978611,
59.885980287036));
#198099=CARTESIAN_POINT('Ctrl Pts',(-5.5123037719867,-3.92514918510637,
59.8942882788755));
#198100=CARTESIAN_POINT('Ctrl Pts',(-5.40990345129323,-4.06895561064379,
59.9025910247626));
#198101=CARTESIAN_POINT('Ctrl Pts',(-5.30181397354251,-4.2088339856821,
59.9108937706497));
#198102=CARTESIAN_POINT('Ctrl Pts',(-5.18836952418654,-4.34431935756251,
59.9191965165367));
#198103=CARTESIAN_POINT('Ctrl Pts',(-5.07497143596165,-4.47974936088924,
59.9274958693562));
#198104=CARTESIAN_POINT('Ctrl Pts',(-4.95622295970471,-4.61078967194648,
59.9357952221756));
#198105=CARTESIAN_POINT('Ctrl Pts',(-4.83249938808486,-4.73700735318824,
59.944094574995));
#198106=CARTESIAN_POINT('Ctrl Pts',(-4.70880213039263,-4.86319819004711,
59.9523921626814));
#198107=CARTESIAN_POINT('Ctrl Pts',(-4.58013212874796,-4.98456819219664,
59.9606897503678));
#198108=CARTESIAN_POINT('Ctrl Pts',(-4.44690262161451,-5.10072015247631,
59.9689873380541));
#198109=CARTESIAN_POINT('Ctrl Pts',(-4.31367931071456,-5.21686671076447,
59.9772845398365));
#198110=CARTESIAN_POINT('Ctrl Pts',(-4.17589717921879,-5.32779548229528,
59.985581741619));
#198111=CARTESIAN_POINT('Ctrl Pts',(-4.0340038712678,-5.43314842118237,
59.9938789434014));
#198112=CARTESIAN_POINT('Ctrl Pts',(-3.89209358438091,-5.53851396658925,
60.0021771380259));
#198113=CARTESIAN_POINT('Ctrl Pts',(-3.7460714204525,-5.63830214297072,
60.0104753326505));
#198114=CARTESIAN_POINT('Ctrl Pts',(-3.59641557339867,-5.73219713752201,
60.0187735272751));
#198115=CARTESIAN_POINT('Ctrl Pts',(-3.44665447164329,-5.82615816951737,
60.0270775581167));
#198116=CARTESIAN_POINT('Ctrl Pts',(-3.29325487521143,-5.91421755254508,
60.0353815889583));
#198117=CARTESIAN_POINT('Ctrl Pts',(-3.13672202977063,-5.99610406080078,
60.0436856197998));
#198118=CARTESIAN_POINT('Ctrl Pts',(-2.98013226467893,-6.07802034524468,
60.0519926702156));
#198119=CARTESIAN_POINT('Ctrl Pts',(-2.8204072913917,-6.15375912639602,
60.0602997206313));
#198120=CARTESIAN_POINT('Ctrl Pts',(-2.65807428976598,-6.22309650174936,
60.0686067710471));
#198121=CARTESIAN_POINT('Ctrl Pts',(-2.49556772676425,-6.29250801045916,
60.0769227031017));
#198122=CARTESIAN_POINT('Ctrl Pts',(-2.3304478871435,-6.35550430868761,
60.0852386351563));
#198123=CARTESIAN_POINT('Ctrl Pts',(-2.16326017726427,-6.4119103553826,
60.093554567211));
#198124=CARTESIAN_POINT('Ctrl Pts',(-2.03723053037763,-6.45443043148374,
60.0998232934297));
#198125=CARTESIAN_POINT('Ctrl Pts',(-1.9100261967052,-6.49320663306443,
60.1060920196485));
#198126=CARTESIAN_POINT('Ctrl Pts',(-1.78188525111659,-6.52818305134385,
60.1123607458673));
#198127=CARTESIAN_POINT('Ctrl Pts',(-1.60915072947773,-6.57533140702662,
60.1208110145907));
#198128=CARTESIAN_POINT('Ctrl Pts',(-1.43439713546218,-6.61565982502612,
60.129261283314));
#198129=CARTESIAN_POINT('Ctrl Pts',(-1.25818914927755,-6.64900361442526,
60.1377115520374));
#198130=CARTESIAN_POINT('Ctrl Pts',(-1.08213667261888,-6.68231797679902,
60.1461543631119));
#198131=CARTESIAN_POINT('Ctrl Pts',(-0.904632686421212,-6.70865993551441,
60.1545971741864));
#198132=CARTESIAN_POINT('Ctrl Pts',(-0.726254821983576,-6.7279151996399,
60.1630399852609));
#198133=CARTESIAN_POINT('Ctrl Pts',(-0.548010095458443,-6.74715609199523,
60.1714764947786));
#198134=CARTESIAN_POINT('Ctrl Pts',(-0.368893119497846,-6.75932079836543,
60.1799130042963));
#198135=CARTESIAN_POINT('Ctrl Pts',(-0.1894898534267,-6.76434642781166,
60.188349513814));
#198136=CARTESIAN_POINT('Ctrl Pts',(-0.0102149600456931,-6.7693684611496,
60.1967799865552));
#198137=CARTESIAN_POINT('Ctrl Pts',(0.169345484178861,-6.76726159781441,
60.2052104592965));
#198138=CARTESIAN_POINT('Ctrl Pts',(0.348602074366175,-6.75801491517647,
60.2136409320377));
#198139=CARTESIAN_POINT('Ctrl Pts',(0.527781602631672,-6.74877220766231,
60.2220677805415));
#198140=CARTESIAN_POINT('Ctrl Pts',(0.706657206732951,-6.73239581682857,
60.2304946290454));
#198141=CARTESIAN_POINT('Ctrl Pts',(0.884640499077104,-6.70892690282079,
60.2389214775492));
#198142=CARTESIAN_POINT('Ctrl Pts',(1.06256885433471,-6.6854652328287,60.2473457249859));
#198143=CARTESIAN_POINT('Ctrl Pts',(1.23960511874426,-6.65491544875998,
60.2557699724225));
#198144=CARTESIAN_POINT('Ctrl Pts',(1.41516666697177,-6.61737049776511,
60.2641942198592));
#198145=CARTESIAN_POINT('Ctrl Pts',(1.4646331941756,-6.60679176706636,60.2665678504702));
#198146=CARTESIAN_POINT('Ctrl Pts',(1.51398269264356,-6.59565800615915,
60.2689414810813));
#198147=CARTESIAN_POINT('Ctrl Pts',(1.5632022599082,-6.5839720302123,60.2713151116923));
#198148=CARTESIAN_POINT('Ctrl Pts',(1.74192116676137,-6.54153962044519,
60.2799338926296));
#198149=CARTESIAN_POINT('Ctrl Pts',(1.91884610224507,-6.4918416236436,60.2885526735668));
#198150=CARTESIAN_POINT('Ctrl Pts',(2.09338843199052,-6.43506129518657,
60.2971714545041));
#198151=CARTESIAN_POINT('Ctrl Pts',(2.26803560825225,-6.37824685913146,
60.3057954126907));
#198152=CARTESIAN_POINT('Ctrl Pts',(2.44029703324883,-6.31434169519958,
60.3144193708772));
#198153=CARTESIAN_POINT('Ctrl Pts',(2.60960195902574,-6.24357802989993,
60.3230433290638));
#198154=CARTESIAN_POINT('Ctrl Pts',(2.78502329410652,-6.17025791481696,
60.3319788414349));
#198155=CARTESIAN_POINT('Ctrl Pts',(2.95727019985895,-6.08957465562102,
60.340914353806));
#198156=CARTESIAN_POINT('Ctrl Pts',(3.12573397915408,-6.00183939234978,
60.3498498661771));
#198157=CARTESIAN_POINT('Ctrl Pts',(3.28862792288728,-5.9170048771886,60.3584899480718));
#198158=CARTESIAN_POINT('Ctrl Pts',(3.44798465443273,-5.82557740016303,
60.3671300299665));
#198159=CARTESIAN_POINT('Ctrl Pts',(3.60328161292256,-5.72788360723,60.3757701118613));
#198160=CARTESIAN_POINT('Ctrl Pts',(3.76654367897481,-5.62517914585595,
60.3848533394706));
#198161=CARTESIAN_POINT('Ctrl Pts',(3.92531826187956,-5.51554891529997,
60.3939365670799));
#198162=CARTESIAN_POINT('Ctrl Pts',(4.07903519798477,-5.39942227035461,
60.4030197946892));
#198163=CARTESIAN_POINT('Ctrl Pts',(4.23275213408994,-5.28329562540929,
60.4121030222984));
#198164=CARTESIAN_POINT('Ctrl Pts',(4.38141114567018,-5.16067283878569,
60.4211862499077));
#198165=CARTESIAN_POINT('Ctrl Pts',(4.52448428868086,-5.032030496875,60.430269477517));
#198166=CARTESIAN_POINT('Ctrl Pts',(4.66694891353778,-4.90393529608911,
60.4393140723768));
#198167=CARTESIAN_POINT('Ctrl Pts',(4.8040072327267,-4.76975399487583,60.4483586672366));
#198168=CARTESIAN_POINT('Ctrl Pts',(4.93516874599835,-4.62994583645652,
60.4574032620964));
#198169=CARTESIAN_POINT('Ctrl Pts',(5.06620989793573,-4.49026597402946,
60.4664395571167));
#198170=CARTESIAN_POINT('Ctrl Pts',(5.19136488491325,-4.34496973675022,
60.475475852137));
#198171=CARTESIAN_POINT('Ctrl Pts',(5.31018039595455,-4.19455279647545,
60.4845121471573));
#198172=CARTESIAN_POINT('Ctrl Pts',(5.42878565363185,-4.0444020307718,60.493532451745));
#198173=CARTESIAN_POINT('Ctrl Pts',(5.54107368942041,-3.88914884314024,
60.5025527563327));
#198174=CARTESIAN_POINT('Ctrl Pts',(5.64663185528263,-3.72932134454882,
60.5115730609204));
#198175=CARTESIAN_POINT('Ctrl Pts',(5.7520570911402,-3.56969511764452,60.5205820061867));
#198176=CARTESIAN_POINT('Ctrl Pts',(5.85076923947305,-3.4055062735836,60.5295909514529));
#198177=CARTESIAN_POINT('Ctrl Pts',(5.94239780336344,-3.23731329138552,
60.5385998967192));
#198178=CARTESIAN_POINT('Ctrl Pts',(6.03381829818286,-3.06950223984383,
60.547588384578));
#198179=CARTESIAN_POINT('Ctrl Pts',(6.11818720265059,-2.89770540819866,
60.5565768724368));
#198180=CARTESIAN_POINT('Ctrl Pts',(6.19517918465154,-2.72250690909321,
60.5655653602955));
#198181=CARTESIAN_POINT('Ctrl Pts',(6.26272905249322,-2.5687943386013,60.573451521311));
#198182=CARTESIAN_POINT('Ctrl Pts',(6.32460099297568,-2.41246380110435,
60.5813376823264));
#198183=CARTESIAN_POINT('Ctrl Pts',(6.38060368627001,-2.25392670660728,
60.5892238433418));
#198184=CARTESIAN_POINT('Ctrl Pts',(6.43827736355753,-2.09065925127133,
60.597345308198));
#198185=CARTESIAN_POINT('Ctrl Pts',(6.48969896103663,-1.92512413876695,
60.6054667730541));
#198186=CARTESIAN_POINT('Ctrl Pts',(6.53469692774071,-1.75784671191094,
60.6135882379103));
#198187=CARTESIAN_POINT('Ctrl Pts',(6.57969168542751,-1.5905812143974,60.6217091235865));
#198188=CARTESIAN_POINT('Ctrl Pts',(6.6182636296851,-1.42157400364193,60.6298300092627));
#198189=CARTESIAN_POINT('Ctrl Pts',(6.65029144888128,-1.25136431343414,
60.6379508949389));
#198190=CARTESIAN_POINT('Ctrl Pts',(6.68232309631771,-1.08113427830118,
60.6460727512932));
#198191=CARTESIAN_POINT('Ctrl Pts',(6.70780899459909,-0.90970183760193,
60.6541946076474));
#198192=CARTESIAN_POINT('Ctrl Pts',(6.72667919659345,-0.737615066357041,
60.6623164640017));
#198193=CARTESIAN_POINT('Ctrl Pts',(6.74556316605373,-0.565402742732858,
60.6704442459619));
#198194=CARTESIAN_POINT('Ctrl Pts',(6.7578217589761,-0.392535499461082,
60.678572027922));
#198195=CARTESIAN_POINT('Ctrl Pts',(6.76343698538826,-0.219565809456372,
60.6866998098822));
#198196=CARTESIAN_POINT('Ctrl Pts',(6.76905449923494,-0.0465256580289172,
60.6948309027986));
#198197=CARTESIAN_POINT('Ctrl Pts',(6.76802325441362,0.126616657394339,
60.7029619957151));
#198198=CARTESIAN_POINT('Ctrl Pts',(6.76037738222586,0.299310290316055,
60.7110930886316));
#198199=CARTESIAN_POINT('Ctrl Pts',(6.75272316488814,0.472192411120845,
60.7192330562961));
#198200=CARTESIAN_POINT('Ctrl Pts',(6.73843993045061,0.644624506798774,
60.7273730239606));
#198201=CARTESIAN_POINT('Ctrl Pts',(6.71761358568088,0.816061709355177,
60.7355129916252));
#198202=CARTESIAN_POINT('Ctrl Pts',(6.70681214280997,0.90497645506959,60.7397347308056));
#198203=CARTESIAN_POINT('Ctrl Pts',(6.69425150488015,0.993623744972743,
60.7439564699861));
#198204=CARTESIAN_POINT('Ctrl Pts',(6.67994901988375,1.08192887555241,60.7481782091665));
#198205=CARTESIAN_POINT('Ctrl Pts',(6.65135441875996,1.25847511816318,60.7566186268942));
#198206=CARTESIAN_POINT('Ctrl Pts',(6.61573536456724,1.43401789943923,60.7650590446218));
#198207=CARTESIAN_POINT('Ctrl Pts',(6.57318024761848,1.60797712431437,60.7734994623495));
#198208=CARTESIAN_POINT('Ctrl Pts',(6.53065765213538,1.78180340609445,60.7819334297423));
#198209=CARTESIAN_POINT('Ctrl Pts',(6.48120963969021,1.95404822115737,60.7903673971351));
#198210=CARTESIAN_POINT('Ctrl Pts',(6.4249757583338,2.12414112168259,60.7988013645279));
#198211=CARTESIAN_POINT('Ctrl Pts',(6.36877620683777,2.29413018328751,60.8072301831222));
#198212=CARTESIAN_POINT('Ctrl Pts',(6.30579915012798,2.46196963365099,60.8156590017165));
#198213=CARTESIAN_POINT('Ctrl Pts',(6.23623422950004,2.6271032782919,60.8240878203108));
#198214=CARTESIAN_POINT('Ctrl Pts',(6.16670109436923,2.79216147032049,60.8325127876222));
#198215=CARTESIAN_POINT('Ctrl Pts',(6.0905862266872,2.95451601501969,60.8409377549336));
#198216=CARTESIAN_POINT('Ctrl Pts',(6.00812787707466,3.11362945976529,60.849362722245));
#198217=CARTESIAN_POINT('Ctrl Pts',(5.92568748457082,3.27270825407906,60.8577858548356));
#198218=CARTESIAN_POINT('Ctrl Pts',(5.83690651507366,3.42854705848998,60.8662089874261));
#198219=CARTESIAN_POINT('Ctrl Pts',(5.74207001323417,3.58063136375653,60.8746321200167));
#198220=CARTESIAN_POINT('Ctrl Pts',(5.64724439076035,3.73269822235713,60.8830542863302));
#198221=CARTESIAN_POINT('Ctrl Pts',(5.54636479713171,3.88101115746608,60.8914764526436));
#198222=CARTESIAN_POINT('Ctrl Pts',(5.43976076561801,4.0250828330412,60.8998986189571));
#198223=CARTESIAN_POINT('Ctrl Pts',(5.33315408214735,4.16915809264479,60.9083209947863));
#198224=CARTESIAN_POINT('Ctrl Pts',(5.2208228754521,4.3089916144373,60.9167433706155));
#198225=CARTESIAN_POINT('Ctrl Pts',(5.10313850903089,4.44412717613324,60.9251657464447));
#198226=CARTESIAN_POINT('Ctrl Pts',(4.98543478604954,4.57928496473754,60.9335895075745));
#198227=CARTESIAN_POINT('Ctrl Pts',(4.86237636728863,4.7097430015437,60.9420132687043));
#198228=CARTESIAN_POINT('Ctrl Pts',(4.73437343314789,4.83507985409791,60.9504370298341));
#198229=CARTESIAN_POINT('Ctrl Pts',(4.60628018313717,4.96050514139743,60.9588667345723));
#198230=CARTESIAN_POINT('Ctrl Pts',(4.4732356842172,5.08080178964516,60.9672964393106));
#198231=CARTESIAN_POINT('Ctrl Pts',(4.33568613525387,5.1955860821054,60.9757261440488));
#198232=CARTESIAN_POINT('Ctrl Pts',(4.19808791635887,5.31041098933838,60.9841588315169));
#198233=CARTESIAN_POINT('Ctrl Pts',(4.05598172897378,5.41971944265584,60.992591518985));
#198234=CARTESIAN_POINT('Ctrl Pts',(3.90984552507733,5.52316910568858,61.0010242064531));
#198235=CARTESIAN_POINT('Ctrl Pts',(3.76356343867773,5.62672203878986,61.0094653119691));
#198236=CARTESIAN_POINT('Ctrl Pts',(3.61324357220252,5.72440430589957,61.0179064174851));
#198237=CARTESIAN_POINT('Ctrl Pts',(3.45939246949101,5.81591718837441,61.026347523001));
#198238=CARTESIAN_POINT('Ctrl Pts',(3.34129762227779,5.88616172795481,61.032826846507));
#198239=CARTESIAN_POINT('Ctrl Pts',(3.22112276878836,5.95277217140621,61.039306170013));
#198240=CARTESIAN_POINT('Ctrl Pts',(3.09910619832126,6.01563211736944,61.0457854935189));
#198241=CARTESIAN_POINT('Ctrl Pts',(3.09910619832129,6.01563211736943,59.0457552630241));
#198242=CARTESIAN_POINT('Ctrl Pts',(2.93375330764824,6.10081787314654,59.0545047109264));
#198243=CARTESIAN_POINT('Ctrl Pts',(2.76488627843071,6.17918207037038,59.0632541588287));
#198244=CARTESIAN_POINT('Ctrl Pts',(2.59307866646706,6.25045854553995,59.072003606731));
#198245=CARTESIAN_POINT('Ctrl Pts',(2.42127244185373,6.32173444515039,59.0807529839813));
#198246=CARTESIAN_POINT('Ctrl Pts',(2.24652594672453,6.38592262741843,59.0895023612316));
#198247=CARTESIAN_POINT('Ctrl Pts',(2.06943269687101,6.44280508110568,59.0982517384819));
#198248=CARTESIAN_POINT('Ctrl Pts',(1.89234081822054,6.49968709436173,59.1070010479873));
#198249=CARTESIAN_POINT('Ctrl Pts',(1.71290249405563,6.54926340459551,59.1157503574927));
#198250=CARTESIAN_POINT('Ctrl Pts',(1.53172716625031,6.5913656315039,59.124499666998));
#198251=CARTESIAN_POINT('Ctrl Pts',(1.35055318107301,6.63346754640717,59.1332489116653));
#198252=CARTESIAN_POINT('Ctrl Pts',(1.16764249714382,6.66809542395783,59.1419981563325));
#198253=CARTESIAN_POINT('Ctrl Pts',(0.98361634061393,6.69513165624674,59.1507474009997));
#198254=CARTESIAN_POINT('Ctrl Pts',(0.799591486713385,6.72216769715966,
59.1594965837354));
#198255=CARTESIAN_POINT('Ctrl Pts',(0.614451459526225,6.74161215869375,
59.1682457664711));
#198256=CARTESIAN_POINT('Ctrl Pts',(0.428825047909765,6.75339900185715,
59.1769949492068));
#198257=CARTESIAN_POINT('Ctrl Pts',(0.243199888596534,6.76518576550223,
59.1857440729174));
#198258=CARTESIAN_POINT('Ctrl Pts',(0.0570886373914115,6.76931499599835,
59.1944931966279));
#198259=CARTESIAN_POINT('Ctrl Pts',(-0.128876626811648,6.76577266947846,
59.2032423203384));
#198260=CARTESIAN_POINT('Ctrl Pts',(-0.314840698188693,6.76223036567991,
59.21199138793));
#198261=CARTESIAN_POINT('Ctrl Pts',(-0.500658497951821,6.75101660879219,
59.2207404555215));
#198262=CARTESIAN_POINT('Ctrl Pts',(-0.685698951926819,6.73216948296212,
59.2294895231131));
#198263=CARTESIAN_POINT('Ctrl Pts',(-0.870738280460326,6.71332247176287,
59.2382385374916));
#198264=CARTESIAN_POINT('Ctrl Pts',(-1.05499998761285,6.68684221356181,
59.2469875518701));
#198265=CARTESIAN_POINT('Ctrl Pts',(-1.23785829161442,6.65281863948518,
59.2557365662486));
#198266=CARTESIAN_POINT('Ctrl Pts',(-1.43007412917425,6.61705395368857,
59.2649332999478));
#198267=CARTESIAN_POINT('Ctrl Pts',(-1.62073882535812,6.57295372727785,
59.274130033647));
#198268=CARTESIAN_POINT('Ctrl Pts',(-1.80913696091533,6.52068343478274,
59.2833267673462));
#198269=CARTESIAN_POINT('Ctrl Pts',(-1.98838356186122,6.47095219815195,
59.2920767650599));
#198270=CARTESIAN_POINT('Ctrl Pts',(-2.16557827572533,6.4138258685089,59.3008267627735));
#198271=CARTESIAN_POINT('Ctrl Pts',(-2.34011918621691,6.34949849943281,
59.3095767604872));
#198272=CARTESIAN_POINT('Ctrl Pts',(-2.51465655691092,6.28517243495553,
59.3183265807455));
#198273=CARTESIAN_POINT('Ctrl Pts',(-2.68653996295324,6.21364572242376,
59.3270764010038));
#198274=CARTESIAN_POINT('Ctrl Pts',(-2.85518555379986,6.13516132252222,
59.3358262212621));
#198275=CARTESIAN_POINT('Ctrl Pts',(-3.02382794858685,6.05667841000508,
59.3445758756996));
#198276=CARTESIAN_POINT('Ctrl Pts',(-3.18923239109276,5.97123819492084,
59.3533255301371));
#198277=CARTESIAN_POINT('Ctrl Pts',(-3.35083705967692,5.87913088810717,
59.3620751845746));
#198278=CARTESIAN_POINT('Ctrl Pts',(-3.51243888042386,5.78702520443111,
59.3708246848236));
#198279=CARTESIAN_POINT('Ctrl Pts',(-3.67024081223669,5.68825280605797,
59.3795741850725));
#198280=CARTESIAN_POINT('Ctrl Pts',(-3.82370687544374,5.58314917682524,
59.3883236853215));
#198281=CARTESIAN_POINT('Ctrl Pts',(-3.97717043817797,5.47804726008034,
59.3970730430119));
#198282=CARTESIAN_POINT('Ctrl Pts',(-4.12629803722453,5.36661448084242,
59.4058224007024));
#198283=CARTESIAN_POINT('Ctrl Pts',(-4.27058317206909,5.24922931204575,
59.4145717583929));
#198284=CARTESIAN_POINT('Ctrl Pts',(-4.41486614774827,5.13184589986797,
59.423320985153));
#198285=CARTESIAN_POINT('Ctrl Pts',(-4.55430658194398,5.00851045723048,
59.432070211913));
#198286=CARTESIAN_POINT('Ctrl Pts',(-4.68843089001822,4.87964187103142,
59.4408194386731));
#198287=CARTESIAN_POINT('Ctrl Pts',(-4.82255336917814,4.75077504207983,
59.449568546129));
#198288=CARTESIAN_POINT('Ctrl Pts',(-4.95135966065113,4.61637541908117,
59.4583176535849));
#198289=CARTESIAN_POINT('Ctrl Pts',(-5.07441230869223,4.47689945401868,
59.4670667610409));
#198290=CARTESIAN_POINT('Ctrl Pts',(-5.197463442264,4.33742520555536,59.4758157608172));
#198291=CARTESIAN_POINT('Ctrl Pts',(-5.31476088454755,4.19287495491353,
59.4845647605936));
#198292=CARTESIAN_POINT('Ctrl Pts',(-5.42590627628845,4.04373961586718,
59.49331376037));
#198293=CARTESIAN_POINT('Ctrl Pts',(-5.53706380672659,3.89458798906747,
59.5020637156647));
#198294=CARTESIAN_POINT('Ctrl Pts',(-5.64206777071855,3.74085050155298,
59.5108136709594));
#198295=CARTESIAN_POINT('Ctrl Pts',(-5.74056148163998,3.58304938223176,
59.5195636262541));
#198296=CARTESIAN_POINT('Ctrl Pts',(-5.83905138951869,3.42525435593306,
59.5283132436952));
#198297=CARTESIAN_POINT('Ctrl Pts',(-5.93103139557634,3.26339625497216,
59.5370628611363));
#198298=CARTESIAN_POINT('Ctrl Pts',(-6.01618907820825,3.09802485065046,
59.5458124785774));
#198299=CARTESIAN_POINT('Ctrl Pts',(-6.10134392544956,2.93265895249697,
59.5545618046932));
#198300=CARTESIAN_POINT('Ctrl Pts',(-6.179676772618,2.76378023986106,59.5633111308091));
#198301=CARTESIAN_POINT('Ctrl Pts',(-6.25092157009188,2.59196229227202,
59.572060456925));
#198302=CARTESIAN_POINT('Ctrl Pts',(-6.32216437407723,2.42014915229171,
59.5808095382274));
#198303=CARTESIAN_POINT('Ctrl Pts',(-6.38631941548896,2.24539720662924,
59.5895586195299));
#198304=CARTESIAN_POINT('Ctrl Pts',(-6.44316881037516,2.06829994947753,
59.5983077008323));
#198305=CARTESIAN_POINT('Ctrl Pts',(-6.50002334524549,1.89118668024526,
59.6070575731747));
#198306=CARTESIAN_POINT('Ctrl Pts',(-6.54957082411074,1.71172794807788,
59.615807445517));
#198307=CARTESIAN_POINT('Ctrl Pts',(-6.59164294296062,1.53053334250435,
59.6245573178594));
#198308=CARTESIAN_POINT('Ctrl Pts',(-6.6337121408212,1.34935131693673,59.6333065827143));
#198309=CARTESIAN_POINT('Ctrl Pts',(-6.66830695239682,1.16643393829814,
59.6420558475692));
#198310=CARTESIAN_POINT('Ctrl Pts',(-6.69530988153984,0.982402458341267,
59.6508051124241));
#198311=CARTESIAN_POINT('Ctrl Pts',(-6.72231419690479,0.798361530947385,
59.6595548264311));
#198312=CARTESIAN_POINT('Ctrl Pts',(-6.74172580829274,0.613206671362852,
59.6683045404382));
#198313=CARTESIAN_POINT('Ctrl Pts',(-6.75347878028177,0.427566795113822,
59.6770542544452));
#198314=CARTESIAN_POINT('Ctrl Pts',(-6.76248992368215,0.285234494205521,
59.6837627642335));
#198315=CARTESIAN_POINT('Ctrl Pts',(-6.76699999999997,0.142617266092203,
59.6904712740217));
#198316=CARTESIAN_POINT('Ctrl Pts',(-6.767,1.33634611793382E-12,59.69717978381));
#198317=CARTESIAN_POINT('',(-6.767,1.48494633473231E-12,59.3028202161899));
#198318=CARTESIAN_POINT('Ctrl Pts',(3.0991061983213,6.01563211736942,58.6514477063419));
#198319=CARTESIAN_POINT('Ctrl Pts',(2.93960420746614,6.09780363299062,58.6598742324576));
#198320=CARTESIAN_POINT('Ctrl Pts',(2.77677729812525,6.17365583256632,58.6683007585734));
#198321=CARTESIAN_POINT('Ctrl Pts',(2.6111549264028,6.24292871578095,58.6767272846892));
#198322=CARTESIAN_POINT('Ctrl Pts',(2.44558185079483,6.31218098050096,58.6851513027199));
#198323=CARTESIAN_POINT('Ctrl Pts',(2.27721527777857,6.37485770660371,58.6935753207507));
#198324=CARTESIAN_POINT('Ctrl Pts',(2.10660567906555,6.43074657508199,58.7019993387814));
#198325=CARTESIAN_POINT('Ctrl Pts',(2.07660891871999,6.44057301513211,58.7034804585538));
#198326=CARTESIAN_POINT('Ctrl Pts',(2.04654286662022,6.45018974321123,58.7049615783262));
#198327=CARTESIAN_POINT('Ctrl Pts',(2.01641057233741,6.45959576163756,58.7064426980986));
#198328=CARTESIAN_POINT('Ctrl Pts',(1.8410678023596,6.51433030358304,58.7150614790358));
#198329=CARTESIAN_POINT('Ctrl Pts',(1.66355914988804,6.56190132396065,58.7236802599731));
#198330=CARTESIAN_POINT('Ctrl Pts',(1.48448433243295,6.60216595268258,58.7322990409103));
#198331=CARTESIAN_POINT('Ctrl Pts',(1.30530194582427,6.64245476812208,58.7409229990969));
#198332=CARTESIAN_POINT('Ctrl Pts',(1.12455181347335,6.6754283662573,58.7495469572834));
#198333=CARTESIAN_POINT('Ctrl Pts',(0.942843268204863,6.70099511801052,
58.75817091547));
#198334=CARTESIAN_POINT('Ctrl Pts',(0.754570213180525,6.7274855092715,58.7671064278411));
#198335=CARTESIAN_POINT('Ctrl Pts',(0.565268564308852,6.74602386384453,
58.7760419402122));
#198336=CARTESIAN_POINT('Ctrl Pts',(0.375620567336058,6.75656704173015,
58.7849774525833));
#198337=CARTESIAN_POINT('Ctrl Pts',(0.192242809356957,6.76676163568053,
58.7936175344779));
#198338=CARTESIAN_POINT('Ctrl Pts',(0.00854154427682233,6.76948131428951,
58.8022576163726));
#198339=CARTESIAN_POINT('Ctrl Pts',(-0.174867137869492,6.76474023773961,
58.8108976982673));
#198340=CARTESIAN_POINT('Ctrl Pts',(-0.367682764592293,6.75975599361543,
58.8199809258766));
#198341=CARTESIAN_POINT('Ctrl Pts',(-0.560174614704952,6.74652560175623,
58.829064153486));
#198342=CARTESIAN_POINT('Ctrl Pts',(-0.751633238131505,6.72512724603304,
58.8381473810953));
#198343=CARTESIAN_POINT('Ctrl Pts',(-0.943091861558059,6.70372889030986,
58.8472306087046));
#198344=CARTESIAN_POINT('Ctrl Pts',(-1.13351688027741,6.67416266347395,
58.8563138363139));
#198345=CARTESIAN_POINT('Ctrl Pts',(-1.32221104142195,6.63656891487928,
58.8653970639232));
#198346=CARTESIAN_POINT('Ctrl Pts',(-1.51010264927044,6.59913505987465,
58.874441658783));
#198347=CARTESIAN_POINT('Ctrl Pts',(-1.69645177588442,6.5537081134136,58.8834862536429));
#198348=CARTESIAN_POINT('Ctrl Pts',(-1.88060221952506,6.50043262344265,
58.8925308485027));
#198349=CARTESIAN_POINT('Ctrl Pts',(-2.06458367614873,6.4472060221192,58.9015671435232));
#198350=CARTESIAN_POINT('Ctrl Pts',(-2.24637024969716,6.38614532271716,
58.9106034385436));
#198351=CARTESIAN_POINT('Ctrl Pts',(-2.42531912408078,6.31744538135219,
58.919639733564));
#198352=CARTESIAN_POINT('Ctrl Pts',(-2.60395133439687,6.24886700992134,
58.9286600381518));
#198353=CARTESIAN_POINT('Ctrl Pts',(-2.77975565110537,6.17267647587612,
58.9376803427395));
#198354=CARTESIAN_POINT('Ctrl Pts',(-2.95210766720634,6.08911728588156,
58.9467006473272));
#198355=CARTESIAN_POINT('Ctrl Pts',(-3.12424263942437,6.00566332245447,
58.9557095925936));
#198356=CARTESIAN_POINT('Ctrl Pts',(-3.29293377373124,5.91485932502222,
58.96471853786));
#198357=CARTESIAN_POINT('Ctrl Pts',(-3.45757740906046,5.81699642946038,
58.9737274831264));
#198358=CARTESIAN_POINT('Ctrl Pts',(-3.62184717354777,5.71935575981746,
58.9827159709853));
#198359=CARTESIAN_POINT('Ctrl Pts',(-3.7820875809945,5.61468830916453,58.9917044588441));
#198360=CARTESIAN_POINT('Ctrl Pts',(-3.93772072437835,5.50333030962173,
59.0006929467029));
#198361=CARTESIAN_POINT('Ctrl Pts',(-4.07426738798728,5.40562899116779,
59.008579107718));
#198362=CARTESIAN_POINT('Ctrl Pts',(-4.20726776641211,5.30277825801675,
59.0164652687331));
#198363=CARTESIAN_POINT('Ctrl Pts',(-4.33634734476151,5.19503423526542,
59.0243514297482));
#198364=CARTESIAN_POINT('Ctrl Pts',(-4.46927834340681,5.08407539324297,
59.0324728946044));
#198365=CARTESIAN_POINT('Ctrl Pts',(-4.59799052346479,4.96797531200298,
59.0405943594606));
#198366=CARTESIAN_POINT('Ctrl Pts',(-4.72206821525421,4.84709818040505,
59.0487158243168));
#198367=CARTESIAN_POINT('Ctrl Pts',(-4.84613705847835,4.72622966912536,
59.056836709993));
#198368=CARTESIAN_POINT('Ctrl Pts',(-4.9655718094636,4.60058504159022,59.0649575956692));
#198369=CARTESIAN_POINT('Ctrl Pts',(-5.0799929100406,4.47056607533512,59.0730784813454));
#198370=CARTESIAN_POINT('Ctrl Pts',(-5.19442768721103,4.34053156809562,
59.0812003376997));
#198371=CARTESIAN_POINT('Ctrl Pts',(-5.30384737966787,4.20612195669019,
59.089322194054));
#198372=CARTESIAN_POINT('Ctrl Pts',(-5.40791208583435,4.06777283926804,
59.0974440504083));
#198373=CARTESIAN_POINT('Ctrl Pts',(-5.51205271632277,3.92932278404173,
59.1055718323684));
#198374=CARTESIAN_POINT('Ctrl Pts',(-5.61083033696595,3.78692777515107,
59.1136996143286));
#198375=CARTESIAN_POINT('Ctrl Pts',(-5.70394748042142,3.64105371295098,
59.1218273962888));
#198376=CARTESIAN_POINT('Ctrl Pts',(-5.79710255633991,3.49512022708019,
59.1299584892052));
#198377=CARTESIAN_POINT('Ctrl Pts',(-5.88459237392545,3.34570517872564,
59.1380895821217));
#198378=CARTESIAN_POINT('Ctrl Pts',(-5.96616511616956,3.19329967378595,
59.1462206750381));
#198379=CARTESIAN_POINT('Ctrl Pts',(-6.04782689165323,3.04072782460603,
59.1543606427027));
#198380=CARTESIAN_POINT('Ctrl Pts',(-6.12355853245191,2.88515932847609,
59.1625006103673));
#198381=CARTESIAN_POINT('Ctrl Pts',(-6.19315579594797,2.72710657787994,
59.1706405780319));
#198382=CARTESIAN_POINT('Ctrl Pts',(-6.22925194598829,2.64513358766136,
59.1748623172122));
#198383=CARTESIAN_POINT('Ctrl Pts',(-6.26369881085293,2.56249264663979,
59.1790840563926));
#198384=CARTESIAN_POINT('Ctrl Pts',(-6.29647317771066,2.47925684880979,
59.1833057955729));
#198385=CARTESIAN_POINT('Ctrl Pts',(-6.373791420635,2.2828946836898,59.1932653306243));
#198386=CARTESIAN_POINT('Ctrl Pts',(-6.44192552376281,2.08289773371365,
59.2032248656757));
#198387=CARTESIAN_POINT('Ctrl Pts',(-6.5005853984413,1.88007406172517,59.2131844007271));
#198388=CARTESIAN_POINT('Ctrl Pts',(-6.55661410572472,1.68634797195297,
59.2226972044474));
#198389=CARTESIAN_POINT('Ctrl Pts',(-6.60399976692655,1.4900433177012,59.2322100081678));
#198390=CARTESIAN_POINT('Ctrl Pts',(-6.64253932075502,1.29188249164675,
59.2417228118881));
#198391=CARTESIAN_POINT('Ctrl Pts',(-6.68098477670612,1.09420549353679,
59.2512123892202));
#198392=CARTESIAN_POINT('Ctrl Pts',(-6.71062720877404,0.894681494081056,
59.2607019665523));
#198393=CARTESIAN_POINT('Ctrl Pts',(-6.73131431791604,0.694043625011065,
59.2701915438844));
#198394=CARTESIAN_POINT('Ctrl Pts',(-6.7519070606708,0.494320986325281,
59.2796378335284));
#198395=CARTESIAN_POINT('Ctrl Pts',(-6.76362593898087,0.293494741529154,
59.2890841231724));
#198396=CARTESIAN_POINT('Ctrl Pts',(-6.76637046870224,0.0923021141375346,
59.2985304128164));
#198397=CARTESIAN_POINT('Ctrl Pts',(-6.76678592257535,0.0618465298379839,
59.2999603472742));
#198398=CARTESIAN_POINT('Ctrl Pts',(-6.76699582823407,0.0313825743895913,
59.3013902817321));
#198399=CARTESIAN_POINT('Ctrl Pts',(-6.76699993843214,0.000912830451469524,
59.3028202161899));
#198400=CARTESIAN_POINT('Ctrl Pts',(-6.767,1.48494626510862E-12,59.3028202161899));
#198401=CARTESIAN_POINT('Ctrl Pts',(-6.76700000000004,-0.186007249525479,
59.3115697280011));
#198402=CARTESIAN_POINT('Ctrl Pts',(-6.75932637294528,-0.372014355748617,
59.3203192398123));
#198403=CARTESIAN_POINT('Ctrl Pts',(-6.7440051826419,-0.557389537486286,
59.3290687516235));
#198404=CARTESIAN_POINT('Ctrl Pts',(-6.72868405705097,-0.742763936250755,
59.3378182264792));
#198405=CARTESIAN_POINT('Ctrl Pts',(-6.70571545645737,-0.927506130241397,
59.3465677013348));
#198406=CARTESIAN_POINT('Ctrl Pts',(-6.67517739404813,-1.1109886399009,
59.3553171761905));
#198407=CARTESIAN_POINT('Ctrl Pts',(-6.64463945808683,-1.29447038982047,
59.3640666148175));
#198408=CARTESIAN_POINT('Ctrl Pts',(-6.60653217008327,-1.47669218313809,
59.3728160534445));
#198409=CARTESIAN_POINT('Ctrl Pts',(-6.56098496092639,-1.65703510599436,
59.3815654920716));
#198410=CARTESIAN_POINT('Ctrl Pts',(-6.51543793658257,-1.83737729708838,
59.3903148951967));
#198411=CARTESIAN_POINT('Ctrl Pts',(-6.4624511216738,-2.01584035511053,
59.3990642983219));
#198412=CARTESIAN_POINT('Ctrl Pts',(-6.40220448374214,-2.19181813760906,
59.407813701447));
#198413=CARTESIAN_POINT('Ctrl Pts',(-6.34195808526463,-2.36779522067251,
59.4165630697971));
#198414=CARTESIAN_POINT('Ctrl Pts',(-6.27445201433063,-2.54128677684266,
59.4253124381472));
#198415=CARTESIAN_POINT('Ctrl Pts',(-6.19991555071861,-2.71170355384904,
59.4340618064973));
#198416=CARTESIAN_POINT('Ctrl Pts',(-6.12537937716646,-2.88211966767577,
59.4428111407991));
#198417=CARTESIAN_POINT('Ctrl Pts',(-6.04381298052467,-3.04946076371892,
59.4515604751009));
#198418=CARTESIAN_POINT('Ctrl Pts',(-5.95549339335771,-3.21315848374659,
59.4603098094027));
#198419=CARTESIAN_POINT('Ctrl Pts',(-5.86717414255346,-3.37685558033602,
59.4690591103829));
#198420=CARTESIAN_POINT('Ctrl Pts',(-5.77210188876532,-3.53690907646864,
59.4778084113631));
#198421=CARTESIAN_POINT('Ctrl Pts',(-5.67059953346928,-3.69277536969392,
59.4865577123432));
#198422=CARTESIAN_POINT('Ctrl Pts',(-5.56909755631311,-3.84864108225029,
59.4953069807285));
#198423=CARTESIAN_POINT('Ctrl Pts',(-5.46116568196773,-4.00031938297623,
59.5040562491138));
#198424=CARTESIAN_POINT('Ctrl Pts',(-5.34717048533521,-4.1472951185996,
59.5128055174991));
#198425=CARTESIAN_POINT('Ctrl Pts',(-5.23317570391758,-4.29427031888012,
59.5215547540161));
#198426=CARTESIAN_POINT('Ctrl Pts',(-5.11311782003439,-4.43654276189633,
59.5303039905332));
#198427=CARTESIAN_POINT('Ctrl Pts',(-4.98740458984683,-4.57362924351928,
59.5390532270502));
#198428=CARTESIAN_POINT('Ctrl Pts',(-4.86169180711664,-4.71071523720349,
59.5478024324257));
#198429=CARTESIAN_POINT('Ctrl Pts',(-4.73032391204083,-4.84261509523324,
59.5565516378011));
#198430=CARTESIAN_POINT('Ctrl Pts',(-4.59374707013501,-4.9688808453842,
59.5653008431765));
#198431=CARTESIAN_POINT('Ctrl Pts',(-4.45717070301346,-5.09514615659551,
59.574050018137));
#198432=CARTESIAN_POINT('Ctrl Pts',(-4.31538563570941,-5.2157772045961,
59.5827991930974));
#198433=CARTESIAN_POINT('Ctrl Pts',(-4.16887341029408,-5.33036429232966,
59.5915483680579));
#198434=CARTESIAN_POINT('Ctrl Pts',(-4.02236168203597,-5.44495099123697,
59.6002975133299));
#198435=CARTESIAN_POINT('Ctrl Pts',(-3.87112305348047,-5.55349359438684,
59.6090466586019));
#198436=CARTESIAN_POINT('Ctrl Pts',(-3.71567117017634,-5.65562346298977,
59.617795803874));
#198437=CARTESIAN_POINT('Ctrl Pts',(-3.56021980145696,-5.7577529935172,
59.6265449201841));
#198438=CARTESIAN_POINT('Ctrl Pts',(-3.40055544538231,-5.85346967463941,
59.6352940364943));
#198439=CARTESIAN_POINT('Ctrl Pts',(-3.23722035986741,-5.94244842986962,
59.6440431528044));
#198440=CARTESIAN_POINT('Ctrl Pts',(-3.07388580147068,-6.03142689794586,
59.6527922408793));
#198441=CARTESIAN_POINT('Ctrl Pts',(-2.90688078896467,-6.11366734656834,
59.6615413289541));
#198442=CARTESIAN_POINT('Ctrl Pts',(-2.7367725072126,-6.18889046952402,
59.670290417029));
#198443=CARTESIAN_POINT('Ctrl Pts',(-2.56666476031357,-6.26411335596379,
59.679039477595));
#198444=CARTESIAN_POINT('Ctrl Pts',(-2.39345402575025,-6.33231884500609,
59.687788538161));
#198445=CARTESIAN_POINT('Ctrl Pts',(-2.21772856065436,-6.39327529762781,
59.6965375987271));
#198446=CARTESIAN_POINT('Ctrl Pts',(-2.04200363348324,-6.45423156365172,
59.7052866325108));
#198447=CARTESIAN_POINT('Ctrl Pts',(-1.86376426189055,-6.50793874375723,
59.7140356662945));
#198448=CARTESIAN_POINT('Ctrl Pts',(-1.68361577752896,-6.55421443909608,
59.7227847000782));
#198449=CARTESIAN_POINT('Ctrl Pts',(-1.50346782967561,-6.60048999661922,
59.731533707806));
#198450=CARTESIAN_POINT('Ctrl Pts',(-1.32141105794769,-6.63933404237755,
59.7402827155338));
#198451=CARTESIAN_POINT('Ctrl Pts',(-1.13806375486826,-6.67061465607594,
59.7490317232617));
#198452=CARTESIAN_POINT('Ctrl Pts',(-0.954716982601011,-6.70189517921325,
59.7577807056601));
#198453=CARTESIAN_POINT('Ctrl Pts',(-0.770079968900096,-6.72561226592252,
59.7665296880585));
#198454=CARTESIAN_POINT('Ctrl Pts',(-0.584779765556168,-6.7416853698312,
59.7752786704569));
#198455=CARTESIAN_POINT('Ctrl Pts',(-0.391489830649242,-6.75845151013865,
59.7844048894667));
#198456=CARTESIAN_POINT('Ctrl Pts',(-0.197478578236303,-6.76689983031631,
59.7935311084766));
#198457=CARTESIAN_POINT('Ctrl Pts',(-0.00346287644933841,-6.76699911397118,
59.8026573274865));
#198458=CARTESIAN_POINT('Ctrl Pts',(0.184489834656752,-6.76709529501183,
59.8114983521523));
#198459=CARTESIAN_POINT('Ctrl Pts',(0.372446404252195,-6.75935639738152,
59.8203393768181));
#198460=CARTESIAN_POINT('Ctrl Pts',(0.559755019491118,-6.74380925873163,
59.8291804014839));
#198461=CARTESIAN_POINT('Ctrl Pts',(0.74513470552457,-6.72842222659775,
59.8379303800937));
#198462=CARTESIAN_POINT('Ctrl Pts',(0.929879431231373,-6.70538706057485,
59.8466803587034));
#198463=CARTESIAN_POINT('Ctrl Pts',(1.11336163627107,-6.6747820089408,59.8554303373131));
#198464=CARTESIAN_POINT('Ctrl Pts',(1.29684196301015,-6.64417727060955,
59.8641802263497));
#198465=CARTESIAN_POINT('Ctrl Pts',(1.47905951217821,-6.60600284890521,
59.8729301153862));
#198466=CARTESIAN_POINT('Ctrl Pts',(1.65939532067409,-6.56038841607149,
59.8816800044227));
#198467=CARTESIAN_POINT('Ctrl Pts',(1.8397293430113,-6.51477443503164,59.8904298067949));
#198468=CARTESIAN_POINT('Ctrl Pts',(2.01818138406596,-6.46172066062038,
59.899179609167));
#198469=CARTESIAN_POINT('Ctrl Pts',(2.19414528354533,-6.40140730423364,
59.9079294115392));
#198470=CARTESIAN_POINT('Ctrl Pts',(2.37010749864323,-6.34109452518521,
59.9166791301555));
#198471=CARTESIAN_POINT('Ctrl Pts',(2.54358134866773,-6.27352239616377,
59.9254288487718));
#198472=CARTESIAN_POINT('Ctrl Pts',(2.71397759435858,-6.19892043966686,
59.9341785673882));
#198473=CARTESIAN_POINT('Ctrl Pts',(2.88437226558423,-6.12431917249374,
59.9429282051569));
#198474=CARTESIAN_POINT('Ctrl Pts',(3.0516891268125,-6.0426883227865,59.9516778429256));
#198475=CARTESIAN_POINT('Ctrl Pts',(3.21535986274144,-5.95430516123178,
59.9604274806943));
#198476=CARTESIAN_POINT('Ctrl Pts',(3.37902914073127,-5.86592278697276,
59.9691770405234));
#198477=CARTESIAN_POINT('Ctrl Pts',(3.53905210621852,-5.7707883574177,59.9779266003524));
#198478=CARTESIAN_POINT('Ctrl Pts',(3.69488522831972,-5.6692250043145,59.9866761601815));
#198479=CARTESIAN_POINT('Ctrl Pts',(3.85071701407214,-5.56766252216904,
59.9954256449786));
#198480=CARTESIAN_POINT('Ctrl Pts',(4.00235878822677,-5.4596713832917,60.0041751297757));
#198481=CARTESIAN_POINT('Ctrl Pts',(4.14929549611596,-5.34561838199397,
60.0129246145728));
#198482=CARTESIAN_POINT('Ctrl Pts',(4.29623099276355,-5.23156632086797,
60.0216740272454));
#198483=CARTESIAN_POINT('Ctrl Pts',(4.43846127436287,-5.11145267304739,
60.030423439918));
#198484=CARTESIAN_POINT('Ctrl Pts',(4.57550326054695,-4.98568540049653,
60.0391728525906));
#198485=CARTESIAN_POINT('Ctrl Pts',(4.71254416258024,-4.85991912290124,
60.0479221960459));
#198486=CARTESIAN_POINT('Ctrl Pts',(4.84439664018995,-4.72849950385179,
60.0566715395011));
#198487=CARTESIAN_POINT('Ctrl Pts',(4.97061286794969,-4.59187289860825,
60.0654208829563));
#198488=CARTESIAN_POINT('Ctrl Pts',(5.09682813912891,-4.45524732884448,
60.0741701601012));
#198489=CARTESIAN_POINT('Ctrl Pts',(5.21740705148029,-4.31341506235557,
60.082919437246));
#198490=CARTESIAN_POINT('Ctrl Pts',(5.3319400754587,-4.16685781275501,60.0916687143908));
#198491=CARTESIAN_POINT('Ctrl Pts',(5.44647226944652,-4.02030162521616,
60.1004179281319));
#198492=CARTESIAN_POINT('Ctrl Pts',(5.55495848628272,-3.86902074887706,
60.1091671418731));
#198493=CARTESIAN_POINT('Ctrl Pts',(5.65703027291939,-3.71352898080432,
60.1179163556142));
#198494=CARTESIAN_POINT('Ctrl Pts',(5.75910135377141,-3.55803828789356,
60.1266655088581));
#198495=CARTESIAN_POINT('Ctrl Pts',(5.85475793592888,-3.39833700106478,
60.1354146621019));
#198496=CARTESIAN_POINT('Ctrl Pts',(5.94367514427526,-3.23496750823319,
60.1441638153458));
#198497=CARTESIAN_POINT('Ctrl Pts',(6.0325917673276,-3.0715990907749,60.1529129109987));
#198498=CARTESIAN_POINT('Ctrl Pts',(6.11476896836036,-2.90456276731199,
60.1616620066517));
#198499=CARTESIAN_POINT('Ctrl Pts',(6.1899276554799,-2.73442583002815,60.1704111023046));
#198500=CARTESIAN_POINT('Ctrl Pts',(6.26508587283144,-2.56428995615949,
60.1791601432726));
#198501=CARTESIAN_POINT('Ctrl Pts',(6.33322554827237,-2.39105376934996,
60.1879091842406));
#198502=CARTESIAN_POINT('Ctrl Pts',(6.39411526733096,-2.21530561053889,
60.1966582252087));
#198503=CARTESIAN_POINT('Ctrl Pts',(6.45500462602905,-2.03955849184915,
60.2054072143977));
#198504=CARTESIAN_POINT('Ctrl Pts',(6.50864402040791,-1.86129970164368,
60.2141562035867));
#198505=CARTESIAN_POINT('Ctrl Pts',(6.55485128368644,-1.6811346313589,60.2229051927757));
#198506=CARTESIAN_POINT('Ctrl Pts',(6.60199809554361,-1.49730620116714,
60.2318320782472));
#198507=CARTESIAN_POINT('Ctrl Pts',(6.64140720707901,-1.31149343245558,
60.2407589637186));
#198508=CARTESIAN_POINT('Ctrl Pts',(6.67293928722905,-1.124353266974,60.24968584919));
#198509=CARTESIAN_POINT('Ctrl Pts',(6.70384625876274,-0.940923067005351,
60.2584357633675));
#198510=CARTESIAN_POINT('Ctrl Pts',(6.7271855457981,-0.756217899520448,
60.2671856775449));
#198511=CARTESIAN_POINT('Ctrl Pts',(6.74287786815338,-0.570865181253302,
60.2759355917224));
#198512=CARTESIAN_POINT('Ctrl Pts',(6.75856988190852,-0.385516108072819,
60.2846853338269));
#198513=CARTESIAN_POINT('Ctrl Pts',(6.76661520773406,-0.19951979522529,
60.2934350759314));
#198514=CARTESIAN_POINT('Ctrl Pts',(6.76698651789579,-0.0135080204546609,
60.3021848180358));
#198515=CARTESIAN_POINT('Ctrl Pts',(6.767357821249,0.172500343513941,60.3109343997008));
#198516=CARTESIAN_POINT('Ctrl Pts',(6.76005538995179,0.358523882211893,
60.3196839813658));
#198517=CARTESIAN_POINT('Ctrl Pts',(6.74510402742353,0.54393074856534,60.3284335630308));
#198518=CARTESIAN_POINT('Ctrl Pts',(6.7301529191802,0.729334461616193,60.3371829958874));
#198519=CARTESIAN_POINT('Ctrl Pts',(6.70755316306582,0.914121237635632,
60.3459324287441));
#198520=CARTESIAN_POINT('Ctrl Pts',(6.67738151874559,1.09766345166216,60.3546818616008));
#198521=CARTESIAN_POINT('Ctrl Pts',(6.64721034747551,1.28120278799758,60.3634311572783));
#198522=CARTESIAN_POINT('Ctrl Pts',(6.60946757205121,1.46349731860422,60.3721804529559));
#198523=CARTESIAN_POINT('Ctrl Pts',(6.564281381115,1.64392790278255,60.3809297486334));
#198524=CARTESIAN_POINT('Ctrl Pts',(6.51909583859825,1.82435589779144,60.389678918759));
#198525=CARTESIAN_POINT('Ctrl Pts',(6.46646716392849,2.00291972192349,60.3984280888846));
#198526=CARTESIAN_POINT('Ctrl Pts',(6.40657409872857,2.17901292274742,60.4071772590102));
#198527=CARTESIAN_POINT('Ctrl Pts',(6.34668181342048,2.35510383059053,60.4159263152093));
#198528=CARTESIAN_POINT('Ctrl Pts',(6.27952541914021,2.52872390822653,60.4246753714084));
#198529=CARTESIAN_POINT('Ctrl Pts',(6.20533299175486,2.69928350890356,60.4334244276075));
#198530=CARTESIAN_POINT('Ctrl Pts',(6.12831602991515,2.87633637965696,60.4425065637657));
#198531=CARTESIAN_POINT('Ctrl Pts',(6.04371690605232,3.05009086601537,60.4515886999239));
#198532=CARTESIAN_POINT('Ctrl Pts',(5.95184520316589,3.21991112882812,60.4606708360821));
#198533=CARTESIAN_POINT('Ctrl Pts',(5.86333549509226,3.38351691183101,60.4694206164257));
#198534=CARTESIAN_POINT('Ctrl Pts',(5.76807618099313,3.54347103712095,60.4781703967692));
#198535=CARTESIAN_POINT('Ctrl Pts',(5.66639083308952,3.69923018027793,60.4869201771128));
#198536=CARTESIAN_POINT('Ctrl Pts',(5.56470914082134,3.85498372382145,60.4956696428977));
#198537=CARTESIAN_POINT('Ctrl Pts',(5.45660203371999,4.00654234702091,60.5044191086826));
#198538=CARTESIAN_POINT('Ctrl Pts',(5.34243669839146,4.15339127986759,60.5131685744675));
#198539=CARTESIAN_POINT('Ctrl Pts',(5.22827486050517,4.3002357140137,60.5219177722136));
#198540=CARTESIAN_POINT('Ctrl Pts',(5.10805534167032,4.4423705202856,60.5306669699596));
#198541=CARTESIAN_POINT('Ctrl Pts',(4.98218644339868,4.57931296628811,60.5394161677056));
#198542=CARTESIAN_POINT('Ctrl Pts',(4.85632073219498,4.71625194483451,60.5481651439172));
#198543=CARTESIAN_POINT('Ctrl Pts',(4.72480612170226,4.84799861524599,60.5569141201289));
#198544=CARTESIAN_POINT('Ctrl Pts',(4.58808925235213,4.97410554898575,60.5656630963405));
#198545=CARTESIAN_POINT('Ctrl Pts',(4.45136349473951,5.10022068121291,60.5744126413422));
#198546=CARTESIAN_POINT('Ctrl Pts',(4.30943501209983,5.22069514871914,60.5831621863439));
#198547=CARTESIAN_POINT('Ctrl Pts',(4.16278587431686,5.33511975166331,60.5919117313456));
#198548=CARTESIAN_POINT('Ctrl Pts',(4.01614535740335,5.44953762807926,60.6006607619993));
#198549=CARTESIAN_POINT('Ctrl Pts',(3.86478496657793,5.55790617532875,60.6094097926531));
#198550=CARTESIAN_POINT('Ctrl Pts',(3.70921874747046,5.65985735539454,60.6181588233068));
#198551=CARTESIAN_POINT('Ctrl Pts',(3.55365041605759,5.76180991977134,60.6269079727564));
#198552=CARTESIAN_POINT('Ctrl Pts',(3.39387638174388,5.85734478552891,60.635657122206));
#198553=CARTESIAN_POINT('Ctrl Pts',(3.23043927904413,5.946137491213,60.6444062716557));
#198554=CARTESIAN_POINT('Ctrl Pts',(3.18691767070344,5.96978206944193,60.6467360795718));
#198555=CARTESIAN_POINT('Ctrl Pts',(3.14313645919583,5.9929488063345,60.6490658874879));
#198556=CARTESIAN_POINT('Ctrl Pts',(3.09910619832132,6.01563211736941,60.6513956954041));
#198557=CARTESIAN_POINT('Origin',(0.,0.,4.30282021618968));
#198558=CARTESIAN_POINT('',(3.09910619832125,6.01563211736945,63.0457521963359));
#198559=CARTESIAN_POINT('',(3.09910619832141,6.01563211736936,62.6510873080017));
#198560=CARTESIAN_POINT('',(3.09910619832133,6.0156321173694,4.30282021618968));
#198561=CARTESIAN_POINT('',(-6.76699974432514,0.00186018910577019,61.6971797837854));
#198562=CARTESIAN_POINT('Ctrl Pts',(-6.76699974432528,0.00186018858652958,
61.69717978381));
#198563=CARTESIAN_POINT('Ctrl Pts',(-6.76700888267723,-0.0313833361700197,
61.698754657245));
#198564=CARTESIAN_POINT('Ctrl Pts',(-6.76677305573693,-0.0646273068054331,
61.70032953068));
#198565=CARTESIAN_POINT('Ctrl Pts',(-6.7662922309777,-0.097869530553651,
61.701904404115));
#198566=CARTESIAN_POINT('Ctrl Pts',(-6.76382858940636,-0.268195460695293,
61.7099737133375));
#198567=CARTESIAN_POINT('Ctrl Pts',(-6.75492480586881,-0.438740522579581,
61.71804302256));
#198568=CARTESIAN_POINT('Ctrl Pts',(-6.7395436862802,-0.608966255814484,
61.7261123317825));
#198569=CARTESIAN_POINT('Ctrl Pts',(-6.72418175112818,-0.778979671294108,
61.7341715763833));
#198570=CARTESIAN_POINT('Ctrl Pts',(-6.70235858813183,-0.948674183693938,
61.742230820984));
#198571=CARTESIAN_POINT('Ctrl Pts',(-6.67408890878531,-1.11750894297491,
61.7502900655848));
#198572=CARTESIAN_POINT('Ctrl Pts',(-6.64584828567779,-1.28617016993328,
61.758341026705));
#198573=CARTESIAN_POINT('Ctrl Pts',(-6.61117439294617,-1.45397303739914,
61.7663919878253));
#198574=CARTESIAN_POINT('Ctrl Pts',(-6.57013387633598,-1.62037953795473,
61.7744429489456));
#198575=CARTESIAN_POINT('Ctrl Pts',(-6.52912654933898,-1.78665146497562,
61.7824873992246));
#198576=CARTESIAN_POINT('Ctrl Pts',(-6.48176293499712,-1.95152891222019,
61.7905318495037));
#198577=CARTESIAN_POINT('Ctrl Pts',(-6.42816110462577,-2.11448192543149,
61.7985762997828));
#198578=CARTESIAN_POINT('Ctrl Pts',(-6.37459088930749,-2.27733882684724,
61.8066160053411));
#198579=CARTESIAN_POINT('Ctrl Pts',(-6.31478989880819,-2.4382732002311,
61.8146557108993));
#198580=CARTESIAN_POINT('Ctrl Pts',(-6.24892658892837,-2.59676827733706,
61.8226954164575));
#198581=CARTESIAN_POINT('Ctrl Pts',(-6.18164165471705,-2.75868438594671,
61.830908654762));
#198582=CARTESIAN_POINT('Ctrl Pts',(-6.10802981782756,-2.91805431215768,
61.8391218930664));
#198583=CARTESIAN_POINT('Ctrl Pts',(-6.02832354973824,-3.07434613855879,
61.8473351313709));
#198584=CARTESIAN_POINT('Ctrl Pts',(-5.9503264647624,-3.22728651774173,
61.8553722489191));
#198585=CARTESIAN_POINT('Ctrl Pts',(-5.86649385885111,-3.37727912908345,
61.8634093664673));
#198586=CARTESIAN_POINT('Ctrl Pts',(-5.77709092958998,-3.5238486617971,
61.8714464840154));
#198587=CARTESIAN_POINT('Ctrl Pts',(-5.68767854206744,-3.67043370063529,
61.8794844518396));
#198588=CARTESIAN_POINT('Ctrl Pts',(-5.59269485227502,-3.81359462072695,
61.8875224196637));
#198589=CARTESIAN_POINT('Ctrl Pts',(-5.4924492683956,-3.95288376177452,
61.8955603874878));
#198590=CARTESIAN_POINT('Ctrl Pts',(-5.39217321682531,-4.09221523704097,
61.9036007982955));
#198591=CARTESIAN_POINT('Ctrl Pts',(-5.28663230600283,-4.22767228787798,
61.9116412091032));
#198592=CARTESIAN_POINT('Ctrl Pts',(-5.17617712363885,-4.35883922446308,
61.9196816199109));
#198593=CARTESIAN_POINT('Ctrl Pts',(-5.06154735835593,-4.49496353146103,
61.9280259128988));
#198594=CARTESIAN_POINT('Ctrl Pts',(-4.94162488735914,-4.62646676344811,
61.9363702058866));
#198595=CARTESIAN_POINT('Ctrl Pts',(-4.81684379510684,-4.75292592552638,
61.9447144988744));
#198596=CARTESIAN_POINT('Ctrl Pts',(-4.69639463760129,-4.8749948965239,
61.9527691090899));
#198597=CARTESIAN_POINT('Ctrl Pts',(-4.57141886569017,-4.9923639484135,
61.9608237193054));
#198598=CARTESIAN_POINT('Ctrl Pts',(-4.44234051109221,-5.10469389714104,
61.968878329521));
#198599=CARTESIAN_POINT('Ctrl Pts',(-4.31316444235635,-5.21710888122664,
61.9769390371902));
#198600=CARTESIAN_POINT('Ctrl Pts',(-4.17987989599693,-5.32447693396655,
61.9849997448595));
#198601=CARTESIAN_POINT('Ctrl Pts',(-4.0429402500153,-5.42650192433452,
61.9930604525288));
#198602=CARTESIAN_POINT('Ctrl Pts',(-3.90580752733713,-5.52867076382641,
62.0011325253129));
#198603=CARTESIAN_POINT('Ctrl Pts',(-3.76500972787653,-5.62548130090922,
62.0092045980971));
#198604=CARTESIAN_POINT('Ctrl Pts',(-3.6210256756095,-5.71668278432316,
62.0172766708812));
#198605=CARTESIAN_POINT('Ctrl Pts',(-3.60594444009007,-5.72623544678425,
62.0181221591757));
#198606=CARTESIAN_POINT('Ctrl Pts',(-3.59082826677618,-5.73572661583186,
62.0189676474702));
#198607=CARTESIAN_POINT('Ctrl Pts',(-3.57567771841961,-5.74515603391218,
62.0198131357647));
#198608=CARTESIAN_POINT('Ctrl Pts',(-3.42635768733166,-5.83809002994699,
62.0281460578114));
#198609=CARTESIAN_POINT('Ctrl Pts',(-3.27322051995201,-5.92531833426816,
62.0364789798581));
#198610=CARTESIAN_POINT('Ctrl Pts',(-3.11673520276891,-6.00651734999751,
62.0448119019049));
#198611=CARTESIAN_POINT('Ctrl Pts',(-2.96043481328268,-6.0876204081812,
62.0531349764585));
#198612=CARTESIAN_POINT('Ctrl Pts',(-2.80079446225958,-6.16270821275327,
62.0614580510121));
#198613=CARTESIAN_POINT('Ctrl Pts',(-2.63831147126212,-6.23150074866454,
62.0697811255657));
#198614=CARTESIAN_POINT('Ctrl Pts',(-2.47599067107149,-6.3002246157457,
62.0780958920117));
#198615=CARTESIAN_POINT('Ctrl Pts',(-2.31083320259564,-6.36266559899581,
62.0864106584577));
#198616=CARTESIAN_POINT('Ctrl Pts',(-2.14336051423539,-6.41858977548937,
62.0947254249036));
#198617=CARTESIAN_POINT('Ctrl Pts',(-1.97602427727905,-6.47446838674796,
62.1030334167432));
#198618=CARTESIAN_POINT('Ctrl Pts',(-1.80637690779052,-6.52384066150702,
62.1113414085827));
#198619=CARTESIAN_POINT('Ctrl Pts',(-1.63495955161181,-6.56652086455174,
62.1196494004222));
#198620=CARTESIAN_POINT('Ctrl Pts',(-1.46365043426143,-6.60917411784484,
62.1279521463093));
#198621=CARTESIAN_POINT('Ctrl Pts',(-1.29057389421217,-6.64514363672157,
62.1362548921963));
#198622=CARTESIAN_POINT('Ctrl Pts',(-1.11628616519195,-6.67429353545385,
62.1445576380834));
#198623=CARTESIAN_POINT('Ctrl Pts',(-0.942069662011984,-6.70343152155154,
62.1528569909028));
#198624=CARTESIAN_POINT('Ctrl Pts',(-0.766643298753215,-6.72575538342788,
62.1611563437222));
#198625=CARTESIAN_POINT('Ctrl Pts',(-0.590573717251133,-6.74118028868033,
62.1694556965417));
#198626=CARTESIAN_POINT('Ctrl Pts',(-0.414541582794685,-6.75660191331425,
62.177753284228));
#198627=CARTESIAN_POINT('Ctrl Pts',(-0.237866849011761,-6.76512747415664,
62.1860508719144));
#198628=CARTESIAN_POINT('Ctrl Pts',(-0.0611217481314931,-6.76672395860104,
62.1943484596007));
#198629=CARTESIAN_POINT('Ctrl Pts',(0.115615132693807,-6.7683203687962,
62.2026456613831));
#198630=CARTESIAN_POINT('Ctrl Pts',(0.292422026227014,-6.76298834178729,
62.2109428631655));
#198631=CARTESIAN_POINT('Ctrl Pts',(0.468726030304149,-6.75074698892762,
62.219240064948));
#198632=CARTESIAN_POINT('Ctrl Pts',(0.645051130896099,-6.73850417126922,
62.2275382595725));
#198633=CARTESIAN_POINT('Ctrl Pts',(0.820872875120574,-6.71935040502058,
62.235836454197));
#198634=CARTESIAN_POINT('Ctrl Pts',(0.995622617714268,-6.69335675151831,
62.2441346488216));
#198635=CARTESIAN_POINT('Ctrl Pts',(1.17049526383936,-6.66734481637648,
62.2524386796632));
#198636=CARTESIAN_POINT('Ctrl Pts',(1.34429405725153,-6.63448343276056,
62.2607427105047));
#198637=CARTESIAN_POINT('Ctrl Pts',(1.51645879770513,-6.59489512538772,
62.2690467413463));
#198638=CARTESIAN_POINT('Ctrl Pts',(1.68868614199685,-6.55529242261673,
62.2773537917621));
#198639=CARTESIAN_POINT('Ctrl Pts',(1.85927791168808,-6.50895800586749,
62.2856608421778));
#198640=CARTESIAN_POINT('Ctrl Pts',(2.02768801864551,-6.45606461391469,
62.2939678925935));
#198641=CARTESIAN_POINT('Ctrl Pts',(2.19627818443031,-6.40311466999893,
62.3022838246482));
#198642=CARTESIAN_POINT('Ctrl Pts',(2.36268169710778,-6.34359185088309,
62.3105997567028));
#198643=CARTESIAN_POINT('Ctrl Pts',(2.52637039754753,-6.27771786674071,
62.3189156887574));
#198644=CARTESIAN_POINT('Ctrl Pts',(2.64976241679885,-6.22806065828575,
62.3251844149763));
#198645=CARTESIAN_POINT('Ctrl Pts',(2.77161212861598,-6.17479543469104,
62.3314531411952));
#198646=CARTESIAN_POINT('Ctrl Pts',(2.89170231692055,-6.11803454634872,
62.337721867414));
#198647=CARTESIAN_POINT('Ctrl Pts',(3.05358438462945,-6.04152063543249,
62.3461721361374));
#198648=CARTESIAN_POINT('Ctrl Pts',(3.21256520260729,-5.95851280788114,
62.3546224048607));
#198649=CARTESIAN_POINT('Ctrl Pts',(3.36810870078526,-5.86925317052303,
62.3630726735841));
#198650=CARTESIAN_POINT('Ctrl Pts',(3.52351492654881,-5.78007230782329,
62.3715154846586));
#198651=CARTESIAN_POINT('Ctrl Pts',(3.67548959267449,-5.68465079682643,
62.3799582957331));
#198652=CARTESIAN_POINT('Ctrl Pts',(3.82351956618513,-5.58327745387953,
62.3884011068076));
#198653=CARTESIAN_POINT('Ctrl Pts',(3.97143905288291,-5.48197977410615,
62.3968376163253));
#198654=CARTESIAN_POINT('Ctrl Pts',(4.11541944346791,-5.37473930466906,
62.405274125843));
#198655=CARTESIAN_POINT('Ctrl Pts',(4.25497470436759,-5.26188932468101,
62.4137106353607));
#198656=CARTESIAN_POINT('Ctrl Pts',(4.39443010596926,-5.14912009492559,
62.4221411081019));
#198657=CARTESIAN_POINT('Ctrl Pts',(4.52946643660968,-5.03074956898987,
62.4305715808431));
#198658=CARTESIAN_POINT('Ctrl Pts',(4.65962884076262,-4.90715274536397,
62.4390020535843));
#198659=CARTESIAN_POINT('Ctrl Pts',(4.7897352884504,-4.78360905567796,62.4474289020881));
#198660=CARTESIAN_POINT('Ctrl Pts',(4.9149717466706,-4.65484377522036,62.4558557505919));
#198661=CARTESIAN_POINT('Ctrl Pts',(5.03491800266433,-4.52127080658156,
62.4642825990957));
#198662=CARTESIAN_POINT('Ctrl Pts',(5.15482723553273,-4.3877390671476,62.4727068465323));
#198663=CARTESIAN_POINT('Ctrl Pts',(5.26944930127381,-4.24940284532616,
62.4811310939689));
#198664=CARTESIAN_POINT('Ctrl Pts',(5.37840204215944,-4.10671163741688,
62.4895553414056));
#198665=CARTESIAN_POINT('Ctrl Pts',(5.40910075594672,-4.0665067144754,62.4919289720167));
#198666=CARTESIAN_POINT('Ctrl Pts',(5.43934962480274,-4.02595625746157,
62.4943026026278));
#198667=CARTESIAN_POINT('Ctrl Pts',(5.46914067786036,-3.98507079557857,
62.4966762332389));
#198668=CARTESIAN_POINT('Ctrl Pts',(5.57731360038267,-3.83661347545612,
62.5052950141761));
#198669=CARTESIAN_POINT('Ctrl Pts',(5.67939881289885,-3.68380335449862,
62.5139137951133));
#198670=CARTESIAN_POINT('Ctrl Pts',(5.77506832117722,-3.52716244107573,
62.5225325760505));
#198671=CARTESIAN_POINT('Ctrl Pts',(5.87079529754818,-3.37042743440748,
62.531156534237));
#198672=CARTESIAN_POINT('Ctrl Pts',(5.9600987199737,-3.20985730249598,62.5397804924236));
#198673=CARTESIAN_POINT('Ctrl Pts',(6.04269602840139,-3.04599962382501,
62.5484044506101));
#198674=CARTESIAN_POINT('Ctrl Pts',(6.12827729576277,-2.87622232630165,
62.5573399629813));
#198675=CARTESIAN_POINT('Ctrl Pts',(6.20665872006912,-2.70291584292701,
62.5662754753524));
#198676=CARTESIAN_POINT('Ctrl Pts',(6.27758023075002,-2.5267123790603,62.5752109877235));
#198677=CARTESIAN_POINT('Ctrl Pts',(6.34615689820091,-2.35633464416332,
62.5838510696182));
#198678=CARTESIAN_POINT('Ctrl Pts',(6.40775898527662,-2.18324872818015,
62.5924911515129));
#198679=CARTESIAN_POINT('Ctrl Pts',(6.46220194008558,-2.0080426005327,62.6011312334076));
#198680=CARTESIAN_POINT('Ctrl Pts',(6.51943724830169,-1.82385023344974,
62.610214461017));
#198681=CARTESIAN_POINT('Ctrl Pts',(6.56875965702786,-1.63731483298587,
62.6192976886263));
#198682=CARTESIAN_POINT('Ctrl Pts',(6.61001524464286,-1.44913334982983,
62.6283809162356));
#198683=CARTESIAN_POINT('Ctrl Pts',(6.65127083225785,-1.26095186667384,
62.6374641438449));
#198684=CARTESIAN_POINT('Ctrl Pts',(6.68445956512924,-1.07112468860344,
62.6465473714543));
#198685=CARTESIAN_POINT('Ctrl Pts',(6.7094903097447,-0.88035719082765,62.6556305990636));
#198686=CARTESIAN_POINT('Ctrl Pts',(6.73441459369128,-0.690401064656113,
62.6646751939234));
#198687=CARTESIAN_POINT('Ctrl Pts',(6.75127402270358,-0.49933729491443,
62.6737197887833));
#198688=CARTESIAN_POINT('Ctrl Pts',(6.75999462970576,-0.307833731662577,
62.6827643836431));
#198689=CARTESIAN_POINT('Ctrl Pts',(6.76870723417835,-0.116505903073646,
62.6918006786634));
#198690=CARTESIAN_POINT('Ctrl Pts',(6.76929591702558,0.0752606758338459,
62.7008369736838));
#198691=CARTESIAN_POINT('Ctrl Pts',(6.76173865261451,0.26679466587419,62.7098732687042));
#198692=CARTESIAN_POINT('Ctrl Pts',(6.75419476137546,0.457989721499053,
62.7188935732919));
#198693=CARTESIAN_POINT('Ctrl Pts',(6.73853371694772,0.648952772738747,
62.7279138778796));
#198694=CARTESIAN_POINT('Ctrl Pts',(6.71478547954788,0.839014280958885,
62.7369341824673));
#198695=CARTESIAN_POINT('Ctrl Pts',(6.6910671484399,1.02883644362932,62.7459431277336));
#198696=CARTESIAN_POINT('Ctrl Pts',(6.65928197802554,1.21775909363292,62.7549520729999));
#198697=CARTESIAN_POINT('Ctrl Pts',(6.61951169806382,1.40511703398552,62.7639610182662));
#198698=CARTESIAN_POINT('Ctrl Pts',(6.5798317279884,1.59204952411984,62.772949506125));
#198699=CARTESIAN_POINT('Ctrl Pts',(6.53220289169279,1.77742416466695,62.7819379939839));
#198700=CARTESIAN_POINT('Ctrl Pts',(6.47675789903176,1.96058565671835,62.7909264818427));
#198701=CARTESIAN_POINT('Ctrl Pts',(6.42811254883714,2.12128465757279,62.7988126428579));
#198702=CARTESIAN_POINT('Ctrl Pts',(6.37345136413233,2.28028003127382,62.8066988038731));
#198703=CARTESIAN_POINT('Ctrl Pts',(6.31289654940264,2.43713482526926,62.8145849648884));
#198704=CARTESIAN_POINT('Ctrl Pts',(6.2505349264596,2.59866978435746,62.8227064297445));
#198705=CARTESIAN_POINT('Ctrl Pts',(6.18194911347087,2.75786161962484,62.8308278946007));
#198706=CARTESIAN_POINT('Ctrl Pts',(6.10735042438937,2.91419968322539,62.8389493594569));
#198707=CARTESIAN_POINT('Ctrl Pts',(6.03275705529221,3.0705265976213,62.8470702451331));
#198708=CARTESIAN_POINT('Ctrl Pts',(5.9521518219221,3.22399981523457,62.8551911308093));
#198709=CARTESIAN_POINT('Ctrl Pts',(5.86579323692356,3.37413080683927,62.8633120164855));
#198710=CARTESIAN_POINT('Ctrl Pts',(5.77942432960469,3.52427974339045,62.8714338728398));
#198711=CARTESIAN_POINT('Ctrl Pts',(5.68730088493318,3.67108534163933,62.8795557291941));
#198712=CARTESIAN_POINT('Ctrl Pts',(5.58972618509928,3.81408575881762,62.8876775855483));
#198713=CARTESIAN_POINT('Ctrl Pts',(5.49208029597166,3.95719050733098,62.8958053675085));
#198714=CARTESIAN_POINT('Ctrl Pts',(5.3889754147992,4.09648422712913,62.9039331494687));
#198715=CARTESIAN_POINT('Ctrl Pts',(5.28075715399485,4.23153552277802,62.9120609314289));
#198716=CARTESIAN_POINT('Ctrl Pts',(5.17249480909339,4.36664183330505,62.9201920243453));
#198717=CARTESIAN_POINT('Ctrl Pts',(5.05911517217354,4.49750199832047,62.9283231172618));
#198718=CARTESIAN_POINT('Ctrl Pts',(4.94100239287162,4.6237197529302,62.9364542101782));
#198719=CARTESIAN_POINT('Ctrl Pts',(4.82276069840703,4.75007526894444,62.9445941778428));
#198720=CARTESIAN_POINT('Ctrl Pts',(4.69977580325369,4.87177799681061,62.9527341455073));
#198721=CARTESIAN_POINT('Ctrl Pts',(4.57246730136593,4.98846988343514,62.9608741131719));
#198722=CARTESIAN_POINT('Ctrl Pts',(4.50643960782099,5.04899134127162,62.9650958523523));
#198723=CARTESIAN_POINT('Ctrl Pts',(4.43924943815944,5.10816559862391,62.9693175915328));
#198724=CARTESIAN_POINT('Ctrl Pts',(4.37095855157181,5.16594718715177,62.9735393307132));
#198725=CARTESIAN_POINT('Ctrl Pts',(4.23442476346711,5.28146976356893,62.9819798426394));
#198726=CARTESIAN_POINT('Ctrl Pts',(4.09320717501415,5.39166184854721,62.9904203545656));
#198727=CARTESIAN_POINT('Ctrl Pts',(3.94775019044169,5.49614023054977,62.9988608664918));
#198728=CARTESIAN_POINT('Ctrl Pts',(3.8024168135024,5.60052982805321,63.0072942057703));
#198729=CARTESIAN_POINT('Ctrl Pts',(3.6528514942629,5.6992152109744,63.0157275450489));
#198730=CARTESIAN_POINT('Ctrl Pts',(3.49953110373262,5.79185385295658,63.0241608843274));
#198731=CARTESIAN_POINT('Ctrl Pts',(3.368685805096,5.87091268351086,63.0313579883302));
#198732=CARTESIAN_POINT('Ctrl Pts',(3.23510629795606,5.94556819997437,63.0385550923331));
#198733=CARTESIAN_POINT('Ctrl Pts',(3.09910619832125,6.01563211736945,63.0457521963359));
#198734=CARTESIAN_POINT('Ctrl Pts',(3.09910619832126,6.01563211736944,61.0457854935189));
#198735=CARTESIAN_POINT('Ctrl Pts',(2.971669387342,6.08128443837155,61.052552642618));
#198736=CARTESIAN_POINT('Ctrl Pts',(2.84222364202814,6.14284547814351,61.059319791717));
#198737=CARTESIAN_POINT('Ctrl Pts',(2.71104814989807,6.20020216839212,61.066086940816));
#198738=CARTESIAN_POINT('Ctrl Pts',(2.55133175682986,6.27003841246547,61.0743264726669));
#198739=CARTESIAN_POINT('Ctrl Pts',(2.38869389354897,6.33379606301573,61.0825660045177));
#198740=CARTESIAN_POINT('Ctrl Pts',(2.22363567814493,6.39122315139136,61.0908055363685));
#198741=CARTESIAN_POINT('Ctrl Pts',(2.05876066582408,6.44858649971248,61.0990359229148));
#198742=CARTESIAN_POINT('Ctrl Pts',(1.89147098367788,6.49963316084281,61.1072663094612));
#198743=CARTESIAN_POINT('Ctrl Pts',(1.72228992832713,6.54415818900972,61.1154966960075));
#198744=CARTESIAN_POINT('Ctrl Pts',(1.55326647177858,6.58864174036297,61.1237194156253));
#198745=CARTESIAN_POINT('Ctrl Pts',(1.38235549301942,6.62661566748188,61.1319421352431));
#198746=CARTESIAN_POINT('Ctrl Pts',(1.21009783489472,6.65792401803919,61.1401648548609));
#198747=CARTESIAN_POINT('Ctrl Pts',(1.03799280946576,6.68920462714224,61.1483802885566));
#198748=CARTESIAN_POINT('Ctrl Pts',(0.864543831775616,6.71383136785693,
61.1565957222524));
#198749=CARTESIAN_POINT('Ctrl Pts',(0.690304263422528,6.73169882153834,
61.1648111559482));
#198750=CARTESIAN_POINT('Ctrl Pts',(0.516154240677573,6.749557092736,61.173022367549));
#198751=CARTESIAN_POINT('Ctrl Pts',(0.341214789640626,6.76066295895982,
61.1812335791498));
#198752=CARTESIAN_POINT('Ctrl Pts',(0.166047180039049,6.76496247838826,
61.1894447907506));
#198753=CARTESIAN_POINT('Ctrl Pts',(-0.00906168801186097,6.76926055599514,
61.1976532487642));
#198754=CARTESIAN_POINT('Ctrl Pts',(-0.184398206791257,6.76675682496721,
61.2058617067777));
#198755=CARTESIAN_POINT('Ctrl Pts',(-0.359398201402664,6.75744936590934,
61.2140701647912));
#198756=CARTESIAN_POINT('Ctrl Pts',(-0.437364520265389,6.75330268966333,
61.2177272120744));
#198757=CARTESIAN_POINT('Ctrl Pts',(-0.515264028797898,6.74780623484948,
61.2213842593576));
#198758=CARTESIAN_POINT('Ctrl Pts',(-0.593046898541615,6.74096316383128,
61.2250413066408));
#198759=CARTESIAN_POINT('Ctrl Pts',(-0.78147328718548,6.72438605419979,
61.2339003808167));
#198760=CARTESIAN_POINT('Ctrl Pts',(-0.969019035950057,6.69992049979116,
61.2427594549926));
#198761=CARTESIAN_POINT('Ctrl Pts',(-1.15504361701545,6.66769549715581,
61.2516185291685));
#198762=CARTESIAN_POINT('Ctrl Pts',(-1.34141770084286,6.63540995022377,
61.2604942477624));
#198763=CARTESIAN_POINT('Ctrl Pts',(-1.5262646500587,6.59533586513905,61.2693699663564));
#198764=CARTESIAN_POINT('Ctrl Pts',(-1.70895641178248,6.54765278421417,
61.2782456849503));
#198765=CARTESIAN_POINT('Ctrl Pts',(-1.89216952417524,6.49983362924904,
61.2871467323373));
#198766=CARTESIAN_POINT('Ctrl Pts',(-2.07321488906964,6.44436209174639,
61.2960477797243));
#198767=CARTESIAN_POINT('Ctrl Pts',(-2.25147890250826,6.3814678367567,61.3049488271113));
#198768=CARTESIAN_POINT('Ctrl Pts',(-2.42998526831839,6.31848807616463,
61.3138619755943));
#198769=CARTESIAN_POINT('Ctrl Pts',(-2.60570248706574,6.2480655324972,61.3227751240773));
#198770=CARTESIAN_POINT('Ctrl Pts',(-2.77803784061023,6.17047767649618,
61.3316882725603));
#198771=CARTESIAN_POINT('Ctrl Pts',(-2.95075582576348,6.09271755423898,
61.3406212106702));
#198772=CARTESIAN_POINT('Ctrl Pts',(-3.12007668965096,6.00776040569,61.3495541487801));
#198773=CARTESIAN_POINT('Ctrl Pts',(-3.28543062583687,5.91593057792374,
61.35848708689));
#198774=CARTESIAN_POINT('Ctrl Pts',(-3.44282359776378,5.82852189666068,
61.3669899487485));
#198775=CARTESIAN_POINT('Ctrl Pts',(-3.59662246647734,5.73488682059762,
61.3754928106071));
#198776=CARTESIAN_POINT('Ctrl Pts',(-3.74636103213043,5.63534098497461,
61.3839956724656));
#198777=CARTESIAN_POINT('Ctrl Pts',(-3.89071306068689,5.53937610616163,
61.3921926613473));
#198778=CARTESIAN_POINT('Ctrl Pts',(-4.03157407539767,5.4377291067025,61.4003896502289));
#198779=CARTESIAN_POINT('Ctrl Pts',(-4.1684661687206,5.33068277054936,61.4085866391106));
#198780=CARTESIAN_POINT('Ctrl Pts',(-4.30521276970425,5.2237502059186,61.4167749160275));
#198781=CARTESIAN_POINT('Ctrl Pts',(-4.43799856612345,5.11142995130479,
61.4249631929445));
#198782=CARTESIAN_POINT('Ctrl Pts',(-4.56637335098806,4.99404880026078,
61.4331514698614));
#198783=CARTESIAN_POINT('Ctrl Pts',(-4.69463793991919,4.87676840829905,
61.4413327180241));
#198784=CARTESIAN_POINT('Ctrl Pts',(-4.8184987922927,4.75443601332382,61.4495139661867));
#198785=CARTESIAN_POINT('Ctrl Pts',(-4.93753757986241,4.62741954521594,
61.4576952143494));
#198786=CARTESIAN_POINT('Ctrl Pts',(-5.05649851333387,4.50048614879242,
61.465871111788));
#198787=CARTESIAN_POINT('Ctrl Pts',(-5.17064341706586,4.36887504342546,
61.4740470092267));
#198788=CARTESIAN_POINT('Ctrl Pts',(-5.2795897143172,4.23299202083775,61.4822229066654));
#198789=CARTESIAN_POINT('Ctrl Pts',(-5.38848701873598,4.09717010444952,
61.4903951274267));
#198790=CARTESIAN_POINT('Ctrl Pts',(-5.49219014816907,3.95708037907291,
61.4985673481881));
#198791=CARTESIAN_POINT('Ctrl Pts',(-5.59035580617994,3.81316285520436,
61.5067395689495));
#198792=CARTESIAN_POINT('Ctrl Pts',(-5.68851400498286,3.66925626704143,
61.5149111687372));
#198793=CARTESIAN_POINT('Ctrl Pts',(-5.78113535964076,3.52152275299368,
61.5230827685248));
#198794=CARTESIAN_POINT('Ctrl Pts',(-5.86791885457339,3.37043280843012,
61.5312543683125));
#198795=CARTESIAN_POINT('Ctrl Pts',(-5.95470251620644,3.21934257364135,
61.5394259837968));
#198796=CARTESIAN_POINT('Ctrl Pts',(-6.0356481148912,3.0648962084235,61.5475975992811));
#198797=CARTESIAN_POINT('Ctrl Pts',(-6.11049980374545,2.90759026488032,
61.5557692147654));
#198798=CARTESIAN_POINT('Ctrl Pts',(-6.18536549273228,2.75025489910103,
61.5639423586548));
#198799=CARTESIAN_POINT('Ctrl Pts',(-6.25413484616501,2.59005921596141,
61.5721155025442));
#198800=CARTESIAN_POINT('Ctrl Pts',(-6.3165995158996,2.4275212781224,61.5802886464335));
#198801=CARTESIAN_POINT('Ctrl Pts',(-6.3790874324696,2.26492285020627,61.588464832038));
#198802=CARTESIAN_POINT('Ctrl Pts',(-6.43526586246192,2.09998076852402,
61.5966410176425));
#198803=CARTESIAN_POINT('Ctrl Pts',(-6.48497581727025,1.93322984909193,
61.604817203247));
#198804=CARTESIAN_POINT('Ctrl Pts',(-6.53474271347514,1.76628792103258,
61.6130027544489));
#198805=CARTESIAN_POINT('Ctrl Pts',(-6.57802623055246,1.59753336300356,
61.6211883056509));
#198806=CARTESIAN_POINT('Ctrl Pts',(-6.61471793604195,1.42751379208924,
61.6293738568529));
#198807=CARTESIAN_POINT('Ctrl Pts',(-6.65143212392997,1.25739004374022,
61.6375644236523));
#198808=CARTESIAN_POINT('Ctrl Pts',(-6.68154638808421,1.08600009285269,
61.6457549904517));
#198809=CARTESIAN_POINT('Ctrl Pts',(-6.70500403871336,0.913898156709823,
61.6539455572511));
#198810=CARTESIAN_POINT('Ctrl Pts',(-6.72849721039538,0.741535612969445,
61.6621485267229));
#198811=CARTESIAN_POINT('Ctrl Pts',(-6.7453135950495,0.568459289010249,
61.6703514961947));
#198812=CARTESIAN_POINT('Ctrl Pts',(-6.75544856672205,0.39522609019773,
61.6785544656666));
#198813=CARTESIAN_POINT('Ctrl Pts',(-6.76311924712526,0.264114080589015,
61.6847629050395));
#198814=CARTESIAN_POINT('Ctrl Pts',(-6.76696371925884,0.132912249167229,
61.6909713444125));
#198815=CARTESIAN_POINT('Ctrl Pts',(-6.76699974432514,0.00186018910577469,
61.6971797837854));
#198816=CARTESIAN_POINT('',(-6.76699994399638,-0.00056233818115236,61.3028202161899));
#198817=CARTESIAN_POINT('Ctrl Pts',(3.09910619832132,6.01563211736941,60.6513956954041));
#198818=CARTESIAN_POINT('Ctrl Pts',(2.93375330764824,6.10081787314654,60.6601451433064));
#198819=CARTESIAN_POINT('Ctrl Pts',(2.76488627843068,6.1791820703704,60.6688945912087));
#198820=CARTESIAN_POINT('Ctrl Pts',(2.59307866646699,6.25045854553998,60.677644039111));
#198821=CARTESIAN_POINT('Ctrl Pts',(2.42127244185368,6.3217344451504,60.6863934163613));
#198822=CARTESIAN_POINT('Ctrl Pts',(2.24652594672451,6.38592262741843,60.6951427936116));
#198823=CARTESIAN_POINT('Ctrl Pts',(2.06943269687102,6.44280508110568,60.7038921708619));
#198824=CARTESIAN_POINT('Ctrl Pts',(1.89234081822058,6.49968709436172,60.7126414803672));
#198825=CARTESIAN_POINT('Ctrl Pts',(1.7129024940557,6.5492634045955,60.7213907898726));
#198826=CARTESIAN_POINT('Ctrl Pts',(1.5317271662504,6.59136563150388,60.7301400993779));
#198827=CARTESIAN_POINT('Ctrl Pts',(1.3505531810732,6.63346754640713,60.7388893440452));
#198828=CARTESIAN_POINT('Ctrl Pts',(1.1676424971441,6.66809542395777,60.7476385887124));
#198829=CARTESIAN_POINT('Ctrl Pts',(0.983616340614309,6.69513165624669,
60.7563878333796));
#198830=CARTESIAN_POINT('Ctrl Pts',(0.799591486713858,6.7221676971596,60.7651370161153));
#198831=CARTESIAN_POINT('Ctrl Pts',(0.614451459526792,6.7416121586937,60.773886198851));
#198832=CARTESIAN_POINT('Ctrl Pts',(0.428825047910427,6.75339900185711,
60.7826353815867));
#198833=CARTESIAN_POINT('Ctrl Pts',(0.243199888597162,6.7651857655022,60.7913845052973));
#198834=CARTESIAN_POINT('Ctrl Pts',(0.0570886373920053,6.76931499599834,
60.8001336290078));
#198835=CARTESIAN_POINT('Ctrl Pts',(-0.128876626811089,6.76577266947847,
60.8088827527183));
#198836=CARTESIAN_POINT('Ctrl Pts',(-0.314840698188105,6.76223036567993,
60.8176318203099));
#198837=CARTESIAN_POINT('Ctrl Pts',(-0.500658497951205,6.75101660879223,
60.8263808879014));
#198838=CARTESIAN_POINT('Ctrl Pts',(-0.685698951926176,6.73216948296219,
60.835129955493));
#198839=CARTESIAN_POINT('Ctrl Pts',(-0.870738280459975,6.71332247176292,
60.8438789698715));
#198840=CARTESIAN_POINT('Ctrl Pts',(-1.05499998761279,6.68684221356183,
60.85262798425));
#198841=CARTESIAN_POINT('Ctrl Pts',(-1.23785829161464,6.65281863948514,
60.8613769986286));
#198842=CARTESIAN_POINT('Ctrl Pts',(-1.43007412917444,6.61705395368852,
60.8705737323277));
#198843=CARTESIAN_POINT('Ctrl Pts',(-1.62073882535828,6.57295372727781,
60.8797704660269));
#198844=CARTESIAN_POINT('Ctrl Pts',(-1.80913696091546,6.52068343478271,
60.8889671997261));
#198845=CARTESIAN_POINT('Ctrl Pts',(-1.98838356186138,6.4709521981519,60.8977171974398));
#198846=CARTESIAN_POINT('Ctrl Pts',(-2.16557827572553,6.41382586850884,
60.9064671951535));
#198847=CARTESIAN_POINT('Ctrl Pts',(-2.34011918621713,6.34949849943273,
60.9152171928671));
#198848=CARTESIAN_POINT('Ctrl Pts',(-2.51465655691111,6.28517243495545,
60.9239670131255));
#198849=CARTESIAN_POINT('Ctrl Pts',(-2.6865399629534,6.21364572242369,60.9327168333838));
#198850=CARTESIAN_POINT('Ctrl Pts',(-2.8551855538,6.13516132252216,60.9414666536421));
#198851=CARTESIAN_POINT('Ctrl Pts',(-3.0238279485869,6.05667841000506,60.9502163080796));
#198852=CARTESIAN_POINT('Ctrl Pts',(-3.18923239109273,5.97123819492085,
60.9589659625171));
#198853=CARTESIAN_POINT('Ctrl Pts',(-3.3508370596768,5.87913088810723,60.9677156169546));
#198854=CARTESIAN_POINT('Ctrl Pts',(-3.51243888042383,5.78702520443113,
60.9764651172035));
#198855=CARTESIAN_POINT('Ctrl Pts',(-3.67024081223675,5.68825280605793,
60.9852146174524));
#198856=CARTESIAN_POINT('Ctrl Pts',(-3.82370687544387,5.58314917682514,
60.9939641177014));
#198857=CARTESIAN_POINT('Ctrl Pts',(-3.97717043817798,5.47804726008034,
61.0027134753919));
#198858=CARTESIAN_POINT('Ctrl Pts',(-4.1262980372244,5.36661448084251,61.0114628330823));
#198859=CARTESIAN_POINT('Ctrl Pts',(-4.27058317206885,5.24922931204595,
61.0202121907728));
#198860=CARTESIAN_POINT('Ctrl Pts',(-4.41486614774807,5.13184589986815,
61.0289614175329));
#198861=CARTESIAN_POINT('Ctrl Pts',(-4.5543065819438,5.00851045723065,61.0377106442929));
#198862=CARTESIAN_POINT('Ctrl Pts',(-4.68843089001807,4.87964187103156,
61.046459871053));
#198863=CARTESIAN_POINT('Ctrl Pts',(-4.82255336917802,4.75077504207996,
61.0552089785089));
#198864=CARTESIAN_POINT('Ctrl Pts',(-4.95135966065103,4.61637541908127,
61.0639580859649));
#198865=CARTESIAN_POINT('Ctrl Pts',(-5.07441230869217,4.47689945401876,
61.0727071934208));
#198866=CARTESIAN_POINT('Ctrl Pts',(-5.19746344226367,4.33742520555575,
61.0814561931971));
#198867=CARTESIAN_POINT('Ctrl Pts',(-5.31476088454696,4.19287495491425,
61.0902051929735));
#198868=CARTESIAN_POINT('Ctrl Pts',(-5.42590627628765,4.04373961586825,
61.0989541927498));
#198869=CARTESIAN_POINT('Ctrl Pts',(-5.53706380672587,3.89458798906849,
61.1077041480445));
#198870=CARTESIAN_POINT('Ctrl Pts',(-5.64206777071792,3.74085050155394,
61.1164541033392));
#198871=CARTESIAN_POINT('Ctrl Pts',(-5.74056148163943,3.58304938223265,
61.1252040586339));
#198872=CARTESIAN_POINT('Ctrl Pts',(-5.83905138951818,3.42525435593393,
61.133953676075));
#198873=CARTESIAN_POINT('Ctrl Pts',(-5.93103139557587,3.26339625497302,
61.1427032935161));
#198874=CARTESIAN_POINT('Ctrl Pts',(-6.01618907820782,3.0980248506513,61.1514529109573));
#198875=CARTESIAN_POINT('Ctrl Pts',(-6.10134392544923,2.93265895249767,
61.1602022370731));
#198876=CARTESIAN_POINT('Ctrl Pts',(-6.17967677261775,2.76378023986162,
61.168951563189));
#198877=CARTESIAN_POINT('Ctrl Pts',(-6.25092157009171,2.59196229227244,
61.1777008893049));
#198878=CARTESIAN_POINT('Ctrl Pts',(-6.32216437407705,2.42014915229216,
61.1864499706073));
#198879=CARTESIAN_POINT('Ctrl Pts',(-6.38631941548879,2.24539720662972,
61.1951990519098));
#198880=CARTESIAN_POINT('Ctrl Pts',(-6.443168810375,2.06829994947804,61.2039481332122));
#198881=CARTESIAN_POINT('Ctrl Pts',(-6.50002334524539,1.89118668024562,
61.2126980055546));
#198882=CARTESIAN_POINT('Ctrl Pts',(-6.54957082411068,1.71172794807809,
61.2214478778969));
#198883=CARTESIAN_POINT('Ctrl Pts',(-6.5916429429606,1.5305333425044,61.2301977502393));
#198884=CARTESIAN_POINT('Ctrl Pts',(-6.63371214082117,1.34935131693687,
61.2389470150942));
#198885=CARTESIAN_POINT('Ctrl Pts',(-6.66830695239677,1.16643393829838,
61.2476962799491));
#198886=CARTESIAN_POINT('Ctrl Pts',(-6.69530988153979,0.982402458341598,
61.256445544804));
#198887=CARTESIAN_POINT('Ctrl Pts',(-6.72231419690476,0.798361530947682,
61.265195258811));
#198888=CARTESIAN_POINT('Ctrl Pts',(-6.74172580829272,0.613206671363114,
61.2739449728181));
#198889=CARTESIAN_POINT('Ctrl Pts',(-6.75347878028175,0.42756679511405,
61.2826946868251));
#198890=CARTESIAN_POINT('Ctrl Pts',(-6.76248992368214,0.285234494205772,
61.2894031966134));
#198891=CARTESIAN_POINT('Ctrl Pts',(-6.76699999999997,0.142617266092478,
61.2961117064016));
#198892=CARTESIAN_POINT('Ctrl Pts',(-6.767,1.6338561345563E-12,61.3028202161899));
#198893=CARTESIAN_POINT('Ctrl Pts',(-6.76699986576577,-0.00134785983437084,
61.3028202161899));
#198894=CARTESIAN_POINT('Ctrl Pts',(-6.76696237706181,-0.189561832946977,
61.3116407746007));
#198895=CARTESIAN_POINT('Ctrl Pts',(-6.759067555259,-0.377645677084734,
61.3204613330115));
#198896=CARTESIAN_POINT('Ctrl Pts',(-6.74337774695477,-0.564929696400553,
61.3292818914223));
#198897=CARTESIAN_POINT('Ctrl Pts',(-6.72825252948937,-0.7454743827994,
61.3377850459251));
#198898=CARTESIAN_POINT('Ctrl Pts',(-6.70588363470456,-0.9252754993788,
61.3462882004278));
#198899=CARTESIAN_POINT('Ctrl Pts',(-6.67637932502589,-1.10374277273595,
61.3547913549306));
#198900=CARTESIAN_POINT('Ctrl Pts',(-6.64684860413504,-1.28236980367006,
61.3633021211558));
#198901=CARTESIAN_POINT('Ctrl Pts',(-6.61016978531227,-1.45966029532048,
61.3718128873811));
#198902=CARTESIAN_POINT('Ctrl Pts',(-6.56650166905042,-1.6350366449588,
61.3803236536064));
#198903=CARTESIAN_POINT('Ctrl Pts',(-6.5227698219134,-1.81066894537313,
61.3888468407608));
#198904=CARTESIAN_POINT('Ctrl Pts',(-6.47202838418072,-1.98438121467708,
61.3973700279153));
#198905=CARTESIAN_POINT('Ctrl Pts',(-6.41448557730058,-2.1556121586693,
61.4058932150697));
#198906=CARTESIAN_POINT('Ctrl Pts',(-6.4082435225972,-2.17418672910234,
61.4068177824196));
#198907=CARTESIAN_POINT('Ctrl Pts',(-6.4019214808727,-2.1927321220714,61.4077423497696));
#198908=CARTESIAN_POINT('Ctrl Pts',(-6.39551975129775,-2.21124763668847,
61.4086669171195));
#198909=CARTESIAN_POINT('Ctrl Pts',(-6.33707951056536,-2.3802724476926,
61.4171071265771));
#198910=CARTESIAN_POINT('Ctrl Pts',(-6.27189122696682,-2.54710435637577,
61.4255473360348));
#198911=CARTESIAN_POINT('Ctrl Pts',(-6.20014143025623,-2.7111870545612,
61.4339875454924));
#198912=CARTESIAN_POINT('Ctrl Pts',(-6.12844599464654,-2.87514543579355,
61.4424213602409));
#198913=CARTESIAN_POINT('Ctrl Pts',(-6.05019908904357,-3.03635845426718,
61.4508551749895));
#198914=CARTESIAN_POINT('Ctrl Pts',(-5.96563598925893,-3.19428806522809,
61.459288989738));
#198915=CARTESIAN_POINT('Ctrl Pts',(-5.88112395892767,-3.35212229914009,
61.4677177111265));
#198916=CARTESIAN_POINT('Ctrl Pts',(-5.79030349615835,-3.50667678551837,
61.4761464325151));
#198917=CARTESIAN_POINT('Ctrl Pts',(-5.69345678670816,-3.65743609894784,
61.4845751539036));
#198918=CARTESIAN_POINT('Ctrl Pts',(-5.59665369346201,-3.80812751591481,
61.4930000793053));
#198919=CARTESIAN_POINT('Ctrl Pts',(-5.49382994488778,-3.95502688778638,
61.5014250047071));
#198920=CARTESIAN_POINT('Ctrl Pts',(-5.38531240739392,-4.0976455770075,
61.5098499301088));
#198921=CARTESIAN_POINT('Ctrl Pts',(-5.27682709241016,-4.24022191793856,
61.5182723538665));
#198922=CARTESIAN_POINT('Ctrl Pts',(-5.16265156180884,-4.37851984591891,
61.5266947776243));
#198923=CARTESIAN_POINT('Ctrl Pts',(-5.04315475927423,-4.51208145693422,
61.5351172013821));
#198924=CARTESIAN_POINT('Ctrl Pts',(-4.92365607739932,-4.64564516848874,
61.5435397576003));
#198925=CARTESIAN_POINT('Ctrl Pts',(-4.79883617372676,-4.77447216134442,
61.5519623138185));
#198926=CARTESIAN_POINT('Ctrl Pts',(-4.66910331208577,-4.89813875477918,
61.5603848700367));
#198927=CARTESIAN_POINT('Ctrl Pts',(-4.53936606804406,-5.02180952569497,
61.5688077107704));
#198928=CARTESIAN_POINT('Ctrl Pts',(-4.40471577645939,-5.14031931932873,
61.5772305515042));
#198929=CARTESIAN_POINT('Ctrl Pts',(-4.26559659618971,-5.253282276689,61.5856533922379));
#198930=CARTESIAN_POINT('Ctrl Pts',(-4.12645329387145,-5.36626482083765,
61.5940776934186));
#198931=CARTESIAN_POINT('Ctrl Pts',(-3.98283981695724,-5.47369840096132,
61.6025019945992));
#198932=CARTESIAN_POINT('Ctrl Pts',(-3.83523262147287,-5.57523808811699,
61.6109262957798));
#198933=CARTESIAN_POINT('Ctrl Pts',(-3.68757921828049,-5.67680956177331,
61.6193532341466));
#198934=CARTESIAN_POINT('Ctrl Pts',(-3.53592987864075,-5.77248327495003,
61.6277801725134));
#198935=CARTESIAN_POINT('Ctrl Pts',(-3.38078948463484,-5.86195798864019,
61.6362071108802));
#198936=CARTESIAN_POINT('Ctrl Pts',(-3.22550959991312,-5.95151315134518,
61.6446416261238));
#198937=CARTESIAN_POINT('Ctrl Pts',(-3.06673267804151,-6.03485801066074,
61.6530761413674));
#198938=CARTESIAN_POINT('Ctrl Pts',(-2.90498863006585,-6.11173707379401,
61.6615106566111));
#198939=CARTESIAN_POINT('Ctrl Pts',(-2.74316645832919,-6.18865327017347,
61.6699492457979));
#198940=CARTESIAN_POINT('Ctrl Pts',(-2.57837460676043,-6.25909730608732,
61.6783878349847));
#198941=CARTESIAN_POINT('Ctrl Pts',(-2.41116284016113,-6.32286191200046,
61.6868264241714));
#198942=CARTESIAN_POINT('Ctrl Pts',(-2.24376416863754,-6.38669779231661,
61.6952744457917));
#198943=CARTESIAN_POINT('Ctrl Pts',(-2.07394049172099,-6.44383921289698,
61.7037224674121));
#198944=CARTESIAN_POINT('Ctrl Pts',(-1.90225776955778,-6.49412845408505,
61.7121704890324));
#198945=CARTESIAN_POINT('Ctrl Pts',(-1.80467606550361,-6.5227120517173,
61.7169722089446));
#198946=CARTESIAN_POINT('Ctrl Pts',(-1.70649401278955,-6.54908290613419,
61.7217739288568));
#198947=CARTESIAN_POINT('Ctrl Pts',(-1.60781698503205,-6.57321941993742,
61.726575648769));
#198948=CARTESIAN_POINT('Ctrl Pts',(-1.43849171658337,-6.6146365741832,
61.7348151806199));
#198949=CARTESIAN_POINT('Ctrl Pts',(-1.2673304742322,-6.64956423790568,
61.7430547124707));
#198950=CARTESIAN_POINT('Ctrl Pts',(-1.09487015751772,-6.67784009528359,
61.7512942443215));
#198951=CARTESIAN_POINT('Ctrl Pts',(-0.922601259701609,-6.706084568436,
61.7595246308678));
#198952=CARTESIAN_POINT('Ctrl Pts',(-0.749036506673693,-6.72769187903942,
61.7677550174141));
#198953=CARTESIAN_POINT('Ctrl Pts',(-0.574726585545867,-6.74254984051781,
61.7759854039605));
#198954=CARTESIAN_POINT('Ctrl Pts',(-0.400579040960036,-6.75739396122117,
61.7842081235783));
#198955=CARTESIAN_POINT('Ctrl Pts',(-0.225688063228557,-6.76550122398285,
61.7924308431961));
#198956=CARTESIAN_POINT('Ctrl Pts',(-0.0506132254557434,-6.76681071860363,
61.8006535628139));
#198957=CARTESIAN_POINT('Ctrl Pts',(0.124306483397012,-6.76811905291783,
61.8088689965097));
#198958=CARTESIAN_POINT('Ctrl Pts',(0.299409373049765,-6.76264162146797,
61.8170844302054));
#198959=CARTESIAN_POINT('Ctrl Pts',(0.474132201514215,-6.75036944585163,
61.8252998639012));
#198960=CARTESIAN_POINT('Ctrl Pts',(0.648765236012361,-6.73810357718061,
61.833511075502));
#198961=CARTESIAN_POINT('Ctrl Pts',(0.823018244159236,-6.71904994378684,
61.8417222871029));
#198962=CARTESIAN_POINT('Ctrl Pts',(0.996329019139121,-6.69325163770355,
61.8499334987037));
#198963=CARTESIAN_POINT('Ctrl Pts',(1.16958167524828,-6.66746198294859,
61.8581419567172));
#198964=CARTESIAN_POINT('Ctrl Pts',(1.3418923759856,-6.63493221353315,61.8663504147307));
#198965=CARTESIAN_POINT('Ctrl Pts',(1.51270497212881,-6.59575717164427,
61.8745588727443));
#198966=CARTESIAN_POINT('Ctrl Pts',(1.58880571353783,-6.57830383506496,
61.8782159200274));
#198967=CARTESIAN_POINT('Ctrl Pts',(1.66460920161152,-6.55953216383277,
61.8818729673106));
#198968=CARTESIAN_POINT('Ctrl Pts',(1.74006688801004,-6.53945381704398,
61.8855300145937));
#198969=CARTESIAN_POINT('Ctrl Pts',(1.9228605981222,-6.49081469653002,61.8943890887696));
#198970=CARTESIAN_POINT('Ctrl Pts',(2.10343416063342,-6.43455494400628,
61.9032481629455));
#198971=CARTESIAN_POINT('Ctrl Pts',(2.28117865088128,-6.37091147032852,
61.9121072371214));
#198972=CARTESIAN_POINT('Ctrl Pts',(2.45925708726672,-6.30714842336785,
61.9209829557153));
#198973=CARTESIAN_POINT('Ctrl Pts',(2.63449558509462,-6.23597401919902,
61.9298586743092));
#198974=CARTESIAN_POINT('Ctrl Pts',(2.80630617645485,-6.15767282696892,
61.9387343929031));
#198975=CARTESIAN_POINT('Ctrl Pts',(2.97860706669801,-6.07914818526007,
61.9476354402901));
#198976=CARTESIAN_POINT('Ctrl Pts',(3.14746023740388,-5.99345616483172,
61.9565364876771));
#198977=CARTESIAN_POINT('Ctrl Pts',(3.3123005496344,-5.9009282379039,61.9654375350641));
#198978=CARTESIAN_POINT('Ctrl Pts',(3.47736496453052,-5.80827451799022,
61.9743506835471));
#198979=CARTESIAN_POINT('Ctrl Pts',(3.63840540035195,-5.7087664597678,61.9832638320301));
#198980=CARTESIAN_POINT('Ctrl Pts',(3.79488549142437,-5.60277905212911,
61.9921769805131));
#198981=CARTESIAN_POINT('Ctrl Pts',(3.95171301108731,-5.49655632346399,
62.0011099186229));
#198982=CARTESIAN_POINT('Ctrl Pts',(4.10395971820272,-5.38382561686846,
62.0100428567328));
#198983=CARTESIAN_POINT('Ctrl Pts',(4.25111985689851,-5.26500417495401,
62.0189757948427));
#198984=CARTESIAN_POINT('Ctrl Pts',(4.39119497160725,-5.15190339064156,
62.0274786567013));
#198985=CARTESIAN_POINT('Ctrl Pts',(4.52666163290563,-5.03328466039966,
62.0359815185599));
#198986=CARTESIAN_POINT('Ctrl Pts',(4.65711466349043,-4.90953887968131,
62.0444843804185));
#198987=CARTESIAN_POINT('Ctrl Pts',(4.78326974701439,-4.7898700668352,62.0527071042844));
#198988=CARTESIAN_POINT('Ctrl Pts',(4.90497722864513,-4.66517639283559,
62.0609298281503));
#198989=CARTESIAN_POINT('Ctrl Pts',(5.02181355715097,-4.53582160112307,
62.0691525520162));
#198990=CARTESIAN_POINT('Ctrl Pts',(5.13852621836105,-4.40660372707556,
62.0773665724074));
#198991=CARTESIAN_POINT('Ctrl Pts',(5.25037775515071,-4.27273482376444,
62.0855805927986));
#198992=CARTESIAN_POINT('Ctrl Pts',(5.35697957741249,-4.13461712945534,
62.0937946131898));
#198993=CARTESIAN_POINT('Ctrl Pts',(5.46348996788871,-3.99661789791863,
62.1020015884618));
#198994=CARTESIAN_POINT('Ctrl Pts',(5.56475939331671,-3.85437741541928,
62.1102085637338));
#198995=CARTESIAN_POINT('Ctrl Pts',(5.66043781350638,-3.70833288142086,
62.1184155390057));
#198996=CARTESIAN_POINT('Ctrl Pts',(5.75605337488338,-3.56238429576674,
62.1266171224587));
#198997=CARTESIAN_POINT('Ctrl Pts',(5.84608505167637,-3.41263693567997,
62.1348187059117));
#198998=CARTESIAN_POINT('Ctrl Pts',(5.93022457683854,-3.25955909108275,
62.1430202893647));
#198999=CARTESIAN_POINT('Ctrl Pts',(6.01432570856698,-3.10655109694012,
62.1512181303798));
#199000=CARTESIAN_POINT('Ctrl Pts',(6.09253987263445,-2.95021595966294,
62.1594159713948));
#199001=CARTESIAN_POINT('Ctrl Pts',(6.16460340125909,-2.79104888978764,
62.1676138124099));
#199002=CARTESIAN_POINT('Ctrl Pts',(6.23666057050211,-2.63189586590981,
62.175810929991));
#199003=CARTESIAN_POINT('Ctrl Pts',(6.30256802977629,-2.46991173022405,
62.1840080475722));
#199004=CARTESIAN_POINT('Ctrl Pts',(6.3621090071535,-2.30561444762482,62.1922051651534));
#199005=CARTESIAN_POINT('Ctrl Pts',(6.42164932207101,-2.14131899301588,
62.2004021915324));
#199006=CARTESIAN_POINT('Ctrl Pts',(6.47482317290785,-1.97471077975065,
62.2085992179115));
#199007=CARTESIAN_POINT('Ctrl Pts',(6.52146275381584,-1.80632570445994,
62.2167962442906));
#199008=CARTESIAN_POINT('Ctrl Pts',(6.56811029629741,-1.6379118851252,62.2249946699368));
#199009=CARTESIAN_POINT('Ctrl Pts',(6.60822125080081,-1.46772094528846,
62.2331930955829));
#199010=CARTESIAN_POINT('Ctrl Pts',(6.64167828662358,-1.2963018695477,62.241391521229));
#199011=CARTESIAN_POINT('Ctrl Pts',(6.6751471172736,-1.12482236232115,62.2495928371197));
#199012=CARTESIAN_POINT('Ctrl Pts',(6.70195728778965,-0.952114208696751,
62.2577941530104));
#199013=CARTESIAN_POINT('Ctrl Pts',(6.7220429603744,-0.778734511166019,
62.265995468901));
#199014=CARTESIAN_POINT('Ctrl Pts',(6.74215150717799,-0.605157363182644,
62.2742061247176));
#199015=CARTESIAN_POINT('Ctrl Pts',(6.75552021523821,-0.430907500224963,
62.2824167805342));
#199016=CARTESIAN_POINT('Ctrl Pts',(6.76213524652309,-0.256546112288071,
62.2906274363508));
#199017=CARTESIAN_POINT('Ctrl Pts',(6.76875417588565,-0.0820819774095412,
62.2988429305079));
#199018=CARTESIAN_POINT('Ctrl Pts',(6.76861149569004,0.0924934552098535,
62.3070584246651));
#199019=CARTESIAN_POINT('Ctrl Pts',(6.76174549413847,0.266621215393907,
62.3152739188222));
#199020=CARTESIAN_POINT('Ctrl Pts',(6.75486883985914,0.441019138002136,
62.3235021594698));
#199021=CARTESIAN_POINT('Ctrl Pts',(6.74124804625857,0.614967642646063,
62.3317304001173));
#199022=CARTESIAN_POINT('Ctrl Pts',(6.72097321320831,0.787913743588968,
62.3399586407648));
#199023=CARTESIAN_POINT('Ctrl Pts',(6.7025466268647,0.945094138313558,62.3474367978658));
#199024=CARTESIAN_POINT('Ctrl Pts',(6.67862454825568,1.10144647497973,62.3549149549669));
#199025=CARTESIAN_POINT('Ctrl Pts',(6.64931066512028,1.25656542954104,62.3623931120679));
#199026=CARTESIAN_POINT('Ctrl Pts',(6.6176772789028,1.42395839404954,62.3704629890842));
#199027=CARTESIAN_POINT('Ctrl Pts',(6.57966065066864,1.59046289650428,62.3785328661005));
#199028=CARTESIAN_POINT('Ctrl Pts',(6.53531647488157,1.75554195994901,62.3866027431168));
#199029=CARTESIAN_POINT('Ctrl Pts',(6.4910282548947,1.92041271799784,62.3946624371402));
#199030=CARTESIAN_POINT('Ctrl Pts',(6.44042847067859,2.08386126021791,62.4027221311636));
#199031=CARTESIAN_POINT('Ctrl Pts',(6.38362437276625,2.2453571803668,62.410781825187));
#199032=CARTESIAN_POINT('Ctrl Pts',(6.32687948517417,2.40668476362619,62.4188331181077));
#199033=CARTESIAN_POINT('Ctrl Pts',(6.26394327721674,2.56606342631572,62.4268844110283));
#199034=CARTESIAN_POINT('Ctrl Pts',(6.19497368113208,2.72297449310141,62.434935703949));
#199035=CARTESIAN_POINT('Ctrl Pts',(6.12606086135194,2.87975638948426,62.4429803689831));
#199036=CARTESIAN_POINT('Ctrl Pts',(6.05112468911279,3.03407439342175,62.4510250340171));
#199037=CARTESIAN_POINT('Ctrl Pts',(5.97037237837069,3.18542660621593,62.4590696990512));
#199038=CARTESIAN_POINT('Ctrl Pts',(5.88966799418435,3.3366889913606,62.4671095895707));
#199039=CARTESIAN_POINT('Ctrl Pts',(5.80315451859122,3.48498876107766,62.4751494800902));
#199040=CARTESIAN_POINT('Ctrl Pts',(5.71108654476726,3.62984565486997,62.4831893706097));
#199041=CARTESIAN_POINT('Ctrl Pts',(5.61904760808922,3.7746568625177,62.4912267254431));
#199042=CARTESIAN_POINT('Ctrl Pts',(5.52145785861991,3.91602703986738,62.4992640802766));
#199043=CARTESIAN_POINT('Ctrl Pts',(5.41861692502185,4.05350214257582,62.50730143511));
#199044=CARTESIAN_POINT('Ctrl Pts',(5.31578805542593,4.19096111843793,62.5153378471023));
#199045=CARTESIAN_POINT('Ctrl Pts',(5.20770945131625,4.32452563004555,62.5233742590946));
#199046=CARTESIAN_POINT('Ctrl Pts',(5.09472290864114,4.45377227574191,62.5314106710869));
#199047=CARTESIAN_POINT('Ctrl Pts',(4.98172723908565,4.58302936178492,62.5394477322483));
#199048=CARTESIAN_POINT('Ctrl Pts',(4.86382308829119,4.70796760708525,62.5474847934097));
#199049=CARTESIAN_POINT('Ctrl Pts',(4.74139110618502,4.8281983573782,62.555521854571));
#199050=CARTESIAN_POINT('Ctrl Pts',(4.61886417636146,4.94852234830244,62.5635651485859));
#199051=CARTESIAN_POINT('Ctrl Pts',(4.49180266700234,5.06413128877575,62.5716084426008));
#199052=CARTESIAN_POINT('Ctrl Pts',(4.36062298791606,5.17467449771075,62.5796517366157));
#199053=CARTESIAN_POINT('Ctrl Pts',(4.22939315943916,5.28525996680834,62.5876981055451));
#199054=CARTESIAN_POINT('Ctrl Pts',(4.0940423186118,5.39077561596903,62.5957444744745));
#199055=CARTESIAN_POINT('Ctrl Pts',(3.95501784946542,5.49091274838801,62.6037908434039));
#199056=CARTESIAN_POINT('Ctrl Pts',(3.81581422947476,5.59117892033454,62.6118475811108));
#199057=CARTESIAN_POINT('Ctrl Pts',(3.67292783343855,5.68605252033276,62.6199043188176));
#199058=CARTESIAN_POINT('Ctrl Pts',(3.52683359618341,5.77526915258778,62.6279610565245));
#199059=CARTESIAN_POINT('Ctrl Pts',(3.38704947209315,5.86063233342477,62.6356698070169));
#199060=CARTESIAN_POINT('Ctrl Pts',(3.24432906216674,5.94081685794192,62.6433785575093));
#199061=CARTESIAN_POINT('Ctrl Pts',(3.09910619832141,6.01563211736936,62.6510873080018));
#199062=CARTESIAN_POINT('Origin',(0.,0.,4.30282021618968));
#199063=CARTESIAN_POINT('',(3.09910619832142,6.01563211736936,65.0458684084508));
#199064=CARTESIAN_POINT('',(3.09910619832139,6.01563211736938,64.6516994535812));
#199065=CARTESIAN_POINT('',(3.09910619832133,6.0156321173694,4.30282021618968));
#199066=CARTESIAN_POINT('',(-6.7669979781149,0.00523107913431084,63.6971797837701));
#199067=CARTESIAN_POINT('Ctrl Pts',(-6.76699797811555,0.00523107828453301,
63.69717978381));
#199068=CARTESIAN_POINT('Ctrl Pts',(-6.76713328191249,-0.169799856163699,
63.7053954717453));
#199069=CARTESIAN_POINT('Ctrl Pts',(-6.76047344531109,-0.344918086105988,
63.7136111596805));
#199070=CARTESIAN_POINT('Ctrl Pts',(-6.74702499707155,-0.519560091704129,
63.7218268476158));
#199071=CARTESIAN_POINT('Ctrl Pts',(-6.73301302667077,-0.70152001522752,
63.7303867925343));
#199072=CARTESIAN_POINT('Ctrl Pts',(-6.71163121841307,-0.882962538116192,
63.7389467374529));
#199073=CARTESIAN_POINT('Ctrl Pts',(-6.6829470971477,-1.06325307275606,
63.7475066823715));
#199074=CARTESIAN_POINT('Ctrl Pts',(-6.65542018410509,-1.23627011669901,
63.7557212920241));
#199075=CARTESIAN_POINT('Ctrl Pts',(-6.62116869467487,-1.40822592771657,
63.7639359016767));
#199076=CARTESIAN_POINT('Ctrl Pts',(-6.58030494640585,-1.57856764578107,
63.7721505113294));
#199077=CARTESIAN_POINT('Ctrl Pts',(-6.53943488854242,-1.74893566557253,
63.7803663893643));
#199078=CARTESIAN_POINT('Ctrl Pts',(-6.49195062043139,-1.91768874898435,
63.7885822673992));
#199079=CARTESIAN_POINT('Ctrl Pts',(-6.43801499756835,-2.08428690229655,
63.7967981454341));
#199080=CARTESIAN_POINT('Ctrl Pts',(-6.38406140330354,-2.2509405662748,
63.8050167610075));
#199081=CARTESIAN_POINT('Ctrl Pts',(-6.32365228135544,-2.41543753051153,
63.813235376581));
#199082=CARTESIAN_POINT('Ctrl Pts',(-6.25699953357942,-2.57725548535394,
63.8214539921544));
#199083=CARTESIAN_POINT('Ctrl Pts',(-6.19031265947404,-2.73915629128662,
63.8296768156741));
#199084=CARTESIAN_POINT('Ctrl Pts',(-6.11737592623212,-2.8983750258755,
63.8378996391938));
#199085=CARTESIAN_POINT('Ctrl Pts',(-6.03844831996388,-3.05441170884433,
63.8461224627135));
#199086=CARTESIAN_POINT('Ctrl Pts',(-5.95942328610895,-3.21064100220864,
63.8543554364188));
#199087=CARTESIAN_POINT('Ctrl Pts',(-5.87439277112278,-3.36368008137496,
63.8625884101241));
#199088=CARTESIAN_POINT('Ctrl Pts',(-5.78366093910566,-3.51305495850314,
63.8708213838294));
#199089=CARTESIAN_POINT('Ctrl Pts',(-5.69286329287895,-3.66253818778569,
63.8790603294923));
#199090=CARTESIAN_POINT('Ctrl Pts',(-5.59635628255329,-3.80835162114177,
63.8872992751553));
#199091=CARTESIAN_POINT('Ctrl Pts',(-5.49448584051031,-3.95005244882036,
63.8955382208182));
#199092=CARTESIAN_POINT('Ctrl Pts',(-5.3924709029499,-4.09195426840597,
63.9037888528024));
#199093=CARTESIAN_POINT('Ctrl Pts',(-5.28507755990454,-4.22973155355144,
63.9120394847866));
#199094=CARTESIAN_POINT('Ctrl Pts',(-5.17269082950643,-4.36297588605989,
63.9202901167709));
#199095=CARTESIAN_POINT('Ctrl Pts',(-5.14101877497245,-4.40052588640781,
63.9226152530678));
#199096=CARTESIAN_POINT('Ctrl Pts',(-5.10895036825335,-4.4377161192415,
63.9249403893648));
#199097=CARTESIAN_POINT('Ctrl Pts',(-5.07649472080399,-4.47453800404569,
63.9272655256617));
#199098=CARTESIAN_POINT('Ctrl Pts',(-4.96385846131697,-4.60232714700078,
63.9353348348842));
#199099=CARTESIAN_POINT('Ctrl Pts',(-4.84618732405444,-4.72609466676973,
63.9434041441068));
#199100=CARTESIAN_POINT('Ctrl Pts',(-4.72380322017864,-4.84540732416068,
63.9514734533293));
#199101=CARTESIAN_POINT('Ctrl Pts',(-4.60157176254317,-4.96457116623986,
63.95953269793));
#199102=CARTESIAN_POINT('Ctrl Pts',(-4.47463929844225,-5.0792909445658,
63.9675919425308));
#199103=CARTESIAN_POINT('Ctrl Pts',(-4.34336872409291,-5.18916535933974,
63.9756511871316));
#199104=CARTESIAN_POINT('Ctrl Pts',(-4.21223307271646,-5.29892684261506,
63.9837021482519));
#199105=CARTESIAN_POINT('Ctrl Pts',(-4.0767684679249,-5.40385263551516,
63.9917531093721));
#199106=CARTESIAN_POINT('Ctrl Pts',(-3.93737541017347,-5.50357737107068,
63.9998040704924));
#199107=CARTESIAN_POINT('Ctrl Pts',(-3.79809508008873,-5.60322145887422,
64.0078485207715));
#199108=CARTESIAN_POINT('Ctrl Pts',(-3.6548929221624,-5.69767264488414,
64.0158929710506));
#199109=CARTESIAN_POINT('Ctrl Pts',(-3.50820326619095,-5.78660512244331,
64.0239374213297));
#199110=CARTESIAN_POINT('Ctrl Pts',(-3.36160012967582,-5.875485146477,64.031977126888));
#199111=CARTESIAN_POINT('Ctrl Pts',(-3.21151390820272,-5.9588527488499,
64.0400168324462));
#199112=CARTESIAN_POINT('Ctrl Pts',(-3.05840863208465,-6.0364249054544,
64.0480565380045));
#199113=CARTESIAN_POINT('Ctrl Pts',(-2.90199866043684,-6.1156714155865,
64.056269776309));
#199114=CARTESIAN_POINT('Ctrl Pts',(-2.74243814764586,-6.18886922066618,
64.0644830146134));
#199115=CARTESIAN_POINT('Ctrl Pts',(-2.58024960638838,-6.25576541829476,
64.0726962529179));
#199116=CARTESIAN_POINT('Ctrl Pts',(-2.42153895868367,-6.32122712583771,
64.080733370466));
#199117=CARTESIAN_POINT('Ctrl Pts',(-2.26031221230842,-6.38065460705794,
64.0887704880142));
#199118=CARTESIAN_POINT('Ctrl Pts',(-2.09707992906674,-6.43385924396124,
64.0968076055624));
#199119=CARTESIAN_POINT('Ctrl Pts',(-1.93383037688703,-6.48706950957693,
64.1048455733865));
#199120=CARTESIAN_POINT('Ctrl Pts',(-1.76857522058572,-6.53405550412845,
64.1128835412106));
#199121=CARTESIAN_POINT('Ctrl Pts',(-1.60184062597471,-6.5746783654394,
64.1209215090347));
#199122=CARTESIAN_POINT('Ctrl Pts',(-1.43505535563428,-6.61531357327708,
64.1289619198425));
#199123=CARTESIAN_POINT('Ctrl Pts',(-1.26679011476239,-6.6495817099803,
64.1370023306502));
#199124=CARTESIAN_POINT('Ctrl Pts',(-1.09758156123894,-6.67739497981273,
64.1450427414579));
#199125=CARTESIAN_POINT('Ctrl Pts',(-0.921977878740528,-6.70625943437602,
64.1533870344457));
#199126=CARTESIAN_POINT('Ctrl Pts',(-0.745358626195725,-6.72817150190247,
64.1617313274335));
#199127=CARTESIAN_POINT('Ctrl Pts',(-0.568328641914355,-6.74309213601444,
64.1700756204213));
#199128=CARTESIAN_POINT('Ctrl Pts',(-0.397444479296954,-6.75749478128549,
64.1781302306368));
#199129=CARTESIAN_POINT('Ctrl Pts',(-0.226177995334895,-6.76538334120345,
64.1861848408523));
#199130=CARTESIAN_POINT('Ctrl Pts',(-0.0550718885309028,-6.7667759004635,
64.1942394510679));
#199131=CARTESIAN_POINT('Ctrl Pts',(0.116163748012738,-6.76816951391058,
64.2023001587371));
#199132=CARTESIAN_POINT('Ctrl Pts',(0.2872383948486,-6.76305734633575,64.2103608664064));
#199133=CARTESIAN_POINT('Ctrl Pts',(0.457615057850005,-6.75150927266111,
64.2184215740756));
#199134=CARTESIAN_POINT('Ctrl Pts',(0.628231941739058,-6.73994491689443,
64.2264936468598));
#199135=CARTESIAN_POINT('Ctrl Pts',(0.798148510376524,-6.7219265893989,
64.2345657196439));
#199136=CARTESIAN_POINT('Ctrl Pts',(0.966837950055704,-6.69757518646354,
64.2426377924281));
#199137=CARTESIAN_POINT('Ctrl Pts',(0.984506887198725,-6.69502456202239,
64.2434832807225));
#199138=CARTESIAN_POINT('Ctrl Pts',(1.00216237568927,-6.69240450255315,
64.2443287690169));
#199139=CARTESIAN_POINT('Ctrl Pts',(1.01980382053253,-6.68971517836352,
64.2451742573113));
#199140=CARTESIAN_POINT('Ctrl Pts',(1.19367350701362,-6.66320986897132,
64.253507179358));
#199141=CARTESIAN_POINT('Ctrl Pts',(1.36673248224403,-6.62988780120963,
64.2618401014047));
#199142=CARTESIAN_POINT('Ctrl Pts',(1.53841403349182,-6.58980813541301,
64.2701730234514));
#199143=CARTESIAN_POINT('Ctrl Pts',(1.70989269877938,-6.5497758340619,64.278496098005));
#199144=CARTESIAN_POINT('Ctrl Pts',(1.87999684680696,-6.50300192152489,
64.2868191725586));
#199145=CARTESIAN_POINT('Ctrl Pts',(2.04816658128681,-6.44959709247794,
64.2951422471122));
#199146=CARTESIAN_POINT('Ctrl Pts',(2.216168448443,-6.39624557222493,64.3034570135582));
#199147=CARTESIAN_POINT('Ctrl Pts',(2.38223941952868,-6.33627642728021,
64.3117717800042));
#199148=CARTESIAN_POINT('Ctrl Pts',(2.54583124403592,-6.26985105699414,
64.3200865464502));
#199149=CARTESIAN_POINT('Ctrl Pts',(2.70928977914283,-6.20347980798093,
64.3283945382897));
#199150=CARTESIAN_POINT('Ctrl Pts',(2.87027287155391,-6.1306629456,64.3367025301292));
#199151=CARTESIAN_POINT('Ctrl Pts',(3.02824864419703,-6.05161128534532,
64.3450105219688));
#199152=CARTESIAN_POINT('Ctrl Pts',(3.18612466549118,-5.97260954103419,
64.3533132678558));
#199153=CARTESIAN_POINT('Ctrl Pts',(3.34099684106431,-5.88738099982339,
64.3616160137429));
#199154=CARTESIAN_POINT('Ctrl Pts',(3.49235424968499,-5.79618415810844,
64.36991875963));
#199155=CARTESIAN_POINT('Ctrl Pts',(3.64364980335661,-5.7050245856362,64.3782181124494));
#199156=CARTESIAN_POINT('Ctrl Pts',(3.79143315461349,-5.60790175193272,
64.3865174652688));
#199157=CARTESIAN_POINT('Ctrl Pts',(3.93521867601476,-5.50511970550547,
64.3948168180883));
#199158=CARTESIAN_POINT('Ctrl Pts',(4.07897361664801,-5.40235951909506,
64.4031144057746));
#199159=CARTESIAN_POINT('Ctrl Pts',(4.21873213849263,-5.29394272004307,
64.411411993461));
#199160=CARTESIAN_POINT('Ctrl Pts',(4.35403806620837,-5.18021635822371,
64.4197095811473));
#199161=CARTESIAN_POINT('Ctrl Pts',(4.48933770112075,-5.066495285586,64.4280067829297));
#199162=CARTESIAN_POINT('Ctrl Pts',(4.62018488836009,-4.9474653662196,64.4363039847121));
#199163=CARTESIAN_POINT('Ctrl Pts',(4.74615684040595,-4.82351368260398,
64.4446011864945));
#199164=CARTESIAN_POINT('Ctrl Pts',(4.87214386623956,-4.69954716694567,
64.4528993811191));
#199165=CARTESIAN_POINT('Ctrl Pts',(4.99325424689754,-4.57065795793107,
64.4611975757436));
#199166=CARTESIAN_POINT('Ctrl Pts',(5.1091022123032,-4.43726983450844,64.4694957703681));
#199167=CARTESIAN_POINT('Ctrl Pts',(5.225031654934,-4.30378789766299,64.4777998012097));
#199168=CARTESIAN_POINT('Ctrl Pts',(5.3356910583431,-4.16580098682759,64.4861038320513));
#199169=CARTESIAN_POINT('Ctrl Pts',(5.44073453503616,-4.02376648418679,
64.4944078628929));
#199170=CARTESIAN_POINT('Ctrl Pts',(5.54581620842777,-3.88168033389254,
64.5027149133086));
#199171=CARTESIAN_POINT('Ctrl Pts',(5.64527768402938,-3.73554394235127,
64.5110219637242));
#199172=CARTESIAN_POINT('Ctrl Pts',(5.73881644959561,-3.58584366054223,
64.5193290141399));
#199173=CARTESIAN_POINT('Ctrl Pts',(5.83245522388936,-3.43598332386606,
64.5276449461946));
#199174=CARTESIAN_POINT('Ctrl Pts',(5.92015845780619,-3.28255178282144,
64.5359608782492));
#199175=CARTESIAN_POINT('Ctrl Pts',(6.00166910580818,-3.12606093101009,
64.5442768103038));
#199176=CARTESIAN_POINT('Ctrl Pts',(6.06311356361502,-3.00809480293999,
64.5505455365228));
#199177=CARTESIAN_POINT('Ctrl Pts',(6.12104004933156,-2.88839075719545,
64.5568142627418));
#199178=CARTESIAN_POINT('Ctrl Pts',(6.17535661332451,-2.76717540070542,
64.5630829889607));
#199179=CARTESIAN_POINT('Ctrl Pts',(6.24857556496458,-2.60377660165715,
64.5715332576841));
#199180=CARTESIAN_POINT('Ctrl Pts',(6.31536746712272,-2.43733129013988,
64.5799835264075));
#199181=CARTESIAN_POINT('Ctrl Pts',(6.37548252872376,-2.26837199902002,
64.5884337951309));
#199182=CARTESIAN_POINT('Ctrl Pts',(6.43554453674333,-2.09956182020709,
64.5968766062054));
#199183=CARTESIAN_POINT('Ctrl Pts',(6.48894133846522,-1.92824239494811,
64.60531941728));
#199184=CARTESIAN_POINT('Ctrl Pts',(6.53547094308591,-1.75496682364076,
64.6137622283545));
#199185=CARTESIAN_POINT('Ctrl Pts',(6.58196581887717,-1.58182058198945,
64.6221987378723));
#199186=CARTESIAN_POINT('Ctrl Pts',(6.62160362934667,-1.40672142396835,
64.63063524739));
#199187=CARTESIAN_POINT('Ctrl Pts',(6.65423188485467,-1.23023860392345,
64.6390717569077));
#199188=CARTESIAN_POINT('Ctrl Pts',(6.68683679309019,-1.05388206683248,
64.647502229649));
#199189=CARTESIAN_POINT('Ctrl Pts',(6.71244209087706,-0.876144167867102,
64.6559327023902));
#199190=CARTESIAN_POINT('Ctrl Pts',(6.73094610410198,-0.697605578872706,
64.6643631751315));
#199191=CARTESIAN_POINT('Ctrl Pts',(6.74944216250176,-0.519143743133937,
64.6727900236353));
#199192=CARTESIAN_POINT('Ctrl Pts',(6.76084298812794,-0.339882232780162,
64.6812168721391));
#199193=CARTESIAN_POINT('Ctrl Pts',(6.76509852362996,-0.160408745334515,
64.689643720643));
#199194=CARTESIAN_POINT('Ctrl Pts',(6.76935274560013,0.0190093450545052,
64.6980679680796));
#199195=CARTESIAN_POINT('Ctrl Pts',(6.76646606787668,0.198638950950581,
64.7064922155163));
#199196=CARTESIAN_POINT('Ctrl Pts',(6.75644048928006,0.3778900829832,64.7149164629529));
#199197=CARTESIAN_POINT('Ctrl Pts',(6.75361566481618,0.428396193734256,
64.7172900935638));
#199198=CARTESIAN_POINT('Ctrl Pts',(6.75022440287827,0.478872257101879,
64.7196637241747));
#199199=CARTESIAN_POINT('Ctrl Pts',(6.74626749549761,0.529305090843154,
64.7220373547856));
#199200=CARTESIAN_POINT('Ctrl Pts',(6.73189975110381,0.712429433805857,
64.7306561357227));
#199201=CARTESIAN_POINT('Ctrl Pts',(6.71007669283438,0.894901562660722,
64.7392749166599));
#199202=CARTESIAN_POINT('Ctrl Pts',(6.6808886211682,1.07611162596884,64.747893697597));
#199203=CARTESIAN_POINT('Ctrl Pts',(6.6516830164047,1.25743054106107,64.7565176557835));
#199204=CARTESIAN_POINT('Ctrl Pts',(6.61510361741735,1.43748557733641,64.76514161397));
#199205=CARTESIAN_POINT('Ctrl Pts',(6.57129186811685,1.61567700485629,64.7737655721564));
#199206=CARTESIAN_POINT('Ctrl Pts',(6.52589734979804,1.80030588067048,64.7827010845276));
#199207=CARTESIAN_POINT('Ctrl Pts',(6.4727382702726,1.98293363628355,64.7916365968987));
#199208=CARTESIAN_POINT('Ctrl Pts',(6.41202819173572,2.16291087851218,64.8005721092699));
#199209=CARTESIAN_POINT('Ctrl Pts',(6.35332534084163,2.33693762117996,64.8092121911645));
#199210=CARTESIAN_POINT('Ctrl Pts',(6.28756296160559,2.5084860426836,64.8178522730591));
#199211=CARTESIAN_POINT('Ctrl Pts',(6.21498321831187,2.67698946507115,64.8264923549537));
#199212=CARTESIAN_POINT('Ctrl Pts',(6.1386808943046,2.85413534831456,64.8355755825631));
#199213=CARTESIAN_POINT('Ctrl Pts',(6.05484368962889,3.02791532052571,64.8446588101726));
#199214=CARTESIAN_POINT('Ctrl Pts',(5.96380790906726,3.19769983327811,64.853742037782));
#199215=CARTESIAN_POINT('Ctrl Pts',(5.87277212850563,3.36748434603051,64.8628252653914));
#199216=CARTESIAN_POINT('Ctrl Pts',(5.77453799868445,3.53327308287001,64.8719084930009));
#199217=CARTESIAN_POINT('Ctrl Pts',(5.66949500109843,3.69447092728038,64.8809917206103));
#199218=CARTESIAN_POINT('Ctrl Pts',(5.56489877199312,3.85498316562754,64.8900363154704));
#199219=CARTESIAN_POINT('Ctrl Pts',(5.45345561315619,4.01109218780394,64.8990809103304));
#199220=CARTESIAN_POINT('Ctrl Pts',(5.3355436438952,4.16224254748441,64.9081255051905));
#199221=CARTESIAN_POINT('Ctrl Pts',(5.21773987742674,4.31325420291703,64.917161800211));
#199222=CARTESIAN_POINT('Ctrl Pts',(5.09347929828821,4.4593160932476,64.9261980952316));
#199223=CARTESIAN_POINT('Ctrl Pts',(4.96318175308897,4.59990389962711,64.9352343902522));
#199224=CARTESIAN_POINT('Ctrl Pts',(4.83311477961333,4.74024292485895,64.9442546948401));
#199225=CARTESIAN_POINT('Ctrl Pts',(4.69703233393514,4.87512703523263,64.953274999428));
#199226=CARTESIAN_POINT('Ctrl Pts',(4.55539258376835,5.00406708665545,64.9622953040159));
#199227=CARTESIAN_POINT('Ctrl Pts',(4.4139312013527,5.13284476313072,64.9713042492825));
#199228=CARTESIAN_POINT('Ctrl Pts',(4.2669266561315,5.2556931592491,64.980313194549));
#199229=CARTESIAN_POINT('Ctrl Pts',(4.11487362009876,5.37216009540067,64.9893221398155));
#199230=CARTESIAN_POINT('Ctrl Pts',(3.96316586432145,5.48836255979612,64.9983106276745));
#199231=CARTESIAN_POINT('Ctrl Pts',(3.80643268948294,5.59821234500969,65.0072991155336));
#199232=CARTESIAN_POINT('Ctrl Pts',(3.64520105873866,5.70129794357132,65.0162876033926));
#199233=CARTESIAN_POINT('Ctrl Pts',(3.50374249300808,5.79174136867774,65.0241737644067));
#199234=CARTESIAN_POINT('Ctrl Pts',(3.35882177251838,5.87697844240007,65.0320599254209));
#199235=CARTESIAN_POINT('Ctrl Pts',(3.21081588693835,5.95675669640655,65.039946086435));
#199236=CARTESIAN_POINT('Ctrl Pts',(3.17376623700652,5.97672722914266,65.0419201937736));
#199237=CARTESIAN_POINT('Ctrl Pts',(3.13652736059032,5.99635365191914,65.0438943011122));
#199238=CARTESIAN_POINT('Ctrl Pts',(3.09910619832142,6.01563211736936,65.0458684084508));
#199239=CARTESIAN_POINT('Ctrl Pts',(3.09910619832125,6.01563211736945,63.0457521963359));
#199240=CARTESIAN_POINT('Ctrl Pts',(2.93989560984711,6.09765350962745,63.0541775957781));
#199241=CARTESIAN_POINT('Ctrl Pts',(2.77736734802791,6.17338115804527,63.0626029952203));
#199242=CARTESIAN_POINT('Ctrl Pts',(2.61204854936917,6.24255487566897,63.0710283946625));
#199243=CARTESIAN_POINT('Ctrl Pts',(2.44678254603495,6.31170650234537,63.0794511034144));
#199244=CARTESIAN_POINT('Ctrl Pts',(2.27872809028716,6.37430824348362,63.0878738121662));
#199245=CARTESIAN_POINT('Ctrl Pts',(2.10843344773471,6.43014754080134,63.0962965209181));
#199246=CARTESIAN_POINT('Ctrl Pts',(1.93814073881744,6.48598620408367,63.104719134033));
#199247=CARTESIAN_POINT('Ctrl Pts',(1.76560820845957,6.53506246626283,63.113141747148));
#199248=CARTESIAN_POINT('Ctrl Pts',(1.59140111308797,6.57721304940492,63.121564360263));
#199249=CARTESIAN_POINT('Ctrl Pts',(1.41719168729634,6.61936419640787,63.1299870860498));
#199250=CARTESIAN_POINT('Ctrl Pts',(1.24130797598144,6.65458940095232,63.1384098118365));
#199251=CARTESIAN_POINT('Ctrl Pts',(1.06432747400704,6.68277607196843,63.1468325376233));
#199252=CARTESIAN_POINT('Ctrl Pts',(0.887319896724574,6.7109670551138,63.1552565519582));
#199253=CARTESIAN_POINT('Ctrl Pts',(0.709215523668136,6.73211730545359,
63.1636805662931));
#199254=CARTESIAN_POINT('Ctrl Pts',(0.530599419496047,6.74616581889524,
63.172104580628));
#199255=CARTESIAN_POINT('Ctrl Pts',(0.351931046830005,6.76021844335836,
63.1805310600852));
#199256=CARTESIAN_POINT('Ctrl Pts',(0.172750976923394,6.76716516146341,
63.1889575395424));
#199257=CARTESIAN_POINT('Ctrl Pts',(-0.0063528875793088,6.76699701794078,
63.1973840189996));
#199258=CARTESIAN_POINT('Ctrl Pts',(-0.185616827994484,6.76682872413816,
63.2058180297091));
#199259=CARTESIAN_POINT('Ctrl Pts',(-0.364804092962102,6.75953286179767,
63.2142520404186));
#199260=CARTESIAN_POINT('Ctrl Pts',(-0.543327885455411,6.74515261568532,
63.2226860511281));
#199261=CARTESIAN_POINT('Ctrl Pts',(-0.721934564639815,6.73076569297822,
63.2311239776587));
#199262=CARTESIAN_POINT('Ctrl Pts',(-0.899876825311956,6.70928786130205,
63.2395619041894));
#199263=CARTESIAN_POINT('Ctrl Pts',(-1.07657472139828,6.6808140124723,63.24799983072));
#199264=CARTESIAN_POINT('Ctrl Pts',(-1.25347601309279,6.6523073876111,63.2564474700839));
#199265=CARTESIAN_POINT('Ctrl Pts',(-1.42912974948983,6.6167887129663,63.2648951094477));
#199266=CARTESIAN_POINT('Ctrl Pts',(-1.60296658039716,6.57440393816275,
63.2733427488116));
#199267=CARTESIAN_POINT('Ctrl Pts',(-1.72715789565616,6.54412369834052,
63.2793778533286));
#199268=CARTESIAN_POINT('Ctrl Pts',(-1.85042214059953,6.51034016194635,
63.2854129578456));
#199269=CARTESIAN_POINT('Ctrl Pts',(-1.97255701527909,6.47312195323657,
63.2914480623626));
#199270=CARTESIAN_POINT('Ctrl Pts',(-2.13930378613897,6.42230914374357,
63.2996875942134));
#199271=CARTESIAN_POINT('Ctrl Pts',(-2.30431693438982,6.36497875493986,
63.3079271260642));
#199272=CARTESIAN_POINT('Ctrl Pts',(-2.46705191850273,6.30126525639193,
63.316166657915));
#199273=CARTESIAN_POINT('Ctrl Pts',(-2.62960627815627,6.23762247537466,
63.3243970444613));
#199274=CARTESIAN_POINT('Ctrl Pts',(-2.78988718005324,6.16761082026071,
63.3326274310076));
#199275=CARTESIAN_POINT('Ctrl Pts',(-2.94736381379206,6.09141490535238,
63.3408578175538));
#199276=CARTESIAN_POINT('Ctrl Pts',(-3.10469375185753,6.01528996993338,
63.3490805371716));
#199277=CARTESIAN_POINT('Ctrl Pts',(-3.25922430568567,5.93299240171641,
63.3573032567893));
#199278=CARTESIAN_POINT('Ctrl Pts',(-3.41044319650045,5.84475544428027,
63.3655259764071));
#199279=CARTESIAN_POINT('Ctrl Pts',(-3.5615280964841,5.75659667114504,63.3737414101029));
#199280=CARTESIAN_POINT('Ctrl Pts',(-3.70930687570434,5.66250917658713,
63.3819568437987));
#199281=CARTESIAN_POINT('Ctrl Pts',(-3.85329060785493,5.56277273411534,
63.3901722774944));
#199282=CARTESIAN_POINT('Ctrl Pts',(-3.99720034354836,5.46308754842986,
63.3983834890953));
#199283=CARTESIAN_POINT('Ctrl Pts',(-4.13731862462951,5.35775939881728,
63.4065947006961));
#199284=CARTESIAN_POINT('Ctrl Pts',(-4.27318399314307,5.24711230685468,
63.414805912297));
#199285=CARTESIAN_POINT('Ctrl Pts',(-4.40900379990856,5.13650231982164,
63.4230143703105));
#199286=CARTESIAN_POINT('Ctrl Pts',(-4.54057325953186,5.02057716818818,
63.4312228283241));
#199287=CARTESIAN_POINT('Ctrl Pts',(-4.66746253781183,4.89970228260077,
63.4394312863376));
#199288=CARTESIAN_POINT('Ctrl Pts',(-4.72399448201461,4.8458498816716,63.4430883336209));
#199289=CARTESIAN_POINT('Ctrl Pts',(-4.77959789758538,4.79101554368635,
63.4467453809042));
#199290=CARTESIAN_POINT('Ctrl Pts',(-4.83423698792236,4.73523407495378,
63.4504024281874));
#199291=CARTESIAN_POINT('Ctrl Pts',(-4.96659834852405,4.60010534106987,
63.4592615023634));
#199292=CARTESIAN_POINT('Ctrl Pts',(-5.09316077763605,4.45955669194881,
63.4681205765393));
#199293=CARTESIAN_POINT('Ctrl Pts',(-5.21352157412158,4.31410266407382,
63.4769796507152));
#199294=CARTESIAN_POINT('Ctrl Pts',(-5.33410850432773,4.16837535734506,
63.4858553693091));
#199295=CARTESIAN_POINT('Ctrl Pts',(-5.44847035155232,4.01772445350142,
63.494731087903));
#199296=CARTESIAN_POINT('Ctrl Pts',(-5.55624676190952,3.86269477447675,
63.5036068064969));
#199297=CARTESIAN_POINT('Ctrl Pts',(-5.66433073569032,3.70722268455082,
63.5125078538839));
#199298=CARTESIAN_POINT('Ctrl Pts',(-5.76579151634374,3.5473470278303,63.5214089012709));
#199299=CARTESIAN_POINT('Ctrl Pts',(-5.86031232171138,3.3836413066396,63.5303099486579));
#199300=CARTESIAN_POINT('Ctrl Pts',(-5.95496162941053,3.21971302527529,
63.5392230971409));
#199301=CARTESIAN_POINT('Ctrl Pts',(-6.04265199088647,3.05194450580542,
63.5481362456239));
#199302=CARTESIAN_POINT('Ctrl Pts',(-6.12311357881597,2.88093198477844,
63.5570493941069));
#199303=CARTESIAN_POINT('Ctrl Pts',(-6.20375381347223,2.70953976919284,
63.5659823322168));
#199304=CARTESIAN_POINT('Ctrl Pts',(-6.27713306111496,2.53488938112438,
63.5749152703266));
#199305=CARTESIAN_POINT('Ctrl Pts',(-6.34302938388745,2.35759776788587,
63.5838482084365));
#199306=CARTESIAN_POINT('Ctrl Pts',(-6.40575312859799,2.18884185829608,
63.592351070295));
#199307=CARTESIAN_POINT('Ctrl Pts',(-6.46169745694369,2.0176932339583,63.6008539321535));
#199308=CARTESIAN_POINT('Ctrl Pts',(-6.51071347235249,1.84469484764495,
63.609356794012));
#199309=CARTESIAN_POINT('Ctrl Pts',(-6.56661490996948,1.64739487497929,
63.6190540775996));
#199310=CARTESIAN_POINT('Ctrl Pts',(-6.61358342331807,1.44741283947396,
63.6287513611871));
#199311=CARTESIAN_POINT('Ctrl Pts',(-6.65139328240953,1.2454944410624,63.6384486447746));
#199312=CARTESIAN_POINT('Ctrl Pts',(-6.68955888603213,1.04167623747579,
63.6482371679405));
#199313=CARTESIAN_POINT('Ctrl Pts',(-6.71839248848192,0.835885082081672,
63.6580256911065));
#199314=CARTESIAN_POINT('Ctrl Pts',(-6.73771199660313,0.628908618823391,
63.6678142142724));
#199315=CARTESIAN_POINT('Ctrl Pts',(-6.75703150472433,0.42193215556511,
63.6776027374383));
#199316=CARTESIAN_POINT('Ctrl Pts',(-6.76683677133875,0.213770445537998,
63.6873912606042));
#199317=CARTESIAN_POINT('Ctrl Pts',(-6.7669979781149,0.00523107913429214,
63.6971797837701));
#199318=CARTESIAN_POINT('',(-6.76699985002101,-0.00142471597195355,63.3028202161558));
#199319=CARTESIAN_POINT('Ctrl Pts',(3.09910619832141,6.01563211736936,62.6510873080018));
#199320=CARTESIAN_POINT('Ctrl Pts',(2.94704750109924,6.09396903057741,62.659158919634));
#199321=CARTESIAN_POINT('Ctrl Pts',(2.79224544225794,6.16641885136224,62.6672305312663));
#199322=CARTESIAN_POINT('Ctrl Pts',(2.63521336584288,6.23281152582709,62.6753021428986));
#199323=CARTESIAN_POINT('Ctrl Pts',(2.60279053890997,6.2465197964106,62.6769687098383));
#199324=CARTESIAN_POINT('Ctrl Pts',(2.57027268699037,6.259970017224,62.678635276778));
#199325=CARTESIAN_POINT('Ctrl Pts',(2.5376643900067,6.27316096108588,62.6803018437177));
#199326=CARTESIAN_POINT('Ctrl Pts',(2.37462119601859,6.33911637176053,62.6886347657644));
#199327=CARTESIAN_POINT('Ctrl Pts',(2.20879568825379,6.39879610100219,62.6969676878111));
#199328=CARTESIAN_POINT('Ctrl Pts',(2.04070539182329,6.45196175622449,62.7053006098578));
#199329=CARTESIAN_POINT('Ctrl Pts',(1.87281373736084,6.50506458253512,62.7136236844114));
#199330=CARTESIAN_POINT('Ctrl Pts',(1.70266295480959,6.55166856592118,62.7219467589651));
#199331=CARTESIAN_POINT('Ctrl Pts',(1.53079101222576,6.59158310854751,62.7302698335187));
#199332=CARTESIAN_POINT('Ctrl Pts',(1.35909063251716,6.63145780840722,62.7385845999646));
#199333=CARTESIAN_POINT('Ctrl Pts',(1.1856728525344,6.66465629283506,62.7468993664106));
#199334=CARTESIAN_POINT('Ctrl Pts',(1.01109150694816,6.69103751032508,62.7552141328566));
#199335=CARTESIAN_POINT('Ctrl Pts',(0.836652404672212,6.71739723324081,
62.7635221246961));
#199336=CARTESIAN_POINT('Ctrl Pts',(0.661051968390811,6.73695070523883,
62.7718301165357));
#199337=CARTESIAN_POINT('Ctrl Pts',(0.484855176277834,6.74960772623392,
62.7801381083752));
#199338=CARTESIAN_POINT('Ctrl Pts',(0.308769640893683,6.7622567551496,62.7884408542623));
#199339=CARTESIAN_POINT('Ctrl Pts',(0.132088846190396,6.76801798651536,
62.7967436001494));
#199340=CARTESIAN_POINT('Ctrl Pts',(-0.0446159123753718,6.7668529184816,
62.8050463460365));
#199341=CARTESIAN_POINT('Ctrl Pts',(-0.221248457337557,6.76568832657402,
62.8133456988559));
#199342=CARTESIAN_POINT('Ctrl Pts',(-0.397904599277771,6.75760307765305,
62.8216450516754));
#199343=CARTESIAN_POINT('Ctrl Pts',(-0.574011542342586,6.74261075172351,
62.8299444044948));
#199344=CARTESIAN_POINT('Ctrl Pts',(-0.750081030415655,6.72762161441013,
62.8382419921812));
#199345=CARTESIAN_POINT('Ctrl Pts',(-0.925601205865563,6.70572835620025,
62.8465395798675));
#199346=CARTESIAN_POINT('Ctrl Pts',(-1.10000265022993,6.67699656803021,
62.8548371675539));
#199347=CARTESIAN_POINT('Ctrl Pts',(-1.27439598353772,6.64826611611721,
62.8631343693363));
#199348=CARTESIAN_POINT('Ctrl Pts',(-1.44767034621451,6.61269782473572,
62.8714315711187));
#199349=CARTESIAN_POINT('Ctrl Pts',(-1.61926459693325,6.57040875175347,
62.8797287729011));
#199350=CARTESIAN_POINT('Ctrl Pts',(-1.79087938059843,6.52811461846607,
62.8880269675257));
#199351=CARTESIAN_POINT('Ctrl Pts',(-1.96081331407444,6.47909818492569,
62.8963251621502));
#199352=CARTESIAN_POINT('Ctrl Pts',(-2.12851835721448,6.42352695977848,
62.9046233567748));
#199353=CARTESIAN_POINT('Ctrl Pts',(-2.29634134926671,6.3679166507407,62.9129273876164));
#199354=CARTESIAN_POINT('Ctrl Pts',(-2.4619319879509,6.30574244785182,62.9212314184579));
#199355=CARTESIAN_POINT('Ctrl Pts',(-2.62475937696367,6.23722111304716,
62.9295354492995));
#199356=CARTESIAN_POINT('Ctrl Pts',(-2.78764597449635,6.16867486199935,
62.9378424997152));
#199357=CARTESIAN_POINT('Ctrl Pts',(-2.94776700192038,6.09377702065205,
62.946149550131));
#199358=CARTESIAN_POINT('Ctrl Pts',(-3.1046140757391,6.01279140173037,62.9544566005467));
#199359=CARTESIAN_POINT('Ctrl Pts',(-3.26162884555125,5.9317191955139,62.9627725326013));
#199360=CARTESIAN_POINT('Ctrl Pts',(-3.41536236199939,5.84454637321634,
62.9710884646559));
#199361=CARTESIAN_POINT('Ctrl Pts',(-3.56533230169483,5.75158191965406,
62.9794043967106));
#199362=CARTESIAN_POINT('Ctrl Pts',(-3.67838282770091,5.68150333993049,
62.9856731229294));
#199363=CARTESIAN_POINT('Ctrl Pts',(-3.78929525749684,5.60813461886252,
62.9919418491483));
#199364=CARTESIAN_POINT('Ctrl Pts',(-3.89787485526575,5.53162368682894,
62.9982105753671));
#199365=CARTESIAN_POINT('Ctrl Pts',(-4.0442405995954,5.42848663579396,63.0066608440905));
#199366=CARTESIAN_POINT('Ctrl Pts',(-4.1866346144784,5.31944928235414,63.0151111128138));
#199367=CARTESIAN_POINT('Ctrl Pts',(-4.32457027994008,5.20484206233571,
63.0235613815371));
#199368=CARTESIAN_POINT('Ctrl Pts',(-4.46238421249748,5.09033598707702,
63.0320041926116));
#199369=CARTESIAN_POINT('Ctrl Pts',(-4.59574738424135,4.97027005382572,
63.0404470036862));
#199370=CARTESIAN_POINT('Ctrl Pts',(-4.72420378140878,4.84501678343047,
63.0488898147607));
#199371=CARTESIAN_POINT('Ctrl Pts',(-4.85256430111656,4.71985699974079,
63.0573263242784));
#199372=CARTESIAN_POINT('Ctrl Pts',(-4.97602511025851,4.58951782771408,
63.0657628337962));
#199373=CARTESIAN_POINT('Ctrl Pts',(-5.09416451673034,4.45441094607194,
63.074199343314));
#199374=CARTESIAN_POINT('Ctrl Pts',(-5.21221938809949,4.31940074067403,
63.0826298160552));
#199375=CARTESIAN_POINT('Ctrl Pts',(-5.32496023423207,4.17962987956021,
63.0910602887964));
#199376=CARTESIAN_POINT('Ctrl Pts',(-5.43200323254407,4.03554579724115,
63.0994907615376));
#199377=CARTESIAN_POINT('Ctrl Pts',(-5.53900021336142,3.89152365627831,
63.1079176100414));
#199378=CARTESIAN_POINT('Ctrl Pts',(-5.64030403212136,3.74319225628524,
63.1163444585452));
#199379=CARTESIAN_POINT('Ctrl Pts',(-5.73557166646664,3.59103141991616,
63.1247713070491));
#199380=CARTESIAN_POINT('Ctrl Pts',(-5.83080989509528,3.43891755016349,
63.1331955544857));
#199381=CARTESIAN_POINT('Ctrl Pts',(-5.92001547912602,3.28297688195782,
63.1416198019224));
#199382=CARTESIAN_POINT('Ctrl Pts',(-6.0028889905621,3.1237177796639,63.150044049359));
#199383=CARTESIAN_POINT('Ctrl Pts',(-6.02623957529533,3.0788446579847,63.15241767997));
#199384=CARTESIAN_POINT('Ctrl Pts',(-6.04908773166963,3.0337082493871,63.1547913105809));
#199385=CARTESIAN_POINT('Ctrl Pts',(-6.07142741218927,2.98832029383009,
63.1571649411919));
#199386=CARTESIAN_POINT('Ctrl Pts',(-6.15179288111495,2.82504023578669,
63.1657039145644));
#199387=CARTESIAN_POINT('Ctrl Pts',(-6.22554386788738,2.65856491521556,
63.1742428879368));
#199388=CARTESIAN_POINT('Ctrl Pts',(-6.29244860583804,2.48945366353481,
63.1827818613093));
#199389=CARTESIAN_POINT('Ctrl Pts',(-6.35938647625348,2.32025866483163,
63.1913250633395));
#199390=CARTESIAN_POINT('Ctrl Pts',(-6.41947121772726,2.14842542445335,
63.1998682653696));
#199391=CARTESIAN_POINT('Ctrl Pts',(-6.47252014396247,1.97453082680419,
63.2084114673998));
#199392=CARTESIAN_POINT('Ctrl Pts',(-6.5256272545327,1.80044550066633,63.2169640396579));
#199393=CARTESIAN_POINT('Ctrl Pts',(-6.57168303404136,1.62429460107207,
63.2255166119159));
#199394=CARTESIAN_POINT('Ctrl Pts',(-6.61055500926353,1.4466690946795,63.234069184174));
#199395=CARTESIAN_POINT('Ctrl Pts',(-6.64944878854188,1.26894395464352,
63.2426265537382));
#199396=CARTESIAN_POINT('Ctrl Pts',(-6.68115066323215,1.08974286753986,
63.2511839233024));
#199397=CARTESIAN_POINT('Ctrl Pts',(-6.70557961935685,0.909665305739452,
63.2597412928667));
#199398=CARTESIAN_POINT('Ctrl Pts',(-6.73003791924544,0.729371436970054,
63.2683089414387));
#199399=CARTESIAN_POINT('Ctrl Pts',(-6.74720580367184,0.548199303442522,
63.2768765900108));
#199400=CARTESIAN_POINT('Ctrl Pts',(-6.75705416573981,0.366753324808809,
63.2854442385829));
#199401=CARTESIAN_POINT('Ctrl Pts',(-6.76371195976512,0.244090292709951,
63.2912362311072));
#199402=CARTESIAN_POINT('Ctrl Pts',(-6.76702568878971,0.121302162455473,
63.2970282236315));
#199403=CARTESIAN_POINT('Ctrl Pts',(-6.76699985002101,-0.00142471597195272,
63.3028202161558));
#199404=CARTESIAN_POINT('Ctrl Pts',(-6.76699985002086,-0.00142471669502992,
63.3028202161899));
#199405=CARTESIAN_POINT('Ctrl Pts',(-6.76698007373462,-0.0953564621888831,
63.3072532464654));
#199406=CARTESIAN_POINT('Ctrl Pts',(-6.76500440002413,-0.189266792552925,
63.311686276741));
#199407=CARTESIAN_POINT('Ctrl Pts',(-6.76107620035431,-0.283085875667693,
63.3161193070166));
#199408=CARTESIAN_POINT('Ctrl Pts',(-6.75306159807707,-0.474502478789027,
63.3251639018765));
#199409=CARTESIAN_POINT('Ctrl Pts',(-6.73691165593163,-0.665627526396733,
63.3342084967363));
#199410=CARTESIAN_POINT('Ctrl Pts',(-6.71266801146048,-0.855790376152495,
63.3432530915961));
#199411=CARTESIAN_POINT('Ctrl Pts',(-6.6884466143493,-1.04577872156024,
63.3522893866164));
#199412=CARTESIAN_POINT('Ctrl Pts',(-6.65614637350505,-1.23480639618576,
63.3613256816367));
#199413=CARTESIAN_POINT('Ctrl Pts',(-6.61586069696472,-1.42220822608981,
63.370361976657));
#199414=CARTESIAN_POINT('Ctrl Pts',(-6.57564630908804,-1.60927843376065,
63.3793822812447));
#199415=CARTESIAN_POINT('Ctrl Pts',(-6.52747475296321,-1.79472830955393,
63.3884025858324));
#199416=CARTESIAN_POINT('Ctrl Pts',(-6.47149034390523,-1.97790336688663,
63.3974228904201));
#199417=CARTESIAN_POINT('Ctrl Pts',(-6.41557643633529,-2.16084775081699,
63.4064318356864));
#199418=CARTESIAN_POINT('Ctrl Pts',(-6.35186937996053,-2.34152280640211,
63.4154407809527));
#199419=CARTESIAN_POINT('Ctrl Pts',(-6.28056374857452,-2.51928720079541,
63.424449726219));
#199420=CARTESIAN_POINT('Ctrl Pts',(-6.20942003718207,-2.69664792988155,
63.4334382140778));
#199421=CARTESIAN_POINT('Ctrl Pts',(-6.1307122811609,-2.87111097051372,
63.4424267019366));
#199422=CARTESIAN_POINT('Ctrl Pts',(-6.04468358232521,-3.04205348236485,
63.4514151897954));
#199423=CARTESIAN_POINT('Ctrl Pts',(-5.96920523918043,-3.19203200978827,
63.4593013508107));
#199424=CARTESIAN_POINT('Ctrl Pts',(-5.88809225212156,-3.33930066668055,
63.467187511826));
#199425=CARTESIAN_POINT('Ctrl Pts',(-5.80153993560371,-3.48344992437029,
63.4750736728414));
#199426=CARTESIAN_POINT('Ctrl Pts',(-5.71240510872753,-3.63190024488659,
63.4831951376975));
#199427=CARTESIAN_POINT('Ctrl Pts',(-5.61754001569764,-3.7769749438643,
63.4913166025537));
#199428=CARTESIAN_POINT('Ctrl Pts',(-5.51724039658921,-3.91820716734633,
63.4994380674098));
#199429=CARTESIAN_POINT('Ctrl Pts',(-5.41694793031973,-4.05942931889232,
63.507558953086));
#199430=CARTESIAN_POINT('Ctrl Pts',(-5.31122192196806,-4.19680924220401,
63.5156798387622));
#199431=CARTESIAN_POINT('Ctrl Pts',(-5.20040081889535,-4.32990996705851,
63.5238007244384));
#199432=CARTESIAN_POINT('Ctrl Pts',(-5.08956646953165,-4.46302660125593,
63.5319225807927));
#199433=CARTESIAN_POINT('Ctrl Pts',(-4.97363604799523,-4.59186273787047,
63.540044437147));
#199434=CARTESIAN_POINT('Ctrl Pts',(-4.85298753256088,-4.71601537410648,
63.5481662935012));
#199435=CARTESIAN_POINT('Ctrl Pts',(-4.73225099346262,-4.84025859056958,
63.5562940754614));
#199436=CARTESIAN_POINT('Ctrl Pts',(-4.60678974079254,-4.95981121904418,
63.5644218574216));
#199437=CARTESIAN_POINT('Ctrl Pts',(-4.47701823570153,-5.07430751109902,
63.5725496393817));
#199438=CARTESIAN_POINT('Ctrl Pts',(-4.34719386652271,-5.18885044468764,
63.5806807322981));
#199439=CARTESIAN_POINT('Ctrl Pts',(-4.21305602853732,-5.29833270478728,
63.5888118252146));
#199440=CARTESIAN_POINT('Ctrl Pts',(-4.07505112596264,-5.40242976083824,
63.596942918131));
#199441=CARTESIAN_POINT('Ctrl Pts',(-3.93689559680428,-5.50664043447546,
63.6050828857956));
#199442=CARTESIAN_POINT('Ctrl Pts',(-3.7948648730645,-5.60545395541145,
63.6132228534601));
#199443=CARTESIAN_POINT('Ctrl Pts',(-3.64943372661247,-5.69858951628063,
63.6213628211247));
#199444=CARTESIAN_POINT('Ctrl Pts',(-3.5740068460226,-5.74689364507099,
63.6255845603051));
#199445=CARTESIAN_POINT('Ctrl Pts',(-3.49766569458399,-5.79367120624689,
63.6298062994856));
#199446=CARTESIAN_POINT('Ctrl Pts',(-3.42047891288538,-5.83888799400249,
63.6340280386661));
#199447=CARTESIAN_POINT('Ctrl Pts',(-3.26616511540881,-5.92928655804038,
63.6424682481237));
#199448=CARTESIAN_POINT('Ctrl Pts',(-3.10815110810223,-6.01363092103054,
63.6509084575814));
#199449=CARTESIAN_POINT('Ctrl Pts',(-2.94694036471961,-6.09161977529673,
63.659348667039));
#199450=CARTESIAN_POINT('Ctrl Pts',(-2.78585176235865,-6.16954954145169,
63.6677824817875));
#199451=CARTESIAN_POINT('Ctrl Pts',(-2.62157155114009,-6.24113325303317,
63.676216296536));
#199452=CARTESIAN_POINT('Ctrl Pts',(-2.45462835877894,-6.30611517657886,
63.6846501112846));
#199453=CARTESIAN_POINT('Ctrl Pts',(-2.28778598696022,-6.37105785615966,
63.6930788326731));
#199454=CARTESIAN_POINT('Ctrl Pts',(-2.11828415023037,-6.42940657561799,
63.7015075540616));
#199455=CARTESIAN_POINT('Ctrl Pts',(-1.94667240273159,-6.48095329071605,
63.7099362754501));
#199456=CARTESIAN_POINT('Ctrl Pts',(-1.77513794286605,-6.53247679106531,
63.7183612008519));
#199457=CARTESIAN_POINT('Ctrl Pts',(-1.60149578573184,-6.57720429930089,
63.7267861262536));
#199458=CARTESIAN_POINT('Ctrl Pts',(-1.42631200754099,-6.61497717737139,
63.7352110516553));
#199459=CARTESIAN_POINT('Ctrl Pts',(-1.25118024731205,-6.65273883940264,
63.7436334754131));
#199460=CARTESIAN_POINT('Ctrl Pts',(-1.074508104543,-6.68354991924383,63.7520558991708));
#199461=CARTESIAN_POINT('Ctrl Pts',(-0.896873633896095,-6.70730248943806,
63.7604783229285));
#199462=CARTESIAN_POINT('Ctrl Pts',(-0.719236369570615,-6.7310554331918,
63.7689008791467));
#199463=CARTESIAN_POINT('Ctrl Pts',(-0.540637076705376,-6.74774959471769,
63.7773234353649));
#199464=CARTESIAN_POINT('Ctrl Pts',(-0.361661424485507,-6.75732861521764,
63.7857459915831));
#199465=CARTESIAN_POINT('Ctrl Pts',(-0.182679726434212,-6.76690795929871,
63.7941688323169));
#199466=CARTESIAN_POINT('Ctrl Pts',(-0.00332197677035101,-6.76937166511965,
63.8025916730506));
#199467=CARTESIAN_POINT('Ctrl Pts',(0.175823482853185,-6.76471544877369,
63.8110145137843));
#199468=CARTESIAN_POINT('Ctrl Pts',(0.355000004732227,-6.76005842508055,
63.8194388149649));
#199469=CARTESIAN_POINT('Ctrl Pts',(0.533963829738483,-6.74827902659319,
63.8278631161456));
#199470=CARTESIAN_POINT('Ctrl Pts',(0.71212869830463,-6.72942506586194,
63.8362874173262));
#199471=CARTESIAN_POINT('Ctrl Pts',(0.89034934050912,-6.71056520299075,
63.844714355693));
#199472=CARTESIAN_POINT('Ctrl Pts',(1.06777019604266,-6.68462639753977,
63.8531412940599));
#199473=CARTESIAN_POINT('Ctrl Pts',(1.24381182296976,-6.6517081376922,63.8615682324267));
#199474=CARTESIAN_POINT('Ctrl Pts',(1.42001173344752,-6.61876028019127,
63.8700027476703));
#199475=CARTESIAN_POINT('Ctrl Pts',(1.5948296092077,-6.57882049040694,63.8784372629139));
#199476=CARTESIAN_POINT('Ctrl Pts',(1.76769674382886,-6.53203928508218,
63.8868717781576));
#199477=CARTESIAN_POINT('Ctrl Pts',(1.94064737475684,-6.48523548403451,
63.8953103673443));
#199478=CARTESIAN_POINT('Ctrl Pts',(2.11164506577398,-6.43158377198406,
63.9037489565311));
#199479=CARTESIAN_POINT('Ctrl Pts',(2.28013738826408,-6.37128421047439,
63.9121875457179));
#199480=CARTESIAN_POINT('Ctrl Pts',(2.44881804705034,-6.31091724769736,
63.9206355673382));
#199481=CARTESIAN_POINT('Ctrl Pts',(2.6149874303068,-6.24388770752694,63.9290835889585));
#199482=CARTESIAN_POINT('Ctrl Pts',(2.7781130291179,-6.17044382499714,63.9375316105788));
#199483=CARTESIAN_POINT('Ctrl Pts',(2.8708310015874,-6.12869950081945,63.942333330491));
#199484=CARTESIAN_POINT('Ctrl Pts',(2.96256607040804,-6.08488381200273,
63.9471350504033));
#199485=CARTESIAN_POINT('Ctrl Pts',(3.05322414153299,-6.03904887722894,
63.9519367703156));
#199486=CARTESIAN_POINT('Ctrl Pts',(3.20878924699882,-5.96039822457744,
63.9601763021664));
#199487=CARTESIAN_POINT('Ctrl Pts',(3.36152890175195,-5.8756237564737,63.9684158340172));
#199488=CARTESIAN_POINT('Ctrl Pts',(3.51092968437654,-5.78495131797699,
63.9766553658681));
#199489=CARTESIAN_POINT('Ctrl Pts',(3.66016464257403,-5.69437951954991,
63.9848857524144));
#199490=CARTESIAN_POINT('Ctrl Pts',(3.80606780616563,-5.5979229686101,63.9931161389607));
#199491=CARTESIAN_POINT('Ctrl Pts',(3.94814787931328,-5.495854558035,64.0013465255071));
#199492=CARTESIAN_POINT('Ctrl Pts',(4.09009559928871,-5.39388122819587,
64.0095692451249));
#199493=CARTESIAN_POINT('Ctrl Pts',(4.2282270339751,-5.28630665614089,64.0177919647427));
#199494=CARTESIAN_POINT('Ctrl Pts',(4.36207748268065,-5.1734484664574,64.0260146843605));
#199495=CARTESIAN_POINT('Ctrl Pts',(4.49580933024509,-5.0606902772611,64.0342301180563));
#199496=CARTESIAN_POINT('Ctrl Pts',(4.62526748109972,-4.94265802998371,
64.0424455517521));
#199497=CARTESIAN_POINT('Ctrl Pts',(4.75001821919929,-4.8197111860852,64.0506609854479));
#199498=CARTESIAN_POINT('Ctrl Pts',(4.87470484510672,-4.69682752731729,
64.0588721970487));
#199499=CARTESIAN_POINT('Ctrl Pts',(4.9946886235279,-4.56903455133817,64.0670834086495));
#199500=CARTESIAN_POINT('Ctrl Pts',(5.10957048674683,-4.4367306027035,64.0752946202503));
#199501=CARTESIAN_POINT('Ctrl Pts',(5.22441382492784,-4.30447102151289,
64.0835030782639));
#199502=CARTESIAN_POINT('Ctrl Pts',(5.33415842307217,-4.16770374960559,
64.0917115362774));
#199503=CARTESIAN_POINT('Ctrl Pts',(5.43844346888631,-4.02686250519282,
64.099919994291));
#199504=CARTESIAN_POINT('Ctrl Pts',(5.48490473394169,-3.9641146554287,64.1035770415741));
#199505=CARTESIAN_POINT('Ctrl Pts',(5.53028285833373,-3.90055861502764,
64.1072340888572));
#199506=CARTESIAN_POINT('Ctrl Pts',(5.57454854343968,-3.83623481252576,
64.1108911361403));
#199507=CARTESIAN_POINT('Ctrl Pts',(5.68178067839527,-3.68041256207988,
64.1197502103162));
#199508=CARTESIAN_POINT('Ctrl Pts',(5.78237046120215,-3.52024494104774,
64.1286092844921));
#199509=CARTESIAN_POINT('Ctrl Pts',(5.87600937643769,-3.3563079131713,64.137468358668));
#199510=CARTESIAN_POINT('Ctrl Pts',(5.96982422035596,-3.19206288060161,
64.1463440772619));
#199511=CARTESIAN_POINT('Ctrl Pts',(6.05666196990865,-3.02403451340599,
64.1552197958559));
#199512=CARTESIAN_POINT('Ctrl Pts',(6.13626102253946,-2.85282135144545,
64.1640955144498));
#199513=CARTESIAN_POINT('Ctrl Pts',(6.21608722837607,-2.68111959549629,
64.1729965618368));
#199514=CARTESIAN_POINT('Ctrl Pts',(6.28863328939886,-2.50621509397389,
64.1818976092238));
#199515=CARTESIAN_POINT('Ctrl Pts',(6.35368544705852,-2.32872717161902,
64.1907986566108));
#199516=CARTESIAN_POINT('Ctrl Pts',(6.41882604401885,-2.15099795199912,
64.1997118050938));
#199517=CARTESIAN_POINT('Ctrl Pts',(6.47645230324947,-1.97067854131893,
64.2086249535769));
#199518=CARTESIAN_POINT('Ctrl Pts',(6.52640062368902,-1.78840261102236,
64.2175381020599));
#199519=CARTESIAN_POINT('Ctrl Pts',(6.57645984305797,-1.60572197831846,
64.2264710401698));
#199520=CARTESIAN_POINT('Ctrl Pts',(6.61880695747251,-1.42107638823298,
64.2354039782797));
#199521=CARTESIAN_POINT('Ctrl Pts',(6.65332909720839,-1.23511170516685,
64.2443369163896));
#199522=CARTESIAN_POINT('Ctrl Pts',(6.68618916873535,-1.05810029064291,
64.2528397782481));
#199523=CARTESIAN_POINT('Ctrl Pts',(6.71195996542605,-0.879893990178444,
64.2613426401067));
#199524=CARTESIAN_POINT('Ctrl Pts',(6.73058789011606,-0.701053245783138,
64.2698455019653));
#199525=CARTESIAN_POINT('Ctrl Pts',(6.74860209327117,-0.528104645466156,
64.2780682258312));
#199526=CARTESIAN_POINT('Ctrl Pts',(6.75996987356229,-0.354231136869663,
64.2862909496971));
#199527=CARTESIAN_POINT('Ctrl Pts',(6.76460601849349,-0.179984484224986,
64.2945136735629));
#199528=CARTESIAN_POINT('Ctrl Pts',(6.76923725622233,-0.00592226575934016,
64.3027276939542));
#199529=CARTESIAN_POINT('Ctrl Pts',(6.76715103770652,0.168511954645426,
64.3109417143454));
#199530=CARTESIAN_POINT('Ctrl Pts',(6.75831374290271,0.342759905024563,
64.3191557347366));
#199531=CARTESIAN_POINT('Ctrl Pts',(6.74948402779712,0.516858403913161,
64.3273627100086));
#199532=CARTESIAN_POINT('Ctrl Pts',(6.73391478647192,0.690770594724244,
64.3355696852805));
#199533=CARTESIAN_POINT('Ctrl Pts',(6.71162441967599,0.86393671597462,64.3437766605525));
#199534=CARTESIAN_POINT('Ctrl Pts',(6.6893486972062,1.03698907053911,64.3519782440055));
#199535=CARTESIAN_POINT('Ctrl Pts',(6.66036069033445,1.20929597735572,64.3601798274585));
#199536=CARTESIAN_POINT('Ctrl Pts',(6.62473075200399,1.38030122199928,64.3683814109115));
#199537=CARTESIAN_POINT('Ctrl Pts',(6.5891170718551,1.55122843579444,64.3765792519265));
#199538=CARTESIAN_POINT('Ctrl Pts',(6.54686757127822,1.72085482026698,64.3847770929416));
#199539=CARTESIAN_POINT('Ctrl Pts',(6.49810399063429,1.88863271360599,64.3929749339566));
#199540=CARTESIAN_POINT('Ctrl Pts',(6.44934471322425,2.05639580106923,64.4011720515378));
#199541=CARTESIAN_POINT('Ctrl Pts',(6.39407259256909,2.22231037571562,64.4093691691189));
#199542=CARTESIAN_POINT('Ctrl Pts',(6.33245979173458,2.38584198681826,64.4175662867001));
#199543=CARTESIAN_POINT('Ctrl Pts',(6.27084767641108,2.54937177844962,64.4257633130792));
#199544=CARTESIAN_POINT('Ctrl Pts',(6.20289514693037,2.71051832317652,64.4339603394583));
#199545=CARTESIAN_POINT('Ctrl Pts',(6.12882322554851,2.86876539124013,64.4421573658374));
#199546=CARTESIAN_POINT('Ctrl Pts',(6.05473865977661,3.02703947274709,64.4503557914835));
#199547=CARTESIAN_POINT('Ctrl Pts',(5.97453277306417,3.1824127664959,64.4585542171297));
#199548=CARTESIAN_POINT('Ctrl Pts',(5.88847344329453,3.33439192471657,64.4667526427758));
#199549=CARTESIAN_POINT('Ctrl Pts',(5.80238377446761,3.48642466114196,64.4749539586665));
#199550=CARTESIAN_POINT('Ctrl Pts',(5.71043672867051,3.63506056642938,64.4831552745571));
#199551=CARTESIAN_POINT('Ctrl Pts',(5.61294458048369,3.7798336122664,64.4913565904477));
#199552=CARTESIAN_POINT('Ctrl Pts',(5.51534140505971,3.92477153036843,64.4995672462643));
#199553=CARTESIAN_POINT('Ctrl Pts',(5.41218071175398,4.06583750235549,64.5077779020809));
#199554=CARTESIAN_POINT('Ctrl Pts',(5.30381693588577,4.20259621075012,64.5159885578975));
#199555=CARTESIAN_POINT('Ctrl Pts',(5.19538930386982,4.33943550773829,64.5242040520547));
#199556=CARTESIAN_POINT('Ctrl Pts',(5.08175271078018,4.47196220973772,64.5324195462119));
#199557=CARTESIAN_POINT('Ctrl Pts',(4.96329974703248,4.59977658382527,64.540635040369));
#199558=CARTESIAN_POINT('Ctrl Pts',(4.8446630013318,4.72778926426622,64.5488632810165));
#199559=CARTESIAN_POINT('Ctrl Pts',(4.72119520535234,4.85107475263417,64.557091521664));
#199560=CARTESIAN_POINT('Ctrl Pts',(4.59332441746952,4.9692715558599,64.5653197623115));
#199561=CARTESIAN_POINT('Ctrl Pts',(4.47711028599368,5.07669357974457,64.5727979194126));
#199562=CARTESIAN_POINT('Ctrl Pts',(4.35725989585569,5.17991277858773,64.5802760765137));
#199563=CARTESIAN_POINT('Ctrl Pts',(4.23411560178897,5.27868866961173,64.5877542336147));
#199564=CARTESIAN_POINT('Ctrl Pts',(4.10121601260401,5.38528942962222,64.5958247984275));
#199565=CARTESIAN_POINT('Ctrl Pts',(3.96404432174565,5.48706334156706,64.6038953632403));
#199566=CARTESIAN_POINT('Ctrl Pts',(3.82299214193917,5.58363860602308,64.6119659280531));
#199567=CARTESIAN_POINT('Ctrl Pts',(3.68214381142925,5.68007429943702,64.6200248292464));
#199568=CARTESIAN_POINT('Ctrl Pts',(3.53742646164195,5.77132609532913,64.6280837304396));
#199569=CARTESIAN_POINT('Ctrl Pts',(3.38926637153549,5.85706090652801,64.6361426316329));
#199570=CARTESIAN_POINT('Ctrl Pts',(3.29393078808783,5.91222811276787,64.641328238949));
#199571=CARTESIAN_POINT('Ctrl Pts',(3.1971704820577,5.96511180235815,64.6465138462651));
#199572=CARTESIAN_POINT('Ctrl Pts',(3.09910619832139,6.01563211736938,64.6516994535812));
#199573=CARTESIAN_POINT('Origin',(0.,0.,4.30282021618968));
#199574=CARTESIAN_POINT('',(3.09910619832127,6.01563211736944,67.045599963736));
#199575=CARTESIAN_POINT('',(3.09910619832135,6.0156321173694,66.651425676538));
#199576=CARTESIAN_POINT('',(3.09910619832133,6.0156321173694,4.30282021618968));
#199577=CARTESIAN_POINT('',(-6.76699920770444,-0.00327458815153042,65.6971797838342));
#199578=CARTESIAN_POINT('Ctrl Pts',(-6.76699920770444,-0.00327458815152907,
65.6971797838342));
#199579=CARTESIAN_POINT('Ctrl Pts',(-6.76690542650691,-0.197075231149046,
65.7062649518173));
#199580=CARTESIAN_POINT('Ctrl Pts',(-6.75848210553396,-0.390632917290863,
65.7153501198004));
#199581=CARTESIAN_POINT('Ctrl Pts',(-6.74181645938078,-0.583266515430461,
65.7244352877836));
#199582=CARTESIAN_POINT('Ctrl Pts',(-6.72495810982722,-0.778127518919279,
65.7336255067648));
#199583=CARTESIAN_POINT('Ctrl Pts',(-6.69966572931804,-0.972042707940345,
65.7428157257461));
#199584=CARTESIAN_POINT('Ctrl Pts',(-6.66608169134746,-1.16432121181491,
65.7520059447274));
#199585=CARTESIAN_POINT('Ctrl Pts',(-6.63266310140719,-1.35565247701127,
65.7611508891163));
#199586=CARTESIAN_POINT('Ctrl Pts',(-6.59103450047461,-1.54536296153818,
65.7702958335053));
#199587=CARTESIAN_POINT('Ctrl Pts',(-6.54138605026677,-1.73278894888422,
65.7794407778942));
#199588=CARTESIAN_POINT('Ctrl Pts',(-6.49136890235314,-1.92160679300023,
65.7886536341717));
#199589=CARTESIAN_POINT('Ctrl Pts',(-6.43321240571779,-2.1081058685722,
65.7978664904491));
#199590=CARTESIAN_POINT('Ctrl Pts',(-6.36716032525063,-2.29162789138077,
65.8070793467265));
#199591=CARTESIAN_POINT('Ctrl Pts',(-6.30110824478346,-2.4751499141894,
65.816292203004));
#199592=CARTESIAN_POINT('Ctrl Pts',(-6.22716070257162,-2.65569469998394,
65.8255050592814));
#199593=CARTESIAN_POINT('Ctrl Pts',(-6.14560918242237,-2.83262718636356,
65.8347179155589));
#199594=CARTESIAN_POINT('Ctrl Pts',(-6.07282224090383,-2.99054422476176,
65.8429406394255));
#199595=CARTESIAN_POINT('Ctrl Pts',(-5.99384780368116,-3.14586409371244,
65.851163363292));
#199596=CARTESIAN_POINT('Ctrl Pts',(-5.90889423041982,-3.29806882489,65.8593860871586));
#199597=CARTESIAN_POINT('Ctrl Pts',(-5.82403057763788,-3.45011245251572,
65.8676001075505));
#199598=CARTESIAN_POINT('Ctrl Pts',(-5.73320056469686,-3.59904719765596,
65.8758141279424));
#199599=CARTESIAN_POINT('Ctrl Pts',(-5.63666023840997,-3.74437583005874,
65.8840281483343));
#199600=CARTESIAN_POINT('Ctrl Pts',(-5.54020271421983,-3.88957981490807,
65.892235123607));
#199601=CARTESIAN_POINT('Ctrl Pts',(-5.43804482825019,-4.03118354977133,
65.9004420988796));
#199602=CARTESIAN_POINT('Ctrl Pts',(-5.33048812136502,-4.16871507637383,
65.9086490741523));
#199603=CARTESIAN_POINT('Ctrl Pts',(-5.22300207708986,-4.30615624750794,
65.9168506576059));
#199604=CARTESIAN_POINT('Ctrl Pts',(-5.1101244971274,-4.43953025781604,
65.9250522410596));
#199605=CARTESIAN_POINT('Ctrl Pts',(-4.99219978659632,-4.56839471704314,
65.9332538245133));
#199606=CARTESIAN_POINT('Ctrl Pts',(-4.87432888590749,-4.69720037454673,
65.941451665529));
#199607=CARTESIAN_POINT('Ctrl Pts',(-4.75141568454248,-4.8215003163931,
65.9496495065448));
#199608=CARTESIAN_POINT('Ctrl Pts',(-4.62384441123766,-4.94088573645113,
65.9578473475605));
#199609=CARTESIAN_POINT('Ctrl Pts',(-4.49628439569947,-5.06026062111853,
65.9660444651423));
#199610=CARTESIAN_POINT('Ctrl Pts',(-4.36406738285808,-5.17472159665961,
65.9742415827242));
#199611=CARTESIAN_POINT('Ctrl Pts',(-4.22761421767973,-5.28389695456604,
65.9824387003061));
#199612=CARTESIAN_POINT('Ctrl Pts',(-4.09116257069484,-5.39307109777499,
65.9906357266859));
#199613=CARTESIAN_POINT('Ctrl Pts',(-3.95047514476605,-5.49695951546655,
65.9988327530656));
#199614=CARTESIAN_POINT('Ctrl Pts',(-3.80600549940807,-5.5952311067976,
66.0070297794454));
#199615=CARTESIAN_POINT('Ctrl Pts',(-3.66151119247102,-5.69351947350465,
66.0152282050923));
#199616=CARTESIAN_POINT('Ctrl Pts',(-3.51323367650264,-5.78618890177864,
66.0234266307391));
#199617=CARTESIAN_POINT('Ctrl Pts',(-3.36165512354724,-5.87295188387651,
66.0316250563859));
#199618=CARTESIAN_POINT('Ctrl Pts',(-3.21002313361495,-5.95974545309491,
66.0398263722773));
#199619=CARTESIAN_POINT('Ctrl Pts',(-3.05508809975564,-6.04062825014876,
66.0480276881687));
#199620=CARTESIAN_POINT('Ctrl Pts',(-2.89735642705186,-6.11535892116082,
66.05622900406));
#199621=CARTESIAN_POINT('Ctrl Pts',(-2.73944512437668,-6.19017469789748,
66.0644396598773));
#199622=CARTESIAN_POINT('Ctrl Pts',(-2.57873114460146,-6.25882419757173,
66.0726503156946));
#199623=CARTESIAN_POINT('Ctrl Pts',(-2.4157414720476,-6.32111399519336,
66.0808609715119));
#199624=CARTESIAN_POINT('Ctrl Pts',(-2.25265575362824,-6.38344049868371,
66.0890764656697));
#199625=CARTESIAN_POINT('Ctrl Pts',(-2.08729200866785,-6.439399714989,66.0972919598276));
#199626=CARTESIAN_POINT('Ctrl Pts',(-1.92019186851095,-6.48884829442825,
66.1055074539854));
#199627=CARTESIAN_POINT('Ctrl Pts',(-1.75283246941213,-6.53837359424831,
66.1137356946336));
#199628=CARTESIAN_POINT('Ctrl Pts',(-1.58373163888332,-6.58136798231884,
66.1219639352818));
#199629=CARTESIAN_POINT('Ctrl Pts',(-1.41344198922957,-6.61773909602689,
66.13019217593));
#199630=CARTESIAN_POINT('Ctrl Pts',(-1.25867588480477,-6.65079463166063,
66.1376703330228));
#199631=CARTESIAN_POINT('Ctrl Pts',(-1.10292812370035,-6.67838002420534,
66.1451484901156));
#199632=CARTESIAN_POINT('Ctrl Pts',(-0.946615852892707,-6.70046322481157,
66.1526266472084));
#199633=CARTESIAN_POINT('Ctrl Pts',(-0.777947017418176,-6.72429211367971,
66.1606959564304));
#199634=CARTESIAN_POINT('Ctrl Pts',(-0.608068646005757,-6.74179166845406,
66.1687652656524));
#199635=CARTESIAN_POINT('Ctrl Pts',(-0.437507024395419,-6.7528421130369,
66.1768345748744));
#199636=CARTESIAN_POINT('Ctrl Pts',(-0.26715813948428,-6.76387877471194,
66.1848938194746));
#199637=CARTESIAN_POINT('Ctrl Pts',(-0.09612806766793,-6.76848230737992,
66.1929530640749));
#199638=CARTESIAN_POINT('Ctrl Pts',(0.0750465407677626,-6.76658385130332,
66.2010123086751));
#199639=CARTESIAN_POINT('Ctrl Pts',(0.24604521192923,-6.76468734650436,
66.2090632697949));
#199640=CARTESIAN_POINT('Ctrl Pts',(0.417187754117139,-6.75630215615335,
66.2171142309146));
#199641=CARTESIAN_POINT('Ctrl Pts',(0.587932317773019,-6.74141117198158,
66.2251651920344));
#199642=CARTESIAN_POINT('Ctrl Pts',(0.75853879968691,-6.72653223020221,
66.2332096423129));
#199643=CARTESIAN_POINT('Ctrl Pts',(0.928747573812776,-6.70515799850142,
66.2412540925915));
#199644=CARTESIAN_POINT('Ctrl Pts',(1.09801681797997,-6.67732342090999,
66.2492985428701));
#199645=CARTESIAN_POINT('Ctrl Pts',(1.26718622495699,-6.64950526051255,
66.2573382484278));
#199646=CARTESIAN_POINT('Ctrl Pts',(1.43541683785557,-6.61523439997803,
66.2653779539856));
#199647=CARTESIAN_POINT('Ctrl Pts',(1.6021720938859,-6.57459759845219,66.2734176595433));
#199648=CARTESIAN_POINT('Ctrl Pts',(1.77252667298302,-6.53308367328674,
66.2816308978481));
#199649=CARTESIAN_POINT('Ctrl Pts',(1.94134108426297,-6.48492590695746,
66.2898441361528));
#199650=CARTESIAN_POINT('Ctrl Pts',(2.10805392617354,-6.430271972813,66.2980573744576));
#199651=CARTESIAN_POINT('Ctrl Pts',(2.27119185757413,-6.37679001151325,
66.3060944920053));
#199652=CARTESIAN_POINT('Ctrl Pts',(2.43231707074948,-6.31708779256848,
66.3141316095529));
#199653=CARTESIAN_POINT('Ctrl Pts',(2.59091904766208,-6.25135405240031,
66.3221687271006));
#199654=CARTESIAN_POINT('Ctrl Pts',(2.74953780365543,-6.18561335802038,
66.3302066949242));
#199655=CARTESIAN_POINT('Ctrl Pts',(2.90563244664924,-6.11384001482513,
66.3382446627478));
#199656=CARTESIAN_POINT('Ctrl Pts',(3.0587129614512,-6.03627070461974,66.3462826305714));
#199657=CARTESIAN_POINT('Ctrl Pts',(3.21184000209162,-5.95867781873457,
66.3543230413786));
#199658=CARTESIAN_POINT('Ctrl Pts',(3.36195075799938,-5.8752856282353,66.3623634521859));
#199659=CARTESIAN_POINT('Ctrl Pts',(3.50858045251912,-5.78637643160214,
66.3704038629931));
#199660=CARTESIAN_POINT('Ctrl Pts',(3.66075192251652,-5.69410696877423,
66.3787481559819));
#199661=CARTESIAN_POINT('Ctrl Pts',(3.80917368031177,-5.59589555959404,
66.3870924489706));
#199662=CARTESIAN_POINT('Ctrl Pts',(3.95336085692254,-5.49210587433934,
66.3954367419593));
#199663=CARTESIAN_POINT('Ctrl Pts',(4.09254239179647,-5.39191938038484,
66.4034913521744));
#199664=CARTESIAN_POINT('Ctrl Pts',(4.22777818736746,-5.28653571229999,
66.4115459623895));
#199665=CARTESIAN_POINT('Ctrl Pts',(4.35866773324423,-5.17632153089195,
66.4196005726045));
#199666=CARTESIAN_POINT('Ctrl Pts',(4.48965636435639,-5.06602391579152,
66.4276612802733));
#199667=CARTESIAN_POINT('Ctrl Pts',(4.61629192016794,-4.95088875587905,
66.4357219879421));
#199668=CARTESIAN_POINT('Ctrl Pts',(4.7382119034419,-4.83131834576045,66.4437826956108));
#199669=CARTESIAN_POINT('Ctrl Pts',(4.8603037865879,-4.71157934852719,66.4518547683945));
#199670=CARTESIAN_POINT('Ctrl Pts',(4.97766657782695,-4.58739289333984,
66.4599268411782));
#199671=CARTESIAN_POINT('Ctrl Pts',(5.08997869338911,-4.45919341370667,
66.4679989139619));
#199672=CARTESIAN_POINT('Ctrl Pts',(5.10174253423307,-4.44576549217625,
66.4688444022605));
#199673=CARTESIAN_POINT('Ctrl Pts',(5.11345100424188,-4.43229356882661,
66.4696898905592));
#199674=CARTESIAN_POINT('Ctrl Pts',(5.12510376216945,-4.41877815996646,
66.4705353788579));
#199675=CARTESIAN_POINT('Ctrl Pts',(5.23995044138292,-4.28557365718281,
66.4788683009027));
#199676=CARTESIAN_POINT('Ctrl Pts',(5.34974824041682,-4.14771789045397,
66.4872012229475));
#199677=CARTESIAN_POINT('Ctrl Pts',(5.45410511793379,-4.00562434116437,
66.4955341449923));
#199678=CARTESIAN_POINT('Ctrl Pts',(5.55833867092831,-3.86369871199201,
66.503857219544));
#199679=CARTESIAN_POINT('Ctrl Pts',(5.65714390696477,-3.7175455546957,66.5121802940957));
#199680=CARTESIAN_POINT('Ctrl Pts',(5.75016747625841,-3.56761306688099,
66.5205033686474));
#199681=CARTESIAN_POINT('Ctrl Pts',(5.8430981892616,-3.41783024193927,66.5288181350915));
#199682=CARTESIAN_POINT('Ctrl Pts',(5.93025855144572,-3.26427589640551,
66.5371329015355));
#199683=CARTESIAN_POINT('Ctrl Pts',(6.01133703373258,-3.10742917326769,
66.5454476679795));
#199684=CARTESIAN_POINT('Ctrl Pts',(6.0923494558588,-2.95071024383589,66.5537556598172));
#199685=CARTESIAN_POINT('Ctrl Pts',(6.16728971288715,-2.79070458971096,
66.5620636516548));
#199686=CARTESIAN_POINT('Ctrl Pts',(6.23589084995342,-2.62791824596337,
66.5703716434924));
#199687=CARTESIAN_POINT('Ctrl Pts',(6.30444866989683,-2.46523469112503,
66.5786743893776));
#199688=CARTESIAN_POINT('Ctrl Pts',(6.36667521211871,-2.29977426554493,
66.5869771352627));
#199689=CARTESIAN_POINT('Ctrl Pts',(6.42235044863246,-2.13206559818182,
66.5952798811479));
#199690=CARTESIAN_POINT('Ctrl Pts',(6.47800293245139,-1.96442546800629,
66.6035792339654));
#199691=CARTESIAN_POINT('Ctrl Pts',(6.52710933585228,-1.79453925648026,
66.611878586783));
#199692=CARTESIAN_POINT('Ctrl Pts',(6.569498468757,-1.62295374826254,66.6201779396005));
#199693=CARTESIAN_POINT('Ctrl Pts',(6.61187858620445,-1.45140473340319,
66.6284755272849));
#199694=CARTESIAN_POINT('Ctrl Pts',(6.64754419595931,-1.27815747942175,
66.6367731149694));
#199695=CARTESIAN_POINT('Ctrl Pts',(6.67637444601388,-1.10377228476385,
66.6450707026538));
#199696=CARTESIAN_POINT('Ctrl Pts',(6.7052033552322,-0.929395200406484,
66.6533679044343));
#199697=CARTESIAN_POINT('Ctrl Pts',(6.72719748165547,-0.753880624083096,
66.6616651062149));
#199698=CARTESIAN_POINT('Ctrl Pts',(6.74228737057286,-0.57779755331233,
66.6699623079954));
#199699=CARTESIAN_POINT('Ctrl Pts',(6.7573790651445,-0.401693412462954,
66.6782605026181));
#199700=CARTESIAN_POINT('Ctrl Pts',(6.76556484688301,-0.225020988278597,
66.6865586972408));
#199701=CARTESIAN_POINT('Ctrl Pts',(6.76682724616212,-0.0483530826106249,
66.6948568918634));
#199702=CARTESIAN_POINT('Ctrl Pts',(6.76809053330137,0.128439075655805,
66.7031609227031));
#199703=CARTESIAN_POINT('Ctrl Pts',(6.76242070568186,0.305226360734584,
66.7114649535429));
#199704=CARTESIAN_POINT('Ctrl Pts',(6.74985244375693,0.481436379502573,
66.7197689843826));
#199705=CARTESIAN_POINT('Ctrl Pts',(6.73727961166603,0.657710473083544,
66.7280760347965));
#199706=CARTESIAN_POINT('Ctrl Pts',(6.71780337770929,0.83340653552811,66.7363830852104));
#199707=CARTESIAN_POINT('Ctrl Pts',(6.69151021186395,1.0079583743987,66.7446901356244));
#199708=CARTESIAN_POINT('Ctrl Pts',(6.66518893418664,1.18269683864544,66.7530060676772));
#199709=CARTESIAN_POINT('Ctrl Pts',(6.63203622137704,1.35628829190802,66.76132199973));
#199710=CARTESIAN_POINT('Ctrl Pts',(6.59218969367674,1.52817670528714,66.7696379317829));
#199711=CARTESIAN_POINT('Ctrl Pts',(6.56215253461373,1.65774984281592,66.7759066580244));
#199712=CARTESIAN_POINT('Ctrl Pts',(6.52831269653172,1.78635544844846,66.7821753842659));
#199713=CARTESIAN_POINT('Ctrl Pts',(6.49074769299697,1.91376158020129,66.7884441105074));
#199714=CARTESIAN_POINT('Ctrl Pts',(6.44010991381911,2.08550556951401,66.7968943792489));
#199715=CARTESIAN_POINT('Ctrl Pts',(6.38260852795585,2.25538432239095,66.8053446479904));
#199716=CARTESIAN_POINT('Ctrl Pts',(6.31840008856451,2.4228308485794,66.813794916732));
#199717=CARTESIAN_POINT('Ctrl Pts',(6.25424831530007,2.59012959752562,66.8222377278245));
#199718=CARTESIAN_POINT('Ctrl Pts',(6.18340140471071,2.75500009003148,66.8306805389171));
#199719=CARTESIAN_POINT('Ctrl Pts',(6.10606559760062,2.91689079634432,66.8391233500096));
#199720=CARTESIAN_POINT('Ctrl Pts',(6.02878751249635,3.07866067044965,66.8475598595453));
#199721=CARTESIAN_POINT('Ctrl Pts',(5.94503032796038,3.23745489367703,66.8559963690809));
#199722=CARTESIAN_POINT('Ctrl Pts',(5.85504839435968,3.39274185574236,66.8644328786165));
#199723=CARTESIAN_POINT('Ctrl Pts',(5.76513084767753,3.54791770162495,66.8728633513753));
#199724=CARTESIAN_POINT('Ctrl Pts',(5.66899760227697,3.69959100601353,66.8812938241341));
#199725=CARTESIAN_POINT('Ctrl Pts',(5.56694903640641,3.84725453096799,66.8897242968929));
#199726=CARTESIAN_POINT('Ctrl Pts',(5.46494434094009,3.99485457576989,66.8981511454141));
#199727=CARTESIAN_POINT('Ctrl Pts',(5.35702958269231,4.1384480053,66.9065779939354));
#199728=CARTESIAN_POINT('Ctrl Pts',(5.2435489204202,4.27755581134369,66.9150048424566));
#199729=CARTESIAN_POINT('Ctrl Pts',(5.13010328558069,4.41662067976962,66.9234290899102));
#199730=CARTESIAN_POINT('Ctrl Pts',(5.01109538216323,4.55120242920022,66.9318533373639));
#199731=CARTESIAN_POINT('Ctrl Pts',(4.88691040477964,4.68085416304081,66.9402775848175));
#199732=CARTESIAN_POINT('Ctrl Pts',(4.85191983117837,4.71738505937837,66.9426512153224));
#199733=CARTESIAN_POINT('Ctrl Pts',(4.81651849292903,4.75352476956623,66.9450248458273));
#199734=CARTESIAN_POINT('Ctrl Pts',(4.78071556426013,4.7892637945347,66.9473984763321));
#199735=CARTESIAN_POINT('Ctrl Pts',(4.65068866603528,4.91905861118802,66.956018883197));
#199736=CARTESIAN_POINT('Ctrl Pts',(4.51542036286421,5.0435076761011,66.9646392900618));
#199737=CARTESIAN_POINT('Ctrl Pts',(4.37537611229567,5.162206202386,66.9732596969266));
#199738=CARTESIAN_POINT('Ctrl Pts',(4.23526607529101,5.28096048785404,66.9818841532675));
#199739=CARTESIAN_POINT('Ctrl Pts',(4.09037584969622,5.39395865182629,66.9905086096085));
#199740=CARTESIAN_POINT('Ctrl Pts',(3.94120298921011,5.50083702702064,66.9991330659494));
#199741=CARTESIAN_POINT('Ctrl Pts',(3.79187566396558,5.60782607209389,67.0077664526987));
#199742=CARTESIAN_POINT('Ctrl Pts',(3.63825708990562,5.70868248803072,67.0163998394481));
#199743=CARTESIAN_POINT('Ctrl Pts',(3.48087406380763,5.80308579567038,67.0250332261974));
#199744=CARTESIAN_POINT('Ctrl Pts',(3.35589972543279,5.87804934927062,67.0318888053769));
#199745=CARTESIAN_POINT('Ctrl Pts',(3.22855226664415,5.94894467623928,67.0387443845565));
#199746=CARTESIAN_POINT('Ctrl Pts',(3.09910619832127,6.01563211736944,67.045599963736));
#199747=CARTESIAN_POINT('Ctrl Pts',(3.09910619832142,6.01563211736936,65.0458684084508));
#199748=CARTESIAN_POINT('Ctrl Pts',(2.94516114955274,6.09494083265172,65.0539895899452));
#199749=CARTESIAN_POINT('Ctrl Pts',(2.78812931881981,6.16835713904708,65.0621107714396));
#199750=CARTESIAN_POINT('Ctrl Pts',(2.62850896512945,6.23564187716342,65.0702319529339));
#199751=CARTESIAN_POINT('Ctrl Pts',(2.46889259069812,6.30292493790344,65.0783529319711));
#199752=CARTESIAN_POINT('Ctrl Pts',(2.30668815948071,6.36407659300713,65.0864739110084));
#199753=CARTESIAN_POINT('Ctrl Pts',(2.14241424949784,6.4189056842696,65.0945948900456));
#199754=CARTESIAN_POINT('Ctrl Pts',(1.97811308399406,6.4737438725058,65.1027172164757));
#199755=CARTESIAN_POINT('Ctrl Pts',(1.81174210374682,6.52225729344709,65.1108395429059));
#199756=CARTESIAN_POINT('Ctrl Pts',(1.64383534460238,6.56430456025892,65.1189618693361));
#199757=CARTESIAN_POINT('Ctrl Pts',(1.47580182462047,6.60638357056207,65.1270903276987));
#199758=CARTESIAN_POINT('Ctrl Pts',(1.30623056605353,6.64198659017616,65.1352187860613));
#199759=CARTESIAN_POINT('Ctrl Pts',(1.13566669900318,6.67102317105669,65.1433472444239));
#199760=CARTESIAN_POINT('Ctrl Pts',(0.96502626010918,6.70007278743278,65.1514793519243));
#199761=CARTESIAN_POINT('Ctrl Pts',(0.79339268720288,6.72255004250854,65.1596114594246));
#199762=CARTESIAN_POINT('Ctrl Pts',(0.621316279714828,6.73841636295661,
65.167743566925));
#199763=CARTESIAN_POINT('Ctrl Pts',(0.449060062493121,6.75429926277715,
65.1758841719998));
#199764=CARTESIAN_POINT('Ctrl Pts',(0.276360451521886,6.7635574159956,65.1840247770746));
#199765=CARTESIAN_POINT('Ctrl Pts',(0.103768411007834,6.76620433602747,
65.1921653821493));
#199766=CARTESIAN_POINT('Ctrl Pts',(0.0561708232495194,6.7669343060083,
65.1944104055195));
#199767=CARTESIAN_POINT('Ctrl Pts',(0.00858139259991337,6.76716176248498,
65.1966554288896));
#199768=CARTESIAN_POINT('Ctrl Pts',(-0.0389883963188912,6.76688768230658,
65.1989004522597));
#199769=CARTESIAN_POINT('Ctrl Pts',(-0.217827952145001,6.76585727249229,
65.2073406617175));
#199770=CARTESIAN_POINT('Ctrl Pts',(-0.396759164286741,6.75773204046498,
65.2157808711752));
#199771=CARTESIAN_POINT('Ctrl Pts',(-0.575195289471173,6.74250987236728,
65.2242210806329));
#199772=CARTESIAN_POINT('Ctrl Pts',(-0.753496222855277,6.72729923731709,
65.2326548953815));
#199773=CARTESIAN_POINT('Ctrl Pts',(-0.931302485939268,6.70500241309035,
65.2410887101301));
#199774=CARTESIAN_POINT('Ctrl Pts',(-1.10802896737074,6.67566931531718,
65.2495225248788));
#199775=CARTESIAN_POINT('Ctrl Pts',(-1.28464871992387,6.64635393242521,
65.2579512462674));
#199776=CARTESIAN_POINT('Ctrl Pts',(-1.46018966272657,6.61001080215337,
65.266379967656));
#199777=CARTESIAN_POINT('Ctrl Pts',(-1.63407303125078,6.56674153051107,
65.2748086890447));
#199778=CARTESIAN_POINT('Ctrl Pts',(-1.80787808908676,6.52349174576088,
65.2832336144465));
#199779=CARTESIAN_POINT('Ctrl Pts',(-1.98002673802562,6.47332211952744,
65.2916585398483));
#199780=CARTESIAN_POINT('Ctrl Pts',(-2.14995122414666,6.4163851765453,65.3000834652502));
#199781=CARTESIAN_POINT('Ctrl Pts',(-2.31982525396339,6.35946514005961,
65.3085058890078));
#199782=CARTESIAN_POINT('Ctrl Pts',(-2.48747612213423,6.29578189993621,
65.3169283127655));
#199783=CARTESIAN_POINT('Ctrl Pts',(-2.65235165830439,6.22553770213385,
65.3253507365232));
#199784=CARTESIAN_POINT('Ctrl Pts',(-2.81722978749479,6.15529239959132,
65.3337732927415));
#199785=CARTESIAN_POINT('Ctrl Pts',(-2.97933218814459,6.07848605776204,
65.3421958489597));
#199786=CARTESIAN_POINT('Ctrl Pts',(-3.13812646407643,5.99536915422755,
65.350618405178));
#199787=CARTESIAN_POINT('Ctrl Pts',(-3.29692610410909,5.91224944298827,
65.3590412459118));
#199788=CARTESIAN_POINT('Ctrl Pts',(-3.45241710098796,5.82281889954178,
65.3674640866457));
#199789=CARTESIAN_POINT('Ctrl Pts',(-3.6040913408839,5.72737414585128,65.3758869273795));
#199790=CARTESIAN_POINT('Ctrl Pts',(-3.75579187976612,5.63191284287549,
65.3843112285603));
#199791=CARTESIAN_POINT('Ctrl Pts',(-3.9036740599332,5.53043542824901,65.392735529741));
#199792=CARTESIAN_POINT('Ctrl Pts',(-4.04725814945114,5.42328226000651,
65.4011598309217));
#199793=CARTESIAN_POINT('Ctrl Pts',(-4.19088718726476,5.31609554798974,
65.4095867692886));
#199794=CARTESIAN_POINT('Ctrl Pts',(-4.33021518465237,5.20322973938779,
65.4180137076555));
#199795=CARTESIAN_POINT('Ctrl Pts',(-4.46479464896943,5.0850661492781,65.4264406460225));
#199796=CARTESIAN_POINT('Ctrl Pts',(-4.59949511714048,4.96679631524867,
65.4348751612662));
#199797=CARTESIAN_POINT('Ctrl Pts',(-4.72943827015068,4.84321940203399,
65.4433096765099));
#199798=CARTESIAN_POINT('Ctrl Pts',(-4.8542118934293,4.71475512552768,65.4517441917537));
#199799=CARTESIAN_POINT('Ctrl Pts',(-4.9790457834363,4.58622879967588,65.4601827809405));
#199800=CARTESIAN_POINT('Ctrl Pts',(-5.09870493747933,4.45281064726322,
65.4686213701273));
#199801=CARTESIAN_POINT('Ctrl Pts',(-5.21281642764112,4.31495468014612,
65.4770599593141));
#199802=CARTESIAN_POINT('Ctrl Pts',(-5.3270554686324,4.17694462124623,65.4855079809345));
#199803=CARTESIAN_POINT('Ctrl Pts',(-5.43573424864483,4.03448709788232,
65.4939560025548));
#199804=CARTESIAN_POINT('Ctrl Pts',(-5.53852155820174,3.88806737973181,
65.5024040241752));
#199805=CARTESIAN_POINT('Ctrl Pts',(-5.59694421537717,3.80484476174419,
65.5072057440866));
#199806=CARTESIAN_POINT('Ctrl Pts',(-5.65346437173352,3.7203426353821,65.512007463998));
#199807=CARTESIAN_POINT('Ctrl Pts',(-5.70802771665664,3.63465384677545,
65.5168091839094));
#199808=CARTESIAN_POINT('Ctrl Pts',(-5.80165592211089,3.48761580290016,
65.5250487157605));
#199809=CARTESIAN_POINT('Ctrl Pts',(-5.88972869975506,3.3367539508084,65.5332882476116));
#199810=CARTESIAN_POINT('Ctrl Pts',(-5.9719198253901,3.1825245637878,65.5415277794628));
#199811=CARTESIAN_POINT('Ctrl Pts',(-6.05401972462032,3.02846636060714,
65.5497581660094));
#199812=CARTESIAN_POINT('Ctrl Pts',(-6.13025080472018,2.87104837626483,
65.5579885525561));
#199813=CARTESIAN_POINT('Ctrl Pts',(-6.20032988223659,2.71075604794014,
65.5662189391027));
#199814=CARTESIAN_POINT('Ctrl Pts',(-6.27034367833743,2.55061303822049,
65.5744416587208));
#199815=CARTESIAN_POINT('Ctrl Pts',(-6.33421674317225,2.38760134111947,
65.5826643783388));
#199816=CARTESIAN_POINT('Ctrl Pts',(-6.39171159530326,2.22223128464746,
65.5908870979569));
#199817=CARTESIAN_POINT('Ctrl Pts',(-6.44915550285331,2.05700775795885,
65.599102531653));
#199818=CARTESIAN_POINT('Ctrl Pts',(-6.50023234535129,1.88943037170787,
65.6073179653491));
#199819=CARTESIAN_POINT('Ctrl Pts',(-6.54475264039243,1.72002961488351,
65.6155333990451));
#199820=CARTESIAN_POINT('Ctrl Pts',(-6.58925005545882,1.55071591689458,
65.6237446106462));
#199821=CARTESIAN_POINT('Ctrl Pts',(-6.62719754359413,1.37958105796757,
65.6319558222473));
#199822=CARTESIAN_POINT('Ctrl Pts',(-6.65845526421439,1.2071712780114,65.6401670338484));
#199823=CARTESIAN_POINT('Ctrl Pts',(-6.68970250272006,1.03481931478131,
65.6483754918623));
#199824=CARTESIAN_POINT('Ctrl Pts',(-6.71426437929343,0.861193632037482,
65.6565839498761));
#199825=CARTESIAN_POINT('Ctrl Pts',(-6.73205200567082,0.686851361608561,
65.6647924078899));
#199826=CARTESIAN_POINT('Ctrl Pts',(-6.73997678162466,0.609178073272046,
65.6684494551713));
#199827=CARTESIAN_POINT('Ctrl Pts',(-6.74655761967025,0.53136266984976,
65.6721065024528));
#199828=CARTESIAN_POINT('Ctrl Pts',(-6.75178996115178,0.453454871503358,
65.6757635497342));
#199829=CARTESIAN_POINT('Ctrl Pts',(-6.76200376127612,0.301374835586867,
65.6829022944261));
#199830=CARTESIAN_POINT('Ctrl Pts',(-6.76707289703235,0.149005845051979,
65.690041039118));
#199831=CARTESIAN_POINT('Ctrl Pts',(-6.76699920770469,-0.00327458763509952,
65.69717978381));
#199832=CARTESIAN_POINT('',(-6.76699956272236,0.00243271768895434,65.3028202162318));
#199833=CARTESIAN_POINT('Ctrl Pts',(3.09910619832139,6.01563211736938,64.6516994535812));
#199834=CARTESIAN_POINT('Ctrl Pts',(2.94693875536856,6.09402505371204,64.6597460182975));
#199835=CARTESIAN_POINT('Ctrl Pts',(2.79163034931604,6.16672520808967,64.6677925830138));
#199836=CARTESIAN_POINT('Ctrl Pts',(2.63365580949279,6.23346982643895,64.6758391477302));
#199837=CARTESIAN_POINT('Ctrl Pts',(2.47578674824321,6.3001698798403,64.6838803398075));
#199838=CARTESIAN_POINT('Ctrl Pts',(2.31525543930568,6.36092216788117,64.6919215318849));
#199839=CARTESIAN_POINT('Ctrl Pts',(2.15256031046411,6.41551035458713,64.6999627239623));
#199840=CARTESIAN_POINT('Ctrl Pts',(1.98993821690109,6.47007403617453,64.7080003062776));
#199841=CARTESIAN_POINT('Ctrl Pts',(1.82515459071054,6.51847900726484,64.7160378885929));
#199842=CARTESIAN_POINT('Ctrl Pts',(1.65872668409159,6.56055750584373,64.7240754709082));
#199843=CARTESIAN_POINT('Ctrl Pts',(1.49230647245128,6.60263405887662,64.7321126815969));
#199844=CARTESIAN_POINT('Ctrl Pts',(1.32424249096148,6.6383846199015,64.7401498922857));
#199845=CARTESIAN_POINT('Ctrl Pts',(1.15506613979514,6.66769159549981,64.7481871029745));
#199846=CARTESIAN_POINT('Ctrl Pts',(0.985884552355947,6.69699947819488,
64.7562245624276));
#199847=CARTESIAN_POINT('Ctrl Pts',(0.815590894709271,6.71986331380237,
64.7642620218806));
#199848=CARTESIAN_POINT('Ctrl Pts',(0.644725380944703,6.73621690440307,
64.7722994813336));
#199849=CARTESIAN_POINT('Ctrl Pts',(0.473820727341555,6.75257424108971,
64.7803387819122));
#199850=CARTESIAN_POINT('Ctrl Pts',(0.302344328702447,6.76241832863058,
64.7883780824908));
#199851=CARTESIAN_POINT('Ctrl Pts',(0.130839972253854,6.76573498606475,
64.7964173830694));
#199852=CARTESIAN_POINT('Ctrl Pts',(-0.0407376591175529,6.76905306053475,
64.8044601184245));
#199853=CARTESIAN_POINT('Ctrl Pts',(-0.212342899062803,6.7658381466579,
64.8125028537795));
#199854=CARTESIAN_POINT('Ctrl Pts',(-0.383433663236555,6.75612815345424,
64.8205455891346));
#199855=CARTESIAN_POINT('Ctrl Pts',(-0.554732208459059,6.7464063679567,
64.8285980919835));
#199856=CARTESIAN_POINT('Ctrl Pts',(-0.725514657581686,6.73017377492276,
64.8366505948325));
#199857=CARTESIAN_POINT('Ctrl Pts',(-0.895244939809831,6.70752007061812,
64.8447030976814));
#199858=CARTESIAN_POINT('Ctrl Pts',(-1.06509117150887,6.68485089067181,
64.8527611015136));
#199859=CARTESIAN_POINT('Ctrl Pts',(-1.23388343868523,6.65575192782333,
64.8608191053458));
#199860=CARTESIAN_POINT('Ctrl Pts',(-1.40109804990698,6.62036352888169,
64.868877109178));
#199861=CARTESIAN_POINT('Ctrl Pts',(-1.56856798368071,6.58492109485148,
64.8769474168997));
#199862=CARTESIAN_POINT('Ctrl Pts',(-1.73445509191011,6.54317014206269,
64.8850177246215));
#199863=CARTESIAN_POINT('Ctrl Pts',(-1.89825211904073,6.49530044667353,
64.8930880323432));
#199864=CARTESIAN_POINT('Ctrl Pts',(-1.98332680267741,6.47043736300005,
64.8972796766502));
#199865=CARTESIAN_POINT('Ctrl Pts',(-2.06783799326545,6.44392443317852,
64.9014713209572));
#199866=CARTESIAN_POINT('Ctrl Pts',(-2.15171708220286,6.4157932165989,64.9056629652642));
#199867=CARTESIAN_POINT('Ctrl Pts',(-2.31846737356143,6.35986880658982,
64.9139958873109));
#199868=CARTESIAN_POINT('Ctrl Pts',(-2.48325016122551,6.29736759062251,
64.9223288093576));
#199869=CARTESIAN_POINT('Ctrl Pts',(-2.64551726842098,6.22844502123013,
64.9306617314043));
#199870=CARTESIAN_POINT('Ctrl Pts',(-2.80759261524595,6.15960390160087,
64.9389848059579));
#199871=CARTESIAN_POINT('Ctrl Pts',(-2.96715788637728,6.08435668026371,
64.9473078805115));
#199872=CARTESIAN_POINT('Ctrl Pts',(-3.12368045659504,6.0029084121854,64.9556309550651));
#199873=CARTESIAN_POINT('Ctrl Pts',(-3.28004678570824,5.92154144591137,
64.9639457215111));
#199874=CARTESIAN_POINT('Ctrl Pts',(-3.43337615830418,5.83398592477317,
64.9722604879571));
#199875=CARTESIAN_POINT('Ctrl Pts',(-3.58315611628153,5.74049486075497,
64.980575254403));
#199876=CARTESIAN_POINT('Ctrl Pts',(-3.73281403832754,5.64707997027311,
64.9888832462426));
#199877=CARTESIAN_POINT('Ctrl Pts',(-3.87892801431128,5.54773935666794,
64.9971912380821));
#199878=CARTESIAN_POINT('Ctrl Pts',(-4.02101018996412,5.44277190889024,
65.0054992299216));
#199879=CARTESIAN_POINT('Ctrl Pts',(-4.1630026500332,5.33787074117765,65.0138019758087));
#199880=CARTESIAN_POINT('Ctrl Pts',(-4.30096810421492,5.2273500261231,65.0221047216957));
#199881=CARTESIAN_POINT('Ctrl Pts',(-4.43444751909432,5.1115520344019,65.0304074675828));
#199882=CARTESIAN_POINT('Ctrl Pts',(-4.56787238519079,4.9958013656295,65.0387068204023));
#199883=CARTESIAN_POINT('Ctrl Pts',(-4.69681460257618,4.8747779451232,65.0470061732217));
#199884=CARTESIAN_POINT('Ctrl Pts',(-4.8208478673979,4.74886458423538,65.0553055260411));
#199885=CARTESIAN_POINT('Ctrl Pts',(-4.94485475242528,4.62297800300681,
65.0636031137275));
#199886=CARTESIAN_POINT('Ctrl Pts',(-5.06395452086855,4.49220380103383,
65.0719007014138));
#199887=CARTESIAN_POINT('Ctrl Pts',(-5.17775725781825,4.35696210439229,
65.0801982891002));
#199888=CARTESIAN_POINT('Ctrl Pts',(-5.29155470203395,4.22172669756719,
65.0884954908826));
#199889=CARTESIAN_POINT('Ctrl Pts',(-5.40005538181477,4.0820244763973,65.096792692665));
#199890=CARTESIAN_POINT('Ctrl Pts',(-5.50290913960771,3.93830928206788,
65.1050898944474));
#199891=CARTESIAN_POINT('Ctrl Pts',(-5.60577520486862,3.79457689079602,
65.1133880890719));
#199892=CARTESIAN_POINT('Ctrl Pts',(-5.70299279973539,3.64683085277139,
65.1216862836964));
#199893=CARTESIAN_POINT('Ctrl Pts',(-5.7942545278726,3.49555481522288,65.129984478321));
#199894=CARTESIAN_POINT('Ctrl Pts',(-5.88558044144718,3.34417238347352,
65.1382885091626));
#199895=CARTESIAN_POINT('Ctrl Pts',(-5.97094193825195,3.18925528955587,
65.1465925400041));
#199896=CARTESIAN_POINT('Ctrl Pts',(-6.05007667551407,3.03131344806185,
65.1548965708457));
#199897=CARTESIAN_POINT('Ctrl Pts',(-6.12924018834468,2.87331417456723,
65.1632036212614));
#199898=CARTESIAN_POINT('Ctrl Pts',(-6.20217227953624,2.71228827560603,
65.1715106716772));
#199899=CARTESIAN_POINT('Ctrl Pts',(-6.26865830620369,2.54876676847128,
65.1798177220929));
#199900=CARTESIAN_POINT('Ctrl Pts',(-6.33521541765463,2.38507042924754,
65.1881336541475));
#199901=CARTESIAN_POINT('Ctrl Pts',(-6.39531257017017,2.21887347594715,
65.1964495862022));
#199902=CARTESIAN_POINT('Ctrl Pts',(-6.44878429378962,2.05072429452921,
65.2047655182568));
#199903=CARTESIAN_POINT('Ctrl Pts',(-6.48909241483055,1.92396986997085,
65.2110342444758));
#199904=CARTESIAN_POINT('Ctrl Pts',(-6.52563667831421,1.79610645408708,
65.2173029706947));
#199905=CARTESIAN_POINT('Ctrl Pts',(-6.55836535018998,1.66737306366255,
65.2235716969137));
#199906=CARTESIAN_POINT('Ctrl Pts',(-6.60705778437594,1.47584857514759,
65.2328980618821));
#199907=CARTESIAN_POINT('Ctrl Pts',(-6.64737822743416,1.28210408866333,
65.2422244268506));
#199908=CARTESIAN_POINT('Ctrl Pts',(-6.6791523671754,1.0868360759817,65.251550791819));
#199909=CARTESIAN_POINT('Ctrl Pts',(-6.71082043881711,0.8922199049289,65.2608460236139));
#199910=CARTESIAN_POINT('Ctrl Pts',(-6.73399911643487,0.696090530314812,
65.2701412554088));
#199911=CARTESIAN_POINT('Ctrl Pts',(-6.74856552832742,0.499151590071463,
65.2794364872037));
#199912=CARTESIAN_POINT('Ctrl Pts',(-6.76078028658603,0.334007176709741,
65.2872310635324));
#199913=CARTESIAN_POINT('Ctrl Pts',(-6.76693993610197,0.168293790692667,
65.2950256398612));
#199914=CARTESIAN_POINT('Ctrl Pts',(-6.76699956272204,0.00243271858094791,
65.3028202161899));
#199915=CARTESIAN_POINT('Ctrl Pts',(-6.76699956272236,0.00243271768885066,
65.3028202162319));
#199916=CARTESIAN_POINT('Ctrl Pts',(-6.76706085584476,-0.16806406225308,
65.3108326458402));
#199917=CARTESIAN_POINT('Ctrl Pts',(-6.76067426950852,-0.338686686387149,
65.3188450754485));
#199918=CARTESIAN_POINT('Ctrl Pts',(-6.74783765965278,-0.508896766517312,
65.3268575050568));
#199919=CARTESIAN_POINT('Ctrl Pts',(-6.73500553438279,-0.679047382216446,
65.3348671354504));
#199920=CARTESIAN_POINT('Ctrl Pts',(-6.71572789968542,-0.848785364849528,
65.3428767658439));
#199921=CARTESIAN_POINT('Ctrl Pts',(-6.69005467462822,-1.01757429728013,
65.3508863962375));
#199922=CARTESIAN_POINT('Ctrl Pts',(-6.664383039394,-1.18635277740006,65.358895530632));
#199923=CARTESIAN_POINT('Ctrl Pts',(-6.6323166558608,-1.35418195066118,
65.3669046650266));
#199924=CARTESIAN_POINT('Ctrl Pts',(-6.59395706489379,-1.520532546951,65.3749137994211));
#199925=CARTESIAN_POINT('Ctrl Pts',(-6.5818041366329,-1.57323506050504,
65.3774512205269));
#199926=CARTESIAN_POINT('Ctrl Pts',(-6.56901992964328,-1.62578924170528,
65.3799886416327));
#199927=CARTESIAN_POINT('Ctrl Pts',(-6.5556087376292,-1.67817850037464,
65.3825260627384));
#199928=CARTESIAN_POINT('Ctrl Pts',(-6.51005535044735,-1.85612749863156,
65.3911448436755));
#199929=CARTESIAN_POINT('Ctrl Pts',(-6.45726888221967,-2.03215565675692,
65.3997636246127));
#199930=CARTESIAN_POINT('Ctrl Pts',(-6.39744286101652,-2.20567763737787,
65.4083824055498));
#199931=CARTESIAN_POINT('Ctrl Pts',(-6.33758090268591,-2.37930385159831,
65.4170063637363));
#199932=CARTESIAN_POINT('Ctrl Pts',(-6.27067105148898,-2.55042059634021,
65.4256303219227));
#199933=CARTESIAN_POINT('Ctrl Pts',(-6.1969554861256,-2.71846127487183,
65.4342542801092));
#199934=CARTESIAN_POINT('Ctrl Pts',(-6.12057682889995,-2.89257268977132,
65.4431897924804));
#199935=CARTESIAN_POINT('Ctrl Pts',(-6.03689170568422,-3.06338131077366,
65.4521253048515));
#199936=CARTESIAN_POINT('Ctrl Pts',(-5.9462218607113,-3.23028397872371,
65.4610608172227));
#199937=CARTESIAN_POINT('Ctrl Pts',(-5.85854978849024,-3.39166842536938,
65.4697008991173));
#199938=CARTESIAN_POINT('Ctrl Pts',(-5.7643476630778,-3.5494008285431,65.4783409810119));
#199939=CARTESIAN_POINT('Ctrl Pts',(-5.66395122491822,-3.70296442350551,
65.4869810629065));
#199940=CARTESIAN_POINT('Ctrl Pts',(-5.55840550091867,-3.86440422263979,
65.4960642905159));
#199941=CARTESIAN_POINT('Ctrl Pts',(-5.44601359654986,-4.02123602892285,
65.5051475181254));
#199942=CARTESIAN_POINT('Ctrl Pts',(-5.3272147783848,-4.17289727946407,
65.5142307457348));
#199943=CARTESIAN_POINT('Ctrl Pts',(-5.2084159602197,-4.32455853000534,
65.5233139733443));
#199944=CARTESIAN_POINT('Ctrl Pts',(-5.08321050578771,-4.47104895189418,
65.5323972009538));
#199945=CARTESIAN_POINT('Ctrl Pts',(-4.95208416720997,-4.61184902190742,
65.5414804285632));
#199946=CARTESIAN_POINT('Ctrl Pts',(-4.82151553468037,-4.75205024159449,
65.5505250234233));
#199947=CARTESIAN_POINT('Ctrl Pts',(-4.68495634081004,-4.88673948031103,
65.5595696182834));
#199948=CARTESIAN_POINT('Ctrl Pts',(-4.54287434196174,-5.01543434940042,
65.5686142131435));
#199949=CARTESIAN_POINT('Ctrl Pts',(-4.40092272571211,-5.14401112068995,
65.5776505081641));
#199950=CARTESIAN_POINT('Ctrl Pts',(-4.25345859902276,-5.2666043451153,
65.5866868031847));
#199951=CARTESIAN_POINT('Ctrl Pts',(-4.1009854905234,-5.38276945507762,
65.5957230982053));
#199952=CARTESIAN_POINT('Ctrl Pts',(-3.94878219514641,-5.49872900176823,
65.6047434027933));
#199953=CARTESIAN_POINT('Ctrl Pts',(-3.79158780679507,-5.60828300454349,
65.6137637073812));
#199954=CARTESIAN_POINT('Ctrl Pts',(-3.62993757666583,-5.71102812018199,
65.6227840119692));
#199955=CARTESIAN_POINT('Ctrl Pts',(-3.46849091359974,-5.8136438483063,
65.6317929572358));
#199956=CARTESIAN_POINT('Ctrl Pts',(-3.30259980708626,-5.90946767376026,
65.6408019025023));
#199957=CARTESIAN_POINT('Ctrl Pts',(-3.13282913410349,-5.99813892941072,
65.6498108477689));
#199958=CARTESIAN_POINT('Ctrl Pts',(-2.96344397437972,-6.08660883141073,
65.6587993356279));
#199959=CARTESIAN_POINT('Ctrl Pts',(-2.79019704353166,-6.16795847405367,
65.6677878234869));
#199960=CARTESIAN_POINT('Ctrl Pts',(-2.61367805787869,-6.24187279666636,
65.6767763113459));
#199961=CARTESIAN_POINT('Ctrl Pts',(-2.45880694221107,-6.30672244195804,
65.68466247236));
#199962=CARTESIAN_POINT('Ctrl Pts',(-2.30141762078234,-6.36584921646203,
65.692548633374));
#199963=CARTESIAN_POINT('Ctrl Pts',(-2.14192478858306,-6.41906902907683,
65.700434794388));
#199964=CARTESIAN_POINT('Ctrl Pts',(-1.97767307863398,-6.47387679131049,
65.708556259244));
#199965=CARTESIAN_POINT('Ctrl Pts',(-1.81126346644537,-6.52239374843791,
65.7166777240999));
#199966=CARTESIAN_POINT('Ctrl Pts',(-1.64322421643041,-6.56445756894937,
65.7247991889559));
#199967=CARTESIAN_POINT('Ctrl Pts',(-1.47519695008643,-6.60651838969152,
65.7329200746319));
#199968=CARTESIAN_POINT('Ctrl Pts',(-1.30554063263069,-6.64212690155737,
65.741040960308));
#199969=CARTESIAN_POINT('Ctrl Pts',(-1.13479653816351,-6.67117124776243,
65.749161845984));
#199970=CARTESIAN_POINT('Ctrl Pts',(-0.964032034895708,-6.70021906559719,
65.757283702338));
#199971=CARTESIAN_POINT('Ctrl Pts',(-0.792179856911885,-6.72270109521926,
65.7654055586921));
#199972=CARTESIAN_POINT('Ctrl Pts',(-0.61978921934128,-6.7385569911954,
65.7735274150461));
#199973=CARTESIAN_POINT('Ctrl Pts',(-0.447272807694267,-6.75442445543707,
65.781655197006));
#199974=CARTESIAN_POINT('Ctrl Pts',(-0.274217516847378,-6.76365609695529,
65.789782978966));
#199975=CARTESIAN_POINT('Ctrl Pts',(-0.101176049930937,-6.76624359648102,
65.7979107609259));
#199976=CARTESIAN_POINT('Ctrl Pts',(0.0719359076474961,-6.76883215005788,
65.8060418538421));
#199977=CARTESIAN_POINT('Ctrl Pts',(0.245033664242083,-6.76477117525787,
65.8141729467584));
#199978=CARTESIAN_POINT('Ctrl Pts',(0.417567054982159,-6.75410443764335,
65.8223040396746));
#199979=CARTESIAN_POINT('Ctrl Pts',(0.590288758708181,-6.74342605773047,
65.830444007339));
#199980=CARTESIAN_POINT('Ctrl Pts',(0.762444502348168,-6.72612755096827,
65.8385839750033));
#199981=CARTESIAN_POINT('Ctrl Pts',(0.933491004658623,-6.7023043458367,
65.8467239426677));
#199982=CARTESIAN_POINT('Ctrl Pts',(1.02220311636091,-6.68994860160228,
65.8509456818493));
#199983=CARTESIAN_POINT('Ctrl Pts',(1.1106170283355,-6.67583861200521,65.855167421031));
#199984=CARTESIAN_POINT('Ctrl Pts',(1.19865835208879,-6.65999302964859,
65.8593891602127));
#199985=CARTESIAN_POINT('Ctrl Pts',(1.37467282892736,-6.62831413421854,
65.8678293696704));
#199986=CARTESIAN_POINT('Ctrl Pts',(1.5495611299319,-6.5896297672765,65.8762695791281));
#199987=CARTESIAN_POINT('Ctrl Pts',(1.72274483837265,-6.54403844899007,
65.8847097885858));
#199988=CARTESIAN_POINT('Ctrl Pts',(1.89579733449684,-6.49848167288167,
65.8931436033344));
#199989=CARTESIAN_POINT('Ctrl Pts',(2.06714749120149,-6.44602846173389,
65.901577418083));
#199990=CARTESIAN_POINT('Ctrl Pts',(2.23622742046157,-6.38682831489745,
65.9100112328316));
#199991=CARTESIAN_POINT('Ctrl Pts',(2.40520523875857,-6.32766392028798,
65.9184399542203));
#199992=CARTESIAN_POINT('Ctrl Pts',(2.57191524901281,-6.26176082325196,
65.9268686756089));
#199993=CARTESIAN_POINT('Ctrl Pts',(2.73580467884222,-6.18931835982162,
65.9352973969975));
#199994=CARTESIAN_POINT('Ctrl Pts',(2.89962029888659,-6.11690852181844,
65.9437223223993));
#199995=CARTESIAN_POINT('Ctrl Pts',(3.06061756680526,-6.03796532419842,
65.9521472478012));
#199996=CARTESIAN_POINT('Ctrl Pts',(3.21826328826953,-5.95273637979851,
65.960572173203));
#199997=CARTESIAN_POINT('Ctrl Pts',(3.37586219941044,-5.86753274274223,
65.9689945969607));
#199998=CARTESIAN_POINT('Ctrl Pts',(3.53011125567466,-5.77604723944603,
65.9774170207185));
#199999=CARTESIAN_POINT('Ctrl Pts',(3.68050114070233,-5.67857379570688,
65.9858394444762));
#200000=CARTESIAN_POINT('Ctrl Pts',(3.8308933909307,-5.58109881899059,65.9942620006945));
#200001=CARTESIAN_POINT('Ctrl Pts',(3.97742606526254,-5.47763588942274,
66.0026845569128));
#200002=CARTESIAN_POINT('Ctrl Pts',(4.1196175984539,-5.36852305969798,66.0111071131311));
#200003=CARTESIAN_POINT('Ctrl Pts',(4.26181393490254,-5.25940654412089,
66.0195299538649));
#200004=CARTESIAN_POINT('Ctrl Pts',(4.39966857307213,-5.14463995078146,
66.0279527945988));
#200005=CARTESIAN_POINT('Ctrl Pts',(4.5327317823673,-5.02460262997158,66.0363756353326));
#200006=CARTESIAN_POINT('Ctrl Pts',(4.66581806365872,-4.90454449574056,
66.0447999365133));
#200007=CARTESIAN_POINT('Ctrl Pts',(4.79411101204902,-4.77921403542229,
66.0532242376941));
#200008=CARTESIAN_POINT('Ctrl Pts',(4.91719635750109,-4.64902882135377,
66.0616485388748));
#200009=CARTESIAN_POINT('Ctrl Pts',(5.04032023421727,-4.51880285344207,
66.0700754772417));
#200010=CARTESIAN_POINT('Ctrl Pts',(5.15823302871722,-4.38371934408376,
66.0785024156087));
#200011=CARTESIAN_POINT('Ctrl Pts',(5.27055925530196,-4.24423068839936,
66.0869293539756));
#200012=CARTESIAN_POINT('Ctrl Pts',(5.38298647728311,-4.10461661488063,
66.0953638692193));
#200013=CARTESIAN_POINT('Ctrl Pts',(5.48981688513591,-3.96058974081905,
66.103798384463));
#200014=CARTESIAN_POINT('Ctrl Pts',(5.59071633299359,-3.8126342447183,66.1122328997068));
#200015=CARTESIAN_POINT('Ctrl Pts',(5.69166451614895,-3.66460728484547,
66.1206714888936));
#200016=CARTESIAN_POINT('Ctrl Pts',(5.78667584490498,-3.51264819841815,
66.1291100780805));
#200017=CARTESIAN_POINT('Ctrl Pts',(5.87546075862826,-3.35726821594872,
66.1375486672673));
#200018=CARTESIAN_POINT('Ctrl Pts',(5.96434491379795,-3.20171455381279,
66.1459966888877));
#200019=CARTESIAN_POINT('Ctrl Pts',(6.04698858884251,-3.04273264866924,
66.1544447105081));
#200020=CARTESIAN_POINT('Ctrl Pts',(6.12314868321863,-2.88085737293569,
66.1628927321284));
#200021=CARTESIAN_POINT('Ctrl Pts',(6.16643685860994,-2.78885006405733,
66.1676944520397));
#200022=CARTESIAN_POINT('Ctrl Pts',(6.20763132310783,-2.69590839671385,
66.172496171951));
#200023=CARTESIAN_POINT('Ctrl Pts',(6.24669448972815,-2.6021331541641,66.1772978918623));
#200024=CARTESIAN_POINT('Ctrl Pts',(6.3137250978264,-2.4412191250029,66.1855374237134));
#200025=CARTESIAN_POINT('Ctrl Pts',(6.37462691919696,-2.27749044476659,
66.1937769555645));
#200026=CARTESIAN_POINT('Ctrl Pts',(6.42915679304084,-2.11145256411241,
66.2020164874156));
#200027=CARTESIAN_POINT('Ctrl Pts',(6.48362614253585,-1.94559897390137,
66.2102468739621));
#200028=CARTESIAN_POINT('Ctrl Pts',(6.53173751680025,-1.77744162189617,
66.2184772605087));
#200029=CARTESIAN_POINT('Ctrl Pts',(6.57329515882468,-1.60750731101666,
66.2267076470553));
#200030=CARTESIAN_POINT('Ctrl Pts',(6.61481408827214,-1.43773130062703,
66.2349303666733));
#200031=CARTESIAN_POINT('Ctrl Pts',(6.64979135976002,-1.26618197162173,
66.2431530862913));
#200032=CARTESIAN_POINT('Ctrl Pts',(6.67808050927068,-1.09340281310184,
66.2513758059093));
#200033=CARTESIAN_POINT('Ctrl Pts',(6.70634459255683,-0.920776749364022,
66.2595912396054));
#200034=CARTESIAN_POINT('Ctrl Pts',(6.72793230796884,-0.746923377912297,
66.2678066733014));
#200035=CARTESIAN_POINT('Ctrl Pts',(6.74274793650412,-0.572397820374476,
66.2760221069974));
#200036=CARTESIAN_POINT('Ctrl Pts',(6.75755595095667,-0.397961955422491,
66.2842333185984));
#200037=CARTESIAN_POINT('Ctrl Pts',(6.76559877987904,-0.222854946145419,
66.2924445301994));
#200038=CARTESIAN_POINT('Ctrl Pts',(6.76683231159713,-0.047638920275371,
66.3006557418004));
#200039=CARTESIAN_POINT('Ctrl Pts',(6.76806542965676,0.12751834780896,66.3088641998142));
#200040=CARTESIAN_POINT('Ctrl Pts',(6.76249379686454,0.302784204143018,
66.3170726578279));
#200041=CARTESIAN_POINT('Ctrl Pts',(6.7501253668455,0.47759452663206,66.3252811158417));
#200042=CARTESIAN_POINT('Ctrl Pts',(6.74461496119987,0.555476342390058,
66.3289381631235));
#200043=CARTESIAN_POINT('Ctrl Pts',(6.7377561528153,0.633267737723453,66.3325952104053));
#200044=CARTESIAN_POINT('Ctrl Pts',(6.72955297553951,0.710918947143271,
66.336252257687));
#200045=CARTESIAN_POINT('Ctrl Pts',(6.70968105418944,0.899026393130531,
66.3451113318621));
#200046=CARTESIAN_POINT('Ctrl Pts',(6.68193730666842,1.08611529098033,66.3539704060371));
#200047=CARTESIAN_POINT('Ctrl Pts',(6.6464619186312,1.27154746831774,66.3628294802121));
#200048=CARTESIAN_POINT('Ctrl Pts',(6.61091987947707,1.45732803540973,66.3717051988051));
#200049=CARTESIAN_POINT('Ctrl Pts',(6.56761721875264,1.64144540693416,66.3805809173982));
#200050=CARTESIAN_POINT('Ctrl Pts',(6.51674444183085,1.82327476806617,66.3894566359913));
#200051=CARTESIAN_POINT('Ctrl Pts',(6.4657264883781,2.00562301881799,66.3983576833773));
#200052=CARTESIAN_POINT('Ctrl Pts',(6.40709525846708,2.1856699418529,66.4072587307633));
#200053=CARTESIAN_POINT('Ctrl Pts',(6.34109111968594,2.36280604617479,66.4161597781494));
#200054=CARTESIAN_POINT('Ctrl Pts',(6.27499724737285,2.54018296946001,66.4250729266314));
#200055=CARTESIAN_POINT('Ctrl Pts',(6.20151054009244,2.714640928483,66.4339860751134));
#200056=CARTESIAN_POINT('Ctrl Pts',(6.12091879831441,2.88559215143812,66.4428992235955));
#200057=CARTESIAN_POINT('Ctrl Pts',(6.04014812083256,3.05692293285325,66.4518321617044));
#200058=CARTESIAN_POINT('Ctrl Pts',(5.95224096672325,3.22473116949826,66.4607650998133));
#200059=CARTESIAN_POINT('Ctrl Pts',(5.8575316046697,3.38845281807135,66.4696980379221));
#200060=CARTESIAN_POINT('Ctrl Pts',(5.76738202422048,3.54429208896595,66.4782008997854));
#200061=CARTESIAN_POINT('Ctrl Pts',(5.67106989706527,3.69642884877683,66.4867037616486));
#200062=CARTESIAN_POINT('Ctrl Pts',(5.56891896833363,3.84440249247317,66.4952066235118));
#200063=CARTESIAN_POINT('Ctrl Pts',(5.4701325162687,3.98750242745548,66.5034294323134));
#200064=CARTESIAN_POINT('Ctrl Pts',(5.36569539072126,4.1269826741663,66.511652241115));
#200065=CARTESIAN_POINT('Ctrl Pts',(5.25590168574291,4.26236864546051,66.5198750499166));
#200066=CARTESIAN_POINT('Ctrl Pts',(5.14622034499035,4.39761606108934,66.5280894433947));
#200067=CARTESIAN_POINT('Ctrl Pts',(5.03119356381535,4.52877726773737,66.5363038368728));
#200068=CARTESIAN_POINT('Ctrl Pts',(4.91115889954411,4.65540624042937,66.5445182303509));
#200069=CARTESIAN_POINT('Ctrl Pts',(4.79122524308017,4.78192865627839,66.5527257115102));
#200070=CARTESIAN_POINT('Ctrl Pts',(4.66629234101214,4.9039261742029,66.5609331926694));
#200071=CARTESIAN_POINT('Ctrl Pts',(4.53673826381348,5.02098545363863,66.5691406738287));
#200072=CARTESIAN_POINT('Ctrl Pts',(4.40728078818542,5.13795744820852,66.5773420351066));
#200073=CARTESIAN_POINT('Ctrl Pts',(4.27320926950222,5.24999830259124,66.5855433963846));
#200074=CARTESIAN_POINT('Ctrl Pts',(4.13493883468289,5.35673126388017,66.5937447576626));
#200075=CARTESIAN_POINT('Ctrl Pts',(3.99672785226157,5.4634183329977,66.6019425925859));
#200076=CARTESIAN_POINT('Ctrl Pts',(3.85432183299172,5.56480183594365,66.6101404275092));
#200077=CARTESIAN_POINT('Ctrl Pts',(3.70816941121728,5.66054490466355,66.6183382624324));
#200078=CARTESIAN_POINT('Ctrl Pts',(3.56204877618386,5.75626715019016,66.6265343144058));
#200079=CARTESIAN_POINT('Ctrl Pts',(3.4121836610716,5.84635120811245,66.6347303663791));
#200080=CARTESIAN_POINT('Ctrl Pts',(3.25905222577131,5.93050314810599,66.6429264183524));
#200081=CARTESIAN_POINT('Ctrl Pts',(3.20612009010448,5.95959150540919,66.6457595044142));
#200082=CARTESIAN_POINT('Ctrl Pts',(3.15279792204455,5.98797145751809,66.6485925904762));
#200083=CARTESIAN_POINT('Ctrl Pts',(3.09910619832135,6.0156321173694,66.651425676538));
#200084=CARTESIAN_POINT('Origin',(0.,0.,4.30282021618968));
#200085=CARTESIAN_POINT('',(3.09910619832131,6.01563211736941,69.0457552630242));
#200086=CARTESIAN_POINT('',(3.09910619832137,6.01563211736939,68.6512130080706));
#200087=CARTESIAN_POINT('',(3.09910619832133,6.0156321173694,4.30282021618968));
#200088=CARTESIAN_POINT('',(-6.76699999999839,-4.66729631973904E-6,67.6970790042622));
#200089=CARTESIAN_POINT('Ctrl Pts',(-6.767,2.1130229668672E-12,67.69717978381));
#200090=CARTESIAN_POINT('Ctrl Pts',(-6.76700000000006,-0.186007249524881,
67.7059292956212));
#200091=CARTESIAN_POINT('Ctrl Pts',(-6.75932637294531,-0.372014355748052,
67.7146788074324));
#200092=CARTESIAN_POINT('Ctrl Pts',(-6.74400518264195,-0.557389537485753,
67.7234283192436));
#200093=CARTESIAN_POINT('Ctrl Pts',(-6.72868405705103,-0.742763936250253,
67.7321777940992));
#200094=CARTESIAN_POINT('Ctrl Pts',(-6.70571545645744,-0.927506130240924,
67.7409272689549));
#200095=CARTESIAN_POINT('Ctrl Pts',(-6.6751773940482,-1.11098863990046,
67.7496767438106));
#200096=CARTESIAN_POINT('Ctrl Pts',(-6.64463945808692,-1.29447038982,67.7584261824376));
#200097=CARTESIAN_POINT('Ctrl Pts',(-6.60653217008338,-1.47669218313759,
67.7671756210647));
#200098=CARTESIAN_POINT('Ctrl Pts',(-6.56098496092652,-1.65703510599384,
67.7759250596917));
#200099=CARTESIAN_POINT('Ctrl Pts',(-6.51543793658267,-1.83737729708808,
67.7846744628169));
#200100=CARTESIAN_POINT('Ctrl Pts',(-6.46245112167384,-2.01584035511044,
67.793423865942));
#200101=CARTESIAN_POINT('Ctrl Pts',(-6.4022044837421,-2.19181813760918,
67.8021732690672));
#200102=CARTESIAN_POINT('Ctrl Pts',(-6.3419580852645,-2.3677952206729,67.8109226374173));
#200103=CARTESIAN_POINT('Ctrl Pts',(-6.27445201433038,-2.5412867768433,
67.8196720057674));
#200104=CARTESIAN_POINT('Ctrl Pts',(-6.19991555071822,-2.71170355384994,
67.8284213741175));
#200105=CARTESIAN_POINT('Ctrl Pts',(-6.1253793771661,-2.88211966767651,
67.8371707084193));
#200106=CARTESIAN_POINT('Ctrl Pts',(-6.04381298052437,-3.0494607637195,
67.8459200427211));
#200107=CARTESIAN_POINT('Ctrl Pts',(-5.95549339335747,-3.21315848374703,
67.8546693770228));
#200108=CARTESIAN_POINT('Ctrl Pts',(-5.86717414255332,-3.37685558033625,
67.863418678003));
#200109=CARTESIAN_POINT('Ctrl Pts',(-5.7721018887653,-3.53690907646867,
67.8721679789832));
#200110=CARTESIAN_POINT('Ctrl Pts',(-5.67059953346938,-3.69277536969376,
67.8809172799634));
#200111=CARTESIAN_POINT('Ctrl Pts',(-5.56909755631334,-3.84864108224995,
67.8896665483486));
#200112=CARTESIAN_POINT('Ctrl Pts',(-5.4611656819681,-4.00031938297571,
67.8984158167339));
#200113=CARTESIAN_POINT('Ctrl Pts',(-5.34717048533573,-4.14729511859892,
67.9071650851192));
#200114=CARTESIAN_POINT('Ctrl Pts',(-5.2331757039181,-4.29427031887948,
67.9159143216362));
#200115=CARTESIAN_POINT('Ctrl Pts',(-5.11311782003492,-4.43654276189572,
67.9246635581532));
#200116=CARTESIAN_POINT('Ctrl Pts',(-4.98740458984735,-4.57362924351871,
67.9334127946703));
#200117=CARTESIAN_POINT('Ctrl Pts',(-4.86169180711733,-4.71071523720276,
67.9421620000457));
#200118=CARTESIAN_POINT('Ctrl Pts',(-4.7303239120417,-4.84261509523238,
67.9509112054212));
#200119=CARTESIAN_POINT('Ctrl Pts',(-4.59374707013607,-4.96888084538322,
67.9596604107966));
#200120=CARTESIAN_POINT('Ctrl Pts',(-4.45717070301462,-5.09514615659448,
67.9684095857571));
#200121=CARTESIAN_POINT('Ctrl Pts',(-4.31538563571067,-5.21577720459505,
67.9771587607175));
#200122=CARTESIAN_POINT('Ctrl Pts',(-4.16887341029545,-5.33036429232858,
67.9859079356779));
#200123=CARTESIAN_POINT('Ctrl Pts',(-4.02236168203755,-5.44495099123579,
67.9946570809499));
#200124=CARTESIAN_POINT('Ctrl Pts',(-3.87112305348227,-5.55349359438558,
68.003406226222));
#200125=CARTESIAN_POINT('Ctrl Pts',(-3.71567117017836,-5.65562346298844,
68.012155371494));
#200126=CARTESIAN_POINT('Ctrl Pts',(-3.56021980145894,-5.75775299351597,
68.0209044878041));
#200127=CARTESIAN_POINT('Ctrl Pts',(-3.40055544538425,-5.85346967463829,
68.0296536041143));
#200128=CARTESIAN_POINT('Ctrl Pts',(-3.23722035986929,-5.9424484298686,
68.0384027204245));
#200129=CARTESIAN_POINT('Ctrl Pts',(-3.07388580147251,-6.03142689794493,
68.0471518084993));
#200130=CARTESIAN_POINT('Ctrl Pts',(-2.90688078896643,-6.11366734656751,
68.0559008965742));
#200131=CARTESIAN_POINT('Ctrl Pts',(-2.7367725072143,-6.18889046952327,
68.064649984649));
#200132=CARTESIAN_POINT('Ctrl Pts',(-2.56666476031555,-6.26411335596296,
68.0733990452151));
#200133=CARTESIAN_POINT('Ctrl Pts',(-2.39345402575253,-6.33231884500522,
68.0821481057811));
#200134=CARTESIAN_POINT('Ctrl Pts',(-2.21772856065693,-6.39327529762692,
68.0908971663471));
#200135=CARTESIAN_POINT('Ctrl Pts',(-2.0420036334863,-6.45423156365074,
68.0996462001308));
#200136=CARTESIAN_POINT('Ctrl Pts',(-1.8637642618941,-6.5079387437562,68.1083952339145));
#200137=CARTESIAN_POINT('Ctrl Pts',(-1.683615777533,-6.55421443909504,68.1171442676981));
#200138=CARTESIAN_POINT('Ctrl Pts',(-1.50346782967971,-6.60048999661828,
68.125893275426));
#200139=CARTESIAN_POINT('Ctrl Pts',(-1.32141105795185,-6.63933404237672,
68.1346422831538));
#200140=CARTESIAN_POINT('Ctrl Pts',(-1.13806375487247,-6.67061465607522,
68.1433912908816));
#200141=CARTESIAN_POINT('Ctrl Pts',(-0.954716982605532,-6.7018951792126,
68.15214027328));
#200142=CARTESIAN_POINT('Ctrl Pts',(-0.77007996890492,-6.72561226592196,
68.1608892556784));
#200143=CARTESIAN_POINT('Ctrl Pts',(-0.584779765561294,-6.74168536983076,
68.1696382380768));
#200144=CARTESIAN_POINT('Ctrl Pts',(-0.391489830654349,-6.75845151013835,
68.1787644570866));
#200145=CARTESIAN_POINT('Ctrl Pts',(-0.197478578241385,-6.76689983031616,
68.1878906760965));
#200146=CARTESIAN_POINT('Ctrl Pts',(-0.00346287645438857,-6.76699911397118,
68.1970168951064));
#200147=CARTESIAN_POINT('Ctrl Pts',(0.184489834651796,-6.76709529501197,
68.2058579197722));
#200148=CARTESIAN_POINT('Ctrl Pts',(0.372446404247341,-6.7593563973818,
68.214698944438));
#200149=CARTESIAN_POINT('Ctrl Pts',(0.55975501948637,-6.74380925873203,
68.2235399691038));
#200150=CARTESIAN_POINT('Ctrl Pts',(0.745134705519926,-6.72842222659826,
68.2322899477135));
#200151=CARTESIAN_POINT('Ctrl Pts',(0.929879431226838,-6.70538706057548,
68.2410399263233));
#200152=CARTESIAN_POINT('Ctrl Pts',(1.11336163626664,-6.67478200894154,
68.2497899049331));
#200153=CARTESIAN_POINT('Ctrl Pts',(1.29684196300578,-6.64417727061041,
68.2585397939696));
#200154=CARTESIAN_POINT('Ctrl Pts',(1.47905951217389,-6.60600284890618,
68.2672896830061));
#200155=CARTESIAN_POINT('Ctrl Pts',(1.65939532066983,-6.56038841607256,
68.2760395720427));
#200156=CARTESIAN_POINT('Ctrl Pts',(1.83972934300704,-6.51477443503284,
68.2847893744148));
#200157=CARTESIAN_POINT('Ctrl Pts',(2.0181813840617,-6.46172066062171,68.293539176787));
#200158=CARTESIAN_POINT('Ctrl Pts',(2.19414528354108,-6.4014073042351,68.3022889791591));
#200159=CARTESIAN_POINT('Ctrl Pts',(2.37010749863917,-6.34109452518673,
68.3110386977754));
#200160=CARTESIAN_POINT('Ctrl Pts',(2.54358134866386,-6.27352239616534,
68.3197884163918));
#200161=CARTESIAN_POINT('Ctrl Pts',(2.71397759435491,-6.19892043966847,
68.3285381350081));
#200162=CARTESIAN_POINT('Ctrl Pts',(2.88437226558068,-6.12431917249542,
68.3372877727768));
#200163=CARTESIAN_POINT('Ctrl Pts',(3.05168912680908,-6.04268832278823,
68.3460374105455));
#200164=CARTESIAN_POINT('Ctrl Pts',(3.21535986273816,-5.95430516123355,
68.3547870483143));
#200165=CARTESIAN_POINT('Ctrl Pts',(3.37902914072811,-5.86592278697458,
68.3635366081433));
#200166=CARTESIAN_POINT('Ctrl Pts',(3.5390521062155,-5.77078835741955,68.3722861679724));
#200167=CARTESIAN_POINT('Ctrl Pts',(3.69488522831682,-5.66922500431639,
68.3810357278015));
#200168=CARTESIAN_POINT('Ctrl Pts',(3.85071701406938,-5.56766252217095,
68.3897852125986));
#200169=CARTESIAN_POINT('Ctrl Pts',(4.00235878822414,-5.45967138329363,
68.3985346973957));
#200170=CARTESIAN_POINT('Ctrl Pts',(4.14929549611346,-5.34561838199591,
68.4072841821928));
#200171=CARTESIAN_POINT('Ctrl Pts',(4.29623099276113,-5.23156632086997,
68.4160335948654));
#200172=CARTESIAN_POINT('Ctrl Pts',(4.43846127436053,-5.11145267304943,
68.424783007538));
#200173=CARTESIAN_POINT('Ctrl Pts',(4.57550326054469,-4.98568540049861,
68.4335324202106));
#200174=CARTESIAN_POINT('Ctrl Pts',(4.71254416257801,-4.85991912290341,
68.4422817636658));
#200175=CARTESIAN_POINT('Ctrl Pts',(4.84439664018775,-4.72849950385404,
68.4510311071211));
#200176=CARTESIAN_POINT('Ctrl Pts',(4.97061286794753,-4.59187289861059,
68.4597804505763));
#200177=CARTESIAN_POINT('Ctrl Pts',(5.09682813912688,-4.4552473288468,68.4685297277211));
#200178=CARTESIAN_POINT('Ctrl Pts',(5.21740705147838,-4.31341506235788,
68.477279004866));
#200179=CARTESIAN_POINT('Ctrl Pts',(5.33194007545692,-4.16685781275729,
68.4860282820108));
#200180=CARTESIAN_POINT('Ctrl Pts',(5.44647226944478,-4.02030162521851,
68.4947774957519));
#200181=CARTESIAN_POINT('Ctrl Pts',(5.55495848628103,-3.86902074887949,
68.503526709493));
#200182=CARTESIAN_POINT('Ctrl Pts',(5.65703027291775,-3.71352898080683,
68.5122759232341));
#200183=CARTESIAN_POINT('Ctrl Pts',(5.75910135376981,-3.55803828789614,
68.521025076478));
#200184=CARTESIAN_POINT('Ctrl Pts',(5.85475793592734,-3.39833700106744,
68.5297742297219));
#200185=CARTESIAN_POINT('Ctrl Pts',(5.94367514427378,-3.23496750823591,
68.5385233829658));
#200186=CARTESIAN_POINT('Ctrl Pts',(6.03259176732621,-3.07159909077763,
68.5472724786187));
#200187=CARTESIAN_POINT('Ctrl Pts',(6.11476896835906,-2.90456276731473,
68.5560215742716));
#200188=CARTESIAN_POINT('Ctrl Pts',(6.18992765547868,-2.7344258300309,68.5647706699246));
#200189=CARTESIAN_POINT('Ctrl Pts',(6.26508587283039,-2.56428995616207,
68.5735197108926));
#200190=CARTESIAN_POINT('Ctrl Pts',(6.33322554827147,-2.39105376935236,
68.5822687518606));
#200191=CARTESIAN_POINT('Ctrl Pts',(6.3941152673302,-2.21530561054111,68.5910177928287));
#200192=CARTESIAN_POINT('Ctrl Pts',(6.45500462602829,-2.03955849185153,
68.5997667820177));
#200193=CARTESIAN_POINT('Ctrl Pts',(6.50864402040717,-1.86129970164624,
68.6085157712067));
#200194=CARTESIAN_POINT('Ctrl Pts',(6.55485128368574,-1.68113463136163,
68.6172647603957));
#200195=CARTESIAN_POINT('Ctrl Pts',(6.601998095543,-1.49730620116987,68.6261916458672));
#200196=CARTESIAN_POINT('Ctrl Pts',(6.64140720707847,-1.31149343245829,
68.6351185313386));
#200197=CARTESIAN_POINT('Ctrl Pts',(6.67293928722859,-1.12435326697669,
68.64404541681));
#200198=CARTESIAN_POINT('Ctrl Pts',(6.70384625876235,-0.940923067008094,
68.6527953309875));
#200199=CARTESIAN_POINT('Ctrl Pts',(6.72718554579778,-0.756217899523231,
68.6615452451649));
#200200=CARTESIAN_POINT('Ctrl Pts',(6.74287786815314,-0.570865181256125,
68.6702951593424));
#200201=CARTESIAN_POINT('Ctrl Pts',(6.75856988190837,-0.385516108075555,
68.6790449014469));
#200202=CARTESIAN_POINT('Ctrl Pts',(6.76661520773398,-0.199519795227935,
68.6877946435514));
#200203=CARTESIAN_POINT('Ctrl Pts',(6.76698651789579,-0.0135080204572116,
68.6965443856559));
#200204=CARTESIAN_POINT('Ctrl Pts',(6.76735782124907,0.17250034351142,68.7052939673208));
#200205=CARTESIAN_POINT('Ctrl Pts',(6.76005538995192,0.358523882209404,
68.7140435489858));
#200206=CARTESIAN_POINT('Ctrl Pts',(6.74510402742373,0.543930748562886,
68.7227931306508));
#200207=CARTESIAN_POINT('Ctrl Pts',(6.73015291918047,0.729334461613647,
68.7315425635074));
#200208=CARTESIAN_POINT('Ctrl Pts',(6.70755316306617,0.914121237632997,
68.7402919963641));
#200209=CARTESIAN_POINT('Ctrl Pts',(6.67738151874603,1.09766345165944,68.7490414292208));
#200210=CARTESIAN_POINT('Ctrl Pts',(6.64721034747604,1.28120278799484,68.7577907248983));
#200211=CARTESIAN_POINT('Ctrl Pts',(6.60946757205182,1.46349731860147,68.7665400205758));
#200212=CARTESIAN_POINT('Ctrl Pts',(6.56428138111569,1.64392790277978,68.7752893162534));
#200213=CARTESIAN_POINT('Ctrl Pts',(6.51909583859903,1.82435589778866,68.784038486379));
#200214=CARTESIAN_POINT('Ctrl Pts',(6.46646716392936,2.00291972192069,68.7927876565046));
#200215=CARTESIAN_POINT('Ctrl Pts',(6.40657409872952,2.17901292274462,68.8015368266302));
#200216=CARTESIAN_POINT('Ctrl Pts',(6.34668181342152,2.35510383058773,68.8102858828293));
#200217=CARTESIAN_POINT('Ctrl Pts',(6.27952541914134,2.52872390822373,68.8190349390284));
#200218=CARTESIAN_POINT('Ctrl Pts',(6.20533299175608,2.69928350890075,68.8277839952275));
#200219=CARTESIAN_POINT('Ctrl Pts',(6.12831602991641,2.87633637965428,68.8368661313857));
#200220=CARTESIAN_POINT('Ctrl Pts',(6.04371690605362,3.05009086601281,68.8459482675439));
#200221=CARTESIAN_POINT('Ctrl Pts',(5.95184520316721,3.21991112882568,68.8550304037021));
#200222=CARTESIAN_POINT('Ctrl Pts',(5.86333549509366,3.38351691182858,68.8637801840457));
#200223=CARTESIAN_POINT('Ctrl Pts',(5.76807618099461,3.54347103711853,68.8725299643892));
#200224=CARTESIAN_POINT('Ctrl Pts',(5.66639083309109,3.69923018027552,68.8812797447328));
#200225=CARTESIAN_POINT('Ctrl Pts',(5.56470914082296,3.85498372381912,68.8900292105177));
#200226=CARTESIAN_POINT('Ctrl Pts',(5.45660203372165,4.00654234701864,68.8987786763026));
#200227=CARTESIAN_POINT('Ctrl Pts',(5.34243669839317,4.1533912798654,68.9075281420876));
#200228=CARTESIAN_POINT('Ctrl Pts',(5.228274860507,4.30023571401148,68.9162773398336));
#200229=CARTESIAN_POINT('Ctrl Pts',(5.10805534167227,4.44237052028335,68.9250265375796));
#200230=CARTESIAN_POINT('Ctrl Pts',(4.98218644340076,4.57931296628585,68.9337757353256));
#200231=CARTESIAN_POINT('Ctrl Pts',(4.85632073219728,4.71625194483214,68.9425247115372));
#200232=CARTESIAN_POINT('Ctrl Pts',(4.72480612170478,4.84799861524352,68.9512736877488));
#200233=CARTESIAN_POINT('Ctrl Pts',(4.58808925235489,4.97410554898321,68.9600226639604));
#200234=CARTESIAN_POINT('Ctrl Pts',(4.45136349474231,5.10022068121047,68.9687722089622));
#200235=CARTESIAN_POINT('Ctrl Pts',(4.30943501210268,5.22069514871679,68.9775217539639));
#200236=CARTESIAN_POINT('Ctrl Pts',(4.16278587431975,5.33511975166106,68.9862712989656));
#200237=CARTESIAN_POINT('Ctrl Pts',(4.01614535740648,5.44953762807695,68.9950203296193));
#200238=CARTESIAN_POINT('Ctrl Pts',(3.8647849665813,5.5579061753264,69.003769360273));
#200239=CARTESIAN_POINT('Ctrl Pts',(3.70921874747409,5.65985735539216,69.0125183909267));
#200240=CARTESIAN_POINT('Ctrl Pts',(3.55365041606115,5.76180991976914,69.0212675403763));
#200241=CARTESIAN_POINT('Ctrl Pts',(3.39387638174737,5.85734478552689,69.030016689826));
#200242=CARTESIAN_POINT('Ctrl Pts',(3.23043927904753,5.94613749121116,69.0387658392756));
#200243=CARTESIAN_POINT('Ctrl Pts',(3.18691767070571,5.96978206944073,69.0410956471918));
#200244=CARTESIAN_POINT('Ctrl Pts',(3.14313645919698,5.99294880633391,69.043425455108));
#200245=CARTESIAN_POINT('Ctrl Pts',(3.09910619832131,6.01563211736941,69.0457552630242));
#200246=CARTESIAN_POINT('Ctrl Pts',(3.09910619832127,6.01563211736944,67.045599963736));
#200247=CARTESIAN_POINT('Ctrl Pts',(2.93588559344356,6.09971937177612,67.0542442724815));
#200248=CARTESIAN_POINT('Ctrl Pts',(2.76932797444242,6.17711490518632,67.062888581227));
#200249=CARTESIAN_POINT('Ctrl Pts',(2.60000172269813,6.2475819355945,67.0715328899725));
#200250=CARTESIAN_POINT('Ctrl Pts',(2.4304853058764,6.31812810534557,67.0801869068738));
#200251=CARTESIAN_POINT('Ctrl Pts',(2.25819432564532,6.38173011083379,67.0888409237752));
#200252=CARTESIAN_POINT('Ctrl Pts',(2.0837152003389,6.43820005621731,67.0974949406765));
#200253=CARTESIAN_POINT('Ctrl Pts',(2.02418527645254,6.45746683982048,67.1004475745033));
#200254=CARTESIAN_POINT('Ctrl Pts',(1.96440075258064,6.47590382425444,67.1034002083301));
#200255=CARTESIAN_POINT('Ctrl Pts',(1.90438525386509,6.49350489372736,67.1063528421569));
#200256=CARTESIAN_POINT('Ctrl Pts',(1.72054400935479,6.54742100849549,67.1153974371184));
#200257=CARTESIAN_POINT('Ctrl Pts',(1.53436482360287,6.59353950868748,67.12444203208));
#200258=CARTESIAN_POINT('Ctrl Pts',(1.34649615449113,6.63168433400902,67.1334866270416));
#200259=CARTESIAN_POINT('Ctrl Pts',(1.15879988446168,6.66979415544773,67.1425229221633));
#200260=CARTESIAN_POINT('Ctrl Pts',(0.96941745932348,6.69994486335135,67.151559217285));
#200261=CARTESIAN_POINT('Ctrl Pts',(0.779008793363627,6.72201117968887,
67.1605955124067));
#200262=CARTESIAN_POINT('Ctrl Pts',(0.58893707052117,6.74403844794327,67.1696158170932));
#200263=CARTESIAN_POINT('Ctrl Pts',(0.397842969209742,6.75800986447361,
67.1786361217796));
#200264=CARTESIAN_POINT('Ctrl Pts',(0.206392640552195,6.76385179301897,
67.1876564264661));
#200265=CARTESIAN_POINT('Ctrl Pts',(0.0151834064377996,6.76968636478879,
67.1966653718289));
#200266=CARTESIAN_POINT('Ctrl Pts',(-0.176380922700902,6.76741187189506,
67.2056743171917));
#200267=CARTESIAN_POINT('Ctrl Pts',(-0.367630502967207,6.75700649794627,
67.2146832625546));
#200268=CARTESIAN_POINT('Ctrl Pts',(-0.558445795822093,6.74662475240445,
67.2236717505048));
#200269=CARTESIAN_POINT('Ctrl Pts',(-0.748947529360054,6.72814899347496,
67.2326602384551));
#200270=CARTESIAN_POINT('Ctrl Pts',(-0.938467778612769,6.70160930139214,
67.2416487264054));
#200271=CARTESIAN_POINT('Ctrl Pts',(-1.10474570174047,6.67832437591647,
67.2495348869309));
#200272=CARTESIAN_POINT('Ctrl Pts',(-1.27026797150988,6.64883287419998,
67.2574210474564));
#200273=CARTESIAN_POINT('Ctrl Pts',(-1.43458401800579,6.61318816421266,
67.2653072079818));
#200274=CARTESIAN_POINT('Ctrl Pts',(-1.60380286441234,6.57647990088002,
67.2734286727758));
#200275=CARTESIAN_POINT('Ctrl Pts',(-1.7716663356137,6.53326059095723,67.2815501375697));
#200276=CARTESIAN_POINT('Ctrl Pts',(-1.93763730760377,6.4836602829098,67.2896716023637));
#200277=CARTESIAN_POINT('Ctrl Pts',(-2.10359644341587,6.43406351209582,
67.2977924879774));
#200278=CARTESIAN_POINT('Ctrl Pts',(-2.26766299798987,6.37808675442341,
67.3059133735911));
#200279=CARTESIAN_POINT('Ctrl Pts',(-2.42931442370919,6.31591010312516,
67.3140342592048));
#200280=CARTESIAN_POINT('Ctrl Pts',(-2.59098517139225,6.2537260199407,67.3221561154964));
#200281=CARTESIAN_POINT('Ctrl Pts',(-2.75023987405961,6.18534070007898,
67.330277971788));
#200282=CARTESIAN_POINT('Ctrl Pts',(-2.90657544825129,6.11098258577316,
67.3383998280796));
#200283=CARTESIAN_POINT('Ctrl Pts',(-3.06302508294209,6.03657022070787,
67.3465276099769));
#200284=CARTESIAN_POINT('Ctrl Pts',(-3.21655100441934,5.9561765151777,67.3546553918742));
#200285=CARTESIAN_POINT('Ctrl Pts',(-3.36667368540554,5.87007643016664,
67.3627831737716));
#200286=CARTESIAN_POINT('Ctrl Pts',(-3.5168575207906,5.78394127118204,67.3709142666251));
#200287=CARTESIAN_POINT('Ctrl Pts',(-3.66363504208972,5.6920952933114,67.3790453594787));
#200288=CARTESIAN_POINT('Ctrl Pts',(-3.80655549026008,5.59485695076924,
67.3871764523322));
#200289=CARTESIAN_POINT('Ctrl Pts',(-3.94963193013018,5.4975124766376,67.3953164199339));
#200290=CARTESIAN_POINT('Ctrl Pts',(-4.08884259415968,5.39476409964222,
67.4034563875357));
#200291=CARTESIAN_POINT('Ctrl Pts',(-4.2237690128558,5.28697118642037,67.4115963551374));
#200292=CARTESIAN_POINT('Ctrl Pts',(-4.29374769420603,5.23106511554811,
67.4158180946938));
#200293=CARTESIAN_POINT('Ctrl Pts',(-4.36257453206647,5.1738027417705,67.4200398342501));
#200294=CARTESIAN_POINT('Ctrl Pts',(-4.43019507901427,5.11523807479943,
67.4242615738065));
#200295=CARTESIAN_POINT('Ctrl Pts',(-4.56329035016489,4.99996719069407,
67.4325710832136));
#200296=CARTESIAN_POINT('Ctrl Pts',(-4.69201063712768,4.87938866675348,
67.4408805926207));
#200297=CARTESIAN_POINT('Ctrl Pts',(-4.81591620892539,4.7538658025453,67.4491901020279));
#200298=CARTESIAN_POINT('Ctrl Pts',(-4.93971855124055,4.62844751523495,
67.4574926885312));
#200299=CARTESIAN_POINT('Ctrl Pts',(-5.05871392679581,4.49809334240074,
67.4657952750345));
#200300=CARTESIAN_POINT('Ctrl Pts',(-5.17249707351925,4.36320559043862,
67.4740978615378));
#200301=CARTESIAN_POINT('Ctrl Pts',(-5.28620647825334,4.2284052581995,67.4823950671982));
#200302=CARTESIAN_POINT('Ctrl Pts',(-5.394710161456,4.08907746784305,67.4906922728585));
#200303=CARTESIAN_POINT('Ctrl Pts',(-5.49764087114487,3.94566012878929,
67.4989894785188));
#200304=CARTESIAN_POINT('Ctrl Pts',(-5.60052808452494,3.80230339482496,
67.5072831779581));
#200305=CARTESIAN_POINT('Ctrl Pts',(-5.69784681356272,3.65486083838874,
67.5155768773975));
#200306=CARTESIAN_POINT('Ctrl Pts',(-5.78927097556485,3.50380230199743,
67.5238705768368));
#200307=CARTESIAN_POINT('Ctrl Pts',(-5.88067469871569,3.35277753636094,
67.5321624221307));
#200308=CARTESIAN_POINT('Ctrl Pts',(-5.96618629940749,3.19813869939004,
67.5404542674246));
#200309=CARTESIAN_POINT('Ctrl Pts',(-6.045523690687,3.0403835786529,67.5487461127185));
#200310=CARTESIAN_POINT('Ctrl Pts',(-6.12485665051338,2.88263726945358,
67.5570374948648));
#200311=CARTESIAN_POINT('Ctrl Pts',(-6.19801593138472,2.72177533498301,
67.5653288770111));
#200312=CARTESIAN_POINT('Ctrl Pts',(-6.26476589907955,2.55831921966943,
67.5736202591574));
#200313=CARTESIAN_POINT('Ctrl Pts',(-6.33152333219865,2.39484482315973,
67.5819125686252));
#200314=CARTESIAN_POINT('Ctrl Pts',(-6.39186989237051,2.22877599084022,
67.5902048780931));
#200315=CARTESIAN_POINT('Ctrl Pts',(-6.44561842696355,2.06065331727293,
67.598497187561));
#200316=CARTESIAN_POINT('Ctrl Pts',(-6.49940622500276,1.89240782964956,
67.6067955545828));
#200317=CARTESIAN_POINT('Ctrl Pts',(-6.5465862588529,1.72210583522364,67.6150939216046));
#200318=CARTESIAN_POINT('Ctrl Pts',(-6.58702126478448,1.55030315012163,
67.6233922886263));
#200319=CARTESIAN_POINT('Ctrl Pts',(-6.62747075214523,1.37843893545242,
67.6316936276327));
#200320=CARTESIAN_POINT('Ctrl Pts',(-6.66117032425106,1.20507330023746,
67.6399949666391));
#200321=CARTESIAN_POINT('Ctrl Pts',(-6.6880340124061,1.03077157940018,67.6482963056455));
#200322=CARTESIAN_POINT('Ctrl Pts',(-6.71492875010227,0.856268397452345,
67.656607239491));
#200323=CARTESIAN_POINT('Ctrl Pts',(-6.73497176834432,0.680827314055356,
67.6649181733365));
#200324=CARTESIAN_POINT('Ctrl Pts',(-6.748128959665,0.505019349857625,67.673229107182));
#200325=CARTESIAN_POINT('Ctrl Pts',(-6.76071469570443,0.336847239481363,
67.6811790728754));
#200326=CARTESIAN_POINT('Ctrl Pts',(-6.76700011610791,0.168339715120327,
67.6891290385688));
#200327=CARTESIAN_POINT('Ctrl Pts',(-6.76699999999839,-4.66729631973905E-6,
67.6970790042622));
#200328=CARTESIAN_POINT('',(-6.76699969105987,0.00204479721649499,67.3028202162187));
#200329=CARTESIAN_POINT('Ctrl Pts',(3.09910619832135,6.0156321173694,66.651425676538));
#200330=CARTESIAN_POINT('Ctrl Pts',(2.9437528555786,6.09566635118397,66.6596230179432));
#200331=CARTESIAN_POINT('Ctrl Pts',(2.78530404469065,6.16967521411631,66.6678203593483));
#200332=CARTESIAN_POINT('Ctrl Pts',(2.62427106360847,6.23742658351241,66.6760177007535));
#200333=CARTESIAN_POINT('Ctrl Pts',(2.46320047430483,6.30519377580694,66.6842169565952));
#200334=CARTESIAN_POINT('Ctrl Pts',(2.29954484324433,6.36670042414967,66.692416212437));
#200335=CARTESIAN_POINT('Ctrl Pts',(2.13383456016875,6.42176292538345,66.7006154682787));
#200336=CARTESIAN_POINT('Ctrl Pts',(1.96805544484949,6.47684829831496,66.7088181299029));
#200337=CARTESIAN_POINT('Ctrl Pts',(1.80022031761879,6.52548407900047,66.7170207915271));
#200338=CARTESIAN_POINT('Ctrl Pts',(1.63087384812159,6.56753679026719,66.7252234531513));
#200339=CARTESIAN_POINT('Ctrl Pts',(1.46133097115867,6.609638274127,66.7334356281949));
#200340=CARTESIAN_POINT('Ctrl Pts',(1.29027359919294,6.645141352039,66.7416478032385));
#200341=CARTESIAN_POINT('Ctrl Pts',(1.11825667107228,6.67396366618836,66.749859978282));
#200342=CARTESIAN_POINT('Ctrl Pts',(0.946128679145179,6.70280458964527,
66.7580774555678));
#200343=CARTESIAN_POINT('Ctrl Pts',(0.773040251134529,6.72495610647834,
66.7662949328536));
#200344=CARTESIAN_POINT('Ctrl Pts',(0.599550408877115,6.74038784545929,
66.7745124101394));
#200345=CARTESIAN_POINT('Ctrl Pts',(0.425808467513748,6.75584200839053,
66.7827418282896));
#200346=CARTESIAN_POINT('Ctrl Pts',(0.251664304072191,6.76455687037831,
66.7909712464398));
#200347=CARTESIAN_POINT('Ctrl Pts',(0.0776769903517417,6.76655416627769,
66.7992006645899));
#200348=CARTESIAN_POINT('Ctrl Pts',(-0.0203850106945762,6.7676798738272,
66.8038388947804));
#200349=CARTESIAN_POINT('Ctrl Pts',(-0.118397260002335,6.76667260349463,
66.8084771249708));
#200350=CARTESIAN_POINT('Ctrl Pts',(-0.216260647502554,6.76354347456581,
66.8131153551613));
#200351=CARTESIAN_POINT('Ctrl Pts',(-0.386517383979043,6.75809960742568,
66.8211846643833));
#200352=CARTESIAN_POINT('Ctrl Pts',(-0.55688051997641,6.7462127497999,66.8292539736053));
#200353=CARTESIAN_POINT('Ctrl Pts',(-0.726811026680727,6.72785513603669,
66.8373232828273));
#200354=CARTESIAN_POINT('Ctrl Pts',(-0.896529583857726,6.70952041920727,
66.8453825274275));
#200355=CARTESIAN_POINT('Ctrl Pts',(-1.06581621913016,6.68473104453334,
66.8534417720278));
#200356=CARTESIAN_POINT('Ctrl Pts',(-1.23413042271984,6.6535111858114,66.861501016628));
#200357=CARTESIAN_POINT('Ctrl Pts',(-1.40227162902586,6.62232341559203,
66.8695519777477));
#200358=CARTESIAN_POINT('Ctrl Pts',(-1.56944202887194,6.5847183816347,66.8776029388675));
#200359=CARTESIAN_POINT('Ctrl Pts',(-1.7351048634845,6.5407721342906,66.8856538999872));
#200360=CARTESIAN_POINT('Ctrl Pts',(-1.90063372596885,6.49686142643427,
66.8936983502658));
#200361=CARTESIAN_POINT('Ctrl Pts',(-2.06465709094783,6.44661980711828,
66.9017428005445));
#200362=CARTESIAN_POINT('Ctrl Pts',(-2.2266471514926,6.3901746034635,66.9097872508231));
#200363=CARTESIAN_POINT('Ctrl Pts',(-2.38854166820264,6.33376269192054,
66.9178269563808));
#200364=CARTESIAN_POINT('Ctrl Pts',(-2.54840491639844,6.27115460239405,
66.9258666619385));
#200365=CARTESIAN_POINT('Ctrl Pts',(-2.70572315484147,6.20252780802752,
66.9339063674962));
#200366=CARTESIAN_POINT('Ctrl Pts',(-2.86643702337129,6.1324197409871,66.942119605801));
#200367=CARTESIAN_POINT('Ctrl Pts',(-3.02449438234326,6.05603029676614,
66.9503328441057));
#200368=CARTESIAN_POINT('Ctrl Pts',(-3.17936746390975,5.97360121948495,
66.9585460824105));
#200369=CARTESIAN_POINT('Ctrl Pts',(-3.33091952112869,5.89293971194427,
66.9665831999582));
#200370=CARTESIAN_POINT('Ctrl Pts',(-3.47942214373032,5.80649516123075,
66.9746203175059));
#200371=CARTESIAN_POINT('Ctrl Pts',(-3.62440473451101,5.71454104197828,
66.9826574350535));
#200372=CARTESIAN_POINT('Ctrl Pts',(-3.7694026635282,5.62257719456451,66.9906954028771));
#200373=CARTESIAN_POINT('Ctrl Pts',(-3.91087950363473,5.52510281804308,
66.9987333707007));
#200374=CARTESIAN_POINT('Ctrl Pts',(-4.04839307754145,5.42243510700815,
67.0067713385243));
#200375=CARTESIAN_POINT('Ctrl Pts',(-4.18594844601779,5.31973619212421,
67.0148117493315));
#200376=CARTESIAN_POINT('Ctrl Pts',(-4.31953785142545,5.21184102430835,
67.0228521601387));
#200377=CARTESIAN_POINT('Ctrl Pts',(-4.44875180267221,5.09910741191248,
67.030892570946));
#200378=CARTESIAN_POINT('Ctrl Pts',(-4.58284931252452,4.98211310477244,
67.0392368639347));
#200379=CARTESIAN_POINT('Ctrl Pts',(-4.71223383576047,4.85990776844361,
67.0475811569234));
#200380=CARTESIAN_POINT('Ctrl Pts',(-4.83649003847436,4.73293282307475,
67.0559254499121));
#200381=CARTESIAN_POINT('Ctrl Pts',(-4.95643252863061,4.61036597488237,
67.0639800601272));
#200382=CARTESIAN_POINT('Ctrl Pts',(-5.07159660629193,4.4833554512275,67.0720346703422));
#200383=CARTESIAN_POINT('Ctrl Pts',(-5.18165055964601,4.3523311544183,67.0800892805573));
#200384=CARTESIAN_POINT('Ctrl Pts',(-5.29178782539577,4.22120767036752,
67.088149988226));
#200385=CARTESIAN_POINT('Ctrl Pts',(-5.39680703669563,4.08606465611705,
67.0962106958946));
#200386=CARTESIAN_POINT('Ctrl Pts',(-5.49642004171115,3.94736060236154,
67.1042714035632));
#200387=CARTESIAN_POINT('Ctrl Pts',(-5.59617349509784,3.80846098419732,
67.1123434763469));
#200388=CARTESIAN_POINT('Ctrl Pts',(-5.69050532990209,3.66599061758706,
67.1204155491306));
#200389=CARTESIAN_POINT('Ctrl Pts',(-5.77917321239657,3.52043264118459,
67.1284876219143));
#200390=CARTESIAN_POINT('Ctrl Pts',(-5.78846049945894,3.50518654899161,
67.1293331102131));
#200391=CARTESIAN_POINT('Ctrl Pts',(-5.79768569113277,3.489906600452,67.130178598512));
#200392=CARTESIAN_POINT('Ctrl Pts',(-5.8068485397515,3.47459336273842,67.1310240868108));
#200393=CARTESIAN_POINT('Ctrl Pts',(-5.90234831954787,3.3149911592679,67.1398361876887));
#200394=CARTESIAN_POINT('Ctrl Pts',(-5.99134678333706,3.15131174780054,
67.1486482885667));
#200395=CARTESIAN_POINT('Ctrl Pts',(-6.07350709161056,2.98409125332256,
67.1574603894447));
#200396=CARTESIAN_POINT('Ctrl Pts',(-6.15553653987655,2.81713709761112,
67.1662584549374));
#200397=CARTESIAN_POINT('Ctrl Pts',(-6.23074943337021,2.64665335945228,
67.17505652043));
#200398=CARTESIAN_POINT('Ctrl Pts',(-6.29885384418314,2.47320222578328,
67.1838545859227));
#200399=CARTESIAN_POINT('Ctrl Pts',(-6.36684939253087,2.30002834754862,
67.1926385880222));
#200400=CARTESIAN_POINT('Ctrl Pts',(-6.42775901957409,2.12389679511523,
67.2014225901218));
#200401=CARTESIAN_POINT('Ctrl Pts',(-6.48133772067748,1.94539208143841,
67.2102065922214));
#200402=CARTESIAN_POINT('Ctrl Pts',(-6.53479274991776,1.76729939735657,
67.2189703188405));
#200403=CARTESIAN_POINT('Ctrl Pts',(-6.58095053711646,1.58684475049073,
67.2277340454596));
#200404=CARTESIAN_POINT('Ctrl Pts',(-6.61961510243933,1.40462980730055,
67.2364977720788));
#200405=CARTESIAN_POINT('Ctrl Pts',(-6.65822430976861,1.22267575036558,
67.2452489512319));
#200406=CARTESIAN_POINT('Ctrl Pts',(-6.68936163055062,1.03896669613739,
67.2540001303849));
#200407=CARTESIAN_POINT('Ctrl Pts',(-6.71288087981851,0.854119015926434,
67.262751309538));
#200408=CARTESIAN_POINT('Ctrl Pts',(-6.73635188671799,0.669650492795929,
67.2714845383899));
#200409=CARTESIAN_POINT('Ctrl Pts',(-6.75223596278394,0.484048281077616,
67.2802177672417));
#200410=CARTESIAN_POINT('Ctrl Pts',(-6.76043799091104,0.297938200046067,
67.2889509960935));
#200411=CARTESIAN_POINT('Ctrl Pts',(-6.76477986473802,0.199417873457771,
67.2935740694589));
#200412=CARTESIAN_POINT('Ctrl Pts',(-6.76696986347182,0.100755425632308,
67.2981971428244));
#200413=CARTESIAN_POINT('Ctrl Pts',(-6.76699969105968,0.00204479783337229,
67.3028202161898));
#200414=CARTESIAN_POINT('Ctrl Pts',(-6.76699969105987,0.00204479721659033,
67.3028202162187));
#200415=CARTESIAN_POINT('Ctrl Pts',(-6.76705546570766,-0.182534397879825,
67.3114649101052));
#200416=CARTESIAN_POINT('Ctrl Pts',(-6.75955491081402,-0.367004244749094,
67.3201096039916));
#200417=CARTESIAN_POINT('Ctrl Pts',(-6.74455107192691,-0.550744803125321,
67.3287542978781));
#200418=CARTESIAN_POINT('Ctrl Pts',(-6.72953240757911,-0.734666917598438,
67.3374075336831));
#200419=CARTESIAN_POINT('Ctrl Pts',(-6.70699568187137,-0.917858008923771,
67.3460607694881));
#200420=CARTESIAN_POINT('Ctrl Pts',(-6.67704556877224,-1.09970517528065,
67.3547140052931));
#200421=CARTESIAN_POINT('Ctrl Pts',(-6.64704417399101,-1.28186370702515,
67.3633820574858));
#200422=CARTESIAN_POINT('Ctrl Pts',(-6.60960406084239,-1.46267341902971,
67.3720501096786));
#200423=CARTESIAN_POINT('Ctrl Pts',(-6.56488105234982,-1.64153153137497,
67.3807181618713));
#200424=CARTESIAN_POINT('Ctrl Pts',(-6.52011863950898,-1.82054723122584,
67.3893938512726));
#200425=CARTESIAN_POINT('Ctrl Pts',(-6.46806060170046,-1.99760761274257,
67.398069540674));
#200426=CARTESIAN_POINT('Ctrl Pts',(-6.40891241259666,-2.17212584526415,
67.4067452300754));
#200427=CARTESIAN_POINT('Ctrl Pts',(-6.34967138021081,-2.34691801424483,
67.4154345374672));
#200428=CARTESIAN_POINT('Ctrl Pts',(-6.28331804893838,-2.51915977717957,
67.4241238448591));
#200429=CARTESIAN_POINT('Ctrl Pts',(-6.21010645343616,-2.68828325088532,
67.432813152251));
#200430=CARTESIAN_POINT('Ctrl Pts',(-6.16483447225615,-2.79286442639696,
67.4381863743207));
#200431=CARTESIAN_POINT('Ctrl Pts',(-6.11694093386495,-2.89625366352979,
67.4435595963905));
#200432=CARTESIAN_POINT('Ctrl Pts',(-6.06649463752745,-2.99832149924766,
67.4489328184602));
#200433=CARTESIAN_POINT('Ctrl Pts',(-5.98715960250811,-3.15883983079871,
67.4573830872018));
#200434=CARTESIAN_POINT('Ctrl Pts',(-5.90138241536787,-3.31634371716938,
67.4658333559433));
#200435=CARTESIAN_POINT('Ctrl Pts',(-5.80941452677204,-3.47030140710141,
67.4742836246849));
#200436=CARTESIAN_POINT('Ctrl Pts',(-5.71752780295919,-3.62412322414689,
67.4827264357775));
#200437=CARTESIAN_POINT('Ctrl Pts',(-5.619461436692,-3.77440479935361,67.4911692468701));
#200438=CARTESIAN_POINT('Ctrl Pts',(-5.51551317961652,-3.92063813243157,
67.4996120579627));
#200439=CARTESIAN_POINT('Ctrl Pts',(-5.41164250758393,-4.06676231967352,
67.5080485674984));
#200440=CARTESIAN_POINT('Ctrl Pts',(-5.30189888770947,-4.2088440186668,
67.516485077034));
#200441=CARTESIAN_POINT('Ctrl Pts',(-5.18662405337289,-4.34640310244849,
67.5249215865697));
#200442=CARTESIAN_POINT('Ctrl Pts',(-5.07143170438705,-4.48386375529909,
67.5333520593285));
#200443=CARTESIAN_POINT('Ctrl Pts',(-4.95071624802827,-4.61680799448141,
67.5417825320874));
#200444=CARTESIAN_POINT('Ctrl Pts',(-4.82486058506799,-4.74478759636903,
67.5502130048462));
#200445=CARTESIAN_POINT('Ctrl Pts',(-4.69905902711864,-4.87271218017009,
67.5586398533675));
#200446=CARTESIAN_POINT('Ctrl Pts',(-4.56812189987031,-4.99567614546197,
67.5670667018888));
#200447=CARTESIAN_POINT('Ctrl Pts',(-4.43247039600956,-5.11326658687955,
67.5754935504101));
#200448=CARTESIAN_POINT('Ctrl Pts',(-4.29686076293026,-5.23082073232155,
67.5839177978637));
#200449=CARTESIAN_POINT('Ctrl Pts',(-4.1565399054294,-5.3430044446237,67.5923420453174));
#200450=CARTESIAN_POINT('Ctrl Pts',(-4.0119639385121,-5.44944349049318,
67.6007662927711));
#200451=CARTESIAN_POINT('Ctrl Pts',(-3.97122796450357,-5.47943393979456,
67.6031399232758));
#200452=CARTESIAN_POINT('Ctrl Pts',(-3.93015438138309,-5.50896856644706,
67.6055135537804));
#200453=CARTESIAN_POINT('Ctrl Pts',(-3.88875385622549,-5.53803958505999,
67.607887184285));
#200454=CARTESIAN_POINT('Ctrl Pts',(-3.73842630763758,-5.64359802777051,
67.6165059651739));
#200455=CARTESIAN_POINT('Ctrl Pts',(-3.58385315610053,-5.74299352130163,
67.6251247460627));
#200456=CARTESIAN_POINT('Ctrl Pts',(-3.42556206974887,-5.83590725648531,
67.6337435269516));
#200457=CARTESIAN_POINT('Ctrl Pts',(-3.2671758989147,-5.92887680437854,
67.6423674850892));
#200458=CARTESIAN_POINT('Ctrl Pts',(-3.10506759851736,-6.01535666959871,
67.6509914432267));
#200459=CARTESIAN_POINT('Ctrl Pts',(-2.93978960781891,-6.0950739176617,
67.6596154013643));
#200460=CARTESIAN_POINT('Ctrl Pts',(-2.76854068580091,-6.17767107859849,
67.6685509137598));
#200461=CARTESIAN_POINT('Ctrl Pts',(-2.593889111302,-6.25300774026649,67.6774864261553));
#200462=CARTESIAN_POINT('Ctrl Pts',(-2.41647154396405,-6.32083493513413,
67.6864219385507));
#200463=CARTESIAN_POINT('Ctrl Pts',(-2.24491984835737,-6.38641959206735,
67.6950620203958));
#200464=CARTESIAN_POINT('Ctrl Pts',(-2.07078243740811,-6.44498334513258,
67.7037021022409));
#200465=CARTESIAN_POINT('Ctrl Pts',(-1.89465042004698,-6.49635195981682,
67.712342184086));
#200466=CARTESIAN_POINT('Ctrl Pts',(-1.70948467249197,-6.55035524713152,
67.7214254117567));
#200467=CARTESIAN_POINT('Ctrl Pts',(-1.52211472135507,-6.59640584482545,
67.7305086394273));
#200468=CARTESIAN_POINT('Ctrl Pts',(-1.33324010415943,-6.63436205106874,
67.739591867098));
#200469=CARTESIAN_POINT('Ctrl Pts',(-1.14436548696386,-6.67231825731201,
67.7486750947686));
#200470=CARTESIAN_POINT('Ctrl Pts',(-0.95398659201651,-6.70218004526323,
67.7577583224393));
#200471=CARTESIAN_POINT('Ctrl Pts',(-0.762810281316113,-6.72386863901418,
67.76684155011));
#200472=CARTESIAN_POINT('Ctrl Pts',(-0.572447080124421,-6.74546498701698,
67.7758861450716));
#200473=CARTESIAN_POINT('Ctrl Pts',(-0.38111753514558,-6.75897833174049,
67.7849307400332));
#200474=CARTESIAN_POINT('Ctrl Pts',(-0.189490688569759,-6.76434640441672,
67.7939753349948));
#200475=CARTESIAN_POINT('Ctrl Pts',(0.00196031020367951,-6.76970955104109,
67.8030116301165));
#200476=CARTESIAN_POINT('Ctrl Pts',(0.193707828290141,-6.76694234197754,
67.8120479252382));
#200477=CARTESIAN_POINT('Ctrl Pts',(0.385080243852762,-6.75603450300502,
67.8210842203599));
#200478=CARTESIAN_POINT('Ctrl Pts',(0.576114010867229,-6.74514596631189,
67.8301045250464));
#200479=CARTESIAN_POINT('Ctrl Pts',(0.766773763629801,-6.72614557914719,
67.8391248297328));
#200480=CARTESIAN_POINT('Ctrl Pts',(0.956390590301346,-6.6990750136704,
67.8481451344192));
#200481=CARTESIAN_POINT('Ctrl Pts',(1.14576863137019,-6.67203853831845,
67.8571540797821));
#200482=CARTESIAN_POINT('Ctrl Pts',(1.3341061325675,-6.63695219967758,67.866163025145));
#200483=CARTESIAN_POINT('Ctrl Pts',(1.520739428976,-6.59390935554605,67.8751719705078));
#200484=CARTESIAN_POINT('Ctrl Pts',(1.70694892057874,-6.55096425262442,
67.8841604584582));
#200485=CARTESIAN_POINT('Ctrl Pts',(1.89146170064486,-6.50009876195173,
67.8931489464085));
#200486=CARTESIAN_POINT('Ctrl Pts',(2.07362489293906,-6.44145704040503,
67.9021374343588));
#200487=CARTESIAN_POINT('Ctrl Pts',(2.23344801159656,-6.39000700429728,
67.9100235948841));
#200488=CARTESIAN_POINT('Ctrl Pts',(2.39146249064502,-6.33257186807405,
67.9179097554094));
#200489=CARTESIAN_POINT('Ctrl Pts',(2.54723358303126,-6.26928146389024,
67.9257959159347));
#200490=CARTESIAN_POINT('Ctrl Pts',(2.70765251422937,-6.20410262461569,
67.9339173807286));
#200491=CARTESIAN_POINT('Ctrl Pts',(2.86561976081255,-6.13274155174847,
67.9420388455225));
#200492=CARTESIAN_POINT('Ctrl Pts',(3.02062845100306,-6.05541846291327,
67.9501603103164));
#200493=CARTESIAN_POINT('Ctrl Pts',(3.17562608678761,-5.9781008883548,67.9582811959301));
#200494=CARTESIAN_POINT('Ctrl Pts',(3.32766525875864,-5.8948223081832,67.9664020815438));
#200495=CARTESIAN_POINT('Ctrl Pts',(3.47626203632042,-5.80584974442479,
67.9745229671575));
#200496=CARTESIAN_POINT('Ctrl Pts',(3.62487657544279,-5.71686654590291,
67.9826448234491));
#200497=CARTESIAN_POINT('Ctrl Pts',(3.77004758728321,-5.62218819771634,
67.9907666797406));
#200498=CARTESIAN_POINT('Ctrl Pts',(3.91131860705761,-5.52212601758462,
67.9988885360322));
#200499=CARTESIAN_POINT('Ctrl Pts',(4.05269269641907,-5.42199083332506,
68.0070163179295));
#200500=CARTESIAN_POINT('Ctrl Pts',(4.19016081157461,-5.31646418375312,
68.0151440998269));
#200501=CARTESIAN_POINT('Ctrl Pts',(4.32329767116583,-5.20589917751892,
68.0232718817242));
#200502=CARTESIAN_POINT('Ctrl Pts',(4.45648876576363,-5.09528913121197,
68.0314029745777));
#200503=CARTESIAN_POINT('Ctrl Pts',(4.5853448155403,-4.97963688157713,68.0395340674312));
#200504=CARTESIAN_POINT('Ctrl Pts',(4.70947633867659,-4.8593334538232,68.0476651602847));
#200505=CARTESIAN_POINT('Ctrl Pts',(4.83374334618531,-4.73889871990306,
68.0558051278864));
#200506=CARTESIAN_POINT('Ctrl Pts',(4.95327527488596,-4.61380293270163,
68.0639450954882));
#200507=CARTESIAN_POINT('Ctrl Pts',(5.06772146916316,-4.48447188763435,
68.0720850630899));
#200508=CARTESIAN_POINT('Ctrl Pts',(5.12707821959638,-4.41739520925453,
68.0763068026464));
#200509=CARTESIAN_POINT('Ctrl Pts',(5.18506763295147,-4.34917980776911,
68.0805285422028));
#200510=CARTESIAN_POINT('Ctrl Pts',(5.24164532858782,-4.2798882285982,68.0847502817593));
#200511=CARTESIAN_POINT('Ctrl Pts',(5.3547569012016,-4.1413587356459,68.0931904911922));
#200512=CARTESIAN_POINT('Ctrl Pts',(5.46245722300636,-3.99823976917441,
68.1016307006251));
#200513=CARTESIAN_POINT('Ctrl Pts',(5.56437095760982,-3.85098232222746,
68.1100709100579));
#200514=CARTESIAN_POINT('Ctrl Pts',(5.66620747745769,-3.70383644461725,
68.1185047247815));
#200515=CARTESIAN_POINT('Ctrl Pts',(5.76226596060923,-3.55255861019642,
68.1269385395051));
#200516=CARTESIAN_POINT('Ctrl Pts',(5.85221222128754,-3.39763169237231,
68.1353723542286));
#200517=CARTESIAN_POINT('Ctrl Pts',(5.94210416150533,-3.24279833821013,
68.143801075592));
#200518=CARTESIAN_POINT('Ctrl Pts',(6.02589107136909,-3.08432058183424,
68.1522297969554));
#200519=CARTESIAN_POINT('Ctrl Pts',(6.10328265729014,-2.92270932615979,
68.1606585183188));
#200520=CARTESIAN_POINT('Ctrl Pts',(6.18063938888008,-2.76117085426601,
68.1690834436953));
#200521=CARTESIAN_POINT('Ctrl Pts',(6.25160639556577,-2.59650199714855,
68.1775083690719));
#200522=CARTESIAN_POINT('Ctrl Pts',(6.31593965149612,-2.42923760028925,
68.1859332944484));
#200523=CARTESIAN_POINT('Ctrl Pts',(6.38025380471629,-2.26202286986219,
68.1943557181808));
#200524=CARTESIAN_POINT('Ctrl Pts',(6.43793801577486,-2.09221444756755,
68.2027781419133));
#200525=CARTESIAN_POINT('Ctrl Pts',(6.48879651596112,-1.92036683330318,
68.2112005656458));
#200526=CARTESIAN_POINT('Ctrl Pts',(6.53965581600562,-1.74851651636901,
68.2196231218388));
#200527=CARTESIAN_POINT('Ctrl Pts',(6.5836890897008,-1.57462726119323,68.2280456780318));
#200528=CARTESIAN_POINT('Ctrl Pts',(6.6207503461659,-1.39926904265911,68.2364682342248));
#200529=CARTESIAN_POINT('Ctrl Pts',(6.65781285456765,-1.22390490048931,
68.2448910749334));
#200530=CARTESIAN_POINT('Ctrl Pts',(6.68790280699985,-1.04707202235281,
68.2533139156421));
#200531=CARTESIAN_POINT('Ctrl Pts',(6.71092525262042,-0.869351053223966,
68.2617367563508));
#200532=CARTESIAN_POINT('Ctrl Pts',(6.73395169013205,-0.691599268830729,
68.2701610575064));
#200533=CARTESIAN_POINT('Ctrl Pts',(6.74990813480536,-0.512959417234193,
68.2785853586621));
#200534=CARTESIAN_POINT('Ctrl Pts',(6.75875143026366,-0.334018119132661,
68.2870096598178));
#200535=CARTESIAN_POINT('Ctrl Pts',(6.76759749407248,-0.155020804330292,
68.2954365981599));
#200536=CARTESIAN_POINT('Ctrl Pts',(6.76932595269978,0.0242778120923452,
68.303863536502));
#200537=CARTESIAN_POINT('Ctrl Pts',(6.76394575863086,0.20328987751389,68.312290474844));
#200538=CARTESIAN_POINT('Ctrl Pts',(6.75856072709091,0.382462897293245,
68.3207249900634));
#200539=CARTESIAN_POINT('Ctrl Pts',(6.74605428151076,0.56134851752219,68.3291595052828));
#200540=CARTESIAN_POINT('Ctrl Pts',(6.72648744801321,0.739361624457722,
68.3375940205021));
#200541=CARTESIAN_POINT('Ctrl Pts',(6.70691116356695,0.917460713253555,
68.3460326096648));
#200542=CARTESIAN_POINT('Ctrl Pts',(6.68026773438625,1.09468611783465,68.3544711988275));
#200543=CARTESIAN_POINT('Ctrl Pts',(6.64666964879937,1.27046116813119,68.3629097879902));
#200544=CARTESIAN_POINT('Ctrl Pts',(6.61303400815141,1.44643269518036,68.371357809587));
#200545=CARTESIAN_POINT('Ctrl Pts',(6.57242824847864,1.62095030252979,68.3798058311839));
#200546=CARTESIAN_POINT('Ctrl Pts',(6.52501552695931,1.79344957357042,68.3882538527808));
#200547=CARTESIAN_POINT('Ctrl Pts',(6.49806689520091,1.89149539724183,68.3930555729901));
#200548=CARTESIAN_POINT('Ctrl Pts',(6.46892011363864,1.98888946191966,68.3978572931995));
#200549=CARTESIAN_POINT('Ctrl Pts',(6.43761216901738,2.08553076249653,68.4026590134089));
#200550=CARTESIAN_POINT('Ctrl Pts',(6.38388916882985,2.25136281157614,68.4108985455414));
#200551=CARTESIAN_POINT('Ctrl Pts',(6.32367992429258,2.4153474495578,68.4191380776738));
#200552=CARTESIAN_POINT('Ctrl Pts',(6.25712841355242,2.57694257140414,68.4273776098063));
#200553=CARTESIAN_POINT('Ctrl Pts',(6.19065077035214,2.73835833392454,68.4356079966323));
#200554=CARTESIAN_POINT('Ctrl Pts',(6.11784501206133,2.8973895350872,68.4438383834582));
#200555=CARTESIAN_POINT('Ctrl Pts',(6.03890501359738,3.05350867638336,68.4520687702841));
#200556=CARTESIAN_POINT('Ctrl Pts',(5.96003855086308,3.20948238652685,68.4602914901793));
#200557=CARTESIAN_POINT('Ctrl Pts',(5.87504938770952,3.36254912344422,68.4685142100745));
#200558=CARTESIAN_POINT('Ctrl Pts',(5.78417969659149,3.51220076839847,68.4767369299697));
#200559=CARTESIAN_POINT('Ctrl Pts',(5.69339052261084,3.66171981114062,68.4849523639386));
#200560=CARTESIAN_POINT('Ctrl Pts',(5.59673138984904,3.8078294900049,68.4931677979075));
#200561=CARTESIAN_POINT('Ctrl Pts',(5.49449058491127,3.95004584939484,68.5013832318765));
#200562=CARTESIAN_POINT('Ctrl Pts',(5.39230232383676,4.0921891205795,68.509594443748));
#200563=CARTESIAN_POINT('Ctrl Pts',(5.28453831079439,4.23044276891584,68.5178056556195));
#200564=CARTESIAN_POINT('Ctrl Pts',(5.1715305930025,4.36435107726672,68.526016867491));
#200565=CARTESIAN_POINT('Ctrl Pts',(5.05856077182384,4.49821448008843,68.5342253257708));
#200566=CARTESIAN_POINT('Ctrl Pts',(4.94035097817908,4.62773517407047,68.5424337840505));
#200567=CARTESIAN_POINT('Ctrl Pts',(4.81727410861847,4.75248978562123,68.5506422423303));
#200568=CARTESIAN_POINT('Ctrl Pts',(4.76244070224812,4.80807066232178,68.5542992879647));
#200569=CARTESIAN_POINT('Ctrl Pts',(4.70664175875749,4.8627059701033,68.5579563335992));
#200570=CARTESIAN_POINT('Ctrl Pts',(4.64991270549473,4.91636052698322,68.5616133792336));
#200571=CARTESIAN_POINT('Ctrl Pts',(4.51245672008586,5.04636692693925,68.5704744968172));
#200572=CARTESIAN_POINT('Ctrl Pts',(4.36968067268176,5.1704777176743,68.5793356144008));
#200573=CARTESIAN_POINT('Ctrl Pts',(4.22210643219175,5.28829899639242,68.5881967319845));
#200574=CARTESIAN_POINT('Ctrl Pts',(4.07429896157757,5.4063064828889,68.5970718539061));
#200575=CARTESIAN_POINT('Ctrl Pts',(3.92167835441354,5.51800444251662,68.6059469758278));
#200576=CARTESIAN_POINT('Ctrl Pts',(3.76479554898082,5.62304219034272,68.6148220977495));
#200577=CARTESIAN_POINT('Ctrl Pts',(3.60755963427478,5.72831635542757,68.6237171956516));
#200578=CARTESIAN_POINT('Ctrl Pts',(3.4460425524921,5.82690018600769,68.6326122935537));
#200579=CARTESIAN_POINT('Ctrl Pts',(3.28082209799587,5.91848759070271,68.6415073914558));
#200580=CARTESIAN_POINT('Ctrl Pts',(3.22073033337437,5.95179853142133,68.6447425969941));
#200581=CARTESIAN_POINT('Ctrl Pts',(3.16014888048151,5.98418442393441,68.6479778025323));
#200582=CARTESIAN_POINT('Ctrl Pts',(3.09910619832137,6.01563211736939,68.6512130080706));
#200583=CARTESIAN_POINT('Origin',(0.,0.,4.30282021618968));
#200584=CARTESIAN_POINT('',(3.09910619832143,6.01563211736936,71.0458824924514));
#200585=CARTESIAN_POINT('',(3.0991061983213,6.01563211736942,70.6515955249703));
#200586=CARTESIAN_POINT('',(3.09910619832133,6.0156321173694,4.30282021618968));
#200587=CARTESIAN_POINT('',(-6.76699999999972,1.95537661063743E-6,69.6972235144016));
#200588=CARTESIAN_POINT('Ctrl Pts',(-6.76699999999972,1.95537661063744E-6,
69.6972235144016));
#200589=CARTESIAN_POINT('Ctrl Pts',(-6.7670000509717,-0.176397498243203,
69.7055417487154));
#200590=CARTESIAN_POINT('Ctrl Pts',(-6.76009830406571,-0.352944500227869,
69.7138599830292));
#200591=CARTESIAN_POINT('Ctrl Pts',(-6.74628617363261,-0.52906697444988,
69.7221782173429));
#200592=CARTESIAN_POINT('Ctrl Pts',(-6.73248404601485,-0.705061899877223,
69.730490427549));
#200593=CARTESIAN_POINT('Ctrl Pts',(-6.71178153440809,-0.880632564880317,
69.738802637755));
#200594=CARTESIAN_POINT('Ctrl Pts',(-6.6842221106453,-1.05520793001215,
69.747114847961));
#200595=CARTESIAN_POINT('Ctrl Pts',(-6.6566776101285,-1.22968876373652,
69.7554225571601));
#200596=CARTESIAN_POINT('Ctrl Pts',(-6.62228365146343,-1.40317502912908,
69.7637302663592));
#200597=CARTESIAN_POINT('Ctrl Pts',(-6.58113545826471,-1.5751016094116,
69.7720379755583));
#200598=CARTESIAN_POINT('Ctrl Pts',(-6.5399983857192,-1.74698172505669,
69.7803434395275));
#200599=CARTESIAN_POINT('Ctrl Pts',(-6.49211079391409,-1.91730265716737,
69.7886489034967));
#200600=CARTESIAN_POINT('Ctrl Pts',(-6.43761892794818,-2.08550989892719,
69.796954367466));
#200601=CARTESIAN_POINT('Ctrl Pts',(-6.38313412606942,-2.25369533503596,
69.8052587547512));
#200602=CARTESIAN_POINT('Ctrl Pts',(-6.32204686255277,-2.4197672959954,
69.8135631420363));
#200603=CARTESIAN_POINT('Ctrl Pts',(-6.25455317910352,-2.58318670052439,
69.8218675293215));
#200604=CARTESIAN_POINT('Ctrl Pts',(-6.18705706475731,-2.74661199087429,
69.830172215703));
#200605=CARTESIAN_POINT('Ctrl Pts',(-6.11315420338471,-2.90738421309786,
69.8384769020845));
#200606=CARTESIAN_POINT('Ctrl Pts',(-6.03308875844027,-3.0649843446226,
69.8467815884659));
#200607=CARTESIAN_POINT('Ctrl Pts',(-5.95300716678851,-3.22261625918684,
69.8550879496441));
#200608=CARTESIAN_POINT('Ctrl Pts',(-5.86676067270544,-3.37707449853615,
69.8633943108222));
#200609=CARTESIAN_POINT('Ctrl Pts',(-5.77463944592092,-3.52786454808205,
69.8717006720004));
#200610=CARTESIAN_POINT('Ctrl Pts',(-5.68244049543082,-3.67878182087305,
69.880014041348));
#200611=CARTESIAN_POINT('Ctrl Pts',(-5.58435708959756,-3.82602442268361,
69.8883274106956));
#200612=CARTESIAN_POINT('Ctrl Pts',(-5.48072335517361,-3.96912591184187,
69.8966407800432));
#200613=CARTESIAN_POINT('Ctrl Pts',(-5.3770448097465,-4.11228927777527,
69.9049577440738));
#200614=CARTESIAN_POINT('Ctrl Pts',(-5.26781136237028,-4.25130768522227,
69.9132747081044));
#200615=CARTESIAN_POINT('Ctrl Pts',(-5.15339763823301,-4.38574757393246,
69.921591672135));
#200616=CARTESIAN_POINT('Ctrl Pts',(-5.03884469797823,-4.52035104615927,
69.9299187560656));
#200617=CARTESIAN_POINT('Ctrl Pts',(-4.91909911722505,-4.65036460781145,
69.9382458399962));
#200618=CARTESIAN_POINT('Ctrl Pts',(-4.79457345995464,-4.77539049053568,
69.9465729239267));
#200619=CARTESIAN_POINT('Ctrl Pts',(-4.69010025770259,-4.8802833665815,
69.9535590916187));
#200620=CARTESIAN_POINT('Ctrl Pts',(-4.58226322763573,-4.98166615886119,
69.9605452593107));
#200621=CARTESIAN_POINT('Ctrl Pts',(-4.47132378177533,-5.07932600238756,
69.9675314270027));
#200622=CARTESIAN_POINT('Ctrl Pts',(-4.34047883531328,-5.19450863106032,
69.9757710998309));
#200623=CARTESIAN_POINT('Ctrl Pts',(-4.20499906518267,-5.30479169746879,
69.9840107726591));
#200624=CARTESIAN_POINT('Ctrl Pts',(-4.06528500053261,-5.40978251544779,
69.9922504454873));
#200625=CARTESIAN_POINT('Ctrl Pts',(-3.92572602715796,-5.51465678710836,
70.0004809717677));
#200626=CARTESIAN_POINT('Ctrl Pts',(-3.78194240041995,-5.61425029598904,
70.0087114980482));
#200627=CARTESIAN_POINT('Ctrl Pts',(-3.6343701009482,-5.70820838524083,
70.0169420243286));
#200628=CARTESIAN_POINT('Ctrl Pts',(-3.48693529337704,-5.8020789345118,
70.0251648822952));
#200629=CARTESIAN_POINT('Ctrl Pts',(-3.335719141325,-5.89032433055239,70.0333877402618));
#200630=CARTESIAN_POINT('Ctrl Pts',(-3.18118926543502,-5.97263123401077,
70.0416105982285));
#200631=CARTESIAN_POINT('Ctrl Pts',(-3.02679635783686,-6.05486518435308,
70.0498261678257));
#200632=CARTESIAN_POINT('Ctrl Pts',(-2.86909589330713,-6.13117096632485,
70.0580417374231));
#200633=CARTESIAN_POINT('Ctrl Pts',(-2.70858281339615,-6.20127955691203,
70.0662573070204));
#200634=CARTESIAN_POINT('Ctrl Pts',(-2.54815225129109,-6.27135210553256,
70.0744686530941));
#200635=CARTESIAN_POINT('Ctrl Pts',(-2.38491227884607,-6.3352336656696,
70.0826799991678));
#200636=CARTESIAN_POINT('Ctrl Pts',(-2.21938105490168,-6.39270183358676,
70.0908913452415));
#200637=CARTESIAN_POINT('Ctrl Pts',(-2.05390539096749,-6.4501507125026,
70.0990999352039));
#200638=CARTESIAN_POINT('Ctrl Pts',(-1.88614034339804,-6.50119037084162,
70.1073085251663));
#200639=CARTESIAN_POINT('Ctrl Pts',(-1.71662268952433,-6.54564706822865,
70.1155171151288));
#200640=CARTESIAN_POINT('Ctrl Pts',(-1.64111704977945,-6.56544873077202,
70.1191733410283));
#200641=CARTESIAN_POINT('Ctrl Pts',(-1.56526392684188,-6.58394502631183,
70.1228295669278));
#200642=CARTESIAN_POINT('Ctrl Pts',(-1.48911170966338,-6.60112379191176,
70.1264857928273));
#200643=CARTESIAN_POINT('Ctrl Pts',(-1.30459979446344,-6.64274683401154,
70.1353445925855));
#200644=CARTESIAN_POINT('Ctrl Pts',(-1.11852309617017,-6.6765886904504,
70.1442033923436));
#200645=CARTESIAN_POINT('Ctrl Pts',(-0.931530948320751,-6.70257704859263,
70.1530621921018));
#200646=CARTESIAN_POINT('Ctrl Pts',(-0.744187664709552,-6.72861420793875,
70.1619376270044));
#200647=CARTESIAN_POINT('Ctrl Pts',(-0.555925752958089,-6.74676836154393,
70.170813061907));
#200648=CARTESIAN_POINT('Ctrl Pts',(-0.367398066213739,-6.75701914019358,
70.1796884968097));
#200649=CARTESIAN_POINT('Ctrl Pts',(-0.178332559623217,-6.76729916161544,
70.188589250991));
#200650=CARTESIAN_POINT('Ctrl Pts',(0.0109999786631993,-6.76963067577843,
70.1974900051723));
#200651=CARTESIAN_POINT('Ctrl Pts',(0.199945185758436,-6.76404545539813,
70.2063907593536));
#200652=CARTESIAN_POINT('Ctrl Pts',(0.389147190347937,-6.75845264408381,
70.2153036106471));
#200653=CARTESIAN_POINT('Ctrl Pts',(0.577960553243027,-6.74492161920995,
70.2242164619406));
#200654=CARTESIAN_POINT('Ctrl Pts',(0.765736238075063,-6.72353604985492,
70.2331293132341));
#200655=CARTESIAN_POINT('Ctrl Pts',(0.953928818231158,-6.70210300074299,
70.2420619526383));
#200656=CARTESIAN_POINT('Ctrl Pts',(1.14107885356263,-6.67278055646375,
70.2509945920425));
#200657=CARTESIAN_POINT('Ctrl Pts',(1.32654484722671,-6.63570401451845,
70.2599272314466));
#200658=CARTESIAN_POINT('Ctrl Pts',(1.50311753313202,-6.60040533541278,
70.2684315405151));
#200659=CARTESIAN_POINT('Ctrl Pts',(1.67816371471294,-6.55807880117575,
70.2769358495836));
#200660=CARTESIAN_POINT('Ctrl Pts',(1.85114289571097,-6.50888308234668,
70.2854401586521));
#200661=CARTESIAN_POINT('Ctrl Pts',(2.01839540892856,-6.46131604239289,
70.2936629231298));
#200662=CARTESIAN_POINT('Ctrl Pts',(2.18403584818975,-6.4072349802431,70.3018856876075));
#200663=CARTESIAN_POINT('Ctrl Pts',(2.34752030826476,-6.34676590101483,
70.3101084520851));
#200664=CARTESIAN_POINT('Ctrl Pts',(2.51083172901008,-6.28636082498864,
70.3183225132178));
#200665=CARTESIAN_POINT('Ctrl Pts',(2.67199138108945,-6.21958131934453,
70.3265365743505));
#200666=CARTESIAN_POINT('Ctrl Pts',(2.8304684966601,-6.14660370362485,70.3347506354831));
#200667=CARTESIAN_POINT('Ctrl Pts',(2.98880968970572,-6.07368867928793,
70.3429576515865));
#200668=CARTESIAN_POINT('Ctrl Pts',(3.14447260441048,-5.99458628132299,
70.3511646676898));
#200669=CARTESIAN_POINT('Ctrl Pts',(3.29694442810037,-5.90952167590727,
70.3593716837932));
#200670=CARTESIAN_POINT('Ctrl Pts',(3.44931608228028,-5.82451295543892,
70.367573308128));
#200671=CARTESIAN_POINT('Ctrl Pts',(3.59850050918707,-5.73355000385005,
70.3757749324628));
#200672=CARTESIAN_POINT('Ctrl Pts',(3.74400750141711,-5.63690489802094,
70.3839765567976));
#200673=CARTESIAN_POINT('Ctrl Pts',(3.88944809834842,-5.54030389165792,
70.3921744387054));
#200674=CARTESIAN_POINT('Ctrl Pts',(4.03121430544255,-5.43802609457757,
70.4003723206132));
#200675=CARTESIAN_POINT('Ctrl Pts',(4.16884295742833,-5.33038810935003,
70.408570202521));
#200676=CARTESIAN_POINT('Ctrl Pts',(4.30645946216917,-5.22275962436065,
70.4167673608754));
#200677=CARTESIAN_POINT('Ctrl Pts',(4.43993885156485,-5.10977210763387,
70.4249645192298));
#200678=CARTESIAN_POINT('Ctrl Pts',(4.56884896847381,-4.99178406016084,
70.4331616775842));
#200679=CARTESIAN_POINT('Ctrl Pts',(4.69775764991932,-4.87379732652985,
70.4413587446601));
#200680=CARTESIAN_POINT('Ctrl Pts',(4.82209689480017,-4.75081041453655,
70.4495558117359));
#200681=CARTESIAN_POINT('Ctrl Pts',(4.94146962371839,-4.62322040982997,
70.4577528788118));
#200682=CARTESIAN_POINT('Ctrl Pts',(5.06086272833705,-4.49560862681827,
70.465951345043));
#200683=CARTESIAN_POINT('Ctrl Pts',(5.17528738289712,-4.36339244777921,
70.4741498112742));
#200684=CARTESIAN_POINT('Ctrl Pts',(5.28438516793511,-4.22700395042487,
70.4823482775054));
#200685=CARTESIAN_POINT('Ctrl Pts',(5.39352141177922,-4.09056737382881,
70.4905496338339));
#200686=CARTESIAN_POINT('Ctrl Pts',(5.49732682147636,-3.94995582908396,
70.4987509901625));
#200687=CARTESIAN_POINT('Ctrl Pts',(5.59548484289048,-3.80563245374313,
70.506952346491));
#200688=CARTESIAN_POINT('Ctrl Pts',(5.6937546439409,-3.66114472693949,70.515163042297));
#200689=CARTESIAN_POINT('Ctrl Pts',(5.78636400652852,-3.51293702190165,
70.523373738103));
#200690=CARTESIAN_POINT('Ctrl Pts',(5.87304055902589,-3.36150019961875,
70.531584433909));
#200691=CARTESIAN_POINT('Ctrl Pts',(5.95976818572768,-3.20997414310819,
70.5397999678719));
#200692=CARTESIAN_POINT('Ctrl Pts',(6.04055586799709,-3.05521549406296,
70.5480155018348));
#200693=CARTESIAN_POINT('Ctrl Pts',(6.11517845212588,-2.89773730670247,
70.5562310357977));
#200694=CARTESIAN_POINT('Ctrl Pts',(6.1899168077135,-2.74001480349986,70.5644593155581));
#200695=CARTESIAN_POINT('Ctrl Pts',(6.25847081023811,-2.57956466018399,
70.5726875953185));
#200696=CARTESIAN_POINT('Ctrl Pts',(6.32066399006775,-2.41691864254073,
70.5809158750789));
#200697=CARTESIAN_POINT('Ctrl Pts',(6.37718372406161,-2.26910967574503,
70.5883935468198));
#200698=CARTESIAN_POINT('Ctrl Pts',(6.4284507766546,-2.11948757875861,70.5958712185607));
#200699=CARTESIAN_POINT('Ctrl Pts',(6.47436917792388,-1.96845948598118,
70.6033488903015));
#200700=CARTESIAN_POINT('Ctrl Pts',(6.52392164847197,-1.8054787437859,70.611418359152));
#200701=CARTESIAN_POINT('Ctrl Pts',(6.56740671387244,-1.64032697291816,
70.6194878280025));
#200702=CARTESIAN_POINT('Ctrl Pts',(6.60462488707267,-1.47350571802769,
70.627557296853));
#200703=CARTESIAN_POINT('Ctrl Pts',(6.64179664104419,-1.30689252584746,
70.6356167013052));
#200704=CARTESIAN_POINT('Ctrl Pts',(6.67271697474166,-1.13861435225918,
70.6436761057574));
#200705=CARTESIAN_POINT('Ctrl Pts',(6.6972351109188,-0.969190832125651,
70.6517355102096));
#200706=CARTESIAN_POINT('Ctrl Pts',(6.72172804768124,-0.799941443235838,
70.6597866313129));
#200707=CARTESIAN_POINT('Ctrl Pts',(6.73983182845517,-0.629549416551856,
70.6678377524163));
#200708=CARTESIAN_POINT('Ctrl Pts',(6.75144600718251,-0.458547502554958,
70.6758888735196));
#200709=CARTESIAN_POINT('Ctrl Pts',(6.76305079373281,-0.287683874724291,
70.6839334838264));
#200710=CARTESIAN_POINT('Ctrl Pts',(6.7681763983931,-0.116211711596677,
70.6919780941331));
#200711=CARTESIAN_POINT('Ctrl Pts',(6.76677380928631,0.0553282383315297,
70.7000227044399));
#200712=CARTESIAN_POINT('Ctrl Pts',(6.76537204743504,0.226767012961965,
70.708062569987));
#200713=CARTESIAN_POINT('Ctrl Pts',(6.75744975980007,0.398273122635417,
70.7161024355341));
#200714=CARTESIAN_POINT('Ctrl Pts',(6.74300994095709,0.569303026650945,
70.7241423010811));
#200715=CARTESIAN_POINT('Ctrl Pts',(6.72825891937657,0.744018916959518,
70.7323554394507));
#200716=CARTESIAN_POINT('Ctrl Pts',(6.70670622290195,0.918237444618071,
70.7405685778203));
#200717=CARTESIAN_POINT('Ctrl Pts',(6.67841119570085,1.09138118965717,70.7487817161899));
#200718=CARTESIAN_POINT('Ctrl Pts',(6.65072202773904,1.26081754339706,70.7568189930652));
#200719=CARTESIAN_POINT('Ctrl Pts',(6.61657641809556,1.42922429421833,70.7648562699405));
#200720=CARTESIAN_POINT('Ctrl Pts',(6.57608213318645,1.5960679113327,70.7728935468158));
#200721=CARTESIAN_POINT('Ctrl Pts',(6.53558356602429,1.7629291720872,70.7809316736296));
#200722=CARTESIAN_POINT('Ctrl Pts',(6.4887350748122,1.92822660688197,70.7889698004435));
#200723=CARTESIAN_POINT('Ctrl Pts',(6.43569495932967,2.09143954979786,70.7970079272573));
#200724=CARTESIAN_POINT('Ctrl Pts',(6.38263872636932,2.25470208877821,70.8050484966437));
#200725=CARTESIAN_POINT('Ctrl Pts',(6.32338723949669,2.41587851994996,70.8130890660301));
#200726=CARTESIAN_POINT('Ctrl Pts',(6.25814776127096,2.5744660801998,70.8211296354165));
#200727=CARTESIAN_POINT('Ctrl Pts',(6.19044632037162,2.7390383090039,70.8294736342944));
#200728=CARTESIAN_POINT('Ctrl Pts',(6.11629629914263,2.90082204906028,70.8378176331723));
#200729=CARTESIAN_POINT('Ctrl Pts',(6.03598221320989,3.05928222330237,70.8461616320502));
#200730=CARTESIAN_POINT('Ctrl Pts',(5.95845209476938,3.21224961295032,70.8542163987049));
#200731=CARTESIAN_POINT('Ctrl Pts',(5.87517833461974,3.36211970571117,70.8622711653595));
#200732=CARTESIAN_POINT('Ctrl Pts',(5.78646145606593,3.50844022572187,70.8703259320142));
#200733=CARTESIAN_POINT('Ctrl Pts',(5.6976774256564,3.6548714991158,70.8783867955079));
#200734=CARTESIAN_POINT('Ctrl Pts',(5.60344227763731,3.79774754043969,70.8864476590016));
#200735=CARTESIAN_POINT('Ctrl Pts',(5.50409760496662,3.93664813705781,70.8945085224953));
#200736=CARTESIAN_POINT('Ctrl Pts',(5.40461288606755,4.07574454190754,70.9025807493918));
#200737=CARTESIAN_POINT('Ctrl Pts',(5.30000449801997,4.21085402819647,70.9106529762883));
#200738=CARTESIAN_POINT('Ctrl Pts',(5.1906520976173,4.34159185109576,70.9187252031847));
#200739=CARTESIAN_POINT('Ctrl Pts',(5.17921675375252,4.35526353965021,70.9195693427736));
#200740=CARTESIAN_POINT('Ctrl Pts',(5.16772956208614,4.36888745707087,70.9204134823624));
#200741=CARTESIAN_POINT('Ctrl Pts',(5.15619097792548,4.38246318856872,70.9212576219513));
#200742=CARTESIAN_POINT('Ctrl Pts',(5.04227564832462,4.51649037133375,70.9295914381418));
#200743=CARTESIAN_POINT('Ctrl Pts',(4.9229849074674,4.64624541472378,70.9379252543322));
#200744=CARTESIAN_POINT('Ctrl Pts',(4.79866696305716,4.77127701749372,70.9462590705227));
#200745=CARTESIAN_POINT('Ctrl Pts',(4.67453741010077,4.89611914733169,70.9545802576453));
#200746=CARTESIAN_POINT('Ctrl Pts',(4.54539608396193,5.01625186105031,70.962901444768));
#200747=CARTESIAN_POINT('Ctrl Pts',(4.41163109147194,5.13125716688982,70.9712226318906));
#200748=CARTESIAN_POINT('Ctrl Pts',(4.27798265779982,5.24616226054191,70.9795365681795));
#200749=CARTESIAN_POINT('Ctrl Pts',(4.13971884260089,5.35594861784384,70.9878505044683));
#200750=CARTESIAN_POINT('Ctrl Pts',(3.99726491673493,5.4602346273251,70.9961644407571));
#200751=CARTESIAN_POINT('Ctrl Pts',(3.85493607555099,5.56442906627045,71.0044710768184));
#200752=CARTESIAN_POINT('Ctrl Pts',(3.70842473619227,5.66313257878805,71.0127777128796));
#200753=CARTESIAN_POINT('Ctrl Pts',(3.55818952006788,5.75600350410588,71.0210843489409));
#200754=CARTESIAN_POINT('Ctrl Pts',(3.40868838939289,5.84842063971509,71.0293503967777));
#200755=CARTESIAN_POINT('Ctrl Pts',(3.25549998152355,5.9350618741357,71.0376164446146));
#200756=CARTESIAN_POINT('Ctrl Pts',(3.09910619832143,6.01563211736936,71.0458824924514));
#200757=CARTESIAN_POINT('Ctrl Pts',(3.09910619832131,6.01563211736941,69.0457552630242));
#200758=CARTESIAN_POINT('Ctrl Pts',(2.93375330764821,6.10081787314656,69.0545047109265));
#200759=CARTESIAN_POINT('Ctrl Pts',(2.76488627843062,6.17918207037043,69.0632541588288));
#200760=CARTESIAN_POINT('Ctrl Pts',(2.5930786664669,6.25045854554002,69.0720036067311));
#200761=CARTESIAN_POINT('Ctrl Pts',(2.42127244185368,6.3217344451504,69.0807529839814));
#200762=CARTESIAN_POINT('Ctrl Pts',(2.2465259467246,6.38592262741839,69.0895023612317));
#200763=CARTESIAN_POINT('Ctrl Pts',(2.06943269687121,6.44280508110562,69.098251738482));
#200764=CARTESIAN_POINT('Ctrl Pts',(1.89234081822074,6.49968709436167,69.1070010479874));
#200765=CARTESIAN_POINT('Ctrl Pts',(1.71290249405583,6.54926340459546,69.1157503574927));
#200766=CARTESIAN_POINT('Ctrl Pts',(1.53172716625051,6.59136563150385,69.1244996669981));
#200767=CARTESIAN_POINT('Ctrl Pts',(1.35055318107328,6.63346754640711,69.1332489116653));
#200768=CARTESIAN_POINT('Ctrl Pts',(1.16764249714415,6.66809542395777,69.1419981563325));
#200769=CARTESIAN_POINT('Ctrl Pts',(0.983616340614323,6.69513165624669,
69.1507474009998));
#200770=CARTESIAN_POINT('Ctrl Pts',(0.799591486713716,6.72216769715963,
69.1594965837355));
#200771=CARTESIAN_POINT('Ctrl Pts',(0.614451459526494,6.74161215869373,
69.1682457664712));
#200772=CARTESIAN_POINT('Ctrl Pts',(0.428825047909969,6.75339900185714,
69.1769949492069));
#200773=CARTESIAN_POINT('Ctrl Pts',(0.243199888596737,6.76518576550222,
69.1857440729174));
#200774=CARTESIAN_POINT('Ctrl Pts',(0.0570886373916137,6.76931499599834,
69.194493196628));
#200775=CARTESIAN_POINT('Ctrl Pts',(-0.128876626811447,6.76577266947846,
69.2032423203385));
#200776=CARTESIAN_POINT('Ctrl Pts',(-0.314840698188492,6.76223036567992,
69.21199138793));
#200777=CARTESIAN_POINT('Ctrl Pts',(-0.500658497951622,6.7510166087922,
69.2207404555216));
#200778=CARTESIAN_POINT('Ctrl Pts',(-0.685698951926621,6.73216948296214,
69.2294895231131));
#200779=CARTESIAN_POINT('Ctrl Pts',(-0.870738280460322,6.71332247176287,
69.2382385374916));
#200780=CARTESIAN_POINT('Ctrl Pts',(-1.05499998761304,6.68684221356178,
69.2469875518702));
#200781=CARTESIAN_POINT('Ctrl Pts',(-1.23785829161479,6.65281863948511,
69.2557365662487));
#200782=CARTESIAN_POINT('Ctrl Pts',(-1.43007412917462,6.61705395368849,
69.2649332999479));
#200783=CARTESIAN_POINT('Ctrl Pts',(-1.62073882535849,6.57295372727776,
69.2741300336471));
#200784=CARTESIAN_POINT('Ctrl Pts',(-1.8091369609157,6.52068343478264,69.2833267673463));
#200785=CARTESIAN_POINT('Ctrl Pts',(-1.98838356186171,6.47095219815181,
69.2920767650599));
#200786=CARTESIAN_POINT('Ctrl Pts',(-2.16557827572594,6.4138258685087,69.3008267627736));
#200787=CARTESIAN_POINT('Ctrl Pts',(-2.34011918621764,6.34949849943254,
69.3095767604873));
#200788=CARTESIAN_POINT('Ctrl Pts',(-2.51465655691164,6.28517243495525,
69.3183265807456));
#200789=CARTESIAN_POINT('Ctrl Pts',(-2.68653996295395,6.21364572242345,
69.3270764010039));
#200790=CARTESIAN_POINT('Ctrl Pts',(-2.85518555380057,6.13516132252189,
69.3358262212622));
#200791=CARTESIAN_POINT('Ctrl Pts',(-3.02382794858766,6.05667841000468,
69.3445758756997));
#200792=CARTESIAN_POINT('Ctrl Pts',(-3.18923239109367,5.97123819492035,
69.3533255301373));
#200793=CARTESIAN_POINT('Ctrl Pts',(-3.35083705967792,5.87913088810659,
69.3620751845748));
#200794=CARTESIAN_POINT('Ctrl Pts',(-3.51243888042485,5.78702520443051,
69.3708246848237));
#200795=CARTESIAN_POINT('Ctrl Pts',(-3.67024081223767,5.68825280605734,
69.3795741850726));
#200796=CARTESIAN_POINT('Ctrl Pts',(-3.82370687544469,5.58314917682458,
69.3883236853216));
#200797=CARTESIAN_POINT('Ctrl Pts',(-3.97717043817886,5.4780472600797,69.397073043012));
#200798=CARTESIAN_POINT('Ctrl Pts',(-4.12629803722535,5.36661448084179,
69.4058224007025));
#200799=CARTESIAN_POINT('Ctrl Pts',(-4.27058317206984,5.24922931204514,
69.414571758393));
#200800=CARTESIAN_POINT('Ctrl Pts',(-4.41486614774901,5.13184589986733,
69.4233209851531));
#200801=CARTESIAN_POINT('Ctrl Pts',(-4.5543065819447,5.00851045722983,69.4320702119131));
#200802=CARTESIAN_POINT('Ctrl Pts',(-4.68843089001892,4.87964187103074,
69.4408194386732));
#200803=CARTESIAN_POINT('Ctrl Pts',(-4.82255336917882,4.75077504207914,
69.4495685461291));
#200804=CARTESIAN_POINT('Ctrl Pts',(-4.95135966065179,4.61637541908045,
69.458317653585));
#200805=CARTESIAN_POINT('Ctrl Pts',(-5.07441230869288,4.47689945401795,
69.467066761041));
#200806=CARTESIAN_POINT('Ctrl Pts',(-5.19746344226455,4.3374252055547,69.4758157608173));
#200807=CARTESIAN_POINT('Ctrl Pts',(-5.31476088454799,4.19287495491296,
69.4845647605937));
#200808=CARTESIAN_POINT('Ctrl Pts',(-5.4259062762888,4.0437396158667,69.49331376037));
#200809=CARTESIAN_POINT('Ctrl Pts',(-5.53706380672693,3.89458798906698,
69.5020637156647));
#200810=CARTESIAN_POINT('Ctrl Pts',(-5.64206777071888,3.74085050155248,
69.5108136709594));
#200811=CARTESIAN_POINT('Ctrl Pts',(-5.7405614816403,3.58304938223125,69.5195636262541));
#200812=CARTESIAN_POINT('Ctrl Pts',(-5.83905138951903,3.42525435593249,
69.5283132436952));
#200813=CARTESIAN_POINT('Ctrl Pts',(-5.9310313955767,3.26339625497152,69.5370628611363));
#200814=CARTESIAN_POINT('Ctrl Pts',(-6.01618907820861,3.09802485064976,
69.5458124785775));
#200815=CARTESIAN_POINT('Ctrl Pts',(-6.1013439254499,2.93265895249625,69.5545618046933));
#200816=CARTESIAN_POINT('Ctrl Pts',(-6.17967677261832,2.76378023986033,
69.5633111308092));
#200817=CARTESIAN_POINT('Ctrl Pts',(-6.25092157009219,2.59196229227129,
69.572060456925));
#200818=CARTESIAN_POINT('Ctrl Pts',(-6.32216437407761,2.42014915229073,
69.5808095382275));
#200819=CARTESIAN_POINT('Ctrl Pts',(-6.3863194154894,2.24539720662801,69.58955861953));
#200820=CARTESIAN_POINT('Ctrl Pts',(-6.44316881037564,2.06829994947604,
69.5983077008325));
#200821=CARTESIAN_POINT('Ctrl Pts',(-6.50002334524597,1.89118668024363,
69.6070575731748));
#200822=CARTESIAN_POINT('Ctrl Pts',(-6.5495708241112,1.71172794807611,69.6158074455171));
#200823=CARTESIAN_POINT('Ctrl Pts',(-6.59164294296106,1.53053334250245,
69.6245573178595));
#200824=CARTESIAN_POINT('Ctrl Pts',(-6.63371214082156,1.34935131693493,
69.6333065827144));
#200825=CARTESIAN_POINT('Ctrl Pts',(-6.66830695239711,1.16643393829647,
69.6420558475693));
#200826=CARTESIAN_POINT('Ctrl Pts',(-6.69530988154007,0.982402458339712,
69.6508051124242));
#200827=CARTESIAN_POINT('Ctrl Pts',(-6.72231419690497,0.798361530945886,
69.6595548264312));
#200828=CARTESIAN_POINT('Ctrl Pts',(-6.74172580829287,0.613206671361408,
69.6683045404383));
#200829=CARTESIAN_POINT('Ctrl Pts',(-6.75347878028186,0.427566795112439,
69.6770542544453));
#200830=CARTESIAN_POINT('Ctrl Pts',(-6.76248992368216,0.28523449420484,
69.6837627642335));
#200831=CARTESIAN_POINT('Ctrl Pts',(-6.76699999999996,0.142617266092229,
69.6904712740218));
#200832=CARTESIAN_POINT('Ctrl Pts',(-6.767,2.06659797691628E-12,69.69717978381));
#200833=CARTESIAN_POINT('',(-6.76699385815225,-0.00911722160370732,69.3028202161582));
#200834=CARTESIAN_POINT('Ctrl Pts',(3.09910619832137,6.01563211736939,68.6512130080706));
#200835=CARTESIAN_POINT('Ctrl Pts',(2.93085026217071,6.10231345101066,68.6601304166315));
#200836=CARTESIAN_POINT('Ctrl Pts',(2.75908892941873,6.18186318284619,68.6690478251925));
#200837=CARTESIAN_POINT('Ctrl Pts',(2.58443008893269,6.25403950382626,68.6779652337535));
#200838=CARTESIAN_POINT('Ctrl Pts',(2.40942174209233,6.32636025541599,68.6869004867645));
#200839=CARTESIAN_POINT('Ctrl Pts',(2.23150453288923,6.39127799148669,68.6958357397755));
#200840=CARTESIAN_POINT('Ctrl Pts',(2.05130448005828,6.44859976507248,68.7047709927865));
#200841=CARTESIAN_POINT('Ctrl Pts',(1.94511179249288,6.48237973959225,68.7100365768772));
#200842=CARTESIAN_POINT('Ctrl Pts',(1.8381265741877,6.51352274644971,68.7153021609678));
#200843=CARTESIAN_POINT('Ctrl Pts',(1.73047874464825,6.54199757828759,68.7205677450584));
#200844=CARTESIAN_POINT('Ctrl Pts',(1.56237613924332,6.58646381082468,68.7287904691802));
#200845=CARTESIAN_POINT('Ctrl Pts',(1.39233485484454,6.6245057207038,68.737013193302));
#200846=CARTESIAN_POINT('Ctrl Pts',(1.22088691786,6.65595403633456,68.7452359174238));
#200847=CARTESIAN_POINT('Ctrl Pts',(1.04962045267677,6.68736906499445,68.7534499380722));
#200848=CARTESIAN_POINT('Ctrl Pts',(0.876950649677882,6.71220433284285,
68.7616639587206));
#200849=CARTESIAN_POINT('Ctrl Pts',(0.703423920370135,6.73034054028852,
68.769877979369));
#200850=CARTESIAN_POINT('Ctrl Pts',(0.530046023940738,6.7484611924133,68.7780849548991));
#200851=CARTESIAN_POINT('Ctrl Pts',(0.355813019738684,6.759894190205,68.7862919304292));
#200852=CARTESIAN_POINT('Ctrl Pts',(0.181280812215935,6.76457140306186,
68.7944989059593));
#200853=CARTESIAN_POINT('Ctrl Pts',(0.00686326885021005,6.76924554308376,
68.8027004896712));
#200854=CARTESIAN_POINT('Ctrl Pts',(-0.167852728981888,6.76717272938516,
68.8109020733832));
#200855=CARTESIAN_POINT('Ctrl Pts',(-0.342306770803061,6.75833670918092,
68.8191036570951));
#200856=CARTESIAN_POINT('Ctrl Pts',(-0.516681208078639,6.74950472091178,
68.8273014983695));
#200857=CARTESIAN_POINT('Ctrl Pts',(-0.690793569955339,6.73391569250349,
68.8354993396439));
#200858=CARTESIAN_POINT('Ctrl Pts',(-0.864083972708392,6.71160546278672,
68.8436971809184));
#200859=CARTESIAN_POINT('Ctrl Pts',(-1.03735908312204,6.68929720187837,
68.8518942987588));
#200860=CARTESIAN_POINT('Ctrl Pts',(-1.2098120222788,6.66026895834882,68.8600914165992));
#200861=CARTESIAN_POINT('Ctrl Pts',(-1.38088818471595,6.62460842777231,
68.8682885344396));
#200862=CARTESIAN_POINT('Ctrl Pts',(-1.55196244373833,6.58894829395932,
68.8764855610779));
#200863=CARTESIAN_POINT('Ctrl Pts',(-1.72165960505051,6.54665609224798,
68.8846825877162));
#200864=CARTESIAN_POINT('Ctrl Pts',(-1.88943553250399,6.49787060262909,
68.8928796143544));
#200865=CARTESIAN_POINT('Ctrl Pts',(-2.05724010001063,6.4490767851229,68.9010780402594));
#200866=CARTESIAN_POINT('Ctrl Pts',(-2.22312243568794,6.39378757157837,
68.9092764661645));
#200867=CARTESIAN_POINT('Ctrl Pts',(-2.38655378691528,6.33219156549771,
68.9174748920695));
#200868=CARTESIAN_POINT('Ctrl Pts',(-2.55004275365022,6.27057384458003,
68.9256762082184));
#200869=CARTESIAN_POINT('Ctrl Pts',(-2.71107867914499,6.20264502861652,
68.9338775243674));
#200870=CARTESIAN_POINT('Ctrl Pts',(-2.86915295785607,6.12864179932437,
68.9420788405164));
#200871=CARTESIAN_POINT('Ctrl Pts',(-3.02740725666124,6.05455429276454,
68.950289496589));
#200872=CARTESIAN_POINT('Ctrl Pts',(-3.18269284507116,5.97437870476695,
68.9585001526617));
#200873=CARTESIAN_POINT('Ctrl Pts',(-3.33452496020774,5.88839810897256,
68.9667108087343));
#200874=CARTESIAN_POINT('Ctrl Pts',(-3.4864465463123,5.80236684690689,68.9749263031467));
#200875=CARTESIAN_POINT('Ctrl Pts',(-3.6349102979326,5.71052394677286,68.983141797559));
#200876=CARTESIAN_POINT('Ctrl Pts',(-3.77946072793055,5.61319566789104,
68.9913572919714));
#200877=CARTESIAN_POINT('Ctrl Pts',(-3.92423543050626,5.51571638244359,
68.9995855328703));
#200878=CARTESIAN_POINT('Ctrl Pts',(-4.06508438856073,5.41273492224001,
69.0078137737691));
#200879=CARTESIAN_POINT('Ctrl Pts',(-4.2015844285781,5.30461848670855,69.016042014668));
#200880=CARTESIAN_POINT('Ctrl Pts',(-4.32564111756129,5.20635795129044,
69.0235201686813));
#200881=CARTESIAN_POINT('Ctrl Pts',(-4.44610593272397,5.10385660146879,
69.0309983226946));
#200882=CARTESIAN_POINT('Ctrl Pts',(-4.56268847893731,4.99741561651348,
69.0384764767079));
#200883=CARTESIAN_POINT('Ctrl Pts',(-4.68678626522264,4.88411314515715,
69.0464366936417));
#200884=CARTESIAN_POINT('Ctrl Pts',(-4.80691272293021,4.76595505720867,
69.0543969105755));
#200885=CARTESIAN_POINT('Ctrl Pts',(-4.92264556725855,4.64325851306491,
69.0623571275092));
#200886=CARTESIAN_POINT('Ctrl Pts',(-5.03823363716505,4.52071545448823,
69.0703073867183));
#200887=CARTESIAN_POINT('Ctrl Pts',(-5.14943876600774,4.3936455058644,69.0782576459274));
#200888=CARTESIAN_POINT('Ctrl Pts',(-5.2558708782261,4.26240663374752,69.0862079051364));
#200889=CARTESIAN_POINT('Ctrl Pts',(-5.36219426084468,4.13130183347927,
69.0941500424687));
#200890=CARTESIAN_POINT('Ctrl Pts',(-5.46375408763842,3.99603687626425,
69.102092179801));
#200891=CARTESIAN_POINT('Ctrl Pts',(-5.56019655573902,3.85700703415847,
69.1100343171333));
#200892=CARTESIAN_POINT('Ctrl Pts',(-5.65773929486102,3.71639105982909,
69.118067062926));
#200893=CARTESIAN_POINT('Ctrl Pts',(-5.75004689685807,3.57192403130099,
69.1260998087187));
#200894=CARTESIAN_POINT('Ctrl Pts',(-5.83679413100016,3.42405071112011,
69.1341325545114));
#200895=CARTESIAN_POINT('Ctrl Pts',(-5.92244724556388,3.27804247743251,
69.1420639854377));
#200896=CARTESIAN_POINT('Ctrl Pts',(-6.00267923238474,3.12871371410209,
69.149995416364));
#200897=CARTESIAN_POINT('Ctrl Pts',(-6.07721996602323,2.97652254897702,
69.1579268472902));
#200898=CARTESIAN_POINT('Ctrl Pts',(-6.1517403892892,2.82437285190715,69.165856117112));
#200899=CARTESIAN_POINT('Ctrl Pts',(-6.22057247550348,2.66936264776593,
69.1737853869337));
#200900=CARTESIAN_POINT('Ctrl Pts',(-6.28349206592725,2.51197461321353,
69.1817146567555));
#200901=CARTESIAN_POINT('Ctrl Pts',(-6.34640746558075,2.3545970615186,69.1896433984469));
#200902=CARTESIAN_POINT('Ctrl Pts',(-6.40341101168622,2.19484235030835,
69.1975721401382));
#200903=CARTESIAN_POINT('Ctrl Pts',(-6.45432681739407,2.03321281086555,
69.2055008818296));
#200904=CARTESIAN_POINT('Ctrl Pts',(-6.50640624890183,1.86788940270147,
69.213610826357));
#200905=CARTESIAN_POINT('Ctrl Pts',(-6.55211619024014,1.70060483428536,
69.2217207708844));
#200906=CARTESIAN_POINT('Ctrl Pts',(-6.59132264495505,1.53191213524234,
69.2298307154118));
#200907=CARTESIAN_POINT('Ctrl Pts',(-6.6296864870876,1.36684492572138,69.2377663636058));
#200908=CARTESIAN_POINT('Ctrl Pts',(-6.66182351159207,1.20042988543856,
69.2457020117998));
#200909=CARTESIAN_POINT('Ctrl Pts',(-6.68766023032856,1.03319390420274,
69.2536376599938));
#200910=CARTESIAN_POINT('Ctrl Pts',(-6.71434815464369,0.860448237250684,
69.2618347526879));
#200911=CARTESIAN_POINT('Ctrl Pts',(-6.73431347837947,0.686827057175144,
69.270031845382));
#200912=CARTESIAN_POINT('Ctrl Pts',(-6.74753347295097,0.512914253463772,
69.278228938076));
#200913=CARTESIAN_POINT('Ctrl Pts',(-6.76075346752246,0.339001449752463,
69.2864260307701));
#200914=CARTESIAN_POINT('Ctrl Pts',(-6.7672281747193,0.164797468529505,
69.2946231234641));
#200915=CARTESIAN_POINT('Ctrl Pts',(-6.76699385815225,-0.00911722160361701,
69.3028202161582));
#200916=CARTESIAN_POINT('Ctrl Pts',(-6.76699385815134,-0.00911722227638602,
69.3028202161899));
#200917=CARTESIAN_POINT('Ctrl Pts',(-6.76665361760903,-0.261650898689682,
69.3147228447278));
#200918=CARTESIAN_POINT('Ctrl Pts',(-6.75217477231416,-0.513499531784462,
69.3266254732657));
#200919=CARTESIAN_POINT('Ctrl Pts',(-6.72380134021238,-0.763403259986641,
69.3385281018036));
#200920=CARTESIAN_POINT('Ctrl Pts',(-6.70961211025288,-0.888377265756445,
69.3444804706548));
#200921=CARTESIAN_POINT('Ctrl Pts',(-6.69194860585264,-1.01286553647403,
69.3504328395061));
#200922=CARTESIAN_POINT('Ctrl Pts',(-6.67084484497365,-1.13671370814663,
69.3563852083574));
#200923=CARTESIAN_POINT('Ctrl Pts',(-6.64130098240993,-1.31009291688794,
69.3647181291235));
#200924=CARTESIAN_POINT('Ctrl Pts',(-6.60495559427541,-1.48254225000074,
69.3730510498896));
#200925=CARTESIAN_POINT('Ctrl Pts',(-6.56187774888001,-1.65349611694537,
69.3813839706556));
#200926=CARTESIAN_POINT('Ctrl Pts',(-6.51885081105692,-1.82424795785407,
69.3897070439291));
#200927=CARTESIAN_POINT('Ctrl Pts',(-6.46910734950525,-1.99350751863075,
69.3980301172025));
#200928=CARTESIAN_POINT('Ctrl Pts',(-6.41276783970255,-2.16071692594765,
69.4063531904759));
#200929=CARTESIAN_POINT('Ctrl Pts',(-6.35648456809074,-2.32775942456054,
69.4146679556439));
#200930=CARTESIAN_POINT('Ctrl Pts',(-6.29361847645192,-2.49275551924861,
69.422982720812));
#200931=CARTESIAN_POINT('Ctrl Pts',(-6.22434053338133,-2.65515986797524,
69.43129748598));
#200932=CARTESIAN_POINT('Ctrl Pts',(-6.15511903574275,-2.81743189488023,
69.4396054765458));
#200933=CARTESIAN_POINT('Ctrl Pts',(-6.07949623219774,-2.97711606483858,
69.4479134671115));
#200934=CARTESIAN_POINT('Ctrl Pts',(-5.99769221339464,-3.13368427149024,
69.4562214576773));
#200935=CARTESIAN_POINT('Ctrl Pts',(-5.91593984841844,-3.2901536156757,
69.4645242022965));
#200936=CARTESIAN_POINT('Ctrl Pts',(-5.8280142071297,-3.4435106100762,69.4728269469158));
#200937=CARTESIAN_POINT('Ctrl Pts',(-5.73418268706396,-3.5932489353475,
69.481129691535));
#200938=CARTESIAN_POINT('Ctrl Pts',(-5.64038951279486,-3.7429260675851,
69.4894290431009));
#200939=CARTESIAN_POINT('Ctrl Pts',(-5.54069545335148,-3.88898718300963,
69.4977283946668));
#200940=CARTESIAN_POINT('Ctrl Pts',(-5.43541300878158,-4.03095204932631,
69.5060277462326));
#200941=CARTESIAN_POINT('Ctrl Pts',(-5.33015295590187,-4.17288672225873,
69.5143253326751));
#200942=CARTESIAN_POINT('Ctrl Pts',(-5.2193070928737,-4.3107266024241,69.5226229191175));
#200943=CARTESIAN_POINT('Ctrl Pts',(-5.10323039913294,-4.4440216576166,
69.53092050556));
#200944=CARTESIAN_POINT('Ctrl Pts',(-4.98715910372594,-4.57731051370769,
69.5392177061098));
#200945=CARTESIAN_POINT('Ctrl Pts',(-4.86585769095836,-4.70605470377706,
69.5475149066596));
#200946=CARTESIAN_POINT('Ctrl Pts',(-4.7397205824734,-4.82983827887415,
69.5558121072094));
#200947=CARTESIAN_POINT('Ctrl Pts',(-4.61356838023744,-4.953636666095,69.5641103006144));
#200948=CARTESIAN_POINT('Ctrl Pts',(-4.48257957797818,-5.07247301230305,
69.5724084940193));
#200949=CARTESIAN_POINT('Ctrl Pts',(-4.34718464040284,-5.1859690224919,
69.5807066874243));
#200950=CARTESIAN_POINT('Ctrl Pts',(-4.21169447753411,-5.29954485612957,
69.5890107170734));
#200951=CARTESIAN_POINT('Ctrl Pts',(-4.07179225408218,-5.40777262487352,
69.5973147467224));
#200952=CARTESIAN_POINT('Ctrl Pts',(-3.92794133492156,-5.51031449823099,
69.6056187763714));
#200953=CARTESIAN_POINT('Ctrl Pts',(-3.78403810735694,-5.6128936588145,
69.6139258256087));
#200954=CARTESIAN_POINT('Ctrl Pts',(-3.636183609776,-5.70978260720938,69.6222328748459));
#200955=CARTESIAN_POINT('Ctrl Pts',(-3.48486941236484,-5.80068738847078,
69.6305399240832));
#200956=CARTESIAN_POINT('Ctrl Pts',(-3.33339343391278,-5.89168936266177,
69.6388558549924));
#200957=CARTESIAN_POINT('Ctrl Pts',(-3.17845066714642,-5.97669421330461,
69.6471717859017));
#200958=CARTESIAN_POINT('Ctrl Pts',(-3.02055742531773,-6.0554538921833,
69.6554877168109));
#200959=CARTESIAN_POINT('Ctrl Pts',(-2.90153384758541,-6.11482475981906,
69.6617564578763));
#200960=CARTESIAN_POINT('Ctrl Pts',(-2.7808341726981,-6.17064776489301,
69.6680251989417));
#200961=CARTESIAN_POINT('Ctrl Pts',(-2.65868658361936,-6.2228349367537,
69.674293940007));
#200962=CARTESIAN_POINT('Ctrl Pts',(-2.49403137172798,-6.2931833562808,
69.6827442163997));
#200963=CARTESIAN_POINT('Ctrl Pts',(-2.32644257904295,-6.35705238656149,
69.6911944927923));
#200964=CARTESIAN_POINT('Ctrl Pts',(-2.15645702901611,-6.41420159349603,
69.6996447691849));
#200965=CARTESIAN_POINT('Ctrl Pts',(-1.98662149816884,-6.47130036392502,
69.7080875878641));
#200966=CARTESIAN_POINT('Ctrl Pts',(-1.81439373885687,-6.52169102642675,
69.7165304065432));
#200967=CARTESIAN_POINT('Ctrl Pts',(-1.64033030242613,-6.56518129977708,
69.7249732252224));
#200968=CARTESIAN_POINT('Ctrl Pts',(-1.46639678524654,-6.60863911241158,
69.733409742264));
#200969=CARTESIAN_POINT('Ctrl Pts',(-1.2906306428674,-6.64520672278109,
69.7418462593056));
#200970=CARTESIAN_POINT('Ctrl Pts',(-1.11360371186735,-6.67474162592945,
69.7502827763472));
#200971=CARTESIAN_POINT('Ctrl Pts',(-0.936703456296356,-6.70425539474244,
69.7587132564576));
#200972=CARTESIAN_POINT('Ctrl Pts',(-0.758544537924352,-6.72674643984214,
69.7671437365679));
#200973=CARTESIAN_POINT('Ctrl Pts',(-0.579709319837329,-6.74212326381636,
69.7755742166783));
#200974=CARTESIAN_POINT('Ctrl Pts',(-0.40095098455304,-6.75749347716132,
69.7840010724525));
#200975=CARTESIAN_POINT('Ctrl Pts',(-0.221517258924335,-6.76575553818316,
69.7924279282268));
#200976=CARTESIAN_POINT('Ctrl Pts',(-0.0419966274007469,-6.76686968126969,
69.800854784001));
#200977=CARTESIAN_POINT('Ctrl Pts',(0.137468588909518,-6.76798348043766,
69.8092790385366));
#200978=CARTESIAN_POINT('Ctrl Pts',(0.317020326428212,-6.76195375980029,
69.8177032930721));
#200979=CARTESIAN_POINT('Ctrl Pts',(0.496068720137571,-6.74879284204969,
69.8261275476077));
#200980=CARTESIAN_POINT('Ctrl Pts',(0.546516717905963,-6.74508467167431,
69.8285011336824));
#200981=CARTESIAN_POINT('Ctrl Pts',(0.596924762029775,-6.74081069757095,
69.8308747197571));
#200982=CARTESIAN_POINT('Ctrl Pts',(0.647279686896179,-6.73597194226131,
69.8332483058319));
#200983=CARTESIAN_POINT('Ctrl Pts',(0.83012424644261,-6.71840186176389,
69.841867071554));
#200984=CARTESIAN_POINT('Ctrl Pts',(1.01218623286149,-6.69338904782141,
69.8504858372761));
#200985=CARTESIAN_POINT('Ctrl Pts',(1.19285747028278,-6.66103445836985,
69.8591046029982));
#200986=CARTESIAN_POINT('Ctrl Pts',(1.37363723248664,-6.62866043430969,
69.8677285458016));
#200987=CARTESIAN_POINT('Ctrl Pts',(1.55302427909818,-6.58893588728978,
69.8763524886049));
#200988=CARTESIAN_POINT('Ctrl Pts',(1.73042144915389,-6.54201273373174,
69.8849764314083));
#200989=CARTESIAN_POINT('Ctrl Pts',(1.91422785891201,-6.4933942783904,69.8939119514289));
#200990=CARTESIAN_POINT('Ctrl Pts',(2.09589757769514,-6.43704745443902,
69.9028474714496));
#200991=CARTESIAN_POINT('Ctrl Pts',(2.27478504603368,-6.37319715639973,
69.9117829914703));
#200992=CARTESIAN_POINT('Ctrl Pts',(2.44775758702257,-6.3114580731798,69.9204230578617));
#200993=CARTESIAN_POINT('Ctrl Pts',(2.61812865798086,-6.2427039361286,69.9290631242531));
#200994=CARTESIAN_POINT('Ctrl Pts',(2.78533590748944,-6.16718678835415,
69.9377031906445));
#200995=CARTESIAN_POINT('Ctrl Pts',(2.96111982524427,-6.08779609128523,
69.9467864374799));
#200996=CARTESIAN_POINT('Ctrl Pts',(3.13340647645933,-6.00093053651775,
69.9558696843152));
#200997=CARTESIAN_POINT('Ctrl Pts',(3.30157228940492,-5.90693739748726,
69.9649529311505));
#200998=CARTESIAN_POINT('Ctrl Pts',(3.46973810235057,-5.81294425845674,
69.9740361779858));
#200999=CARTESIAN_POINT('Ctrl Pts',(3.633782764579,-5.71182376729964,69.9831194248212));
#201000=CARTESIAN_POINT('Ctrl Pts',(3.79311806221927,-5.603975764229,69.9922026716565));
#201001=CARTESIAN_POINT('Ctrl Pts',(3.95177566344159,-5.49658646808924,
70.0012472849691));
#201002=CARTESIAN_POINT('Ctrl Pts',(4.10591088612372,-5.38242831851227,
70.0102918982817));
#201003=CARTESIAN_POINT('Ctrl Pts',(4.25497498377582,-5.2618890987403,70.0193365115943));
#201004=CARTESIAN_POINT('Ctrl Pts',(4.40390228927358,-5.14146049460157,
70.028372824906));
#201005=CARTESIAN_POINT('Ctrl Pts',(4.54776757593037,-5.01466266073103,
70.0374091382178));
#201006=CARTESIAN_POINT('Ctrl Pts',(4.6860539502047,-4.88192455654232,70.0464454515295));
#201007=CARTESIAN_POINT('Ctrl Pts',(4.8240956070903,-4.74942135129006,70.0554657738009));
#201008=CARTESIAN_POINT('Ctrl Pts',(4.95657789467508,-4.610999031669,70.0644860960722));
#201009=CARTESIAN_POINT('Ctrl Pts',(5.08301975945316,-4.46712425672365,
70.0735064183435));
#201010=CARTESIAN_POINT('Ctrl Pts',(5.20930238895615,-4.32343067128705,
70.0825153808212));
#201011=CARTESIAN_POINT('Ctrl Pts',(5.32955962012002,-4.17429851201609,
70.0915243432988));
#201012=CARTESIAN_POINT('Ctrl Pts',(5.44334799706848,-4.02023028977329,
70.1005333057765));
#201013=CARTESIAN_POINT('Ctrl Pts',(5.55687797233936,-3.86651194058568,
70.1095218098288));
#201014=CARTESIAN_POINT('Ctrl Pts',(5.66396827503575,-3.70788009414105,
70.1185103138811));
#201015=CARTESIAN_POINT('Ctrl Pts',(5.76421668031801,-3.54486883570375,
70.1274988179333));
#201016=CARTESIAN_POINT('Ctrl Pts',(5.8521697207688,-3.40185074213007,70.135384891116));
#201017=CARTESIAN_POINT('Ctrl Pts',(5.93485673755005,-3.25546220835644,
70.1432709642987));
#201018=CARTESIAN_POINT('Ctrl Pts',(6.01203190609037,-3.10608457066955,
70.1511570374813));
#201019=CARTESIAN_POINT('Ctrl Pts',(6.09151067956367,-2.95224815343529,
70.1592785024024));
#201020=CARTESIAN_POINT('Ctrl Pts',(6.16510661331008,-2.79530964361943,
70.1673999673235));
#201021=CARTESIAN_POINT('Ctrl Pts',(6.23257786278774,-2.63576595779826,
70.1755214322446));
#201022=CARTESIAN_POINT('Ctrl Pts',(6.30004430105979,-2.47623364863726,
70.1836423180444));
#201023=CARTESIAN_POINT('Ctrl Pts',(6.36138678234842,-2.31409687076289,
70.1917632038442));
#201024=CARTESIAN_POINT('Ctrl Pts',(6.41641132721038,-2.14987317766569,
70.199884089644));
#201025=CARTESIAN_POINT('Ctrl Pts',(6.47144244947437,-1.9856298539608,70.2080059461802));
#201026=CARTESIAN_POINT('Ctrl Pts',(6.52015401630036,-1.81929946588932,
70.2161278027164));
#201027=CARTESIAN_POINT('Ctrl Pts',(6.56240171911994,-1.65141535565455,
70.2242496592526));
#201028=CARTESIAN_POINT('Ctrl Pts',(6.6046802457916,-1.4834087574587,70.2323774414816));
#201029=CARTESIAN_POINT('Ctrl Pts',(6.64048539981623,-1.31384652848552,
70.2405052237105));
#201030=CARTESIAN_POINT('Ctrl Pts',(6.66972373877747,-1.14327347926393,
70.2486330059394));
#201031=CARTESIAN_POINT('Ctrl Pts',(6.69897398852963,-0.97263094388149,
70.2567640991743));
#201032=CARTESIAN_POINT('Ctrl Pts',(6.72165204303201,-0.800977130240748,
70.2648951924092));
#201033=CARTESIAN_POINT('Ctrl Pts',(6.7377163131901,-0.628862372043433,
70.2730262856441));
#201034=CARTESIAN_POINT('Ctrl Pts',(6.75379811697253,-0.456559756228839,
70.2811662537008));
#201035=CARTESIAN_POINT('Ctrl Pts',(6.76325169822012,-0.283795556184407,
70.2893062217574));
#201036=CARTESIAN_POINT('Ctrl Pts',(6.7660875743135,-0.111121270333465,
70.2974461898141));
#201037=CARTESIAN_POINT('Ctrl Pts',(6.76755838172983,-0.021564952681512,
70.3016679276447));
#201038=CARTESIAN_POINT('Ctrl Pts',(6.76724994423267,0.0679672234920894,
70.3058896654754));
#201039=CARTESIAN_POINT('Ctrl Pts',(6.76516922120448,0.157398883311155,
70.310111403306));
#201040=CARTESIAN_POINT('Ctrl Pts',(6.76100939962017,0.336192381434253,
70.3185515829519));
#201041=CARTESIAN_POINT('Ctrl Pts',(6.74975428889474,0.514953378025566,
70.3269917625978));
#201042=CARTESIAN_POINT('Ctrl Pts',(6.73141204075728,0.69309518649888,70.3354319422436));
#201043=CARTESIAN_POINT('Ctrl Pts',(6.71308369016171,0.871102020609852,
70.34386572694));
#201044=CARTESIAN_POINT('Ctrl Pts',(6.68767894047735,1.04849027127232,70.3522995116364));
#201045=CARTESIAN_POINT('Ctrl Pts',(6.65525793640312,1.22467579380965,70.3607332963328));
#201046=CARTESIAN_POINT('Ctrl Pts',(6.62285651279589,1.40075491017886,70.3691619874966));
#201047=CARTESIAN_POINT('Ctrl Pts',(6.58344734291239,1.57563241940692,70.3775906786603));
#201048=CARTESIAN_POINT('Ctrl Pts',(6.53714214287557,1.74873142701793,70.3860193698241));
#201049=CARTESIAN_POINT('Ctrl Pts',(6.49085779765335,1.9217524747517,70.394444264896));
#201050=CARTESIAN_POINT('Ctrl Pts',(6.43768370096074,2.09299629634186,70.4028691599679));
#201051=CARTESIAN_POINT('Ctrl Pts',(6.37778228720542,2.26189789712287,70.4112940550398));
#201052=CARTESIAN_POINT('Ctrl Pts',(6.31789866052679,2.43074934440101,70.4197164484303));
#201053=CARTESIAN_POINT('Ctrl Pts',(6.251291811796,2.59725964387249,70.4281388418207));
#201054=CARTESIAN_POINT('Ctrl Pts',(6.1781736163657,2.76088025202882,70.4365612352112));
#201055=CARTESIAN_POINT('Ctrl Pts',(6.10505426995744,2.92450343579186,70.4449837611814));
#201056=CARTESIAN_POINT('Ctrl Pts',(6.0254235020109,3.08523653024769,70.4534062871516));
#201057=CARTESIAN_POINT('Ctrl Pts',(5.93954106611889,3.24255160697364,70.4618288131218));
#201058=CARTESIAN_POINT('Ctrl Pts',(5.85365572792102,3.39987199999579,70.4702516237223));
#201059=CARTESIAN_POINT('Ctrl Pts',(5.76151846022177,3.55377385210287,70.4786744343228));
#201060=CARTESIAN_POINT('Ctrl Pts',(5.66343472902432,3.70375432096694,70.4870972449233));
#201061=CARTESIAN_POINT('Ctrl Pts',(5.56533398886973,3.85376079833756,70.4955215161456));
#201062=CARTESIAN_POINT('Ctrl Pts',(5.46128491189105,3.99984425754618,70.5039457873678));
#201063=CARTESIAN_POINT('Ctrl Pts',(5.35163619679929,4.14153099917261,70.51237005859));
#201064=CARTESIAN_POINT('Ctrl Pts',(5.24195315353632,4.28326209924611,70.5207969672332));
#201065=CARTESIAN_POINT('Ctrl Pts',(5.12666718102087,4.42059347367828,70.5292238758764));
#201066=CARTESIAN_POINT('Ctrl Pts',(5.00616736453775,4.55308437416189,70.5376507845196));
#201067=CARTESIAN_POINT('Ctrl Pts',(4.88555919513755,4.68569440989378,70.5460852706028));
#201068=CARTESIAN_POINT('Ctrl Pts',(4.7597280385235,4.81345502761942,70.5545197566861));
#201069=CARTESIAN_POINT('Ctrl Pts',(4.6291007575472,4.93596142372243,70.5629542427694));
#201070=CARTESIAN_POINT('Ctrl Pts',(4.49841037744726,5.05852699617954,70.5713928031063));
#201071=CARTESIAN_POINT('Ctrl Pts',(4.36291950116576,5.17583306310957,70.5798313634432));
#201072=CARTESIAN_POINT('Ctrl Pts',(4.22308859466462,5.28751470178699,70.5882699237801));
#201073=CARTESIAN_POINT('Ctrl Pts',(4.08310137591308,5.3993211855985,70.5967179172988));
#201074=CARTESIAN_POINT('Ctrl Pts',(3.93876469835609,5.50549047618272,70.6051659108175));
#201075=CARTESIAN_POINT('Ctrl Pts',(3.79056955085271,5.60569990992635,70.6136139043362));
#201076=CARTESIAN_POINT('Ctrl Pts',(3.70633126528106,5.66266176757744,70.6184159812093));
#201077=CARTESIAN_POINT('Ctrl Pts',(3.62084677305327,5.71769874142581,70.6232180580824));
#201078=CARTESIAN_POINT('Ctrl Pts',(3.5342098779379,5.77075814245288,70.6280201349556));
#201079=CARTESIAN_POINT('Ctrl Pts',(3.39243104307275,5.85758835544981,70.6358785982938));
#201080=CARTESIAN_POINT('Ctrl Pts',(3.24726311766159,5.93930530447707,70.643737061632));
#201081=CARTESIAN_POINT('Ctrl Pts',(3.0991061983213,6.01563211736942,70.6515955249703));
#201082=CARTESIAN_POINT('Origin',(0.,0.,4.30282021618968));
#201083=CARTESIAN_POINT('',(3.09910619832135,6.0156321173694,73.0457552630242));
#201084=CARTESIAN_POINT('',(3.09910619832134,6.0156321173694,72.6513713193949));
#201085=CARTESIAN_POINT('',(3.09910619832133,6.0156321173694,4.30282021618968));
#201086=CARTESIAN_POINT('',(-6.76699982792737,0.000627241189940232,71.69717978381));
#201087=CARTESIAN_POINT('Ctrl Pts',(-6.767,2.40452268012357E-12,71.69717978381));
#201088=CARTESIAN_POINT('Ctrl Pts',(-6.76700000000007,-0.186007249524524,
71.7059292956212));
#201089=CARTESIAN_POINT('Ctrl Pts',(-6.75932637294533,-0.372014355747631,
71.7146788074324));
#201090=CARTESIAN_POINT('Ctrl Pts',(-6.74400518264199,-0.557389537485268,
71.7234283192436));
#201091=CARTESIAN_POINT('Ctrl Pts',(-6.72868405705108,-0.742763936249769,
71.7321777940992));
#201092=CARTESIAN_POINT('Ctrl Pts',(-6.70571545645751,-0.927506130240439,
71.7409272689549));
#201093=CARTESIAN_POINT('Ctrl Pts',(-6.67517739404828,-1.11098863989998,
71.7496767438106));
#201094=CARTESIAN_POINT('Ctrl Pts',(-6.64463945808704,-1.29447038981933,
71.7584261824376));
#201095=CARTESIAN_POINT('Ctrl Pts',(-6.60653217008357,-1.47669218313674,
71.7671756210646));
#201096=CARTESIAN_POINT('Ctrl Pts',(-6.56098496092678,-1.6570351059928,
71.7759250596916));
#201097=CARTESIAN_POINT('Ctrl Pts',(-6.51543793658297,-1.83737729708699,
71.7846744628168));
#201098=CARTESIAN_POINT('Ctrl Pts',(-6.4624511216742,-2.01584035510929,
71.793423865942));
#201099=CARTESIAN_POINT('Ctrl Pts',(-6.40220448374251,-2.19181813760798,
71.8021732690671));
#201100=CARTESIAN_POINT('Ctrl Pts',(-6.341958085265,-2.36779522067153,71.8109226374172));
#201101=CARTESIAN_POINT('Ctrl Pts',(-6.27445201433099,-2.54128677684177,
71.8196720057673));
#201102=CARTESIAN_POINT('Ctrl Pts',(-6.19991555071896,-2.71170355384825,
71.8284213741174));
#201103=CARTESIAN_POINT('Ctrl Pts',(-6.12537937716686,-2.8821196676749,
71.8371707084192));
#201104=CARTESIAN_POINT('Ctrl Pts',(-6.04381298052514,-3.04946076371797,
71.845920042721));
#201105=CARTESIAN_POINT('Ctrl Pts',(-5.95549339335826,-3.21315848374558,
71.8546693770228));
#201106=CARTESIAN_POINT('Ctrl Pts',(-5.86717414255411,-3.37685558033488,
71.8634186780029));
#201107=CARTESIAN_POINT('Ctrl Pts',(-5.77210188876609,-3.53690907646737,
71.8721679789831));
#201108=CARTESIAN_POINT('Ctrl Pts',(-5.67059953347017,-3.69277536969254,
71.8809172799633));
#201109=CARTESIAN_POINT('Ctrl Pts',(-5.56909755631399,-3.84864108224901,
71.8896665483486));
#201110=CARTESIAN_POINT('Ctrl Pts',(-5.46116568196859,-4.00031938297506,
71.8984158167339));
#201111=CARTESIAN_POINT('Ctrl Pts',(-5.34717048533604,-4.14729511859852,
71.9071650851192));
#201112=CARTESIAN_POINT('Ctrl Pts',(-5.23317570391827,-4.29427031887929,
71.9159143216362));
#201113=CARTESIAN_POINT('Ctrl Pts',(-5.11311782003492,-4.43654276189573,
71.9246635581533));
#201114=CARTESIAN_POINT('Ctrl Pts',(-4.98740458984718,-4.57362924351891,
71.9334127946703));
#201115=CARTESIAN_POINT('Ctrl Pts',(-4.86169180711711,-4.710715237203,71.9421620000458));
#201116=CARTESIAN_POINT('Ctrl Pts',(-4.73032391204143,-4.84261509523266,
71.9509112054212));
#201117=CARTESIAN_POINT('Ctrl Pts',(-4.59374707013574,-4.96888084538353,
71.9596604107966));
#201118=CARTESIAN_POINT('Ctrl Pts',(-4.45717070301414,-5.09514615659491,
71.9684095857571));
#201119=CARTESIAN_POINT('Ctrl Pts',(-4.31538563571003,-5.21577720459559,
71.9771587607175));
#201120=CARTESIAN_POINT('Ctrl Pts',(-4.16887341029464,-5.33036429232921,
71.985907935678));
#201121=CARTESIAN_POINT('Ctrl Pts',(-4.02236168203657,-5.44495099123652,
71.99465708095));
#201122=CARTESIAN_POINT('Ctrl Pts',(-3.87112305348112,-5.55349359438639,
72.003406226222));
#201123=CARTESIAN_POINT('Ctrl Pts',(-3.71567117017702,-5.65562346298932,
72.0121553714941));
#201124=CARTESIAN_POINT('Ctrl Pts',(-3.5602198014578,-5.75775299351668,
72.0209044878042));
#201125=CARTESIAN_POINT('Ctrl Pts',(-3.4005554453833,-5.85346967463883,
72.0296536041144));
#201126=CARTESIAN_POINT('Ctrl Pts',(-3.23722035986856,-5.942448429869,72.0384027204245));
#201127=CARTESIAN_POINT('Ctrl Pts',(-3.07388580147188,-6.03142689794525,
72.0471518084994));
#201128=CARTESIAN_POINT('Ctrl Pts',(-2.90688078896591,-6.11366734656775,
72.0559008965742));
#201129=CARTESIAN_POINT('Ctrl Pts',(-2.73677250721389,-6.18889046952345,
72.064649984649));
#201130=CARTESIAN_POINT('Ctrl Pts',(-2.56666476031491,-6.26411335596324,
72.0733990452151));
#201131=CARTESIAN_POINT('Ctrl Pts',(-2.39345402575164,-6.33231884500557,
72.0821481057811));
#201132=CARTESIAN_POINT('Ctrl Pts',(-2.21772856065579,-6.39327529762731,
72.0908971663472));
#201133=CARTESIAN_POINT('Ctrl Pts',(-2.04200363348509,-6.45423156365112,
72.0996462001308));
#201134=CARTESIAN_POINT('Ctrl Pts',(-1.86376426189281,-6.50793874375657,
72.1083952339145));
#201135=CARTESIAN_POINT('Ctrl Pts',(-1.68361577753164,-6.55421443909539,
72.1171442676982));
#201136=CARTESIAN_POINT('Ctrl Pts',(-1.50346782967816,-6.60048999661864,
72.1258932754261));
#201137=CARTESIAN_POINT('Ctrl Pts',(-1.32141105795011,-6.63933404237707,
72.1346422831539));
#201138=CARTESIAN_POINT('Ctrl Pts',(-1.13806375487053,-6.67061465607556,
72.1433912908817));
#201139=CARTESIAN_POINT('Ctrl Pts',(-0.954716982603581,-6.70189517921288,
72.1521402732801));
#201140=CARTESIAN_POINT('Ctrl Pts',(-0.770079968902963,-6.72561226592218,
72.1608892556785));
#201141=CARTESIAN_POINT('Ctrl Pts',(-0.584779765559332,-6.74168536983093,
72.1696382380769));
#201142=CARTESIAN_POINT('Ctrl Pts',(-0.391489830652384,-6.75845151013847,
72.1787644570868));
#201143=CARTESIAN_POINT('Ctrl Pts',(-0.197478578239416,-6.76689983031622,
72.1878906760966));
#201144=CARTESIAN_POINT('Ctrl Pts',(-0.0034628764524202,-6.76699911397118,
72.1970168951065));
#201145=CARTESIAN_POINT('Ctrl Pts',(0.1844898346537,-6.76709529501191,72.2058579197723));
#201146=CARTESIAN_POINT('Ctrl Pts',(0.372446404249175,-6.75935639738169,
72.2146989444381));
#201147=CARTESIAN_POINT('Ctrl Pts',(0.559755019488135,-6.74380925873188,
72.2235399691039));
#201148=CARTESIAN_POINT('Ctrl Pts',(0.745134705521623,-6.72842222659807,
72.2322899477137));
#201149=CARTESIAN_POINT('Ctrl Pts',(0.929879431228464,-6.70538706057525,
72.2410399263234));
#201150=CARTESIAN_POINT('Ctrl Pts',(1.1133616362682,-6.67478200894128,72.2497899049331));
#201151=CARTESIAN_POINT('Ctrl Pts',(1.29684196300732,-6.6441772706101,72.2585397939697));
#201152=CARTESIAN_POINT('Ctrl Pts',(1.47905951217543,-6.60600284890583,
72.2672896830062));
#201153=CARTESIAN_POINT('Ctrl Pts',(1.65939532067136,-6.56038841607218,
72.2760395720427));
#201154=CARTESIAN_POINT('Ctrl Pts',(1.83972934300849,-6.51477443503243,
72.2847893744149));
#201155=CARTESIAN_POINT('Ctrl Pts',(2.01818138406308,-6.46172066062127,
72.2935391767871));
#201156=CARTESIAN_POINT('Ctrl Pts',(2.19414528354239,-6.40140730423465,
72.3022889791592));
#201157=CARTESIAN_POINT('Ctrl Pts',(2.37010749864034,-6.34109452518629,
72.3110386977755));
#201158=CARTESIAN_POINT('Ctrl Pts',(2.5435813486649,-6.27352239616492,72.3197884163918));
#201159=CARTESIAN_POINT('Ctrl Pts',(2.71397759435581,-6.19892043966808,
72.3285381350081));
#201160=CARTESIAN_POINT('Ctrl Pts',(2.8843722655814,-6.12431917249507,72.3372877727768));
#201161=CARTESIAN_POINT('Ctrl Pts',(3.05168912680962,-6.04268832278795,
72.3460374105456));
#201162=CARTESIAN_POINT('Ctrl Pts',(3.21535986273852,-5.95430516123335,
72.3547870483143));
#201163=CARTESIAN_POINT('Ctrl Pts',(3.37902914072853,-5.86592278697435,
72.3635366081433));
#201164=CARTESIAN_POINT('Ctrl Pts',(3.53905210621596,-5.77078835741928,
72.3722861679724));
#201165=CARTESIAN_POINT('Ctrl Pts',(3.69488522831733,-5.66922500431606,
72.3810357278015));
#201166=CARTESIAN_POINT('Ctrl Pts',(3.85071701406976,-5.56766252217068,
72.3897852125986));
#201167=CARTESIAN_POINT('Ctrl Pts',(4.00235878822441,-5.45967138329342,
72.3985346973957));
#201168=CARTESIAN_POINT('Ctrl Pts',(4.14929549611363,-5.34561838199578,
72.4072841821929));
#201169=CARTESIAN_POINT('Ctrl Pts',(4.29623099276135,-5.23156632086979,
72.4160335948655));
#201170=CARTESIAN_POINT('Ctrl Pts',(4.43846127436079,-5.1114526730492,72.424783007538));
#201171=CARTESIAN_POINT('Ctrl Pts',(4.57550326054499,-4.98568540049833,
72.4335324202106));
#201172=CARTESIAN_POINT('Ctrl Pts',(4.71254416257839,-4.85991912290304,
72.4422817636659));
#201173=CARTESIAN_POINT('Ctrl Pts',(4.84439664018822,-4.72849950385357,
72.4510311071211));
#201174=CARTESIAN_POINT('Ctrl Pts',(4.97061286794807,-4.59187289861001,
72.4597804505764));
#201175=CARTESIAN_POINT('Ctrl Pts',(5.09682813912745,-4.45524732884616,
72.4685297277212));
#201176=CARTESIAN_POINT('Ctrl Pts',(5.21740705147897,-4.31341506235717,
72.477279004866));
#201177=CARTESIAN_POINT('Ctrl Pts',(5.33194007545752,-4.16685781275652,
72.4860282820109));
#201178=CARTESIAN_POINT('Ctrl Pts',(5.4464722694454,-4.02030162521768,72.494777495752));
#201179=CARTESIAN_POINT('Ctrl Pts',(5.55495848628166,-3.86902074887858,
72.5035267094931));
#201180=CARTESIAN_POINT('Ctrl Pts',(5.65703027291839,-3.71352898080585,
72.5122759232342));
#201181=CARTESIAN_POINT('Ctrl Pts',(5.75910135377053,-3.55803828789498,
72.5210250764781));
#201182=CARTESIAN_POINT('Ctrl Pts',(5.85475793592812,-3.3983370010661,72.529774229722));
#201183=CARTESIAN_POINT('Ctrl Pts',(5.94367514427461,-3.23496750823438,
72.5385233829659));
#201184=CARTESIAN_POINT('Ctrl Pts',(6.03259176732693,-3.07159909077619,
72.5472724786188));
#201185=CARTESIAN_POINT('Ctrl Pts',(6.11476896835969,-2.90456276731339,
72.5560215742717));
#201186=CARTESIAN_POINT('Ctrl Pts',(6.18992765547923,-2.73442583002966,
72.5647706699247));
#201187=CARTESIAN_POINT('Ctrl Pts',(6.26508587283093,-2.56428995616076,
72.5735197108927));
#201188=CARTESIAN_POINT('Ctrl Pts',(6.333225548272,-2.39105376935097,72.5822687518607));
#201189=CARTESIAN_POINT('Ctrl Pts',(6.3941152673307,-2.21530561053964,72.5910177928288));
#201190=CARTESIAN_POINT('Ctrl Pts',(6.45500462602884,-2.03955849184981,
72.5997667820178));
#201191=CARTESIAN_POINT('Ctrl Pts',(6.50864402040774,-1.86129970164427,
72.6085157712068));
#201192=CARTESIAN_POINT('Ctrl Pts',(6.55485128368631,-1.68113463135939,
72.6172647603958));
#201193=CARTESIAN_POINT('Ctrl Pts',(6.60199809554351,-1.49730620116761,
72.6261916458673));
#201194=CARTESIAN_POINT('Ctrl Pts',(6.64140720707892,-1.31149343245602,
72.6351185313387));
#201195=CARTESIAN_POINT('Ctrl Pts',(6.67293928722898,-1.12435326697442,
72.6440454168101));
#201196=CARTESIAN_POINT('Ctrl Pts',(6.70384625876269,-0.940923067005743,
72.6527953309876));
#201197=CARTESIAN_POINT('Ctrl Pts',(6.72718554579806,-0.75621789952081,
72.6615452451651));
#201198=CARTESIAN_POINT('Ctrl Pts',(6.74287786815335,-0.570865181253636,
72.6702951593425));
#201199=CARTESIAN_POINT('Ctrl Pts',(6.7585698819085,-0.385516108073125,
72.679044901447));
#201200=CARTESIAN_POINT('Ctrl Pts',(6.76661520773405,-0.199519795225566,
72.6877946435515));
#201201=CARTESIAN_POINT('Ctrl Pts',(6.76698651789579,-0.0135080204549074,
72.696544385656));
#201202=CARTESIAN_POINT('Ctrl Pts',(6.76735782124901,0.172500343513724,
72.705293967321));
#201203=CARTESIAN_POINT('Ctrl Pts',(6.7600553899518,0.358523882211705,72.7140435489859));
#201204=CARTESIAN_POINT('Ctrl Pts',(6.74510402742355,0.543930748565181,
72.7227931306509));
#201205=CARTESIAN_POINT('Ctrl Pts',(6.73015291918022,0.729334461616064,
72.7315425635076));
#201206=CARTESIAN_POINT('Ctrl Pts',(6.70755316306583,0.914121237635533,
72.7402919963642));
#201207=CARTESIAN_POINT('Ctrl Pts',(6.6773815187456,1.09766345166209,72.7490414292209));
#201208=CARTESIAN_POINT('Ctrl Pts',(6.64721034747552,1.28120278799754,72.7577907248985));
#201209=CARTESIAN_POINT('Ctrl Pts',(6.60946757205121,1.46349731860421,72.766540020576));
#201210=CARTESIAN_POINT('Ctrl Pts',(6.56428138111499,1.64392790278256,72.7752893162535));
#201211=CARTESIAN_POINT('Ctrl Pts',(6.51909583859826,1.82435589779142,72.7840384863791));
#201212=CARTESIAN_POINT('Ctrl Pts',(6.46646716392851,2.00291972192344,72.7927876565047));
#201213=CARTESIAN_POINT('Ctrl Pts',(6.40657409872859,2.17901292274734,72.8015368266303));
#201214=CARTESIAN_POINT('Ctrl Pts',(6.34668181342048,2.35510383059054,72.8102858828294));
#201215=CARTESIAN_POINT('Ctrl Pts',(6.27952541914017,2.52872390822663,72.8190349390286));
#201216=CARTESIAN_POINT('Ctrl Pts',(6.20533299175478,2.69928350890373,72.8277839952277));
#201217=CARTESIAN_POINT('Ctrl Pts',(6.12831602991508,2.87633637965711,72.8368661313858));
#201218=CARTESIAN_POINT('Ctrl Pts',(6.04371690605227,3.05009086601548,72.845948267544));
#201219=CARTESIAN_POINT('Ctrl Pts',(5.95184520316585,3.2199111288282,72.8550304037022));
#201220=CARTESIAN_POINT('Ctrl Pts',(5.86333549509223,3.38351691183107,72.8637801840458));
#201221=CARTESIAN_POINT('Ctrl Pts',(5.76807618099311,3.54347103712097,72.8725299643894));
#201222=CARTESIAN_POINT('Ctrl Pts',(5.66639083308953,3.69923018027792,72.881279744733));
#201223=CARTESIAN_POINT('Ctrl Pts',(5.5647091408213,3.85498372382152,72.8900292105179));
#201224=CARTESIAN_POINT('Ctrl Pts',(5.45660203371988,4.00654234702105,72.8987786763028));
#201225=CARTESIAN_POINT('Ctrl Pts',(5.34243669839129,4.15339127986781,72.9075281420877));
#201226=CARTESIAN_POINT('Ctrl Pts',(5.22827486050502,4.30023571401389,72.9162773398337));
#201227=CARTESIAN_POINT('Ctrl Pts',(5.10805534167019,4.44237052028576,72.9250265375797));
#201228=CARTESIAN_POINT('Ctrl Pts',(4.98218644339857,4.57931296628824,72.9337757353257));
#201229=CARTESIAN_POINT('Ctrl Pts',(4.85632073219489,4.71625194483461,72.9425247115374));
#201230=CARTESIAN_POINT('Ctrl Pts',(4.72480612170219,4.84799861524606,72.951273687749));
#201231=CARTESIAN_POINT('Ctrl Pts',(4.58808925235209,4.9741055489858,72.9600226639606));
#201232=CARTESIAN_POINT('Ctrl Pts',(4.45136349473944,5.10022068121298,72.9687722089623));
#201233=CARTESIAN_POINT('Ctrl Pts',(4.30943501209974,5.22069514871922,72.9775217539641));
#201234=CARTESIAN_POINT('Ctrl Pts',(4.16278587431674,5.33511975166341,72.9862712989658));
#201235=CARTESIAN_POINT('Ctrl Pts',(4.01614535740315,5.44953762807941,72.9950203296195));
#201236=CARTESIAN_POINT('Ctrl Pts',(3.86478496657765,5.55790617532895,73.0037693602732));
#201237=CARTESIAN_POINT('Ctrl Pts',(3.7092187474701,5.65985735539478,73.012518390927));
#201238=CARTESIAN_POINT('Ctrl Pts',(3.55365041605714,5.76180991977161,73.0212675403766));
#201239=CARTESIAN_POINT('Ctrl Pts',(3.39387638174335,5.85734478552922,73.0300166898262));
#201240=CARTESIAN_POINT('Ctrl Pts',(3.23043927904351,5.94613749121334,73.0387658392758));
#201241=CARTESIAN_POINT('Ctrl Pts',(3.18691767070303,5.96978206944215,73.0410956471919));
#201242=CARTESIAN_POINT('Ctrl Pts',(3.14313645919564,5.99294880633459,73.0434254551081));
#201243=CARTESIAN_POINT('Ctrl Pts',(3.09910619832135,6.0156321173694,73.0457552630242));
#201244=CARTESIAN_POINT('Ctrl Pts',(3.09910619832143,6.01563211736936,71.0458824924514));
#201245=CARTESIAN_POINT('Ctrl Pts',(2.94209088868808,6.09652255578414,71.0541813904892));
#201246=CARTESIAN_POINT('Ctrl Pts',(2.78184495475602,6.17129344529748,71.0624802885271));
#201247=CARTESIAN_POINT('Ctrl Pts',(2.61888209128078,6.23969114555912,71.0707791865649));
#201248=CARTESIAN_POINT('Ctrl Pts',(2.45595392010595,6.3080742849968,71.0790763178943));
#201249=CARTESIAN_POINT('Ctrl Pts',(2.2903102923292,6.37008680354989,71.0873734492237));
#201250=CARTESIAN_POINT('Ctrl Pts',(2.12248603660498,6.42552270437331,71.0956705805531));
#201251=CARTESIAN_POINT('Ctrl Pts',(1.95466960589001,6.48095602043069,71.1039673250187));
#201252=CARTESIAN_POINT('Ctrl Pts',(1.78467308026214,6.52981322083523,71.1122640694844));
#201253=CARTESIAN_POINT('Ctrl Pts',(1.61304782859842,6.57193774336412,71.12056081395));
#201254=CARTESIAN_POINT('Ctrl Pts',(1.44140204628814,6.61406730503309,71.1288585509125));
#201255=CARTESIAN_POINT('Ctrl Pts',(1.26812748775522,6.6494625016262,71.137156287875));
#201256=CARTESIAN_POINT('Ctrl Pts',(1.09378731642981,6.67801754313489,71.1454540248375));
#201257=CARTESIAN_POINT('Ctrl Pts',(0.919324345418592,6.70659269790891,
71.1537576064626));
#201258=CARTESIAN_POINT('Ctrl Pts',(0.743794605599573,6.72831801397396,
71.1620611880878));
#201259=CARTESIAN_POINT('Ctrl Pts',(0.567768919042361,6.74313928779241,
71.170364769713));
#201260=CARTESIAN_POINT('Ctrl Pts',(0.391679210801089,6.75796595220428,
71.1786713714047));
#201261=CARTESIAN_POINT('Ctrl Pts',(0.215093543606871,6.76588354772439,
71.1869779730963));
#201262=CARTESIAN_POINT('Ctrl Pts',(0.0385846176868022,6.76688999668814,
71.195284574788));
#201263=CARTESIAN_POINT('Ctrl Pts',(-0.138113486797284,6.76789752434277,
71.2036000793211));
#201264=CARTESIAN_POINT('Ctrl Pts',(-0.314734337484856,6.76197911106946,
71.2119155838542));
#201265=CARTESIAN_POINT('Ctrl Pts',(-0.490707366630687,6.74918478635267,
71.2202310883874));
#201266=CARTESIAN_POINT('Ctrl Pts',(-0.624276972018795,6.73947345211058,
71.2265428434585));
#201267=CARTESIAN_POINT('Ctrl Pts',(-0.75747339057754,6.72580174936138,
71.2328545985296));
#201268=CARTESIAN_POINT('Ctrl Pts',(-0.890050485105451,6.70821132150468,
71.2391663536007));
#201269=CARTESIAN_POINT('Ctrl Pts',(-1.06758137864267,6.68465639004218,
71.2476182775288));
#201270=CARTESIAN_POINT('Ctrl Pts',(-1.24432731076763,6.65402972143532,
71.256070201457));
#201271=CARTESIAN_POINT('Ctrl Pts',(-1.41970372915277,6.61639859148689,
71.2645221253851));
#201272=CARTESIAN_POINT('Ctrl Pts',(-1.59492497311713,6.5788007578553,71.2729665709851));
#201273=CARTESIAN_POINT('Ctrl Pts',(-1.76877879611551,6.53421088507903,
71.2814110165852));
#201274=CARTESIAN_POINT('Ctrl Pts',(-1.940688259322,6.48274772609036,71.2898554621852));
#201275=CARTESIAN_POINT('Ctrl Pts',(-2.1124689467072,6.43132311768781,71.2982935821276));
#201276=CARTESIAN_POINT('Ctrl Pts',(-2.28230786135585,6.37303558151365,
71.3067317020699));
#201277=CARTESIAN_POINT('Ctrl Pts',(-2.44964032459495,6.30805447662894,
71.3151698220122));
#201278=CARTESIAN_POINT('Ctrl Pts',(-2.61685222017403,6.2431201924245,71.3236018620562));
#201279=CARTESIAN_POINT('Ctrl Pts',(-2.78156095851281,6.17150207928877,
71.3320339021001));
#201280=CARTESIAN_POINT('Ctrl Pts',(-2.94321884257679,6.09341873209949,
71.340465942144));
#201281=CARTESIAN_POINT('Ctrl Pts',(-3.10480672631541,6.01536919618852,
71.3488943309863));
#201282=CARTESIAN_POINT('Ctrl Pts',(-3.26334609153346,5.93086015107284,
71.3573227198284));
#201283=CARTESIAN_POINT('Ctrl Pts',(-3.41831037467832,5.84015780457742,
71.3657511086706));
#201284=CARTESIAN_POINT('Ctrl Pts',(-3.57322600690949,5.7494839340117,71.3741768514268));
#201285=CARTESIAN_POINT('Ctrl Pts',(-3.72456850976261,5.65262080686151,
71.3826025941831));
#201286=CARTESIAN_POINT('Ctrl Pts',(-3.87183671278643,5.54988013109466,
71.3910283369393));
#201287=CARTESIAN_POINT('Ctrl Pts',(-3.91315779486081,5.52105275486156,
71.3933924644347));
#201288=CARTESIAN_POINT('Ctrl Pts',(-3.95415828337546,5.49176292349081,
71.3957565919301));
#201289=CARTESIAN_POINT('Ctrl Pts',(-3.9948275075642,5.46201814211638,71.3981207194255));
#201290=CARTESIAN_POINT('Ctrl Pts',(-4.14307559491541,5.35359200330005,
71.4067384736718));
#201291=CARTESIAN_POINT('Ctrl Pts',(-4.28685262780211,5.23916646674295,
71.4153562279182));
#201292=CARTESIAN_POINT('Ctrl Pts',(-4.42568726955956,5.11913871584453,
71.4239739821645));
#201293=CARTESIAN_POINT('Ctrl Pts',(-4.56460539846278,4.99903878717976,
71.4325969186312));
#201294=CARTESIAN_POINT('Ctrl Pts',(-4.69857497469454,4.87333012001369,
71.4412198550979));
#201295=CARTESIAN_POINT('Ctrl Pts',(-4.8271601468813,4.74244809316464,71.4498427915645));
#201296=CARTESIAN_POINT('Ctrl Pts',(-4.96041408538231,4.60681390408956,
71.4587788160383));
#201297=CARTESIAN_POINT('Ctrl Pts',(-5.08788504301749,4.46562390260936,
71.4677148405121));
#201298=CARTESIAN_POINT('Ctrl Pts',(-5.20913259310723,4.31940118852462,
71.4766508649859));
#201299=CARTESIAN_POINT('Ctrl Pts',(-5.32635123376672,4.17803727836012,
71.4852899561754));
#201300=CARTESIAN_POINT('Ctrl Pts',(-5.43775325768484,4.03197000708245,
71.4939290473648));
#201301=CARTESIAN_POINT('Ctrl Pts',(-5.54298386833789,3.88170308438782,
71.5025681385542));
#201302=CARTESIAN_POINT('Ctrl Pts',(-5.65363978417994,3.72368894906779,
71.5116526296702));
#201303=CARTESIAN_POINT('Ctrl Pts',(-5.75747092364945,3.56103102480029,
71.5207371207862));
#201304=CARTESIAN_POINT('Ctrl Pts',(-5.85411822018246,3.3943466034169,71.5298216119022));
#201305=CARTESIAN_POINT('Ctrl Pts',(-5.95076551671542,3.22766218203356,
71.5389061030182));
#201306=CARTESIAN_POINT('Ctrl Pts',(-6.0402288200107,3.05695162330793,71.5479905941342));
#201307=CARTESIAN_POINT('Ctrl Pts',(-6.12220636438889,2.88285938467976,
71.5570750852501));
#201308=CARTESIAN_POINT('Ctrl Pts',(-6.2044003493801,2.70830750028961,71.5661835616275));
#201309=CARTESIAN_POINT('Ctrl Pts',(-6.27914351223528,2.53020004223149,
71.5752920380048));
#201310=CARTESIAN_POINT('Ctrl Pts',(-6.346159090972,2.34916023124721,71.5844005143822));
#201311=CARTESIAN_POINT('Ctrl Pts',(-6.41530684317836,2.16236044192347,
71.5937987868345));
#201312=CARTESIAN_POINT('Ctrl Pts',(-6.47622707583673,1.97243884563274,
71.6031970592868));
#201313=CARTESIAN_POINT('Ctrl Pts',(-6.52866917929949,1.78010329679626,
71.6125953317391));
#201314=CARTESIAN_POINT('Ctrl Pts',(-6.57935300770177,1.5942163603615,71.6216784995909));
#201315=CARTESIAN_POINT('Ctrl Pts',(-6.62211787258374,1.40607494706007,
71.6307616674427));
#201316=CARTESIAN_POINT('Ctrl Pts',(-6.65678721428408,1.21633588442669,
71.6398448352944));
#201317=CARTESIAN_POINT('Ctrl Pts',(-6.69140850982577,1.02685976976572,
71.6489154153293));
#201318=CARTESIAN_POINT('Ctrl Pts',(-6.71795663055262,0.835790645655826,
71.6579859953642));
#201319=CARTESIAN_POINT('Ctrl Pts',(-6.73630570661486,0.643796883363165,
71.6670565753991));
#201320=CARTESIAN_POINT('Ctrl Pts',(-6.75461468962947,0.45222263075211,
71.6761073360602));
#201321=CARTESIAN_POINT('Ctrl Pts',(-6.76476036071652,0.259727996698518,
71.6851580967213));
#201322=CARTESIAN_POINT('Ctrl Pts',(-6.76666842810398,0.0669879399656761,
71.6942088573824));
#201323=CARTESIAN_POINT('Ctrl Pts',(-6.76687720347802,0.0458988643382756,
71.6951991661916));
#201324=CARTESIAN_POINT('Ctrl Pts',(-6.76698740789083,0.0248068593588396,
71.6961894750008));
#201325=CARTESIAN_POINT('Ctrl Pts',(-6.76699898145417,0.00371281540544154,
71.69717978381));
#201326=CARTESIAN_POINT('',(-6.76699597401548,0.00738157559828298,71.3028202162182));
#201327=CARTESIAN_POINT('Ctrl Pts',(3.0991061983213,6.01563211736942,70.6515955249703));
#201328=CARTESIAN_POINT('Ctrl Pts',(2.9439273477698,6.0955764570846,70.6598264419829));
#201329=CARTESIAN_POINT('Ctrl Pts',(2.78546950025012,6.16960710176201,70.6680573589954));
#201330=CARTESIAN_POINT('Ctrl Pts',(2.62422176771963,6.2374473235312,70.676288276008));
#201331=CARTESIAN_POINT('Ctrl Pts',(2.46312559961411,6.30522377904431,70.6845114563896));
#201332=CARTESIAN_POINT('Ctrl Pts',(2.29924509497393,6.36682126235569,70.6927346367712));
#201333=CARTESIAN_POINT('Ctrl Pts',(2.1330936584178,6.42200906604918,70.7009578171528));
#201334=CARTESIAN_POINT('Ctrl Pts',(1.96709140408611,6.47714731832446,70.7091736141957));
#201335=CARTESIAN_POINT('Ctrl Pts',(1.79882261816966,6.52588724955767,70.7173894112385));
#201336=CARTESIAN_POINT('Ctrl Pts',(1.62882023362179,6.56804641020024,70.7256052082814));
#201337=CARTESIAN_POINT('Ctrl Pts',(1.45890650422525,6.6101835851114,70.7338167208389));
#201338=CARTESIAN_POINT('Ctrl Pts',(1.28726132124077,6.64574673866785,70.7420282333963));
#201339=CARTESIAN_POINT('Ctrl Pts',(1.11443272197364,6.67460326223173,70.7502397459538));
#201340=CARTESIAN_POINT('Ctrl Pts',(0.941663085746926,6.70344994096453,
70.7584484570319));
#201341=CARTESIAN_POINT('Ctrl Pts',(0.767711188125084,6.72559448896618,
70.7666571681101));
#201342=CARTESIAN_POINT('Ctrl Pts',(0.593135298543037,6.74095538611718,
70.7748658791882));
#201343=CARTESIAN_POINT('Ctrl Pts',(0.507296674755447,6.74850830923126,
70.7789020863856));
#201344=CARTESIAN_POINT('Ctrl Pts',(0.421307322622372,6.75442195559597,
70.7829382935829));
#201345=CARTESIAN_POINT('Ctrl Pts',(0.335234169516869,6.75869122327602,
70.7869745007803));
#201346=CARTESIAN_POINT('Ctrl Pts',(0.146317993851626,6.76806155181527,
70.7958333005385));
#201347=CARTESIAN_POINT('Ctrl Pts',(-0.0428056339176083,6.76949762802394,
70.8046921002967));
#201348=CARTESIAN_POINT('Ctrl Pts',(-0.231484597436673,6.76303954455019,
70.8135509000549));
#201349=CARTESIAN_POINT('Ctrl Pts',(-0.420517864236536,6.75656933402147,
70.8224263349576));
#201350=CARTESIAN_POINT('Ctrl Pts',(-0.609104538966915,6.74217534833842,
70.8313017698603));
#201351=CARTESIAN_POINT('Ctrl Pts',(-0.796597943978947,6.7199494578195,
70.840177204763));
#201352=CARTESIAN_POINT('Ctrl Pts',(-0.984626218303849,6.69766016268755,
70.8490779589443));
#201353=CARTESIAN_POINT('Ctrl Pts',(-1.17155472263993,6.66749428329949,
70.8579787131257));
#201354=CARTESIAN_POINT('Ctrl Pts',(-1.35674423218656,6.62959531860192,
70.866879467307));
#201355=CARTESIAN_POINT('Ctrl Pts',(-1.54218543481759,6.59164484500764,
70.8757923186005));
#201356=CARTESIAN_POINT('Ctrl Pts',(-1.7258826687811,6.5459403498651,70.884705169894));
#201357=CARTESIAN_POINT('Ctrl Pts',(-1.90721085504091,6.49267554667674,
70.8936180211876));
#201358=CARTESIAN_POINT('Ctrl Pts',(-2.08894162203473,6.43929248617822,
70.9025506605918));
#201359=CARTESIAN_POINT('Ctrl Pts',(-2.26829257115235,6.37831561749839,
70.911483299996));
#201360=CARTESIAN_POINT('Ctrl Pts',(-2.44465490341659,6.3099882252823,70.9204159394002));
#201361=CARTESIAN_POINT('Ctrl Pts',(-2.61256045895414,6.24493721012967,
70.9289202484684));
#201362=CARTESIAN_POINT('Ctrl Pts',(-2.77775712323498,6.1732241478927,70.9374245575367));
#201363=CARTESIAN_POINT('Ctrl Pts',(-2.93973960969522,6.09509803261514,
70.945928866605));
#201364=CARTESIAN_POINT('Ctrl Pts',(-3.09635948615719,6.01955836909586,
70.9541516310826));
#201365=CARTESIAN_POINT('Ctrl Pts',(-3.2502742704664,5.9378775538885,70.9623743955603));
#201366=CARTESIAN_POINT('Ctrl Pts',(-3.40096971677294,5.85027298385242,
70.970597160038));
#201367=CARTESIAN_POINT('Ctrl Pts',(-3.55150566021883,5.76276113844649,
70.9788112211706));
#201368=CARTESIAN_POINT('Ctrl Pts',(-3.6988287435289,5.66933820252418,70.9870252823033));
#201369=CARTESIAN_POINT('Ctrl Pts',(-3.84244629057806,5.57026888974158,
70.995239343436));
#201370=CARTESIAN_POINT('Ctrl Pts',(-3.98594065984513,5.47128454664739,
71.0034463595393));
#201371=CARTESIAN_POINT('Ctrl Pts',(-4.12573552882683,5.36666367404273,
71.0116533756427));
#201372=CARTESIAN_POINT('Ctrl Pts',(-4.26136428589238,5.25671603027222,
71.019860391746));
#201373=CARTESIAN_POINT('Ctrl Pts',(-4.39690393884729,5.14684061887505,
71.0280620160808));
#201374=CARTESIAN_POINT('Ctrl Pts',(-4.52828265402812,5.03164563204686,
71.0362636404155));
#201375=CARTESIAN_POINT('Ctrl Pts',(-4.65506413360352,4.91148316825357,
71.0444652647503));
#201376=CARTESIAN_POINT('Ctrl Pts',(-4.78178776239174,4.79137553496978,
71.0526631466581));
#201377=CARTESIAN_POINT('Ctrl Pts',(-4.90391807495056,4.66630518674944,
71.0608610285659));
#201378=CARTESIAN_POINT('Ctrl Pts',(-5.02105304947212,4.53666345174367,
71.0690589104738));
#201379=CARTESIAN_POINT('Ctrl Pts',(-5.13817768554101,4.40703315905003,
71.0772560688281));
#201380=CARTESIAN_POINT('Ctrl Pts',(-5.25030761510098,4.27283254345412,
71.0854532271825));
#201381=CARTESIAN_POINT('Ctrl Pts',(-5.35707854916275,4.13448889442219,
71.0936503855369));
#201382=CARTESIAN_POINT('Ctrl Pts',(-5.46384829428941,3.99614678589959,
71.1018474526128));
#201383=CARTESIAN_POINT('Ctrl Pts',(-5.56525894268932,3.85366201923922,
71.1100445196887));
#201384=CARTESIAN_POINT('Ctrl Pts',(-5.66098737936329,3.70749388275822,
71.1182415867646));
#201385=CARTESIAN_POINT('Ctrl Pts',(-5.7567321558999,3.56130079687496,71.1264400529958));
#201386=CARTESIAN_POINT('Ctrl Pts',(-5.84679259179066,3.41142338877672,
71.134638519227));
#201387=CARTESIAN_POINT('Ctrl Pts',(-5.9308896591847,3.25834879203808,71.1428369854582));
#201388=CARTESIAN_POINT('Ctrl Pts',(-6.0150163722104,3.10522023392775,71.1510383417867));
#201389=CARTESIAN_POINT('Ctrl Pts',(-6.09317535648685,2.9488925563572,71.1592396981152));
#201390=CARTESIAN_POINT('Ctrl Pts',(-6.16513415501936,2.78987631457271,
71.1674410544438));
#201391=CARTESIAN_POINT('Ctrl Pts',(-6.23717489823892,2.63067898949561,
71.1756517502498));
#201392=CARTESIAN_POINT('Ctrl Pts',(-6.30300120180254,2.46878731080094,
71.1838624460558));
#201393=CARTESIAN_POINT('Ctrl Pts',(-6.36242889037979,2.30473157110771,
71.1920731418618));
#201394=CARTESIAN_POINT('Ctrl Pts',(-6.42189159675405,2.14057916148287,
71.2002886758246));
#201395=CARTESIAN_POINT('Ctrl Pts',(-6.4749480635796,1.97426049028573,71.2085042097875));
#201396=CARTESIAN_POINT('Ctrl Pts',(-6.52146443944355,1.80631961874782,
71.2167197437504));
#201397=CARTESIAN_POINT('Ctrl Pts',(-6.56805298204831,1.63811819928194,
71.2249480235108));
#201398=CARTESIAN_POINT('Ctrl Pts',(-6.60808107478164,1.46828989909528,
71.2331763032712));
#201399=CARTESIAN_POINT('Ctrl Pts',(-6.64146603762873,1.29738886654086,
71.2414045830316));
#201400=CARTESIAN_POINT('Ctrl Pts',(-6.67180552541044,1.14207793171024,
71.2488822547726));
#201401=CARTESIAN_POINT('Ctrl Pts',(-6.69665923944538,0.985881339277095,
71.2563599265136));
#201402=CARTESIAN_POINT('Ctrl Pts',(-6.71600243808305,0.829216649412278,
71.2638375982546));
#201403=CARTESIAN_POINT('Ctrl Pts',(-6.74961577604237,0.556975058692978,
71.276831804233));
#201404=CARTESIAN_POINT('Ctrl Pts',(-6.76669584267219,0.282524382040331,
71.2898260102114));
#201405=CARTESIAN_POINT('Ctrl Pts',(-6.76699597401482,0.00738157620036175,
71.3028202161898));
#201406=CARTESIAN_POINT('Ctrl Pts',(-6.76699597401548,0.00738157559829199,
71.3028202162182));
#201407=CARTESIAN_POINT('Ctrl Pts',(-6.76717949212259,-0.160857071485397,
71.3107656452367));
#201408=CARTESIAN_POINT('Ctrl Pts',(-6.7610850101191,-0.329400696816224,
71.3187110742551));
#201409=CARTESIAN_POINT('Ctrl Pts',(-6.74867107799455,-0.497722494006376,
71.3266565032735));
#201410=CARTESIAN_POINT('Ctrl Pts',(-6.7362701632057,-0.665867787787545,
71.3345936006597));
#201411=CARTESIAN_POINT('Ctrl Pts',(-6.71756300615423,-0.833791337887429,
71.3425306980459));
#201412=CARTESIAN_POINT('Ctrl Pts',(-6.69256010162055,-1.00096367876002,
71.3504677954321));
#201413=CARTESIAN_POINT('Ctrl Pts',(-6.66757768956765,-1.16799900451186,
71.3583983875414));
#201414=CARTESIAN_POINT('Ctrl Pts',(-6.63630985110431,-1.33428396923348,
71.3663289796508));
#201415=CARTESIAN_POINT('Ctrl Pts',(-6.59881906361541,-1.49929182138296,
71.3742595717602));
#201416=CARTESIAN_POINT('Ctrl Pts',(-6.56135044359369,-1.66420210806662,
71.3821854746871));
#201417=CARTESIAN_POINT('Ctrl Pts',(-6.51766628029368,-1.82783641220349,
71.3901113776141));
#201418=CARTESIAN_POINT('Ctrl Pts',(-6.46788050486346,-1.98967604770404,
71.3980372805411));
#201419=CARTESIAN_POINT('Ctrl Pts',(-6.41810573509665,-2.15147990687013,
71.4059614313648));
#201420=CARTESIAN_POINT('Ctrl Pts',(-6.36223214141232,-2.31148951843576,
71.4138855821885));
#201421=CARTESIAN_POINT('Ctrl Pts',(-6.30042409209219,-2.46919931552401,
71.4218097330122));
#201422=CARTESIAN_POINT('Ctrl Pts',(-6.2386211534355,-2.62689607221217,
71.4297332286192));
#201423=CARTESIAN_POINT('Ctrl Pts',(-6.17088487408092,-2.78229303526583,
71.4376567242262));
#201424=CARTESIAN_POINT('Ctrl Pts',(-6.09742840847457,-2.93490303136702,
71.4455802198332));
#201425=CARTESIAN_POINT('Ctrl Pts',(-6.02396286604566,-3.08753188508468,
71.4535046945257));
#201426=CARTESIAN_POINT('Ctrl Pts',(-5.94477589758388,-3.23737274119463,
71.4614291692182));
#201427=CARTESIAN_POINT('Ctrl Pts',(-5.86012727107888,-3.38396178565267,
71.4693536439107));
#201428=CARTESIAN_POINT('Ctrl Pts',(-5.77545071334609,-3.53059919961369,
71.477280733416));
#201429=CARTESIAN_POINT('Ctrl Pts',(-5.68530910465292,-3.6739823359453,
71.4852078229213));
#201430=CARTESIAN_POINT('Ctrl Pts',(-5.59000613642062,-3.81367544434235,
71.4931349124265));
#201431=CARTESIAN_POINT('Ctrl Pts',(-5.49459454317271,-3.95352777302772,
71.5010710371197));
#201432=CARTESIAN_POINT('Ctrl Pts',(-5.39401006165389,-4.08968136020956,
71.5090071618128));
#201433=CARTESIAN_POINT('Ctrl Pts',(-5.28859776599477,-4.22173218827475,
71.5169432865059));
#201434=CARTESIAN_POINT('Ctrl Pts',(-5.18312107389773,-4.35386368627413,
71.5248842593827));
#201435=CARTESIAN_POINT('Ctrl Pts',(-5.07281094777323,-4.4818871483275,
71.5328252322594));
#201436=CARTESIAN_POINT('Ctrl Pts',(-4.95804951925956,-4.60543526331335,
71.5407662051361));
#201437=CARTESIAN_POINT('Ctrl Pts',(-4.84310963577557,-4.72917549663965,
71.5487195262913));
#201438=CARTESIAN_POINT('Ctrl Pts',(-4.72370490072325,-4.84842621974421,
71.5566728474464));
#201439=CARTESIAN_POINT('Ctrl Pts',(-4.60025136267833,-4.96285969982793,
71.5646261686016));
#201440=CARTESIAN_POINT('Ctrl Pts',(-4.51167015056788,-5.0449687793437,
71.5703328890358));
#201441=CARTESIAN_POINT('Ctrl Pts',(-4.42100511994707,-5.12459858535971,
71.57603960947));
#201442=CARTESIAN_POINT('Ctrl Pts',(-4.32841875408156,-5.20164205701575,
71.5817463299042));
#201443=CARTESIAN_POINT('Ctrl Pts',(-4.193232474238,-5.31413400139708,71.59007876955));
#201444=CARTESIAN_POINT('Ctrl Pts',(-4.05348439408398,-5.42149710211226,
71.5984112091959));
#201445=CARTESIAN_POINT('Ctrl Pts',(-3.90959473330228,-5.523346632372,71.6067436488417));
#201446=CARTESIAN_POINT('Ctrl Pts',(-3.76587510147774,-5.62507581090303,
71.6150662423595));
#201447=CARTESIAN_POINT('Ctrl Pts',(-3.61802391975303,-5.72130419835902,
71.6233888358773));
#201448=CARTESIAN_POINT('Ctrl Pts',(-3.46649544371141,-5.81168635928747,
71.6317114293951));
#201449=CARTESIAN_POINT('Ctrl Pts',(-3.31511819536944,-5.90197831745903,
71.6400257168393));
#201450=CARTESIAN_POINT('Ctrl Pts',(-3.16007126151928,-5.98643549636477,
71.6483400042835));
#201451=CARTESIAN_POINT('Ctrl Pts',(-3.00183910827763,-6.0647548151607,
71.6566542917277));
#201452=CARTESIAN_POINT('Ctrl Pts',(-2.84373583348108,-6.14301034368507,
71.6649618072712));
#201453=CARTESIAN_POINT('Ctrl Pts',(-2.68245281923756,-6.21513781974245,
71.6732693228146));
#201454=CARTESIAN_POINT('Ctrl Pts',(-2.5185006408941,-6.28087919974712,
71.6815768383581));
#201455=CARTESIAN_POINT('Ctrl Pts',(-2.35465192683352,-6.34657909274743,
71.6898791113293));
#201456=CARTESIAN_POINT('Ctrl Pts',(-2.18813772759051,-6.40590079190939,
71.6981813843006));
#201457=CARTESIAN_POINT('Ctrl Pts',(-2.0194903885204,-6.45863356838532,
71.7064836572718));
#201458=CARTESIAN_POINT('Ctrl Pts',(-1.85091183091813,-6.5113448382203,
71.7147825442274));
#201459=CARTESIAN_POINT('Ctrl Pts',(-1.68020219858506,-6.55747243617869,
71.723081431183));
#201460=CARTESIAN_POINT('Ctrl Pts',(-1.5079111359526,-6.59685478133862,
71.7313803181387));
#201461=CARTESIAN_POINT('Ctrl Pts',(-1.33565662207888,-6.6362287721718,
71.7396774446198));
#201462=CARTESIAN_POINT('Ctrl Pts',(-1.16182168525784,-6.6688602833746,
71.7479745711009));
#201463=CARTESIAN_POINT('Ctrl Pts',(-0.986968600323926,-6.69463830105665,
71.7562716975821));
#201464=CARTESIAN_POINT('Ctrl Pts',(-0.812123536843244,-6.72041513616211,
71.7645684434293));
#201465=CARTESIAN_POINT('Ctrl Pts',(-0.636260762562076,-6.73933905368834,
71.7728651892766));
#201466=CARTESIAN_POINT('Ctrl Pts',(-0.459950349535424,-6.7513505816216,
71.7811619351239));
#201467=CARTESIAN_POINT('Ctrl Pts',(-0.283618713020177,-6.76336355545088,
71.7894596796977));
#201468=CARTESIAN_POINT('Ctrl Pts',(-0.106839677556948,-6.76846245861269,
71.7977574242715));
#201469=CARTESIAN_POINT('Ctrl Pts',(0.0698137925328148,-6.76663986291366,
71.8060551688453));
#201470=CARTESIAN_POINT('Ctrl Pts',(0.246591760216356,-6.76481598272937,
71.8143587613044));
#201471=CARTESIAN_POINT('Ctrl Pts',(0.423243637336409,-6.75606086014889,
71.8226623537635));
#201472=CARTESIAN_POINT('Ctrl Pts',(0.599197782242467,-6.74041920193067,
71.8309659462226));
#201473=CARTESIAN_POINT('Ctrl Pts',(0.775216041911384,-6.72477184415245,
71.8392725643727));
#201474=CARTESIAN_POINT('Ctrl Pts',(0.950535716746082,-6.70223298749084,
71.8475791825227));
#201475=CARTESIAN_POINT('Ctrl Pts',(1.12459227441324,-6.67289901139902,
71.8558858006728));
#201476=CARTESIAN_POINT('Ctrl Pts',(1.29883522503714,-6.64353362226188,
71.8642013141793));
#201477=CARTESIAN_POINT('Ctrl Pts',(1.47181201382979,-6.60735863986934,
71.8725168276857));
#201478=CARTESIAN_POINT('Ctrl Pts',(1.64296916808702,-6.56452140774295,
71.8808323411922));
#201479=CARTESIAN_POINT('Ctrl Pts',(1.77211105250717,-6.53219976215265,
71.8871065813127));
#201480=CARTESIAN_POINT('Ctrl Pts',(1.900217244485,-6.49608632537552,71.8933808214331));
#201481=CARTESIAN_POINT('Ctrl Pts',(2.02705658233125,-6.45626289830484,
71.8996550615536));
#201482=CARTESIAN_POINT('Ctrl Pts',(2.19791973292639,-6.40261742575404,
71.9081069854818));
#201483=CARTESIAN_POINT('Ctrl Pts',(2.36679702980146,-6.34213952935364,
71.9165589094099));
#201484=CARTESIAN_POINT('Ctrl Pts',(2.53312411224464,-6.27499571569294,
71.9250108333381));
#201485=CARTESIAN_POINT('Ctrl Pts',(2.69930402719014,-6.20791131140141,
71.9334552789382));
#201486=CARTESIAN_POINT('Ctrl Pts',(2.86293791938998,-6.13417286926218,
71.9418997245382));
#201487=CARTESIAN_POINT('Ctrl Pts',(3.02347775513098,-6.05399630527044,
71.9503441701383));
#201488=CARTESIAN_POINT('Ctrl Pts',(3.18389733193687,-5.97387980081571,
71.9587822900807));
#201489=CARTESIAN_POINT('Ctrl Pts',(3.34122717708123,-5.88733493597742,
71.9672204100231));
#201490=CARTESIAN_POINT('Ctrl Pts',(3.49494001234784,-5.79462538134175,
71.9756585299656));
#201491=CARTESIAN_POINT('Ctrl Pts',(3.64854209327107,-5.70198262650086,
71.9840905700095));
#201492=CARTESIAN_POINT('Ctrl Pts',(3.79853207968093,-5.60318421259049,
71.9925226100535));
#201493=CARTESIAN_POINT('Ctrl Pts',(3.94440786547106,-5.49853940522481,
72.0009546500974));
#201494=CARTESIAN_POINT('Ctrl Pts',(4.09022048482257,-5.39393991065567,
72.0093830389395));
#201495=CARTESIAN_POINT('Ctrl Pts',(4.23192218629874,-5.28349926221459,
72.0178114277816));
#201496=CARTESIAN_POINT('Ctrl Pts',(4.36903984800602,-5.16757000983398,
72.0262398166237));
#201497=CARTESIAN_POINT('Ctrl Pts',(4.50611446173429,-5.05167715334841,
72.03466555938));
#201498=CARTESIAN_POINT('Ctrl Pts',(4.63860765299018,-4.93029934301154,
72.0430913021362));
#201499=CARTESIAN_POINT('Ctrl Pts',(4.76607911837203,-4.80382960120549,
72.0515170448924));
#201500=CARTESIAN_POINT('Ctrl Pts',(4.80184555521866,-4.76834423183466,
72.0538811723878));
#201501=CARTESIAN_POINT('Ctrl Pts',(4.83721685378571,-4.73245822456643,
72.0562452998831));
#201502=CARTESIAN_POINT('Ctrl Pts',(4.87218378815524,-4.69618080299697,
72.0586094273784));
#201503=CARTESIAN_POINT('Ctrl Pts',(4.99964580014173,-4.56394178272546,
72.0672271816248));
#201504=CARTESIAN_POINT('Ctrl Pts',(5.12167431490016,-4.42655881366438,
72.0758449358711));
#201505=CARTESIAN_POINT('Ctrl Pts',(5.23787307658841,-4.28450401254921,
72.0844626901175));
#201506=CARTESIAN_POINT('Ctrl Pts',(5.35414171350818,-4.14236378787211,
72.0930856265841));
#201507=CARTESIAN_POINT('Ctrl Pts',(5.46457340843163,-3.99554636005134,
72.1017085630506));
#201508=CARTESIAN_POINT('Ctrl Pts',(5.56881341428031,-3.84455539132053,
72.1103314995172));
#201509=CARTESIAN_POINT('Ctrl Pts',(5.67683824399188,-3.68808212990486,
72.119267523991));
#201510=CARTESIAN_POINT('Ctrl Pts',(5.7782131351049,-3.52712687832724,72.1282035484649));
#201511=CARTESIAN_POINT('Ctrl Pts',(5.87259387358752,-3.36228050523783,
72.1371395729387));
#201512=CARTESIAN_POINT('Ctrl Pts',(5.96383845429135,-3.20291177773142,
72.1457786641281));
#201513=CARTESIAN_POINT('Ctrl Pts',(6.04854611952049,-3.03990665473596,
72.1544177553175));
#201514=CARTESIAN_POINT('Ctrl Pts',(6.1264536926981,-2.87382221983647,72.1630568465069));
#201515=CARTESIAN_POINT('Ctrl Pts',(6.20837789524314,-2.69917507926562,
72.1721413376229));
#201516=CARTESIAN_POINT('Ctrl Pts',(6.28278216656654,-2.5211230917456,72.181225828739));
#201517=CARTESIAN_POINT('Ctrl Pts',(6.34941859802417,-2.34033597311686,
72.1903103198551));
#201518=CARTESIAN_POINT('Ctrl Pts',(6.41605502948179,-2.15954885448812,
72.1993948109711));
#201519=CARTESIAN_POINT('Ctrl Pts',(6.47492353468485,-1.97602698496696,
72.2084793020871));
#201520=CARTESIAN_POINT('Ctrl Pts',(6.52583731511666,-1.79045701892869,
72.2175637932032));
#201521=CARTESIAN_POINT('Ctrl Pts',(6.57649029466412,-1.6058376169782,72.2266017498978));
#201522=CARTESIAN_POINT('Ctrl Pts',(6.61931794910389,-1.41901897994379,
72.2356397065923));
#201523=CARTESIAN_POINT('Ctrl Pts',(6.6541555407529,-1.23065146953451,72.2446776632869));
#201524=CARTESIAN_POINT('Ctrl Pts',(6.68896102508442,-1.04245756399213,
72.253707290343));
#201525=CARTESIAN_POINT('Ctrl Pts',(6.71579110493589,-0.852717869978947,
72.2627369173991));
#201526=CARTESIAN_POINT('Ctrl Pts',(6.73453201061368,-0.662093345397558,
72.2717665444551));
#201527=CARTESIAN_POINT('Ctrl Pts',(6.75323990762897,-0.471804570896919,
72.280780267482));
#201528=CARTESIAN_POINT('Ctrl Pts',(6.76388705756375,-0.280634315568752,
72.2897939905088));
#201529=CARTESIAN_POINT('Ctrl Pts',(6.76641142943289,-0.0892489083408666,
72.2988077135356));
#201530=CARTESIAN_POINT('Ctrl Pts',(6.76893264769673,0.101897408109752,
72.3078101760485));
#201531=CARTESIAN_POINT('Ctrl Pts',(6.76335133547306,0.293258101645628,
72.3168126385614));
#201532=CARTESIAN_POINT('Ctrl Pts',(6.74965733845046,0.484164035737715,
72.3258151010743));
#201533=CARTESIAN_POINT('Ctrl Pts',(6.73599407242338,0.674641553685474,
72.334797360966));
#201534=CARTESIAN_POINT('Ctrl Pts',(6.7142544792872,0.864666111181729,72.3437796208576));
#201535=CARTESIAN_POINT('Ctrl Pts',(6.68448026343205,1.05357135865941,72.3527618807493));
#201536=CARTESIAN_POINT('Ctrl Pts',(6.65823131769849,1.22011020602814,72.3606806401755));
#201537=CARTESIAN_POINT('Ctrl Pts',(6.62573845447481,1.38577897350931,72.3685993996017));
#201538=CARTESIAN_POINT('Ctrl Pts',(6.58706384370005,1.55012222712261,72.3765181590279));
#201539=CARTESIAN_POINT('Ctrl Pts',(6.54734312603064,1.71891079013266,72.3846511124348));
#201540=CARTESIAN_POINT('Ctrl Pts',(6.50111849405804,1.88622290372998,72.3927840658416));
#201541=CARTESIAN_POINT('Ctrl Pts',(6.44853036231096,2.05152264583009,72.4009170192485));
#201542=CARTESIAN_POINT('Ctrl Pts',(6.39594542355418,2.21681235143613,72.4090494788474));
#201543=CARTESIAN_POINT('Ctrl Pts',(6.33699786538176,2.38008958109444,72.4171819384462));
#201544=CARTESIAN_POINT('Ctrl Pts',(6.27187786437763,2.54083392891583,72.4253143980451));
#201545=CARTESIAN_POINT('Ctrl Pts',(6.20674947342521,2.70159898676096,72.433447905416));
#201546=CARTESIAN_POINT('Ctrl Pts',(6.13544719416951,2.85983017505991,72.4415814127868));
#201547=CARTESIAN_POINT('Ctrl Pts',(6.05820918349794,3.01502744415058,72.4497149201577));
#201548=CARTESIAN_POINT('Ctrl Pts',(5.98091415083708,3.1703392896906,72.4578544321986));
#201549=CARTESIAN_POINT('Ctrl Pts',(5.89767479720669,3.32261241532188,72.4659939442396));
#201550=CARTESIAN_POINT('Ctrl Pts',(5.80877536252484,3.47137116824525,72.4741334562806));
#201551=CARTESIAN_POINT('Ctrl Pts',(5.71983918507499,3.62019140421818,72.4822763324397));
#201552=CARTESIAN_POINT('Ctrl Pts',(5.62523846237361,3.76549406637753,72.4904192085988));
#201553=CARTESIAN_POINT('Ctrl Pts',(5.52530040407406,3.90683304541402,72.4985620847579));
#201554=CARTESIAN_POINT('Ctrl Pts',(5.42525311104038,4.04832651140034,72.5067138612791));
#201555=CARTESIAN_POINT('Ctrl Pts',(5.3198570518838,4.1858473514988,72.5148656378004));
#201556=CARTESIAN_POINT('Ctrl Pts',(5.20947977010969,4.31898246405538,72.5230174143216));
#201557=CARTESIAN_POINT('Ctrl Pts',(5.1532645700232,4.38678823776724,72.527169117832));
#201558=CARTESIAN_POINT('Ctrl Pts',(5.09575791151799,4.45345698846682,72.5313208213423));
#201559=CARTESIAN_POINT('Ctrl Pts',(5.03701193096813,4.51893790699593,72.5354725248527));
#201560=CARTESIAN_POINT('Ctrl Pts',(4.9177793359016,4.65183993315137,72.5438989461814));
#201561=CARTESIAN_POINT('Ctrl Pts',(4.79319172920386,4.78012248674441,72.5523253675102));
#201562=CARTESIAN_POINT('Ctrl Pts',(4.66363485474412,4.90334568856978,72.5607517888389));
#201563=CARTESIAN_POINT('Ctrl Pts',(4.53420009938071,5.0264527413593,72.5691702675019));
#201564=CARTESIAN_POINT('Ctrl Pts',(4.39980566021988,5.14450972332865,72.5775887461648));
#201565=CARTESIAN_POINT('Ctrl Pts',(4.26087500532992,5.25711262852098,72.5860072248278));
#201566=CARTESIAN_POINT('Ctrl Pts',(4.12202222607367,5.36965241573113,72.5944209846303));
#201567=CARTESIAN_POINT('Ctrl Pts',(3.9786385581983,5.4767440083115,72.6028347444329));
#201568=CARTESIAN_POINT('Ctrl Pts',(3.8311820745088,5.57802231189177,72.6112485042355));
#201569=CARTESIAN_POINT('Ctrl Pts',(3.68379394012754,5.6792536707612,72.6196583640762));
#201570=CARTESIAN_POINT('Ctrl Pts',(3.53233702992624,5.77467692376878,72.6280682239169));
#201571=CARTESIAN_POINT('Ctrl Pts',(3.37730026173126,5.86396895814686,72.6364780837576));
#201572=CARTESIAN_POINT('Ctrl Pts',(3.28578073723264,5.91667880641666,72.6414424956367));
#201573=CARTESIAN_POINT('Ctrl Pts',(3.19301433768587,5.96725294605387,72.6464069075158));
#201574=CARTESIAN_POINT('Ctrl Pts',(3.09910619832134,6.0156321173694,72.6513713193949));
#201575=CARTESIAN_POINT('Origin',(0.,0.,4.30282021618968));
#201576=CARTESIAN_POINT('',(3.09910619832135,6.0156321173694,75.0457552630242));
#201577=CARTESIAN_POINT('',(3.09910619832131,6.01563211736941,74.651395695404));
#201578=CARTESIAN_POINT('',(3.09910619832133,6.0156321173694,4.30282021618968));
#201579=CARTESIAN_POINT('',(-6.767,-9.23806438532518E-10,73.6971797838536));
#201580=CARTESIAN_POINT('Ctrl Pts',(-6.767,-9.23711102397149E-10,73.6971797838536));
#201581=CARTESIAN_POINT('Ctrl Pts',(-6.76699999997461,-0.18600725045061,
73.7059292956648));
#201582=CARTESIAN_POINT('Ctrl Pts',(-6.75932637289442,-0.372014356672636,
73.7146788074759));
#201583=CARTESIAN_POINT('Ctrl Pts',(-6.74400518256571,-0.557389538408147,
73.7234283192871));
#201584=CARTESIAN_POINT('Ctrl Pts',(-6.72868405694944,-0.742763937170584,
73.7321777941428));
#201585=CARTESIAN_POINT('Ctrl Pts',(-6.70571545633057,-0.927506131158146,
73.7409272689985));
#201586=CARTESIAN_POINT('Ctrl Pts',(-6.67517739389623,-1.11098864081354,
73.7496767438542));
#201587=CARTESIAN_POINT('Ctrl Pts',(-6.64463945790987,-1.29447039072881,
73.7584261824812));
#201588=CARTESIAN_POINT('Ctrl Pts',(-6.60653216988143,-1.47669218404109,
73.7671756211082));
#201589=CARTESIAN_POINT('Ctrl Pts',(-6.56098496069993,-1.65703510689102,
73.7759250597352));
#201590=CARTESIAN_POINT('Ctrl Pts',(-6.51543793633142,-1.837377297979,73.7846744628604));
#201591=CARTESIAN_POINT('Ctrl Pts',(-6.4624511213982,-2.01584035599409,
73.7934238659855));
#201592=CARTESIAN_POINT('Ctrl Pts',(-6.40220448344241,-2.19181813848456,
73.8021732691107));
#201593=CARTESIAN_POINT('Ctrl Pts',(-6.34195808494076,-2.36779522154001,
73.8109226374608));
#201594=CARTESIAN_POINT('Ctrl Pts',(-6.27445201398293,-2.54128677770116,
73.8196720058109));
#201595=CARTESIAN_POINT('Ctrl Pts',(-6.19991555034748,-2.71170355469758,
73.8284213741611));
#201596=CARTESIAN_POINT('Ctrl Pts',(-6.12537937677203,-2.88211966851404,
73.8371707084628));
#201597=CARTESIAN_POINT('Ctrl Pts',(-6.04381298010737,-3.04946076454597,
73.8459200427646));
#201598=CARTESIAN_POINT('Ctrl Pts',(-5.95549339291804,-3.2131584845615,
73.8546693770664));
#201599=CARTESIAN_POINT('Ctrl Pts',(-5.86717414209145,-3.37685558113873,
73.8634186780466));
#201600=CARTESIAN_POINT('Ctrl Pts',(-5.77210188828149,-3.53690907725823,
73.8721679790267));
#201601=CARTESIAN_POINT('Ctrl Pts',(-5.67059953296419,-3.69277537046952,
73.8809172800069));
#201602=CARTESIAN_POINT('Ctrl Pts',(-5.56909755578688,-3.84864108301174,
73.8896665483922));
#201603=CARTESIAN_POINT('Ctrl Pts',(-5.46116568142095,-4.00031938372266,
73.8984158167775));
#201604=CARTESIAN_POINT('Ctrl Pts',(-5.34717048476855,-4.1472951193302,
73.9071650851627));
#201605=CARTESIAN_POINT('Ctrl Pts',(-5.23317570333084,-4.29427031959514,
73.9159143216798));
#201606=CARTESIAN_POINT('Ctrl Pts',(-5.11311781942821,-4.43654276259495,
73.9246635581968));
#201607=CARTESIAN_POINT('Ctrl Pts',(-4.98740458922192,-4.57362924420073,
73.9334127947139));
#201608=CARTESIAN_POINT('Ctrl Pts',(-4.86169180647313,-4.71071523786761,
73.9421620000893));
#201609=CARTESIAN_POINT('Ctrl Pts',(-4.73032391137944,-4.84261509587929,
73.9509112054647));
#201610=CARTESIAN_POINT('Ctrl Pts',(-4.59374706945652,-4.96888084601147,
73.9596604108402));
#201611=CARTESIAN_POINT('Ctrl Pts',(-4.45717070231763,-5.09514615720421,
73.9684095858006));
#201612=CARTESIAN_POINT('Ctrl Pts',(-4.31538563499701,-5.21577720518553,
73.977158760761));
#201613=CARTESIAN_POINT('Ctrl Pts',(-4.16887340956593,-5.33036429289914,
73.9859079357215));
#201614=CARTESIAN_POINT('Ctrl Pts',(-4.02236168129221,-5.4449509917864,
73.9946570809935));
#201615=CARTESIAN_POINT('Ctrl Pts',(-3.87112305272195,-5.55349359491558,
74.0034062262656));
#201616=CARTESIAN_POINT('Ctrl Pts',(-3.71567116940392,-5.65562346349724,
74.0121553715376));
#201617=CARTESIAN_POINT('Ctrl Pts',(-3.56021980067038,-5.75775299400358,
74.0209044878477));
#201618=CARTESIAN_POINT('Ctrl Pts',(-3.40055544458243,-5.85346967510411,
74.0296536041579));
#201619=CARTESIAN_POINT('Ctrl Pts',(-3.23722035905514,-5.94244843031212,
74.0384027204681));
#201620=CARTESIAN_POINT('Ctrl Pts',(-3.07388580064597,-6.03142689836618,
74.047151808543));
#201621=CARTESIAN_POINT('Ctrl Pts',(-2.90688078812843,-6.11366734696596,
74.0559008966178));
#201622=CARTESIAN_POINT('Ctrl Pts',(-2.73677250636577,-6.1888904698985,
74.0646499846927));
#201623=CARTESIAN_POINT('Ctrl Pts',(-2.56666475945633,-6.26411335631504,
74.0733990452587));
#201624=CARTESIAN_POINT('Ctrl Pts',(-2.39345402488356,-6.33231884533368,
74.0821481058248));
#201625=CARTESIAN_POINT('Ctrl Pts',(-2.2177285597792,-6.39327529793139,
74.0908971663908));
#201626=CARTESIAN_POINT('Ctrl Pts',(-2.04200363259986,-6.4542315639312,
74.0996462001745));
#201627=CARTESIAN_POINT('Ctrl Pts',(-1.86376426099994,-6.50793874401228,
74.1083952339582));
#201628=CARTESIAN_POINT('Ctrl Pts',(-1.68361577663215,-6.55421443932645,
74.1171442677419));
#201629=CARTESIAN_POINT('Ctrl Pts',(-1.50346782877241,-6.60048999682495,
74.1258932754697));
#201630=CARTESIAN_POINT('Ctrl Pts',(-1.32141105703911,-6.63933404255839,
74.1346422831975));
#201631=CARTESIAN_POINT('Ctrl Pts',(-1.13806375395533,-6.6706146562317,
74.1433912909254));
#201632=CARTESIAN_POINT('Ctrl Pts',(-0.954716981684124,-6.70189517934386,
74.1521402733238));
#201633=CARTESIAN_POINT('Ctrl Pts',(-0.770079967980283,-6.72561226602783,
74.1608892557222));
#201634=CARTESIAN_POINT('Ctrl Pts',(-0.584779764634478,-6.74168536991115,
74.1696382381205));
#201635=CARTESIAN_POINT('Ctrl Pts',(-0.391489829734905,-6.75845151019133,
74.17876445713));
#201636=CARTESIAN_POINT('Ctrl Pts',(-0.197478577330526,-6.76689983034247,
74.1878906761394));
#201637=CARTESIAN_POINT('Ctrl Pts',(-0.00346287555322934,-6.76699911397164,
74.1970168951488));
#201638=CARTESIAN_POINT('Ctrl Pts',(0.184489835543577,-6.7670952949874,
74.2058579198142));
#201639=CARTESIAN_POINT('Ctrl Pts',(0.372446405128696,-6.75935639733297,
74.2146989444795));
#201640=CARTESIAN_POINT('Ctrl Pts',(0.55975502035636,-6.74380925865982,
74.2235399691449));
#201641=CARTESIAN_POINT('Ctrl Pts',(0.745134706387836,-6.72842222650215,
74.2322899477546));
#201642=CARTESIAN_POINT('Ctrl Pts',(0.929879432091684,-6.70538706045554,
74.2410399263644));
#201643=CARTESIAN_POINT('Ctrl Pts',(1.11336163712745,-6.67478200879796,
74.2497899049741));
#201644=CARTESIAN_POINT('Ctrl Pts',(1.29684196386254,-6.64417727044318,
74.2585397940106));
#201645=CARTESIAN_POINT('Ctrl Pts',(1.47905951302564,-6.60600284871547,
74.2672896830472));
#201646=CARTESIAN_POINT('Ctrl Pts',(1.65939532151561,-6.56038841585863,
74.2760395720837));
#201647=CARTESIAN_POINT('Ctrl Pts',(1.83972934384697,-6.51477443479565,
74.2847893744559));
#201648=CARTESIAN_POINT('Ctrl Pts',(2.01818138489482,-6.4617206603615,74.293539176828));
#201649=CARTESIAN_POINT('Ctrl Pts',(2.19414528436645,-6.40140730395219,
74.3022889792002));
#201650=CARTESIAN_POINT('Ctrl Pts',(2.37010749945662,-6.34109452488119,
74.3110386978165));
#201651=CARTESIAN_POINT('Ctrl Pts',(2.54358134947245,-6.2735223958375,74.3197884164328));
#201652=CARTESIAN_POINT('Ctrl Pts',(2.71397759515373,-6.19892043931874,
74.3285381350491));
#201653=CARTESIAN_POINT('Ctrl Pts',(2.88437226636986,-6.12431917212373,
74.3372877728178));
#201654=CARTESIAN_POINT('Ctrl Pts',(3.05168912758772,-6.042688322395,74.3460374105866));
#201655=CARTESIAN_POINT('Ctrl Pts',(3.21535986350538,-5.95430516081924,
74.3547870483553));
#201656=CARTESIAN_POINT('Ctrl Pts',(3.37902914148398,-5.86592278653917,
74.3635366081844));
#201657=CARTESIAN_POINT('Ctrl Pts',(3.53905210695913,-5.77078835696351,
74.3722861680134));
#201658=CARTESIAN_POINT('Ctrl Pts',(3.6948852290474,-5.66922500384024,74.3810357278425));
#201659=CARTESIAN_POINT('Ctrl Pts',(3.85071701478684,-5.56766252167474,
74.3897852126396));
#201660=CARTESIAN_POINT('Ctrl Pts',(4.00235878892765,-5.4596713827779,74.3985346974367));
#201661=CARTESIAN_POINT('Ctrl Pts',(4.14929549680226,-5.34561838146126,
74.4072841822339));
#201662=CARTESIAN_POINT('Ctrl Pts',(4.29623099343515,-5.23156632031645,
74.4160335949065));
#201663=CARTESIAN_POINT('Ctrl Pts',(4.43846127501901,-5.11145267247764,
74.424783007579));
#201664=CARTESIAN_POINT('Ctrl Pts',(4.5755032611869,-4.98568539990923,74.4335324202516));
#201665=CARTESIAN_POINT('Ctrl Pts',(4.71254416320399,-4.8599191222964,74.4422817637069));
#201666=CARTESIAN_POINT('Ctrl Pts',(4.84439664079679,-4.72849950323008,
74.4510311071621));
#201667=CARTESIAN_POINT('Ctrl Pts',(4.97061286853895,-4.59187289797039,
74.4597804506173));
#201668=CARTESIAN_POINT('Ctrl Pts',(5.09682813970068,-4.45524732819037,
74.4685297277622));
#201669=CARTESIAN_POINT('Ctrl Pts',(5.2174070520339,-4.31341506168594,74.477279004907));
#201670=CARTESIAN_POINT('Ctrl Pts',(5.33194007599354,-4.16685781207063,
74.4860282820518));
#201671=CARTESIAN_POINT('Ctrl Pts',(5.44647226996243,-4.02030162451723,
74.4947774957929));
#201672=CARTESIAN_POINT('Ctrl Pts',(5.55495848677911,-3.86902074816436,
74.503526709534));
#201673=CARTESIAN_POINT('Ctrl Pts',(5.65703027339572,-3.7135289800787,74.5122759232751));
#201674=CARTESIAN_POINT('Ctrl Pts',(5.75910135422783,-3.55803828715479,
74.521025076519));
#201675=CARTESIAN_POINT('Ctrl Pts',(5.85475793636485,-3.39833700031369,
74.5297742297629));
#201676=CARTESIAN_POINT('Ctrl Pts',(5.9436751446903,-3.23496750747063,74.5385233830068));
#201677=CARTESIAN_POINT('Ctrl Pts',(6.03259176772167,-3.07159909000093,
74.5472724786597));
#201678=CARTESIAN_POINT('Ctrl Pts',(6.11476896873301,-2.90456276652748,
74.5560215743127));
#201679=CARTESIAN_POINT('Ctrl Pts',(6.18992765583072,-2.734425829234,74.5647706699656));
#201680=CARTESIAN_POINT('Ctrl Pts',(6.26508587316051,-2.56428995535552,
74.5735197109336));
#201681=CARTESIAN_POINT('Ctrl Pts',(6.33322554857928,-2.39105376853707,
74.5822687519016));
#201682=CARTESIAN_POINT('Ctrl Pts',(6.39411526761537,-2.21530560971801,
74.5910177928697));
#201683=CARTESIAN_POINT('Ctrl Pts',(6.45500462629089,-2.03955849102044,
74.5997667820587));
#201684=CARTESIAN_POINT('Ctrl Pts',(6.50864402064686,-1.86129970080809,
74.6085157712477));
#201685=CARTESIAN_POINT('Ctrl Pts',(6.55485128390227,-1.68113463051737,
74.6172647604367));
#201686=CARTESIAN_POINT('Ctrl Pts',(6.60199809573133,-1.49730620033714,
74.6261916459073));
#201687=CARTESIAN_POINT('Ctrl Pts',(6.64140720723984,-1.31149343163847,
74.6351185313779));
#201688=CARTESIAN_POINT('Ctrl Pts',(6.67293928736435,-1.12435326617099,
74.6440454168485));
#201689=CARTESIAN_POINT('Ctrl Pts',(6.70384625887597,-0.940923066198626,
74.6527953310259));
#201690=CARTESIAN_POINT('Ctrl Pts',(6.7271855458891,-0.756217898710915,
74.6615452452034));
#201691=CARTESIAN_POINT('Ctrl Pts',(6.74287786822208,-0.570865180441881,
74.6702951593809));
#201692=CARTESIAN_POINT('Ctrl Pts',(6.75856988195491,-0.385516107259511,
74.6790449014853));
#201693=CARTESIAN_POINT('Ctrl Pts',(6.76661520775807,-0.199519794411015,
74.6877946435898));
#201694=CARTESIAN_POINT('Ctrl Pts',(6.76698651789742,-0.0135080196403423,
74.6965443856943));
#201695=CARTESIAN_POINT('Ctrl Pts',(6.76735782122824,0.172500344328303,
74.7052939673593));
#201696=CARTESIAN_POINT('Ctrl Pts',(6.76005538990864,0.358523883025376,
74.7140435490242));
#201697=CARTESIAN_POINT('Ctrl Pts',(6.74510402735808,0.543930749377023,
74.7227931306892));
#201698=CARTESIAN_POINT('Ctrl Pts',(6.73015291909244,0.729334462426012,
74.7315425635459));
#201699=CARTESIAN_POINT('Ctrl Pts',(6.70755316295583,0.914121238442667,
74.7402919964026));
#201700=CARTESIAN_POINT('Ctrl Pts',(6.67738151861353,1.0976634524655,74.7490414292593));
#201701=CARTESIAN_POINT('Ctrl Pts',(6.64721034732138,1.28120278879723,74.7577907249368));
#201702=CARTESIAN_POINT('Ctrl Pts',(6.60946757187517,1.46349731939927,74.7665400206143));
#201703=CARTESIAN_POINT('Ctrl Pts',(6.56428138091727,1.64392790357209,74.7752893162918));
#201704=CARTESIAN_POINT('Ctrl Pts',(6.51909583837885,1.82435589857543,74.7840384864174));
#201705=CARTESIAN_POINT('Ctrl Pts',(6.46646716368766,2.00291972270102,74.792787656543));
#201706=CARTESIAN_POINT('Ctrl Pts',(6.4065740984666,2.17901292351763,74.8015368266686));
#201707=CARTESIAN_POINT('Ctrl Pts',(6.34668181313732,2.3551038313536,74.8102858828677));
#201708=CARTESIAN_POINT('Ctrl Pts',(6.27952541883615,2.52872390898159,74.8190349390668));
#201709=CARTESIAN_POINT('Ctrl Pts',(6.20533299143027,2.69928350964975,74.8277839952659));
#201710=CARTESIAN_POINT('Ctrl Pts',(6.1283160295828,2.87633638036279,74.8368661314225));
#201711=CARTESIAN_POINT('Ctrl Pts',(6.04371690571527,3.05009086668109,74.8459482675791));
#201712=CARTESIAN_POINT('Ctrl Pts',(5.95184520282711,3.21991112945433,74.8550304037357));
#201713=CARTESIAN_POINT('Ctrl Pts',(5.8633354947363,3.38351691244787,74.8637801840793));
#201714=CARTESIAN_POINT('Ctrl Pts',(5.76807618062037,3.54347103772773,74.8725299644229));
#201715=CARTESIAN_POINT('Ctrl Pts',(5.66639083270042,3.69923018087395,74.8812797447664));
#201716=CARTESIAN_POINT('Ctrl Pts',(5.56470914041585,3.85498372440678,74.8900292105513));
#201717=CARTESIAN_POINT('Ctrl Pts',(5.45660203329856,4.00654234759486,74.8987786763363));
#201718=CARTESIAN_POINT('Ctrl Pts',(5.34243669795458,4.15339128042954,74.9075281421212));
#201719=CARTESIAN_POINT('Ctrl Pts',(5.22827486005289,4.30023571456359,74.9162773398672));
#201720=CARTESIAN_POINT('Ctrl Pts',(5.10805534120313,4.4423705208228,74.9250265376132));
#201721=CARTESIAN_POINT('Ctrl Pts',(4.98218644291713,4.57931296681202,74.9337757353592));
#201722=CARTESIAN_POINT('Ctrl Pts',(4.85632073169895,4.71625194534528,74.9425247115708));
#201723=CARTESIAN_POINT('Ctrl Pts',(4.72480612119228,4.84799861574302,74.9512736877825));
#201724=CARTESIAN_POINT('Ctrl Pts',(4.58808925182879,4.97410554946848,74.9600226639941));
#201725=CARTESIAN_POINT('Ctrl Pts',(4.45136349420285,5.1002206816813,74.9687722089958));
#201726=CARTESIAN_POINT('Ctrl Pts',(4.30943501155045,5.22069514917263,74.9775217539975));
#201727=CARTESIAN_POINT('Ctrl Pts',(4.16278587375539,5.33511975210141,74.9862712989992));
#201728=CARTESIAN_POINT('Ctrl Pts',(4.01614535682984,5.44953762850192,74.995020329653));
#201729=CARTESIAN_POINT('Ctrl Pts',(3.86478496599301,5.55790617573548,75.0037693603067));
#201730=CARTESIAN_POINT('Ctrl Pts',(3.70921874687482,5.6598573557849,75.0125183909605));
#201731=CARTESIAN_POINT('Ctrl Pts',(3.5536504154511,5.76180992014539,75.0212675404101));
#201732=CARTESIAN_POINT('Ctrl Pts',(3.39387638112723,5.85734478588621,75.0300166898597));
#201733=CARTESIAN_POINT('Ctrl Pts',(3.23043927841802,5.94613749155316,75.0387658393093));
#201734=CARTESIAN_POINT('Ctrl Pts',(3.18691767028355,5.96978206966411,75.0410956472143));
#201735=CARTESIAN_POINT('Ctrl Pts',(3.14313645898471,5.99294880644326,75.0434254551192));
#201736=CARTESIAN_POINT('Ctrl Pts',(3.09910619832135,6.0156321173694,75.0457552630242));
#201737=CARTESIAN_POINT('Ctrl Pts',(3.09910619832135,6.0156321173694,73.0457552630242));
#201738=CARTESIAN_POINT('Ctrl Pts',(2.93375330764824,6.10081787314654,73.0545047109265));
#201739=CARTESIAN_POINT('Ctrl Pts',(2.76488627843065,6.17918207037041,73.0632541588288));
#201740=CARTESIAN_POINT('Ctrl Pts',(2.59307866646694,6.25045854554,73.0720036067311));
#201741=CARTESIAN_POINT('Ctrl Pts',(2.4212724418536,6.32173444515043,73.0807529839814));
#201742=CARTESIAN_POINT('Ctrl Pts',(2.2465259467244,6.38592262741847,73.0895023612317));
#201743=CARTESIAN_POINT('Ctrl Pts',(2.06943269687088,6.44280508110572,73.098251738482));
#201744=CARTESIAN_POINT('Ctrl Pts',(1.89234081822042,6.49968709436177,73.1070010479874));
#201745=CARTESIAN_POINT('Ctrl Pts',(1.7129024940555,6.54926340459555,73.1157503574927));
#201746=CARTESIAN_POINT('Ctrl Pts',(1.53172716625018,6.59136563150393,73.1244996669981));
#201747=CARTESIAN_POINT('Ctrl Pts',(1.35055318107301,6.63346754640716,73.1332489116653));
#201748=CARTESIAN_POINT('Ctrl Pts',(1.16764249714394,6.6680954239578,73.1419981563326));
#201749=CARTESIAN_POINT('Ctrl Pts',(0.983616340614181,6.69513165624671,
73.1507474009998));
#201750=CARTESIAN_POINT('Ctrl Pts',(0.799591486713637,6.72216769715963,
73.1594965837355));
#201751=CARTESIAN_POINT('Ctrl Pts',(0.614451459526477,6.74161215869373,
73.1682457664712));
#201752=CARTESIAN_POINT('Ctrl Pts',(0.428825047910017,6.75339900185714,
73.1769949492069));
#201753=CARTESIAN_POINT('Ctrl Pts',(0.243199888596786,6.76518576550222,
73.1857440729174));
#201754=CARTESIAN_POINT('Ctrl Pts',(0.0570886373916655,6.76931499599834,
73.194493196628));
#201755=CARTESIAN_POINT('Ctrl Pts',(-0.128876626811394,6.76577266947846,
73.2032423203385));
#201756=CARTESIAN_POINT('Ctrl Pts',(-0.314840698188439,6.76223036567992,
73.21199138793));
#201757=CARTESIAN_POINT('Ctrl Pts',(-0.500658497951567,6.75101660879221,
73.2207404555216));
#201758=CARTESIAN_POINT('Ctrl Pts',(-0.685698951926566,6.73216948296215,
73.2294895231131));
#201759=CARTESIAN_POINT('Ctrl Pts',(-0.870738280460138,6.71332247176289,
73.2382385374917));
#201760=CARTESIAN_POINT('Ctrl Pts',(-1.05499998761273,6.68684221356183,
73.2469875518702));
#201761=CARTESIAN_POINT('Ctrl Pts',(-1.23785829161436,6.65281863948519,
73.2557365662487));
#201762=CARTESIAN_POINT('Ctrl Pts',(-1.43007412917419,6.61705395368858,
73.2649332999479));
#201763=CARTESIAN_POINT('Ctrl Pts',(-1.62073882535806,6.57295372727786,
73.2741300336471));
#201764=CARTESIAN_POINT('Ctrl Pts',(-1.80913696091527,6.52068343478276,
73.2833267673463));
#201765=CARTESIAN_POINT('Ctrl Pts',(-1.98838356186122,6.47095219815195,
73.2920767650599));
#201766=CARTESIAN_POINT('Ctrl Pts',(-2.1655782757254,6.41382586850888,73.3008267627736));
#201767=CARTESIAN_POINT('Ctrl Pts',(-2.34011918621703,6.34949849943277,
73.3095767604873));
#201768=CARTESIAN_POINT('Ctrl Pts',(-2.51465655691098,6.28517243495551,
73.3183265807456));
#201769=CARTESIAN_POINT('Ctrl Pts',(-2.68653996295324,6.21364572242376,
73.3270764010039));
#201770=CARTESIAN_POINT('Ctrl Pts',(-2.85518555379981,6.13516132252225,
73.3358262212622));
#201771=CARTESIAN_POINT('Ctrl Pts',(-3.02382794858674,6.05667841000514,
73.3445758756997));
#201772=CARTESIAN_POINT('Ctrl Pts',(-3.18923239109259,5.97123819492092,
73.3533255301372));
#201773=CARTESIAN_POINT('Ctrl Pts',(-3.3508370596767,5.87913088810729,73.3620751845747));
#201774=CARTESIAN_POINT('Ctrl Pts',(-3.51243888042375,5.78702520443118,
73.3708246848237));
#201775=CARTESIAN_POINT('Ctrl Pts',(-3.67024081223669,5.68825280605797,
73.3795741850726));
#201776=CARTESIAN_POINT('Ctrl Pts',(-3.82370687544384,5.58314917682516,
73.3883236853215));
#201777=CARTESIAN_POINT('Ctrl Pts',(-3.97717043817797,5.47804726008034,
73.397073043012));
#201778=CARTESIAN_POINT('Ctrl Pts',(-4.12629803722442,5.3666144808425,73.4058224007025));
#201779=CARTESIAN_POINT('Ctrl Pts',(-4.27058317206889,5.24922931204591,
73.4145717583929));
#201780=CARTESIAN_POINT('Ctrl Pts',(-4.41486614774828,5.13184589986797,
73.423320985153));
#201781=CARTESIAN_POINT('Ctrl Pts',(-4.55430658194418,5.00851045723032,
73.4320702119131));
#201782=CARTESIAN_POINT('Ctrl Pts',(-4.68843089001859,4.87964187103106,
73.4408194386732));
#201783=CARTESIAN_POINT('Ctrl Pts',(-4.82255336917864,4.75077504207933,
73.4495685461291));
#201784=CARTESIAN_POINT('Ctrl Pts',(-4.95135966065174,4.61637541908051,
73.458317653585));
#201785=CARTESIAN_POINT('Ctrl Pts',(-5.07441230869295,4.47689945401787,
73.467066761041));
#201786=CARTESIAN_POINT('Ctrl Pts',(-5.19746344226441,4.33742520555486,
73.4758157608173));
#201787=CARTESIAN_POINT('Ctrl Pts',(-5.31476088454766,4.19287495491336,
73.4845647605937));
#201788=CARTESIAN_POINT('Ctrl Pts',(-5.4259062762883,4.04373961586738,73.49331376037));
#201789=CARTESIAN_POINT('Ctrl Pts',(-5.53706380672648,3.89458798906763,
73.5020637156647));
#201790=CARTESIAN_POINT('Ctrl Pts',(-5.64206777071848,3.74085050155308,
73.5108136709594));
#201791=CARTESIAN_POINT('Ctrl Pts',(-5.74056148163995,3.58304938223181,
73.5195636262541));
#201792=CARTESIAN_POINT('Ctrl Pts',(-5.83905138951866,3.42525435593311,
73.5283132436952));
#201793=CARTESIAN_POINT('Ctrl Pts',(-5.93103139557631,3.26339625497221,
73.5370628611363));
#201794=CARTESIAN_POINT('Ctrl Pts',(-6.01618907820822,3.09802485065052,
73.5458124785774));
#201795=CARTESIAN_POINT('Ctrl Pts',(-6.1013439254495,2.93265895249708,73.5545618046933));
#201796=CARTESIAN_POINT('Ctrl Pts',(-6.17967677261792,2.76378023986123,
73.5633111308091));
#201797=CARTESIAN_POINT('Ctrl Pts',(-6.25092157009179,2.59196229227226,
73.572060456925));
#201798=CARTESIAN_POINT('Ctrl Pts',(-6.32216437407704,2.42014915229219,
73.5808095382274));
#201799=CARTESIAN_POINT('Ctrl Pts',(-6.3863194154887,2.24539720662996,73.5895586195299));
#201800=CARTESIAN_POINT('Ctrl Pts',(-6.44316881037485,2.0682999494785,73.5983077008324));
#201801=CARTESIAN_POINT('Ctrl Pts',(-6.50002334524525,1.89118668024612,
73.6070575731747));
#201802=CARTESIAN_POINT('Ctrl Pts',(-6.54957082411054,1.71172794807862,
73.615807445517));
#201803=CARTESIAN_POINT('Ctrl Pts',(-6.59164294296047,1.53053334250498,
73.6245573178594));
#201804=CARTESIAN_POINT('Ctrl Pts',(-6.633712140821,1.34935131693767,73.6333065827143));
#201805=CARTESIAN_POINT('Ctrl Pts',(-6.66830695239659,1.1664339382994,73.6420558475692));
#201806=CARTESIAN_POINT('Ctrl Pts',(-6.69530988153961,0.982402458342849,
73.6508051124241));
#201807=CARTESIAN_POINT('Ctrl Pts',(-6.7223141969046,0.798361530948973,
73.6595548264311));
#201808=CARTESIAN_POINT('Ctrl Pts',(-6.7417258082926,0.613206671364441,
73.6683045404382));
#201809=CARTESIAN_POINT('Ctrl Pts',(-6.75347878028167,0.427566795115414,
73.6770542544452));
#201810=CARTESIAN_POINT('Ctrl Pts',(-6.76248992368209,0.285234494206924,
73.6837627642335));
#201811=CARTESIAN_POINT('Ctrl Pts',(-6.76699999999995,0.142617266093417,
73.6904712740217));
#201812=CARTESIAN_POINT('Ctrl Pts',(-6.767,2.35809769017265E-12,73.69717978381));
#201813=CARTESIAN_POINT('',(-6.767,2.50669764893102E-12,73.3028202161898));
#201814=CARTESIAN_POINT('Ctrl Pts',(3.09910619832134,6.0156321173694,72.6513713193949));
#201815=CARTESIAN_POINT('Ctrl Pts',(2.93988645429697,6.09765822634244,72.6597884001077));
#201816=CARTESIAN_POINT('Ctrl Pts',(2.77738341495137,6.17337193593024,72.6682054808205));
#201817=CARTESIAN_POINT('Ctrl Pts',(2.61212887414432,6.24252126507083,72.6766225615333));
#201818=CARTESIAN_POINT('Ctrl Pts',(2.44706009708545,6.31159286298236,72.6850301805487));
#201819=CARTESIAN_POINT('Ctrl Pts',(2.27924631418403,6.37411470828925,72.6934377995641));
#201820=CARTESIAN_POINT('Ctrl Pts',(2.10923781216841,6.42988373547446,72.7018454185794));
#201821=CARTESIAN_POINT('Ctrl Pts',(1.9392079965238,6.4856597543121,72.7102540916413));
#201822=CARTESIAN_POINT('Ctrl Pts',(1.7669832318752,6.53468116261311,72.7186627647033));
#201823=CARTESIAN_POINT('Ctrl Pts',(1.59312956559307,6.57679459822437,72.7270714377652));
#201824=CARTESIAN_POINT('Ctrl Pts',(1.41922918817829,6.6189193489049,72.7354823700756));
#201825=CARTESIAN_POINT('Ctrl Pts',(1.24369936248274,6.65413234769309,72.7438933023861));
#201826=CARTESIAN_POINT('Ctrl Pts',(1.06711727979176,6.68233115844836,72.7523042346965));
#201827=CARTESIAN_POINT('Ctrl Pts',(0.89028005608688,6.71057071327607,72.760727319847));
#201828=CARTESIAN_POINT('Ctrl Pts',(0.712387866442494,6.73177575353592,
72.7691504049975));
#201829=CARTESIAN_POINT('Ctrl Pts',(0.534026146759807,6.74589542422478,
72.7775734901479));
#201830=CARTESIAN_POINT('Ctrl Pts',(0.355678451507069,6.76001398469599,
72.7859959129984));
#201831=CARTESIAN_POINT('Ctrl Pts',(0.176861636599639,6.76704829543591,
72.7944183358488));
#201832=CARTESIAN_POINT('Ctrl Pts',(-0.00183830437997168,6.76699975030567,
72.8028407586993));
#201833=CARTESIAN_POINT('Ctrl Pts',(-0.180763637529803,6.76695114394602,
72.8112738046543));
#201834=CARTESIAN_POINT('Ctrl Pts',(-0.359571466234763,6.75980183235657,
72.8197068506094));
#201835=CARTESIAN_POINT('Ctrl Pts',(-0.537677928093749,6.74560534315793,
72.8281398965644));
#201836=CARTESIAN_POINT('Ctrl Pts',(-0.715377632129388,6.73144127576468,
72.8365536832103));
#201837=CARTESIAN_POINT('Ctrl Pts',(-0.892378847347759,6.71026227561055,
72.8449674698562));
#201838=CARTESIAN_POINT('Ctrl Pts',(-1.06811095478611,6.68217240036995,
72.853381256502));
#201839=CARTESIAN_POINT('Ctrl Pts',(-1.24105052271581,6.65452889823411,
72.8616613405937));
#201840=CARTESIAN_POINT('Ctrl Pts',(-1.41315275857235,6.6201296392588,72.8699414246853));
#201841=CARTESIAN_POINT('Ctrl Pts',(-1.58385521493082,6.57903424965522,
72.878221508777));
#201842=CARTESIAN_POINT('Ctrl Pts',(-1.75435970041444,6.53798652011703,
72.8864919901041));
#201843=CARTESIAN_POINT('Ctrl Pts',(-1.92346730065479,6.49025820684884,
72.8947624714312));
#201844=CARTESIAN_POINT('Ctrl Pts',(-2.09062233285272,6.43596047699001,
72.9030329527583));
#201845=CARTESIAN_POINT('Ctrl Pts',(-2.25761228179066,6.38171637187784,
72.911295266111));
#201846=CARTESIAN_POINT('Ctrl Pts',(-2.42265317135319,6.32091588086906,
72.9195575794638));
#201847=CARTESIAN_POINT('Ctrl Pts',(-2.58520099042713,6.25372087953201,
72.9278198928165));
#201848=CARTESIAN_POINT('Ctrl Pts',(-2.74758855745376,6.18659212415626,
72.9360740605501));
#201849=CARTESIAN_POINT('Ctrl Pts',(-2.9074876300941,6.11308155919282,72.9443282282837));
#201850=CARTESIAN_POINT('Ctrl Pts',(-3.06437093980389,6.03340034667727,
72.9525823960172));
#201851=CARTESIAN_POINT('Ctrl Pts',(-3.22116441104271,5.95376476322394,
72.9608318370414));
#201852=CARTESIAN_POINT('Ctrl Pts',(-3.37494524653128,5.86796572892841,
72.9690812780657));
#201853=CARTESIAN_POINT('Ctrl Pts',(-3.52520718160036,5.7762620548927,72.9773307190899));
#201854=CARTESIAN_POINT('Ctrl Pts',(-3.67540325881703,5.68459857338498,
72.9855765444914));
#201855=CARTESIAN_POINT('Ctrl Pts',(-3.82208320952256,5.58703579223704,
72.9938223698928));
#201856=CARTESIAN_POINT('Ctrl Pts',(-3.96476629094543,5.48387793975968,
73.0020681952943));
#201857=CARTESIAN_POINT('Ctrl Pts',(-4.02398769717215,5.44106169955715,
73.0054906709719));
#201858=CARTESIAN_POINT('Ctrl Pts',(-4.08252088026485,5.39728211963936,
73.0089131466495));
#201859=CARTESIAN_POINT('Ctrl Pts',(-4.14033291405278,5.35256315804038,
73.0123356223271));
#201860=CARTESIAN_POINT('Ctrl Pts',(-4.28903258164251,5.23754048388367,
73.0211386510782));
#201861=CARTESIAN_POINT('Ctrl Pts',(-4.43279665683033,5.11642600515404,
73.0299416798293));
#201862=CARTESIAN_POINT('Ctrl Pts',(-4.57116043698929,4.98966744977097,
73.0387447085803));
#201863=CARTESIAN_POINT('Ctrl Pts',(-4.70976229709573,4.86269078333185,
73.047562884537));
#201864=CARTESIAN_POINT('Ctrl Pts',(-4.84294509763682,4.73005081790123,
73.0563810604937));
#201865=CARTESIAN_POINT('Ctrl Pts',(-4.97028196065051,4.59223107341433,
73.0651992364503));
#201866=CARTESIAN_POINT('Ctrl Pts',(-5.09796456485835,4.45403712493097,
73.0740413552513));
#201867=CARTESIAN_POINT('Ctrl Pts',(-5.21976928819236,4.31063545580153,
73.0828834740522));
#201868=CARTESIAN_POINT('Ctrl Pts',(-5.33530858817898,4.16254384588362,
73.0917255928532));
#201869=CARTESIAN_POINT('Ctrl Pts',(-5.45099905431521,4.01425847991506,
73.1005792802638));
#201870=CARTESIAN_POINT('Ctrl Pts',(-5.56040756458574,3.86127113423292,
73.1094329676743));
#201871=CARTESIAN_POINT('Ctrl Pts',(-5.66319003382627,3.70412845899961,
73.1182866550849));
#201872=CARTESIAN_POINT('Ctrl Pts',(-5.76620337901913,3.54663280076187,
73.1271602301623));
#201873=CARTESIAN_POINT('Ctrl Pts',(-5.86256076602242,3.38496337047203,
73.1360338052398));
#201874=CARTESIAN_POINT('Ctrl Pts',(-5.95196277818806,3.21969378777918,
73.1449073803172));
#201875=CARTESIAN_POINT('Ctrl Pts',(-6.04056510611099,3.055902510528,73.1537015829288));
#201876=CARTESIAN_POINT('Ctrl Pts',(-6.12233592568479,2.88857547846388,
73.1624957855403));
#201877=CARTESIAN_POINT('Ctrl Pts',(-6.19703066141498,2.71828990019141,
73.1712899881518));
#201878=CARTESIAN_POINT('Ctrl Pts',(-6.27195892853884,2.54747192792858,
73.1801116856379));
#201879=CARTESIAN_POINT('Ctrl Pts',(-6.33989644591468,2.37338102034605,
73.1889333831241));
#201880=CARTESIAN_POINT('Ctrl Pts',(-6.40056814536355,2.19659200047652,
73.1977550806102));
#201881=CARTESIAN_POINT('Ctrl Pts',(-6.46106297879402,2.02031834395308,
73.2065510616828));
#201882=CARTESIAN_POINT('Ctrl Pts',(-6.51433416114382,1.84136252602717,
73.2153470427554));
#201883=CARTESIAN_POINT('Ctrl Pts',(-6.56015486384009,1.66031839188609,
73.2241430238281));
#201884=CARTESIAN_POINT('Ctrl Pts',(-6.60589579977616,1.47958942759585,
73.2329236924574));
#201885=CARTESIAN_POINT('Ctrl Pts',(-6.64421205068951,1.29677966067728,
73.2417043610867));
#201886=CARTESIAN_POINT('Ctrl Pts',(-6.67492564861701,1.11250015075723,
73.250485029716));
#201887=CARTESIAN_POINT('Ctrl Pts',(-6.70555455524957,0.928728782877719,
73.2592414860665));
#201888=CARTESIAN_POINT('Ctrl Pts',(-6.72862258426218,0.74349602688161,
73.267997942417));
#201889=CARTESIAN_POINT('Ctrl Pts',(-6.74400230942963,0.557424300159112,
73.2767543987675));
#201890=CARTESIAN_POINT('Ctrl Pts',(-6.75926286279254,0.372794374457539,
73.2854430045749));
#201891=CARTESIAN_POINT('Ctrl Pts',(-6.76695376716036,0.187338701658777,
73.2941316103824));
#201892=CARTESIAN_POINT('Ctrl Pts',(-6.76699979207347,0.00167752126097696,
73.3028202161898));
#201893=CARTESIAN_POINT('Ctrl Pts',(-6.767,2.50669783734745E-12,73.3028202161898));
#201894=CARTESIAN_POINT('Ctrl Pts',(-6.76700000000007,-0.18600724952452,
73.311569728001));
#201895=CARTESIAN_POINT('Ctrl Pts',(-6.75932637294533,-0.372014355747722,
73.3203192398122));
#201896=CARTESIAN_POINT('Ctrl Pts',(-6.74400518264197,-0.557389537485457,
73.3290687516234));
#201897=CARTESIAN_POINT('Ctrl Pts',(-6.72868405705108,-0.742763936249799,
73.337818226479));
#201898=CARTESIAN_POINT('Ctrl Pts',(-6.70571545645752,-0.927506130240312,
73.3465677013347));
#201899=CARTESIAN_POINT('Ctrl Pts',(-6.67517739404833,-1.1109886398997,
73.3553171761904));
#201900=CARTESIAN_POINT('Ctrl Pts',(-6.64463945808708,-1.29447038981914,
73.3640666148174));
#201901=CARTESIAN_POINT('Ctrl Pts',(-6.60653217008359,-1.47669218313665,
73.3728160534444));
#201902=CARTESIAN_POINT('Ctrl Pts',(-6.56098496092678,-1.65703510599281,
73.3815654920714));
#201903=CARTESIAN_POINT('Ctrl Pts',(-6.51543793658299,-1.8373772970869,
73.3903148951966));
#201904=CARTESIAN_POINT('Ctrl Pts',(-6.46245112167425,-2.01584035510912,
73.3990642983218));
#201905=CARTESIAN_POINT('Ctrl Pts',(-6.4022044837426,-2.19181813760772,
73.4078137014469));
#201906=CARTESIAN_POINT('Ctrl Pts',(-6.34195808526509,-2.3677952206713,
73.416563069797));
#201907=CARTESIAN_POINT('Ctrl Pts',(-6.27445201433107,-2.54128677684158,
73.4253124381471));
#201908=CARTESIAN_POINT('Ctrl Pts',(-6.19991555071903,-2.71170355384809,
73.4340618064972));
#201909=CARTESIAN_POINT('Ctrl Pts',(-6.12537937716695,-2.88211966767471,
73.442811140799));
#201910=CARTESIAN_POINT('Ctrl Pts',(-6.04381298052524,-3.04946076371776,
73.4515604751008));
#201911=CARTESIAN_POINT('Ctrl Pts',(-5.95549339335838,-3.21315848374535,
73.4603098094026));
#201912=CARTESIAN_POINT('Ctrl Pts',(-5.86717414255423,-3.37685558033468,
73.4690591103828));
#201913=CARTESIAN_POINT('Ctrl Pts',(-5.7721018887662,-3.5369090764672,73.4778084113629));
#201914=CARTESIAN_POINT('Ctrl Pts',(-5.67059953347026,-3.6927753696924,
73.4865577123431));
#201915=CARTESIAN_POINT('Ctrl Pts',(-5.56909755631424,-3.84864108224864,
73.4953069807284));
#201916=CARTESIAN_POINT('Ctrl Pts',(-5.46116568196902,-4.00031938297446,
73.5040562491137));
#201917=CARTESIAN_POINT('Ctrl Pts',(-5.34717048533667,-4.14729511859772,
73.5128055174989));
#201918=CARTESIAN_POINT('Ctrl Pts',(-5.23317570391897,-4.29427031887843,
73.521554754016));
#201919=CARTESIAN_POINT('Ctrl Pts',(-5.11311782003571,-4.43654276189482,
73.530303990533));
#201920=CARTESIAN_POINT('Ctrl Pts',(-4.98740458984806,-4.57362924351795,
73.5390532270501));
#201921=CARTESIAN_POINT('Ctrl Pts',(-4.86169180711799,-4.71071523720209,
73.5478024324255));
#201922=CARTESIAN_POINT('Ctrl Pts',(-4.73032391204231,-4.84261509523179,
73.556551637801));
#201923=CARTESIAN_POINT('Ctrl Pts',(-4.59374707013663,-4.96888084538271,
73.5653008431764));
#201924=CARTESIAN_POINT('Ctrl Pts',(-4.45717070301521,-5.09514615659397,
73.5740500181368));
#201925=CARTESIAN_POINT('Ctrl Pts',(-4.3153856357113,-5.21577720459453,
73.5827991930973));
#201926=CARTESIAN_POINT('Ctrl Pts',(-4.16887341029612,-5.33036429232806,
73.5915483680577));
#201927=CARTESIAN_POINT('Ctrl Pts',(-4.0223616820382,-5.44495099123531,
73.6002975133297));
#201928=CARTESIAN_POINT('Ctrl Pts',(-3.87112305348291,-5.55349359438513,
73.6090466586018));
#201929=CARTESIAN_POINT('Ctrl Pts',(-3.71567117017898,-5.65562346298803,
73.6177958038738));
#201930=CARTESIAN_POINT('Ctrl Pts',(-3.56021980145966,-5.75775299351553,
73.6265449201839));
#201931=CARTESIAN_POINT('Ctrl Pts',(-3.40055544538506,-5.85346967463782,
73.6352940364941));
#201932=CARTESIAN_POINT('Ctrl Pts',(-3.23722035987019,-5.94244842986811,
73.6440431528043));
#201933=CARTESIAN_POINT('Ctrl Pts',(-3.07388580147368,-6.03142689794433,
73.6527922408791));
#201934=CARTESIAN_POINT('Ctrl Pts',(-2.90688078896788,-6.11366734656681,
73.6615413289539));
#201935=CARTESIAN_POINT('Ctrl Pts',(-2.73677250721603,-6.18889046952251,
73.6702904170288));
#201936=CARTESIAN_POINT('Ctrl Pts',(-2.5666647603171,-6.26411335596234,
73.6790394775948));
#201937=CARTESIAN_POINT('Ctrl Pts',(-2.39345402575388,-6.33231884500472,
73.6877885381608));
#201938=CARTESIAN_POINT('Ctrl Pts',(-2.21772856065808,-6.39327529762652,
73.6965375987268));
#201939=CARTESIAN_POINT('Ctrl Pts',(-2.04200363348718,-6.45423156365047,
73.7052866325105));
#201940=CARTESIAN_POINT('Ctrl Pts',(-1.86376426189471,-6.50793874375603,
73.7140356662942));
#201941=CARTESIAN_POINT('Ctrl Pts',(-1.68361577753334,-6.55421443909496,
73.7227847000779));
#201942=CARTESIAN_POINT('Ctrl Pts',(-1.50346782968002,-6.60048999661821,
73.7315337078058));
#201943=CARTESIAN_POINT('Ctrl Pts',(-1.32141105795213,-6.63933404237667,
73.7402827155336));
#201944=CARTESIAN_POINT('Ctrl Pts',(-1.13806375487272,-6.67061465607518,
73.7490317232614));
#201945=CARTESIAN_POINT('Ctrl Pts',(-0.954716982605621,-6.70189517921259,
73.7577807056598));
#201946=CARTESIAN_POINT('Ctrl Pts',(-0.770079968904851,-6.72561226592197,
73.7665296880582));
#201947=CARTESIAN_POINT('Ctrl Pts',(-0.584779765561063,-6.74168536983078,
73.7752786704566));
#201948=CARTESIAN_POINT('Ctrl Pts',(-0.391489830654086,-6.75845151013837,
73.7844048894665));
#201949=CARTESIAN_POINT('Ctrl Pts',(-0.197478578241089,-6.76689983031617,
73.7935311084764));
#201950=CARTESIAN_POINT('Ctrl Pts',(-0.00346287645406101,-6.76699911397118,
73.8026573274862));
#201951=CARTESIAN_POINT('Ctrl Pts',(0.184489834652092,-6.76709529501196,
73.811498352152));
#201952=CARTESIAN_POINT('Ctrl Pts',(0.372446404247607,-6.75935639738178,
73.8203393768178));
#201953=CARTESIAN_POINT('Ctrl Pts',(0.559755019486604,-6.74380925873201,
73.8291804014837));
#201954=CARTESIAN_POINT('Ctrl Pts',(0.745134705520065,-6.72842222659825,
73.8379303800934));
#201955=CARTESIAN_POINT('Ctrl Pts',(0.92987943122688,-6.70538706057547,
73.8466803587031));
#201956=CARTESIAN_POINT('Ctrl Pts',(1.11336163626659,-6.67478200894155,
73.8554303373129));
#201957=CARTESIAN_POINT('Ctrl Pts',(1.2968419630057,-6.64417727061042,73.8641802263494));
#201958=CARTESIAN_POINT('Ctrl Pts',(1.47905951217378,-6.6060028489062,73.872930115386));
#201959=CARTESIAN_POINT('Ctrl Pts',(1.65939532066969,-6.5603884160726,73.8816800044225));
#201960=CARTESIAN_POINT('Ctrl Pts',(1.83972934300687,-6.51477443503289,
73.8904298067946));
#201961=CARTESIAN_POINT('Ctrl Pts',(2.0181813840615,-6.46172066062177,73.8991796091668));
#201962=CARTESIAN_POINT('Ctrl Pts',(2.19414528354085,-6.40140730423517,
73.907929411539));
#201963=CARTESIAN_POINT('Ctrl Pts',(2.37010749863886,-6.34109452518685,
73.9166791301553));
#201964=CARTESIAN_POINT('Ctrl Pts',(2.54358134866346,-6.2735223961655,73.9254288487716));
#201965=CARTESIAN_POINT('Ctrl Pts',(2.71397759435442,-6.19892043966869,
73.9341785673879));
#201966=CARTESIAN_POINT('Ctrl Pts',(2.88437226558005,-6.12431917249571,
73.9429282051566));
#201967=CARTESIAN_POINT('Ctrl Pts',(3.05168912680833,-6.0426883227886,73.9516778429253));
#201968=CARTESIAN_POINT('Ctrl Pts',(3.21535986273728,-5.95430516123402,
73.960427480694));
#201969=CARTESIAN_POINT('Ctrl Pts',(3.37902914072727,-5.86592278697507,
73.9691770405231));
#201970=CARTESIAN_POINT('Ctrl Pts',(3.5390521062147,-5.77078835742004,73.9779266003522));
#201971=CARTESIAN_POINT('Ctrl Pts',(3.69488522831607,-5.66922500431688,
73.9866761601812));
#201972=CARTESIAN_POINT('Ctrl Pts',(3.85071701406866,-5.56766252217145,
73.9954256449784));
#201973=CARTESIAN_POINT('Ctrl Pts',(4.00235878822346,-5.45967138329413,
74.0041751297755));
#201974=CARTESIAN_POINT('Ctrl Pts',(4.14929549611283,-5.3456183819964,74.0129246145726));
#201975=CARTESIAN_POINT('Ctrl Pts',(4.29623099276058,-5.23156632087042,
74.0216740272452));
#201976=CARTESIAN_POINT('Ctrl Pts',(4.43846127436007,-5.11145267304983,
74.0304234399178));
#201977=CARTESIAN_POINT('Ctrl Pts',(4.57550326054431,-4.98568540049895,
74.0391728525904));
#201978=CARTESIAN_POINT('Ctrl Pts',(4.71254416257766,-4.85991912290374,
74.0479221960457));
#201979=CARTESIAN_POINT('Ctrl Pts',(4.84439664018744,-4.72849950385436,
74.0566715395009));
#201980=CARTESIAN_POINT('Ctrl Pts',(4.97061286794725,-4.59187289861089,
74.0654208829561));
#201981=CARTESIAN_POINT('Ctrl Pts',(5.09682813912663,-4.45524732884709,
74.0741701601009));
#201982=CARTESIAN_POINT('Ctrl Pts',(5.21740705147816,-4.31341506235815,
74.0829194372458));
#201983=CARTESIAN_POINT('Ctrl Pts',(5.33194007545673,-4.16685781275754,
74.0916687143906));
#201984=CARTESIAN_POINT('Ctrl Pts',(5.44647226944465,-4.02030162521869,
74.1004179281317));
#201985=CARTESIAN_POINT('Ctrl Pts',(5.55495848628096,-3.86902074887959,
74.1091671418728));
#201986=CARTESIAN_POINT('Ctrl Pts',(5.65703027291773,-3.71352898080685,
74.117916355614));
#201987=CARTESIAN_POINT('Ctrl Pts',(5.75910135376982,-3.55803828789613,
74.1266655088579));
#201988=CARTESIAN_POINT('Ctrl Pts',(5.85475793592736,-3.3983370010674,74.1354146621017));
#201989=CARTESIAN_POINT('Ctrl Pts',(5.94367514427382,-3.23496750823584,
74.1441638153456));
#201990=CARTESIAN_POINT('Ctrl Pts',(6.03259176732619,-3.07159909077765,
74.1529129109985));
#201991=CARTESIAN_POINT('Ctrl Pts',(6.114768968359,-2.90456276731484,74.1616620066515));
#201992=CARTESIAN_POINT('Ctrl Pts',(6.1899276554786,-2.73442583003109,74.1704111023044));
#201993=CARTESIAN_POINT('Ctrl Pts',(6.2650858728303,-2.5642899561623,74.1791601432724));
#201994=CARTESIAN_POINT('Ctrl Pts',(6.33322554827137,-2.39105376935261,
74.1879091842405));
#201995=CARTESIAN_POINT('Ctrl Pts',(6.3941152673301,-2.21530561054139,74.1966582252085));
#201996=CARTESIAN_POINT('Ctrl Pts',(6.45500462602821,-2.03955849185179,
74.2054072143975));
#201997=CARTESIAN_POINT('Ctrl Pts',(6.5086440204071,-1.86129970164647,74.2141562035865));
#201998=CARTESIAN_POINT('Ctrl Pts',(6.55485128368569,-1.68113463136183,
74.2229051927756));
#201999=CARTESIAN_POINT('Ctrl Pts',(6.60199809554296,-1.49730620117003,
74.231832078247));
#202000=CARTESIAN_POINT('Ctrl Pts',(6.64140720707845,-1.31149343245843,
74.2407589637184));
#202001=CARTESIAN_POINT('Ctrl Pts',(6.67293928722858,-1.1243532669768,74.2496858491898));
#202002=CARTESIAN_POINT('Ctrl Pts',(6.70384625876233,-0.940923067008231,
74.2584357633673));
#202003=CARTESIAN_POINT('Ctrl Pts',(6.72718554579776,-0.756217899523402,
74.2671856775448));
#202004=CARTESIAN_POINT('Ctrl Pts',(6.74287786815312,-0.570865181256328,
74.2759355917222));
#202005=CARTESIAN_POINT('Ctrl Pts',(6.75856988190835,-0.385516108075853,
74.2846853338267));
#202006=CARTESIAN_POINT('Ctrl Pts',(6.76661520773397,-0.199519795228328,
74.2934350759312));
#202007=CARTESIAN_POINT('Ctrl Pts',(6.76698651789579,-0.0135080204576999,
74.3021848180357));
#202008=CARTESIAN_POINT('Ctrl Pts',(6.76735782124908,0.172500343510837,
74.3109343997006));
#202009=CARTESIAN_POINT('Ctrl Pts',(6.76005538995195,0.358523882208727,
74.3196839813656));
#202010=CARTESIAN_POINT('Ctrl Pts',(6.74510402742379,0.543930748562116,
74.3284335630306));
#202011=CARTESIAN_POINT('Ctrl Pts',(6.73015291918055,0.729334461612975,
74.3371829958872));
#202012=CARTESIAN_POINT('Ctrl Pts',(6.70755316306626,0.914121237632424,
74.3459324287439));
#202013=CARTESIAN_POINT('Ctrl Pts',(6.67738151874611,1.09766345165897,74.3546818616006));
#202014=CARTESIAN_POINT('Ctrl Pts',(6.64721034747613,1.28120278799434,74.3634311572781));
#202015=CARTESIAN_POINT('Ctrl Pts',(6.60946757205194,1.46349731860093,74.3721804529556));
#202016=CARTESIAN_POINT('Ctrl Pts',(6.56428138111583,1.64392790277922,74.3809297486332));
#202017=CARTESIAN_POINT('Ctrl Pts',(6.51909583859919,1.82435589778807,74.3896789187588));
#202018=CARTESIAN_POINT('Ctrl Pts',(6.46646716392955,2.00291972192008,74.3984280888844));
#202019=CARTESIAN_POINT('Ctrl Pts',(6.40657409872973,2.17901292274399,74.40717725901));
#202020=CARTESIAN_POINT('Ctrl Pts',(6.34668181342172,2.35510383058719,74.4159263152091));
#202021=CARTESIAN_POINT('Ctrl Pts',(6.27952541914152,2.52872390822329,74.4246753714082));
#202022=CARTESIAN_POINT('Ctrl Pts',(6.20533299175623,2.69928350890041,74.4334244276073));
#202023=CARTESIAN_POINT('Ctrl Pts',(6.12831602991656,2.87633637965397,74.4425065637655));
#202024=CARTESIAN_POINT('Ctrl Pts',(6.04371690605376,3.05009086601253,74.4515886999237));
#202025=CARTESIAN_POINT('Ctrl Pts',(5.95184520316735,3.21991112882543,74.4606708360819));
#202026=CARTESIAN_POINT('Ctrl Pts',(5.86333549509379,3.38351691182837,74.4694206164255));
#202027=CARTESIAN_POINT('Ctrl Pts',(5.76807618099473,3.54347103711835,74.478170396769));
#202028=CARTESIAN_POINT('Ctrl Pts',(5.66639083309119,3.69923018027537,74.4869201771126));
#202029=CARTESIAN_POINT('Ctrl Pts',(5.56470914082305,3.85498372381899,74.4956696428975));
#202030=CARTESIAN_POINT('Ctrl Pts',(5.45660203372172,4.00654234701855,74.5044191086824));
#202031=CARTESIAN_POINT('Ctrl Pts',(5.34243669839322,4.15339127986533,74.5131685744674));
#202032=CARTESIAN_POINT('Ctrl Pts',(5.22827486050695,4.30023571401154,74.5219177722134));
#202033=CARTESIAN_POINT('Ctrl Pts',(5.10805534167212,4.44237052028354,74.5306669699594));
#202034=CARTESIAN_POINT('Ctrl Pts',(4.98218644340049,4.57931296628614,74.5394161677054));
#202035=CARTESIAN_POINT('Ctrl Pts',(4.85632073219707,4.71625194483236,74.548165143917));
#202036=CARTESIAN_POINT('Ctrl Pts',(4.72480612170463,4.84799861524367,74.5569141201287));
#202037=CARTESIAN_POINT('Ctrl Pts',(4.58808925235481,4.97410554898329,74.5656630963403));
#202038=CARTESIAN_POINT('Ctrl Pts',(4.45136349474225,5.10022068121052,74.574412641342));
#202039=CARTESIAN_POINT('Ctrl Pts',(4.30943501210264,5.22069514871682,74.5831621863437));
#202040=CARTESIAN_POINT('Ctrl Pts',(4.16278587431974,5.33511975166107,74.5919117313454));
#202041=CARTESIAN_POINT('Ctrl Pts',(4.01614535740639,5.44953762807702,74.6006607619991));
#202042=CARTESIAN_POINT('Ctrl Pts',(3.86478496658113,5.55790617532652,74.6094097926528));
#202043=CARTESIAN_POINT('Ctrl Pts',(3.70921874747383,5.65985735539233,74.6181588233066));
#202044=CARTESIAN_POINT('Ctrl Pts',(3.55365041606096,5.76180991976925,74.6269079727562));
#202045=CARTESIAN_POINT('Ctrl Pts',(3.39387638174726,5.85734478552695,74.6356571222058));
#202046=CARTESIAN_POINT('Ctrl Pts',(3.23043927904751,5.94613749121117,74.6444062716554));
#202047=CARTESIAN_POINT('Ctrl Pts',(3.1869176707057,5.96978206944073,74.6467360795716));
#202048=CARTESIAN_POINT('Ctrl Pts',(3.14313645919697,5.99294880633391,74.6490658874878));
#202049=CARTESIAN_POINT('Ctrl Pts',(3.09910619832131,6.01563211736942,74.651395695404));
#202050=CARTESIAN_POINT('Origin',(0.,0.,4.30282021618968));
#202051=CARTESIAN_POINT('',(3.09910619832125,6.01563211736945,77.0457552630242));
#202052=CARTESIAN_POINT('',(3.09910619832139,6.01563211736937,76.6513581962709));
#202053=CARTESIAN_POINT('',(3.09910619832133,6.0156321173694,4.30282021618968));
#202054=CARTESIAN_POINT('',(-6.767,6.79793587124441E-10,75.6971797837782));
#202055=CARTESIAN_POINT('Ctrl Pts',(-6.767,2.69602239337994E-12,75.69717978381));
#202056=CARTESIAN_POINT('Ctrl Pts',(-6.76700000000007,-0.186007249524269,
75.7059292956212));
#202057=CARTESIAN_POINT('Ctrl Pts',(-6.75932637294534,-0.372014355747412,
75.7146788074323));
#202058=CARTESIAN_POINT('Ctrl Pts',(-6.744005182642,-0.557389537485085,
75.7234283192435));
#202059=CARTESIAN_POINT('Ctrl Pts',(-6.72868405705111,-0.742763936249558,
75.7321777940992));
#202060=CARTESIAN_POINT('Ctrl Pts',(-6.70571545645754,-0.927506130240202,
75.7409272689549));
#202061=CARTESIAN_POINT('Ctrl Pts',(-6.67517739404833,-1.11098863989971,
75.7496767438106));
#202062=CARTESIAN_POINT('Ctrl Pts',(-6.64463945808705,-1.29447038981935,
75.7584261824376));
#202063=CARTESIAN_POINT('Ctrl Pts',(-6.60653217008351,-1.47669218313704,
75.7671756210647));
#202064=CARTESIAN_POINT('Ctrl Pts',(-6.56098496092664,-1.65703510599339,
75.7759250596917));
#202065=CARTESIAN_POINT('Ctrl Pts',(-6.5154379365828,-1.8373772970876,75.7846744628168));
#202066=CARTESIAN_POINT('Ctrl Pts',(-6.462451121674,-2.01584035510994,75.793423865942));
#202067=CARTESIAN_POINT('Ctrl Pts',(-6.40220448374228,-2.19181813760866,
75.8021732690672));
#202068=CARTESIAN_POINT('Ctrl Pts',(-6.34195808526476,-2.36779522067217,
75.8109226374173));
#202069=CARTESIAN_POINT('Ctrl Pts',(-6.27445201433075,-2.54128677684238,
75.8196720057674));
#202070=CARTESIAN_POINT('Ctrl Pts',(-6.19991555071871,-2.71170355384883,
75.8284213741175));
#202071=CARTESIAN_POINT('Ctrl Pts',(-6.12537937716666,-2.88211966767532,
75.8371707084193));
#202072=CARTESIAN_POINT('Ctrl Pts',(-6.043812980525,-3.04946076371825,75.845920042721));
#202073=CARTESIAN_POINT('Ctrl Pts',(-5.95549339335818,-3.21315848374571,
75.8546693770228));
#202074=CARTESIAN_POINT('Ctrl Pts',(-5.86717414255396,-3.37685558033516,
75.863418678003));
#202075=CARTESIAN_POINT('Ctrl Pts',(-5.77210188876585,-3.53690907646778,
75.8721679789832));
#202076=CARTESIAN_POINT('Ctrl Pts',(-5.67059953346982,-3.69277536969308,
75.8809172799633));
#202077=CARTESIAN_POINT('Ctrl Pts',(-5.56909755631364,-3.84864108224952,
75.8896665483486));
#202078=CARTESIAN_POINT('Ctrl Pts',(-5.46116568196824,-4.00031938297553,
75.8984158167339));
#202079=CARTESIAN_POINT('Ctrl Pts',(-5.3471704853357,-4.14729511859896,
75.9071650851192));
#202080=CARTESIAN_POINT('Ctrl Pts',(-5.23317570391805,-4.29427031887955,
75.9159143216363));
#202081=CARTESIAN_POINT('Ctrl Pts',(-5.11311782003484,-4.43654276189582,
75.9246635581533));
#202082=CARTESIAN_POINT('Ctrl Pts',(-4.98740458984725,-4.57362924351883,
75.9334127946703));
#202083=CARTESIAN_POINT('Ctrl Pts',(-4.86169180711724,-4.71071523720286,
75.9421620000458));
#202084=CARTESIAN_POINT('Ctrl Pts',(-4.73032391204163,-4.84261509523246,
75.9509112054212));
#202085=CARTESIAN_POINT('Ctrl Pts',(-4.59374707013602,-4.96888084538327,
75.9596604107966));
#202086=CARTESIAN_POINT('Ctrl Pts',(-4.45717070301449,-5.0951461565946,
75.9684095857571));
#202087=CARTESIAN_POINT('Ctrl Pts',(-4.31538563571046,-5.21577720459523,
75.9771587607175));
#202088=CARTESIAN_POINT('Ctrl Pts',(-4.16887341029516,-5.33036429232881,
75.985907935678));
#202089=CARTESIAN_POINT('Ctrl Pts',(-4.02236168203702,-5.44495099123619,
75.99465708095));
#202090=CARTESIAN_POINT('Ctrl Pts',(-3.8711230534815,-5.55349359438613,
76.003406226222));
#202091=CARTESIAN_POINT('Ctrl Pts',(-3.71567117017732,-5.65562346298912,
76.0121553714941));
#202092=CARTESIAN_POINT('Ctrl Pts',(-3.56021980145791,-5.75775299351661,
76.0209044878042));
#202093=CARTESIAN_POINT('Ctrl Pts',(-3.40055544538322,-5.85346967463889,
76.0296536041144));
#202094=CARTESIAN_POINT('Ctrl Pts',(-3.23722035986827,-5.94244842986915,
76.0384027204246));
#202095=CARTESIAN_POINT('Ctrl Pts',(-3.07388580147139,-6.03142689794551,
76.0471518084994));
#202096=CARTESIAN_POINT('Ctrl Pts',(-2.90688078896521,-6.11366734656809,
76.0559008965743));
#202097=CARTESIAN_POINT('Ctrl Pts',(-2.73677250721297,-6.18889046952386,
76.0646499846491));
#202098=CARTESIAN_POINT('Ctrl Pts',(-2.56666476031406,-6.26411335596358,
76.0733990452152));
#202099=CARTESIAN_POINT('Ctrl Pts',(-2.39345402575087,-6.33231884500586,
76.0821481057812));
#202100=CARTESIAN_POINT('Ctrl Pts',(-2.2177285606551,-6.39327529762755,
76.0908971663472));
#202101=CARTESIAN_POINT('Ctrl Pts',(-2.04200363348435,-6.45423156365136,
76.0996462001309));
#202102=CARTESIAN_POINT('Ctrl Pts',(-1.86376426189204,-6.5079387437568,
76.1083952339146));
#202103=CARTESIAN_POINT('Ctrl Pts',(-1.68361577753084,-6.5542144390956,
76.1171442676983));
#202104=CARTESIAN_POINT('Ctrl Pts',(-1.5034678296775,-6.60048999661879,
76.1258932754261));
#202105=CARTESIAN_POINT('Ctrl Pts',(-1.32141105794959,-6.63933404237717,
76.1346422831539));
#202106=CARTESIAN_POINT('Ctrl Pts',(-1.13806375487016,-6.67061465607562,
76.1433912908817));
#202107=CARTESIAN_POINT('Ctrl Pts',(-0.954716982603054,-6.70189517921296,
76.1521402732801));
#202108=CARTESIAN_POINT('Ctrl Pts',(-0.770079968902272,-6.72561226592226,
76.1608892556785));
#202109=CARTESIAN_POINT('Ctrl Pts',(-0.584779765558476,-6.741685369831,
76.1696382380769));
#202110=CARTESIAN_POINT('Ctrl Pts',(-0.391489830651555,-6.75845151013851,
76.1787644570868));
#202111=CARTESIAN_POINT('Ctrl Pts',(-0.197478578238618,-6.76689983031624,
76.1878906760966));
#202112=CARTESIAN_POINT('Ctrl Pts',(-0.00346287645165238,-6.76699911397118,
76.1970168951065));
#202113=CARTESIAN_POINT('Ctrl Pts',(0.184489834654503,-6.76709529501189,
76.2058579197723));
#202114=CARTESIAN_POINT('Ctrl Pts',(0.372446404250014,-6.75935639738165,
76.2146989444381));
#202115=CARTESIAN_POINT('Ctrl Pts',(0.559755019489007,-6.74380925873181,
76.2235399691039));
#202116=CARTESIAN_POINT('Ctrl Pts',(0.745134705522528,-6.72842222659797,
76.2322899477137));
#202117=CARTESIAN_POINT('Ctrl Pts',(0.929879431229403,-6.70538706057512,
76.2410399263234));
#202118=CARTESIAN_POINT('Ctrl Pts',(1.11336163626917,-6.67478200894112,
76.2497899049332));
#202119=CARTESIAN_POINT('Ctrl Pts',(1.29684196300826,-6.64417727060992,
76.2585397939697));
#202120=CARTESIAN_POINT('Ctrl Pts',(1.47905951217633,-6.60600284890563,
76.2672896830063));
#202121=CARTESIAN_POINT('Ctrl Pts',(1.65939532067223,-6.56038841607196,
76.2760395720428));
#202122=CARTESIAN_POINT('Ctrl Pts',(1.83972934300939,-6.51477443503218,
76.284789374415));
#202123=CARTESIAN_POINT('Ctrl Pts',(2.018181384064,-6.46172066062099,76.2935391767871));
#202124=CARTESIAN_POINT('Ctrl Pts',(2.19414528354333,-6.40140730423432,
76.3022889791593));
#202125=CARTESIAN_POINT('Ctrl Pts',(2.37010749864125,-6.34109452518595,
76.3110386977756));
#202126=CARTESIAN_POINT('Ctrl Pts',(2.54358134866577,-6.27352239616456,
76.3197884163919));
#202127=CARTESIAN_POINT('Ctrl Pts',(2.71397759435665,-6.19892043966771,
76.3285381350082));
#202128=CARTESIAN_POINT('Ctrl Pts',(2.88437226558232,-6.12431917249464,
76.3372877727769));
#202129=CARTESIAN_POINT('Ctrl Pts',(3.05168912681062,-6.04268832278745,
76.3460374105456));
#202130=CARTESIAN_POINT('Ctrl Pts',(3.21535986273959,-5.95430516123277,
76.3547870483143));
#202131=CARTESIAN_POINT('Ctrl Pts',(3.37902914072956,-5.86592278697375,
76.3635366081434));
#202132=CARTESIAN_POINT('Ctrl Pts',(3.53905210621695,-5.77078835741867,
76.3722861679725));
#202133=CARTESIAN_POINT('Ctrl Pts',(3.69488522831828,-5.66922500431544,
76.3810357278016));
#202134=CARTESIAN_POINT('Ctrl Pts',(3.85071701407078,-5.56766252216998,
76.3897852125987));
#202135=CARTESIAN_POINT('Ctrl Pts',(4.00235878822549,-5.45967138329264,
76.3985346973958));
#202136=CARTESIAN_POINT('Ctrl Pts',(4.14929549611476,-5.3456183819949,76.4072841821929));
#202137=CARTESIAN_POINT('Ctrl Pts',(4.29623099276238,-5.23156632086894,
76.4160335948655));
#202138=CARTESIAN_POINT('Ctrl Pts',(4.43846127436172,-5.11145267304839,
76.4247830075381));
#202139=CARTESIAN_POINT('Ctrl Pts',(4.57550326054583,-4.98568540049755,
76.4335324202107));
#202140=CARTESIAN_POINT('Ctrl Pts',(4.71254416257915,-4.8599191229023,76.4422817636659));
#202141=CARTESIAN_POINT('Ctrl Pts',(4.84439664018889,-4.72849950385288,
76.4510311071212));
#202142=CARTESIAN_POINT('Ctrl Pts',(4.97061286794866,-4.59187289860937,
76.4597804505764));
#202143=CARTESIAN_POINT('Ctrl Pts',(5.096828139128,-4.45524732884553,76.4685297277212));
#202144=CARTESIAN_POINT('Ctrl Pts',(5.21740705147949,-4.31341506235654,
76.4772790048661));
#202145=CARTESIAN_POINT('Ctrl Pts',(5.33194007545801,-4.1668578127559,76.4860282820109));
#202146=CARTESIAN_POINT('Ctrl Pts',(5.44647226944581,-4.02030162521712,
76.494777495752));
#202147=CARTESIAN_POINT('Ctrl Pts',(5.554958486282,-3.86902074887809,76.5035267094931));
#202148=CARTESIAN_POINT('Ctrl Pts',(5.65703027291867,-3.71352898080543,
76.5122759232343));
#202149=CARTESIAN_POINT('Ctrl Pts',(5.75910135377071,-3.55803828789468,
76.5210250764781));
#202150=CARTESIAN_POINT('Ctrl Pts',(5.85475793592822,-3.39833700106593,
76.529774229722));
#202151=CARTESIAN_POINT('Ctrl Pts',(5.94367514427463,-3.23496750823435,
76.5385233829659));
#202152=CARTESIAN_POINT('Ctrl Pts',(6.032591767327,-3.07159909077607,76.5472724786188));
#202153=CARTESIAN_POINT('Ctrl Pts',(6.11476896835979,-2.90456276731318,
76.5560215742717));
#202154=CARTESIAN_POINT('Ctrl Pts',(6.18992765547937,-2.73442583002935,
76.5647706699247));
#202155=CARTESIAN_POINT('Ctrl Pts',(6.26508587283102,-2.56428995616053,
76.5735197108927));
#202156=CARTESIAN_POINT('Ctrl Pts',(6.33322554827205,-2.39105376935083,
76.5822687518607));
#202157=CARTESIAN_POINT('Ctrl Pts',(6.39411526733072,-2.21530561053959,
76.5910177928288));
#202158=CARTESIAN_POINT('Ctrl Pts',(6.45500462602877,-2.03955849185003,
76.5997667820178));
#202159=CARTESIAN_POINT('Ctrl Pts',(6.50864402040759,-1.86129970164475,
76.6085157712068));
#202160=CARTESIAN_POINT('Ctrl Pts',(6.55485128368612,-1.68113463136017,
76.6172647603958));
#202161=CARTESIAN_POINT('Ctrl Pts',(6.60199809554333,-1.49730620116842,
76.6261916458672));
#202162=CARTESIAN_POINT('Ctrl Pts',(6.64140720707875,-1.31149343245686,
76.6351185313387));
#202163=CARTESIAN_POINT('Ctrl Pts',(6.67293928722883,-1.12435326697529,
76.6440454168101));
#202164=CARTESIAN_POINT('Ctrl Pts',(6.70384625876256,-0.940923067006646,
76.6527953309876));
#202165=CARTESIAN_POINT('Ctrl Pts',(6.72718554579795,-0.756217899521745,
76.661545245165));
#202166=CARTESIAN_POINT('Ctrl Pts',(6.74287786815327,-0.570865181254601,
76.6702951593425));
#202167=CARTESIAN_POINT('Ctrl Pts',(6.75856988190845,-0.385516108074057,
76.679044901447));
#202168=CARTESIAN_POINT('Ctrl Pts',(6.76661520773403,-0.199519795226464,
76.6877946435515));
#202169=CARTESIAN_POINT('Ctrl Pts',(6.76698651789579,-0.0135080204557706,
76.696544385656));
#202170=CARTESIAN_POINT('Ctrl Pts',(6.76735782124903,0.172500343512832,
76.7052939673209));
#202171=CARTESIAN_POINT('Ctrl Pts',(6.76005538995184,0.358523882210785,
76.7140435489859));
#202172=CARTESIAN_POINT('Ctrl Pts',(6.74510402742362,0.543930748564235,
76.7227931306508));
#202173=CARTESIAN_POINT('Ctrl Pts',(6.73015291918033,0.729334461615028,
76.7315425635075));
#202174=CARTESIAN_POINT('Ctrl Pts',(6.70755316306598,0.914121237634409,
76.7402919963642));
#202175=CARTESIAN_POINT('Ctrl Pts',(6.6773815187458,1.09766345166088,76.7490414292209));
#202176=CARTESIAN_POINT('Ctrl Pts',(6.64721034747576,1.28120278799631,76.7577907248984));
#202177=CARTESIAN_POINT('Ctrl Pts',(6.60946757205149,1.46349731860296,76.7665400205759));
#202178=CARTESIAN_POINT('Ctrl Pts',(6.56428138111531,1.64392790278129,76.7752893162535));
#202179=CARTESIAN_POINT('Ctrl Pts',(6.51909583859862,1.82435589779013,76.7840384863791));
#202180=CARTESIAN_POINT('Ctrl Pts',(6.46646716392891,2.00291972192213,76.7927876565046));
#202181=CARTESIAN_POINT('Ctrl Pts',(6.40657409872904,2.17901292274602,76.8015368266302));
#202182=CARTESIAN_POINT('Ctrl Pts',(6.34668181342102,2.35510383058908,76.8102858828293));
#202183=CARTESIAN_POINT('Ctrl Pts',(6.27952541914081,2.52872390822504,76.8190349390285));
#202184=CARTESIAN_POINT('Ctrl Pts',(6.20533299175553,2.69928350890202,76.8277839952276));
#202185=CARTESIAN_POINT('Ctrl Pts',(6.12831602991583,2.87633637965551,76.8368661313858));
#202186=CARTESIAN_POINT('Ctrl Pts',(6.04371690605302,3.05009086601399,76.845948267544));
#202187=CARTESIAN_POINT('Ctrl Pts',(5.9518452031666,3.21991112882681,76.8550304037022));
#202188=CARTESIAN_POINT('Ctrl Pts',(5.86333549509303,3.38351691182968,76.8637801840457));
#202189=CARTESIAN_POINT('Ctrl Pts',(5.76807618099397,3.54347103711958,76.8725299643893));
#202190=CARTESIAN_POINT('Ctrl Pts',(5.66639083309043,3.69923018027653,76.8812797447329));
#202191=CARTESIAN_POINT('Ctrl Pts',(5.56470914082226,3.85498372382014,76.8900292105178));
#202192=CARTESIAN_POINT('Ctrl Pts',(5.4566020337209,4.00654234701967,76.8987786763027));
#202193=CARTESIAN_POINT('Ctrl Pts',(5.34243669839236,4.15339127986643,76.9075281420876));
#202194=CARTESIAN_POINT('Ctrl Pts',(5.22827486050614,4.30023571401251,76.9162773398336));
#202195=CARTESIAN_POINT('Ctrl Pts',(5.10805534167137,4.4423705202844,76.9250265375796));
#202196=CARTESIAN_POINT('Ctrl Pts',(4.9821864433998,4.57931296628689,76.9337757353256));
#202197=CARTESIAN_POINT('Ctrl Pts',(4.85632073219606,4.71625194483342,76.9425247115373));
#202198=CARTESIAN_POINT('Ctrl Pts',(4.72480612170326,4.84799861524501,76.9512736877489));
#202199=CARTESIAN_POINT('Ctrl Pts',(4.58808925235307,4.97410554898489,76.9600226639606));
#202200=CARTESIAN_POINT('Ctrl Pts',(4.45136349474047,5.10022068121208,76.9687722089623));
#202201=CARTESIAN_POINT('Ctrl Pts',(4.30943501210082,5.22069514871833,76.977521753964));
#202202=CARTESIAN_POINT('Ctrl Pts',(4.16278587431787,5.33511975166253,76.9862712989657));
#202203=CARTESIAN_POINT('Ctrl Pts',(4.01614535740453,5.44953762807839,76.9950203296194));
#202204=CARTESIAN_POINT('Ctrl Pts',(3.86478496657928,5.5579061753278,77.0037693602731));
#202205=CARTESIAN_POINT('Ctrl Pts',(3.70921874747201,5.65985735539353,77.0125183909269));
#202206=CARTESIAN_POINT('Ctrl Pts',(3.55365041605916,5.76180991977037,77.0212675403765));
#202207=CARTESIAN_POINT('Ctrl Pts',(3.39387638174548,5.85734478552798,77.0300166898261));
#202208=CARTESIAN_POINT('Ctrl Pts',(3.23043927904575,5.94613749121212,77.0387658392757));
#202209=CARTESIAN_POINT('Ctrl Pts',(3.1869176707045,5.96978206944137,77.0410956471919));
#202210=CARTESIAN_POINT('Ctrl Pts',(3.14313645919633,5.99294880633424,77.043425455108));
#202211=CARTESIAN_POINT('Ctrl Pts',(3.09910619832125,6.01563211736945,77.0457552630242));
#202212=CARTESIAN_POINT('Ctrl Pts',(3.09910619832135,6.0156321173694,75.0457552630242));
#202213=CARTESIAN_POINT('Ctrl Pts',(2.93375330764827,6.10081787314653,75.0545047109265));
#202214=CARTESIAN_POINT('Ctrl Pts',(2.76488627843071,6.17918207037039,75.0632541588288));
#202215=CARTESIAN_POINT('Ctrl Pts',(2.59307866646703,6.25045854553997,75.0720036067311));
#202216=CARTESIAN_POINT('Ctrl Pts',(2.42127244185378,6.32173444515037,75.0807529839814));
#202217=CARTESIAN_POINT('Ctrl Pts',(2.24652594672467,6.38592262741837,75.0895023612317));
#202218=CARTESIAN_POINT('Ctrl Pts',(2.06943269687124,6.44280508110561,75.098251738482));
#202219=CARTESIAN_POINT('Ctrl Pts',(1.89234081822075,6.49968709436167,75.1070010479874));
#202220=CARTESIAN_POINT('Ctrl Pts',(1.7129024940558,6.54926340459547,75.1157503574927));
#202221=CARTESIAN_POINT('Ctrl Pts',(1.53172716625045,6.59136563150387,75.1244996669981));
#202222=CARTESIAN_POINT('Ctrl Pts',(1.35055318107325,6.63346754640712,75.1332489116653));
#202223=CARTESIAN_POINT('Ctrl Pts',(1.16764249714415,6.66809542395777,75.1419981563325));
#202224=CARTESIAN_POINT('Ctrl Pts',(0.983616340614355,6.69513165624668,
75.1507474009998));
#202225=CARTESIAN_POINT('Ctrl Pts',(0.799591486713841,6.72216769715961,
75.1594965837355));
#202226=CARTESIAN_POINT('Ctrl Pts',(0.614451459526713,6.74161215869371,
75.1682457664712));
#202227=CARTESIAN_POINT('Ctrl Pts',(0.428825047910284,6.75339900185712,
75.1769949492069));
#202228=CARTESIAN_POINT('Ctrl Pts',(0.24319988859702,6.76518576550221,75.1857440729174));
#202229=CARTESIAN_POINT('Ctrl Pts',(0.0570886373918631,6.76931499599834,
75.194493196628));
#202230=CARTESIAN_POINT('Ctrl Pts',(-0.128876626811231,6.76577266947847,
75.2032423203385));
#202231=CARTESIAN_POINT('Ctrl Pts',(-0.314840698188245,6.76223036567993,
75.21199138793));
#202232=CARTESIAN_POINT('Ctrl Pts',(-0.500658497951343,6.75101660879222,
75.2207404555216));
#202233=CARTESIAN_POINT('Ctrl Pts',(-0.685698951926312,6.73216948296217,
75.2294895231131));
#202234=CARTESIAN_POINT('Ctrl Pts',(-0.870738280459918,6.71332247176292,
75.2382385374916));
#202235=CARTESIAN_POINT('Ctrl Pts',(-1.05499998761255,6.68684221356186,
75.2469875518701));
#202236=CARTESIAN_POINT('Ctrl Pts',(-1.23785829161421,6.65281863948522,
75.2557365662487));
#202237=CARTESIAN_POINT('Ctrl Pts',(-1.43007412916014,6.6170539536912,75.2649332999472));
#202238=CARTESIAN_POINT('Ctrl Pts',(-1.62073882533034,6.57295372728428,
75.2741300336457));
#202239=CARTESIAN_POINT('Ctrl Pts',(-1.80913696087426,6.52068343479414,
75.2833267673442));
#202240=CARTESIAN_POINT('Ctrl Pts',(-1.98838356182049,6.47095219816447,
75.2920767650579));
#202241=CARTESIAN_POINT('Ctrl Pts',(-2.165578275685,6.41382586852252,75.3008267627716));
#202242=CARTESIAN_POINT('Ctrl Pts',(-2.34011918617701,6.34949849944751,
75.3095767604853));
#202243=CARTESIAN_POINT('Ctrl Pts',(-2.5146565568714,6.28517243497134,75.3183265807436));
#202244=CARTESIAN_POINT('Ctrl Pts',(-2.68653996291414,6.21364572244067,
75.3270764010019));
#202245=CARTESIAN_POINT('Ctrl Pts',(-2.85518555376123,6.1351613225402,75.3358262212602));
#202246=CARTESIAN_POINT('Ctrl Pts',(-3.02382794854874,6.05667841002411,
75.3445758756977));
#202247=CARTESIAN_POINT('Ctrl Pts',(-3.18923239105522,5.97123819494089,
75.3533255301352));
#202248=CARTESIAN_POINT('Ctrl Pts',(-3.35083705963998,5.87913088812822,
75.3620751845727));
#202249=CARTESIAN_POINT('Ctrl Pts',(-3.51243888038759,5.78702520445313,
75.3708246848217));
#202250=CARTESIAN_POINT('Ctrl Pts',(-3.67024081220112,5.68825280608092,
75.3795741850706));
#202251=CARTESIAN_POINT('Ctrl Pts',(-3.8237068754089,5.58314917684909,75.3883236853195));
#202252=CARTESIAN_POINT('Ctrl Pts',(-3.97717043814377,5.47804726010517,
75.39707304301));
#202253=CARTESIAN_POINT('Ctrl Pts',(-4.12629803719099,5.3666144808682,75.4058224007005));
#202254=CARTESIAN_POINT('Ctrl Pts',(-4.27058317203627,5.24922931207246,
75.414571758391));
#202255=CARTESIAN_POINT('Ctrl Pts',(-4.41486614771621,5.13184589989555,
75.423320985151));
#202256=CARTESIAN_POINT('Ctrl Pts',(-4.55430658191271,5.00851045725891,
75.4320702119111));
#202257=CARTESIAN_POINT('Ctrl Pts',(-4.68843088998778,4.87964187106066,
75.4408194386712));
#202258=CARTESIAN_POINT('Ctrl Pts',(-4.82255336914844,4.75077504210998,
75.4495685461271));
#202259=CARTESIAN_POINT('Ctrl Pts',(-4.9513596606222,4.61637541911219,75.458317653583));
#202260=CARTESIAN_POINT('Ctrl Pts',(-5.07441230866412,4.47689945405055,
75.4670667610389));
#202261=CARTESIAN_POINT('Ctrl Pts',(-5.19746344223641,4.3374252055884,75.4758157608153));
#202262=CARTESIAN_POINT('Ctrl Pts',(-5.31476088452053,4.19287495494774,
75.4845647605916));
#202263=CARTESIAN_POINT('Ctrl Pts',(-5.42590627626208,4.04373961590256,
75.493313760368));
#202264=CARTESIAN_POINT('Ctrl Pts',(-5.53706380670121,3.89458798910355,
75.5020637156627));
#202265=CARTESIAN_POINT('Ctrl Pts',(-5.64206777069419,3.74085050158971,
75.5108136709573));
#202266=CARTESIAN_POINT('Ctrl Pts',(-5.74056148161667,3.5830493822691,75.5195636262521));
#202267=CARTESIAN_POINT('Ctrl Pts',(-5.83905138949643,3.42525435597101,
75.5283132436932));
#202268=CARTESIAN_POINT('Ctrl Pts',(-5.93103139555515,3.26339625501068,
75.5370628611343));
#202269=CARTESIAN_POINT('Ctrl Pts',(-6.01618907818814,3.09802485068951,
75.5458124785754));
#202270=CARTESIAN_POINT('Ctrl Pts',(-6.10134392543066,2.9326589525363,75.5545618046913));
#202271=CARTESIAN_POINT('Ctrl Pts',(-6.1796767726003,2.76378023990064,75.5633111308071));
#202272=CARTESIAN_POINT('Ctrl Pts',(-6.25092157007539,2.59196229231179,
75.572060456923));
#202273=CARTESIAN_POINT('Ctrl Pts',(-6.32216437406182,2.42014915233196,
75.5808095382255));
#202274=CARTESIAN_POINT('Ctrl Pts',(-6.38631941547465,2.24539720666993,
75.5895586195279));
#202275=CARTESIAN_POINT('Ctrl Pts',(-6.44316881036197,2.06829994951861,
75.5983077008304));
#202276=CARTESIAN_POINT('Ctrl Pts',(-6.50002334523345,1.89118668028667,
75.6070575731727));
#202277=CARTESIAN_POINT('Ctrl Pts',(-6.54957082409984,1.71172794811957,
75.6158074455151));
#202278=CARTESIAN_POINT('Ctrl Pts',(-6.59164294295088,1.53053334254628,
75.6245573178574));
#202279=CARTESIAN_POINT('Ctrl Pts',(-6.63371214081254,1.34935131697926,
75.6333065827123));
#202280=CARTESIAN_POINT('Ctrl Pts',(-6.66830695238927,1.16643393834124,
75.6420558475672));
#202281=CARTESIAN_POINT('Ctrl Pts',(-6.69530988153344,0.982402458384889,
75.6508051124221));
#202282=CARTESIAN_POINT('Ctrl Pts',(-6.72231419689959,0.798361530991149,
75.6595548264291));
#202283=CARTESIAN_POINT('Ctrl Pts',(-6.74172580828875,0.61320667140671,
75.6683045404362));
#202284=CARTESIAN_POINT('Ctrl Pts',(-6.75347878027899,0.427566795157723,
75.6770542544432));
#202285=CARTESIAN_POINT('Ctrl Pts',(-6.76248992366693,0.285234494460517,
75.6837627642215));
#202286=CARTESIAN_POINT('Ctrl Pts',(-6.76699999998568,0.142617266559108,
75.6904712739998));
#202287=CARTESIAN_POINT('Ctrl Pts',(-6.767,6.79698250989073E-10,75.6971797837782));
#202288=CARTESIAN_POINT('',(-6.76699840339575,-0.00267271979378576,75.3028202161898));
#202289=CARTESIAN_POINT('Ctrl Pts',(3.09910619832131,6.01563211736942,74.651395695404));
#202290=CARTESIAN_POINT('Ctrl Pts',(2.93375330764829,6.10081787314652,74.6601451433063));
#202291=CARTESIAN_POINT('Ctrl Pts',(2.76488627843079,6.17918207037035,74.6688945912086));
#202292=CARTESIAN_POINT('Ctrl Pts',(2.59307866646717,6.25045854553991,74.6776440391109));
#202293=CARTESIAN_POINT('Ctrl Pts',(2.42127244185392,6.32173444515031,74.6863934163612));
#202294=CARTESIAN_POINT('Ctrl Pts',(2.24652594672481,6.38592262741832,74.6951427936115));
#202295=CARTESIAN_POINT('Ctrl Pts',(2.06943269687138,6.44280508110556,74.7038921708618));
#202296=CARTESIAN_POINT('Ctrl Pts',(1.89234081822095,6.49968709436161,74.7126414803672));
#202297=CARTESIAN_POINT('Ctrl Pts',(1.71290249405607,6.5492634045954,74.7213907898725));
#202298=CARTESIAN_POINT('Ctrl Pts',(1.53172716625078,6.59136563150379,74.7301400993779));
#202299=CARTESIAN_POINT('Ctrl Pts',(1.35055318107365,6.63346754640703,74.7388893440451));
#202300=CARTESIAN_POINT('Ctrl Pts',(1.16764249714461,6.66809542395768,74.7476385887124));
#202301=CARTESIAN_POINT('Ctrl Pts',(0.983616340614882,6.6951316562466,74.7563878333796));
#202302=CARTESIAN_POINT('Ctrl Pts',(0.799591486714308,6.72216769715955,
74.7651370161153));
#202303=CARTESIAN_POINT('Ctrl Pts',(0.614451459527118,6.74161215869367,
74.773886198851));
#202304=CARTESIAN_POINT('Ctrl Pts',(0.428825047910626,6.7533990018571,74.7826353815867));
#202305=CARTESIAN_POINT('Ctrl Pts',(0.243199888597299,6.7651857655022,74.7913845052972));
#202306=CARTESIAN_POINT('Ctrl Pts',(0.0570886373920775,6.76931499599834,
74.8001336290077));
#202307=CARTESIAN_POINT('Ctrl Pts',(-0.12887662681108,6.76577266947847,
74.8088827527183));
#202308=CARTESIAN_POINT('Ctrl Pts',(-0.314840698188095,6.76223036567993,
74.8176318203098));
#202309=CARTESIAN_POINT('Ctrl Pts',(-0.500658497951193,6.75101660879223,
74.8263808879014));
#202310=CARTESIAN_POINT('Ctrl Pts',(-0.685698951926162,6.73216948296219,
74.8351299554929));
#202311=CARTESIAN_POINT('Ctrl Pts',(-0.870738280459833,6.71332247176294,
74.8438789698715));
#202312=CARTESIAN_POINT('Ctrl Pts',(-1.05499998761252,6.68684221356186,
74.85262798425));
#202313=CARTESIAN_POINT('Ctrl Pts',(-1.23785829161425,6.65281863948521,
74.8613769986285));
#202314=CARTESIAN_POINT('Ctrl Pts',(-1.43007412917405,6.61705395368861,
74.8705737323277));
#202315=CARTESIAN_POINT('Ctrl Pts',(-1.62073882535789,6.5729537272779,74.8797704660269));
#202316=CARTESIAN_POINT('Ctrl Pts',(-1.80913696091507,6.52068343478281,
74.8889671997261));
#202317=CARTESIAN_POINT('Ctrl Pts',(-1.98838356186106,6.47095219815201,
74.8977171974397));
#202318=CARTESIAN_POINT('Ctrl Pts',(-2.16557827572526,6.41382586850893,
74.9064671951534));
#202319=CARTESIAN_POINT('Ctrl Pts',(-2.34011918621693,6.3494984994328,74.9152171928671));
#202320=CARTESIAN_POINT('Ctrl Pts',(-2.51465655691097,6.28517243495551,
74.9239670131254));
#202321=CARTESIAN_POINT('Ctrl Pts',(-2.68653996295333,6.21364572242373,
74.9327168333837));
#202322=CARTESIAN_POINT('Ctrl Pts',(-2.85518555379998,6.13516132252217,
74.941466653642));
#202323=CARTESIAN_POINT('Ctrl Pts',(-3.023827948587,6.05667841000501,74.9502163080795));
#202324=CARTESIAN_POINT('Ctrl Pts',(-3.18923239109293,5.97123819492075,
74.958965962517));
#202325=CARTESIAN_POINT('Ctrl Pts',(-3.35083705967711,5.87913088810706,
74.9677156169545));
#202326=CARTESIAN_POINT('Ctrl Pts',(-3.51243888042414,5.78702520443095,
74.9764651172035));
#202327=CARTESIAN_POINT('Ctrl Pts',(-3.67024081223705,5.68825280605774,
74.9852146174524));
#202328=CARTESIAN_POINT('Ctrl Pts',(-3.82370687544417,5.58314917682494,
74.9939641177014));
#202329=CARTESIAN_POINT('Ctrl Pts',(-3.97717043817832,5.47804726008009,
75.0027134753918));
#202330=CARTESIAN_POINT('Ctrl Pts',(-4.12629803722479,5.36661448084222,
75.0114628330823));
#202331=CARTESIAN_POINT('Ctrl Pts',(-4.27058317206927,5.24922931204561,
75.0202121907728));
#202332=CARTESIAN_POINT('Ctrl Pts',(-4.41486614774858,5.13184589986771,
75.0289614175329));
#202333=CARTESIAN_POINT('Ctrl Pts',(-4.5543065819444,5.00851045723011,75.0377106442929));
#202334=CARTESIAN_POINT('Ctrl Pts',(-4.68843089001874,4.87964187103092,
75.046459871053));
#202335=CARTESIAN_POINT('Ctrl Pts',(-4.82255336917867,4.75077504207929,
75.0552089785089));
#202336=CARTESIAN_POINT('Ctrl Pts',(-4.95135966065167,4.61637541908059,
75.0639580859649));
#202337=CARTESIAN_POINT('Ctrl Pts',(-5.07441230869278,4.47689945401807,
75.0727071934208));
#202338=CARTESIAN_POINT('Ctrl Pts',(-5.19746344226443,4.33742520555484,
75.0814561931972));
#202339=CARTESIAN_POINT('Ctrl Pts',(-5.31476088454786,4.19287495491313,
75.0902051929735));
#202340=CARTESIAN_POINT('Ctrl Pts',(-5.42590627628866,4.0437396158669,75.0989541927499));
#202341=CARTESIAN_POINT('Ctrl Pts',(-5.53706380672681,3.89458798906716,
75.1077041480446));
#202342=CARTESIAN_POINT('Ctrl Pts',(-5.64206777071878,3.74085050155263,
75.1164541033393));
#202343=CARTESIAN_POINT('Ctrl Pts',(-5.74056148164022,3.58304938223138,
75.125204058634));
#202344=CARTESIAN_POINT('Ctrl Pts',(-5.83905138951894,3.42525435593264,
75.1339536760751));
#202345=CARTESIAN_POINT('Ctrl Pts',(-5.9310313955766,3.2633962549717,75.1427032935162));
#202346=CARTESIAN_POINT('Ctrl Pts',(-6.0161890782085,3.09802485064997,75.1514529109573));
#202347=CARTESIAN_POINT('Ctrl Pts',(-6.10134392544987,2.93265895249632,
75.1602022370732));
#202348=CARTESIAN_POINT('Ctrl Pts',(-6.17967677261836,2.76378023986026,
75.168951563189));
#202349=CARTESIAN_POINT('Ctrl Pts',(-6.25092157009228,2.59196229227106,
75.1777008893049));
#202350=CARTESIAN_POINT('Ctrl Pts',(-6.32216437407759,2.42014915229077,
75.1864499706074));
#202351=CARTESIAN_POINT('Ctrl Pts',(-6.38631941548928,2.24539720662832,
75.1951990519098));
#202352=CARTESIAN_POINT('Ctrl Pts',(-6.44316881037545,2.06829994947663,
75.2039481332122));
#202353=CARTESIAN_POINT('Ctrl Pts',(-6.50002334524579,1.89118668024426,
75.2126980055546));
#202354=CARTESIAN_POINT('Ctrl Pts',(-6.54957082411103,1.71172794807677,
75.221447877897));
#202355=CARTESIAN_POINT('Ctrl Pts',(-6.5916429429609,1.53053334250314,75.2301977502393));
#202356=CARTESIAN_POINT('Ctrl Pts',(-6.63371214082141,1.34935131693566,
75.2389470150942));
#202357=CARTESIAN_POINT('Ctrl Pts',(-6.66830695239697,1.16643393829723,
75.2476962799491));
#202358=CARTESIAN_POINT('Ctrl Pts',(-6.69530988153995,0.982402458340512,
75.256445544804));
#202359=CARTESIAN_POINT('Ctrl Pts',(-6.72231419690488,0.798361530946657,
75.265195258811));
#202360=CARTESIAN_POINT('Ctrl Pts',(-6.74172580829281,0.613206671362151,
75.2739449728181));
#202361=CARTESIAN_POINT('Ctrl Pts',(-6.75347878028181,0.42756679511315,
75.2826946868251));
#202362=CARTESIAN_POINT('Ctrl Pts',(-6.76248992368213,0.285234494205576,
75.2894031966133));
#202363=CARTESIAN_POINT('Ctrl Pts',(-6.76699999999994,0.142617266092986,
75.2961117064016));
#202364=CARTESIAN_POINT('Ctrl Pts',(-6.767,2.84793741451067E-12,75.3028202161898));
#202365=CARTESIAN_POINT('Ctrl Pts',(-6.76699517037156,-0.00808481094492364,
75.3028202161898));
#202366=CARTESIAN_POINT('Ctrl Pts',(-6.76674412400169,-0.218210883648386,
75.3126841961279));
#202367=CARTESIAN_POINT('Ctrl Pts',(-6.75670250884975,-0.427869699865752,
75.3225481760661));
#202368=CARTESIAN_POINT('Ctrl Pts',(-6.73702211524587,-0.636256252376383,
75.3324121560042));
#202369=CARTESIAN_POINT('Ctrl Pts',(-6.71715949916007,-0.846572274163036,
75.3423674673933));
#202370=CARTESIAN_POINT('Ctrl Pts',(-6.6874788848665,-1.05559238172179,
75.3523227787825));
#202371=CARTESIAN_POINT('Ctrl Pts',(-6.6481840108267,-1.26251271605013,
75.3622780901717));
#202372=CARTESIAN_POINT('Ctrl Pts',(-6.60849008442896,-1.47153439436636,
75.3723345010193));
#202373=CARTESIAN_POINT('Ctrl Pts',(-6.55898568021543,-1.67841345953767,
75.3823909118669));
#202374=CARTESIAN_POINT('Ctrl Pts',(-6.49992815531097,-1.88234507351753,
75.3924473227145));
#202375=CARTESIAN_POINT('Ctrl Pts',(-6.49169906780799,-1.91076094598729,
75.3938485850425));
#202376=CARTESIAN_POINT('Ctrl Pts',(-6.48328457375079,-1.9391196286264,
75.3952498473704));
#202377=CARTESIAN_POINT('Ctrl Pts',(-6.47468544086907,-1.96741897972905,
75.3966511096984));
#202378=CARTESIAN_POINT('Ctrl Pts',(-6.42430666958161,-2.13321320065739,
75.4048605274739));
#202379=CARTESIAN_POINT('Ctrl Pts',(-6.36747888064407,-2.29732383691437,
75.4130699452495));
#202380=CARTESIAN_POINT('Ctrl Pts',(-6.30432968657984,-2.45921048365287,
75.4212793630251));
#202381=CARTESIAN_POINT('Ctrl Pts',(-6.2412567587065,-2.62090161755726,
75.4294788661686));
#202382=CARTESIAN_POINT('Ctrl Pts',(-6.17187775572661,-2.78037377723096,
75.4376783693121));
#202383=CARTESIAN_POINT('Ctrl Pts',(-6.09637055659032,-2.93709976622154,
75.4458778724557));
#202384=CARTESIAN_POINT('Ctrl Pts',(-6.02093917221881,-3.09366839082666,
75.4540691426968));
#202385=CARTESIAN_POINT('Ctrl Pts',(-5.93939199977997,-3.24749601291137,
75.4622604129379));
#202386=CARTESIAN_POINT('Ctrl Pts',(-5.85195570584304,-3.39807348608753,
75.470451683179));
#202387=CARTESIAN_POINT('Ctrl Pts',(-5.76458940576276,-3.5485304200963,
75.4786363962049));
#202388=CARTESIAN_POINT('Ctrl Pts',(-5.67134355334986,-3.69574207647182,
75.4868211092309));
#202389=CARTESIAN_POINT('Ctrl Pts',(-5.57249165080646,-3.83922203078857,
75.4950058222568));
#202390=CARTESIAN_POINT('Ctrl Pts',(-5.47369876359507,-3.98261632648953,
75.5031856489473));
#202391=CARTESIAN_POINT('Ctrl Pts',(-5.36930669694921,-4.1222830617013,
75.5113654756377));
#202392=CARTESIAN_POINT('Ctrl Pts',(-5.25963338298041,-4.25776298972101,
75.5195453023282));
#202393=CARTESIAN_POINT('Ctrl Pts',(-5.14999231549889,-4.3932030835129,
75.5277227239607));
#202394=CARTESIAN_POINT('Ctrl Pts',(-5.03507331681905,-4.5244585393973,
75.5359001455932));
#202395=CARTESIAN_POINT('Ctrl Pts',(-4.91523602282502,-4.65110135773489,
75.5440775672257));
#202396=CARTESIAN_POINT('Ctrl Pts',(-4.79541506395904,-4.77772691327736,
75.5522538741865));
#202397=CARTESIAN_POINT('Ctrl Pts',(-4.67067739207716,-4.89974082083716,
75.5604301811474));
#202398=CARTESIAN_POINT('Ctrl Pts',(-4.54142108047619,-5.01675029972656,
75.5686064881083));
#202399=CARTESIAN_POINT('Ctrl Pts',(-4.4121585599736,-5.13376539923389,
75.5767831878228));
#202400=CARTESIAN_POINT('Ctrl Pts',(-4.27837723475216,-5.24577534900321,
75.5849598875373));
#202401=CARTESIAN_POINT('Ctrl Pts',(-4.14050999471701,-5.35242617731889,
75.5931365872518));
#202402=CARTESIAN_POINT('Ctrl Pts',(-4.00261071665158,-5.45910178949524,
75.601315187094));
#202403=CARTESIAN_POINT('Ctrl Pts',(-3.86062391808235,-5.56041557933863,
75.6094937869362));
#202404=CARTESIAN_POINT('Ctrl Pts',(-3.71501334252604,-5.65605559244722,
75.6176723867783));
#202405=CARTESIAN_POINT('Ctrl Pts',(-3.56926220338754,-5.75178793060015,
75.6258588817427));
#202406=CARTESIAN_POINT('Ctrl Pts',(-3.41988060024241,-5.84183535108088,
75.6340453767071));
#202407=CARTESIAN_POINT('Ctrl Pts',(-3.26735967916884,-5.92593028367207,
75.6422318716715));
#202408=CARTESIAN_POINT('Ctrl Pts',(-3.11476398037107,-6.01006644619835,
75.6504223802981));
#202409=CARTESIAN_POINT('Ctrl Pts',(-2.95902621751108,-6.08824414126907,
75.6586128889247));
#202410=CARTESIAN_POINT('Ctrl Pts',(-2.80065947731021,-6.1602431357985,
75.6668033975513));
#202411=CARTESIAN_POINT('Ctrl Pts',(-2.64206886595309,-6.23234390989435,
75.6750054844843));
#202412=CARTESIAN_POINT('Ctrl Pts',(-2.48084218411102,-6.29824839147717,
75.6832075714173));
#202413=CARTESIAN_POINT('Ctrl Pts',(-2.31751088050882,-6.35778517399914,
75.6914096583503));
#202414=CARTESIAN_POINT('Ctrl Pts',(-2.16384472218788,-6.41379886180526,
75.6991263860162));
#202415=CARTESIAN_POINT('Ctrl Pts',(-2.00831603636468,-6.46417655449741,
75.706843113682));
#202416=CARTESIAN_POINT('Ctrl Pts',(-1.85137628097049,-6.50881670246289,
75.7145598413479));
#202417=CARTESIAN_POINT('Ctrl Pts',(-1.67084417500735,-6.56016748928215,
75.7234366048752));
#202418=CARTESIAN_POINT('Ctrl Pts',(-1.4880440107246,-6.60404021423144,
75.7323133684024));
#202419=CARTESIAN_POINT('Ctrl Pts',(-1.30359371124132,-6.64025093170522,
75.7411901319297));
#202420=CARTESIAN_POINT('Ctrl Pts',(-1.11942465968586,-6.67640643544781,
75.7500533602588));
#202421=CARTESIAN_POINT('Ctrl Pts',(-0.933610755225823,-6.70492318822488,
75.758916588588));
#202422=CARTESIAN_POINT('Ctrl Pts',(-0.746782833147205,-6.72566758025675,
75.7677798169171));
#202423=CARTESIAN_POINT('Ctrl Pts',(-0.56040117232329,-6.74636242178078,
75.7766218743455));
#202424=CARTESIAN_POINT('Ctrl Pts',(-0.373010593702273,-6.7593219234436,
75.7854639317739));
#202425=CARTESIAN_POINT('Ctrl Pts',(-0.185249234690844,-6.76446389014285,
75.7943059892023));
#202426=CARTESIAN_POINT('Ctrl Pts',(0.00223489196362983,-6.76959826465404,
75.8031349912053));
#202427=CARTESIAN_POINT('Ctrl Pts',(0.190088440290167,-6.76693811895071,
75.8119639932082));
#202428=CARTESIAN_POINT('Ctrl Pts',(0.377668239005517,-6.75645289343798,
75.8207929952111));
#202429=CARTESIAN_POINT('Ctrl Pts',(0.564800489672221,-6.74599268470344,
75.829600932032));
#202430=CARTESIAN_POINT('Ctrl Pts',(0.751660027069486,-6.72774466541701,
75.8384088688529));
#202431=CARTESIAN_POINT('Ctrl Pts',(0.937604438106017,-6.70173014360053,
75.8472168056738));
#202432=CARTESIAN_POINT('Ctrl Pts',(1.1226593089935,-6.67584007275025,75.8559826061734));
#202433=CARTESIAN_POINT('Ctrl Pts',(1.30680752142655,-6.64225764464012,
75.864748406673));
#202434=CARTESIAN_POINT('Ctrl Pts',(1.48941603416143,-6.60105513362696,
75.8735142071727));
#202435=CARTESIAN_POINT('Ctrl Pts',(1.66120466573386,-6.56229394512435,
75.8817606183061));
#202436=CARTESIAN_POINT('Ctrl Pts',(1.83145444700487,-6.51682806607553,
75.8900070294395));
#202437=CARTESIAN_POINT('Ctrl Pts',(1.9996179046617,-6.46481378195508,75.8982534405729));
#202438=CARTESIAN_POINT('Ctrl Pts',(2.16783559744715,-6.41278272248148,
75.9065025112922));
#202439=CARTESIAN_POINT('Ctrl Pts',(2.33396528980005,-6.35419915322431,
75.9147515820116));
#202440=CARTESIAN_POINT('Ctrl Pts',(2.49747641154605,-6.28926868354112,
75.9230006527309));
#202441=CARTESIAN_POINT('Ctrl Pts',(2.66106837863366,-6.2243061100723,75.9312538020654));
#202442=CARTESIAN_POINT('Ctrl Pts',(2.82203886860477,-6.15299051241487,
75.9395069513999));
#202443=CARTESIAN_POINT('Ctrl Pts',(2.97987883364944,-6.07557496347202,
75.9477601007344));
#202444=CARTESIAN_POINT('Ctrl Pts',(3.13791136499413,-5.99806496680284,
75.9560233189918));
#202445=CARTESIAN_POINT('Ctrl Pts',(3.292805426646,-5.91444030848025,75.9642865372491));
#202446=CARTESIAN_POINT('Ctrl Pts',(3.44407711282112,-5.8249997288362,75.9725497555064));
#202447=CARTESIAN_POINT('Ctrl Pts',(3.59545431035029,-5.73549676477041,
75.9808187373232));
#202448=CARTESIAN_POINT('Ctrl Pts',(3.74320380036393,-5.6401699817092,75.9890877191399));
#202449=CARTESIAN_POINT('Ctrl Pts',(3.88687203736883,-5.53936050145866,
75.9973567009567));
#202450=CARTESIAN_POINT('Ctrl Pts',(4.03074592888161,-5.43840671704957,
76.0056375194426));
#202451=CARTESIAN_POINT('Ctrl Pts',(4.17052661860345,-5.3319547707308,76.0139183379284));
#202452=CARTESIAN_POINT('Ctrl Pts',(4.30579407760629,-5.22038565254049,
76.0221991564143));
#202453=CARTESIAN_POINT('Ctrl Pts',(4.36171117038323,-5.17426502028438,
76.0256222952753));
#202454=CARTESIAN_POINT('Ctrl Pts',(4.41685746241446,-5.12727037495087,
76.0290454341363));
#202455=CARTESIAN_POINT('Ctrl Pts',(4.47120520070793,-5.07943038668338,
76.0324685729973));
#202456=CARTESIAN_POINT('Ctrl Pts',(4.60511039071803,-4.9615593782442,76.0409027061187));
#202457=CARTESIAN_POINT('Ctrl Pts',(4.73447418182554,-4.83828225145958,
76.0493368392401));
#202458=CARTESIAN_POINT('Ctrl Pts',(4.8588497279284,-4.70997540560565,76.0577709723616));
#202459=CARTESIAN_POINT('Ctrl Pts',(4.98310726230948,-4.58179030162358,
76.0661971028924));
#202460=CARTESIAN_POINT('Ctrl Pts',(5.10238575313522,-4.44858523015409,
76.0746232334233));
#202461=CARTESIAN_POINT('Ctrl Pts',(5.21627314881857,-4.31077527098252,
76.0830493639542));
#202462=CARTESIAN_POINT('Ctrl Pts',(5.33007048663557,-4.17307428674017,
76.0914688314181));
#202463=CARTESIAN_POINT('Ctrl Pts',(5.438485014381,-4.03077593088117,76.0998882988821));
#202464=CARTESIAN_POINT('Ctrl Pts',(5.54114287740415,-3.88433065175885,
76.1083077663461));
#202465=CARTESIAN_POINT('Ctrl Pts',(5.64373576883996,-3.7379780570346,76.1167219051761));
#202466=CARTESIAN_POINT('Ctrl Pts',(5.7405790669913,-3.58748404522176,76.1251360440062));
#202467=CARTESIAN_POINT('Ctrl Pts',(5.83134019552794,-3.43333082064927,
76.1335501828363));
#202468=CARTESIAN_POINT('Ctrl Pts',(5.92205819511733,-3.2792508484305,76.1419603233363));
#202469=CARTESIAN_POINT('Ctrl Pts',(6.00669961796768,-3.1215154188964,76.1503704638363));
#202470=CARTESIAN_POINT('Ctrl Pts',(6.08497590004447,-2.96063461032902,
76.1587806043364));
#202471=CARTESIAN_POINT('Ctrl Pts',(6.16323324838128,-2.79979271617243,
76.1671887105623));
#202472=CARTESIAN_POINT('Ctrl Pts',(6.23512837671761,-2.63580725995374,
76.1755968167882));
#202473=CARTESIAN_POINT('Ctrl Pts',(6.30041904326799,-2.46921219809601,
76.1840049230141));
#202474=CARTESIAN_POINT('Ctrl Pts',(6.36570165658729,-2.30263768478833,
76.1924119921481));
#202475=CARTESIAN_POINT('Ctrl Pts',(6.42438130965619,-2.13345451955307,
76.2008190612821));
#202476=CARTESIAN_POINT('Ctrl Pts',(6.47626410273575,-1.96221616332564,
76.2092261304161));
#202477=CARTESIAN_POINT('Ctrl Pts',(6.5281479297892,-1.79097439448334,76.2176333670949));
#202478=CARTESIAN_POINT('Ctrl Pts',(6.57323452992889,-1.61767767396493,
76.2260406037737));
#202479=CARTESIAN_POINT('Ctrl Pts',(6.61137992921407,-1.44289446307947,
76.2344478404524));
#202480=CARTESIAN_POINT('Ctrl Pts',(6.6495315541235,-1.26808272622187,76.2428564492572));
#202481=CARTESIAN_POINT('Ctrl Pts',(6.68073964883631,-1.0917843429905,76.251265058062));
#202482=CARTESIAN_POINT('Ctrl Pts',(6.70491132087542,-0.914578142750349,
76.2596736668669));
#202483=CARTESIAN_POINT('Ctrl Pts',(6.72909954479188,-0.737250598182512,
76.2680880335796));
#202484=CARTESIAN_POINT('Ctrl Pts',(6.74624167263049,-0.559014326970189,
76.2765024002923));
#202485=CARTESIAN_POINT('Ctrl Pts',(6.75629657398825,-0.380454470751356,
76.2849167670051));
#202486=CARTESIAN_POINT('Ctrl Pts',(6.7663551044929,-0.201830166366891,
76.2933341707414));
#202487=CARTESIAN_POINT('Ctrl Pts',(6.76932129565298,-0.0228823791739918,
76.3017515744777));
#202488=CARTESIAN_POINT('Ctrl Pts',(6.76520616228446,0.155803022397947,
76.3101689782141));
#202489=CARTESIAN_POINT('Ctrl Pts',(6.7610871303496,0.334657705699289,76.3185943563717));
#202490=CARTESIAN_POINT('Ctrl Pts',(6.7498733840753,0.513249171542303,76.3270197345293));
#202491=CARTESIAN_POINT('Ctrl Pts',(6.73162797166826,0.690994827081569,
76.3354451126868));
#202492=CARTESIAN_POINT('Ctrl Pts',(6.72084926653247,0.796000291879156,
76.3404225100069));
#202493=CARTESIAN_POINT('Ctrl Pts',(6.70761749134104,0.900710687160406,
76.345399907327));
#202494=CARTESIAN_POINT('Ctrl Pts',(6.6919540555666,1.00500742195553,76.350377304647));
#202495=CARTESIAN_POINT('Ctrl Pts',(6.66630198399042,1.17581460274618,76.3585288081968));
#202496=CARTESIAN_POINT('Ctrl Pts',(6.6340736292976,1.34585493051098,76.3666803117466));
#202497=CARTESIAN_POINT('Ctrl Pts',(6.59532689361421,1.51457986463876,76.3748318152964));
#202498=CARTESIAN_POINT('Ctrl Pts',(6.55661414630117,1.68315679441345,76.3829761684032));
#202499=CARTESIAN_POINT('Ctrl Pts',(6.51139448118651,1.85042027404336,76.3911205215101));
#202500=CARTESIAN_POINT('Ctrl Pts',(6.45977736301567,2.01582871798928,76.399264874617));
#202501=CARTESIAN_POINT('Ctrl Pts',(6.40819573438519,2.18112343474826,76.4074036280438));
#202502=CARTESIAN_POINT('Ctrl Pts',(6.35022551883061,2.34456530823284,76.4155423814706));
#202503=CARTESIAN_POINT('Ctrl Pts',(6.28602684114741,2.50562478283846,76.4236811348974));
#202504=CARTESIAN_POINT('Ctrl Pts',(6.22185949988904,2.6666056416797,76.4318159156655));
#202505=CARTESIAN_POINT('Ctrl Pts',(6.15146988600607,2.82520607917462,76.4399506964336));
#202506=CARTESIAN_POINT('Ctrl Pts',(6.07506737664011,2.98091351254663,76.4480854772017));
#202507=CARTESIAN_POINT('Ctrl Pts',(5.9986867476782,3.13657635390741,76.4562179283043));
#202508=CARTESIAN_POINT('Ctrl Pts',(5.91629681453725,3.28934751432502,76.4643503794069));
#202509=CARTESIAN_POINT('Ctrl Pts',(5.8281543087654,3.43873615638351,76.4724828305095));
#202510=CARTESIAN_POINT('Ctrl Pts',(5.74000821130039,3.58813088583606,76.480615612999));
#202511=CARTESIAN_POINT('Ctrl Pts',(5.64610925481213,3.73414250504625,76.4887483954885));
#202512=CARTESIAN_POINT('Ctrl Pts',(5.54675927222819,3.87630630574399,76.4968811779779));
#202513=CARTESIAN_POINT('Ctrl Pts',(5.49606091185689,3.94885258519037,76.5010313421425));
#202514=CARTESIAN_POINT('Ctrl Pts',(5.44394377425027,4.02039731685149,76.5051815063071));
#202515=CARTESIAN_POINT('Ctrl Pts',(5.39045223894833,4.09088177042762,76.5093316704717));
#202516=CARTESIAN_POINT('Ctrl Pts',(5.2747518899463,4.24333721654526,76.5183083326585));
#202517=CARTESIAN_POINT('Ctrl Pts',(5.15267820629121,4.39075272790816,76.5272849948453));
#202518=CARTESIAN_POINT('Ctrl Pts',(5.02468706398398,4.53263818421811,76.5362616570321));
#202519=CARTESIAN_POINT('Ctrl Pts',(4.89647541171931,4.67476808834974,76.5452537846907));
#202520=CARTESIAN_POINT('Ctrl Pts',(4.76232608452548,4.81134871614229,76.5542459123493));
#202521=CARTESIAN_POINT('Ctrl Pts',(4.62273175352707,4.94192676341248,76.5632380400078));
#202522=CARTESIAN_POINT('Ctrl Pts',(4.48282650171009,5.07279564937973,76.5722501959847));
#202523=CARTESIAN_POINT('Ctrl Pts',(4.33745215952732,5.19763504337567,76.5812623519615));
#202524=CARTESIAN_POINT('Ctrl Pts',(4.18713634973639,5.31603030359273,76.5902745079383));
#202525=CARTESIAN_POINT('Ctrl Pts',(4.03666276173279,5.43454983678262,76.5992961234781));
#202526=CARTESIAN_POINT('Ctrl Pts',(3.88123753537951,5.54661157850362,76.6083177390179));
#202527=CARTESIAN_POINT('Ctrl Pts',(3.72141859327451,5.65184329698115,76.6173393545577));
#202528=CARTESIAN_POINT('Ctrl Pts',(3.56139431352945,5.75721021866079,76.6263725611969));
#202529=CARTESIAN_POINT('Ctrl Pts',(3.39696523344041,5.85572944270786,76.6354057678361));
#202530=CARTESIAN_POINT('Ctrl Pts',(3.22871696210916,5.94707287483419,76.6444389744753));
#202531=CARTESIAN_POINT('Ctrl Pts',(3.18575890182591,5.97039517486565,76.6467453817405));
#202532=CARTESIAN_POINT('Ctrl Pts',(3.14255198469688,5.99324991326842,76.6490517890057));
#202533=CARTESIAN_POINT('Ctrl Pts',(3.09910619832139,6.01563211736937,76.6513581962709));
#202534=CARTESIAN_POINT('Origin',(0.,0.,4.30282021618968));
#202535=CARTESIAN_POINT('',(3.09910619832139,6.01563211736937,79.0457552630242));
#202536=CARTESIAN_POINT('',(3.09910619832128,6.01563211736943,78.6515182808518));
#202537=CARTESIAN_POINT('',(3.09910619832133,6.0156321173694,4.30282021618968));
#202538=CARTESIAN_POINT('',(-6.767,9.59489064569771E-10,77.697179783765));
#202539=CARTESIAN_POINT('Ctrl Pts',(-6.767,2.64793996645105E-12,77.69717978381));
#202540=CARTESIAN_POINT('Ctrl Pts',(-6.76700000000007,-0.186007249524281,
77.7059292956212));
#202541=CARTESIAN_POINT('Ctrl Pts',(-6.75932637294534,-0.372014355747388,
77.7146788074324));
#202542=CARTESIAN_POINT('Ctrl Pts',(-6.74400518264201,-0.557389537485025,
77.7234283192436));
#202543=CARTESIAN_POINT('Ctrl Pts',(-6.72868405705112,-0.742763936249463,
77.7321777940992));
#202544=CARTESIAN_POINT('Ctrl Pts',(-6.70571545645755,-0.927506130240071,
77.7409272689549));
#202545=CARTESIAN_POINT('Ctrl Pts',(-6.67517739404835,-1.11098863989955,
77.7496767438106));
#202546=CARTESIAN_POINT('Ctrl Pts',(-6.64463945808713,-1.2944703898189,
77.7584261824376));
#202547=CARTESIAN_POINT('Ctrl Pts',(-6.60653217008366,-1.47669218313631,
77.7671756210646));
#202548=CARTESIAN_POINT('Ctrl Pts',(-6.56098496092689,-1.65703510599238,
77.7759250596916));
#202549=CARTESIAN_POINT('Ctrl Pts',(-6.51543793658309,-1.83737729708656,
77.7846744628168));
#202550=CARTESIAN_POINT('Ctrl Pts',(-6.46245112167433,-2.01584035510887,
77.793423865942));
#202551=CARTESIAN_POINT('Ctrl Pts',(-6.40220448374265,-2.19181813760757,
77.8021732690671));
#202552=CARTESIAN_POINT('Ctrl Pts',(-6.3419580852652,-2.367795220671,77.8109226374172));
#202553=CARTESIAN_POINT('Ctrl Pts',(-6.27445201433125,-2.54128677684113,
77.8196720057673));
#202554=CARTESIAN_POINT('Ctrl Pts',(-6.19991555071929,-2.7117035538475,
77.8284213741174));
#202555=CARTESIAN_POINT('Ctrl Pts',(-6.12537937716719,-2.88211966767422,
77.8371707084192));
#202556=CARTESIAN_POINT('Ctrl Pts',(-6.04381298052545,-3.04946076371735,
77.845920042721));
#202557=CARTESIAN_POINT('Ctrl Pts',(-5.95549339335856,-3.21315848374502,
77.8546693770228));
#202558=CARTESIAN_POINT('Ctrl Pts',(-5.8671741425544,-3.37685558033439,
77.8634186780029));
#202559=CARTESIAN_POINT('Ctrl Pts',(-5.77210188876636,-3.53690907646694,
77.8721679789831));
#202560=CARTESIAN_POINT('Ctrl Pts',(-5.67059953347041,-3.69277536969217,
77.8809172799633));
#202561=CARTESIAN_POINT('Ctrl Pts',(-5.56909755631438,-3.84864108224844,
77.8896665483486));
#202562=CARTESIAN_POINT('Ctrl Pts',(-5.46116568196915,-4.00031938297428,
77.8984158167338));
#202563=CARTESIAN_POINT('Ctrl Pts',(-5.34717048533678,-4.14729511859757,
77.9071650851191));
#202564=CARTESIAN_POINT('Ctrl Pts',(-5.23317570391911,-4.29427031887825,
77.9159143216362));
#202565=CARTESIAN_POINT('Ctrl Pts',(-5.11311782003588,-4.43654276189462,
77.9246635581532));
#202566=CARTESIAN_POINT('Ctrl Pts',(-4.98740458984825,-4.57362924351774,
77.9334127946703));
#202567=CARTESIAN_POINT('Ctrl Pts',(-4.86169180711813,-4.71071523720195,
77.9421620000457));
#202568=CARTESIAN_POINT('Ctrl Pts',(-4.73032391204238,-4.84261509523173,
77.9509112054212));
#202569=CARTESIAN_POINT('Ctrl Pts',(-4.59374707013663,-4.96888084538271,
77.9596604107966));
#202570=CARTESIAN_POINT('Ctrl Pts',(-4.45717070301509,-5.09514615659408,
77.968409585757));
#202571=CARTESIAN_POINT('Ctrl Pts',(-4.31538563571106,-5.21577720459474,
77.9771587607175));
#202572=CARTESIAN_POINT('Ctrl Pts',(-4.16887341029574,-5.33036429232835,
77.9859079356779));
#202573=CARTESIAN_POINT('Ctrl Pts',(-4.02236168203749,-5.44495099123585,
77.99465708095));
#202574=CARTESIAN_POINT('Ctrl Pts',(-3.87112305348185,-5.55349359438589,
78.003406226222));
#202575=CARTESIAN_POINT('Ctrl Pts',(-3.71567117017754,-5.65562346298898,
78.0121553714941));
#202576=CARTESIAN_POINT('Ctrl Pts',(-3.56021980145811,-5.75775299351649,
78.0209044878042));
#202577=CARTESIAN_POINT('Ctrl Pts',(-3.4005554453834,-5.85346967463878,
78.0296536041144));
#202578=CARTESIAN_POINT('Ctrl Pts',(-3.23722035986843,-5.94244842986907,
78.0384027204246));
#202579=CARTESIAN_POINT('Ctrl Pts',(-3.07388580147141,-6.0314268979455,
78.0471518084994));
#202580=CARTESIAN_POINT('Ctrl Pts',(-2.90688078896509,-6.11366734656815,
78.0559008965743));
#202581=CARTESIAN_POINT('Ctrl Pts',(-2.7367725072127,-6.18889046952398,
78.0646499846491));
#202582=CARTESIAN_POINT('Ctrl Pts',(-2.56666476031348,-6.26411335596383,
78.0733990452152));
#202583=CARTESIAN_POINT('Ctrl Pts',(-2.39345402574995,-6.33231884500621,
78.0821481057812));
#202584=CARTESIAN_POINT('Ctrl Pts',(-2.21772856065384,-6.39327529762799,
78.0908971663472));
#202585=CARTESIAN_POINT('Ctrl Pts',(-2.04200363348287,-6.45423156365183,
78.0996462001309));
#202586=CARTESIAN_POINT('Ctrl Pts',(-1.86376426189034,-6.50793874375729,
78.1083952339147));
#202587=CARTESIAN_POINT('Ctrl Pts',(-1.6836157775289,-6.5542144390961,78.1171442676984));
#202588=CARTESIAN_POINT('Ctrl Pts',(-1.50346782967559,-6.60048999661922,
78.1258932754262));
#202589=CARTESIAN_POINT('Ctrl Pts',(-1.3214110579477,-6.63933404237755,
78.134642283154));
#202590=CARTESIAN_POINT('Ctrl Pts',(-1.1380637548683,-6.67061465607594,
78.1433912908818));
#202591=CARTESIAN_POINT('Ctrl Pts',(-0.954716982601156,-6.70189517921323,
78.1521402732802));
#202592=CARTESIAN_POINT('Ctrl Pts',(-0.770079968900338,-6.72561226592249,
78.1608892556786));
#202593=CARTESIAN_POINT('Ctrl Pts',(-0.584779765556509,-6.74168536983117,
78.169638238077));
#202594=CARTESIAN_POINT('Ctrl Pts',(-0.391489830649617,-6.75845151013863,
78.1787644570869));
#202595=CARTESIAN_POINT('Ctrl Pts',(-0.197478578236712,-6.7668998303163,
78.1878906760967));
#202596=CARTESIAN_POINT('Ctrl Pts',(-0.00346287644978017,-6.76699911397118,
78.1970168951066));
#202597=CARTESIAN_POINT('Ctrl Pts',(0.18448983465634,-6.76709529501184,
78.2058579197724));
#202598=CARTESIAN_POINT('Ctrl Pts',(0.372446404251812,-6.75935639738155,
78.2146989444382));
#202599=CARTESIAN_POINT('Ctrl Pts',(0.559755019490766,-6.74380925873166,
78.2235399691041));
#202600=CARTESIAN_POINT('Ctrl Pts',(0.745134705524248,-6.72842222659778,
78.2322899477138));
#202601=CARTESIAN_POINT('Ctrl Pts',(0.929879431231083,-6.70538706057489,
78.2410399263235));
#202602=CARTESIAN_POINT('Ctrl Pts',(1.11336163627081,-6.67478200894085,
78.2497899049333));
#202603=CARTESIAN_POINT('Ctrl Pts',(1.29684196300992,-6.6441772706096,78.2585397939698));
#202604=CARTESIAN_POINT('Ctrl Pts',(1.47905951217801,-6.60600284890526,
78.2672896830064));
#202605=CARTESIAN_POINT('Ctrl Pts',(1.65939532067392,-6.56038841607153,
78.2760395720429));
#202606=CARTESIAN_POINT('Ctrl Pts',(1.83972934301116,-6.51477443503168,
78.2847893744151));
#202607=CARTESIAN_POINT('Ctrl Pts',(2.01818138406585,-6.46172066062041,
78.2935391767872));
#202608=CARTESIAN_POINT('Ctrl Pts',(2.19414528354525,-6.40140730423367,
78.3022889791594));
#202609=CARTESIAN_POINT('Ctrl Pts',(2.37010749864318,-6.34109452518523,
78.3110386977757));
#202610=CARTESIAN_POINT('Ctrl Pts',(2.5435813486677,-6.27352239616378,78.319788416392));
#202611=CARTESIAN_POINT('Ctrl Pts',(2.71397759435858,-6.19892043966686,
78.3285381350083));
#202612=CARTESIAN_POINT('Ctrl Pts',(2.88437226558419,-6.12431917249376,
78.337287772777));
#202613=CARTESIAN_POINT('Ctrl Pts',(3.05168912681244,-6.04268832278653,
78.3460374105457));
#202614=CARTESIAN_POINT('Ctrl Pts',(3.21535986274135,-5.95430516123182,
78.3547870483144));
#202615=CARTESIAN_POINT('Ctrl Pts',(3.37902914073126,-5.86592278697277,
78.3635366081435));
#202616=CARTESIAN_POINT('Ctrl Pts',(3.53905210621859,-5.77078835741766,
78.3722861679726));
#202617=CARTESIAN_POINT('Ctrl Pts',(3.69488522831986,-5.66922500431441,
78.3810357278017));
#202618=CARTESIAN_POINT('Ctrl Pts',(3.85071701407236,-5.56766252216889,
78.3897852125988));
#202619=CARTESIAN_POINT('Ctrl Pts',(4.00235878822706,-5.45967138329149,
78.3985346973959));
#202620=CARTESIAN_POINT('Ctrl Pts',(4.14929549611633,-5.34561838199369,
78.407284182193));
#202621=CARTESIAN_POINT('Ctrl Pts',(4.29623099276398,-5.23156632086763,
78.4160335948656));
#202622=CARTESIAN_POINT('Ctrl Pts',(4.43846127436336,-5.11145267304697,
78.4247830075382));
#202623=CARTESIAN_POINT('Ctrl Pts',(4.5755032605475,-4.98568540049603,78.4335324202108));
#202624=CARTESIAN_POINT('Ctrl Pts',(4.7125441625808,-4.85991912290071,78.4422817636661));
#202625=CARTESIAN_POINT('Ctrl Pts',(4.84439664019051,-4.72849950385122,
78.4510311071213));
#202626=CARTESIAN_POINT('Ctrl Pts',(4.97061286795025,-4.59187289860765,
78.4597804505765));
#202627=CARTESIAN_POINT('Ctrl Pts',(5.09682813912948,-4.45524732884383,
78.4685297277214));
#202628=CARTESIAN_POINT('Ctrl Pts',(5.21740705148085,-4.31341506235489,
78.4772790048662));
#202629=CARTESIAN_POINT('Ctrl Pts',(5.33194007545927,-4.16685781275429,
78.486028282011));
#202630=CARTESIAN_POINT('Ctrl Pts',(5.44647226944708,-4.0203016252154,78.4947774957521));
#202631=CARTESIAN_POINT('Ctrl Pts',(5.55495848628328,-3.86902074887626,
78.5035267094932));
#202632=CARTESIAN_POINT('Ctrl Pts',(5.65703027291994,-3.71352898080348,
78.5122759232344));
#202633=CARTESIAN_POINT('Ctrl Pts',(5.75910135377191,-3.55803828789274,
78.5210250764783));
#202634=CARTESIAN_POINT('Ctrl Pts',(5.85475793592935,-3.39833700106398,
78.5297742297221));
#202635=CARTESIAN_POINT('Ctrl Pts',(5.94367514427569,-3.2349675082324,78.538523382966));
#202636=CARTESIAN_POINT('Ctrl Pts',(6.03259176732793,-3.07159909077424,
78.5472724786189));
#202637=CARTESIAN_POINT('Ctrl Pts',(6.1147689683606,-2.90456276731147,78.5560215742719));
#202638=CARTESIAN_POINT('Ctrl Pts',(6.18992765548007,-2.73442583002777,
78.5647706699248));
#202639=CARTESIAN_POINT('Ctrl Pts',(6.26508587283174,-2.56428995615879,
78.5735197108928));
#202640=CARTESIAN_POINT('Ctrl Pts',(6.33322554827277,-2.39105376934892,
78.5822687518609));
#202641=CARTESIAN_POINT('Ctrl Pts',(6.39411526733144,-2.21530561053751,
78.5910177928289));
#202642=CARTESIAN_POINT('Ctrl Pts',(6.45500462602948,-2.03955849184779,
78.5997667820179));
#202643=CARTESIAN_POINT('Ctrl Pts',(6.50864402040829,-1.86129970164234,
78.608515771207));
#202644=CARTESIAN_POINT('Ctrl Pts',(6.55485128368678,-1.68113463135758,
78.617264760396));
#202645=CARTESIAN_POINT('Ctrl Pts',(6.60199809554391,-1.49730620116585,
78.6261916458674));
#202646=CARTESIAN_POINT('Ctrl Pts',(6.64140720707925,-1.31149343245431,
78.6351185313388));
#202647=CARTESIAN_POINT('Ctrl Pts',(6.67293928722926,-1.12435326697276,
78.6440454168102));
#202648=CARTESIAN_POINT('Ctrl Pts',(6.70384625876291,-0.940923067004143,
78.6527953309877));
#202649=CARTESIAN_POINT('Ctrl Pts',(6.72718554579823,-0.756217899519271,
78.6615452451652));
#202650=CARTESIAN_POINT('Ctrl Pts',(6.74287786815348,-0.570865181252157,
78.6702951593426));
#202651=CARTESIAN_POINT('Ctrl Pts',(6.75856988190858,-0.385516108071707,
78.6790449014471));
#202652=CARTESIAN_POINT('Ctrl Pts',(6.76661520773409,-0.199519795224209,
78.6877946435516));
#202653=CARTESIAN_POINT('Ctrl Pts',(6.76698651789579,-0.0135080204536151,
78.6965443856561));
#202654=CARTESIAN_POINT('Ctrl Pts',(6.76735782124898,0.172500343515016,
78.705293967321));
#202655=CARTESIAN_POINT('Ctrl Pts',(6.76005538995173,0.358523882212996,
78.714043548986));
#202656=CARTESIAN_POINT('Ctrl Pts',(6.74510402742344,0.543930748566469,
78.722793130651));
#202657=CARTESIAN_POINT('Ctrl Pts',(6.73015291918008,0.729334461617285,
78.7315425635077));
#202658=CARTESIAN_POINT('Ctrl Pts',(6.70755316306567,0.914121237636686,
78.7402919963643));
#202659=CARTESIAN_POINT('Ctrl Pts',(6.67738151874542,1.09766345166318,78.749041429221));
#202660=CARTESIAN_POINT('Ctrl Pts',(6.64721034747533,1.2812027879985,78.7577907248985));
#202661=CARTESIAN_POINT('Ctrl Pts',(6.60946757205103,1.46349731860504,78.7665400205761));
#202662=CARTESIAN_POINT('Ctrl Pts',(6.56428138111482,1.64392790278326,78.7752893162536));
#202663=CARTESIAN_POINT('Ctrl Pts',(6.51909583859806,1.82435589779211,78.7840384863792));
#202664=CARTESIAN_POINT('Ctrl Pts',(6.4664671639283,2.00291972192412,78.7927876565048));
#202665=CARTESIAN_POINT('Ctrl Pts',(6.40657409872836,2.17901292274802,78.8015368266304));
#202666=CARTESIAN_POINT('Ctrl Pts',(6.34668181342027,2.35510383059109,78.8102858828295));
#202667=CARTESIAN_POINT('Ctrl Pts',(6.27952541914,2.52872390822705,78.8190349390286));
#202668=CARTESIAN_POINT('Ctrl Pts',(6.20533299175465,2.69928350890404,78.8277839952277));
#202669=CARTESIAN_POINT('Ctrl Pts',(6.12831602991494,2.87633637965741,78.8368661313859));
#202670=CARTESIAN_POINT('Ctrl Pts',(6.04371690605212,3.05009086601578,78.8459482675441));
#202671=CARTESIAN_POINT('Ctrl Pts',(5.95184520316569,3.21991112882849,78.8550304037022));
#202672=CARTESIAN_POINT('Ctrl Pts',(5.86333549509206,3.38351691183135,78.8637801840458));
#202673=CARTESIAN_POINT('Ctrl Pts',(5.76807618099294,3.54347103712125,78.8725299643894));
#202674=CARTESIAN_POINT('Ctrl Pts',(5.66639083308935,3.6992301802782,78.881279744733));
#202675=CARTESIAN_POINT('Ctrl Pts',(5.56470914082114,3.85498372382174,78.8900292105179));
#202676=CARTESIAN_POINT('Ctrl Pts',(5.45660203371976,4.00654234702121,78.8987786763028));
#202677=CARTESIAN_POINT('Ctrl Pts',(5.34243669839121,4.15339127986792,78.9075281420877));
#202678=CARTESIAN_POINT('Ctrl Pts',(5.22827486050489,4.30023571401404,78.9162773398337));
#202679=CARTESIAN_POINT('Ctrl Pts',(5.10805534167001,4.44237052028596,78.9250265375797));
#202680=CARTESIAN_POINT('Ctrl Pts',(4.98218644339834,4.57931296628848,78.9337757353258));
#202681=CARTESIAN_POINT('Ctrl Pts',(4.85632073219466,4.71625194483485,78.9425247115374));
#202682=CARTESIAN_POINT('Ctrl Pts',(4.72480612170195,4.84799861524629,78.951273687749));
#202683=CARTESIAN_POINT('Ctrl Pts',(4.58808925235184,4.97410554898602,78.9600226639607));
#202684=CARTESIAN_POINT('Ctrl Pts',(4.45136349473924,5.10022068121315,78.9687722089624));
#202685=CARTESIAN_POINT('Ctrl Pts',(4.30943501209958,5.22069514871934,78.9775217539641));
#202686=CARTESIAN_POINT('Ctrl Pts',(4.16278587431664,5.33511975166349,78.9862712989658));
#202687=CARTESIAN_POINT('Ctrl Pts',(4.01614535740314,5.44953762807941,78.9950203296195));
#202688=CARTESIAN_POINT('Ctrl Pts',(3.86478496657775,5.55790617532888,79.0037693602732));
#202689=CARTESIAN_POINT('Ctrl Pts',(3.70921874747031,5.65985735539464,79.012518390927));
#202690=CARTESIAN_POINT('Ctrl Pts',(3.5536504160574,5.76180991977145,79.0212675403766));
#202691=CARTESIAN_POINT('Ctrl Pts',(3.39387638174367,5.85734478552903,79.0300166898262));
#202692=CARTESIAN_POINT('Ctrl Pts',(3.23043927904389,5.94613749121313,79.0387658392758));
#202693=CARTESIAN_POINT('Ctrl Pts',(3.1869176707033,5.969782069442,79.041095647192));
#202694=CARTESIAN_POINT('Ctrl Pts',(3.14313645919581,5.99294880633451,79.0434254551081));
#202695=CARTESIAN_POINT('Ctrl Pts',(3.09910619832139,6.01563211736937,79.0457552630242));
#202696=CARTESIAN_POINT('Ctrl Pts',(3.09910619832125,6.01563211736945,77.0457552630242));
#202697=CARTESIAN_POINT('Ctrl Pts',(2.93375330764817,6.10081787314658,77.0545047109265));
#202698=CARTESIAN_POINT('Ctrl Pts',(2.7648862784306,6.17918207037043,77.0632541588288));
#202699=CARTESIAN_POINT('Ctrl Pts',(2.59307866646692,6.25045854554001,77.0720036067311));
#202700=CARTESIAN_POINT('Ctrl Pts',(2.42127244185367,6.32173444515041,77.0807529839814));
#202701=CARTESIAN_POINT('Ctrl Pts',(2.24652594672455,6.38592262741841,77.0895023612317));
#202702=CARTESIAN_POINT('Ctrl Pts',(2.06943269687112,6.44280508110565,77.098251738482));
#202703=CARTESIAN_POINT('Ctrl Pts',(1.89234081822075,6.49968709436167,77.1070010479874));
#202704=CARTESIAN_POINT('Ctrl Pts',(1.71290249405593,6.54926340459543,77.1157503574927));
#202705=CARTESIAN_POINT('Ctrl Pts',(1.53172716625069,6.59136563150381,77.124499666998));
#202706=CARTESIAN_POINT('Ctrl Pts',(1.35055318107337,6.6334675464071,77.1332489116653));
#202707=CARTESIAN_POINT('Ctrl Pts',(1.16764249714414,6.66809542395777,77.1419981563325));
#202708=CARTESIAN_POINT('Ctrl Pts',(0.983616340614221,6.6951316562467,77.1507474009998));
#202709=CARTESIAN_POINT('Ctrl Pts',(0.799591486713706,6.72216769715962,
77.1594965837355));
#202710=CARTESIAN_POINT('Ctrl Pts',(0.614451459526574,6.74161215869372,
77.1682457664712));
#202711=CARTESIAN_POINT('Ctrl Pts',(0.428825047910143,6.75339900185713,
77.1769949492069));
#202712=CARTESIAN_POINT('Ctrl Pts',(0.243199888596877,6.76518576550222,
77.1857440729174));
#202713=CARTESIAN_POINT('Ctrl Pts',(0.0570886373917205,6.76931499599834,
77.194493196628));
#202714=CARTESIAN_POINT('Ctrl Pts',(-0.128876626811375,6.76577266947846,
77.2032423203385));
#202715=CARTESIAN_POINT('Ctrl Pts',(-0.314840698188391,6.76223036567992,
77.21199138793));
#202716=CARTESIAN_POINT('Ctrl Pts',(-0.500658497951491,6.75101660879221,
77.2207404555216));
#202717=CARTESIAN_POINT('Ctrl Pts',(-0.685698951926461,6.73216948296216,
77.2294895231131));
#202718=CARTESIAN_POINT('Ctrl Pts',(-0.870738280459878,6.71332247176292,
77.2382385374916));
#202719=CARTESIAN_POINT('Ctrl Pts',(-1.05499998761232,6.68684221356189,
77.2469875518701));
#202720=CARTESIAN_POINT('Ctrl Pts',(-1.23785829161379,6.6528186394853,77.2557365662487));
#202721=CARTESIAN_POINT('Ctrl Pts',(-1.43007412915399,6.61705395369235,
77.2649332999469));
#202722=CARTESIAN_POINT('Ctrl Pts',(-1.62073882531856,6.57295372728701,
77.2741300336452));
#202723=CARTESIAN_POINT('Ctrl Pts',(-1.809136960857,6.52068343479893,77.2833267673434));
#202724=CARTESIAN_POINT('Ctrl Pts',(-1.98838356180342,6.47095219816971,
77.2920767650571));
#202725=CARTESIAN_POINT('Ctrl Pts',(-2.16557827566814,6.41382586852822,
77.3008267627708));
#202726=CARTESIAN_POINT('Ctrl Pts',(-2.34011918616039,6.34949849945364,
77.3095767604844));
#202727=CARTESIAN_POINT('Ctrl Pts',(-2.514656556855,6.28517243497791,77.3183265807427));
#202728=CARTESIAN_POINT('Ctrl Pts',(-2.68653996289799,6.21364572244765,
77.3270764010011));
#202729=CARTESIAN_POINT('Ctrl Pts',(-2.85518555374534,6.13516132254759,
77.3358262212594));
#202730=CARTESIAN_POINT('Ctrl Pts',(-3.023827948533,6.05667841003197,77.3445758756969));
#202731=CARTESIAN_POINT('Ctrl Pts',(-3.18923239103964,5.97123819494921,
77.3533255301344));
#202732=CARTESIAN_POINT('Ctrl Pts',(-3.35083705962459,5.87913088813699,
77.3620751845719));
#202733=CARTESIAN_POINT('Ctrl Pts',(-3.51243888037233,5.78702520446239,
77.3708246848208));
#202734=CARTESIAN_POINT('Ctrl Pts',(-3.67024081218602,5.68825280609066,
77.3795741850698));
#202735=CARTESIAN_POINT('Ctrl Pts',(-3.82370687539398,5.58314917685931,
77.3883236853187));
#202736=CARTESIAN_POINT('Ctrl Pts',(-3.97717043812908,5.47804726011584,
77.3970730430092));
#202737=CARTESIAN_POINT('Ctrl Pts',(-4.12629803717655,5.36661448087931,
77.4058224006996));
#202738=CARTESIAN_POINT('Ctrl Pts',(-4.27058317202209,5.24922931208399,
77.4145717583901));
#202739=CARTESIAN_POINT('Ctrl Pts',(-4.41486614770225,5.13184589990755,
77.4233209851502));
#202740=CARTESIAN_POINT('Ctrl Pts',(-4.554306581899,5.00851045727138,77.4320702119102));
#202741=CARTESIAN_POINT('Ctrl Pts',(-4.68843088997433,4.87964187107359,
77.4408194386703));
#202742=CARTESIAN_POINT('Ctrl Pts',(-4.82255336913539,4.75077504212323,
77.4495685461262));
#202743=CARTESIAN_POINT('Ctrl Pts',(-4.95135966060956,4.61637541912574,
77.4583176535821));
#202744=CARTESIAN_POINT('Ctrl Pts',(-5.07441230865191,4.47689945406439,
77.4670667610381));
#202745=CARTESIAN_POINT('Ctrl Pts',(-5.19746344222487,4.33742520560224,
77.4758157608144));
#202746=CARTESIAN_POINT('Ctrl Pts',(-5.31476088450967,4.19287495496154,
77.4845647605908));
#202747=CARTESIAN_POINT('Ctrl Pts',(-5.42590627625186,4.04373961591627,
77.4933137603671));
#202748=CARTESIAN_POINT('Ctrl Pts',(-5.53706380669141,3.89458798911749,
77.5020637156618));
#202749=CARTESIAN_POINT('Ctrl Pts',(-5.64206777068481,3.74085050160387,
77.5108136709566));
#202750=CARTESIAN_POINT('Ctrl Pts',(-5.74056148160772,3.58304938228345,
77.5195636262513));
#202751=CARTESIAN_POINT('Ctrl Pts',(-5.83905138948787,3.4252543559856,77.5283132436924));
#202752=CARTESIAN_POINT('Ctrl Pts',(-5.931031395547,3.2633962550255,77.5370628611334));
#202753=CARTESIAN_POINT('Ctrl Pts',(-6.0161890781804,3.09802485070454,77.5458124785746));
#202754=CARTESIAN_POINT('Ctrl Pts',(-6.10134392542327,2.93265895255166,
77.5545618046904));
#202755=CARTESIAN_POINT('Ctrl Pts',(-6.17967677259329,2.76378023991631,
77.5633111308063));
#202756=CARTESIAN_POINT('Ctrl Pts',(-6.25092157006877,2.59196229232775,
77.5720604569222));
#202757=CARTESIAN_POINT('Ctrl Pts',(-6.32216437405561,2.42014915234817,
77.5808095382246));
#202758=CARTESIAN_POINT('Ctrl Pts',(-6.38631941546887,2.24539720668636,
77.5895586195271));
#202759=CARTESIAN_POINT('Ctrl Pts',(-6.44316881035664,2.06829994953524,
77.5983077008295));
#202760=CARTESIAN_POINT('Ctrl Pts',(-6.50002334522858,1.89118668030339,
77.6070575731719));
#202761=CARTESIAN_POINT('Ctrl Pts',(-6.54957082409546,1.71172794813635,
77.6158074455142));
#202762=CARTESIAN_POINT('Ctrl Pts',(-6.59164294294697,1.5305333425631,77.6245573178566));
#202763=CARTESIAN_POINT('Ctrl Pts',(-6.63371214080915,1.34935131699594,
77.6333065827115));
#202764=CARTESIAN_POINT('Ctrl Pts',(-6.66830695238639,1.16643393835776,
77.6420558475664));
#202765=CARTESIAN_POINT('Ctrl Pts',(-6.69530988153105,0.982402458401216,
77.6508051124213));
#202766=CARTESIAN_POINT('Ctrl Pts',(-6.72231419689764,0.798361531007603,
77.6595548264283));
#202767=CARTESIAN_POINT('Ctrl Pts',(-6.74172580828725,0.61320667142327,
77.6683045404354));
#202768=CARTESIAN_POINT('Ctrl Pts',(-6.75347878027793,0.427566795174375,
77.6770542544424));
#202769=CARTESIAN_POINT('Ctrl Pts',(-6.76248992366069,0.285234494564716,
77.6837627642166));
#202770=CARTESIAN_POINT('Ctrl Pts',(-6.76699999997978,0.142617266751198,
77.6904712739908));
#202771=CARTESIAN_POINT('Ctrl Pts',(-6.767,9.5948989328826E-10,77.697179783765));
#202772=CARTESIAN_POINT('',(-6.76699925239411,0.00318089572253539,77.3028202162312));
#202773=CARTESIAN_POINT('Ctrl Pts',(3.09910619832139,6.01563211736937,76.6513581962709));
#202774=CARTESIAN_POINT('Ctrl Pts',(2.99281630860975,6.07039006293475,76.6570008096127));
#202775=CARTESIAN_POINT('Ctrl Pts',(2.88509649128983,6.12231922629877,76.6626434229546));
#202776=CARTESIAN_POINT('Ctrl Pts',(2.77609525020218,6.17135189093969,76.6682860362965));
#202777=CARTESIAN_POINT('Ctrl Pts',(2.60895175081397,6.24653902707351,76.67693847117));
#202778=CARTESIAN_POINT('Ctrl Pts',(2.43864473878715,6.31498012337952,76.6855909060436));
#202779=CARTESIAN_POINT('Ctrl Pts',(2.2657338029222,6.37642057382476,76.6942433409172));
#202780=CARTESIAN_POINT('Ctrl Pts',(2.09298300908987,6.43780412099452,76.7028877623097));
#202781=CARTESIAN_POINT('Ctrl Pts',(1.91763338705729,6.492199852584,76.7115321837023));
#202782=CARTESIAN_POINT('Ctrl Pts',(1.7402643927085,6.53940126031971,76.7201766050948));
#202783=CARTESIAN_POINT('Ctrl Pts',(1.55720029904399,6.58811824695285,76.7290985881804));
#202784=CARTESIAN_POINT('Ctrl Pts',(1.37198528946647,6.62917107903984,76.7380205712659));
#202785=CARTESIAN_POINT('Ctrl Pts',(1.18527566951571,6.6623877541955,76.7469425543514));
#202786=CARTESIAN_POINT('Ctrl Pts',(1.00471992640263,6.69450962058919,76.7555704723263));
#202787=CARTESIAN_POINT('Ctrl Pts',(0.822766852872387,6.71930357141152,
76.7641983903011));
#202788=CARTESIAN_POINT('Ctrl Pts',(0.640022910290413,6.7366653230143,76.772826308276));
#202789=CARTESIAN_POINT('Ctrl Pts',(0.447936281930944,6.75491468482993,
76.7818953239169));
#202790=CARTESIAN_POINT('Ctrl Pts',(0.254976129764303,6.76495192010977,
76.7909643395577));
#202791=CARTESIAN_POINT('Ctrl Pts',(0.061856499368857,6.76671728192377,
76.8000333551986));
#202792=CARTESIAN_POINT('Ctrl Pts',(-0.131263131026525,6.76848264373778,
76.8091023708395));
#202793=CARTESIAN_POINT('Ctrl Pts',(-0.32454184880341,6.76197609319795,
76.8181713864804));
#202794=CARTESIAN_POINT('Ctrl Pts',(-0.51726136391349,6.74720161855286,
76.8272404021212));
#202795=CARTESIAN_POINT('Ctrl Pts',(-0.696326350455738,6.73347394233917,
76.8356668614902));
#202796=CARTESIAN_POINT('Ctrl Pts',(-0.874829202650989,6.71261476296558,
76.8440933208592));
#202797=CARTESIAN_POINT('Ctrl Pts',(-1.05218417540381,6.68469875619162,
76.8525197802282));
#202798=CARTESIAN_POINT('Ctrl Pts',(-1.22958109821798,6.65677614639899,
76.8609482327213));
#202799=CARTESIAN_POINT('Ctrl Pts',(-1.40582927286509,6.62179343263393,
76.8693766852145));
#202800=CARTESIAN_POINT('Ctrl Pts',(-1.58035202400563,6.57987663107914,
76.8778051377077));
#202801=CARTESIAN_POINT('Ctrl Pts',(-1.75493964854348,6.53794424825884,
76.8862367232156));
#202802=CARTESIAN_POINT('Ctrl Pts',(-1.92780024864766,6.48907271559709,
76.8946683087235));
#202803=CARTESIAN_POINT('Ctrl Pts',(-2.09837082971887,6.43343833894326,
76.9030998942314));
#202804=CARTESIAN_POINT('Ctrl Pts',(-2.26909933190827,6.37775245374137,
76.9115392860409));
#202805=CARTESIAN_POINT('Ctrl Pts',(-2.43753326381252,6.31529131779788,
76.9199786778504));
#202806=CARTESIAN_POINT('Ctrl Pts',(-2.60312712465974,6.24628034696336,
76.92841806966));
#202807=CARTESIAN_POINT('Ctrl Pts',(-2.76880834318714,6.17723296995842,
76.9368619136013));
#202808=CARTESIAN_POINT('Ctrl Pts',(-2.93164620001799,6.10162900134795,
76.9453057575427));
#202809=CARTESIAN_POINT('Ctrl Pts',(-3.09111792290226,6.01974077404604,
76.953749601484));
#202810=CARTESIAN_POINT('Ctrl Pts',(-3.25075828289685,5.93776595211925,
76.962202374566));
#202811=CARTESIAN_POINT('Ctrl Pts',(-3.40702510742384,5.84949375477547,
76.9706551476479));
#202812=CARTESIAN_POINT('Ctrl Pts',(-3.55942190022044,5.75524150112149,
76.9791079207299));
#202813=CARTESIAN_POINT('Ctrl Pts',(-3.60201197790986,5.72890098087916,
76.9814702031352));
#202814=CARTESIAN_POINT('Ctrl Pts',(-3.64429997750867,5.7020936581561,76.9838324855406));
#202815=CARTESIAN_POINT('Ctrl Pts',(-3.68627549597668,5.67482704298218,
76.9861947679459));
#202816=CARTESIAN_POINT('Ctrl Pts',(-3.83391101635315,5.57892540633714,
76.9945033441093));
#202817=CARTESIAN_POINT('Ctrl Pts',(-3.977946997598,5.47716448481761,77.0028119202726));
#202818=CARTESIAN_POINT('Ctrl Pts',(-4.1178974369687,5.36984261395123,77.011120496436));
#202819=CARTESIAN_POINT('Ctrl Pts',(-4.25772887211959,5.26261200221608,
77.0194220075581));
#202820=CARTESIAN_POINT('Ctrl Pts',(-4.39348141141764,5.14983007320495,
77.0277235186802));
#202821=CARTESIAN_POINT('Ctrl Pts',(-4.5246976870573,5.03183861433754,77.0360250298023));
#202822=CARTESIAN_POINT('Ctrl Pts',(-4.65582664447303,4.91392567320413,
77.0443210166615));
#202823=CARTESIAN_POINT('Ctrl Pts',(-4.78242509459466,4.79081034221048,
77.0526170035207));
#202824=CARTESIAN_POINT('Ctrl Pts',(-4.90406829011053,4.66287499359916,
77.0609129903799));
#202825=CARTESIAN_POINT('Ctrl Pts',(-5.02565301772346,4.5350011372194,77.0692049897662));
#202826=CARTESIAN_POINT('Ctrl Pts',(-5.1422869973124,4.40231213236403,77.0774969891524));
#202827=CARTESIAN_POINT('Ctrl Pts',(-5.25358179426859,4.2652276997752,77.0857889885386));
#202828=CARTESIAN_POINT('Ctrl Pts',(-5.36484365830891,4.12818383143743,
77.0940785342637));
#202829=CARTESIAN_POINT('Ctrl Pts',(-5.47076926924061,3.98674739831546,
77.1023680799888));
#202830=CARTESIAN_POINT('Ctrl Pts',(-5.57100986993585,3.84137189413851,
77.1106576257139));
#202831=CARTESIAN_POINT('Ctrl Pts',(-5.671260739849,3.69598149686717,77.1189480206672));
#202832=CARTESIAN_POINT('Ctrl Pts',(-5.76582523161551,3.54665150508406,
77.1272384156206));
#202833=CARTESIAN_POINT('Ctrl Pts',(-5.85439708039725,3.39386561682046,
77.135528810574));
#202834=CARTESIAN_POINT('Ctrl Pts',(-5.94297809515259,3.24106391730942,
77.1438200634697));
#202835=CARTESIAN_POINT('Ctrl Pts',(-6.02556505536327,3.08480591015634,
77.1521113163654));
#202836=CARTESIAN_POINT('Ctrl Pts',(-6.10189701660318,2.92560110041837,
77.1604025692611));
#202837=CARTESIAN_POINT('Ctrl Pts',(-6.17824966789225,2.76635313765138,
77.1686960695304));
#202838=CARTESIAN_POINT('Ctrl Pts',(-6.24834379031075,2.60415709500604,
77.1769895697996));
#202839=CARTESIAN_POINT('Ctrl Pts',(-6.31196599249762,2.4395438732586,77.1852830700689));
#202840=CARTESIAN_POINT('Ctrl Pts',(-6.37561610182397,2.27485844583481,
77.1935802081857));
#202841=CARTESIAN_POINT('Ctrl Pts',(-6.43278850760393,2.10775405146005,
77.2018773463024));
#202842=CARTESIAN_POINT('Ctrl Pts',(-6.48331916495928,1.93877837961736,
77.2101744844191));
#202843=CARTESIAN_POINT('Ctrl Pts',(-6.53390992209061,1.76960173275166,
77.2184814909241));
#202844=CARTESIAN_POINT('Ctrl Pts',(-6.57784304819629,1.59854969635067,
77.2267884974291));
#202845=CARTESIAN_POINT('Ctrl Pts',(-6.61500499862981,1.42618297146709,
77.235095503934));
#202846=CARTESIAN_POINT('Ctrl Pts',(-6.65219072891959,1.25370594946787,
77.2434078260755));
#202847=CARTESIAN_POINT('Ctrl Pts',(-6.682596583137,1.07991290447914,77.2517201482169));
#202848=CARTESIAN_POINT('Ctrl Pts',(-6.70616071005493,0.905371487796915,
77.2600324703583));
#202849=CARTESIAN_POINT('Ctrl Pts',(-6.72975994054969,0.730570056048034,
77.2683571754003));
#202850=CARTESIAN_POINT('Ctrl Pts',(-6.74649704300768,0.55501837173379,
77.2766818804423));
#202851=CARTESIAN_POINT('Ctrl Pts',(-6.75636219965656,0.379287261916324,
77.2850065854842));
#202852=CARTESIAN_POINT('Ctrl Pts',(-6.76339885567066,0.253941115395554,
77.2909444623861));
#202853=CARTESIAN_POINT('Ctrl Pts',(-6.76694034313661,0.128503706369033,
77.296882339288));
#202854=CARTESIAN_POINT('Ctrl Pts',(-6.7669992523937,0.00318089659341924,
77.3028202161899));
#202855=CARTESIAN_POINT('Ctrl Pts',(-6.76699925239411,0.0031808957225354,
77.3028202162312));
#202856=CARTESIAN_POINT('Ctrl Pts',(-6.7670034961808,-0.00584728497919235,
77.3032479773526));
#202857=CARTESIAN_POINT('Ctrl Pts',(-6.76698967266099,-0.0148756381434245,
77.3036757384741));
#202858=CARTESIAN_POINT('Ctrl Pts',(-6.76695777975772,-0.0239041204926956,
77.3041034995956));
#202859=CARTESIAN_POINT('Ctrl Pts',(-6.76635609879876,-0.194232480717908,
77.3121734993558));
#202860=CARTESIAN_POINT('Ctrl Pts',(-6.75931813085109,-0.364852553213374,
77.3202434991159));
#202861=CARTESIAN_POINT('Ctrl Pts',(-6.74580030092629,-0.535226400715402,
77.328313498876));
#202862=CARTESIAN_POINT('Ctrl Pts',(-6.73229947583749,-0.705385925404503,
77.3363733469311));
#202863=CARTESIAN_POINT('Ctrl Pts',(-6.7123350369203,-0.875299474224632,
77.3444331949862));
#202864=CARTESIAN_POINT('Ctrl Pts',(-6.6859152800386,-1.04442609510985,
77.3524930430413));
#202865=CARTESIAN_POINT('Ctrl Pts',(-6.65952296016933,-1.21337707739172,
77.3605445209152));
#202866=CARTESIAN_POINT('Ctrl Pts',(-6.62668872020822,-1.38154239255614,
77.3685959987892));
#202867=CARTESIAN_POINT('Ctrl Pts',(-6.58747281898622,-1.54838330497255,
77.3766474766631));
#202868=CARTESIAN_POINT('Ctrl Pts',(-6.54828905067751,-1.71508751048173,
77.3846923572785));
#202869=CARTESIAN_POINT('Ctrl Pts',(-6.50273411351098,-1.88046911180129,
77.3927372378938));
#202870=CARTESIAN_POINT('Ctrl Pts',(-6.45091978386893,-2.04399680579214,
77.4007821185092));
#202871=CARTESIAN_POINT('Ctrl Pts',(-6.39913656869029,-2.20742630153382,
77.4088221681802));
#202872=CARTESIAN_POINT('Ctrl Pts',(-6.34110155597938,-2.36900375136368,
77.4168622178512));
#202873=CARTESIAN_POINT('Ctrl Pts',(-6.27697706098986,-2.52821042949497,
77.4249022675222));
#202874=CARTESIAN_POINT('Ctrl Pts',(-6.2114738541361,-2.69084013865428,
77.4331151826773));
#202875=CARTESIAN_POINT('Ctrl Pts',(-6.13961643550004,-2.85099558755428,
77.4413280978324));
#202876=CARTESIAN_POINT('Ctrl Pts',(-6.06163090484721,-3.00814224620467,
77.4495410129875));
#202877=CARTESIAN_POINT('Ctrl Pts',(-5.98531343435147,-3.16192763927256,
77.4575782591893));
#202878=CARTESIAN_POINT('Ctrl Pts',(-5.90312753748605,-3.31283131003964,
77.4656155053911));
#202879=CARTESIAN_POINT('Ctrl Pts',(-5.81533275626469,-3.46037482563882,
77.4736527515929));
#202880=CARTESIAN_POINT('Ctrl Pts',(-5.72752956685935,-3.60793247161122,
77.4816907675289));
#202881=CARTESIAN_POINT('Ctrl Pts',(-5.63411661445339,-3.75212900050376,
77.4897287834649));
#202882=CARTESIAN_POINT('Ctrl Pts',(-5.53539798233441,-3.89251309274203,
77.4977667994009));
#202883=CARTESIAN_POINT('Ctrl Pts',(-5.43665033767426,-4.03293844263521,
77.5058071776393));
#202884=CARTESIAN_POINT('Ctrl Pts',(-5.33259412436941,-4.16954882023107,
77.5138475558778));
#202885=CARTESIAN_POINT('Ctrl Pts',(-5.22357498902705,-4.30192437567318,
77.5218879341162));
#202886=CARTESIAN_POINT('Ctrl Pts',(-5.11044324347957,-4.43929363298708,
77.5302316255436));
#202887=CARTESIAN_POINT('Ctrl Pts',(-4.99196711566391,-4.57210198637334,
77.538575316971));
#202888=CARTESIAN_POINT('Ctrl Pts',(-4.86857559278257,-4.69992135012512,
77.5469190083984));
#202889=CARTESIAN_POINT('Ctrl Pts',(-4.74946264636408,-4.82330860291436,
77.5549733839885));
#202890=CARTESIAN_POINT('Ctrl Pts',(-4.62576979130375,-4.94204685259125,
77.5630277595787));
#202891=CARTESIAN_POINT('Ctrl Pts',(-4.4979170327914,-5.05579186341023,
77.5710821351688));
#202892=CARTESIAN_POINT('Ctrl Pts',(-4.36996859712787,-5.16962199400856,
77.5791425381589));
#202893=CARTESIAN_POINT('Ctrl Pts',(-4.23785434596213,-5.27845120972642,
77.587202941149));
#202894=CARTESIAN_POINT('Ctrl Pts',(-4.10202415288264,-5.38197796810498,
77.5952633441391));
#202895=CARTESIAN_POINT('Ctrl Pts',(-3.96600407471664,-5.48564945268194,
77.6033350152448));
#202896=CARTESIAN_POINT('Ctrl Pts',(-3.82625799285657,-5.58400347747621,
77.6114066863504));
#202897=CARTESIAN_POINT('Ctrl Pts',(-3.68326177367805,-5.67678357052319,
77.6194783574561));
#202898=CARTESIAN_POINT('Ctrl Pts',(-3.66829856193257,-5.68649213614824,
77.6203229820524));
#202899=CARTESIAN_POINT('Ctrl Pts',(-3.65329978129029,-5.69613971216436,
77.6211676066487));
#202900=CARTESIAN_POINT('Ctrl Pts',(-3.63826598985281,-5.70572603505289,
77.622012231245));
#202901=CARTESIAN_POINT('Ctrl Pts',(-3.49178978095392,-5.79912684081984,
77.630241519866));
#202902=CARTESIAN_POINT('Ctrl Pts',(-3.3414993947806,-5.88702079688458,
77.638470808487));
#202903=CARTESIAN_POINT('Ctrl Pts',(-3.1878464031111,-5.96908069221481,
77.646700097108));
#202904=CARTESIAN_POINT('Ctrl Pts',(-3.03437627491775,-6.05104292750244,
77.6549195919963));
#202905=CARTESIAN_POINT('Ctrl Pts',(-2.87755182299575,-6.12718476003757,
77.6631390868847));
#202906=CARTESIAN_POINT('Ctrl Pts',(-2.71785402812939,-6.19722183577293,
77.671358581773));
#202907=CARTESIAN_POINT('Ctrl Pts',(-2.55831422038495,-6.26718962466541,
77.6795699452132));
#202908=CARTESIAN_POINT('Ctrl Pts',(-2.39590705676496,-6.33106454094299,
77.6877813086534));
#202909=CARTESIAN_POINT('Ctrl Pts',(-2.23113866516536,-6.38860777140092,
77.6959926720936));
#202910=CARTESIAN_POINT('Ctrl Pts',(-2.06650020033913,-6.44610562661307,
77.70419756053));
#202911=CARTESIAN_POINT('Ctrl Pts',(-1.89950455311075,-6.49728162276076,
77.7124024489664));
#202912=CARTESIAN_POINT('Ctrl Pts',(-1.73067849209804,-6.54194473814853,
77.7206073374028));
#202913=CARTESIAN_POINT('Ctrl Pts',(-1.56195167504958,-6.58658159843919,
77.7288074026167));
#202914=CARTESIAN_POINT('Ctrl Pts',(-1.3913969335109,-6.62471311340633,
77.7370074678306));
#202915=CARTESIAN_POINT('Ctrl Pts',(-1.2195569702114,-6.65619784835223,
77.7452075330445));
#202916=CARTESIAN_POINT('Ctrl Pts',(-1.04776673447968,-6.68767347215039,
77.7534052252988));
#202917=CARTESIAN_POINT('Ctrl Pts',(-0.874692369420627,-6.71250607877256,
77.761602917553));
#202918=CARTESIAN_POINT('Ctrl Pts',(-0.700887814206145,-6.73060511929628,
77.7698006098073));
#202919=CARTESIAN_POINT('Ctrl Pts',(-0.527106528455025,-6.74870173666741,
77.7779972045305));
#202920=CARTESIAN_POINT('Ctrl Pts',(-0.352595603862347,-6.76006654543032,
77.7861937992537));
#202921=CARTESIAN_POINT('Ctrl Pts',(-0.177915176489748,-6.76466075941541,
77.7943903939769));
#202922=CARTESIAN_POINT('Ctrl Pts',(-0.00322637531430903,-6.76925519363721,
77.8025873816272));
#202923=CARTESIAN_POINT('Ctrl Pts',(0.171631586183683,-6.76707837697295,
77.8107843692774));
#202924=CARTESIAN_POINT('Ctrl Pts',(0.346097434095885,-6.75814364793412,
77.8189813569277));
#202925=CARTESIAN_POINT('Ctrl Pts',(0.520603366968703,-6.74920686606795,
77.8271802279032));
#202926=CARTESIAN_POINT('Ctrl Pts',(0.69471664861912,-6.73350909768876,
77.8353790988787));
#202927=CARTESIAN_POINT('Ctrl Pts',(0.867879937213135,-6.71111566094513,
77.8435779698541));
#202928=CARTESIAN_POINT('Ctrl Pts',(1.04120723211177,-6.68870101494381,
77.8517846061391));
#202929=CARTESIAN_POINT('Ctrl Pts',(1.21358238007501,-6.65957807671737,
77.8599912424241));
#202930=CARTESIAN_POINT('Ctrl Pts',(1.38445612301583,-6.62386369450972,
77.868197878709));
#202931=CARTESIAN_POINT('Ctrl Pts',(1.55541257027319,-6.58813202624326,
77.8764084870744));
#202932=CARTESIAN_POINT('Ctrl Pts',(1.72486581581406,-6.54580264016105,
77.8846190954398));
#202933=CARTESIAN_POINT('Ctrl Pts',(1.8922807084994,-6.49704261339273,77.8928297038051));
#202934=CARTESIAN_POINT('Ctrl Pts',(2.05992648291789,-6.44821534171382,
77.9010516354134));
#202935=CARTESIAN_POINT('Ctrl Pts',(2.22552794612087,-6.39293981922132,
77.9092735670216));
#202936=CARTESIAN_POINT('Ctrl Pts',(2.38856775122155,-6.33143215219309,
77.9174954986298));
#202937=CARTESIAN_POINT('Ctrl Pts',(2.53679907111127,-6.27551106800569,
77.9249706533847));
#202938=CARTESIAN_POINT('Ctrl Pts',(2.68291301063721,-6.21443920689228,
77.9324458081395));
#202939=CARTESIAN_POINT('Ctrl Pts',(2.82653848469758,-6.14841192459675,
77.9399209628944));
#202940=CARTESIAN_POINT('Ctrl Pts',(2.99822540390185,-6.06948427784806,
77.9488566081818));
#202941=CARTESIAN_POINT('Ctrl Pts',(3.16671399792719,-5.98331117677076,
77.9577922534692));
#202942=CARTESIAN_POINT('Ctrl Pts',(3.33140873755182,-5.89016169755665,
77.9667278987566));
#202943=CARTESIAN_POINT('Ctrl Pts',(3.49585590525969,-5.79715224221438,
77.975650111831));
#202944=CARTESIAN_POINT('Ctrl Pts',(3.65652037369879,-5.69718746075504,
77.9845723249053));
#202945=CARTESIAN_POINT('Ctrl Pts',(3.81282991248378,-5.59058289076094,
77.9934945379797));
#202946=CARTESIAN_POINT('Ctrl Pts',(3.96875653449884,-5.48423947359167,
78.0023948940065));
#202947=CARTESIAN_POINT('Ctrl Pts',(4.12034930615262,-5.37128887660934,
78.0112952500334));
#202948=CARTESIAN_POINT('Ctrl Pts',(4.26706426309935,-5.25209021005736,
78.0201956060603));
#202949=CARTESIAN_POINT('Ctrl Pts',(4.41355256407153,-5.13307569030606,
78.0290822121675));
#202950=CARTESIAN_POINT('Ctrl Pts',(4.55517788244426,-5.00783251716709,
78.0379688182747));
#202951=CARTESIAN_POINT('Ctrl Pts',(4.69142623686737,-4.87676212912138,
78.0468554243819));
#202952=CARTESIAN_POINT('Ctrl Pts',(4.82732454476724,-4.74602848447216,
78.0557191992));
#202953=CARTESIAN_POINT('Ctrl Pts',(4.95787326881555,-4.60949767734603,
78.0645829740182));
#202954=CARTESIAN_POINT('Ctrl Pts',(5.08259301445811,-4.46760979153077,
78.0734467488363));
#202955=CARTESIAN_POINT('Ctrl Pts',(5.20185920672812,-4.33192616113814,
78.0819229421307));
#202956=CARTESIAN_POINT('Ctrl Pts',(5.31579507035545,-4.19134408557049,
78.090399135425));
#202957=CARTESIAN_POINT('Ctrl Pts',(5.42401037482033,-4.04628230031488,
78.0988753287194));
#202958=CARTESIAN_POINT('Ctrl Pts',(5.5288150275785,-3.90579246750081,78.1070843754834));
#202959=CARTESIAN_POINT('Ctrl Pts',(5.62815222232991,-3.76123570369797,
78.1152934222473));
#202960=CARTESIAN_POINT('Ctrl Pts',(5.72170744990241,-3.61308079867187,
78.1235024690113));
#202961=CARTESIAN_POINT('Ctrl Pts',(5.81528494302509,-3.46489063371899,
78.1317134694763));
#202962=CARTESIAN_POINT('Ctrl Pts',(5.90307753732829,-3.31310092255337,
78.1399244699413));
#202963=CARTESIAN_POINT('Ctrl Pts',(5.98481544779825,-3.15820725345812,
78.1481354704063));
#202964=CARTESIAN_POINT('Ctrl Pts',(6.06658737979926,-3.00324911342468,
78.156349888512));
#202965=CARTESIAN_POINT('Ctrl Pts',(6.14229944130406,-2.84518475627035,
78.1645643066176));
#202966=CARTESIAN_POINT('Ctrl Pts',(6.21172893037401,-2.68453211855521,
78.1727787247233));
#202967=CARTESIAN_POINT('Ctrl Pts',(6.28123658616688,-2.5236986111493,78.1810023909763));
#202968=CARTESIAN_POINT('Ctrl Pts',(6.34444740071612,-2.36027132994105,
78.1892260572292));
#202969=CARTESIAN_POINT('Ctrl Pts',(6.40118739729601,-2.19478675608787,
78.1974497234822));
#202970=CARTESIAN_POINT('Ctrl Pts',(6.45796377112014,-2.02919608647997,
78.2056786621063));
#202971=CARTESIAN_POINT('Ctrl Pts',(6.50826095498072,-1.86154583509582,
78.2139076007304));
#202972=CARTESIAN_POINT('Ctrl Pts',(6.551955547683,-1.69238515154973,78.2221365393544));
#202973=CARTESIAN_POINT('Ctrl Pts',(6.59571028861772,-1.52299160815792,
78.230376805607));
#202974=CARTESIAN_POINT('Ctrl Pts',(6.63284420883924,-1.3520838265177,78.2386170718595));
#202975=CARTESIAN_POINT('Ctrl Pts',(6.66328527878965,-1.18021959544197,
78.2468573381121));
#202976=CARTESIAN_POINT('Ctrl Pts',(6.67679658451016,-1.10393744858353,
78.2505147902561));
#202977=CARTESIAN_POINT('Ctrl Pts',(6.68899005946708,-1.02746692907892,
78.2541722424001));
#202978=CARTESIAN_POINT('Ctrl Pts',(6.69986269242552,-0.95085693069184,
78.2578296945441));
#202979=CARTESIAN_POINT('Ctrl Pts',(6.72497633512527,-0.773902909151978,
78.2662776893111));
#202980=CARTESIAN_POINT('Ctrl Pts',(6.74309704629527,-0.595799682392562,
78.2747256840781));
#202981=CARTESIAN_POINT('Ctrl Pts',(6.75413168918437,-0.417126030301919,
78.2831736788451));
#202982=CARTESIAN_POINT('Ctrl Pts',(6.76515622657292,-0.238616007130643,
78.291613936958));
#202983=CARTESIAN_POINT('Ctrl Pts',(6.76910761052382,-0.0595369311969636,
78.3000541950708));
#202984=CARTESIAN_POINT('Ctrl Pts',(6.76594432205611,0.119525858443792,
78.3084944531836));
#202985=CARTESIAN_POINT('Ctrl Pts',(6.76278344352315,0.298452230035839,
78.31692828113));
#202986=CARTESIAN_POINT('Ctrl Pts',(6.75251870377821,0.477362007777319,
78.3253621090764));
#202987=CARTESIAN_POINT('Ctrl Pts',(6.73516061201328,0.655668003172985,
78.3337959370228));
#202988=CARTESIAN_POINT('Ctrl Pts',(6.71781307574966,0.833865570223439,
78.3422246363362));
#202989=CARTESIAN_POINT('Ctrl Pts',(6.6933808196366,1.01145975582435,78.3506533356496));
#202990=CARTESIAN_POINT('Ctrl Pts',(6.66192635602018,1.18786624961048,78.3590820349631));
#202991=CARTESIAN_POINT('Ctrl Pts',(6.63048618943762,1.36419256114826,78.36750690317));
#202992=CARTESIAN_POINT('Ctrl Pts',(6.5920302382928,1.53933192953616,78.375931771377));
#202993=CARTESIAN_POINT('Ctrl Pts',(6.54667255803846,1.71270762765458,78.3843566395839));
#202994=CARTESIAN_POINT('Ctrl Pts',(6.50132492192615,1.88604493293353,78.3927796421625));
#202995=CARTESIAN_POINT('Ctrl Pts',(6.44907868569588,2.0576190236097,78.4012026447411));
#202996=CARTESIAN_POINT('Ctrl Pts',(6.39009859827946,2.22686526405773,78.4096256473198));
#202997=CARTESIAN_POINT('Ctrl Pts',(6.33112518559704,2.39609235103065,78.4180476966732));
#202998=CARTESIAN_POINT('Ctrl Pts',(6.265419550659,2.56299179811782,78.4264697460267));
#202999=CARTESIAN_POINT('Ctrl Pts',(6.19319581895587,2.72701568533581,78.4348917953802));
#203000=CARTESIAN_POINT('Ctrl Pts',(6.12097017831694,2.89104390784724,78.4433140673357));
#203001=CARTESIAN_POINT('Ctrl Pts',(6.04222623217052,3.05219611391376,78.4517363392913));
#203002=CARTESIAN_POINT('Ctrl Pts',(5.95722575605389,3.20994552779455,78.4601586112468));
#203003=CARTESIAN_POINT('Ctrl Pts',(5.87221116653224,3.3677211342506,78.4685822816291));
#203004=CARTESIAN_POINT('Ctrl Pts',(5.78093813462091,3.52209252883972,78.4770059520113));
#203005=CARTESIAN_POINT('Ctrl Pts',(5.68371395501394,3.67255832868313,78.4854296223935));
#203006=CARTESIAN_POINT('Ctrl Pts',(5.58642398122583,3.82312595272429,78.4938589932969));
#203007=CARTESIAN_POINT('Ctrl Pts',(5.48317499339245,3.96978242025217,78.5022883642004));
#203008=CARTESIAN_POINT('Ctrl Pts',(5.37431768637092,4.11205525327187,78.5107177351038));
#203009=CARTESIAN_POINT('Ctrl Pts',(5.26542153821299,4.25437885034834,78.5191501136725));
#203010=CARTESIAN_POINT('Ctrl Pts',(5.15091328830068,4.3923154330655,78.5275824922412));
#203011=CARTESIAN_POINT('Ctrl Pts',(5.03118370671966,4.52542589258057,78.53601487081));
#203012=CARTESIAN_POINT('Ctrl Pts',(4.91134334234396,4.65865951588283,78.5444550516482));
#203013=CARTESIAN_POINT('Ctrl Pts',(4.78627222134462,4.78705785004376,78.5528952324864));
#203014=CARTESIAN_POINT('Ctrl Pts',(4.65639849937839,4.91021812295408,78.5613354133247));
#203015=CARTESIAN_POINT('Ctrl Pts',(4.58252279597567,4.98027503404259,78.5661364176143));
#203016=CARTESIAN_POINT('Ctrl Pts',(4.50709378487479,5.04863779999002,78.5709374219039));
#203017=CARTESIAN_POINT('Ctrl Pts',(4.43019502857091,5.11523811848732,78.5757384261936));
#203018=CARTESIAN_POINT('Ctrl Pts',(4.29981660656457,5.22815599711311,78.5838783154898));
#203019=CARTESIAN_POINT('Ctrl Pts',(4.16495145988663,5.33623038679091,78.5920182047859));
#203020=CARTESIAN_POINT('Ctrl Pts',(4.02599897334997,5.43908275967419,78.6001580940821));
#203021=CARTESIAN_POINT('Ctrl Pts',(3.87987442953529,5.54724387605595,78.6087181252104));
#203022=CARTESIAN_POINT('Ctrl Pts',(3.72922967744379,5.64962931001102,78.6172781563387));
#203023=CARTESIAN_POINT('Ctrl Pts',(3.57457188011347,5.74584413936735,78.625838187467));
#203024=CARTESIAN_POINT('Ctrl Pts',(3.42774035267585,5.837190134205,78.6339650486222));
#203025=CARTESIAN_POINT('Ctrl Pts',(3.27729224908201,5.92297436546511,78.6420919097774));
#203026=CARTESIAN_POINT('Ctrl Pts',(3.12369381422815,6.00290146137289,78.6502187709327));
#203027=CARTESIAN_POINT('Ctrl Pts',(3.11550686128119,6.0071616569537,78.6506519409057));
#203028=CARTESIAN_POINT('Ctrl Pts',(3.10731096502865,6.01140522269527,78.6510851108788));
#203029=CARTESIAN_POINT('Ctrl Pts',(3.09910619832128,6.01563211736943,78.6515182808518));
#203030=CARTESIAN_POINT('Origin',(0.,0.,4.30282021618968));
#203031=CARTESIAN_POINT('',(3.09910619832132,6.01563211736941,81.0456744569491));
#203032=CARTESIAN_POINT('',(3.0991061983213,6.01563211736942,80.6514477536361));
#203033=CARTESIAN_POINT('',(3.09910619832133,6.0156321173694,4.30282021618968));
#203034=CARTESIAN_POINT('',(-6.76705444505815,-9.75274733681431E-5,79.6970855167737));
#203035=CARTESIAN_POINT('Ctrl Pts',(-6.7669997635994,-0.00178869944433293,
79.69717978381));
#203036=CARTESIAN_POINT('Ctrl Pts',(-6.76695191418748,-0.182812381294488,
79.7056559560052));
#203037=CARTESIAN_POINT('Ctrl Pts',(-6.75963595610949,-0.363702158404258,
79.7141321282003));
#203038=CARTESIAN_POINT('Ctrl Pts',(-6.74510958551482,-0.543861820130901,
79.7226083003955));
#203039=CARTESIAN_POINT('Ctrl Pts',(-6.73055597313459,-0.7243593412588,
79.731100368238));
#203040=CARTESIAN_POINT('Ctrl Pts',(-6.7087649410064,-0.904123688643009,
79.7395924360806));
#203041=CARTESIAN_POINT('Ctrl Pts',(-6.6798459273942,-1.08256518800263,
79.7480845039232));
#203042=CARTESIAN_POINT('Ctrl Pts',(-6.6508989142315,-1.26117945541856,
79.7565847938333));
#203043=CARTESIAN_POINT('Ctrl Pts',(-6.61481021078436,-1.43846800435146,
79.7650850837434));
#203044=CARTESIAN_POINT('Ctrl Pts',(-6.57173980833,-1.61385404904248,79.7735853736534));
#203045=CARTESIAN_POINT('Ctrl Pts',(-6.52858281749277,-1.7895926883953,
79.7821027524765));
#203046=CARTESIAN_POINT('Ctrl Pts',(-6.47841614982349,-1.96342086604332,
79.7906201312995));
#203047=CARTESIAN_POINT('Ctrl Pts',(-6.42144951339353,-2.13477754038636,
79.7991375101225));
#203048=CARTESIAN_POINT('Ctrl Pts',(-6.3689139499044,-2.29280546705363,
79.8069923761276));
#203049=CARTESIAN_POINT('Ctrl Pts',(-6.31059574714776,-2.44873146061933,
79.8148472421327));
#203050=CARTESIAN_POINT('Ctrl Pts',(-6.24669448988538,-2.60213315378664,
79.8227021081378));
#203051=CARTESIAN_POINT('Ctrl Pts',(-6.17796775742869,-2.76711890800152,
79.8311501308769));
#203052=CARTESIAN_POINT('Ctrl Pts',(-6.10264102872985,-2.92952346695329,
79.8395981536161));
#203053=CARTESIAN_POINT('Ctrl Pts',(-6.02092964377854,-3.08880158389444,
79.8480461763553));
#203054=CARTESIAN_POINT('Ctrl Pts',(-5.93929308438736,-3.24793384509806,
79.8564864629873));
#203055=CARTESIAN_POINT('Ctrl Pts',(-5.85128367428993,-3.40394507573357,
79.8649267496193));
#203056=CARTESIAN_POINT('Ctrl Pts',(-5.7571644884972,-3.55631073619654,
79.8733670362513));
#203057=CARTESIAN_POINT('Ctrl Pts',(-5.66311700133879,-3.70856032670332,
79.881800893195));
#203058=CARTESIAN_POINT('Ctrl Pts',(-5.56296919158213,-3.8571696005349,
79.8902347501387));
#203059=CARTESIAN_POINT('Ctrl Pts',(-5.45702981818307,-4.00163898464877,
79.8986686070824));
#203060=CARTESIAN_POINT('Ctrl Pts',(-5.35115486142754,-4.14602052387062,
79.9070973358029));
#203061=CARTESIAN_POINT('Ctrl Pts',(-5.23949555883428,-4.2862669238484,
79.9155260645234));
#203062=CARTESIAN_POINT('Ctrl Pts',(-5.12240391870074,-4.42190763061366,
79.9239547932438));
#203063=CARTESIAN_POINT('Ctrl Pts',(-5.00536549543674,-4.55748669016151,
79.9323796911993));
#203064=CARTESIAN_POINT('Ctrl Pts',(-4.88289987527993,-4.68846397839237,
79.9408045891548));
#203065=CARTESIAN_POINT('Ctrl Pts',(-4.75539951864566,-4.81440177156671,
79.9492294871103));
#203066=CARTESIAN_POINT('Ctrl Pts',(-4.62792739080197,-4.94031168190461,
79.9576525197794));
#203067=CARTESIAN_POINT('Ctrl Pts',(-4.4954229841731,-5.06118408575414,
79.9660755524485));
#203068=CARTESIAN_POINT('Ctrl Pts',(-4.35831617956601,-5.17661753261077,
79.9744985851175));
#203069=CARTESIAN_POINT('Ctrl Pts',(-4.22122488844035,-5.29203791830211,
79.9829206647299));
#203070=CARTESIAN_POINT('Ctrl Pts',(-4.07953249253786,-5.40202035912182,
79.9913427443423));
#203071=CARTESIAN_POINT('Ctrl Pts',(-3.93370280031777,-5.50620298198061,
79.9997648239546));
#203072=CARTESIAN_POINT('Ctrl Pts',(-3.78786925182711,-5.61038835980909,
80.0081871262776));
#203073=CARTESIAN_POINT('Ctrl Pts',(-3.63789846045687,-5.70877342036208,
80.0166094286006));
#203074=CARTESIAN_POINT('Ctrl Pts',(-3.48428441719833,-5.80103879491155,
80.0250317309236));
#203075=CARTESIAN_POINT('Ctrl Pts',(-3.33064486720266,-5.89331948960107,
80.0334554317219));
#203076=CARTESIAN_POINT('Ctrl Pts',(-3.17336114538983,-5.97947830124503,
80.0418791325202));
#203077=CARTESIAN_POINT('Ctrl Pts',(-3.01295342430362,-6.05924093125344,
80.0503028333185));
#203078=CARTESIAN_POINT('Ctrl Pts',(-2.85243715384369,-6.13905753736398,
80.0587322345123));
#203079=CARTESIAN_POINT('Ctrl Pts',(-2.68879295864841,-6.21246916411479,
80.0671616357061));
#203080=CARTESIAN_POINT('Ctrl Pts',(-2.52256357802893,-6.27924852150334,
80.0755910368999));
#203081=CARTESIAN_POINT('Ctrl Pts',(-2.35627488699592,-6.34605170567442,
80.0840234456924));
#203082=CARTESIAN_POINT('Ctrl Pts',(-2.18739948304234,-6.40621778344014,
80.0924558544848));
#203083=CARTESIAN_POINT('Ctrl Pts',(-2.01649753443931,-6.45956861513215,
80.1008882632773));
#203084=CARTESIAN_POINT('Ctrl Pts',(-1.84543746237381,-6.51296880856813,
80.1093284739801));
#203085=CARTESIAN_POINT('Ctrl Pts',(-1.67234741967609,-6.55954106372498,
80.1177686846829));
#203086=CARTESIAN_POINT('Ctrl Pts',(-1.49780117594638,-6.5991575702762,
80.1262088953857));
#203087=CARTESIAN_POINT('Ctrl Pts',(-1.39852224456197,-6.62169076464089,
80.1310095435196));
#203088=CARTESIAN_POINT('Ctrl Pts',(-1.29877240465794,-6.64197461059254,
80.1358101916534));
#203089=CARTESIAN_POINT('Ctrl Pts',(-1.19865835252534,-6.65999302957002,
80.1406108397873));
#203090=CARTESIAN_POINT('Ctrl Pts',(-1.02891047137568,-6.69054406988795,
80.1487505547574));
#203091=CARTESIAN_POINT('Ctrl Pts',(-0.857776673190221,-6.71464022138195,
80.1568902697276));
#203092=CARTESIAN_POINT('Ctrl Pts',(-0.685793573818161,-6.73215984466425,
80.1650299846978));
#203093=CARTESIAN_POINT('Ctrl Pts',(-0.513960889834913,-6.74966414538893,
80.173162580722));
#203094=CARTESIAN_POINT('Ctrl Pts',(-0.341280745019906,-6.7606033299496,
80.1812951767462));
#203095=CARTESIAN_POINT('Ctrl Pts',(-0.16829978686302,-6.76490681249505,
80.1894277727704));
#203096=CARTESIAN_POINT('Ctrl Pts',(0.00456291223020466,-6.76920735294894,
80.1975548089156));
#203097=CARTESIAN_POINT('Ctrl Pts',(0.177725650628405,-6.76688121430026,
80.2056818450608));
#203098=CARTESIAN_POINT('Ctrl Pts',(0.350636859967422,-6.75790964666088,
80.213808881206));
#203099=CARTESIAN_POINT('Ctrl Pts',(0.523465414621692,-6.74894236759307,
80.221932032481));
#203100=CARTESIAN_POINT('Ctrl Pts',(0.696042314705396,-6.73333600419254,
80.230055183756));
#203101=CARTESIAN_POINT('Ctrl Pts',(0.867816211774448,-6.71112390159662,
80.238178335031));
#203102=CARTESIAN_POINT('Ctrl Pts',(1.03954183910317,-6.68891804076643,
80.2462992036402));
#203103=CARTESIAN_POINT('Ctrl Pts',(1.21046455009964,-6.66011018575533,
80.2544200722494));
#203104=CARTESIAN_POINT('Ctrl Pts',(1.38003837161272,-6.62478551297146,
80.2625409408585));
#203105=CARTESIAN_POINT('Ctrl Pts',(1.54962135755058,-6.58945893110573,
80.2706622483508));
#203106=CARTESIAN_POINT('Ctrl Pts',(1.71785494902696,-6.54761489864508,
80.2787835558431));
#203107=CARTESIAN_POINT('Ctrl Pts',(1.88420342907505,-6.49938969733789,
80.2869048633355));
#203108=CARTESIAN_POINT('Ctrl Pts',(1.97064389023608,-6.47433020392158,
80.2911249774276));
#203109=CARTESIAN_POINT('Ctrl Pts',(2.05657553629773,-6.44754849835256,
80.2953450915198));
#203110=CARTESIAN_POINT('Ctrl Pts',(2.14192478895576,-6.41906902895247,
80.299565205612));
#203111=CARTESIAN_POINT('Ctrl Pts',(2.32362962080415,-6.35843748225097,
80.3085496442289));
#203112=CARTESIAN_POINT('Ctrl Pts',(2.5026037720119,-6.29013824560206,80.3175340828458));
#203113=CARTESIAN_POINT('Ctrl Pts',(2.67823555666833,-6.21444633921619,
80.3265185214627));
#203114=CARTESIAN_POINT('Ctrl Pts',(2.85417047137847,-6.13862379308483,
80.3355184666883));
#203115=CARTESIAN_POINT('Ctrl Pts',(3.02675126992934,-6.05538316938616,
80.3445184119138));
#203116=CARTESIAN_POINT('Ctrl Pts',(3.19538935917925,-5.96504617276715,
80.3535183571394));
#203117=CARTESIAN_POINT('Ctrl Pts',(3.36442484848985,-5.87449629465679,
80.3625395109709));
#203118=CARTESIAN_POINT('Ctrl Pts',(3.52949882702707,-5.77681669733902,
80.3715606648025));
#203119=CARTESIAN_POINT('Ctrl Pts',(3.69004790648951,-5.67237476263799,
80.380581818634));
#203120=CARTESIAN_POINT('Ctrl Pts',(3.85076034593405,-5.56782655742679,
80.3896121515622));
#203121=CARTESIAN_POINT('Ctrl Pts',(4.0069384915457,-5.45650240403707,80.3986424844904));
#203122=CARTESIAN_POINT('Ctrl Pts',(4.15804947416783,-5.33881199990903,
80.4076728174186));
#203123=CARTESIAN_POINT('Ctrl Pts',(4.3093746845413,-5.22095474787759,80.4167159525131));
#203124=CARTESIAN_POINT('Ctrl Pts',(4.45561817943725,-5.09671334563674,
80.4257590876075));
#203125=CARTESIAN_POINT('Ctrl Pts',(4.5962798198103,-4.96653811200565,80.434802222702));
#203126=CARTESIAN_POINT('Ctrl Pts',(4.71925049106152,-4.85273497550414,
80.4427080056136));
#203127=CARTESIAN_POINT('Ctrl Pts',(4.83795553226584,-4.73439739749656,
80.4506137885252));
#203128=CARTESIAN_POINT('Ctrl Pts',(4.95208416706777,-4.61184902206011,
80.4585195714368));
#203129=CARTESIAN_POINT('Ctrl Pts',(5.07700530268695,-4.47771193845811,
80.4671729596158));
#203130=CARTESIAN_POINT('Ctrl Pts',(5.19655298764959,-4.33841063385692,
80.4758263477947));
#203131=CARTESIAN_POINT('Ctrl Pts',(5.31030630322139,-4.19439339666264,
80.4844797359737));
#203132=CARTESIAN_POINT('Ctrl Pts',(5.42395455953369,-4.05050916960719,
80.4931251321345));
#203133=CARTESIAN_POINT('Ctrl Pts',(5.53181893237289,-3.90191793484356,
80.5017705282954));
#203134=CARTESIAN_POINT('Ctrl Pts',(5.63351767492406,-3.74910224004603,
80.5104159244563));
#203135=CARTESIAN_POINT('Ctrl Pts',(5.73846433362059,-3.59140612539331,
80.5193374255234));
#203136=CARTESIAN_POINT('Ctrl Pts',(5.83684479616741,-3.42921148636016,
80.5282589265905));
#203137=CARTESIAN_POINT('Ctrl Pts',(5.92828549141526,-3.26308445068089,
80.5371804276576));
#203138=CARTESIAN_POINT('Ctrl Pts',(6.01672749005155,-3.10240536766239,
80.5458093579503));
#203139=CARTESIAN_POINT('Ctrl Pts',(6.09867748891445,-2.93804799946783,
80.554438288243));
#203140=CARTESIAN_POINT('Ctrl Pts',(6.17384187110355,-2.77055329322657,
80.5630672185357));
#203141=CARTESIAN_POINT('Ctrl Pts',(6.25282901592219,-2.59454002426963,
80.57213500499));
#203142=CARTESIAN_POINT('Ctrl Pts',(6.32432215343465,-2.41506226223281,
80.5812027914443));
#203143=CARTESIAN_POINT('Ctrl Pts',(6.38803548828711,-2.23277665707622,
80.5902705778986));
#203144=CARTESIAN_POINT('Ctrl Pts',(6.45174882313959,-2.05049105191957,
80.5993383643529));
#203145=CARTESIAN_POINT('Ctrl Pts',(6.50768219324855,-1.86539796067073,
80.6084061508072));
#203146=CARTESIAN_POINT('Ctrl Pts',(6.55560873764775,-1.67817850030218,
80.6174739372615));
#203147=CARTESIAN_POINT('Ctrl Pts',(6.600137690445,-1.50423133557365,80.6258988934118));
#203148=CARTESIAN_POINT('Ctrl Pts',(6.63773550657051,-1.32852498474019,
80.6343238495621));
#203149=CARTESIAN_POINT('Ctrl Pts',(6.66828457498004,-1.15163788887098,
80.6427488057124));
#203150=CARTESIAN_POINT('Ctrl Pts',(6.69884073412276,-0.974709735802147,
80.6511757173762));
#203151=CARTESIAN_POINT('Ctrl Pts',(6.7223448270092,-0.796600618026984,
80.65960262904));
#203152=CARTESIAN_POINT('Ctrl Pts',(6.7387307722117,-0.617896900499686,
80.6680295407039));
#203153=CARTESIAN_POINT('Ctrl Pts',(6.75512274316502,-0.439127466649144,
80.6764595512716));
#203154=CARTESIAN_POINT('Ctrl Pts',(6.76439131688234,-0.259763327125723,
80.6848895618393));
#203155=CARTESIAN_POINT('Ctrl Pts',(6.76652242990444,-0.0803940644580883,
80.6933195724071));
#203156=CARTESIAN_POINT('Ctrl Pts',(6.76865550606336,0.0991404294287381,
80.7017573485245));
#203157=CARTESIAN_POINT('Ctrl Pts',(6.76363798155557,0.278679724072522,
80.710195124642));
#203158=CARTESIAN_POINT('Ctrl Pts',(6.75150792001702,0.45763501390017,80.7186329007594));
#203159=CARTESIAN_POINT('Ctrl Pts',(6.73937149109012,0.636684242066582,
80.7270751060875));
#203160=CARTESIAN_POINT('Ctrl Pts',(6.72011510918539,0.815148524095448,
80.7355173114155));
#203161=CARTESIAN_POINT('Ctrl Pts',(6.6938285714976,0.992445492408714,80.7439595167436));
#203162=CARTESIAN_POINT('Ctrl Pts',(6.6675143029586,1.16992949927035,80.7524106281339));
#203163=CARTESIAN_POINT('Ctrl Pts',(6.63415511997451,1.34624340598651,80.7608617395242));
#203164=CARTESIAN_POINT('Ctrl Pts',(6.59389186493309,1.52081526608897,80.7693128509144));
#203165=CARTESIAN_POINT('Ctrl Pts',(6.58259192057082,1.56980912672804,80.771684668305));
#203166=CARTESIAN_POINT('Ctrl Pts',(6.57074847723041,1.61866586484798,80.7740564856957));
#203167=CARTESIAN_POINT('Ctrl Pts',(6.55836535019449,1.66737306364483,80.7764283030862));
#203168=CARTESIAN_POINT('Ctrl Pts',(6.51494345992729,1.83816664714307,80.7847451679758));
#203169=CARTESIAN_POINT('Ctrl Pts',(6.46480354114859,2.00742856727076,80.7930620328654));
#203170=CARTESIAN_POINT('Ctrl Pts',(6.408072719558,2.17460180742512,80.801378897755));
#203171=CARTESIAN_POINT('Ctrl Pts',(6.35139096768909,2.34163044991392,80.8096885689141));
#203172=CARTESIAN_POINT('Ctrl Pts',(6.28812978339475,2.5065736842362,80.8179982400731));
#203173=CARTESIAN_POINT('Ctrl Pts',(6.2184666305487,2.66888773925625,80.8263079112321));
#203174=CARTESIAN_POINT('Ctrl Pts',(6.14885095995114,2.83109116138101,80.8346119185379));
#203175=CARTESIAN_POINT('Ctrl Pts',(6.07284215340048,2.99066865668409,80.8429159258438));
#203176=CARTESIAN_POINT('Ctrl Pts',(5.99066656967292,3.14709438228398,80.8512199331496));
#203177=CARTESIAN_POINT('Ctrl Pts',(5.90853068887912,3.30344453117431,80.8595199283945));
#203178=CARTESIAN_POINT('Ctrl Pts',(5.82023413035652,3.45664563774094,80.8678199236393));
#203179=CARTESIAN_POINT('Ctrl Pts',(5.7260502758238,3.60619428743631,80.8761199188842));
#203180=CARTESIAN_POINT('Ctrl Pts',(5.6318908357205,3.75570417098675,80.8844177625963));
#203181=CARTESIAN_POINT('Ctrl Pts',(5.53184732523244,3.90156318976282,80.8927156063084));
#203182=CARTESIAN_POINT('Ctrl Pts',(5.42623788480702,4.04329462412586,80.9010134500205));
#203183=CARTESIAN_POINT('Ctrl Pts',(5.32063827053594,4.18501287145804,80.9093105216814));
#203184=CARTESIAN_POINT('Ctrl Pts',(5.20947396623572,4.32260402083056,80.9176075933423));
#203185=CARTESIAN_POINT('Ctrl Pts',(5.09310515724321,4.45562216275827,80.9259046650033));
#203186=CARTESIAN_POINT('Ctrl Pts',(4.97672783879117,4.5886500316266,80.9342023433869));
#203187=CARTESIAN_POINT('Ctrl Pts',(4.85514548688546,4.71710396536243,80.9425000217705));
#203188=CARTESIAN_POINT('Ctrl Pts',(4.72875723190401,4.84057269769968,80.9507977001541));
#203189=CARTESIAN_POINT('Ctrl Pts',(4.60228805140475,4.96412048620476,80.9591006914832));
#203190=CARTESIAN_POINT('Ctrl Pts',(4.47100706759699,5.08267645108949,80.9674036828124));
#203191=CARTESIAN_POINT('Ctrl Pts',(4.33534942909444,5.19586704291502,80.9757066741416));
#203192=CARTESIAN_POINT('Ctrl Pts',(4.19964792631716,5.30909423439887,80.9840123502049));
#203193=CARTESIAN_POINT('Ctrl Pts',(4.05956721992392,5.41695237756055,80.9923180262682));
#203194=CARTESIAN_POINT('Ctrl Pts',(3.91557410022157,5.51910939062401,81.0006237023315));
#203195=CARTESIAN_POINT('Ctrl Pts',(3.77143300909909,5.621371383136,81.0089379135435));
#203196=CARTESIAN_POINT('Ctrl Pts',(3.62337175921483,5.71792034346677,81.0172521247555));
#203197=CARTESIAN_POINT('Ctrl Pts',(3.471885496088,5.80846796513967,81.0255663359674));
#203198=CARTESIAN_POINT('Ctrl Pts',(3.3497610985411,5.8814651697565,81.0322690429613));
#203199=CARTESIAN_POINT('Ctrl Pts',(3.22541130420994,5.95056282308713,81.0389717499552));
#203200=CARTESIAN_POINT('Ctrl Pts',(3.09910619832132,6.01563211736941,81.0456744569491));
#203201=CARTESIAN_POINT('Ctrl Pts',(3.09910619832139,6.01563211736937,79.0457552630242));
#203202=CARTESIAN_POINT('Ctrl Pts',(2.93375330764829,6.10081787314652,79.0545047109265));
#203203=CARTESIAN_POINT('Ctrl Pts',(2.7648862784307,6.17918207037039,79.0632541588288));
#203204=CARTESIAN_POINT('Ctrl Pts',(2.59307866646699,6.25045854553998,79.0720036067311));
#203205=CARTESIAN_POINT('Ctrl Pts',(2.42127244185365,6.32173444515041,79.0807529839814));
#203206=CARTESIAN_POINT('Ctrl Pts',(2.24652594672445,6.38592262741845,79.0895023612317));
#203207=CARTESIAN_POINT('Ctrl Pts',(2.06943269687093,6.44280508110571,79.098251738482));
#203208=CARTESIAN_POINT('Ctrl Pts',(1.89234081822047,6.49968709436175,79.1070010479874));
#203209=CARTESIAN_POINT('Ctrl Pts',(1.71290249405556,6.54926340459553,79.1157503574927));
#203210=CARTESIAN_POINT('Ctrl Pts',(1.53172716625023,6.59136563150392,79.1244996669981));
#203211=CARTESIAN_POINT('Ctrl Pts',(1.350553181073,6.63346754640717,79.1332489116653));
#203212=CARTESIAN_POINT('Ctrl Pts',(1.16764249714387,6.66809542395782,79.1419981563326));
#203213=CARTESIAN_POINT('Ctrl Pts',(0.983616340614045,6.69513165624673,
79.1507474009998));
#203214=CARTESIAN_POINT('Ctrl Pts',(0.799591486713628,6.72216769715963,
79.1594965837355));
#203215=CARTESIAN_POINT('Ctrl Pts',(0.614451459526594,6.74161215869372,
79.1682457664712));
#203216=CARTESIAN_POINT('Ctrl Pts',(0.428825047910263,6.75339900185712,
79.1769949492069));
#203217=CARTESIAN_POINT('Ctrl Pts',(0.243199888597033,6.76518576550221,
79.1857440729174));
#203218=CARTESIAN_POINT('Ctrl Pts',(0.0570886373919136,6.76931499599834,
79.194493196628));
#203219=CARTESIAN_POINT('Ctrl Pts',(-0.128876626811146,6.76577266947847,
79.2032423203385));
#203220=CARTESIAN_POINT('Ctrl Pts',(-0.314840698188063,6.76223036567993,
79.21199138793));
#203221=CARTESIAN_POINT('Ctrl Pts',(-0.500658497951067,6.75101660879224,
79.2207404555216));
#203222=CARTESIAN_POINT('Ctrl Pts',(-0.68569895192594,6.73216948296221,
79.2294895231131));
#203223=CARTESIAN_POINT('Ctrl Pts',(-0.870738280459641,6.71332247176296,
79.2382385374917));
#203224=CARTESIAN_POINT('Ctrl Pts',(-1.05499998761236,6.68684221356189,
79.2469875518702));
#203225=CARTESIAN_POINT('Ctrl Pts',(-1.23785829161412,6.65281863948524,
79.2557365662487));
#203226=CARTESIAN_POINT('Ctrl Pts',(-1.43007412917395,6.61705395368863,
79.2649332999479));
#203227=CARTESIAN_POINT('Ctrl Pts',(-1.62073882535782,6.57295372727792,
79.2741300336471));
#203228=CARTESIAN_POINT('Ctrl Pts',(-1.80913696091504,6.52068343478282,
79.2833267673463));
#203229=CARTESIAN_POINT('Ctrl Pts',(-1.98838356186099,6.47095219815203,
79.2920767650599));
#203230=CARTESIAN_POINT('Ctrl Pts',(-2.16557827572516,6.41382586850896,
79.3008267627736));
#203231=CARTESIAN_POINT('Ctrl Pts',(-2.3401191862168,6.34949849943285,79.3095767604873));
#203232=CARTESIAN_POINT('Ctrl Pts',(-2.51465655691069,6.28517243495562,
79.3183265807456));
#203233=CARTESIAN_POINT('Ctrl Pts',(-2.6865399629529,6.21364572242391,79.3270764010039));
#203234=CARTESIAN_POINT('Ctrl Pts',(-2.85518555379941,6.13516132252243,
79.3358262212622));
#203235=CARTESIAN_POINT('Ctrl Pts',(-3.02382794858646,6.05667841000528,
79.3445758756997));
#203236=CARTESIAN_POINT('Ctrl Pts',(-3.18923239109243,5.97123819492101,
79.3533255301372));
#203237=CARTESIAN_POINT('Ctrl Pts',(-3.35083705967665,5.87913088810732,
79.3620751845747));
#203238=CARTESIAN_POINT('Ctrl Pts',(-3.51243888042359,5.78702520443127,
79.3708246848237));
#203239=CARTESIAN_POINT('Ctrl Pts',(-3.67024081223643,5.68825280605813,
79.3795741850726));
#203240=CARTESIAN_POINT('Ctrl Pts',(-3.82370687544348,5.58314917682541,
79.3883236853216));
#203241=CARTESIAN_POINT('Ctrl Pts',(-3.97717043817767,5.47804726008056,
79.397073043012));
#203242=CARTESIAN_POINT('Ctrl Pts',(-4.12629803722418,5.36661448084269,
79.4058224007025));
#203243=CARTESIAN_POINT('Ctrl Pts',(-4.2705831720687,5.24922931204607,79.4145717583929));
#203244=CARTESIAN_POINT('Ctrl Pts',(-4.41486614774809,5.13184589986813,
79.423320985153));
#203245=CARTESIAN_POINT('Ctrl Pts',(-4.55430658194399,5.00851045723048,
79.4320702119131));
#203246=CARTESIAN_POINT('Ctrl Pts',(-4.68843089001841,4.87964187103123,
79.4408194386732));
#203247=CARTESIAN_POINT('Ctrl Pts',(-4.82255336917833,4.75077504207964,
79.4495685461291));
#203248=CARTESIAN_POINT('Ctrl Pts',(-4.95135966065131,4.61637541908097,
79.458317653585));
#203249=CARTESIAN_POINT('Ctrl Pts',(-5.07441230869241,4.47689945401848,
79.467066761041));
#203250=CARTESIAN_POINT('Ctrl Pts',(-5.19746344226413,4.3374252055552,79.4758157608173));
#203251=CARTESIAN_POINT('Ctrl Pts',(-5.31476088454763,4.19287495491341,
79.4845647605937));
#203252=CARTESIAN_POINT('Ctrl Pts',(-5.4259062762885,4.04373961586711,79.4933137603701));
#203253=CARTESIAN_POINT('Ctrl Pts',(-5.53706380672667,3.89458798906735,
79.5020637156648));
#203254=CARTESIAN_POINT('Ctrl Pts',(-5.64206777071866,3.74085050155281,
79.5108136709595));
#203255=CARTESIAN_POINT('Ctrl Pts',(-5.74056148164012,3.58304938223153,
79.5195636262542));
#203256=CARTESIAN_POINT('Ctrl Pts',(-5.83905138951886,3.42525435593277,
79.5283132436953));
#203257=CARTESIAN_POINT('Ctrl Pts',(-5.93103139557654,3.26339625497181,
79.5370628611363));
#203258=CARTESIAN_POINT('Ctrl Pts',(-6.01618907820846,3.09802485065005,
79.5458124785775));
#203259=CARTESIAN_POINT('Ctrl Pts',(-6.10134392544988,2.93265895249632,
79.5545618046933));
#203260=CARTESIAN_POINT('Ctrl Pts',(-6.1796767726184,2.76378023986017,79.5633111308092));
#203261=CARTESIAN_POINT('Ctrl Pts',(-6.25092157009235,2.59196229227089,
79.5720604569251));
#203262=CARTESIAN_POINT('Ctrl Pts',(-6.32216437407757,2.4201491522908,79.5808095382275));
#203263=CARTESIAN_POINT('Ctrl Pts',(-6.38631941548919,2.24539720662856,
79.58955861953));
#203264=CARTESIAN_POINT('Ctrl Pts',(-6.4431688103753,2.06829994947709,79.5983077008324));
#203265=CARTESIAN_POINT('Ctrl Pts',(-6.50002334524564,1.89118668024476,
79.6070575731748));
#203266=CARTESIAN_POINT('Ctrl Pts',(-6.54957082411089,1.71172794807731,
79.6158074455171));
#203267=CARTESIAN_POINT('Ctrl Pts',(-6.59164294296076,1.53053334250371,
79.6245573178595));
#203268=CARTESIAN_POINT('Ctrl Pts',(-6.63371214082133,1.34935131693608,
79.6333065827144));
#203269=CARTESIAN_POINT('Ctrl Pts',(-6.66830695239693,1.16643393829749,
79.6420558475693));
#203270=CARTESIAN_POINT('Ctrl Pts',(-6.69530988153994,0.982402458340616,
79.6508051124242));
#203271=CARTESIAN_POINT('Ctrl Pts',(-6.72231419690488,0.798361530946668,
79.6595548264313));
#203272=CARTESIAN_POINT('Ctrl Pts',(-6.74172580829282,0.613206671362071,
79.6683045404383));
#203273=CARTESIAN_POINT('Ctrl Pts',(-6.75347878028182,0.427566795112976,
79.6770542544453));
#203274=CARTESIAN_POINT('Ctrl Pts',(-6.76248992368213,0.285234494205442,
79.6837627642335));
#203275=CARTESIAN_POINT('Ctrl Pts',(-6.76699999999994,0.142617266092895,
79.6904712740218));
#203276=CARTESIAN_POINT('Ctrl Pts',(-6.767,2.79684983589873E-12,79.69717978381));
#203277=CARTESIAN_POINT('',(-6.76699963750513,0.00221495044038298,79.3028202161514));
#203278=CARTESIAN_POINT('Ctrl Pts',(3.09910619832128,6.01563211736943,78.6515182808518));
#203279=CARTESIAN_POINT('Ctrl Pts',(2.94524964427127,6.09489524234211,78.6596411247725));
#203280=CARTESIAN_POINT('Ctrl Pts',(2.78827182354791,6.16829232074604,78.6677639686933));
#203281=CARTESIAN_POINT('Ctrl Pts',(2.62866640743604,6.23557550819628,78.675886812614));
#203282=CARTESIAN_POINT('Ctrl Pts',(2.46910295246842,6.30284100652542,78.6840075209942));
#203283=CARTESIAN_POINT('Ctrl Pts',(2.30691361570877,6.36399567440877,78.6921282293744));
#203284=CARTESIAN_POINT('Ctrl Pts',(2.14261340044974,6.41883921096433,78.7002489377547));
#203285=CARTESIAN_POINT('Ctrl Pts',(1.97830368986549,6.47368591706666,78.7083701154512));
#203286=CARTESIAN_POINT('Ctrl Pts',(1.8118832036047,6.52222064474138,78.7164912931477));
#203287=CARTESIAN_POINT('Ctrl Pts',(1.64388366608236,6.56429245938872,78.7246124708442));
#203288=CARTESIAN_POINT('Ctrl Pts',(1.57437448245534,6.58169951617574,78.7279725779022));
#203289=CARTESIAN_POINT('Ctrl Pts',(1.50459515420102,6.59800080675089,78.7313326849603));
#203290=CARTESIAN_POINT('Ctrl Pts',(1.43458395721529,6.6131881773998,78.7346927920183));
#203291=CARTESIAN_POINT('Ctrl Pts',(1.2473838437369,6.65379707470939,78.7436772466434));
#203292=CARTESIAN_POINT('Ctrl Pts',(1.05861809858462,6.68641852117337,78.7526617012684));
#203293=CARTESIAN_POINT('Ctrl Pts',(0.868953103732096,6.71097679205601,
78.7616461558935));
#203294=CARTESIAN_POINT('Ctrl Pts',(0.678960741941393,6.73557745118194,
78.7706461179315));
#203295=CARTESIAN_POINT('Ctrl Pts',(0.488066265174348,6.75208708718582,
78.7796460799695));
#203296=CARTESIAN_POINT('Ctrl Pts',(0.296940026432046,6.76048190743105,
78.7886460420075));
#203297=CARTESIAN_POINT('Ctrl Pts',(0.105363375775685,6.76889651107745,
78.7976672135359));
#203298=CARTESIAN_POINT('Ctrl Pts',(-0.0864458899679037,6.7691580253438,
78.8066883850644));
#203299=CARTESIAN_POINT('Ctrl Pts',(-0.277815777047764,6.76129480159114,
78.8157095565928));
#203300=CARTESIAN_POINT('Ctrl Pts',(-0.469380392114852,6.75342357663328,
78.8247399075935));
#203301=CARTESIAN_POINT('Ctrl Pts',(-0.660504497049267,6.73741111340131,
78.8337702585942));
#203302=CARTESIAN_POINT('Ctrl Pts',(-0.850520743133508,6.71333772914037,
78.8428006095949));
#203303=CARTESIAN_POINT('Ctrl Pts',(-1.04080637744029,6.68923021576506,
78.8518437630284));
#203304=CARTESIAN_POINT('Ctrl Pts',(-1.22998077520956,6.65703896072662,
78.8608869164618));
#203305=CARTESIAN_POINT('Ctrl Pts',(-1.41738399877022,6.61689591878474,
78.8699300698952));
#203306=CARTESIAN_POINT('Ctrl Pts',(-1.58121544568112,6.58180211132623,
78.8778357658778));
#203307=CARTESIAN_POINT('Ctrl Pts',(-1.74369331824502,6.54063188396889,
78.8857414618605));
#203308=CARTESIAN_POINT('Ctrl Pts',(-1.90438519169257,6.49350491196103,
78.8936471578431));
#203309=CARTESIAN_POINT('Ctrl Pts',(-2.08027441159858,6.44192093222917,
78.9023005307198));
#203310=CARTESIAN_POINT('Ctrl Pts',(-2.25417886235738,6.38315339922036,
78.9109539035965));
#203311=CARTESIAN_POINT('Ctrl Pts',(-2.42550777024041,6.31737295531168,
78.9196072764732));
#203312=CARTESIAN_POINT('Ctrl Pts',(-2.59667844159213,6.25165326512752,
78.9282526572386));
#203313=CARTESIAN_POINT('Ctrl Pts',(-2.76527803165542,6.17893369116949,
78.936898038004));
#203314=CARTESIAN_POINT('Ctrl Pts',(-2.93073196446853,6.09943433052955,
78.9455434187693));
#203315=CARTESIAN_POINT('Ctrl Pts',(-3.10147039091569,6.01739581075286,
78.9544649275109));
#203316=CARTESIAN_POINT('Ctrl Pts',(-3.26885857849907,5.92813733407461,
78.9633864362524));
#203317=CARTESIAN_POINT('Ctrl Pts',(-3.43228631538297,5.83195504520009,
78.972307944994));
#203318=CARTESIAN_POINT('Ctrl Pts',(-3.59035420242436,5.73892719409548,
78.980936859907));
#203319=CARTESIAN_POINT('Ctrl Pts',(-3.74471699772877,5.63942263458006,
78.98956577482));
#203320=CARTESIAN_POINT('Ctrl Pts',(-3.89484610130794,5.53375666677948,
78.998194689733));
#203321=CARTESIAN_POINT('Ctrl Pts',(-4.05261119092361,5.42271623236701,
79.0072624953888));
#203322=CARTESIAN_POINT('Ctrl Pts',(-4.20570038323733,5.30487142910128,
79.0163303010447));
#203323=CARTESIAN_POINT('Ctrl Pts',(-4.35353273977685,5.18064104949292,
79.0253981067005));
#203324=CARTESIAN_POINT('Ctrl Pts',(-4.50136509631636,5.05641066988457,
79.0344659123563));
#203325=CARTESIAN_POINT('Ctrl Pts',(-4.64394029545781,4.92579493822377,
79.0435337180121));
#203326=CARTESIAN_POINT('Ctrl Pts',(-4.78071558962921,4.78926376921091,
79.0526015236679));
#203327=CARTESIAN_POINT('Ctrl Pts',(-4.90779449631454,4.66241168096109,
79.0610264869316));
#203328=CARTESIAN_POINT('Ctrl Pts',(-5.02981110075196,4.53050898203097,
79.0694514501953));
#203329=CARTESIAN_POINT('Ctrl Pts',(-5.14636901431176,4.39399305513013,
79.077876413459));
#203330=CARTESIAN_POINT('Ctrl Pts',(-5.26295398405147,4.25744543926569,
79.0863033323799));
#203331=CARTESIAN_POINT('Ctrl Pts',(-5.37407752116965,4.11628271249826,
79.0947302513008));
#203332=CARTESIAN_POINT('Ctrl Pts',(-5.47938350389405,3.97097537353907,
79.1031571702217));
#203333=CARTESIAN_POINT('Ctrl Pts',(-5.58472821329221,3.82561459725595,
79.1115871881739));
#203334=CARTESIAN_POINT('Ctrl Pts',(-5.68425090798292,3.67610643805485,
79.1200172061261));
#203335=CARTESIAN_POINT('Ctrl Pts',(-5.77763855521455,3.52295071286816,
79.1284472240783));
#203336=CARTESIAN_POINT('Ctrl Pts',(-5.87111223070906,3.36965390134536,
79.1368850077236));
#203337=CARTESIAN_POINT('Ctrl Pts',(-5.95843939463506,3.21270309393495,
79.1453227913688));
#203338=CARTESIAN_POINT('Ctrl Pts',(-6.03935223600749,3.05262404652643,
79.153760575014));
#203339=CARTESIAN_POINT('Ctrl Pts',(-6.12030755138395,2.89246096798033,
79.1622027879495));
#203340=CARTESIAN_POINT('Ctrl Pts',(-6.19484168647654,2.72916667353424,
79.1706450008849));
#203341=CARTESIAN_POINT('Ctrl Pts',(-6.26273460320383,2.56328778911644,
79.1790872138204));
#203342=CARTESIAN_POINT('Ctrl Pts',(-6.3306991437123,2.39723391040623,79.1875383328869));
#203343=CARTESIAN_POINT('Ctrl Pts',(-6.39200835218371,2.22859030456305,
79.1959894519534));
#203344=CARTESIAN_POINT('Ctrl Pts',(-6.44649140458477,2.057920691041,79.2044405710198));
#203345=CARTESIAN_POINT('Ctrl Pts',(-6.46178185571332,2.01002294541771,
79.2068123438441));
#203346=CARTESIAN_POINT('Ctrl Pts',(-6.47653496985489,1.96196570363734,
79.2091841166684));
#203347=CARTESIAN_POINT('Ctrl Pts',(-6.49074769014697,1.91376158986739,
79.2115558894926));
#203348=CARTESIAN_POINT('Ctrl Pts',(-6.54928341862,1.7152307768398,79.2213241426621));
#203349=CARTESIAN_POINT('Ctrl Pts',(-6.59872468730928,1.51395107279027,
79.2310923958316));
#203350=CARTESIAN_POINT('Ctrl Pts',(-6.63885430811011,1.31068778726586,
79.2408606490011));
#203351=CARTESIAN_POINT('Ctrl Pts',(-6.67885051141634,1.10810028381354,
79.2505964260137));
#203352=CARTESIAN_POINT('Ctrl Pts',(-6.70959683203901,0.903542416313194,
79.2603322030262));
#203353=CARTESIAN_POINT('Ctrl Pts',(-6.73092711602759,0.697788763684628,
79.2700679800387));
#203354=CARTESIAN_POINT('Ctrl Pts',(-6.75211763844694,0.493383262509683,
79.2797399657078));
#203355=CARTESIAN_POINT('Ctrl Pts',(-6.76401506195236,0.287797655196327,
79.2894119513768));
#203356=CARTESIAN_POINT('Ctrl Pts',(-6.76650549202476,0.0818072515051274,
79.2990839370458));
#203357=CARTESIAN_POINT('Ctrl Pts',(-6.76682617563486,0.0552826174535358,
79.3003293634144));
#203358=CARTESIAN_POINT('Ctrl Pts',(-6.76699095172329,0.0287512925092576,
79.3015747897828));
#203359=CARTESIAN_POINT('Ctrl Pts',(-6.76699963750513,0.00221495044041987,
79.3028202161514));
#203360=CARTESIAN_POINT('Ctrl Pts',(-6.7669996375054,0.00221494962268042,
79.3028202161898));
#203361=CARTESIAN_POINT('Ctrl Pts',(-6.76705768574337,-0.175131027606415,
79.3111435697184));
#203362=CARTESIAN_POINT('Ctrl Pts',(-6.7601397171255,-0.352517298753123,
79.319466923247));
#203363=CARTESIAN_POINT('Ctrl Pts',(-6.74626262667905,-0.529367142797431,
79.3277902767756));
#203364=CARTESIAN_POINT('Ctrl Pts',(-6.7322525829915,-0.707911344895013,
79.3361933744575));
#203365=CARTESIAN_POINT('Ctrl Pts',(-6.71114937080536,-0.88590843078606,
79.3445964721395));
#203366=CARTESIAN_POINT('Ctrl Pts',(-6.6830241242902,-1.0627688150088,79.3529995698214));
#203367=CARTESIAN_POINT('Ctrl Pts',(-6.655157240719,-1.23800453188821,79.3613254753246));
#203368=CARTESIAN_POINT('Ctrl Pts',(-6.62039688252329,-1.41212400484039,
79.3696513808278));
#203369=CARTESIAN_POINT('Ctrl Pts',(-6.5788638914875,-1.58456268329212,
79.3779772863311));
#203370=CARTESIAN_POINT('Ctrl Pts',(-6.53731874143279,-1.75705184414598,
79.3863056292904));
#203371=CARTESIAN_POINT('Ctrl Pts',(-6.488997086651,-1.92785889472785,79.3946339722497));
#203372=CARTESIAN_POINT('Ctrl Pts',(-6.43407015601563,-2.09643273859884,
79.402962315209));
#203373=CARTESIAN_POINT('Ctrl Pts',(-6.37911835254023,-2.26508291861684,
79.4112944295341));
#203374=CARTESIAN_POINT('Ctrl Pts',(-6.31755541741858,-2.43149754880781,
79.4196265438591));
#203375=CARTESIAN_POINT('Ctrl Pts',(-6.24960146698585,-2.59514363838466,
79.4279586581841));
#203376=CARTESIAN_POINT('Ctrl Pts',(-6.18061406368497,-2.76127847982298,
79.4364174884306));
#203377=CARTESIAN_POINT('Ctrl Pts',(-6.10503982736518,-2.92455955110825,
79.4448763186771));
#203378=CARTESIAN_POINT('Ctrl Pts',(-6.02315802361306,-3.08445399099835,
79.4533351489236));
#203379=CARTESIAN_POINT('Ctrl Pts',(-5.9423486357773,-3.24225427401333,
79.4616831928443));
#203380=CARTESIAN_POINT('Ctrl Pts',(-5.85539611981876,-3.39675582751105,
79.4700312367649));
#203381=CARTESIAN_POINT('Ctrl Pts',(-5.76261325153627,-3.54747480797519,
79.4783792806856));
#203382=CARTESIAN_POINT('Ctrl Pts',(-5.66798341050639,-3.7011940605217,
79.486893504095));
#203383=CARTESIAN_POINT('Ctrl Pts',(-5.56728888392529,-3.85097825478445,
79.4954077275044));
#203384=CARTESIAN_POINT('Ctrl Pts',(-5.46090525826983,-3.99634867850654,
79.5039219509138));
#203385=CARTESIAN_POINT('Ctrl Pts',(-5.35452163261437,-4.14171910222862,
79.5124361743232));
#203386=CARTESIAN_POINT('Ctrl Pts',(-5.24244918545136,-4.2826754981324,
79.5209503977326));
#203387=CARTESIAN_POINT('Ctrl Pts',(-5.12510375959006,-4.41877816295816,
79.529464621142));
#203388=CARTESIAN_POINT('Ctrl Pts',(-5.01388286691539,-4.54777731027228,
79.5375344672487));
#203389=CARTESIAN_POINT('Ctrl Pts',(-4.8975829761562,-4.67281272641128,
79.5456043133554));
#203390=CARTESIAN_POINT('Ctrl Pts',(-4.77652078403894,-4.79344742326898,
79.5536741594621));
#203391=CARTESIAN_POINT('Ctrl Pts',(-4.6556109035564,-4.91393034633537,
79.5617338526761));
#203392=CARTESIAN_POINT('Ctrl Pts',(-4.52995090422578,-5.03002330656301,
79.5697935458901));
#203393=CARTESIAN_POINT('Ctrl Pts',(-4.39989884924542,-5.14132075603233,
79.577853239104));
#203394=CARTESIAN_POINT('Ctrl Pts',(-4.26998187397997,-5.25250260542331,
79.5859045610464));
#203395=CARTESIAN_POINT('Ctrl Pts',(-4.13568220223781,-5.35889861557442,
79.5939558829889));
#203396=CARTESIAN_POINT('Ctrl Pts',(-3.99739593178139,-5.46013871294289,
79.6020072049313));
#203397=CARTESIAN_POINT('Ctrl Pts',(-3.85922299034842,-5.56129584154424,
79.610051928616));
#203398=CARTESIAN_POINT('Ctrl Pts',(-3.71707025231958,-5.65730524799441,
79.6180966523007));
#203399=CARTESIAN_POINT('Ctrl Pts',(-3.57136811959561,-5.74783600621453,
79.6261413759855));
#203400=CARTESIAN_POINT('Ctrl Pts',(-3.42575349911879,-5.83831238945783,
79.6341812678133));
#203401=CARTESIAN_POINT('Ctrl Pts',(-3.27659404391417,-5.92331647864713,
79.6422211596412));
#203402=CARTESIAN_POINT('Ctrl Pts',(-3.12435037074722,-6.0025597673669,
79.6502610514691));
#203403=CARTESIAN_POINT('Ctrl Pts',(-2.96882847742748,-6.08350937951311,
79.6584740640242));
#203404=CARTESIAN_POINT('Ctrl Pts',(-2.81008835775638,-6.15844704994757,
79.6666870765793));
#203405=CARTESIAN_POINT('Ctrl Pts',(-2.64864941067012,-6.22711372140873,
79.6749000891344));
#203406=CARTESIAN_POINT('Ctrl Pts',(-2.49066854835798,-6.29430952617163,
79.6829371757796));
#203407=CARTESIAN_POINT('Ctrl Pts',(-2.33010367007658,-6.35550012483698,
79.6909742624247));
#203408=CARTESIAN_POINT('Ctrl Pts',(-2.16746305262348,-6.41049084825118,
79.6990113490699));
#203409=CARTESIAN_POINT('Ctrl Pts',(-2.00480686971419,-6.46548683453089,
79.7070492049013));
#203410=CARTESIAN_POINT('Ctrl Pts',(-1.84007490598416,-6.51428164429123,
79.7150870607326));
#203411=CARTESIAN_POINT('Ctrl Pts',(-1.6737916435351,-6.55673017090318,
79.723124916564));
#203412=CARTESIAN_POINT('Ctrl Pts',(-1.50745952074804,-6.59919117050447,
79.7311651342227));
#203413=CARTESIAN_POINT('Ctrl Pts',(-1.33957555373981,-6.63530208281808,
79.7392053518814));
#203414=CARTESIAN_POINT('Ctrl Pts',(-1.17067533445569,-6.66496873670815,
79.7472455695401));
#203415=CARTESIAN_POINT('Ctrl Pts',(-0.995393962881926,-6.69575621469898,
79.7555895514778));
#203416=CARTESIAN_POINT('Ctrl Pts',(-0.819018488221558,-6.71960291021645,
79.7639335334154));
#203417=CARTESIAN_POINT('Ctrl Pts',(-0.64215326736394,-6.73646258664099,
79.772277515353));
#203418=CARTESIAN_POINT('Ctrl Pts',(-0.471430162501238,-6.75273676588449,
79.780331730288));
#203419=CARTESIAN_POINT('Ctrl Pts',(-0.300251127745629,-6.76250112163038,
79.788385945223));
#203420=CARTESIAN_POINT('Ctrl Pts',(-0.1291590707959,-6.76576728349647,
79.7964401601579));
#203421=CARTESIAN_POINT('Ctrl Pts',(0.0420610202531481,-6.76903588954436,
79.8045004023403));
#203422=CARTESIAN_POINT('Ctrl Pts',(0.21319363292898,-6.76579662622857,
79.8125606445227));
#203423=CARTESIAN_POINT('Ctrl Pts',(0.383700933640461,-6.75611297962989,
79.8206208867051));
#203424=CARTESIAN_POINT('Ctrl Pts',(0.55444661522343,-6.74641579463076,
79.8286923976575));
#203425=CARTESIAN_POINT('Ctrl Pts',(0.724564872197164,-6.73025628546016,
79.8367639086099));
#203426=CARTESIAN_POINT('Ctrl Pts',(0.893527435234065,-6.70774908016721,
79.8448354195623));
#203427=CARTESIAN_POINT('Ctrl Pts',(0.911236457571604,-6.70539009250672,
79.8456813973054));
#203428=CARTESIAN_POINT('Ctrl Pts',(0.928932797974419,-6.70296141928674,
79.8465273750486));
#203429=CARTESIAN_POINT('Ctrl Pts',(0.946615858222378,-6.70046322405861,
79.8473733527917));
#203430=CARTESIAN_POINT('Ctrl Pts',(1.11862785791944,-6.67616202557831,
79.8556026027777));
#203431=CARTESIAN_POINT('Ctrl Pts',(1.2899562381074,-6.6451971130301,79.8638318527636));
#203432=CARTESIAN_POINT('Ctrl Pts',(1.46004516960714,-6.60761357092762,
79.8720611027496));
#203433=CARTESIAN_POINT('Ctrl Pts',(1.62993166766089,-6.57007475934273,
79.8802805585918));
#203434=CARTESIAN_POINT('Ctrl Pts',(1.79858130760347,-6.52593308004909,
79.8885000144341));
#203435=CARTESIAN_POINT('Ctrl Pts',(1.96544378896078,-6.47528529969418,
79.8967194702764));
#203436=CARTESIAN_POINT('Ctrl Pts',(2.13214118695583,-6.42468762710348,
79.9049307943002));
#203437=CARTESIAN_POINT('Ctrl Pts',(2.29705460668081,-6.36759677547963,
79.9131421183241));
#203438=CARTESIAN_POINT('Ctrl Pts',(2.45964425939344,-6.30416046093633,
79.9213534423479));
#203439=CARTESIAN_POINT('Ctrl Pts',(2.62210569620719,-6.24077417137282,
79.9295582910378));
#203440=CARTESIAN_POINT('Ctrl Pts',(2.78224668328266,-6.17105251532309,
79.9377631397277));
#203441=CARTESIAN_POINT('Ctrl Pts',(2.93954283066635,-6.09519293760895,
79.9459679884176));
#203442=CARTESIAN_POINT('Ctrl Pts',(3.09674650590379,-6.01937795665121,
79.9541680135948));
#203443=CARTESIAN_POINT('Ctrl Pts',(3.25110835094132,-5.93743239769007,
79.962368038772));
#203444=CARTESIAN_POINT('Ctrl Pts',(3.40212411776653,-5.84960173749558,
79.9705680639492));
#203445=CARTESIAN_POINT('Ctrl Pts',(3.55309617723402,-5.76179649746857,
79.9787657158548));
#203446=CARTESIAN_POINT('Ctrl Pts',(3.70072377584982,-5.66810972558389,
79.9869633677604));
#203447=CARTESIAN_POINT('Ctrl Pts',(3.84452722089665,-5.5688328622598,79.9951610196659));
#203448=CARTESIAN_POINT('Ctrl Pts',(3.98831140979427,-5.46956929270689,
80.0033575738564));
#203449=CARTESIAN_POINT('Ctrl Pts',(4.12827216937939,-5.36471732559827,
80.011554128047));
#203450=CARTESIAN_POINT('Ctrl Pts',(4.26395876097249,-5.25461175394776,
80.0197506822375));
#203451=CARTESIAN_POINT('Ctrl Pts',(4.39965185465598,-5.14450090604725,
80.0279476292062));
#203452=CARTESIAN_POINT('Ctrl Pts',(4.53107009367345,-5.02913617807617,
80.0361445761749));
#203453=CARTESIAN_POINT('Ctrl Pts',(4.65779577200375,-4.90889270063056,
80.0443415231436));
#203454=CARTESIAN_POINT('Ctrl Pts',(4.78455056498328,-4.78862159779195,
80.0525403533237));
#203455=CARTESIAN_POINT('Ctrl Pts',(4.9066103898475,-4.6634697599225,80.0607391835038));
#203456=CARTESIAN_POINT('Ctrl Pts',(5.0235943304235,-4.53384924797207,80.0689380136838));
#203457=CARTESIAN_POINT('Ctrl Pts',(5.14068906973142,-4.40410596884279,
80.0771446092032));
#203458=CARTESIAN_POINT('Ctrl Pts',(5.25269807911143,-4.2698858263462,80.0853512047225));
#203459=CARTESIAN_POINT('Ctrl Pts',(5.35928009382647,-4.13163477039239,
80.0935578002418));
#203460=CARTESIAN_POINT('Ctrl Pts',(5.46591369484532,-3.99331680013794,
80.1017683678002));
#203461=CARTESIAN_POINT('Ctrl Pts',(5.56711485645141,-3.8509643188439,80.1099789353586));
#203462=CARTESIAN_POINT('Ctrl Pts',(5.66258569484486,-3.70505225989302,
80.1181895029171));
#203463=CARTESIAN_POINT('Ctrl Pts',(5.75818820115869,-3.55893896737507,
80.1264113940207));
#203464=CARTESIAN_POINT('Ctrl Pts',(5.84804440549935,-3.40925659385929,
80.1346332851244));
#203465=CARTESIAN_POINT('Ctrl Pts',(5.93190183353251,-3.25650574041159,
80.142855176228));
#203466=CARTESIAN_POINT('Ctrl Pts',(6.00814799222413,-3.1176192268919,80.1503308122991));
#203467=CARTESIAN_POINT('Ctrl Pts',(6.07943540432172,-2.97619644230726,
80.1578064483702));
#203468=CARTESIAN_POINT('Ctrl Pts',(6.14560918025433,-2.83262719106729,
80.1652820844413));
#203469=CARTESIAN_POINT('Ctrl Pts',(6.22470948231096,-2.66101281695794,
80.1742180271611));
#203470=CARTESIAN_POINT('Ctrl Pts',(6.29666781814262,-2.48597403768251,
80.1831539698809));
#203471=CARTESIAN_POINT('Ctrl Pts',(6.36120676037905,-2.30810258691158,
80.1920899126008));
#203472=CARTESIAN_POINT('Ctrl Pts',(6.42564868348748,-2.13049852405331,
80.2010124222314));
#203473=CARTESIAN_POINT('Ctrl Pts',(6.48269337982514,-1.95007052854569,
80.2099349318619));
#203474=CARTESIAN_POINT('Ctrl Pts',(6.53211133643309,-1.76743047626838,
80.2188574414925));
#203475=CARTESIAN_POINT('Ctrl Pts',(6.58140820379596,-1.58523794848564,
80.2277580882209));
#203476=CARTESIAN_POINT('Ctrl Pts',(6.62311556177473,-1.40084443052398,
80.2366587349492));
#203477=CARTESIAN_POINT('Ctrl Pts',(6.65705370659433,-1.21487651533753,
80.2455593816775));
#203478=CARTESIAN_POINT('Ctrl Pts',(6.69093940424708,-1.02919599035258,
80.2544462735672));
#203479=CARTESIAN_POINT('Ctrl Pts',(6.71707979213586,-0.84194617415011,
80.263333165457));
#203480=CARTESIAN_POINT('Ctrl Pts',(6.73534547030215,-0.653766315804292,
80.2722200573467));
#203481=CARTESIAN_POINT('Ctrl Pts',(6.75356419891538,-0.466070149340212,
80.2810841066352));
#203482=CARTESIAN_POINT('Ctrl Pts',(6.76394858228651,-0.277448967141324,
80.2899481559237));
#203483=CARTESIAN_POINT('Ctrl Pts',(6.76642062655753,-0.0885488819625929,
80.2988122052122));
#203484=CARTESIAN_POINT('Ctrl Pts',(6.76878410090522,0.0920548842518706,
80.3072869535635));
#203485=CARTESIAN_POINT('Ctrl Pts',(6.76391525614064,0.272913323144809,
80.3157617019147));
#203486=CARTESIAN_POINT('Ctrl Pts',(6.75178996101479,0.453454873542969,
80.3242364502659));
#203487=CARTESIAN_POINT('Ctrl Pts',(6.74004500892569,0.62833324454433,80.332445364962));
#203488=CARTESIAN_POINT('Ctrl Pts',(6.72150205526021,0.802745656646183,
80.3406542796581));
#203489=CARTESIAN_POINT('Ctrl Pts',(6.69622702346234,0.976131471807344,
80.3488631943541));
#203490=CARTESIAN_POINT('Ctrl Pts',(6.6709459826429,1.14955850864174,80.3570740606815));
#203491=CARTESIAN_POINT('Ctrl Pts',(6.63892972637024,1.32195810991732,80.365284927009));
#203492=CARTESIAN_POINT('Ctrl Pts',(6.60029558116797,1.49277836305817,80.3734957933364));
#203493=CARTESIAN_POINT('Ctrl Pts',(6.56164536418001,1.66366967734154,80.3817100753803));
#203494=CARTESIAN_POINT('Ctrl Pts',(6.5163718521155,1.83297998756787,80.3899243574241));
#203495=CARTESIAN_POINT('Ctrl Pts',(6.46464267260206,2.00017102158102,80.398138639468));
#203496=CARTESIAN_POINT('Ctrl Pts',(6.41285526779065,2.16755024237514,80.4063621673384));
#203497=CARTESIAN_POINT('Ctrl Pts',(6.35459778749166,2.33280508219615,80.4145856952087));
#203498=CARTESIAN_POINT('Ctrl Pts',(6.29008693431294,2.49541486706832,80.4228092230791));
#203499=CARTESIAN_POINT('Ctrl Pts',(6.22553473216907,2.65812887853181,80.4310380219132));
#203500=CARTESIAN_POINT('Ctrl Pts',(6.15472131080019,2.81819413062466,80.4392668207473));
#203501=CARTESIAN_POINT('Ctrl Pts',(6.07791003216543,2.97511321480425,80.4474956195814));
#203502=CARTESIAN_POINT('Ctrl Pts',(6.00099302893615,3.13224828557905,80.4557357447003));
#203503=CARTESIAN_POINT('Ctrl Pts',(5.91806184704512,3.2862282261816,80.4639758698193));
#203504=CARTESIAN_POINT('Ctrl Pts',(5.82942449224626,3.43658247234071,80.4722159949382));
#203505=CARTESIAN_POINT('Ctrl Pts',(5.79007318376855,3.50333352030426,80.4758742686557));
#203506=CARTESIAN_POINT('Ctrl Pts',(5.74959774891652,3.56937035449353,80.4795325423732));
#203507=CARTESIAN_POINT('Ctrl Pts',(5.70802771687682,3.63465384642967,80.4831908160907));
#203508=CARTESIAN_POINT('Ctrl Pts',(5.61203314018049,3.78540814865593,80.4916385949285));
#203509=CARTESIAN_POINT('Ctrl Pts',(5.50997922611138,3.93248806020852,80.5000863737663));
#203510=CARTESIAN_POINT('Ctrl Pts',(5.40217158634465,4.0753933738586,80.5085341526041));
#203511=CARTESIAN_POINT('Ctrl Pts',(5.29445862764512,4.21817318223248,80.5169745122579));
#203512=CARTESIAN_POINT('Ctrl Pts',(5.18100221423595,4.35678543482519,80.5254148719117));
#203513=CARTESIAN_POINT('Ctrl Pts',(5.06215147060626,4.49075845360657,80.5338552315655));
#203514=CARTESIAN_POINT('Ctrl Pts',(4.94338845035151,4.6246325873074,80.5422893614153));
#203515=CARTESIAN_POINT('Ctrl Pts',(4.81923925685959,4.75387406404093,80.5507234912651));
#203516=CARTESIAN_POINT('Ctrl Pts',(4.69009377095809,4.87804360575222,80.5591576211149));
#203517=CARTESIAN_POINT('Ctrl Pts',(4.56103691621416,5.00212793124292,80.5675859627122));
#203518=CARTESIAN_POINT('Ctrl Pts',(4.42699084761324,5.121147033405,80.5760143043094));
#203519=CARTESIAN_POINT('Ctrl Pts',(4.28838298229058,5.23469773694724,80.5844426459066));
#203520=CARTESIAN_POINT('Ctrl Pts',(4.14983311762816,5.34820092503456,80.5928674606523));
#203521=CARTESIAN_POINT('Ctrl Pts',(4.00672551906653,5.45624006508905,80.6012922753979));
#203522=CARTESIAN_POINT('Ctrl Pts',(3.85952187208725,5.55845121584063,80.6097170901435));
#203523=CARTESIAN_POINT('Ctrl Pts',(3.71235445181019,5.66063721250806,80.6181398315488));
#203524=CARTESIAN_POINT('Ctrl Pts',(3.56109326579427,5.75699788833466,80.6265625729541));
#203525=CARTESIAN_POINT('Ctrl Pts',(3.40623060849283,5.84721147571786,80.6349853143594));
#203526=CARTESIAN_POINT('Ctrl Pts',(3.30533641544299,5.90598631052804,80.6404727941183));
#203527=CARTESIAN_POINT('Ctrl Pts',(3.20291415697681,5.96215280184155,80.6459602738772));
#203528=CARTESIAN_POINT('Ctrl Pts',(3.0991061983213,6.01563211736942,80.6514477536361));
#203529=CARTESIAN_POINT('Origin',(0.,0.,4.30282021618968));
#203530=CARTESIAN_POINT('',(3.09910619832137,6.01563211736938,83.0458350405685));
#203531=CARTESIAN_POINT('',(3.09910619832129,6.01563211736943,82.6511646947363));
#203532=CARTESIAN_POINT('',(3.09910619832133,6.0156321173694,4.30282021618968));
#203533=CARTESIAN_POINT('',(-6.76699851999205,-0.00447553632174044,81.6971797837716));
#203534=CARTESIAN_POINT('Ctrl Pts',(-6.76699851999152,-0.00447553713416882,
81.6971797838099));
#203535=CARTESIAN_POINT('Ctrl Pts',(-6.76684449886227,-0.237355015602491,
81.7081713552182));
#203536=CARTESIAN_POINT('Ctrl Pts',(-6.75466803722761,-0.469867458515164,
81.7191629266265));
#203537=CARTESIAN_POINT('Ctrl Pts',(-6.73058789011693,-0.70105324577479,
81.7301544980348));
#203538=CARTESIAN_POINT('Ctrl Pts',(-6.71101117766606,-0.889002997871695,
81.7390904414846));
#203539=CARTESIAN_POINT('Ctrl Pts',(-6.68354502816971,-1.07625201055286,
81.7480263849344));
#203540=CARTESIAN_POINT('Ctrl Pts',(-6.64825291327549,-1.2621498330721,
81.7569623283841));
#203541=CARTESIAN_POINT('Ctrl Pts',(-6.61301385179067,-1.44776820185748,
81.7658848387408));
#203542=CARTESIAN_POINT('Ctrl Pts',(-6.56997234717697,-1.63203918032549,
81.7748073490974));
#203543=CARTESIAN_POINT('Ctrl Pts',(-6.51924335481708,-1.8143194538651,
81.7837298594541));
#203544=CARTESIAN_POINT('Ctrl Pts',(-6.46863866423085,-1.99615308416877,
81.7926305068915));
#203545=CARTESIAN_POINT('Ctrl Pts',(-6.41038414977033,-2.17600549655582,
81.8015311543289));
#203546=CARTESIAN_POINT('Ctrl Pts',(-6.34464511076868,-2.35324614488138,
81.8104318017663));
#203547=CARTESIAN_POINT('Ctrl Pts',(-6.27900766333836,-2.53021288965983,
81.8193186943516));
#203548=CARTESIAN_POINT('Ctrl Pts',(-6.20590885266379,-2.70457568057547,
81.8282055869369));
#203549=CARTESIAN_POINT('Ctrl Pts',(-6.12556369540599,-2.87571876467852,
81.8370924795222));
#203550=CARTESIAN_POINT('Ctrl Pts',(-6.04542505519367,-3.04642194717093,
81.8459565294763));
#203551=CARTESIAN_POINT('Ctrl Pts',(-5.9580773443216,-3.21392170370398,
81.8548205794303));
#203552=CARTESIAN_POINT('Ctrl Pts',(-5.86378328803403,-3.37762261819949,
81.8636846293844));
#203553=CARTESIAN_POINT('Ctrl Pts',(-5.7736305847321,-3.5341338613871,81.8721593742094));
#203554=CARTESIAN_POINT('Ctrl Pts',(-5.67712867345867,-3.68717253080188,
81.8806341190345));
#203555=CARTESIAN_POINT('Ctrl Pts',(-5.57454854344113,-3.83623481252365,
81.8891088638596));
#203556=CARTESIAN_POINT('Ctrl Pts',(-5.47518608158014,-3.98062140357163,
81.897317778289));
#203557=CARTESIAN_POINT('Ctrl Pts',(-5.37021571557012,-4.12113741998357,
81.9055266927183));
#203558=CARTESIAN_POINT('Ctrl Pts',(-5.25998029941111,-4.25733440662195,
81.9137356071477));
#203559=CARTESIAN_POINT('Ctrl Pts',(-5.14971867534191,-4.393563773402,81.9219464732047));
#203560=CARTESIAN_POINT('Ctrl Pts',(-5.03418973133497,-4.52547178789233,
81.9301573392618));
#203561=CARTESIAN_POINT('Ctrl Pts',(-4.91377607024943,-4.65264373571027,
81.9383682053188));
#203562=CARTESIAN_POINT('Ctrl Pts',(-4.79331231718771,-4.77986858694569,
81.9465824870889));
#203563=CARTESIAN_POINT('Ctrl Pts',(-4.66796004342189,-4.90235318810453,
81.9547967688589));
#203564=CARTESIAN_POINT('Ctrl Pts',(-4.53813814433031,-5.01972022955207,
81.963011050629));
#203565=CARTESIAN_POINT('Ctrl Pts',(-4.40817012044269,-5.13721937687014,
81.9712345782216));
#203566=CARTESIAN_POINT('Ctrl Pts',(-4.27372268707219,-5.24958922053345,
81.9794581058142));
#203567=CARTESIAN_POINT('Ctrl Pts',(-4.13524795759656,-5.35649263316898,
81.9876816334069));
#203568=CARTESIAN_POINT('Ctrl Pts',(-3.99668447120583,-5.46346456673359,
81.9959104319608));
#203569=CARTESIAN_POINT('Ctrl Pts',(-3.85408883231614,-5.56496287877393,
82.0041392305148));
#203570=CARTESIAN_POINT('Ctrl Pts',(-3.70794140233327,-5.66069426456356,
82.0123680290687));
#203571=CARTESIAN_POINT('Ctrl Pts',(-3.5615928121081,-5.75655741694507,
82.0206081539054));
#203572=CARTESIAN_POINT('Ctrl Pts',(-3.41168297026833,-5.84663760535682,
82.028848278742));
#203573=CARTESIAN_POINT('Ctrl Pts',(-3.25871692629095,-5.93068739644107,
82.0370884035787));
#203574=CARTESIAN_POINT('Ctrl Pts',(-3.19080631546901,-5.96800203506002,
82.0407466789473));
#203575=CARTESIAN_POINT('Ctrl Pts',(-3.12229359885775,-6.00412872029134,
82.0444049543158));
#203576=CARTESIAN_POINT('Ctrl Pts',(-3.05322414153483,-6.03904887722801,
82.0480632296844));
#203577=CARTESIAN_POINT('Ctrl Pts',(-2.89372265821817,-6.11968968497332,
82.056511252447));
#203578=CARTESIAN_POINT('Ctrl Pts',(-2.73088594234967,-6.19407759388282,
82.0649592752095));
#203579=CARTESIAN_POINT('Ctrl Pts',(-2.56523216055996,-6.26193843489609,
82.0734072979722));
#203580=CARTESIAN_POINT('Ctrl Pts',(-2.39973007288556,-6.32973713371055,
82.081847584628));
#203581=CARTESIAN_POINT('Ctrl Pts',(-2.23141636847651,-6.3910205527999,
82.0902878712839));
#203582=CARTESIAN_POINT('Ctrl Pts',(-2.06083201069516,-6.44556129624831,
82.0987281579397));
#203583=CARTESIAN_POINT('Ctrl Pts',(-1.8903776016018,-6.50006049134993,
82.1071620149077));
#203584=CARTESIAN_POINT('Ctrl Pts',(-1.71765630395417,-6.54782714917387,
82.1155958718757));
#203585=CARTESIAN_POINT('Ctrl Pts',(-1.54322754976388,-6.58868254885981,
82.1240297288437));
#203586=CARTESIAN_POINT('Ctrl Pts',(-1.3689048573118,-6.62951310634169,
82.1324584575887));
#203587=CARTESIAN_POINT('Ctrl Pts',(-1.19287710217506,-6.66344070828384,
82.1408871863339));
#203588=CARTESIAN_POINT('Ctrl Pts',(-1.0157177001322,-6.69033680420038,
82.1493159150789));
#203589=CARTESIAN_POINT('Ctrl Pts',(-0.838638815093584,-6.71722067613647,
82.1577408130593));
#203590=CARTESIAN_POINT('Ctrl Pts',(-0.660429637888545,-6.73707936440374,
82.1661657110397));
#203591=CARTESIAN_POINT('Ctrl Pts',(-0.481672964666132,-6.74983556504229,
82.17459060902));
#203592=CARTESIAN_POINT('Ctrl Pts',(-0.302955868461923,-6.76258894143727,
82.1830136417143));
#203593=CARTESIAN_POINT('Ctrl Pts',(-0.123691850085766,-6.76824293911863,
82.1914366744085));
#203594=CARTESIAN_POINT('Ctrl Pts',(0.0555314560726346,-6.7667721446334,
82.1998597071028));
#203595=CARTESIAN_POINT('Ctrl Pts',(0.234734483317544,-6.76530151656689,
82.2082817867404));
#203596=CARTESIAN_POINT('Ctrl Pts',(0.413896474133007,-6.75670770619259,
82.2167038663781));
#203597=CARTESIAN_POINT('Ctrl Pts',(0.59242975795581,-6.74101742928235,
82.2251259460158));
#203598=CARTESIAN_POINT('Ctrl Pts',(0.770967762853059,-6.72532673746368,
82.2335482483641));
#203599=CARTESIAN_POINT('Ctrl Pts',(0.948876695453036,-6.70253923454659,
82.2419705507124));
#203600=CARTESIAN_POINT('Ctrl Pts',(1.12557359749265,-6.67273355354666,
82.2503928530608));
#203601=CARTESIAN_POINT('Ctrl Pts',(1.30229983904777,-6.64292292348294,
82.2588165538845));
#203602=CARTESIAN_POINT('Ctrl Pts',(1.47781332012457,-6.60609184807301,
82.2672402547082));
#203603=CARTESIAN_POINT('Ctrl Pts',(1.65154050273,-6.56237022483815,82.2756639555319));
#203604=CARTESIAN_POINT('Ctrl Pts',(1.82538524810783,-6.51861901478122,
82.284093356751));
#203605=CARTESIAN_POINT('Ctrl Pts',(1.99744095581411,-6.46796802077563,
82.2925227579701));
#203606=CARTESIAN_POINT('Ctrl Pts',(2.1671475147585,-6.41059752669562,82.3009521591891));
#203607=CARTESIAN_POINT('Ctrl Pts',(2.33691462476739,-6.35320656290303,
82.3093845680068));
#203608=CARTESIAN_POINT('Ctrl Pts',(2.50433060082657,-6.28909143113933,
82.3178169768245));
#203609=CARTESIAN_POINT('Ctrl Pts',(2.66885405457968,-6.21848108748058,
82.3262493856423));
#203610=CARTESIAN_POINT('Ctrl Pts',(2.83352973021915,-6.14780541307741,
82.33468959637));
#203611=CARTESIAN_POINT('Ctrl Pts',(2.99530723229255,-6.0706226569568,82.3431298070977));
#203612=CARTESIAN_POINT('Ctrl Pts',(3.15366756962959,-5.98720885390401,
82.3515700178254));
#203613=CARTESIAN_POINT('Ctrl Pts',(3.24374022720949,-5.93976450612001,
82.3563706656616));
#203614=CARTESIAN_POINT('Ctrl Pts',(3.33270784491619,-5.89030516238423,
82.3611713134978));
#203615=CARTESIAN_POINT('Ctrl Pts',(3.4204789128823,-5.8388879940043,82.365971961334));
#203616=CARTESIAN_POINT('Ctrl Pts',(3.56929871923541,-5.75170786484738,
82.3741116763666));
#203617=CARTESIAN_POINT('Ctrl Pts',(3.71497368254471,-5.65872288260556,
82.3822513913993));
#203618=CARTESIAN_POINT('Ctrl Pts',(3.85701704920413,-5.56018960847098,
82.3903911064319));
#203619=CARTESIAN_POINT('Ctrl Pts',(3.99893618558721,-5.46174251094684,
82.3985237025186));
#203620=CARTESIAN_POINT('Ctrl Pts',(4.13722974863279,-5.35775698770687,
82.4066562986052));
#203621=CARTESIAN_POINT('Ctrl Pts',(4.27143656465306,-5.2485349073951,82.4147888946919));
#203622=CARTESIAN_POINT('Ctrl Pts',(4.40555162969398,-5.13938749715697,
82.4229159308996));
#203623=CARTESIAN_POINT('Ctrl Pts',(4.53558522739118,-5.02501088763539,
82.4310429671073));
#203624=CARTESIAN_POINT('Ctrl Pts',(4.6611061552842,-4.90574952572711,82.439170003315));
#203625=CARTESIAN_POINT('Ctrl Pts',(4.78656708190211,-4.78654517290811,
82.4472931546524));
#203626=CARTESIAN_POINT('Ctrl Pts',(4.90751936936548,-4.66246096916189,
82.4554163059897));
#203627=CARTESIAN_POINT('Ctrl Pts',(5.02356586021245,-4.53388079332793,
82.463539457327));
#203628=CARTESIAN_POINT('Ctrl Pts',(5.13957974113306,-4.40533674947898,
82.4716603259984));
#203629=CARTESIAN_POINT('Ctrl Pts',(5.25069032670882,-4.27229952214212,
82.4797811946698));
#203630=CARTESIAN_POINT('Ctrl Pts',(5.35653824932944,-4.13518886914138,
82.4879020633413));
#203631=CARTESIAN_POINT('Ctrl Pts',(5.46239189237695,-3.99807080615612,
82.4960233708955));
#203632=CARTESIAN_POINT('Ctrl Pts',(5.5629820773229,-3.85687916516457,82.5041446784498));
#203633=CARTESIAN_POINT('Ctrl Pts',(5.65799046218856,-3.71206585741461,
82.512265986004));
#203634=CARTESIAN_POINT('Ctrl Pts',(5.70736012164754,-3.63681582870554,
82.5164860997222));
#203635=CARTESIAN_POINT('Ctrl Pts',(5.75522327816138,-3.5605883772458,82.5207062134404));
#203636=CARTESIAN_POINT('Ctrl Pts',(5.80153993560331,-3.48344992437095,
82.5249263271586));
#203637=CARTESIAN_POINT('Ctrl Pts',(5.90014608446744,-3.31922551381491,
82.5339107656847));
#203638=CARTESIAN_POINT('Ctrl Pts',(5.99169144311935,-3.15095198919124,
82.5428952042108));
#203639=CARTESIAN_POINT('Ctrl Pts',(6.07589018140923,-2.97923606037772,
82.5518796427368));
#203640=CARTESIAN_POINT('Ctrl Pts',(6.16023424169624,-2.80722376011943,
82.5608795878676));
#203641=CARTESIAN_POINT('Ctrl Pts',(6.23720623284492,-2.63175739503266,
82.5698795329984));
#203642=CARTESIAN_POINT('Ctrl Pts',(6.30656822692905,-2.4534641222339,82.5788794781291));
#203643=CARTESIAN_POINT('Ctrl Pts',(6.37609367433266,-2.27475069676127,
82.5879006318616));
#203644=CARTESIAN_POINT('Ctrl Pts',(6.43797315635529,-2.09319725824079,
82.596921785594));
#203645=CARTESIAN_POINT('Ctrl Pts',(6.49201759673769,-1.90944927234219,
82.6059429393265));
#203646=CARTESIAN_POINT('Ctrl Pts',(6.54611702776427,-1.7255143214193,82.614973272154));
#203647=CARTESIAN_POINT('Ctrl Pts',(6.59236542900976,-1.5393805929323,82.6240036049815));
#203648=CARTESIAN_POINT('Ctrl Pts',(6.6306244269346,-1.35170585148481,82.633033937809));
#203649=CARTESIAN_POINT('Ctrl Pts',(6.66893766405852,-1.16376504641265,
82.642077072802));
#203650=CARTESIAN_POINT('Ctrl Pts',(6.69923880258356,-0.974279094345651,
82.6511202077949));
#203651=CARTESIAN_POINT('Ctrl Pts',(6.72144074951205,-0.78391533394807,
82.6601633427879));
#203652=CARTESIAN_POINT('Ctrl Pts',(6.74085036615258,-0.617493550152844,
82.6680691261863));
#203653=CARTESIAN_POINT('Ctrl Pts',(6.75407072242936,-0.450401076252289,
82.6759749095848));
#203654=CARTESIAN_POINT('Ctrl Pts',(6.7610762003542,-0.283085875670381,
82.6838806929833));
#203655=CARTESIAN_POINT('Ctrl Pts',(6.76874414635676,-0.0999486311830835,
82.6925340812115));
#203656=CARTESIAN_POINT('Ctrl Pts',(6.76897170395597,0.0836172998891594,
82.7011874694397));
#203657=CARTESIAN_POINT('Ctrl Pts',(6.76173064094708,0.266997639085809,
82.7098408576679));
#203658=CARTESIAN_POINT('Ctrl Pts',(6.75449626557353,0.450208613531016,
82.7184862538782));
#203659=CARTESIAN_POINT('Ctrl Pts',(6.73980703935953,0.633234035245532,
82.7271316500885));
#203660=CARTESIAN_POINT('Ctrl Pts',(6.71768676693586,0.8154590739791,82.7357770462988));
#203661=CARTESIAN_POINT('Ctrl Pts',(6.69486004752519,1.00350376660773,82.7446985473413));
#203662=CARTESIAN_POINT('Ctrl Pts',(6.66411975782486,1.19069578225963,82.7536200483838));
#203663=CARTESIAN_POINT('Ctrl Pts',(6.62555026623527,1.37636211426706,82.7625415494262));
#203664=CARTESIAN_POINT('Ctrl Pts',(6.58824561820975,1.55593972548965,82.7711704797681));
#203665=CARTESIAN_POINT('Ctrl Pts',(6.54361717444127,1.73408980035634,82.7797994101099));
#203666=CARTESIAN_POINT('Ctrl Pts',(6.4917936668636,1.91021045617222,82.7884283404518));
#203667=CARTESIAN_POINT('Ctrl Pts',(6.4373344838341,2.09528837695898,82.7974961268446));
#203668=CARTESIAN_POINT('Ctrl Pts',(6.37492934271898,2.27812473444926,82.8065639132373));
#203669=CARTESIAN_POINT('Ctrl Pts',(6.3047881599716,2.45803483658835,82.81563169963));
#203670=CARTESIAN_POINT('Ctrl Pts',(6.2346469772242,2.6379449387275,82.8246994860228));
#203671=CARTESIAN_POINT('Ctrl Pts',(6.15676986189347,2.81492840888824,82.8337672724156));
#203672=CARTESIAN_POINT('Ctrl Pts',(6.07142741218859,2.98832029383147,82.8428350588083));
#203673=CARTESIAN_POINT('Ctrl Pts',(5.99213502880834,3.14942014347823,82.8512600149415));
#203674=CARTESIAN_POINT('Ctrl Pts',(5.90643326115009,3.30734900210329,82.8596849710747));
#203675=CARTESIAN_POINT('Ctrl Pts',(5.81460892997491,3.46159096247029,82.8681099272079));
#203676=CARTESIAN_POINT('Ctrl Pts',(5.7227632854908,3.6158687238773,82.8765368388543));
#203677=CARTESIAN_POINT('Ctrl Pts',(5.62479241364502,3.7664575958224,82.8849637505007));
#203678=CARTESIAN_POINT('Ctrl Pts',(5.52102743361863,3.91286916178275,82.8933906621471));
#203679=CARTESIAN_POINT('Ctrl Pts',(5.41722429516715,4.05933456897905,82.9018206726972));
#203680=CARTESIAN_POINT('Ctrl Pts',(5.30762299173378,4.20161933681769,82.9102506832473));
#203681=CARTESIAN_POINT('Ctrl Pts',(5.19259625134287,4.33926643230628,82.9186806937974));
#203682=CARTESIAN_POINT('Ctrl Pts',(5.07746355072462,4.47704032542017,82.9271184698969));
#203683=CARTESIAN_POINT('Ctrl Pts',(4.9568956407762,4.61016775621796,82.9355562459964));
#203684=CARTESIAN_POINT('Ctrl Pts',(4.83130434358136,4.73822618072332,82.9439940220958));
#203685=CARTESIAN_POINT('Ctrl Pts',(4.70564712021333,4.86635182646184,82.9524362274058));
#203686=CARTESIAN_POINT('Ctrl Pts',(4.57496148808737,4.98940292814892,82.9608784327157));
#203687=CARTESIAN_POINT('Ctrl Pts',(4.43969438295703,5.10699547541798,82.9693206380257));
#203688=CARTESIAN_POINT('Ctrl Pts',(4.30428457847358,5.22471207635414,82.9777717493977));
#203689=CARTESIAN_POINT('Ctrl Pts',(4.16428390133668,5.33695840839891,82.9862228607697));
#203690=CARTESIAN_POINT('Ctrl Pts',(4.02017128777912,5.44339157299164,82.9946739721418));
#203691=CARTESIAN_POINT('Ctrl Pts',(3.97972585955839,5.47326220549613,82.9970457896388));
#203692=CARTESIAN_POINT('Ctrl Pts',(3.93895672434481,5.50267522728859,82.9994176071359));
#203693=CARTESIAN_POINT('Ctrl Pts',(3.89787485526619,5.53162368682863,83.0017894246329));
#203694=CARTESIAN_POINT('Ctrl Pts',(3.75383633567919,5.63312085212294,83.0101053335404));
#203695=CARTESIAN_POINT('Ctrl Pts',(3.60569134154582,5.72908693007432,83.0184212424479));
#203696=CARTESIAN_POINT('Ctrl Pts',(3.45389851985335,5.81918155882379,83.0267371513554));
#203697=CARTESIAN_POINT('Ctrl Pts',(3.3376986542595,5.88815045758124,83.0331031144264));
#203698=CARTESIAN_POINT('Ctrl Pts',(3.2193618466181,5.95367935534069,83.0394690774975));
#203699=CARTESIAN_POINT('Ctrl Pts',(3.09910619832137,6.01563211736938,83.0458350405685));
#203700=CARTESIAN_POINT('Ctrl Pts',(3.09910619832132,6.01563211736941,81.0456744569491));
#203701=CARTESIAN_POINT('Ctrl Pts',(2.94210478641535,6.09651539601574,81.0540061427842));
#203702=CARTESIAN_POINT('Ctrl Pts',(2.78208187347672,6.171172809358,81.0623378286193));
#203703=CARTESIAN_POINT('Ctrl Pts',(2.61957258730343,6.23940129017588,81.0706695144544));
#203704=CARTESIAN_POINT('Ctrl Pts',(2.46569449257949,6.30400602065859,81.0785586878816));
#203705=CARTESIAN_POINT('Ctrl Pts',(2.3095875099172,6.36284691913867,81.0864478613087));
#203706=CARTESIAN_POINT('Ctrl Pts',(2.15171708221271,6.41579321659559,81.0943370347359));
#203707=CARTESIAN_POINT('Ctrl Pts',(1.99023121152499,6.46995205475702,81.1024068807382));
#203708=CARTESIAN_POINT('Ctrl Pts',(1.82640100248875,6.51810993784101,81.1104767267405));
#203709=CARTESIAN_POINT('Ctrl Pts',(1.6607218399461,6.56005274142869,81.1185465727428));
#203710=CARTESIAN_POINT('Ctrl Pts',(1.49525112286374,6.60194277563448,81.1266062658523));
#203711=CARTESIAN_POINT('Ctrl Pts',(1.32793643788382,6.63763319832059,81.1346659589618));
#203712=CARTESIAN_POINT('Ctrl Pts',(1.15929269380034,6.66695803572372,81.1427256520714));
#203713=CARTESIAN_POINT('Ctrl Pts',(0.990824113030937,6.69625241462552,
81.1507769739096));
#203714=CARTESIAN_POINT('Ctrl Pts',(0.821029584695862,6.71919430216325,
81.1588282957477));
#203715=CARTESIAN_POINT('Ctrl Pts',(0.650438617202402,6.73566764361573,
81.1668796175859));
#203716=CARTESIAN_POINT('Ctrl Pts',(0.479987453230496,6.75212748475701,
81.1749243411664));
#203717=CARTESIAN_POINT('Ctrl Pts',(0.308741518659208,6.76212929509531,
81.182969064747));
#203718=CARTESIAN_POINT('Ctrl Pts',(0.137239838793602,6.76560819340345,
81.1910137883275));
#203719=CARTESIAN_POINT('Ctrl Pts',(-0.0341588329914937,6.76908500220065,
81.1990536800514));
#203720=CARTESIAN_POINT('Ctrl Pts',(-0.205812572206715,6.76604669058816,
81.2070935717753));
#203721=CARTESIAN_POINT('Ctrl Pts',(-0.377178023321409,6.75648027738729,
81.2151334634992));
#203722=CARTESIAN_POINT('Ctrl Pts',(-0.552233442102512,6.74670787310032,
81.2233464761195));
#203723=CARTESIAN_POINT('Ctrl Pts',(-0.726987619962262,6.73012300380536,
81.2315594887397));
#203724=CARTESIAN_POINT('Ctrl Pts',(-0.900861684984169,6.70676801630469,
81.23977250136));
#203725=CARTESIAN_POINT('Ctrl Pts',(-1.07101129665723,6.68391330215645,
81.2478095879021));
#203726=CARTESIAN_POINT('Ctrl Pts',(-1.24031773478452,6.65457563381443,
81.2558466744441));
#203727=CARTESIAN_POINT('Ctrl Pts',(-1.40824455710652,6.61884704970434,
81.2638837609862));
#203728=CARTESIAN_POINT('Ctrl Pts',(-1.57618745080706,6.58311504620245,
81.2719216167149));
#203729=CARTESIAN_POINT('Ctrl Pts',(-1.74275010031391,6.5409909866855,81.2799594724435));
#203730=CARTESIAN_POINT('Ctrl Pts',(-1.90740742616755,6.4926178010569,81.2879973281722));
#203731=CARTESIAN_POINT('Ctrl Pts',(-2.07211313460704,6.44423040154625,
81.2960375457286));
#203732=CARTESIAN_POINT('Ctrl Pts',(-2.23491204674428,6.38959032622561,
81.3040777632851));
#203733=CARTESIAN_POINT('Ctrl Pts',(-2.39529552841332,6.32888997625675,
81.3121179808415));
#203734=CARTESIAN_POINT('Ctrl Pts',(-2.561738400809,6.26589632816343,81.3204619629702));
#203735=CARTESIAN_POINT('Ctrl Pts',(-2.72557934853586,6.19637569642848,
81.3288059450988));
#203736=CARTESIAN_POINT('Ctrl Pts',(-2.88627507206607,6.12059680165015,
81.3371499272275));
#203737=CARTESIAN_POINT('Ctrl Pts',(-3.04139020298881,6.04744953346841,
81.345204142062));
#203738=CARTESIAN_POINT('Ctrl Pts',(-3.19357460436433,5.96847161385049,
81.3532583568966));
#203739=CARTESIAN_POINT('Ctrl Pts',(-3.34236735467854,5.88395015838673,
81.3613125717311));
#203740=CARTESIAN_POINT('Ctrl Pts',(-3.49127145176187,5.79936545259009,
81.3693728138136));
#203741=CARTESIAN_POINT('Ctrl Pts',(-3.63677852870179,5.70922914630083,
81.3774330558961));
#203742=CARTESIAN_POINT('Ctrl Pts',(-3.77845849628231,5.61387035759395,
81.3854932979786));
#203743=CARTESIAN_POINT('Ctrl Pts',(-3.92033654217598,5.51837825075937,
81.3935648088324));
#203744=CARTESIAN_POINT('Ctrl Pts',(-4.05837650447829,5.41764931211516,
81.4016363196862));
#203745=CARTESIAN_POINT('Ctrl Pts',(-4.19218262275185,5.31205175591291,
81.40970783054));
#203746=CARTESIAN_POINT('Ctrl Pts',(-4.20620690106646,5.30098402943948,
81.4105538091551));
#203747=CARTESIAN_POINT('Ctrl Pts',(-4.22018470439754,5.28986285200514,
81.4113997877703));
#203748=CARTESIAN_POINT('Ctrl Pts',(-4.23411560180295,5.27868866960052,
81.4122457663854));
#203749=CARTESIAN_POINT('Ctrl Pts',(-4.36845503934569,5.17093298555859,
81.4204037685602));
#203750=CARTESIAN_POINT('Ctrl Pts',(-4.4988921346547,5.05787415795229,81.428561770735));
#203751=CARTESIAN_POINT('Ctrl Pts',(-4.62497610536319,4.93982641646643,
81.4367197729098));
#203752=CARTESIAN_POINT('Ctrl Pts',(-4.75090927689525,4.82191986265173,
81.4448680179362));
#203753=CARTESIAN_POINT('Ctrl Pts',(-4.87249942391205,4.69903652038096,
81.4530162629626));
#203754=CARTESIAN_POINT('Ctrl Pts',(-4.98932656618061,4.57153250190835,
81.461164507989));
#203755=CARTESIAN_POINT('Ctrl Pts',(-5.10603856463953,4.44415415028118,
81.4693047221764));
#203756=CARTESIAN_POINT('Ctrl Pts',(-5.21799665939793,4.31216445731424,
81.4774449363638));
#203757=CARTESIAN_POINT('Ctrl Pts',(-5.32481567914318,4.17595821137508,
81.4855851505511));
#203758=CARTESIAN_POINT('Ctrl Pts',(-5.43155188351587,4.03985756433609,
81.4937190537382));
#203759=CARTESIAN_POINT('Ctrl Pts',(-5.53315672209,3.89954716054724,81.5018529569252));
#203760=CARTESIAN_POINT('Ctrl Pts',(-5.62928349726135,3.7554568706698,81.5099868601123));
#203761=CARTESIAN_POINT('Ctrl Pts',(-5.72535678064825,3.61144676289266,
81.5181162370162));
#203762=CARTESIAN_POINT('Ctrl Pts',(-5.81595786936321,3.46366126170424,
81.5262456139202));
#203763=CARTESIAN_POINT('Ctrl Pts',(-5.90078181708742,3.31256138767729,
81.5343749908241));
#203764=CARTESIAN_POINT('Ctrl Pts',(-5.9855811562542,3.16150534973705,81.5425020092875));
#203765=CARTESIAN_POINT('Ctrl Pts',(-6.06460651182814,3.0071371716185,81.5506290277509));
#203766=CARTESIAN_POINT('Ctrl Pts',(-6.1375975210793,2.84994485371932,81.5587560462143));
#203767=CARTESIAN_POINT('Ctrl Pts',(-6.21058124993748,2.69276821476278,
81.5668822540589));
#203768=CARTESIAN_POINT('Ctrl Pts',(-6.27753167707233,2.5327683287134,81.5750084619034));
#203769=CARTESIAN_POINT('Ctrl Pts',(-6.33823548707841,2.37045563348903,
81.5831346697479));
#203770=CARTESIAN_POINT('Ctrl Pts',(-6.39894479854332,2.20812822820593,
81.5912616140536));
#203771=CARTESIAN_POINT('Ctrl Pts',(-6.45340623847369,2.04348793934419,
81.5993885583594));
#203772=CARTESIAN_POINT('Ctrl Pts',(-6.5014555272332,1.87706287252424,81.6075155026651));
#203773=CARTESIAN_POINT('Ctrl Pts',(-6.54953903645635,1.7105192786023,81.6156482349399));
#203774=CARTESIAN_POINT('Ctrl Pts',(-6.5912011704572,1.54218871938156,81.6237809672148));
#203775=CARTESIAN_POINT('Ctrl Pts',(-6.62632804143762,1.3726127229694,81.6319136994897));
#203776=CARTESIAN_POINT('Ctrl Pts',(-6.66146828452887,1.20297217230138,
81.6400495277362));
#203777=CARTESIAN_POINT('Ctrl Pts',(-6.69006824454796,1.03208559991146,
81.6481853559828));
#203778=CARTESIAN_POINT('Ctrl Pts',(-6.71206564568308,0.86050204418177,
81.6563211842293));
#203779=CARTESIAN_POINT('Ctrl Pts',(-6.73408768690814,0.68872629146398,
81.6644661257133));
#203780=CARTESIAN_POINT('Ctrl Pts',(-6.74949236136949,0.516252359863862,
81.6726110671973));
#203781=CARTESIAN_POINT('Ctrl Pts',(-6.75826942861491,0.3436325512072,81.6807560086813));
#203782=CARTESIAN_POINT('Ctrl Pts',(-6.76416890125792,0.227606797918737,
81.686230600378));
#203783=CARTESIAN_POINT('Ctrl Pts',(-6.76707523355838,0.111515163443945,
81.6917051920748));
#203784=CARTESIAN_POINT('Ctrl Pts',(-6.76699851999205,-0.00447553632183878,
81.6971797837716));
#203785=CARTESIAN_POINT('',(-6.76699999999136,-1.0814002431372E-5,81.3028202162286));
#203786=CARTESIAN_POINT('Ctrl Pts',(3.0991061983213,6.01563211736942,80.6514477536361));
#203787=CARTESIAN_POINT('Ctrl Pts',(2.9397834969441,6.09771126744672,80.6598698448734));
#203788=CARTESIAN_POINT('Ctrl Pts',(2.77719573725724,6.1734582995146,80.6682919361106));
#203789=CARTESIAN_POINT('Ctrl Pts',(2.61187701857521,6.24262664587902,80.6767140273478));
#203790=CARTESIAN_POINT('Ctrl Pts',(2.44653889357179,6.31180311173027,80.6851371072317));
#203791=CARTESIAN_POINT('Ctrl Pts',(2.27846947826298,6.37439922403963,80.6935601871156));
#203792=CARTESIAN_POINT('Ctrl Pts',(2.10822248442043,6.43021671144792,80.7019832669995));
#203793=CARTESIAN_POINT('Ctrl Pts',(1.9378637769666,6.48607082548292,80.7104118739865));
#203794=CARTESIAN_POINT('Ctrl Pts',(1.76532495233179,6.53513732031799,80.7188404809734));
#203795=CARTESIAN_POINT('Ctrl Pts',(1.59117553345244,6.57726762582627,80.7272690879603));
#203796=CARTESIAN_POINT('Ctrl Pts',(1.41697174456474,6.61941108455135,80.7357003263855));
#203797=CARTESIAN_POINT('Ctrl Pts',(1.24115668445808,6.65461396335232,80.7441315648106));
#203798=CARTESIAN_POINT('Ctrl Pts',(1.06431026002788,6.68277881351758,80.7525628032357));
#203799=CARTESIAN_POINT('Ctrl Pts',(0.887288511139442,6.71097158614219,
80.7610024003388));
#203800=CARTESIAN_POINT('Ctrl Pts',(0.709233685047566,6.73211233764841,
80.7694419974419));
#203801=CARTESIAN_POINT('Ctrl Pts',(0.530732312228089,6.74615536529934,
80.777881594545));
#203802=CARTESIAN_POINT('Ctrl Pts',(0.36704217122651,6.75903316640507,80.7856209122767));
#203803=CARTESIAN_POINT('Ctrl Pts',(0.202976761306707,6.76594283975284,
80.7933602300084));
#203804=CARTESIAN_POINT('Ctrl Pts',(0.0389883967627574,6.76688768230402,
80.8010995477402));
#203805=CARTESIAN_POINT('Ctrl Pts',(-0.133483982855122,6.76788140672843,
80.8092392627103));
#203806=CARTESIAN_POINT('Ctrl Pts',(-0.30621500353927,6.76227820303757,
80.8173789776805));
#203807=CARTESIAN_POINT('Ctrl Pts',(-0.478655139864533,6.75005024107831,
80.8255186926507));
#203808=CARTESIAN_POINT('Ctrl Pts',(-0.650944461079201,6.73783297362135,
80.8336512886749));
#203809=CARTESIAN_POINT('Ctrl Pts',(-0.822943041537907,6.71900250649092,
80.8417838846991));
#203810=CARTESIAN_POINT('Ctrl Pts',(-0.994100226346764,6.69358302704742,
80.8499164807233));
#203811=CARTESIAN_POINT('Ctrl Pts',(-1.16514039892165,6.66818092572381,
80.8580435168685));
#203812=CARTESIAN_POINT('Ctrl Pts',(-1.33533996033664,6.63619883409692,
80.8661705530137));
#203813=CARTESIAN_POINT('Ctrl Pts',(-1.50415229546543,6.59771285159078,
80.874297589159));
#203814=CARTESIAN_POINT('Ctrl Pts',(-1.6728839352451,6.55924526608028,80.882420740434));
#203815=CARTESIAN_POINT('Ctrl Pts',(-1.84022931293789,6.51428006191169,
80.890543891709));
#203816=CARTESIAN_POINT('Ctrl Pts',(-2.00565096226898,6.46294462436044,
80.898667042984));
#203817=CARTESIAN_POINT('Ctrl Pts',(-2.17102612688705,6.41162361244872,
80.9067879115931));
#203818=CARTESIAN_POINT('Ctrl Pts',(-2.33447829066059,6.35393604184711,
80.9149087802022));
#203819=CARTESIAN_POINT('Ctrl Pts',(-2.49548416997083,6.29005943989602,
80.9230296488113));
#203820=CARTESIAN_POINT('Ctrl Pts',(-2.65649875066311,6.22617938580567,
80.9311509563037));
#203821=CARTESIAN_POINT('Ctrl Pts',(-2.81506644088867,6.15610976349821,
80.939272263796));
#203822=CARTESIAN_POINT('Ctrl Pts',(-2.97068282382818,6.08007669032326,
80.9473935712883));
#203823=CARTESIAN_POINT('Ctrl Pts',(-3.05154651372621,6.0405672586357,80.9516136853805));
#203824=CARTESIAN_POINT('Ctrl Pts',(-3.13161363381079,5.9994483599442,80.9558337994728));
#203825=CARTESIAN_POINT('Ctrl Pts',(-3.21081588728411,5.95675669622018,
80.960053913565));
#203826=CARTESIAN_POINT('Ctrl Pts',(-3.37943402629467,5.86586800842756,
80.9690383521819));
#203827=CARTESIAN_POINT('Ctrl Pts',(-3.54404722440834,5.76789338143807,
80.9780227907987));
#203828=CARTESIAN_POINT('Ctrl Pts',(-3.70410000890383,5.66320864210729,
80.9870072294156));
#203829=CARTESIAN_POINT('Ctrl Pts',(-3.86442903502222,5.558343223119,80.9960071746411));
#203830=CARTESIAN_POINT('Ctrl Pts',(-4.02018171549801,5.44674467480157,
81.0050071198667));
#203831=CARTESIAN_POINT('Ctrl Pts',(-4.17083333289308,5.32883085762984,
81.0140070650922));
#203832=CARTESIAN_POINT('Ctrl Pts',(-4.32183996475892,5.21063917346854,
81.0230282189237));
#203833=CARTESIAN_POINT('Ctrl Pts',(-4.46772129296103,5.08610259167696,
81.0320493727553));
#203834=CARTESIAN_POINT('Ctrl Pts',(-4.60798526343422,4.95567965187148,
81.0410705265868));
#203835=CARTESIAN_POINT('Ctrl Pts',(-4.74839195362789,4.82512400567356,
81.050100859515));
#203836=CARTESIAN_POINT('Ctrl Pts',(-4.88316969675948,4.68867020304724,
81.0591311924432));
#203837=CARTESIAN_POINT('Ctrl Pts',(-5.01186376137092,4.54681323978201,
81.0681615253715));
#203838=CARTESIAN_POINT('Ctrl Pts',(-5.1407402736086,4.40475516804848,81.0772046604659));
#203839=CARTESIAN_POINT('Ctrl Pts',(-5.26351570130875,4.25727879643791,
81.0862477955604));
#203840=CARTESIAN_POINT('Ctrl Pts',(-5.37977452335198,4.10491352867426,
81.0952909306549));
#203841=CARTESIAN_POINT('Ctrl Pts',(-5.48141151086053,3.97171119147293,
81.1031967135665));
#203842=CARTESIAN_POINT('Ctrl Pts',(-5.57806856415838,3.83477294544959,
81.1111024964781));
#203843=CARTESIAN_POINT('Ctrl Pts',(-5.6694950009845,3.69447092745521,81.1190082793898));
#203844=CARTESIAN_POINT('Ctrl Pts',(-5.76956711990332,3.54090133952534,
81.1276616675687));
#203845=CARTESIAN_POINT('Ctrl Pts',(-5.86345990784307,3.38316533597308,
81.1363150557477));
#203846=CARTESIAN_POINT('Ctrl Pts',(-5.95083554270128,3.2217767371007,81.1449684439267));
#203847=CARTESIAN_POINT('Ctrl Pts',(-6.03813047995985,3.06053719205275,
81.1536138400876));
#203848=CARTESIAN_POINT('Ctrl Pts',(-6.11892012502693,2.89565204649202,
81.1622592362485));
#203849=CARTESIAN_POINT('Ctrl Pts',(-6.19291112170672,2.72766215625052,
81.1709046324094));
#203850=CARTESIAN_POINT('Ctrl Pts',(-6.26926514222222,2.55430723333459,
81.1798261334765));
#203851=CARTESIAN_POINT('Ctrl Pts',(-6.33837888946051,2.3776462407962,81.1887476345436));
#203852=CARTESIAN_POINT('Ctrl Pts',(-6.39998139241647,2.19830097500841,
81.1976691356107));
#203853=CARTESIAN_POINT('Ctrl Pts',(-6.45956370932354,2.02483713913816,
81.2062980659034));
#203854=CARTESIAN_POINT('Ctrl Pts',(-6.51211948838974,1.84886260438781,
81.2149269961962));
#203855=CARTESIAN_POINT('Ctrl Pts',(-6.55745221137515,1.67096065050354,
81.2235559264889));
#203856=CARTESIAN_POINT('Ctrl Pts',(-6.60509049763723,1.48401083483837,
81.2326237129432));
#203857=CARTESIAN_POINT('Ctrl Pts',(-6.64475173378035,1.29493275011024,
81.2416914993975));
#203858=CARTESIAN_POINT('Ctrl Pts',(-6.67626694563522,1.10442232439344,
81.2507592858517));
#203859=CARTESIAN_POINT('Ctrl Pts',(-6.70778215749009,0.913911898676632,
81.259827072306));
#203860=CARTESIAN_POINT('Ctrl Pts',(-6.73115124658922,0.721969511502301,
81.2688948587602));
#203861=CARTESIAN_POINT('Ctrl Pts',(-6.74626749550357,0.529305090767147,
81.2779626452145));
#203862=CARTESIAN_POINT('Ctrl Pts',(-6.76008024654131,0.353254425517801,
81.2862485022062));
#203863=CARTESIAN_POINT('Ctrl Pts',(-6.76700028223179,0.176618259281482,
81.294534359198));
#203864=CARTESIAN_POINT('Ctrl Pts',(-6.76699999999136,-1.08131744157636E-5,
81.3028202161898));
#203865=CARTESIAN_POINT('Ctrl Pts',(-6.76699999999136,-1.08140023413723E-5,
81.3028202162286));
#203866=CARTESIAN_POINT('Ctrl Pts',(-6.76699970791981,-0.182778316985658,
81.3113940335024));
#203867=CARTESIAN_POINT('Ctrl Pts',(-6.7595906328111,-0.365468940004556,
81.3199678507761));
#203868=CARTESIAN_POINT('Ctrl Pts',(-6.74481736487667,-0.547473939524143,
81.3285416680498));
#203869=CARTESIAN_POINT('Ctrl Pts',(-6.73003416201002,-0.729601336291533,
81.3371212511632));
#203870=CARTESIAN_POINT('Ctrl Pts',(-6.70787690894711,-0.911041880323436,
81.3457008342765));
#203871=CARTESIAN_POINT('Ctrl Pts',(-6.67844190688181,-1.09119324429949,
81.3542804173899));
#203872=CARTESIAN_POINT('Ctrl Pts',(-6.64897036818727,-1.27156822380576,
81.362870650037));
#203873=CARTESIAN_POINT('Ctrl Pts',(-6.61220307661963,-1.4506505185501,
81.371460882684));
#203874=CARTESIAN_POINT('Ctrl Pts',(-6.56828749042721,-1.62784779481913,
81.3800511153311));
#203875=CARTESIAN_POINT('Ctrl Pts',(-6.52434159461615,-1.80516736894028,
81.388647276777));
#203876=CARTESIAN_POINT('Ctrl Pts',(-6.47323764070425,-1.98059902926588,
81.3972434382229));
#203877=CARTESIAN_POINT('Ctrl Pts',(-6.41517285708126,-2.15356592974719,
81.4058395996688));
#203878=CARTESIAN_POINT('Ctrl Pts',(-6.35703981832765,-2.32673615275291,
81.4144458658991));
#203879=CARTESIAN_POINT('Ctrl Pts',(-6.29192970565408,-2.49743553495125,
81.4230521321295));
#203880=CARTESIAN_POINT('Ctrl Pts',(-6.2200882296409,-2.66510626720264,
81.4316583983598));
#203881=CARTESIAN_POINT('Ctrl Pts',(-6.20545600367273,-2.69925640134103,
81.4334112692529));
#203882=CARTESIAN_POINT('Ctrl Pts',(-6.19054469472299,-2.73328097576781,
81.4351641401461));
#203883=CARTESIAN_POINT('Ctrl Pts',(-6.17535661333137,-2.76717540069012,
81.4369170110392));
#203884=CARTESIAN_POINT('Ctrl Pts',(-6.10329869816184,-2.92798317705082,
81.4452332834416));
#203885=CARTESIAN_POINT('Ctrl Pts',(-6.02488576505313,-3.08613048155137,
81.4535495558439));
#203886=CARTESIAN_POINT('Ctrl Pts',(-5.94033851401064,-3.24109045522674,
81.4618658282463));
#203887=CARTESIAN_POINT('Ctrl Pts',(-5.85586274776895,-3.395919410061,81.4701750692305));
#203888=CARTESIAN_POINT('Ctrl Pts',(-5.76526316296489,-3.54756609939069,
81.4784843102147));
#203889=CARTESIAN_POINT('Ctrl Pts',(-5.66880778399605,-3.69552530881684,
81.4867935511988));
#203890=CARTESIAN_POINT('Ctrl Pts',(-5.57241627341678,-3.84338654634624,
81.4950972901795));
#203891=CARTESIAN_POINT('Ctrl Pts',(-5.47017688428602,-3.98756487879765,
81.5034010291601));
#203892=CARTESIAN_POINT('Ctrl Pts',(-5.36240274750198,-4.1275811044222,
81.5117047681407));
#203893=CARTESIAN_POINT('Ctrl Pts',(-5.25468022266644,-4.26753027768668,
81.5200045305444));
#203894=CARTESIAN_POINT('Ctrl Pts',(-5.14142844419832,-4.4033210411868,
81.528304292948));
#203895=CARTESIAN_POINT('Ctrl Pts',(-5.02300302361465,-4.53450434168477,
81.5366040553517));
#203896=CARTESIAN_POINT('Ctrl Pts',(-4.90461261987558,-4.66564885300029,
81.5449013636244));
#203897=CARTESIAN_POINT('Ctrl Pts',(-4.78105185617886,-4.79218835893123,
81.5531986718971));
#203898=CARTESIAN_POINT('Ctrl Pts',(-4.65271581509934,-4.91370782036585,
81.5614959801698));
#203899=CARTESIAN_POINT('Ctrl Pts',(-4.52436680752477,-5.03523955957903,
81.5697941267651));
#203900=CARTESIAN_POINT('Ctrl Pts',(-4.39124180596366,-5.15174999613048,
81.5780922733604));
#203901=CARTESIAN_POINT('Ctrl Pts',(-4.25377227858367,-5.26286142720413,
81.5863904199557));
#203902=CARTESIAN_POINT('Ctrl Pts',(-4.11628892777808,-5.37398403123103,
81.5946894009819));
#203903=CARTESIAN_POINT('Ctrl Pts',(-3.97446045079063,-5.47970632839051,
81.6029883820081));
#203904=CARTESIAN_POINT('Ctrl Pts',(-3.82875080005061,-5.57969141719431,
81.6112873630342));
#203905=CARTESIAN_POINT('Ctrl Pts',(-3.68300228199366,-5.67970317651797,
81.6195885577718));
#203906=CARTESIAN_POINT('Ctrl Pts',(-3.53337081375088,-5.77397448037678,
81.6278897525095));
#203907=CARTESIAN_POINT('Ctrl Pts',(-3.38034882694759,-5.86221210876526,
81.6361909472471));
#203908=CARTESIAN_POINT('Ctrl Pts',(-3.22726058878378,-5.95048793991827,
81.6444957360137));
#203909=CARTESIAN_POINT('Ctrl Pts',(-3.07077920774856,-6.03272471552547,
81.6528005247802));
#203910=CARTESIAN_POINT('Ctrl Pts',(-2.9114213296124,-6.10867537535577,
81.6611053135468));
#203911=CARTESIAN_POINT('Ctrl Pts',(-2.75187453414262,-6.18471607401132,
81.6694199475658));
#203912=CARTESIAN_POINT('Ctrl Pts',(-2.58944474282217,-6.25445561775319,
81.6777345815849));
#203913=CARTESIAN_POINT('Ctrl Pts',(-2.42466927924726,-6.31769482376876,
81.686049215604));
#203914=CARTESIAN_POINT('Ctrl Pts',(-2.25978962668599,-6.38097401649491,
81.6943691070398));
#203915=CARTESIAN_POINT('Ctrl Pts',(-2.09256167309976,-6.43774456298398,
81.7026889984757));
#203916=CARTESIAN_POINT('Ctrl Pts',(-1.92353762137143,-6.48785727487657,
81.7110088899116));
#203917=CARTESIAN_POINT('Ctrl Pts',(-1.75426082387943,-6.53804492152256,
81.7193412222829));
#203918=CARTESIAN_POINT('Ctrl Pts',(-1.58318289791363,-6.5815547516397,
81.7276735546541));
#203919=CARTESIAN_POINT('Ctrl Pts',(-1.41086728702232,-6.6182884870947,
81.7360058870254));
#203920=CARTESIAN_POINT('Ctrl Pts',(-1.28113350697068,-6.645944753009,81.7422791722466));
#203921=CARTESIAN_POINT('Ctrl Pts',(-1.15069837691565,-6.66976114965995,
81.7485524574677));
#203922=CARTESIAN_POINT('Ctrl Pts',(-1.01980382054277,-6.68971517836196,
81.7548257426889));
#203923=CARTESIAN_POINT('Ctrl Pts',(-0.851423318902484,-6.71538369702073,
81.7628955886912));
#203924=CARTESIAN_POINT('Ctrl Pts',(-0.681762116722721,-6.73473816862062,
81.7709654346935));
#203925=CARTESIAN_POINT('Ctrl Pts',(-0.511344976443914,-6.74765257812416,
81.7790352806958));
#203926=CARTESIAN_POINT('Ctrl Pts',(-0.34114224260392,-6.76055073965788,
81.7870949738053));
#203927=CARTESIAN_POINT('Ctrl Pts',(-0.170185830310789,-6.7670249328393,
81.7951546669149));
#203928=CARTESIAN_POINT('Ctrl Pts',(0.000988519058528649,-6.76699992779888,
81.8032143600244));
#203929=CARTESIAN_POINT('Ctrl Pts',(0.171985076677993,-6.76697494873017,
81.8112656818626));
#203930=CARTESIAN_POINT('Ctrl Pts',(0.34319875099108,-6.76046420495569,
81.8193170037007));
#203931=CARTESIAN_POINT('Ctrl Pts',(0.514087976305923,-6.7474441496479,
81.8273683255389));
#203932=CARTESIAN_POINT('Ctrl Pts',(0.684837153669671,-6.7344347645978,
81.8354130491194));
#203933=CARTESIAN_POINT('Ctrl Pts',(0.855262041130861,-6.71492671366791,
81.8434577727));
#203934=CARTESIAN_POINT('Ctrl Pts',(1.02482047121684,-6.68894849746766,
81.8515024962805));
#203935=CARTESIAN_POINT('Ctrl Pts',(1.19427706038546,-6.66298588441595,
81.8595423880044));
#203936=CARTESIAN_POINT('Ctrl Pts',(1.36286786030057,-6.6305608985558,81.8675822797283));
#203937=CARTESIAN_POINT('Ctrl Pts',(1.53005533614705,-6.59175391442429,
81.8756221714522));
#203938=CARTESIAN_POINT('Ctrl Pts',(1.70084281640561,-6.55211130960179,
81.8838351840725));
#203939=CARTESIAN_POINT('Ctrl Pts',(1.87016545477484,-6.50580877506365,
81.8920481966927));
#203940=CARTESIAN_POINT('Ctrl Pts',(2.03746021251925,-6.45298728360757,
81.900261209313));
#203941=CARTESIAN_POINT('Ctrl Pts',(2.20117144835849,-6.40129725003008,
81.908298295855));
#203942=CARTESIAN_POINT('Ctrl Pts',(2.36294043284138,-6.34336483738883,
81.9163353823971));
#203943=CARTESIAN_POINT('Ctrl Pts',(2.5222544486576,-6.27937269926121,81.9243724689392));
#203944=CARTESIAN_POINT('Ctrl Pts',(2.6815837115667,-6.21537443678809,81.9324103246678));
#203945=CARTESIAN_POINT('Ctrl Pts',(2.83845719122023,-6.14531543321051,
81.9404481803965));
#203946=CARTESIAN_POINT('Ctrl Pts',(2.99238209066652,-6.06942653167977,
81.9484860361251));
#203947=CARTESIAN_POINT('Ctrl Pts',(3.1463522191037,-5.99351533110288,81.9565262536816));
#203948=CARTESIAN_POINT('Ctrl Pts',(3.29737170786323,-5.91177098794107,
81.964566471238));
#203949=CARTESIAN_POINT('Ctrl Pts',(3.44497244406968,-5.82447026429019,
81.9726066887945));
#203950=CARTESIAN_POINT('Ctrl Pts',(3.59814963068672,-5.73387126334909,
81.9809506709231));
#203951=CARTESIAN_POINT('Ctrl Pts',(3.74764431061086,-5.63728806054833,
81.9892946530517));
#203952=CARTESIAN_POINT('Ctrl Pts',(3.8929673046525,-5.5350785509247,81.9976386351804));
#203953=CARTESIAN_POINT('Ctrl Pts',(4.0332435655986,-5.43641854231636,82.0056928500149));
#203954=CARTESIAN_POINT('Ctrl Pts',(4.16963277697767,-5.33251672891265,
82.0137470648495));
#203955=CARTESIAN_POINT('Ctrl Pts',(4.30173007168806,-5.22373500383917,
82.021801279684));
#203956=CARTESIAN_POINT('Ctrl Pts',(4.43392621937963,-5.11487187363287,
82.0298615217665));
#203957=CARTESIAN_POINT('Ctrl Pts',(4.56182377806979,-5.00112180711831,
82.037921763849));
#203958=CARTESIAN_POINT('Ctrl Pts',(4.6850554580905,-4.88288279140677,82.0459820059314));
#203959=CARTESIAN_POINT('Ctrl Pts',(4.80845942445318,-4.76447846944046,
82.0540535167853));
#203960=CARTESIAN_POINT('Ctrl Pts',(4.92718424009014,-4.6415729430195,82.0621250276391));
#203961=CARTESIAN_POINT('Ctrl Pts',(5.04090313915448,-4.51459683046698,
82.0701965384929));
#203962=CARTESIAN_POINT('Ctrl Pts',(5.05282206715812,-4.50128840806624,
82.0710425171081));
#203963=CARTESIAN_POINT('Ctrl Pts',(5.06468604374235,-4.48793529482951,
82.0718884957232));
#203964=CARTESIAN_POINT('Ctrl Pts',(5.07649472081613,-4.47453800403192,
82.0727344743383));
#203965=CARTESIAN_POINT('Ctrl Pts',(5.19136352595938,-4.34421597249018,
82.080963724075));
#203966=CARTESIAN_POINT('Ctrl Pts',(5.30137952524032,-4.20927629108711,
82.0891929738116));
#203967=CARTESIAN_POINT('Ctrl Pts',(5.40614979156494,-4.07011467051757,
82.0974222235483));
#203968=CARTESIAN_POINT('Ctrl Pts',(5.51079536422877,-3.93111867491511,
82.105641679139));
#203969=CARTESIAN_POINT('Ctrl Pts',(5.61020742200935,-3.78791102924984,
82.1138611347297));
#203970=CARTESIAN_POINT('Ctrl Pts',(5.70403084721884,-3.64092311014335,
82.1220805903205));
#203971=CARTESIAN_POINT('Ctrl Pts',(5.79776144934126,-3.49408061178211,
82.1302919140908));
#203972=CARTESIAN_POINT('Ctrl Pts',(5.88591423820863,-3.34346558824972,
82.1385032378611));
#203973=CARTESIAN_POINT('Ctrl Pts',(5.96817521452784,-3.18954128499626,
82.1467145616315));
#203974=CARTESIAN_POINT('Ctrl Pts',(6.05037132098683,-3.03573836430453,
82.1549194100662));
#203975=CARTESIAN_POINT('Ctrl Pts',(6.12668470074347,-2.87863167657969,
82.163124258501));
#203976=CARTESIAN_POINT('Ctrl Pts',(6.19684539157228,-2.7187122306249,82.1713291069358));
#203977=CARTESIAN_POINT('Ctrl Pts',(6.26696483592478,-2.55888679904712,
82.1795291318564));
#203978=CARTESIAN_POINT('Ctrl Pts',(6.33093865322651,-2.39625223088614,
82.187729156777));
#203979=CARTESIAN_POINT('Ctrl Pts',(6.38854341812386,-2.23132292480185,
82.1959291816976));
#203980=CARTESIAN_POINT('Ctrl Pts',(6.44613151089718,-2.06644135299531,
82.2041268333452));
#203981=CARTESIAN_POINT('Ctrl Pts',(6.49735410112811,-1.8992667030229,82.2123244849928));
#203982=CARTESIAN_POINT('Ctrl Pts',(6.54203630798522,-1.73033232212865,
82.2205221366405));
#203983=CARTESIAN_POINT('Ctrl Pts',(6.58671253162069,-1.56142056258448,
82.2287186905722));
#203984=CARTESIAN_POINT('Ctrl Pts',(6.6248500236285,-1.39074988791779,82.236915244504));
#203985=CARTESIAN_POINT('Ctrl Pts',(6.65632409129223,-1.21886774987393,
82.2451117984358));
#203986=CARTESIAN_POINT('Ctrl Pts',(6.68779966718853,-1.04697737526393,
82.2533087451452));
#203987=CARTESIAN_POINT('Ctrl Pts',(6.71261111791783,-0.873875774517605,
82.2615056918546));
#203988=CARTESIAN_POINT('Ctrl Pts',(6.73068507658497,-0.700119561101074,
82.269702638564));
#203989=CARTESIAN_POINT('Ctrl Pts',(6.74876318766153,-0.526323427988551,
82.2779014684844));
#203990=CARTESIAN_POINT('Ctrl Pts',(6.76010068660101,-0.351872739416242,
82.2861002984048));
#203991=CARTESIAN_POINT('Ctrl Pts',(6.76467617079343,-0.177328238866729,
82.2942991283253));
#203992=CARTESIAN_POINT('Ctrl Pts',(6.7692559885543,-0.00261842236166177,
82.3025057235858));
#203993=CARTESIAN_POINT('Ctrl Pts',(6.7670609865657,0.172185024544171,82.3107123188463));
#203994=CARTESIAN_POINT('Ctrl Pts',(6.75812192251174,0.346521399723311,
82.3189189141068));
#203995=CARTESIAN_POINT('Ctrl Pts',(6.74917853189954,0.520942154707554,
82.3271294814065));
#203996=CARTESIAN_POINT('Ctrl Pts',(6.73348460347278,0.694895030160229,
82.3353400487061));
#203997=CARTESIAN_POINT('Ctrl Pts',(6.71112269830597,0.867825517187885,
82.3435506160058));
#203998=CARTESIAN_POINT('Ctrl Pts',(6.68872995287063,1.04099450011368,82.3517725068532));
#203999=CARTESIAN_POINT('Ctrl Pts',(6.6596509120071,1.21313792285201,82.3599943977005));
#204000=CARTESIAN_POINT('Ctrl Pts',(6.62401932489763,1.38371130781775,82.3682162885479));
#204001=CARTESIAN_POINT('Ctrl Pts',(6.59162180316011,1.53880277007267,82.3756919276945));
#204002=CARTESIAN_POINT('Ctrl Pts',(6.55380790922888,1.69259623300692,82.3831675668412));
#204003=CARTESIAN_POINT('Ctrl Pts',(6.51071347235611,1.84469484763215,82.3906432059878));
#204004=CARTESIAN_POINT('Ctrl Pts',(6.45920089351945,2.02650466916343,82.3995791494376));
#204005=CARTESIAN_POINT('Ctrl Pts',(6.40003585945146,2.20627140930722,82.4085150928874));
#204006=CARTESIAN_POINT('Ctrl Pts',(6.33339242783275,2.3833651325533,82.4174510363371));
#204007=CARTESIAN_POINT('Ctrl Pts',(6.26684917896782,2.56019263696217,82.4263735466938));
#204008=CARTESIAN_POINT('Ctrl Pts',(6.19285005496423,2.73435490116357,82.4352960570504));
#204009=CARTESIAN_POINT('Ctrl Pts',(6.11161861126517,2.90523784748119,82.4442185674071));
#204010=CARTESIAN_POINT('Ctrl Pts',(6.03058620981137,3.07570207755101,82.4531192148445));
#204011=CARTESIAN_POINT('Ctrl Pts',(5.94235696813749,3.24290279408672,82.4620198622819));
#204012=CARTESIAN_POINT('Ctrl Pts',(5.84720185082691,3.40624713074174,82.4709205097193));
#204013=CARTESIAN_POINT('Ctrl Pts',(5.7521937840059,3.56933903888475,82.4798074023046));
#204014=CARTESIAN_POINT('Ctrl Pts',(5.65028132072025,3.72858623291068,82.4886942948899));
#204015=CARTESIAN_POINT('Ctrl Pts',(5.54178187019136,3.88341894510731,82.4975811874752));
#204016=CARTESIAN_POINT('Ctrl Pts',(5.43356130375142,4.03785367943704,82.5064452374293));
#204017=CARTESIAN_POINT('Ctrl Pts',(5.31878768247145,4.18789636300229,82.5153092873833));
#204018=CARTESIAN_POINT('Ctrl Pts',(5.19782193069723,4.33300544388799,82.5241733373373));
#204019=CARTESIAN_POINT('Ctrl Pts',(5.0821689409042,4.4717413985231,82.5326480821624));
#204020=CARTESIAN_POINT('Ctrl Pts',(4.96085617335053,4.6059675719914,82.5411228269875));
#204021=CARTESIAN_POINT('Ctrl Pts',(4.83423698792294,4.73523407495319,82.5495975718126));
#204022=CARTESIAN_POINT('Ctrl Pts',(4.70777943043633,4.86433557070347,82.5580614987229));
#204023=CARTESIAN_POINT('Ctrl Pts',(4.57615374704214,4.98836079582789,82.5665254256332));
#204024=CARTESIAN_POINT('Ctrl Pts',(4.4398150550172,5.10689056836375,82.5749893525435));
#204025=CARTESIAN_POINT('Ctrl Pts',(4.3075405445235,5.22188703347757,82.583200974441));
#204026=CARTESIAN_POINT('Ctrl Pts',(4.17083028506245,5.33171077287963,82.5914125963386));
#204027=CARTESIAN_POINT('Ctrl Pts',(4.03013340544854,5.43602002703152,82.5996242182362));
#204028=CARTESIAN_POINT('Ctrl Pts',(3.88295208309319,5.54513668976138,82.6082142976528));
#204029=CARTESIAN_POINT('Ctrl Pts',(3.73140830947619,5.64821825406331,82.6168043770695));
#204030=CARTESIAN_POINT('Ctrl Pts',(3.5760496501881,5.74492453382894,82.6253944564862));
#204031=CARTESIAN_POINT('Ctrl Pts',(3.42069099090001,5.84163081359456,82.6339845359029));
#204032=CARTESIAN_POINT('Ctrl Pts',(3.26151784721451,5.93196161725502,82.6425746153196));
#204033=CARTESIAN_POINT('Ctrl Pts',(3.09910619832129,6.01563211736943,82.6511646947363));
#204034=CARTESIAN_POINT('Origin',(0.,0.,4.30282021618968));
#204035=CARTESIAN_POINT('',(3.09910619832135,6.0156321173694,85.0458695769521));
#204036=CARTESIAN_POINT('',(3.09910619832134,6.0156321173694,84.651395695404));
#204037=CARTESIAN_POINT('',(3.09910619832133,6.0156321173694,4.30282021618968));
#204038=CARTESIAN_POINT('',(-6.76699823995479,0.00488061971302377,83.6971797838462));
#204039=CARTESIAN_POINT('Ctrl Pts',(-6.76699823995479,0.00488061971293362,
83.6971797838461));
#204040=CARTESIAN_POINT('Ctrl Pts',(-6.76712107896984,-0.165436153062113,
83.7052188399697));
#204041=CARTESIAN_POINT('Ctrl Pts',(-6.76080980226119,-0.336005823343854,
83.7132578960933));
#204042=CARTESIAN_POINT('Ctrl Pts',(-6.74803370927081,-0.50629048830176,
83.7212969522169));
#204043=CARTESIAN_POINT('Ctrl Pts',(-6.73526962568816,-0.67641508726984,
83.729328451703));
#204044=CARTESIAN_POINT('Ctrl Pts',(-6.71605284687801,-0.846254842235936,
83.7373599511891));
#204045=CARTESIAN_POINT('Ctrl Pts',(-6.69040469136798,-1.01527043969643,
83.7453914506752));
#204046=CARTESIAN_POINT('Ctrl Pts',(-6.6647749659965,-1.18416458667371,
83.7534171789218));
#204047=CARTESIAN_POINT('Ctrl Pts',(-6.63272311857364,-1.35223538512838,
83.7614429071684));
#204048=CARTESIAN_POINT('Ctrl Pts',(-6.59432239577663,-1.51894737912768,
83.7694686354151));
#204049=CARTESIAN_POINT('Ctrl Pts',(-6.55593841162304,-1.6855867043744,
83.7774908652951));
#204050=CARTESIAN_POINT('Ctrl Pts',(-6.51121114226346,-1.85086803825692,
83.7855130951752));
#204051=CARTESIAN_POINT('Ctrl Pts',(-6.46026515247052,-2.01426491797257,
83.7935353250553));
#204052=CARTESIAN_POINT('Ctrl Pts',(-6.40933009653302,-2.17762673000443,
83.8015558332316));
#204053=CARTESIAN_POINT('Ctrl Pts',(-6.35217908691007,-2.33910453390513,
83.8095763414079));
#204054=CARTESIAN_POINT('Ctrl Pts',(-6.28898685641384,-2.49818600585585,
83.8175968495842));
#204055=CARTESIAN_POINT('Ctrl Pts',(-6.22579554048134,-2.6572651754643,
83.8256172416819));
#204056=CARTESIAN_POINT('Ctrl Pts',(-6.15656331650125,-2.81394773292535,
83.8336376337797));
#204057=CARTESIAN_POINT('Ctrl Pts',(-6.08151339503498,-2.96774052538462,
83.8416580258774));
#204058=CARTESIAN_POINT('Ctrl Pts',(-6.00644953686954,-3.12156187701944,
83.8496799073543));
#204059=CARTESIAN_POINT('Ctrl Pts',(-5.92556599674474,-3.2724920584335,
83.8577017888312));
#204060=CARTESIAN_POINT('Ctrl Pts',(-5.83913225538147,-3.42006191525296,
83.8657236703081));
#204061=CARTESIAN_POINT('Ctrl Pts',(-5.75262086069104,-3.56776435097263,
83.8737527587597));
#204062=CARTESIAN_POINT('Ctrl Pts',(-5.6605494967974,-3.71210010851727,
83.8817818472114));
#204063=CARTESIAN_POINT('Ctrl Pts',(-5.56323170656305,-3.85262793156718,
83.889810935663));
#204064=CARTESIAN_POINT('Ctrl Pts',(-5.46586746257829,-3.99322283427849,
83.897843856726));
#204065=CARTESIAN_POINT('Ctrl Pts',(-5.36325202968282,-4.13000588231652,
83.905876777789));
#204066=CARTESIAN_POINT('Ctrl Pts',(-5.25573932231426,-4.26256884705451,
83.913909698852));
#204067=CARTESIAN_POINT('Ctrl Pts',(-5.14808399478493,-4.39530766218087,
83.9219532759251));
#204068=CARTESIAN_POINT('Ctrl Pts',(-5.03551866539925,-4.52381493162073,
83.9299968529981));
#204069=CARTESIAN_POINT('Ctrl Pts',(-4.9184347670821,-4.64771862766649,
83.9380404300712));
#204070=CARTESIAN_POINT('Ctrl Pts',(-4.83364399579953,-4.7374482156242,
83.9438654932413));
#204071=CARTESIAN_POINT('Ctrl Pts',(-4.74648423770331,-4.82476424712684,
83.9496905564114));
#204072=CARTESIAN_POINT('Ctrl Pts',(-4.65711466349154,-4.90953887968026,
83.9555156195815));
#204073=CARTESIAN_POINT('Ctrl Pts',(-4.52001718694038,-5.0395874818039,
83.9644515630322));
#204074=CARTESIAN_POINT('Ctrl Pts',(-4.37738205023,-5.1639731719019,83.9733875064829));
#204075=CARTESIAN_POINT('Ctrl Pts',(-4.22968046560856,-5.28224309918139,
83.9823234499336));
#204076=CARTESIAN_POINT('Ctrl Pts',(-4.08220091564451,-5.40033523539078,
83.9912459602912));
#204077=CARTESIAN_POINT('Ctrl Pts',(-3.92967031582237,-5.51232979217855,
84.0001684706487));
#204078=CARTESIAN_POINT('Ctrl Pts',(-3.77259434826907,-5.61781282025383,
84.0090909810063));
#204079=CARTESIAN_POINT('Ctrl Pts',(-3.615903265581,-5.72303738217621,84.0179916284446));
#204080=CARTESIAN_POINT('Ctrl Pts',(-3.45468925772409,-5.82178211557599,
84.0268922758829));
#204081=CARTESIAN_POINT('Ctrl Pts',(-3.28948794808252,-5.91367551015609,
84.0357929233213));
#204082=CARTESIAN_POINT('Ctrl Pts',(-3.12454193667582,-6.00542689483636,
84.0446798159075));
#204083=CARTESIAN_POINT('Ctrl Pts',(-2.95562113934356,-6.09034793589034,
84.0535667084936));
#204084=CARTESIAN_POINT('Ctrl Pts',(-2.78328932799944,-6.16811069263875,
84.0624536010799));
#204085=CARTESIAN_POINT('Ctrl Pts',(-2.61140047374007,-6.24567357007432,
84.0713176510347));
#204086=CARTESIAN_POINT('Ctrl Pts',(-2.43611833521379,-6.31611477217599,
84.0801817009897));
#204087=CARTESIAN_POINT('Ctrl Pts',(-2.25802970177353,-6.37915283293233,
84.0890457509446));
#204088=CARTESIAN_POINT('Ctrl Pts',(-2.08776264196135,-6.43942229007791,
84.0975204957651));
#204089=CARTESIAN_POINT('Ctrl Pts',(-1.91493053823632,-6.49292478630404,
84.1059952405857));
#204090=CARTESIAN_POINT('Ctrl Pts',(-1.74006688801186,-6.5394538170435,
84.1144699854062));
#204091=CARTESIAN_POINT('Ctrl Pts',(-1.57068824926195,-6.58452335481699,
84.1226788998353));
#204092=CARTESIAN_POINT('Ctrl Pts',(-1.39956653595643,-6.62300566039124,
84.1308878142645));
#204093=CARTESIAN_POINT('Ctrl Pts',(-1.22725383853958,-6.65478301793453,
84.1390967286936));
#204094=CARTESIAN_POINT('Ctrl Pts',(-1.05490017465371,-6.68656793038326,
84.1473075947505));
#204095=CARTESIAN_POINT('Ctrl Pts',(-0.881355312725267,-6.71164465439116,
84.1555184608073));
#204096=CARTESIAN_POINT('Ctrl Pts',(-0.707179597201149,-6.72994695501402,
84.1637293268642));
#204097=CARTESIAN_POINT('Ctrl Pts',(-0.532931424732736,-6.74825686937782,
84.1719436086341));
#204098=CARTESIAN_POINT('Ctrl Pts',(-0.358052229684333,-6.75978670881848,
84.180157890404));
#204099=CARTESIAN_POINT('Ctrl Pts',(-0.183105602099797,-6.76452225500661,
84.1883721721739));
#204100=CARTESIAN_POINT('Ctrl Pts',(-0.00796205827666974,-6.76926313142577,
84.1965956997663));
#204101=CARTESIAN_POINT('Ctrl Pts',(0.167248713592808,-6.76719443034825,
84.2048192273588));
#204102=CARTESIAN_POINT('Ctrl Pts',(0.341964019730027,-6.75835406065782,
84.2130427549512));
#204103=CARTESIAN_POINT('Ctrl Pts',(0.516791311582013,-6.74950802463431,
84.2212715535049));
#204104=CARTESIAN_POINT('Ctrl Pts',(0.691122150898044,-6.73388169943994,
84.2295003520586));
#204105=CARTESIAN_POINT('Ctrl Pts',(0.864400883076171,-6.71156465463435,
84.2377291506124));
#204106=CARTESIAN_POINT('Ctrl Pts',(1.03791811956269,-6.68921689220249,
84.2459692754488));
#204107=CARTESIAN_POINT('Ctrl Pts',(1.21038000627911,-6.66016007453195,
84.2542094002852));
#204108=CARTESIAN_POINT('Ctrl Pts',(1.38124196449292,-6.62453467313167,
84.2624495251216));
#204109=CARTESIAN_POINT('Ctrl Pts',(1.45709762272291,-6.60871846511687,
84.2661078004914));
#204110=CARTESIAN_POINT('Ctrl Pts',(1.53263814352889,-6.59160825051821,
84.2697660758612));
#204111=CARTESIAN_POINT('Ctrl Pts',(1.60781698502866,-6.57321941993825,
84.2734243512309));
#204112=CARTESIAN_POINT('Ctrl Pts',(1.78142681481329,-6.53075425709142,
84.2818723739935));
#204113=CARTESIAN_POINT('Ctrl Pts',(1.95350399173718,-6.48137002673282,
84.290320396756));
#204114=CARTESIAN_POINT('Ctrl Pts',(2.12347658587396,-6.42519542031564,
84.2987684195186));
#204115=CARTESIAN_POINT('Ctrl Pts',(2.29329353102955,-6.36907225466338,
84.3072087061743));
#204116=CARTESIAN_POINT('Ctrl Pts',(2.4610094197909,-6.30617121171915,84.3156489928301));
#204117=CARTESIAN_POINT('Ctrl Pts',(2.62606542132665,-6.23667133997876,
84.3240892794859));
#204118=CARTESIAN_POINT('Ctrl Pts',(2.79099568559647,-6.16722441223177,
84.3325231364538));
#204119=CARTESIAN_POINT('Ctrl Pts',(2.95326979570846,-6.09118880578558,
84.3409569934217));
#204120=CARTESIAN_POINT('Ctrl Pts',(3.11234654466722,-6.00879255640416,
84.3493908503896));
#204121=CARTESIAN_POINT('Ctrl Pts',(3.27132656670402,-5.92644640822003,
84.3578195791346));
#204122=CARTESIAN_POINT('Ctrl Pts',(3.42711280831388,-5.83774748107507,
84.3662483078796));
#204123=CARTESIAN_POINT('Ctrl Pts',(3.57918606578331,-5.74297101738313,
84.3746770366247));
#204124=CARTESIAN_POINT('Ctrl Pts',(3.73119020762479,-5.64823762855466,
84.3831019346049));
#204125=CARTESIAN_POINT('Ctrl Pts',(3.87948444766638,-5.54743238707693,
84.3915268325852));
#204126=CARTESIAN_POINT('Ctrl Pts',(4.02357578236501,-5.44087556589616,
84.3999517305654));
#204127=CARTESIAN_POINT('Ctrl Pts',(4.16763521500838,-5.33434233656845,
84.4083747632596));
#204128=CARTESIAN_POINT('Ctrl Pts',(4.30749332813591,-5.22206026246067,
84.4167977959537));
#204129=CARTESIAN_POINT('Ctrl Pts',(4.44268718767619,-5.10439218246971,
84.4252208286479));
#204130=CARTESIAN_POINT('Ctrl Pts',(4.57786575018514,-4.98673741648807,
84.4336429082855));
#204131=CARTESIAN_POINT('Ctrl Pts',(4.70838085972113,-4.86369807842071,
84.4420649879231));
#204132=CARTESIAN_POINT('Ctrl Pts',(4.83380345490516,-4.73567663162795,
84.4504870675607));
#204133=CARTESIAN_POINT('Ctrl Pts',(4.95922936672243,-4.60765179947876,
84.458909369909));
#204134=CARTESIAN_POINT('Ctrl Pts',(5.07956226260474,-4.47464483441219,
84.4673316722572));
#204135=CARTESIAN_POINT('Ctrl Pts',(5.19441042327864,-4.33709457523516,
84.4757539746055));
#204136=CARTESIAN_POINT('Ctrl Pts',(5.30927765383616,-4.19952147662023,
84.4841776754291));
#204137=CARTESIAN_POINT('Ctrl Pts',(5.41865812026474,-4.05740383619905,
84.4926013762528));
#204138=CARTESIAN_POINT('Ctrl Pts',(5.52220059741159,-3.9112133107192,84.5010250770764));
#204139=CARTESIAN_POINT('Ctrl Pts',(5.62581314269915,-3.76492385677452,
84.5094544782954));
#204140=CARTESIAN_POINT('Ctrl Pts',(5.72357961147391,-3.61455628270737,
84.5178838795144));
#204141=CARTESIAN_POINT('Ctrl Pts',(5.81519174534528,-3.4606117905463,84.5263132807334));
#204142=CARTESIAN_POINT('Ctrl Pts',(5.90683656629883,-3.30661237120416,
84.534745689551));
#204143=CARTESIAN_POINT('Ctrl Pts',(5.99232250868261,-3.14903377870128,
84.5431780983686));
#204144=CARTESIAN_POINT('Ctrl Pts',(6.07138718921519,-2.98840201422662,
84.5516105071863));
#204145=CARTESIAN_POINT('Ctrl Pts',(6.15052502269068,-2.82762162856968,
84.5600507179139));
#204146=CARTESIAN_POINT('Ctrl Pts',(6.22322958216186,-2.6637827288813,84.5684909286415));
#204147=CARTESIAN_POINT('Ctrl Pts',(6.28928611455797,-2.49743251545028,
84.5769311393692));
#204148=CARTESIAN_POINT('Ctrl Pts',(6.32685794298873,-2.4028153526696,84.5817317872063));
#204149=CARTESIAN_POINT('Ctrl Pts',(6.36227993459848,-2.30738607939501,
84.5865324350435));
#204150=CARTESIAN_POINT('Ctrl Pts',(6.39551975129777,-2.21124763668844,
84.5913330828807));
#204151=CARTESIAN_POINT('Ctrl Pts',(6.45187936042859,-2.04824056891767,
84.5994727979135));
#204152=CARTESIAN_POINT('Ctrl Pts',(6.50207497499668,-1.88286885991759,
84.6076125129464));
#204153=CARTESIAN_POINT('Ctrl Pts',(6.54590366792075,-1.71564395207796,
84.6157522279793));
#204154=CARTESIAN_POINT('Ctrl Pts',(6.58969402853302,-1.54856529813915,
84.6238848240663));
#204155=CARTESIAN_POINT('Ctrl Pts',(6.62712845929958,-1.37963702336426,
84.6320174201532));
#204156=CARTESIAN_POINT('Ctrl Pts',(6.65805292930488,-1.20938835391066,
84.6401500162402));
#204157=CARTESIAN_POINT('Ctrl Pts',(6.68895625768357,-1.0392560755803,84.6482770524482));
#204158=CARTESIAN_POINT('Ctrl Pts',(6.71335842095531,-0.867805558621238,
84.6564040886562));
#204159=CARTESIAN_POINT('Ctrl Pts',(6.7311558454839,-0.695578883957801,
84.6645311248642));
#204160=CARTESIAN_POINT('Ctrl Pts',(6.74894476252135,-0.52343453676293,
84.6726542762018));
#204161=CARTESIAN_POINT('Ctrl Pts',(6.76013519024366,-0.350515134175944,
84.6807774275394));
#204162=CARTESIAN_POINT('Ctrl Pts',(6.76467506093265,-0.177370572519474,
84.6889005788769));
#204163=CARTESIAN_POINT('Ctrl Pts',(6.76921365588425,-0.00427466577078583,
84.6970214475487));
#204164=CARTESIAN_POINT('Ctrl Pts',(6.76710540739535,0.169045908238103,
84.7051423162204));
#204165=CARTESIAN_POINT('Ctrl Pts',(6.75835028798784,0.34203857217374,84.7132631848921));
#204166=CARTESIAN_POINT('Ctrl Pts',(6.74959469542019,0.515040585294734,
84.7213844924466));
#204167=CARTESIAN_POINT('Ctrl Pts',(6.73419152881631,0.687714286980306,
84.7295058000011));
#204168=CARTESIAN_POINT('Ctrl Pts',(6.7121928362885,0.859509353339107,84.7376271075556));
#204169=CARTESIAN_POINT('Ctrl Pts',(6.70076155093691,0.948780041724772,
84.7418472212722));
#204170=CARTESIAN_POINT('Ctrl Pts',(6.68755019439306,1.03781355316633,84.7460673349888));
#204171=CARTESIAN_POINT('Ctrl Pts',(6.67257157733132,1.12653341956206,84.7502874487054));
#204172=CARTESIAN_POINT('Ctrl Pts',(6.64068275318351,1.31541415576423,84.7592718872312));
#204173=CARTESIAN_POINT('Ctrl Pts',(6.60079688724046,1.50277917244423,84.7682563257569));
#204174=CARTESIAN_POINT('Ctrl Pts',(6.55309139297731,1.68798169281742,84.7772407642827));
#204175=CARTESIAN_POINT('Ctrl Pts',(6.50530356187837,1.8735038616869,84.7862407094131));
#204176=CARTESIAN_POINT('Ctrl Pts',(6.44966918678762,2.05685584286998,84.7952406545436));
#204177=CARTESIAN_POINT('Ctrl Pts',(6.38641536804921,2.23740647776504,84.804240599674));
#204178=CARTESIAN_POINT('Ctrl Pts',(6.32301249006314,2.41838258486618,84.8132617534062));
#204179=CARTESIAN_POINT('Ctrl Pts',(6.25195432189093,2.5965439108255,84.8222829071383));
#204180=CARTESIAN_POINT('Ctrl Pts',(6.17351698119904,2.77127715734951,84.8313040608705));
#204181=CARTESIAN_POINT('Ctrl Pts',(6.09499982989494,2.94618819632867,84.8403343936977));
#204182=CARTESIAN_POINT('Ctrl Pts',(6.0090886094478,3.11766397215953,84.8493647265248));
#204183=CARTESIAN_POINT('Ctrl Pts',(5.91610595291568,3.285114815935,84.858395059352));
#204184=CARTESIAN_POINT('Ctrl Pts',(5.82299147628616,3.45280305222386,84.8674381943446));
#204185=CARTESIAN_POINT('Ctrl Pts',(5.72278563427439,3.61645473798033,84.8764813293372));
#204186=CARTESIAN_POINT('Ctrl Pts',(5.61585624227032,3.77550627944829,84.8855244643298));
#204187=CARTESIAN_POINT('Ctrl Pts',(5.52237531856668,3.91455397002478,84.8934302477299));
#204188=CARTESIAN_POINT('Ctrl Pts',(5.42375645092302,4.05008622305118,84.90133603113));
#204189=CARTESIAN_POINT('Ctrl Pts',(5.32027149338863,4.18174607510264,84.9092418145301));
#204190=CARTESIAN_POINT('Ctrl Pts',(5.20699117754997,4.32586817728066,84.9178959190671));
#204191=CARTESIAN_POINT('Ctrl Pts',(5.08777886983725,4.46547663036308,84.9265500236042));
#204192=CARTESIAN_POINT('Ctrl Pts',(4.9630126903714,4.6000863073656,84.9352041281412));
#204193=CARTESIAN_POINT('Ctrl Pts',(4.83836199103351,4.73457139337084,84.9438502226782));
#204194=CARTESIAN_POINT('Ctrl Pts',(4.70816787888502,4.86406670915905,84.9524963172153));
#204195=CARTESIAN_POINT('Ctrl Pts',(4.57284837415254,4.98812056259775,84.9611424117523));
#204196=CARTESIAN_POINT('Ctrl Pts',(4.43768172844762,5.11203428286467,84.9697787395258));
#204197=CARTESIAN_POINT('Ctrl Pts',(4.29740146827764,5.23051860308039,84.9784150672993));
#204198=CARTESIAN_POINT('Ctrl Pts',(4.1524621651814,5.34315889401925,84.9870513950728));
#204199=CARTESIAN_POINT('Ctrl Pts',(4.00762643038123,5.45571869634839,84.995681551644));
#204200=CARTESIAN_POINT('Ctrl Pts',(3.85813853101576,5.56244261091302,85.0043117082153));
#204201=CARTESIAN_POINT('Ctrl Pts',(3.70448679699984,5.6629556391388,85.0129418647865));
#204202=CARTESIAN_POINT('Ctrl Pts',(3.55096226977574,5.76338545359587,85.0215648765342));
#204203=CARTESIAN_POINT('Ctrl Pts',(3.39328104032662,5.85761447586562,85.0301878882819));
#204204=CARTESIAN_POINT('Ctrl Pts',(3.23196143974569,5.94531027382062,85.0388109000296));
#204205=CARTESIAN_POINT('Ctrl Pts',(3.18794344947024,5.96923912541509,85.0411637923371));
#204206=CARTESIAN_POINT('Ctrl Pts',(3.14365473671839,5.99268180246005,85.0435166846446));
#204207=CARTESIAN_POINT('Ctrl Pts',(3.09910619832135,6.0156321173694,85.0458695769521));
#204208=CARTESIAN_POINT('Ctrl Pts',(3.09910619832137,6.01563211736938,83.0458350405685));
#204209=CARTESIAN_POINT('Ctrl Pts',(2.94222343601837,6.09645427064887,83.0541399300722));
#204210=CARTESIAN_POINT('Ctrl Pts',(2.78207422307906,6.17118846651213,83.0624448195759));
#204211=CARTESIAN_POINT('Ctrl Pts',(2.6191668397426,6.23957162516729,83.0707497090796));
#204212=CARTESIAN_POINT('Ctrl Pts',(2.45634445559085,6.30791910396183,83.0790502653921));
#204213=CARTESIAN_POINT('Ctrl Pts',(2.29076708901272,6.36992201488416,83.0873508217047));
#204214=CARTESIAN_POINT('Ctrl Pts',(2.12296520258661,6.42536440589998,83.0956513780172));
#204215=CARTESIAN_POINT('Ctrl Pts',(1.95522012516891,6.48078802700013,83.1039491241922));
#204216=CARTESIAN_POINT('Ctrl Pts',(1.78525235890356,6.52965544612152,83.1122468703673));
#204217=CARTESIAN_POINT('Ctrl Pts',(1.61361002882069,6.5717997287569,83.1205446165423));
#204218=CARTESIAN_POINT('Ctrl Pts',(1.44195933667373,6.61394606457574,83.1288427669666));
#204219=CARTESIAN_POINT('Ctrl Pts',(1.26863425343041,6.64936851793706,83.1371409173909));
#204220=CARTESIAN_POINT('Ctrl Pts',(1.09419623148279,6.67795055439982,83.1454390678152));
#204221=CARTESIAN_POINT('Ctrl Pts',(0.919747450146447,6.70653435381104,
83.1537377300718));
#204222=CARTESIAN_POINT('Ctrl Pts',(0.744185936702099,6.72827683829004,
83.1620363923285));
#204223=CARTESIAN_POINT('Ctrl Pts',(0.568081393202253,6.7431129703348,83.1703350545852));
#204224=CARTESIAN_POINT('Ctrl Pts',(0.391936721418534,6.7579524830335,83.178635607827));
#204225=CARTESIAN_POINT('Ctrl Pts',(0.215249119809965,6.76588247737562,
83.1869361610688));
#204226=CARTESIAN_POINT('Ctrl Pts',(0.0385916370279971,6.76688995666041,
83.1952367143106));
#204227=CARTESIAN_POINT('Ctrl Pts',(-0.138135460949674,6.76789783296132,
83.2035405385411));
#204228=CARTESIAN_POINT('Ctrl Pts',(-0.31483206857426,6.76197775539134,
83.2118443627717));
#204229=CARTESIAN_POINT('Ctrl Pts',(-0.490926723087211,6.74916883420165,
83.2201481870023));
#204230=CARTESIAN_POINT('Ctrl Pts',(-0.667228372344878,6.736344856454,83.228461772165));
#204231=CARTESIAN_POINT('Ctrl Pts',(-0.842926306957382,6.71661587932008,
83.2367753573277));
#204232=CARTESIAN_POINT('Ctrl Pts',(-1.01745452551502,6.69007289112077,
83.2450889424904));
#204233=CARTESIAN_POINT('Ctrl Pts',(-1.19208697913823,6.66351405041269,
83.2534074928507));
#204234=CARTESIAN_POINT('Ctrl Pts',(-1.36554798195602,6.63013314811858,
83.2617260432111));
#204235=CARTESIAN_POINT('Ctrl Pts',(-1.53728312963927,6.59007204659604,
83.2700445935714));
#204236=CARTESIAN_POINT('Ctrl Pts',(-1.70928687689542,6.54994828815728,
83.2783761544255));
#204237=CARTESIAN_POINT('Ctrl Pts',(-1.87955903735623,6.50312353745619,
83.2867077152797));
#204238=CARTESIAN_POINT('Ctrl Pts',(-2.04756025847315,6.4497896080354,83.2950392761338));
#204239=CARTESIAN_POINT('Ctrl Pts',(-2.21330439089012,6.39717221751008,
83.30325890285));
#204240=CARTESIAN_POINT('Ctrl Pts',(-2.37683794933173,6.33821963469623,
83.3114785295662));
#204241=CARTESIAN_POINT('Ctrl Pts',(-2.53766439000712,6.27316096108571,
83.3196981562824));
#204242=CARTESIAN_POINT('Ctrl Pts',(-2.69556019893281,6.2092878078018,83.3277680022852));
#204243=CARTESIAN_POINT('Ctrl Pts',(-2.8513344453291,6.13933136950248,83.3358378482879));
#204244=CARTESIAN_POINT('Ctrl Pts',(-3.00447155353015,6.06345113644269,
83.3439076942907));
#204245=CARTESIAN_POINT('Ctrl Pts',(-3.15741599577087,5.98766637036764,
83.3519673874007));
#204246=CARTESIAN_POINT('Ctrl Pts',(-3.30772957139011,5.90597280226232,
83.3600270805108));
#204247=CARTESIAN_POINT('Ctrl Pts',(-3.45491318585497,5.81857919755377,
83.3680867736208));
#204248=CARTESIAN_POINT('Ctrl Pts',(-3.60194392675879,5.73127636498458,
83.3761380954595));
#204249=CARTESIAN_POINT('Ctrl Pts',(-3.74585085788079,5.63828546631741,
83.3841894172981));
#204250=CARTESIAN_POINT('Ctrl Pts',(-3.8861562566868,5.53986268319117,83.3922407391367));
#204251=CARTESIAN_POINT('Ctrl Pts',(-4.02634667174486,5.44152055997241,
83.4002854627177));
#204252=CARTESIAN_POINT('Ctrl Pts',(-4.16294112513135,5.33775562550626,
83.4083301862988));
#204253=CARTESIAN_POINT('Ctrl Pts',(-4.29548794327362,5.22886912526896,
83.4163749098798));
#204254=CARTESIAN_POINT('Ctrl Pts',(-4.42795515057297,5.12004802491216,
83.4244148016042));
#204255=CARTESIAN_POINT('Ctrl Pts',(-4.55637927464699,5.0061117186563,83.4324546933286));
#204256=CARTESIAN_POINT('Ctrl Pts',(-4.68033910352281,4.88740369480927,
83.4404945850529));
#204257=CARTESIAN_POINT('Ctrl Pts',(-4.80696812712494,4.76613956198648,
83.4487075976729));
#204258=CARTESIAN_POINT('Ctrl Pts',(-4.92893809121434,4.63989611294284,
83.4569206102929));
#204259=CARTESIAN_POINT('Ctrl Pts',(-5.0458367834887,4.5090819635922,83.4651336229128));
#204260=CARTESIAN_POINT('Ctrl Pts',(-5.16023145813442,4.38106990663177,
83.4731707094554));
#204261=CARTESIAN_POINT('Ctrl Pts',(-5.26976966830451,4.24868127686682,
83.481207795998));
#204262=CARTESIAN_POINT('Ctrl Pts',(-5.37410374915295,4.11233484693796,
83.4892448825405));
#204263=CARTESIAN_POINT('Ctrl Pts',(-5.47844781525869,3.97597536802094,
83.4972827382697));
#204264=CARTESIAN_POINT('Ctrl Pts',(-5.57758653316142,3.83565763137752,
83.5053205939988));
#204265=CARTESIAN_POINT('Ctrl Pts',(-5.67121396523096,3.69183168096399,
83.513358449728));
#204266=CARTESIAN_POINT('Ctrl Pts',(-5.76486890860173,3.54796346901492,
83.521398667285));
#204267=CARTESIAN_POINT('Ctrl Pts',(-5.85300913900852,3.40058530437991,
83.5294388848419));
#204268=CARTESIAN_POINT('Ctrl Pts',(-5.93537338346487,3.25017411823687,
83.5374791023989));
#204269=CARTESIAN_POINT('Ctrl Pts',(-6.02084940184901,3.09408030111023,
83.5458230845266));
#204270=CARTESIAN_POINT('Ctrl Pts',(-6.10010425481225,2.93472019737296,
83.5541670666544));
#204271=CARTESIAN_POINT('Ctrl Pts',(-6.17289996649483,2.77265125893036,
83.5625110487821));
#204272=CARTESIAN_POINT('Ctrl Pts',(-6.24316765067548,2.61621060166151,
83.5705652636172));
#204273=CARTESIAN_POINT('Ctrl Pts',(-6.30741721867655,2.45724646474984,
83.5786194784523));
#204274=CARTESIAN_POINT('Ctrl Pts',(-6.36548523708809,2.2962767029288,83.5866736932873));
#204275=CARTESIAN_POINT('Ctrl Pts',(-6.4235967098092,2.13518648185925,83.5947339353703));
#204276=CARTESIAN_POINT('Ctrl Pts',(-6.47551730969434,1.97208800099019,
83.6027941774533));
#204277=CARTESIAN_POINT('Ctrl Pts',(-6.52113434031348,1.80751097246582,
83.6108544195363));
#204278=CARTESIAN_POINT('Ctrl Pts',(-6.5668151466706,1.64270385396613,83.6189259303907));
#204279=CARTESIAN_POINT('Ctrl Pts',(-6.60617471542386,1.47641442368363,
83.626997441245));
#204280=CARTESIAN_POINT('Ctrl Pts',(-6.6391518532878,1.30917976954475,83.6350689520994));
#204281=CARTESIAN_POINT('Ctrl Pts',(-6.64260820164493,1.29165183172083,
83.6359149307103));
#204282=CARTESIAN_POINT('Ctrl Pts',(-6.64599448470253,1.27411351203699,
83.6367609093211));
#204283=CARTESIAN_POINT('Ctrl Pts',(-6.64931066511964,1.25656542954444,
83.637606887932));
#204284=CARTESIAN_POINT('Ctrl Pts',(-6.70553663204556,0.959037013795542,
83.6519504879214));
#204285=CARTESIAN_POINT('Ctrl Pts',(-6.74178309739482,0.657773115918566,
83.6662940879108));
#204286=CARTESIAN_POINT('Ctrl Pts',(-6.75768976121672,0.354849392202926,
83.6806376879002));
#204287=CARTESIAN_POINT('Ctrl Pts',(-6.76380467329694,0.238398076058037,
83.6861517198701));
#204288=CARTESIAN_POINT('Ctrl Pts',(-6.76691398399781,0.12170181386997,
83.6916657518401));
#204289=CARTESIAN_POINT('Ctrl Pts',(-6.76699823995424,0.0048806204788414,
83.69717978381));
#204290=CARTESIAN_POINT('',(-6.767,3.23694968940892E-12,83.3028202161898));
#204291=CARTESIAN_POINT('Ctrl Pts',(3.09910619832129,6.01563211736943,82.6511646947363));
#204292=CARTESIAN_POINT('Ctrl Pts',(2.94351145532274,6.09579071467805,82.6593942226567));
#204293=CARTESIAN_POINT('Ctrl Pts',(2.78494486261122,6.1698366203801,82.6676237505772));
#204294=CARTESIAN_POINT('Ctrl Pts',(2.62393210008548,6.23756918471779,82.6758532784977));
#204295=CARTESIAN_POINT('Ctrl Pts',(2.46270285731928,6.30539281489142,82.6840938709459));
#204296=CARTESIAN_POINT('Ctrl Pts',(2.29902120868915,6.36688602715692,82.6923344633941));
#204297=CARTESIAN_POINT('Ctrl Pts',(2.13342861867361,6.42189779808309,82.7005750558424));
#204298=CARTESIAN_POINT('Ctrl Pts',(2.07999748796384,6.43964823681139,82.7032340164407));
#204299=CARTESIAN_POINT('Ctrl Pts',(2.0263674867545,6.45672426696228,82.7058929770391));
#204300=CARTESIAN_POINT('Ctrl Pts',(1.97255701528041,6.47312195323617,82.7085519376374));
#204301=CARTESIAN_POINT('Ctrl Pts',(1.80159092869621,6.52522051648016,82.7169999604));
#204302=CARTESIAN_POINT('Ctrl Pts',(1.62841111951404,6.57058692165375,82.7254479831626));
#204303=CARTESIAN_POINT('Ctrl Pts',(1.45357508981669,6.60903990442367,82.7338960059252));
#204304=CARTESIAN_POINT('Ctrl Pts',(1.27889916269323,6.64745767464886,82.742336292581));
#204305=CARTESIAN_POINT('Ctrl Pts',(1.10257036235085,6.67897457038737,82.7507765792369));
#204306=CARTESIAN_POINT('Ctrl Pts',(0.925160630309959,6.70345931651148,
82.7592168658927));
#204307=CARTESIAN_POINT('Ctrl Pts',(0.747886046428055,6.72792541051135,
82.7676507228607));
#204308=CARTESIAN_POINT('Ctrl Pts',(0.5695325015942,6.74536998863663,82.7760845798287));
#204309=CARTESIAN_POINT('Ctrl Pts',(0.39068178667714,6.75571289662007,82.7845184367967));
#204310=CARTESIAN_POINT('Ctrl Pts',(0.21193982227986,6.7660495155785,82.7929471655418));
#204311=CARTESIAN_POINT('Ctrl Pts',(0.0327016226476002,6.76929305449129,
82.8013758942868));
#204312=CARTESIAN_POINT('Ctrl Pts',(-0.146445846855666,6.76541518415084,
82.8098046230319));
#204313=CARTESIAN_POINT('Ctrl Pts',(-0.325511895799725,6.76153907625991,
82.8182295210123));
#204314=CARTESIAN_POINT('Ctrl Pts',(-0.504486963965482,6.75054802012883,
82.8266544189926));
#204315=CARTESIAN_POINT('Ctrl Pts',(-0.682783631235683,6.73246578252847,
82.835079316973));
#204316=CARTESIAN_POINT('Ctrl Pts',(-0.861040823333554,6.71438754836494,
82.8435023496672));
#204317=CARTESIAN_POINT('Ctrl Pts',(-1.03861958224152,6.68922129399911,
82.8519253823615));
#204318=CARTESIAN_POINT('Ctrl Pts',(-1.2149366183719,6.6570427378333,82.8603484150557));
#204319=CARTESIAN_POINT('Ctrl Pts',(-1.39123370443,6.62486782263455,82.8687704946934));
#204320=CARTESIAN_POINT('Ctrl Pts',(-1.56626902432563,6.58568224724365,
82.877192574331));
#204321=CARTESIAN_POINT('Ctrl Pts',(-1.73946819088527,6.53961309351695,
82.8856146539687));
#204322=CARTESIAN_POINT('Ctrl Pts',(-1.91267193746574,6.49354272155296,
82.894036956317));
#204323=CARTESIAN_POINT('Ctrl Pts',(-2.08403911173682,6.44058849442824,
82.9024592586653));
#204324=CARTESIAN_POINT('Ctrl Pts',(-2.25300887074723,6.38092783444025,
82.9108815610136));
#204325=CARTESIAN_POINT('Ctrl Pts',(-2.42200668622488,6.32125726813906,
82.9193052618373));
#204326=CARTESIAN_POINT('Ctrl Pts',(-2.58860597858924,6.25487816043816,
82.927728962661));
#204327=CARTESIAN_POINT('Ctrl Pts',(-2.75226397544351,6.18201682377813,
82.9361526634848));
#204328=CARTESIAN_POINT('Ctrl Pts',(-2.91603272116038,6.10910618118551,
82.9445820647038));
#204329=CARTESIAN_POINT('Ctrl Pts',(-3.07685588910995,6.0297046799482,82.9530114659229));
#204330=CARTESIAN_POINT('Ctrl Pts',(-3.23421257418138,5.94408597052626,
82.9614408671419));
#204331=CARTESIAN_POINT('Ctrl Pts',(-3.39162540389929,5.85843671246782,
82.9698732759596));
#204332=CARTESIAN_POINT('Ctrl Pts',(-3.5455689945942,5.76656598783355,82.9783056847773));
#204333=CARTESIAN_POINT('Ctrl Pts',(-3.69554923193981,5.6687921883157,82.986738093595));
#204334=CARTESIAN_POINT('Ctrl Pts',(-3.84566823536477,5.57092792563375,
82.9951783043227));
#204335=CARTESIAN_POINT('Ctrl Pts',(-3.99181628267492,5.46714986298643,
83.0036185150504));
#204336=CARTESIAN_POINT('Ctrl Pts',(-4.1335293971468,5.35781893338355,83.0120587257781));
#204337=CARTESIAN_POINT('Ctrl Pts',(-4.21413339843345,5.29563336627339,
83.0168593736144));
#204338=CARTESIAN_POINT('Ctrl Pts',(-4.29330323395663,5.23165211256194,
83.0216600214506));
#204339=CARTESIAN_POINT('Ctrl Pts',(-4.37095855156853,5.16594718715455,
83.0264606692868));
#204340=CARTESIAN_POINT('Ctrl Pts',(-4.50262664672873,5.05454152123131,
83.0346003843194));
#204341=CARTESIAN_POINT('Ctrl Pts',(-4.63020117296965,4.93795617861826,
83.0427400993521));
#204342=CARTESIAN_POINT('Ctrl Pts',(-4.75324657479831,4.81652737967596,
83.0508798143848));
#204343=CARTESIAN_POINT('Ctrl Pts',(-4.87618436185678,4.69520478163266,
83.0590124104715));
#204344=CARTESIAN_POINT('Ctrl Pts',(-4.99460065026711,4.5690474145762,83.0671450065582));
#204345=CARTESIAN_POINT('Ctrl Pts',(-5.10809285403984,4.4384317494479,83.0752776026449));
#204346=CARTESIAN_POINT('Ctrl Pts',(-5.22150746845331,4.3079053801957,83.0834046388527));
#204347=CARTESIAN_POINT('Ctrl Pts',(-5.33000446128772,4.17292705644808,
83.0915316750604));
#204348=CARTESIAN_POINT('Ctrl Pts',(-5.43321807438887,4.03391005801246,
83.0996587112681));
#204349=CARTESIAN_POINT('Ctrl Pts',(-5.53638234951505,3.89495951221795,
83.1077818626055));
#204350=CARTESIAN_POINT('Ctrl Pts',(-5.63426805627028,3.75197442951678,
83.1159050139428));
#204351=CARTESIAN_POINT('Ctrl Pts',(-5.72654973831429,3.60540110037878,
83.1240281652802));
#204352=CARTESIAN_POINT('Ctrl Pts',(-5.81880548851989,3.45886895943548,
83.1321490339516));
#204353=CARTESIAN_POINT('Ctrl Pts',(-5.9054601563769,3.30875089049244,83.1402699026231));
#204354=CARTESIAN_POINT('Ctrl Pts',(-5.98623166756643,3.15552205224822,
83.1483907712945));
#204355=CARTESIAN_POINT('Ctrl Pts',(-6.06700754395764,3.002284932931,83.1565120788488));
#204356=CARTESIAN_POINT('Ctrl Pts',(-6.1418994541896,2.84593703056162,83.1646333864031));
#204357=CARTESIAN_POINT('Ctrl Pts',(-6.21067125504395,2.68697814687258,
83.1727546939574));
#204358=CARTESIAN_POINT('Ctrl Pts',(-6.24640747341314,2.6043775851792,83.1769748076754));
#204359=CARTESIAN_POINT('Ctrl Pts',(-6.28049190995254,2.52107237950219,
83.1811949213935));
#204360=CARTESIAN_POINT('Ctrl Pts',(-6.31289654940185,2.43713482527131,
83.1854150351116));
#204361=CARTESIAN_POINT('Ctrl Pts',(-6.38012902587568,2.26298292184015,
83.1941708398695));
#204362=CARTESIAN_POINT('Ctrl Pts',(-6.44010519243268,2.08616622098546,
83.2029266446274));
#204363=CARTESIAN_POINT('Ctrl Pts',(-6.49265040050596,1.90729645750466,
83.2116824493853));
#204364=CARTESIAN_POINT('Ctrl Pts',(-6.54529416165284,1.72809120834186,
83.2204546764108));
#204365=CARTESIAN_POINT('Ctrl Pts',(-6.59047901362006,1.54682546602365,
83.2292269034364));
#204366=CARTESIAN_POINT('Ctrl Pts',(-6.6280807354594,1.36412417478471,83.2379991304619));
#204367=CARTESIAN_POINT('Ctrl Pts',(-6.66571845078739,1.18124799642541,
83.2467797545246));
#204368=CARTESIAN_POINT('Ctrl Pts',(-6.69575849200273,0.996933801297433,
83.2555603785872));
#204369=CARTESIAN_POINT('Ctrl Pts',(-6.71812825172542,0.81181389084494,
83.2643410026499));
#204370=CARTESIAN_POINT('Ctrl Pts',(-6.74053178465382,0.626414491792852,
83.2731348834407));
#204371=CARTESIAN_POINT('Ctrl Pts',(-6.75524185616454,0.440207224918582,
83.2819287642314));
#204372=CARTESIAN_POINT('Ctrl Pts',(-6.76223779849073,0.253828597016198,
83.2907226450222));
#204373=CARTESIAN_POINT('Ctrl Pts',(-6.76541320615378,0.169232684746745,
83.2947141239609));
#204374=CARTESIAN_POINT('Ctrl Pts',(-6.76700007130205,0.0846014611602841,
83.2987056028995));
#204375=CARTESIAN_POINT('Ctrl Pts',(-6.7669999999976,-5.7030305532282E-6,
83.3026970818381));
#204376=CARTESIAN_POINT('Ctrl Pts',(-6.767,3.23694969632991E-12,83.3028202161898));
#204377=CARTESIAN_POINT('Ctrl Pts',(-6.76700000000009,-0.186007249523727,
83.311569728001));
#204378=CARTESIAN_POINT('Ctrl Pts',(-6.75932637294537,-0.372014355746867,
83.3203192398122));
#204379=CARTESIAN_POINT('Ctrl Pts',(-6.74400518264205,-0.55738953748454,
83.3290687516234));
#204380=CARTESIAN_POINT('Ctrl Pts',(-6.72868405705117,-0.742763936248949,
83.337818226479));
#204381=CARTESIAN_POINT('Ctrl Pts',(-6.70571545645763,-0.927506130239531,
83.3465677013347));
#204382=CARTESIAN_POINT('Ctrl Pts',(-6.67517739404845,-1.11098863989898,
83.3553171761904));
#204383=CARTESIAN_POINT('Ctrl Pts',(-6.64463945808724,-1.29447038981831,
83.3640666148174));
#204384=CARTESIAN_POINT('Ctrl Pts',(-6.6065321700838,-1.47669218313569,
83.3728160534444));
#204385=CARTESIAN_POINT('Ctrl Pts',(-6.56098496092705,-1.65703510599173,
83.3815654920714));
#204386=CARTESIAN_POINT('Ctrl Pts',(-6.51543793658328,-1.8373772970859,
83.3903148951966));
#204387=CARTESIAN_POINT('Ctrl Pts',(-6.46245112167454,-2.01584035510819,
83.3990642983218));
#204388=CARTESIAN_POINT('Ctrl Pts',(-6.40220448374289,-2.19181813760686,
83.4078137014469));
#204389=CARTESIAN_POINT('Ctrl Pts',(-6.34195808526534,-2.36779522067063,
83.416563069797));
#204390=CARTESIAN_POINT('Ctrl Pts',(-6.27445201433127,-2.5412867768411,
83.4253124381471));
#204391=CARTESIAN_POINT('Ctrl Pts',(-6.19991555071916,-2.71170355384779,
83.4340618064973));
#204392=CARTESIAN_POINT('Ctrl Pts',(-6.12537937716709,-2.88211966767442,
83.442811140799));
#204393=CARTESIAN_POINT('Ctrl Pts',(-6.04381298052539,-3.04946076371747,
83.4515604751008));
#204394=CARTESIAN_POINT('Ctrl Pts',(-5.95549339335854,-3.21315848374505,
83.4603098094026));
#204395=CARTESIAN_POINT('Ctrl Pts',(-5.86717414255433,-3.37685558033451,
83.4690591103828));
#204396=CARTESIAN_POINT('Ctrl Pts',(-5.77210188876624,-3.53690907646714,
83.477808411363));
#204397=CARTESIAN_POINT('Ctrl Pts',(-5.67059953347023,-3.69277536969245,
83.4865577123431));
#204398=CARTESIAN_POINT('Ctrl Pts',(-5.5690975563141,-3.84864108224885,
83.4953069807284));
#204399=CARTESIAN_POINT('Ctrl Pts',(-5.46116568196876,-4.00031938297482,
83.5040562491137));
#204400=CARTESIAN_POINT('Ctrl Pts',(-5.34717048533628,-4.14729511859822,
83.512805517499));
#204401=CARTESIAN_POINT('Ctrl Pts',(-5.23317570391869,-4.29427031887876,
83.521554754016));
#204402=CARTESIAN_POINT('Ctrl Pts',(-5.11311782003554,-4.436542761895,83.5303039905331));
#204403=CARTESIAN_POINT('Ctrl Pts',(-4.98740458984802,-4.57362924351799,
83.5390532270501));
#204404=CARTESIAN_POINT('Ctrl Pts',(-4.86169180711786,-4.71071523720223,
83.5478024324256));
#204405=CARTESIAN_POINT('Ctrl Pts',(-4.73032391204209,-4.84261509523202,
83.556551637801));
#204406=CARTESIAN_POINT('Ctrl Pts',(-4.59374707013629,-4.96888084538302,
83.5653008431765));
#204407=CARTESIAN_POINT('Ctrl Pts',(-4.45717070301487,-5.09514615659427,
83.5740500181369));
#204408=CARTESIAN_POINT('Ctrl Pts',(-4.31538563571095,-5.21577720459482,
83.5827991930973));
#204409=CARTESIAN_POINT('Ctrl Pts',(-4.16887341029576,-5.33036429232834,
83.5915483680577));
#204410=CARTESIAN_POINT('Ctrl Pts',(-4.02236168203758,-5.44495099123578,
83.6002975133298));
#204411=CARTESIAN_POINT('Ctrl Pts',(-3.87112305348201,-5.55349359438577,
83.6090466586018));
#204412=CARTESIAN_POINT('Ctrl Pts',(-3.7156711701778,-5.65562346298881,
83.6177958038739));
#204413=CARTESIAN_POINT('Ctrl Pts',(-3.56021980145802,-5.75775299351656,
83.626544920184));
#204414=CARTESIAN_POINT('Ctrl Pts',(-3.40055544538295,-5.85346967463906,
83.6352940364942));
#204415=CARTESIAN_POINT('Ctrl Pts',(-3.2372203598676,-5.94244842986952,
83.6440431528044));
#204416=CARTESIAN_POINT('Ctrl Pts',(-3.0738858014707,-6.03142689794585,
83.6527922408793));
#204417=CARTESIAN_POINT('Ctrl Pts',(-2.90688078896451,-6.11366734656842,
83.6615413289541));
#204418=CARTESIAN_POINT('Ctrl Pts',(-2.73677250721226,-6.18889046952417,
83.670290417029));
#204419=CARTESIAN_POINT('Ctrl Pts',(-2.56666476031311,-6.26411335596398,
83.679039477595));
#204420=CARTESIAN_POINT('Ctrl Pts',(-2.39345402574968,-6.33231884500632,
83.6877885381611));
#204421=CARTESIAN_POINT('Ctrl Pts',(-2.21772856065365,-6.39327529762806,
83.6965375987271));
#204422=CARTESIAN_POINT('Ctrl Pts',(-2.04200363348295,-6.4542315636518,
83.7052866325108));
#204423=CARTESIAN_POINT('Ctrl Pts',(-1.86376426189069,-6.50793874375718,
83.7140356662945));
#204424=CARTESIAN_POINT('Ctrl Pts',(-1.68361577752954,-6.55421443909593,
83.7227847000782));
#204425=CARTESIAN_POINT('Ctrl Pts',(-1.50346782967588,-6.60048999661917,
83.731533707806));
#204426=CARTESIAN_POINT('Ctrl Pts',(-1.32141105794765,-6.63933404237757,
83.7402827155339));
#204427=CARTESIAN_POINT('Ctrl Pts',(-1.1380637548679,-6.670614656076,83.7490317232617));
#204428=CARTESIAN_POINT('Ctrl Pts',(-0.954716982600968,-6.70189517921325,
83.7577807056601));
#204429=CARTESIAN_POINT('Ctrl Pts',(-0.770079968900371,-6.72561226592248,
83.7665296880584));
#204430=CARTESIAN_POINT('Ctrl Pts',(-0.584779765556764,-6.74168536983115,
83.7752786704568));
#204431=CARTESIAN_POINT('Ctrl Pts',(-0.391489830649839,-6.75845151013861,
83.7844048894667));
#204432=CARTESIAN_POINT('Ctrl Pts',(-0.1974785782369,-6.76689983031629,
83.7935311084766));
#204433=CARTESIAN_POINT('Ctrl Pts',(-0.00346287644993494,-6.76699911397118,
83.8026573274864));
#204434=CARTESIAN_POINT('Ctrl Pts',(0.184489834656155,-6.76709529501185,
83.8114983521522));
#204435=CARTESIAN_POINT('Ctrl Pts',(0.372446404251599,-6.75935639738156,
83.820339376818));
#204436=CARTESIAN_POINT('Ctrl Pts',(0.559755019490524,-6.74380925873168,
83.8291804014839));
#204437=CARTESIAN_POINT('Ctrl Pts',(0.745134705523977,-6.72842222659781,
83.8379303800936));
#204438=CARTESIAN_POINT('Ctrl Pts',(0.929879431230782,-6.70538706057493,
83.8466803587034));
#204439=CARTESIAN_POINT('Ctrl Pts',(1.11336163627048,-6.6747820089409,83.8554303373131));
#204440=CARTESIAN_POINT('Ctrl Pts',(1.29684196300956,-6.64417727060967,
83.8641802263496));
#204441=CARTESIAN_POINT('Ctrl Pts',(1.47905951217763,-6.60600284890534,
83.8729301153862));
#204442=CARTESIAN_POINT('Ctrl Pts',(1.65939532067351,-6.56038841607163,
83.8816800044227));
#204443=CARTESIAN_POINT('Ctrl Pts',(1.83972934301073,-6.5147744350318,83.8904298067949));
#204444=CARTESIAN_POINT('Ctrl Pts',(2.01818138406539,-6.46172066062056,
83.899179609167));
#204445=CARTESIAN_POINT('Ctrl Pts',(2.19414528354477,-6.40140730423383,
83.9079294115392));
#204446=CARTESIAN_POINT('Ctrl Pts',(2.37010749864279,-6.34109452518538,
83.9166791301555));
#204447=CARTESIAN_POINT('Ctrl Pts',(2.54358134866741,-6.2735223961639,83.9254288487718));
#204448=CARTESIAN_POINT('Ctrl Pts',(2.71397759435839,-6.19892043966695,
83.9341785673881));
#204449=CARTESIAN_POINT('Ctrl Pts',(2.88437226558397,-6.12431917249386,
83.9429282051568));
#204450=CARTESIAN_POINT('Ctrl Pts',(3.0516891268122,-6.04268832278665,83.9516778429255));
#204451=CARTESIAN_POINT('Ctrl Pts',(3.21535986274109,-5.95430516123197,
83.9604274806942));
#204452=CARTESIAN_POINT('Ctrl Pts',(3.37902914073103,-5.8659227869729,83.9691770405233));
#204453=CARTESIAN_POINT('Ctrl Pts',(3.53905210621839,-5.77078835741778,
83.9779266003524));
#204454=CARTESIAN_POINT('Ctrl Pts',(3.6948852283197,-5.66922500431451,83.9866761601815));
#204455=CARTESIAN_POINT('Ctrl Pts',(3.85071701407212,-5.56766252216905,
83.9954256449786));
#204456=CARTESIAN_POINT('Ctrl Pts',(4.00235878822675,-5.45967138329171,
84.0041751297757));
#204457=CARTESIAN_POINT('Ctrl Pts',(4.14929549611595,-5.34561838199398,
84.0129246145728));
#204458=CARTESIAN_POINT('Ctrl Pts',(4.29623099276359,-5.23156632086795,
84.0216740272454));
#204459=CARTESIAN_POINT('Ctrl Pts',(4.43846127436296,-5.11145267304732,
84.030423439918));
#204460=CARTESIAN_POINT('Ctrl Pts',(4.57550326054708,-4.98568540049641,
84.0391728525906));
#204461=CARTESIAN_POINT('Ctrl Pts',(4.71254416258032,-4.85991912290116,
84.0479221960458));
#204462=CARTESIAN_POINT('Ctrl Pts',(4.84439664018998,-4.72849950385176,
84.0566715395011));
#204463=CARTESIAN_POINT('Ctrl Pts',(4.97061286794968,-4.59187289860827,
84.0654208829563));
#204464=CARTESIAN_POINT('Ctrl Pts',(5.09682813912903,-4.45524732884435,
84.0741701601011));
#204465=CARTESIAN_POINT('Ctrl Pts',(5.21740705148052,-4.31341506235529,
84.082919437246));
#204466=CARTESIAN_POINT('Ctrl Pts',(5.33194007545904,-4.16685781275457,
84.0916687143908));
#204467=CARTESIAN_POINT('Ctrl Pts',(5.44647226944677,-4.02030162521581,
84.1004179281319));
#204468=CARTESIAN_POINT('Ctrl Pts',(5.55495848628289,-3.86902074887681,
84.1091671418731));
#204469=CARTESIAN_POINT('Ctrl Pts',(5.65703027291949,-3.71352898080418,
84.1179163556142));
#204470=CARTESIAN_POINT('Ctrl Pts',(5.7591013537715,-3.55803828789341,84.1266655088581));
#204471=CARTESIAN_POINT('Ctrl Pts',(5.85475793592897,-3.39833700106464,
84.1354146621019));
#204472=CARTESIAN_POINT('Ctrl Pts',(5.94367514427535,-3.23496750823304,
84.1441638153458));
#204473=CARTESIAN_POINT('Ctrl Pts',(6.03259176732768,-3.07159909077474,
84.1529129109987));
#204474=CARTESIAN_POINT('Ctrl Pts',(6.11476896836043,-2.90456276731183,
84.1616620066516));
#204475=CARTESIAN_POINT('Ctrl Pts',(6.18992765547997,-2.73442583002799,
84.1704111023046));
#204476=CARTESIAN_POINT('Ctrl Pts',(6.26508587283153,-2.56428995615927,
84.1791601432726));
#204477=CARTESIAN_POINT('Ctrl Pts',(6.33322554827248,-2.39105376934968,
84.1879091842406));
#204478=CARTESIAN_POINT('Ctrl Pts',(6.39411526733108,-2.21530561053855,
84.1966582252087));
#204479=CARTESIAN_POINT('Ctrl Pts',(6.45500462602914,-2.03955849184886,
84.2054072143977));
#204480=CARTESIAN_POINT('Ctrl Pts',(6.50864402040797,-1.86129970164345,
84.2141562035867));
#204481=CARTESIAN_POINT('Ctrl Pts',(6.55485128368649,-1.68113463135873,
84.2229051927757));
#204482=CARTESIAN_POINT('Ctrl Pts',(6.60199809554365,-1.49730620116697,
84.2318320782472));
#204483=CARTESIAN_POINT('Ctrl Pts',(6.64140720707904,-1.31149343245541,
84.2407589637186));
#204484=CARTESIAN_POINT('Ctrl Pts',(6.67293928722908,-1.12435326697383,
84.24968584919));
#204485=CARTESIAN_POINT('Ctrl Pts',(6.70384625876276,-0.940923067005181,
84.2584357633675));
#204486=CARTESIAN_POINT('Ctrl Pts',(6.72718554579811,-0.756217899520276,
84.2671856775449));
#204487=CARTESIAN_POINT('Ctrl Pts',(6.74287786815339,-0.57086518125313,
84.2759355917224));
#204488=CARTESIAN_POINT('Ctrl Pts',(6.75856988190853,-0.385516108072647,
84.2846853338269));
#204489=CARTESIAN_POINT('Ctrl Pts',(6.76661520773406,-0.199519795225118,
84.2934350759314));
#204490=CARTESIAN_POINT('Ctrl Pts',(6.76698651789579,-0.0135080204544889,
84.3021848180358));
#204491=CARTESIAN_POINT('Ctrl Pts',(6.767357821249,0.172500343514049,84.3109343997008));
#204492=CARTESIAN_POINT('Ctrl Pts',(6.76005538995178,0.358523882211937,
84.3196839813658));
#204493=CARTESIAN_POINT('Ctrl Pts',(6.74510402742353,0.54393074856532,84.3284335630308));
#204494=CARTESIAN_POINT('Ctrl Pts',(6.73015291918021,0.729334461616109,
84.3371829958874));
#204495=CARTESIAN_POINT('Ctrl Pts',(6.70755316306584,0.914121237635484,
84.3459324287441));
#204496=CARTESIAN_POINT('Ctrl Pts',(6.67738151874562,1.09766345166195,84.3546818616008));
#204497=CARTESIAN_POINT('Ctrl Pts',(6.64721034747555,1.28120278799737,84.3634311572783));
#204498=CARTESIAN_POINT('Ctrl Pts',(6.60946757205126,1.46349731860402,84.3721804529558));
#204499=CARTESIAN_POINT('Ctrl Pts',(6.56428138111505,1.64392790278234,84.3809297486334));
#204500=CARTESIAN_POINT('Ctrl Pts',(6.51909583859829,1.8243558977913,84.389678918759));
#204501=CARTESIAN_POINT('Ctrl Pts',(6.46646716392852,2.00291972192341,84.3984280888846));
#204502=CARTESIAN_POINT('Ctrl Pts',(6.40657409872857,2.1790129227474,84.4071772590102));
#204503=CARTESIAN_POINT('Ctrl Pts',(6.34668181342049,2.35510383059051,84.4159263152093));
#204504=CARTESIAN_POINT('Ctrl Pts',(6.27952541914021,2.52872390822651,84.4246753714084));
#204505=CARTESIAN_POINT('Ctrl Pts',(6.20533299175487,2.69928350890354,84.4334244276075));
#204506=CARTESIAN_POINT('Ctrl Pts',(6.12831602991515,2.87633637965694,84.4425065637657));
#204507=CARTESIAN_POINT('Ctrl Pts',(6.04371690605233,3.05009086601535,84.4515886999239));
#204508=CARTESIAN_POINT('Ctrl Pts',(5.9518452031659,3.2199111288281,84.460670836082));
#204509=CARTESIAN_POINT('Ctrl Pts',(5.8633354950923,3.38351691183094,84.4694206164256));
#204510=CARTESIAN_POINT('Ctrl Pts',(5.7680761809932,3.54347103712082,84.4781703967692));
#204511=CARTESIAN_POINT('Ctrl Pts',(5.66639083308964,3.69923018027775,84.4869201771128));
#204512=CARTESIAN_POINT('Ctrl Pts',(5.56470914082143,3.85498372382133,84.4956696428977));
#204513=CARTESIAN_POINT('Ctrl Pts',(5.45660203372004,4.00654234702084,84.5044191086826));
#204514=CARTESIAN_POINT('Ctrl Pts',(5.34243669839147,4.15339127986758,84.5131685744675));
#204515=CARTESIAN_POINT('Ctrl Pts',(5.22827486050518,4.30023571401369,84.5219177722135));
#204516=CARTESIAN_POINT('Ctrl Pts',(5.10805534167033,4.44237052028559,84.5306669699595));
#204517=CARTESIAN_POINT('Ctrl Pts',(4.98218644339869,4.5793129662881,84.5394161677056));
#204518=CARTESIAN_POINT('Ctrl Pts',(4.85632073219513,4.71625194483436,84.5481651439172));
#204519=CARTESIAN_POINT('Ctrl Pts',(4.72480612170254,4.84799861524571,84.5569141201288));
#204520=CARTESIAN_POINT('Ctrl Pts',(4.58808925235257,4.97410554898535,84.5656630963404));
#204521=CARTESIAN_POINT('Ctrl Pts',(4.45136349473991,5.10022068121257,84.5744126413421));
#204522=CARTESIAN_POINT('Ctrl Pts',(4.3094350121002,5.22069514871884,84.5831621863439));
#204523=CARTESIAN_POINT('Ctrl Pts',(4.16278587431718,5.33511975166306,84.5919117313456));
#204524=CARTESIAN_POINT('Ctrl Pts',(4.01614535740373,5.44953762807898,84.6006607619993));
#204525=CARTESIAN_POINT('Ctrl Pts',(3.86478496657836,5.55790617532845,84.609409792653));
#204526=CARTESIAN_POINT('Ctrl Pts',(3.70921874747096,5.65985735539421,84.6181588233068));
#204527=CARTESIAN_POINT('Ctrl Pts',(3.55365041605799,5.76180991977109,84.6269079727564));
#204528=CARTESIAN_POINT('Ctrl Pts',(3.39387638174418,5.85734478552874,84.635657122206));
#204529=CARTESIAN_POINT('Ctrl Pts',(3.23043927904432,5.9461374912129,84.6444062716556));
#204530=CARTESIAN_POINT('Ctrl Pts',(3.18691767070357,5.96978206944186,84.6467360795718));
#204531=CARTESIAN_POINT('Ctrl Pts',(3.14313645919591,5.99294880633446,84.6490658874879));
#204532=CARTESIAN_POINT('Ctrl Pts',(3.09910619832133,6.0156321173694,84.651395695404));
#204533=CARTESIAN_POINT('Origin',(0.,0.,4.30282021618968));
#204534=CARTESIAN_POINT('',(3.09910619832123,6.01563211736946,87.0457552630241));
#204535=CARTESIAN_POINT('',(3.09910619832139,6.01563211736938,86.6514537215909));
#204536=CARTESIAN_POINT('',(3.09910619832133,6.0156321173694,4.30282021618968));
#204537=CARTESIAN_POINT('',(-6.767,3.23394441651206E-12,85.6971797838099));
#204538=CARTESIAN_POINT('Ctrl Pts',(-6.767,3.23394454464685E-12,85.6971797838099));
#204539=CARTESIAN_POINT('Ctrl Pts',(-6.76700000000009,-0.186007249523693,
85.7059292956211));
#204540=CARTESIAN_POINT('Ctrl Pts',(-6.75932637294538,-0.372014355746796,
85.7146788074323));
#204541=CARTESIAN_POINT('Ctrl Pts',(-6.74400518264206,-0.557389537484432,
85.7234283192435));
#204542=CARTESIAN_POINT('Ctrl Pts',(-6.72868405705119,-0.742763936248805,
85.7321777940991));
#204543=CARTESIAN_POINT('Ctrl Pts',(-6.70571545645765,-0.927506130239353,
85.7409272689548));
#204544=CARTESIAN_POINT('Ctrl Pts',(-6.67517739404848,-1.11098863989877,
85.7496767438105));
#204545=CARTESIAN_POINT('Ctrl Pts',(-6.64463945808725,-1.29447038981831,
85.7584261824375));
#204546=CARTESIAN_POINT('Ctrl Pts',(-6.60653217008376,-1.47669218313591,
85.7671756210645));
#204547=CARTESIAN_POINT('Ctrl Pts',(-6.56098496092695,-1.65703510599216,
85.7759250596916));
#204548=CARTESIAN_POINT('Ctrl Pts',(-6.51543793658314,-1.83737729708641,
85.7846744628167));
#204549=CARTESIAN_POINT('Ctrl Pts',(-6.46245112167436,-2.01584035510878,
85.7934238659419));
#204550=CARTESIAN_POINT('Ctrl Pts',(-6.40220448374266,-2.19181813760754,
85.8021732690671));
#204551=CARTESIAN_POINT('Ctrl Pts',(-6.34195808526511,-2.36779522067127,
85.8109226374172));
#204552=CARTESIAN_POINT('Ctrl Pts',(-6.27445201433103,-2.54128677684169,
85.8196720057673));
#204553=CARTESIAN_POINT('Ctrl Pts',(-6.19991555071892,-2.71170355384834,
85.8284213741174));
#204554=CARTESIAN_POINT('Ctrl Pts',(-6.12537937716685,-2.88211966767492,
85.8371707084192));
#204555=CARTESIAN_POINT('Ctrl Pts',(-6.04381298052516,-3.04946076371794,
85.8459200427209));
#204556=CARTESIAN_POINT('Ctrl Pts',(-5.95549339335831,-3.21315848374548,
85.8546693770227));
#204557=CARTESIAN_POINT('Ctrl Pts',(-5.86717414255401,-3.37685558033507,
85.8634186780029));
#204558=CARTESIAN_POINT('Ctrl Pts',(-5.77210188876583,-3.53690907646783,
85.8721679789831));
#204559=CARTESIAN_POINT('Ctrl Pts',(-5.67059953346971,-3.69277536969325,
85.8809172799633));
#204560=CARTESIAN_POINT('Ctrl Pts',(-5.56909755631362,-3.84864108224955,
85.8896665483486));
#204561=CARTESIAN_POINT('Ctrl Pts',(-5.46116568196832,-4.00031938297542,
85.8984158167339));
#204562=CARTESIAN_POINT('Ctrl Pts',(-5.34717048533588,-4.14729511859873,
85.9071650851191));
#204563=CARTESIAN_POINT('Ctrl Pts',(-5.2331757039183,-4.29427031887923,
85.9159143216362));
#204564=CARTESIAN_POINT('Ctrl Pts',(-5.11311782003516,-4.43654276189544,
85.9246635581532));
#204565=CARTESIAN_POINT('Ctrl Pts',(-4.98740458984765,-4.57362924351839,
85.9334127946702));
#204566=CARTESIAN_POINT('Ctrl Pts',(-4.86169180711756,-4.71071523720254,
85.9421620000457));
#204567=CARTESIAN_POINT('Ctrl Pts',(-4.73032391204184,-4.84261509523225,
85.9509112054211));
#204568=CARTESIAN_POINT('Ctrl Pts',(-4.59374707013612,-4.96888084538318,
85.9596604107966));
#204569=CARTESIAN_POINT('Ctrl Pts',(-4.45717070301458,-5.09514615659453,
85.968409585757));
#204570=CARTESIAN_POINT('Ctrl Pts',(-4.31538563571053,-5.21577720459517,
85.9771587607174));
#204571=CARTESIAN_POINT('Ctrl Pts',(-4.16887341029521,-5.33036429232877,
85.9859079356779));
#204572=CARTESIAN_POINT('Ctrl Pts',(-4.02236168203715,-5.44495099123609,
85.9946570809499));
#204573=CARTESIAN_POINT('Ctrl Pts',(-3.87112305348171,-5.55349359438598,
86.0034062262219));
#204574=CARTESIAN_POINT('Ctrl Pts',(-3.71567117017763,-5.65562346298892,
86.012155371494));
#204575=CARTESIAN_POINT('Ctrl Pts',(-3.56021980145826,-5.7577529935164,
86.0209044878041));
#204576=CARTESIAN_POINT('Ctrl Pts',(-3.4005554453836,-5.85346967463866,
86.0296536041143));
#204577=CARTESIAN_POINT('Ctrl Pts',(-3.2372203598687,-5.94244842986892,
86.0384027204245));
#204578=CARTESIAN_POINT('Ctrl Pts',(-3.07388580147185,-6.03142689794527,
86.0471518084993));
#204579=CARTESIAN_POINT('Ctrl Pts',(-2.90688078896572,-6.11366734656785,
86.0559008965742));
#204580=CARTESIAN_POINT('Ctrl Pts',(-2.73677250721351,-6.18889046952362,
86.064649984649));
#204581=CARTESIAN_POINT('Ctrl Pts',(-2.56666476031465,-6.26411335596334,
86.073399045215));
#204582=CARTESIAN_POINT('Ctrl Pts',(-2.3934540257515,-6.33231884500562,
86.0821481057811));
#204583=CARTESIAN_POINT('Ctrl Pts',(-2.21772856065578,-6.39327529762732,
86.0908971663471));
#204584=CARTESIAN_POINT('Ctrl Pts',(-2.04200363348489,-6.45423156365119,
86.0996462001308));
#204585=CARTESIAN_POINT('Ctrl Pts',(-1.86376426189243,-6.50793874375669,
86.1083952339145));
#204586=CARTESIAN_POINT('Ctrl Pts',(-1.68361577753108,-6.55421443909554,
86.1171442676982));
#204587=CARTESIAN_POINT('Ctrl Pts',(-1.50346782967784,-6.60048999661871,
86.125893275426));
#204588=CARTESIAN_POINT('Ctrl Pts',(-1.32141105795003,-6.63933404237708,
86.1346422831538));
#204589=CARTESIAN_POINT('Ctrl Pts',(-1.13806375487071,-6.67061465607553,
86.1433912908816));
#204590=CARTESIAN_POINT('Ctrl Pts',(-0.954716982604021,-6.70189517921281,
86.15214027328));
#204591=CARTESIAN_POINT('Ctrl Pts',(-0.770079968903664,-6.72561226592209,
86.1608892556784));
#204592=CARTESIAN_POINT('Ctrl Pts',(-0.584779765560293,-6.74168536983085,
86.1696382380768));
#204593=CARTESIAN_POINT('Ctrl Pts',(-0.391489830653286,-6.75845151013842,
86.1787644570866));
#204594=CARTESIAN_POINT('Ctrl Pts',(-0.197478578240259,-6.7668998303162,
86.1878906760965));
#204595=CARTESIAN_POINT('Ctrl Pts',(-0.00346287645320154,-6.76699911397118,
86.1970168951064));
#204596=CARTESIAN_POINT('Ctrl Pts',(0.184489834652916,-6.76709529501194,
86.2058579197722));
#204597=CARTESIAN_POINT('Ctrl Pts',(0.372446404248391,-6.75935639738173,
86.214698944438));
#204598=CARTESIAN_POINT('Ctrl Pts',(0.559755019487351,-6.74380925873195,
86.2235399691038));
#204599=CARTESIAN_POINT('Ctrl Pts',(0.745134705520902,-6.72842222659816,
86.2322899477135));
#204600=CARTESIAN_POINT('Ctrl Pts',(0.929879431227806,-6.70538706057534,
86.2410399263233));
#204601=CARTESIAN_POINT('Ctrl Pts',(1.11336163626761,-6.67478200894138,
86.249789904933));
#204602=CARTESIAN_POINT('Ctrl Pts',(1.29684196300673,-6.64417727061022,
86.2585397939696));
#204603=CARTESIAN_POINT('Ctrl Pts',(1.47905951217484,-6.60600284890597,
86.2672896830061));
#204604=CARTESIAN_POINT('Ctrl Pts',(1.65939532067077,-6.56038841607233,
86.2760395720427));
#204605=CARTESIAN_POINT('Ctrl Pts',(1.83972934300797,-6.51477443503258,
86.2847893744148));
#204606=CARTESIAN_POINT('Ctrl Pts',(2.01818138406261,-6.46172066062142,
86.293539176787));
#204607=CARTESIAN_POINT('Ctrl Pts',(2.19414528354198,-6.40140730423479,
86.3022889791592));
#204608=CARTESIAN_POINT('Ctrl Pts',(2.37010749864,-6.34109452518642,86.3110386977755));
#204609=CARTESIAN_POINT('Ctrl Pts',(2.54358134866462,-6.27352239616503,
86.3197884163918));
#204610=CARTESIAN_POINT('Ctrl Pts',(2.71397759435559,-6.19892043966817,
86.3285381350081));
#204611=CARTESIAN_POINT('Ctrl Pts',(2.88437226558136,-6.1243191724951,86.3372877727768));
#204612=CARTESIAN_POINT('Ctrl Pts',(3.05168912680975,-6.04268832278789,
86.3460374105455));
#204613=CARTESIAN_POINT('Ctrl Pts',(3.21535986273881,-5.9543051612332,86.3547870483143));
#204614=CARTESIAN_POINT('Ctrl Pts',(3.37902914072875,-5.86592278697421,
86.3635366081433));
#204615=CARTESIAN_POINT('Ctrl Pts',(3.53905210621612,-5.77078835741917,
86.3722861679724));
#204616=CARTESIAN_POINT('Ctrl Pts',(3.69488522831744,-5.66922500431599,
86.3810357278015));
#204617=CARTESIAN_POINT('Ctrl Pts',(3.85071701406992,-5.56766252217057,
86.3897852125986));
#204618=CARTESIAN_POINT('Ctrl Pts',(4.00235878822462,-5.45967138329328,
86.3985346973957));
#204619=CARTESIAN_POINT('Ctrl Pts',(4.14929549611388,-5.34561838199558,
86.4072841821928));
#204620=CARTESIAN_POINT('Ctrl Pts',(4.29623099276148,-5.23156632086967,
86.4160335948654));
#204621=CARTESIAN_POINT('Ctrl Pts',(4.43846127436082,-5.11145267304917,
86.424783007538));
#204622=CARTESIAN_POINT('Ctrl Pts',(4.57550326054493,-4.98568540049838,
86.4335324202106));
#204623=CARTESIAN_POINT('Ctrl Pts',(4.71254416257829,-4.85991912290314,
86.4422817636658));
#204624=CARTESIAN_POINT('Ctrl Pts',(4.84439664018807,-4.72849950385372,
86.4510311071211));
#204625=CARTESIAN_POINT('Ctrl Pts',(4.97061286794788,-4.59187289861021,
86.4597804505763));
#204626=CARTESIAN_POINT('Ctrl Pts',(5.09682813912722,-4.45524732884642,
86.4685297277211));
#204627=CARTESIAN_POINT('Ctrl Pts',(5.2174070514787,-4.31341506235749,86.477279004866));
#204628=CARTESIAN_POINT('Ctrl Pts',(5.33194007545723,-4.1668578127569,86.4860282820108));
#204629=CARTESIAN_POINT('Ctrl Pts',(5.44647226944507,-4.02030162521812,
86.4947774957519));
#204630=CARTESIAN_POINT('Ctrl Pts',(5.55495848628131,-3.86902074887908,
86.503526709493));
#204631=CARTESIAN_POINT('Ctrl Pts',(5.65703027291801,-3.71352898080642,
86.5122759232341));
#204632=CARTESIAN_POINT('Ctrl Pts',(5.75910135377003,-3.55803828789578,
86.521025076478));
#204633=CARTESIAN_POINT('Ctrl Pts',(5.85475793592752,-3.39833700106713,
86.5297742297219));
#204634=CARTESIAN_POINT('Ctrl Pts',(5.94367514427392,-3.23496750823566,
86.5385233829658));
#204635=CARTESIAN_POINT('Ctrl Pts',(6.03259176732633,-3.07159909077738,
86.5472724786187));
#204636=CARTESIAN_POINT('Ctrl Pts',(6.11476896835918,-2.90456276731448,
86.5560215742716));
#204637=CARTESIAN_POINT('Ctrl Pts',(6.1899276554788,-2.73442583003065,86.5647706699245));
#204638=CARTESIAN_POINT('Ctrl Pts',(6.26508587283052,-2.56428995616176,
86.5735197108926));
#204639=CARTESIAN_POINT('Ctrl Pts',(6.33322554827161,-2.39105376935199,
86.5822687518606));
#204640=CARTESIAN_POINT('Ctrl Pts',(6.39411526733035,-2.21530561054067,
86.5910177928287));
#204641=CARTESIAN_POINT('Ctrl Pts',(6.45500462602845,-2.03955849185104,
86.5997667820177));
#204642=CARTESIAN_POINT('Ctrl Pts',(6.50864402040733,-1.86129970164568,
86.6085157712067));
#204643=CARTESIAN_POINT('Ctrl Pts',(6.5548512836859,-1.68113463136101,86.6172647603957));
#204644=CARTESIAN_POINT('Ctrl Pts',(6.60199809554315,-1.49730620116918,
86.6261916458672));
#204645=CARTESIAN_POINT('Ctrl Pts',(6.64140720707862,-1.31149343245754,
86.6351185313386));
#204646=CARTESIAN_POINT('Ctrl Pts',(6.67293928722873,-1.12435326697588,
86.64404541681));
#204647=CARTESIAN_POINT('Ctrl Pts',(6.70384625876248,-0.940923067007218,
86.6527953309875));
#204648=CARTESIAN_POINT('Ctrl Pts',(6.72718554579789,-0.756217899522293,
86.661545245165));
#204649=CARTESIAN_POINT('Ctrl Pts',(6.74287786815322,-0.570865181255125,
86.6702951593424));
#204650=CARTESIAN_POINT('Ctrl Pts',(6.75856988190842,-0.38551610807462,
86.6790449014469));
#204651=CARTESIAN_POINT('Ctrl Pts',(6.76661520773401,-0.199519795227065,
86.6877946435514));
#204652=CARTESIAN_POINT('Ctrl Pts',(6.76698651789579,-0.0135080204564092,
86.6965443856559));
#204653=CARTESIAN_POINT('Ctrl Pts',(6.76735782124905,0.172500343512155,
86.7052939673208));
#204654=CARTESIAN_POINT('Ctrl Pts',(6.76005538995188,0.358523882210071,
86.7140435489858));
#204655=CARTESIAN_POINT('Ctrl Pts',(6.74510402742368,0.543930748563485,
86.7227931306508));
#204656=CARTESIAN_POINT('Ctrl Pts',(6.7301529191804,0.729334461614369,86.7315425635075));
#204657=CARTESIAN_POINT('Ctrl Pts',(6.70755316306606,0.914121237633841,
86.7402919963641));
#204658=CARTESIAN_POINT('Ctrl Pts',(6.67738151874588,1.0976634516604,86.7490414292208));
#204659=CARTESIAN_POINT('Ctrl Pts',(6.64721034747584,1.28120278799586,86.7577907248984));
#204660=CARTESIAN_POINT('Ctrl Pts',(6.60946757205158,1.46349731860254,86.7665400205759));
#204661=CARTESIAN_POINT('Ctrl Pts',(6.56428138111541,1.6439279027809,86.7752893162534));
#204662=CARTESIAN_POINT('Ctrl Pts',(6.5190958385987,1.82435589778983,86.784038486379));
#204663=CARTESIAN_POINT('Ctrl Pts',(6.46646716392898,2.00291972192192,86.7927876565046));
#204664=CARTESIAN_POINT('Ctrl Pts',(6.40657409872909,2.17901292274589,86.8015368266302));
#204665=CARTESIAN_POINT('Ctrl Pts',(6.34668181342099,2.35510383058916,86.8102858828293));
#204666=CARTESIAN_POINT('Ctrl Pts',(6.2795254191407,2.52872390822532,86.8190349390284));
#204667=CARTESIAN_POINT('Ctrl Pts',(6.20533299175532,2.6992835089025,86.8277839952275));
#204668=CARTESIAN_POINT('Ctrl Pts',(6.1283160299156,2.876336379656,86.8368661313857));
#204669=CARTESIAN_POINT('Ctrl Pts',(6.04371690605276,3.05009086601451,86.845948267544));
#204670=CARTESIAN_POINT('Ctrl Pts',(5.95184520316631,3.21991112882734,86.8550304037022));
#204671=CARTESIAN_POINT('Ctrl Pts',(5.86333549509272,3.38351691183022,86.8637801840457));
#204672=CARTESIAN_POINT('Ctrl Pts',(5.76807618099362,3.54347103712014,86.8725299643893));
#204673=CARTESIAN_POINT('Ctrl Pts',(5.66639083309006,3.6992301802771,86.8812797447329));
#204674=CARTESIAN_POINT('Ctrl Pts',(5.56470914082193,3.85498372382061,86.8900292105178));
#204675=CARTESIAN_POINT('Ctrl Pts',(5.45660203372061,4.00654234702005,86.8987786763027));
#204676=CARTESIAN_POINT('Ctrl Pts',(5.34243669839213,4.15339127986673,86.9075281420876));
#204677=CARTESIAN_POINT('Ctrl Pts',(5.22827486050581,4.30023571401293,86.9162773398336));
#204678=CARTESIAN_POINT('Ctrl Pts',(5.10805534167092,4.44237052028491,86.9250265375796));
#204679=CARTESIAN_POINT('Ctrl Pts',(4.98218644339924,4.5793129662875,86.9337757353256));
#204680=CARTESIAN_POINT('Ctrl Pts',(4.85632073219563,4.71625194483385,86.9425247115373));
#204681=CARTESIAN_POINT('Ctrl Pts',(4.72480612170299,4.84799861524527,86.9512736877489));
#204682=CARTESIAN_POINT('Ctrl Pts',(4.58808925235296,4.97410554898499,86.9600226639605));
#204683=CARTESIAN_POINT('Ctrl Pts',(4.45136349474034,5.10022068121219,86.9687722089622));
#204684=CARTESIAN_POINT('Ctrl Pts',(4.30943501210067,5.22069514871845,86.9775217539639));
#204685=CARTESIAN_POINT('Ctrl Pts',(4.16278587431769,5.33511975166267,86.9862712989656));
#204686=CARTESIAN_POINT('Ctrl Pts',(4.01614535740428,5.44953762807857,86.9950203296194));
#204687=CARTESIAN_POINT('Ctrl Pts',(3.86478496657895,5.55790617532803,87.0037693602731));
#204688=CARTESIAN_POINT('Ctrl Pts',(3.7092187474716,5.6598573553938,87.0125183909269));
#204689=CARTESIAN_POINT('Ctrl Pts',(3.55365041605866,5.76180991977067,87.0212675403765));
#204690=CARTESIAN_POINT('Ctrl Pts',(3.3938763817449,5.85734478552832,87.0300166898261));
#204691=CARTESIAN_POINT('Ctrl Pts',(3.23043927904508,5.94613749121249,87.0387658392757));
#204692=CARTESIAN_POINT('Ctrl Pts',(3.18691767070404,5.96978206944161,87.0410956471919));
#204693=CARTESIAN_POINT('Ctrl Pts',(3.1431364591961,5.99294880633436,87.043425455108));
#204694=CARTESIAN_POINT('Ctrl Pts',(3.09910619832123,6.01563211736946,87.0457552630241));
#204695=CARTESIAN_POINT('Ctrl Pts',(3.09910619832135,6.0156321173694,85.0458695769521));
#204696=CARTESIAN_POINT('Ctrl Pts',(2.95819911900836,6.08822399040388,85.0533117780863));
#204697=CARTESIAN_POINT('Ctrl Pts',(2.81469155616859,6.15588807595813,85.0607539792206));
#204698=CARTESIAN_POINT('Ctrl Pts',(2.66893775428139,6.21844516449019,85.0681961803548));
#204699=CARTESIAN_POINT('Ctrl Pts',(2.50393692119552,6.28926302028242,85.076621136488));
#204700=CARTESIAN_POINT('Ctrl Pts',(2.33612920776672,6.35350388484595,85.0850460926212));
#204701=CARTESIAN_POINT('Ctrl Pts',(2.16606800253779,6.41096236210929,85.0934710487543));
#204702=CARTESIAN_POINT('Ctrl Pts',(1.99596732446964,6.46843417603711,85.1018979604007));
#204703=CARTESIAN_POINT('Ctrl Pts',(1.82361242586232,6.5191203576838,85.1103248720472));
#204704=CARTESIAN_POINT('Ctrl Pts',(1.64957246988648,6.56286520253103,85.1187517836936));
#204705=CARTESIAN_POINT('Ctrl Pts',(1.47546851264278,6.60662613406086,85.1271817942435));
#204706=CARTESIAN_POINT('Ctrl Pts',(1.29967858393249,6.64344055835283,85.1356118047934));
#204707=CARTESIAN_POINT('Ctrl Pts',(1.12278304682798,6.67320367063345,85.1440418153433));
#204708=CARTESIAN_POINT('Ctrl Pts',(0.945724557251994,6.70299420007101,
85.1524795914428));
#204709=CARTESIAN_POINT('Ctrl Pts',(0.767558751721852,6.72572038496047,
85.1609173675422));
#204710=CARTESIAN_POINT('Ctrl Pts',(0.58887326327967,6.74132904402347,85.1693551436416));
#204711=CARTESIAN_POINT('Ctrl Pts',(0.410093978127306,6.75694589648193,
85.1777973489516));
#204712=CARTESIAN_POINT('Ctrl Pts',(0.230794796639656,6.76543775071114,
85.1862395542615));
#204713=CARTESIAN_POINT('Ctrl Pts',(0.0515649678104242,6.76680353299065,
85.1946817595714));
#204714=CARTESIAN_POINT('Ctrl Pts',(-0.127853938626412,6.76817075609531,
85.2031328709434));
#204715=CARTESIAN_POINT('Ctrl Pts',(-0.307203014981049,6.76239689544306,
85.2115839823154));
#204716=CARTESIAN_POINT('Ctrl Pts',(-0.48589543792917,6.74953291890629,
85.2200350936874));
#204717=CARTESIAN_POINT('Ctrl Pts',(-0.536045743225493,6.74592262396484,
85.2224069111848));
#204718=CARTESIAN_POINT('Ctrl Pts',(-0.586144369622427,6.74175418650349,
85.2247787286822));
#204719=CARTESIAN_POINT('Ctrl Pts',(-0.636178460520079,6.73702946159287,
85.2271505461796));
#204720=CARTESIAN_POINT('Ctrl Pts',(-0.811612333427688,6.72046322096327,
85.2354668185837));
#204721=CARTESIAN_POINT('Ctrl Pts',(-0.986568801570855,6.69702410260573,
85.2437830909879));
#204722=CARTESIAN_POINT('Ctrl Pts',(-1.16047802969381,6.66675181348443,
85.252099363392));
#204723=CARTESIAN_POINT('Ctrl Pts',(-1.33424021735945,6.63650511961927,
85.260408604378));
#204724=CARTESIAN_POINT('Ctrl Pts',(-1.50695658807425,6.5994368251738,85.2687178453639));
#204725=CARTESIAN_POINT('Ctrl Pts',(-1.67806259715569,6.55563840674782,
85.2770270863499));
#204726=CARTESIAN_POINT('Ctrl Pts',(-1.84905530757672,6.51186898965361,
85.2853308253324));
#204727=CARTESIAN_POINT('Ctrl Pts',(-2.01843944515858,6.46137841441279,
85.2936345643148));
#204728=CARTESIAN_POINT('Ctrl Pts',(-2.18566060489128,6.40430923052801,
85.3019383032972));
#204729=CARTESIAN_POINT('Ctrl Pts',(-2.35280168409568,6.34726737650031,
85.3102380657028));
#204730=CARTESIAN_POINT('Ctrl Pts',(-2.51778152113153,6.2836533044426,85.3185378281083));
#204731=CARTESIAN_POINT('Ctrl Pts',(-2.68006061094702,6.21365947905502,
85.3268375905138));
#204732=CARTESIAN_POINT('Ctrl Pts',(-2.84229171696341,6.14368634992387,
85.3351348987884));
#204733=CARTESIAN_POINT('Ctrl Pts',(-3.00182334843409,6.06733736524985,
85.3434322070629));
#204734=CARTESIAN_POINT('Ctrl Pts',(-3.15813552791922,5.98485329705703,
85.3517295153375));
#204735=CARTESIAN_POINT('Ctrl Pts',(-3.31446350048274,5.90236089504557,
85.3600276619348));
#204736=CARTESIAN_POINT('Ctrl Pts',(-3.46757105987245,5.81373232664027,
85.368325808532));
#204737=CARTESIAN_POINT('Ctrl Pts',(-3.61696189367654,5.71925481681764,
85.3766239551292));
#204738=CARTESIAN_POINT('Ctrl Pts',(-3.76636774966895,5.62476780668695,
85.3849229361573));
#204739=CARTESIAN_POINT('Ctrl Pts',(-3.91205584060509,5.5244308684518,85.3932219171854));
#204740=CARTESIAN_POINT('Ctrl Pts',(-4.05355805395681,5.41857509897223,
85.4015208982135));
#204741=CARTESIAN_POINT('Ctrl Pts',(-4.19509801231297,5.31269109299801,
85.4098220929531));
#204742=CARTESIAN_POINT('Ctrl Pts',(-4.33244958896701,5.20128553019176,
85.4181232876927));
#204743=CARTESIAN_POINT('Ctrl Pts',(-4.46517688560014,5.08473051206278,
85.4264244824323));
#204744=CARTESIAN_POINT('Ctrl Pts',(-4.59796164694242,4.96812503106455,
85.4347292712007));
#204745=CARTESIAN_POINT('Ctrl Pts',(-4.72611787672735,4.84636588087864,
85.4430340599692));
#204746=CARTESIAN_POINT('Ctrl Pts',(-4.84924560815635,4.71986292510454,
85.4513388487377));
#204747=CARTESIAN_POINT('Ctrl Pts',(-4.97251930640533,4.5932100012123,85.4596534827587));
#204748=CARTESIAN_POINT('Ctrl Pts',(-5.09075235283867,4.46180228524923,
85.4679681167797));
#204749=CARTESIAN_POINT('Ctrl Pts',(-5.20358347502239,4.32608460602355,
85.4762827508007));
#204750=CARTESIAN_POINT('Ctrl Pts',(-5.31648594132527,4.19028111130573,
85.4846026422385));
#204751=CARTESIAN_POINT('Ctrl Pts',(-5.42397946013126,4.05016249427654,
85.4929225336763));
#204752=CARTESIAN_POINT('Ctrl Pts',(-5.52574532132024,3.90620373814621,
85.5012424251142));
#204753=CARTESIAN_POINT('Ctrl Pts',(-5.6276633554689,3.76202971699739,85.5095747574874));
#204754=CARTESIAN_POINT('Ctrl Pts',(-5.72383642602608,3.6140043726023,85.5179070898606));
#204755=CARTESIAN_POINT('Ctrl Pts',(-5.81399042155263,3.46262969115876,
85.5262394222338));
#204756=CARTESIAN_POINT('Ctrl Pts',(-5.88186598152559,3.34866201608571,
85.5325127074322));
#204757=CARTESIAN_POINT('Ctrl Pts',(-5.94633065287796,3.23279636145966,
85.5387859926306));
#204758=CARTESIAN_POINT('Ctrl Pts',(-6.0072853954291,3.11525459278439,85.545059277829));
#204759=CARTESIAN_POINT('Ctrl Pts',(-6.09005780069759,2.95564084485329,
85.5535779735543));
#204760=CARTESIAN_POINT('Ctrl Pts',(-6.16659053788697,2.79248414834737,
85.5620966692796));
#204761=CARTESIAN_POINT('Ctrl Pts',(-6.23657570988366,2.62629252271889,
85.5706153650049));
#204762=CARTESIAN_POINT('Ctrl Pts',(-6.30643161256696,2.46040786893491,
85.5791183258836));
#204763=CARTESIAN_POINT('Ctrl Pts',(-6.36976392634525,2.29149974865825,
85.5876212867623));
#204764=CARTESIAN_POINT('Ctrl Pts',(-6.42630967810643,2.12010210156863,
85.5961242476409));
#204765=CARTESIAN_POINT('Ctrl Pts',(-6.48271542230086,1.94912883591822,
85.6046061551455));
#204766=CARTESIAN_POINT('Ctrl Pts',(-6.53236801268392,1.77567863702722,
85.6130880626501));
#204767=CARTESIAN_POINT('Ctrl Pts',(-6.57505205867814,1.60030604125346,
85.6215699701548));
#204768=CARTESIAN_POINT('Ctrl Pts',(-6.61767563375348,1.42518189760665,
85.6300398612554));
#204769=CARTESIAN_POINT('Ctrl Pts',(-6.65335025806408,1.24814109133454,
85.638509752356));
#204770=CARTESIAN_POINT('Ctrl Pts',(-6.68190923369001,1.06975604355769,
85.6469796434566));
#204771=CARTESIAN_POINT('Ctrl Pts',(-6.71041353818299,0.891712482562082,
85.6554333204413));
#204772=CARTESIAN_POINT('Ctrl Pts',(-6.73182930768125,0.712330125957433,
85.6638869974259));
#204773=CARTESIAN_POINT('Ctrl Pts',(-6.74604022591236,0.53219382782244,
85.6723406744106));
#204774=CARTESIAN_POINT('Ctrl Pts',(-6.7599586881881,0.355764674596114,
85.6806203775437));
#204775=CARTESIAN_POINT('Ctrl Pts',(-6.76696587699467,0.178612617432928,
85.6889000806768));
#204776=CARTESIAN_POINT('Ctrl Pts',(-6.76699987560668,0.00129751271649814,
85.6971797838099));
#204777=CARTESIAN_POINT('',(-6.767,3.38585957231421E-12,85.3028202161898));
#204778=CARTESIAN_POINT('Ctrl Pts',(3.09910619832133,6.0156321173694,84.651395695404));
#204779=CARTESIAN_POINT('Ctrl Pts',(2.93375330764826,6.10081787314653,84.6601451433063));
#204780=CARTESIAN_POINT('Ctrl Pts',(2.76488627843069,6.17918207037039,84.6688945912086));
#204781=CARTESIAN_POINT('Ctrl Pts',(2.59307866646701,6.25045854553998,84.6776440391109));
#204782=CARTESIAN_POINT('Ctrl Pts',(2.4212724418537,6.3217344451504,84.6863934163612));
#204783=CARTESIAN_POINT('Ctrl Pts',(2.24652594672453,6.38592262741842,84.6951427936115));
#204784=CARTESIAN_POINT('Ctrl Pts',(2.06943269687104,6.44280508110567,84.7038921708618));
#204785=CARTESIAN_POINT('Ctrl Pts',(1.8923408182206,6.49968709436171,84.7126414803672));
#204786=CARTESIAN_POINT('Ctrl Pts',(1.71290249405572,6.54926340459549,84.7213907898726));
#204787=CARTESIAN_POINT('Ctrl Pts',(1.53172716625042,6.59136563150387,84.7301400993779));
#204788=CARTESIAN_POINT('Ctrl Pts',(1.35055318107316,6.63346754640714,84.7388893440452));
#204789=CARTESIAN_POINT('Ctrl Pts',(1.167642497144,6.66809542395779,84.7476385887124));
#204790=CARTESIAN_POINT('Ctrl Pts',(0.983616340614138,6.69513165624671,
84.7563878333796));
#204791=CARTESIAN_POINT('Ctrl Pts',(0.799591486713623,6.72216769715963,
84.7651370161153));
#204792=CARTESIAN_POINT('Ctrl Pts',(0.614451459526492,6.74161215869373,
84.773886198851));
#204793=CARTESIAN_POINT('Ctrl Pts',(0.428825047910062,6.75339900185713,
84.7826353815867));
#204794=CARTESIAN_POINT('Ctrl Pts',(0.243199888596733,6.76518576550222,
84.7913845052973));
#204795=CARTESIAN_POINT('Ctrl Pts',(0.0570886373915132,6.76931499599835,
84.8001336290078));
#204796=CARTESIAN_POINT('Ctrl Pts',(-0.128876626811645,6.76577266947846,
84.8088827527183));
#204797=CARTESIAN_POINT('Ctrl Pts',(-0.314840698188532,6.76223036567991,
84.8176318203099));
#204798=CARTESIAN_POINT('Ctrl Pts',(-0.500658497951505,6.75101660879221,
84.8263808879014));
#204799=CARTESIAN_POINT('Ctrl Pts',(-0.685698951926348,6.73216948296217,
84.835129955493));
#204800=CARTESIAN_POINT('Ctrl Pts',(-0.870738280460146,6.7133224717629,
84.8438789698715));
#204801=CARTESIAN_POINT('Ctrl Pts',(-1.05499998761296,6.6868422135618,84.85262798425));
#204802=CARTESIAN_POINT('Ctrl Pts',(-1.23785829161481,6.65281863948511,
84.8613769986285));
#204803=CARTESIAN_POINT('Ctrl Pts',(-1.43007412917461,6.61705395368849,
84.8705737323277));
#204804=CARTESIAN_POINT('Ctrl Pts',(-1.62073882535845,6.57295372727777,
84.8797704660269));
#204805=CARTESIAN_POINT('Ctrl Pts',(-1.80913696091563,6.52068343478266,
84.8889671997261));
#204806=CARTESIAN_POINT('Ctrl Pts',(-1.98838356186154,6.47095219815185,
84.8977171974398));
#204807=CARTESIAN_POINT('Ctrl Pts',(-2.16557827572569,6.41382586850878,
84.9064671951535));
#204808=CARTESIAN_POINT('Ctrl Pts',(-2.3401191862173,6.34949849943267,84.9152171928671));
#204809=CARTESIAN_POINT('Ctrl Pts',(-2.51465655691127,6.28517243495539,
84.9239670131254));
#204810=CARTESIAN_POINT('Ctrl Pts',(-2.68653996295356,6.21364572242362,
84.9327168333838));
#204811=CARTESIAN_POINT('Ctrl Pts',(-2.85518555380015,6.13516132252208,
84.9414666536421));
#204812=CARTESIAN_POINT('Ctrl Pts',(-3.02382794858705,6.05667841000498,
84.9502163080796));
#204813=CARTESIAN_POINT('Ctrl Pts',(-3.18923239109288,5.97123819492077,
84.9589659625171));
#204814=CARTESIAN_POINT('Ctrl Pts',(-3.35083705967695,5.87913088810715,
84.9677156169546));
#204815=CARTESIAN_POINT('Ctrl Pts',(-3.51243888042392,5.78702520443108,
84.9764651172035));
#204816=CARTESIAN_POINT('Ctrl Pts',(-3.67024081223678,5.68825280605791,
84.9852146174524));
#204817=CARTESIAN_POINT('Ctrl Pts',(-3.82370687544385,5.58314917682516,
84.9939641177014));
#204818=CARTESIAN_POINT('Ctrl Pts',(-3.97717043817796,5.47804726008035,
85.0027134753918));
#204819=CARTESIAN_POINT('Ctrl Pts',(-4.12629803722439,5.36661448084252,
85.0114628330823));
#204820=CARTESIAN_POINT('Ctrl Pts',(-4.27058317206883,5.24922931204596,
85.0202121907728));
#204821=CARTESIAN_POINT('Ctrl Pts',(-4.4148661477481,5.13184589986812,85.0289614175328));
#204822=CARTESIAN_POINT('Ctrl Pts',(-4.55430658194388,5.00851045723057,
85.0377106442929));
#204823=CARTESIAN_POINT('Ctrl Pts',(-4.6884308900182,4.87964187103144,85.046459871053));
#204824=CARTESIAN_POINT('Ctrl Pts',(-4.82255336917833,4.75077504207965,
85.0552089785089));
#204825=CARTESIAN_POINT('Ctrl Pts',(-4.95135966065151,4.61637541908077,
85.0639580859649));
#204826=CARTESIAN_POINT('Ctrl Pts',(-5.07441230869279,4.47689945401805,
85.0727071934208));
#204827=CARTESIAN_POINT('Ctrl Pts',(-5.19746344226474,4.33742520555449,
85.0814561931972));
#204828=CARTESIAN_POINT('Ctrl Pts',(-5.31476088454844,4.19287495491241,
85.0902051929736));
#204829=CARTESIAN_POINT('Ctrl Pts',(-5.42590627628947,4.0437396158658,85.0989541927499));
#204830=CARTESIAN_POINT('Ctrl Pts',(-5.53706380672759,3.89458798906604,
85.1077041480446));
#204831=CARTESIAN_POINT('Ctrl Pts',(-5.64206777071953,3.74085050155149,
85.1164541033393));
#204832=CARTESIAN_POINT('Ctrl Pts',(-5.74056148164094,3.58304938223022,
85.125204058634));
#204833=CARTESIAN_POINT('Ctrl Pts',(-5.8390513895197,3.42525435593135,85.1339536760752));
#204834=CARTESIAN_POINT('Ctrl Pts',(-5.93103139557738,3.26339625497028,
85.1427032935163));
#204835=CARTESIAN_POINT('Ctrl Pts',(-6.0161890782093,3.09802485064841,85.1514529109574));
#204836=CARTESIAN_POINT('Ctrl Pts',(-6.10134392545072,2.93265895249457,
85.1602022370733));
#204837=CARTESIAN_POINT('Ctrl Pts',(-6.17967677261924,2.76378023985831,
85.1689515631891));
#204838=CARTESIAN_POINT('Ctrl Pts',(-6.25092157009318,2.59196229226891,
85.177700889305));
#204839=CARTESIAN_POINT('Ctrl Pts',(-6.32216437407842,2.42014915228859,
85.1864499706075));
#204840=CARTESIAN_POINT('Ctrl Pts',(-6.38631941549005,2.24539720662612,
85.1951990519099));
#204841=CARTESIAN_POINT('Ctrl Pts',(-6.44316881037616,2.0682999494744,85.2039481332124));
#204842=CARTESIAN_POINT('Ctrl Pts',(-6.50002334524642,1.89118668024207,
85.2126980055547));
#204843=CARTESIAN_POINT('Ctrl Pts',(-6.54957082411158,1.71172794807464,
85.2214478778971));
#204844=CARTESIAN_POINT('Ctrl Pts',(-6.59164294296138,1.53053334250105,
85.2301977502394));
#204845=CARTESIAN_POINT('Ctrl Pts',(-6.63371214082185,1.3493513169335,85.2389470150943));
#204846=CARTESIAN_POINT('Ctrl Pts',(-6.66830695239737,1.16643393829499,
85.2476962799492));
#204847=CARTESIAN_POINT('Ctrl Pts',(-6.69530988154029,0.982402458338193,
85.2564455448041));
#204848=CARTESIAN_POINT('Ctrl Pts',(-6.72231419690515,0.798361530944327,
85.2651952588112));
#204849=CARTESIAN_POINT('Ctrl Pts',(-6.74172580829302,0.613206671359816,
85.2739449728182));
#204850=CARTESIAN_POINT('Ctrl Pts',(-6.75347878028196,0.427566795110811,
85.2826946868252));
#204851=CARTESIAN_POINT('Ctrl Pts',(-6.76248992368217,0.285234494204192,
85.2894031966134));
#204852=CARTESIAN_POINT('Ctrl Pts',(-6.76699999999993,0.142617266092563,
85.2961117064016));
#204853=CARTESIAN_POINT('Ctrl Pts',(-6.767,3.38585956577759E-12,85.3028202161898));
#204854=CARTESIAN_POINT('Ctrl Pts',(-6.76699999999426,8.81760040218907E-6,
85.3030125520247));
#204855=CARTESIAN_POINT('Ctrl Pts',(-6.76700021690518,-0.166457813100077,
85.310839071891));
#204856=CARTESIAN_POINT('Ctrl Pts',(-6.76085354170972,-0.333110924625458,
85.3186655917572));
#204857=CARTESIAN_POINT('Ctrl Pts',(-6.74854471695431,-0.49943288164484,
85.3264921116235));
#204858=CARTESIAN_POINT('Ctrl Pts',(-6.73624143578192,-0.665679931466091,
85.3343151066234));
#204859=CARTESIAN_POINT('Ctrl Pts',(-6.71778154932752,-0.831595732536135,
85.3421381016233));
#204860=CARTESIAN_POINT('Ctrl Pts',(-6.69320189408862,-0.996663135150782,
85.3499610966232));
#204861=CARTESIAN_POINT('Ctrl Pts',(-6.66862904033346,-1.16168486164644,
85.3577819269071));
#204862=CARTESIAN_POINT('Ctrl Pts',(-6.63793984559386,-1.3258582686396,
85.365602757191));
#204863=CARTESIAN_POINT('Ctrl Pts',(-6.60122290099131,-1.48867229819993,
85.3734235874748));
#204864=CARTESIAN_POINT('Ctrl Pts',(-6.56450073493061,-1.65150948128383,
85.3812455299465));
#204865=CARTESIAN_POINT('Ctrl Pts',(-6.52174918981563,-1.81298651663494,
85.3890674724182));
#204866=CARTESIAN_POINT('Ctrl Pts',(-6.47310775543939,-1.9726036060168,
85.3968894148899));
#204867=CARTESIAN_POINT('Ctrl Pts',(-6.44432244876842,-2.06706272151583,
85.4015183288127));
#204868=CARTESIAN_POINT('Ctrl Pts',(-6.41347540245782,-2.16087071110073,
85.4061472427355));
#204869=CARTESIAN_POINT('Ctrl Pts',(-6.38060368627069,-2.25392670660535,
85.4107761566583));
#204870=CARTESIAN_POINT('Ctrl Pts',(-6.31680169767356,-2.43454269666451,
85.4197605951841));
#204871=CARTESIAN_POINT('Ctrl Pts',(-6.24538097869586,-2.61229424427641,
85.4287450337099));
#204872=CARTESIAN_POINT('Ctrl Pts',(-6.16662721156435,-2.78657456989654,
85.4377294722357));
#204873=CARTESIAN_POINT('Ctrl Pts',(-6.08773752013061,-2.96115569295806,
85.4467294173662));
#204874=CARTESIAN_POINT('Ctrl Pts',(-6.00148958222123,-3.13225340160032,
85.4557293624967));
#204875=CARTESIAN_POINT('Ctrl Pts',(-5.90821535324118,-3.29928482246155,
85.4647293076272));
#204876=CARTESIAN_POINT('Ctrl Pts',(-5.81472132114677,-3.46670985715271,
85.4737504613594));
#204877=CARTESIAN_POINT('Ctrl Pts',(-5.71416798582239,-3.63004922193328,
85.4827716150916));
#204878=CARTESIAN_POINT('Ctrl Pts',(-5.60693253178595,-3.78874604374592,
85.4917927688238));
#204879=CARTESIAN_POINT('Ctrl Pts',(-5.49958796482978,-3.94760434082565,
85.500823101651));
#204880=CARTESIAN_POINT('Ctrl Pts',(-5.38554783485579,-4.10181046343896,
85.5098534344783));
#204881=CARTESIAN_POINT('Ctrl Pts',(-5.26523110145149,-4.25083879349804,
85.5188837673055));
#204882=CARTESIAN_POINT('Ctrl Pts',(-5.14474379684518,-4.40007839875279,
85.5279269022981));
#204883=CARTESIAN_POINT('Ctrl Pts',(-5.01796224673951,-4.54412534796465,
85.5369700372908));
#204884=CARTESIAN_POINT('Ctrl Pts',(-4.88534545312323,-4.68248745899529,
85.5460131722834));
#204885=CARTESIAN_POINT('Ctrl Pts',(-4.76940782238251,-4.80344782079978,
85.5539189556833));
#204886=CARTESIAN_POINT('Ctrl Pts',(-4.64901108990684,-4.92006385517504,
85.5618247390832));
#204887=CARTESIAN_POINT('Ctrl Pts',(-4.52448428868203,-5.03203049687395,
85.569730522483));
#204888=CARTESIAN_POINT('Ctrl Pts',(-4.38818169837358,-5.1545851850342,
85.5783839107113));
#204889=CARTESIAN_POINT('Ctrl Pts',(-4.2468097099974,-5.27167687447455,
85.5870372989395));
#204890=CARTESIAN_POINT('Ctrl Pts',(-4.10082390915043,-5.38289255569347,
85.5956906871678));
#204891=CARTESIAN_POINT('Ctrl Pts',(-3.95497293654614,-5.49400552134164,
85.6043360833782));
#204892=CARTESIAN_POINT('Ctrl Pts',(-3.80451689149178,-5.59925311926044,
85.6129814795886));
#204893=CARTESIAN_POINT('Ctrl Pts',(-3.64994492812084,-5.69826210538661,
85.621626875799));
#204894=CARTESIAN_POINT('Ctrl Pts',(-3.49043645693213,-5.8004331050072,
85.6305483768414));
#204895=CARTESIAN_POINT('Ctrl Pts',(-3.32654505478421,-5.89596019245491,
85.6394698778838));
#204896=CARTESIAN_POINT('Ctrl Pts',(-3.15884329998869,-5.98447976069069,
85.6483913789262));
#204897=CARTESIAN_POINT('Ctrl Pts',(-2.99664113765321,-6.07009642817492,
85.6570203092681));
#204898=CARTESIAN_POINT('Ctrl Pts',(-2.83087485950027,-6.14915772209436,
85.6656492396101));
#204899=CARTESIAN_POINT('Ctrl Pts',(-2.66209046795408,-6.22137953676096,
85.6742781699521));
#204900=CARTESIAN_POINT('Ctrl Pts',(-2.48472192419546,-6.29727445795405,
85.6833459563447));
#204901=CARTESIAN_POINT('Ctrl Pts',(-2.30402055860341,-6.36561589289683,
85.6924137427373));
#204902=CARTESIAN_POINT('Ctrl Pts',(-2.12064792181933,-6.42612958099067,
85.7014815291299));
#204903=CARTESIAN_POINT('Ctrl Pts',(-1.93727528503519,-6.48664326908454,
85.7105493155225));
#204904=CARTESIAN_POINT('Ctrl Pts',(-1.75123173686825,-6.53932905451853,
85.7196171019152));
#204905=CARTESIAN_POINT('Ctrl Pts',(-1.56320225990795,-6.58397203021236,
85.7286848883078));
#204906=CARTESIAN_POINT('Ctrl Pts',(-1.3885025011636,-6.62545019209115,
85.737109844441));
#204907=CARTESIAN_POINT('Ctrl Pts',(-1.21216511647651,-6.65996749395453,
85.7455348005742));
#204908=CARTESIAN_POINT('Ctrl Pts',(-1.03477051646232,-6.6874164651426,
85.7539597567074));
#204909=CARTESIAN_POINT('Ctrl Pts',(-0.857334741458616,-6.71487180750037,
85.7623866683537));
#204910=CARTESIAN_POINT('Ctrl Pts',(-0.678841589563437,-6.7352554973071,
85.7708135800001));
#204911=CARTESIAN_POINT('Ctrl Pts',(-0.499878492326469,-6.74851172429221,
85.7792404916465));
#204912=CARTESIAN_POINT('Ctrl Pts',(-0.320849583386895,-6.7617728261084,
85.7876705021966));
#204913=CARTESIAN_POINT('Ctrl Pts',(-0.141350715065076,-6.76790121450158,
85.7961005127466));
#204914=CARTESIAN_POINT('Ctrl Pts',(0.03802837429104,-6.76689314550989,
85.8045305232967));
#204915=CARTESIAN_POINT('Ctrl Pts',(0.217572703912353,-6.76588414790614,
85.8129682993962));
#204916=CARTESIAN_POINT('Ctrl Pts',(0.396996702288371,-6.75772556060025,
85.8214060754956));
#204917=CARTESIAN_POINT('Ctrl Pts',(0.575712320100965,-6.74246574514724,
85.8298438515951));
#204918=CARTESIAN_POINT('Ctrl Pts',(0.754521750438224,-6.72719791941606,
85.838286056905));
#204919=CARTESIAN_POINT('Ctrl Pts',(0.932621729260149,-6.70482146719918,
85.8467282622149));
#204920=CARTESIAN_POINT('Ctrl Pts',(1.10943154956437,-6.6754363630276,85.8551704675248));
#204921=CARTESIAN_POINT('Ctrl Pts',(1.28642789450093,-6.6460202591879,85.8636215788968));
#204922=CARTESIAN_POINT('Ctrl Pts',(1.46213103664878,-6.60958079575246,
85.8720726902688));
#204923=CARTESIAN_POINT('Ctrl Pts',(1.63597158178026,-6.56626880226567,
85.8805238016408));
#204924=CARTESIAN_POINT('Ctrl Pts',(1.68476020004871,-6.55411322420374,
85.8828956191381));
#204925=CARTESIAN_POINT('Ctrl Pts',(1.73340220587232,-6.54141662990167,
85.8852674366353));
#204926=CARTESIAN_POINT('Ctrl Pts',(1.78188525111196,-6.52818305134512,
85.8876392541326));
#204927=CARTESIAN_POINT('Ctrl Pts',(1.95188071309984,-6.48178232941534,
85.8959555265367));
#204928=CARTESIAN_POINT('Ctrl Pts',(2.12022741980042,-6.42869236466029,
85.9042717989408));
#204929=CARTESIAN_POINT('Ctrl Pts',(2.28637078269115,-6.36904997971097,
85.9125880713449));
#204930=CARTESIAN_POINT('Ctrl Pts',(2.45237367117229,-6.30945802246857,
85.9208973123309));
#204931=CARTESIAN_POINT('Ctrl Pts',(2.61617660165709,-6.24332479987565,
85.9292065533169));
#204932=CARTESIAN_POINT('Ctrl Pts',(2.77723907424595,-6.17083723043166,
85.9375157943029));
#204933=CARTESIAN_POINT('Ctrl Pts',(2.93819489855025,-6.09839765897758,
85.9458195332853));
#204934=CARTESIAN_POINT('Ctrl Pts',(3.09641356454046,-6.01961226702696,
85.9541232722678));
#204935=CARTESIAN_POINT('Ctrl Pts',(3.25137331876829,-5.93471655110854,
85.9624270112502));
#204936=CARTESIAN_POINT('Ctrl Pts',(3.40625886433244,-5.84986149089239,
85.9707267736558));
#204937=CARTESIAN_POINT('Ctrl Pts',(3.55788830384298,-5.75890210508579,
85.9790265360614));
#204938=CARTESIAN_POINT('Ctrl Pts',(3.70576312159477,-5.66212051148933,
85.9873262984669));
#204939=CARTESIAN_POINT('Ctrl Pts',(3.85359421470125,-5.56536753494151,
85.9956236067416));
#204940=CARTESIAN_POINT('Ctrl Pts',(3.99767260818949,-5.46279597245703,
86.0039209150161));
#204941=CARTESIAN_POINT('Ctrl Pts',(4.13752730753579,-5.35473218559021,
86.0122182232907));
#204942=CARTESIAN_POINT('Ctrl Pts',(4.27739613717027,-5.24665748044564,
86.020516369888));
#204943=CARTESIAN_POINT('Ctrl Pts',(4.41304014003943,-5.13308964888474,
86.0288145164852));
#204944=CARTESIAN_POINT('Ctrl Pts',(4.54401960099712,-5.01439675990582,
86.0371126630825));
#204945=CARTESIAN_POINT('Ctrl Pts',(4.67501223276379,-4.89569193561004,
86.0454116441105));
#204946=CARTESIAN_POINT('Ctrl Pts',(4.80133912936477,-4.77186126004794,
86.0537106251386));
#204947=CARTESIAN_POINT('Ctrl Pts',(4.92259588018237,-4.64331118927125,
86.0620096061667));
#204948=CARTESIAN_POINT('Ctrl Pts',(5.0438849756283,-4.51472682840981,86.0703108009062));
#204949=CARTESIAN_POINT('Ctrl Pts',(5.16010099092831,-4.38142081646386,
86.0786119956458));
#204950=CARTESIAN_POINT('Ctrl Pts',(5.27087828325675,-4.24383448347039,
86.0869131903853));
#204951=CARTESIAN_POINT('Ctrl Pts',(5.38170353696998,-4.10618858203179,
86.0952179791538));
#204952=CARTESIAN_POINT('Ctrl Pts',(5.48708515662819,-3.96425893704951,
86.1035227679222));
#204953=CARTESIAN_POINT('Ctrl Pts',(5.58669937349187,-3.81851792063696,
86.1118275566907));
#204954=CARTESIAN_POINT('Ctrl Pts',(5.68643168211522,-3.67260412955802,
86.1201421907117));
#204955=CARTESIAN_POINT('Ctrl Pts',(5.78038273072586,-3.52287022708953,
86.1284568247327));
#204956=CARTESIAN_POINT('Ctrl Pts',(5.86827286704844,-3.36981639824236,
86.1367714587537));
#204957=CARTESIAN_POINT('Ctrl Pts',(5.95621857708335,-3.2166657921024,86.1450913501915));
#204958=CARTESIAN_POINT('Ctrl Pts',(6.03809557102104,-3.06019138113712,
86.1534112416293));
#204959=CARTESIAN_POINT('Ctrl Pts',(6.11367129886114,-2.90091576049384,
86.1617311330671));
#204960=CARTESIAN_POINT('Ctrl Pts',(6.18936003691977,-2.7414019711526,86.1700634654403));
#204961=CARTESIAN_POINT('Ctrl Pts',(6.25872854155942,-2.57907892088648,
86.1783957978135));
#204962=CARTESIAN_POINT('Ctrl Pts',(6.32159283092554,-2.41448816107904,
86.1867281301867));
#204963=CARTESIAN_POINT('Ctrl Pts',(6.36892238984446,-2.29057030338326,
86.1930014153852));
#204964=CARTESIAN_POINT('Ctrl Pts',(6.41256614476117,-2.16536740233288,
86.1992747005836));
#204965=CARTESIAN_POINT('Ctrl Pts',(6.45246456311795,-2.03911501924414,
86.205547985782));
#204966=CARTESIAN_POINT('Ctrl Pts',(6.50378920111996,-1.87670612872185,
86.2136178317848));
#204967=CARTESIAN_POINT('Ctrl Pts',(6.54907277841643,-1.71205827198792,
86.2216876777875));
#204968=CARTESIAN_POINT('Ctrl Pts',(6.58810987231774,-1.54567050507847,
86.2297575237903));
#204969=CARTESIAN_POINT('Ctrl Pts',(6.62709785258962,-1.37949207514341,
86.2378172169003));
#204970=CARTESIAN_POINT('Ctrl Pts',(6.65985490231959,-1.21157844919782,
86.2458769100104));
#204971=CARTESIAN_POINT('Ctrl Pts',(6.68622408375805,-1.04244736163216,
86.2539366031204));
#204972=CARTESIAN_POINT('Ctrl Pts',(6.71256587661338,-0.873491943563923,
86.2619879249591));
#204973=CARTESIAN_POINT('Ctrl Pts',(6.73253294754114,-0.703321945801222,
86.2700392467977));
#204974=CARTESIAN_POINT('Ctrl Pts',(6.74601852567449,-0.532468826558542,
86.2780905686363));
#204975=CARTESIAN_POINT('Ctrl Pts',(6.75949305204262,-0.361755725677831,
86.2861352922173));
#204976=CARTESIAN_POINT('Ctrl Pts',(6.76649662848728,-0.190360987609441,
86.2941800157983));
#204977=CARTESIAN_POINT('Ctrl Pts',(6.76697381633973,-0.0188246905025418,
86.3022247393793));
#204978=CARTESIAN_POINT('Ctrl Pts',(6.76745071758155,0.152608577733117,
86.3102646311037));
#204979=CARTESIAN_POINT('Ctrl Pts',(6.76140903252064,0.324182863595643,
86.3183045228282));
#204980=CARTESIAN_POINT('Ctrl Pts',(6.74884529036586,0.495354667593435,
86.3263444145526));
#204981=CARTESIAN_POINT('Ctrl Pts',(6.73601101642186,0.670212269487086,
86.3345574271725));
#204982=CARTESIAN_POINT('Ctrl Pts',(6.71637059217592,0.844649462487381,
86.3427704397925));
#204983=CARTESIAN_POINT('Ctrl Pts',(6.68997648786138,1.01808820436242,86.3509834524125));
#204984=CARTESIAN_POINT('Ctrl Pts',(6.66414775601771,1.18781181770462,86.359020538955));
#204985=CARTESIAN_POINT('Ctrl Pts',(6.63185181772796,1.35657893875707,86.3670576254976));
#204986=CARTESIAN_POINT('Ctrl Pts',(6.59319008474597,1.52385481802155,86.3750947120402));
#204987=CARTESIAN_POINT('Ctrl Pts',(6.55452465165618,1.69114670636625,86.3831325677693));
#204988=CARTESIAN_POINT('Ctrl Pts',(6.50949229479818,1.85694670467716,86.3911704234985));
#204989=CARTESIAN_POINT('Ctrl Pts',(6.4582451107684,2.02073231508681,86.3992082792277));
#204990=CARTESIAN_POINT('Ctrl Pts',(6.40698286836635,2.18456605193971,86.4072484967846));
#204991=CARTESIAN_POINT('Ctrl Pts',(6.34950227540817,2.34638386635018,86.4152887143416));
#204992=CARTESIAN_POINT('Ctrl Pts',(6.28600460439041,2.50568056894382,86.4233289318985));
#204993=CARTESIAN_POINT('Ctrl Pts',(6.22010795067768,2.67099560302524,86.4316729140263));
#204994=CARTESIAN_POINT('Ctrl Pts',(6.14773084491761,2.83359489251654,86.440016896154));
#204995=CARTESIAN_POINT('Ctrl Pts',(6.06915147397983,2.9929399235348,86.4483608782818));
#204996=CARTESIAN_POINT('Ctrl Pts',(5.99330098371672,3.1467512684143,86.4564150931168));
#204997=CARTESIAN_POINT('Ctrl Pts',(5.91167202087316,3.29753029957398,86.4644693079519));
#204998=CARTESIAN_POINT('Ctrl Pts',(5.82455972292786,3.44482119043159,86.4725235227869));
#204999=CARTESIAN_POINT('Ctrl Pts',(5.73738223583291,3.5922223041642,86.4805837648699));
#205000=CARTESIAN_POINT('Ctrl Pts',(5.64471344418015,3.73612976820829,86.4886440069529));
#205001=CARTESIAN_POINT('Ctrl Pts',(5.54688994195431,3.87611931857704,86.4967042490358));
#205002=CARTESIAN_POINT('Ctrl Pts',(5.44892967576163,4.01630458394055,86.5047757598902));
#205003=CARTESIAN_POINT('Ctrl Pts',(5.34580054384363,4.15256071197133,86.5128472707445));
#205004=CARTESIAN_POINT('Ctrl Pts',(5.23787762964169,4.28449844636443,86.5209187815989));
#205005=CARTESIAN_POINT('Ctrl Pts',(5.22656618142751,4.29832689846952,86.5217647602097));
#205006=CARTESIAN_POINT('Ctrl Pts',(5.21520210372238,4.31210794734796,86.5226107388206));
#205007=CARTESIAN_POINT('Ctrl Pts',(5.20378584998983,4.32584116992818,86.5234567174315));
#205008=CARTESIAN_POINT('Ctrl Pts',(5.09271791362746,4.4594507346177,86.5316871843359));
#205009=CARTESIAN_POINT('Ctrl Pts',(4.97633771015214,4.58897633015651,86.5399176512402));
#205010=CARTESIAN_POINT('Ctrl Pts',(4.85497578109233,4.71396851548745,86.5481481181446));
#205011=CARTESIAN_POINT('Ctrl Pts',(4.72803515647347,4.84470626991591,86.5567569184318));
#205012=CARTESIAN_POINT('Ctrl Pts',(4.59564415093411,4.97048364059416,86.565365718719));
#205013=CARTESIAN_POINT('Ctrl Pts',(4.45823065755993,5.09082197724422,86.5739745190062));
#205014=CARTESIAN_POINT('Ctrl Pts',(4.32717392744067,5.20559344925974,86.5821850752491));
#205015=CARTESIAN_POINT('Ctrl Pts',(4.19154920801982,5.31541745721965,86.5903956314921));
#205016=CARTESIAN_POINT('Ctrl Pts',(4.0517674352365,5.41991417374454,86.598606187735));
#205017=CARTESIAN_POINT('Ctrl Pts',(3.91208318633185,5.52433798430395,86.6068110155824));
#205018=CARTESIAN_POINT('Ctrl Pts',(3.76824794408863,5.62344168917379,86.6150158434298));
#205019=CARTESIAN_POINT('Ctrl Pts',(3.62070678920349,5.71688475890635,86.6232206712771));
#205020=CARTESIAN_POINT('Ctrl Pts',(3.47325584970364,5.81027069202138,86.6314204822076));
#205021=CARTESIAN_POINT('Ctrl Pts',(3.32210381493285,5.89800269529541,86.6396202931382));
#205022=CARTESIAN_POINT('Ctrl Pts',(3.16772581273165,5.97978278663645,86.6478201040687));
#205023=CARTESIAN_POINT('Ctrl Pts',(3.14492241646647,5.99186264129749,86.6490313099094));
#205024=CARTESIAN_POINT('Ctrl Pts',(3.1220486842215,6.00381271105085,86.6502425157501));
#205025=CARTESIAN_POINT('Ctrl Pts',(3.09910619832139,6.01563211736938,86.6514537215909));
#205026=CARTESIAN_POINT('Origin',(0.,0.,4.30282021618968));
#205027=CARTESIAN_POINT('',(3.09910619832144,6.01563211736935,89.0458803684832));
#205028=CARTESIAN_POINT('',(3.09910619832125,6.01563211736945,88.6513956954041));
#205029=CARTESIAN_POINT('',(3.09910619832133,6.0156321173694,4.30282021618968));
#205030=CARTESIAN_POINT('',(-6.76699899245737,-0.00240081800135623,87.6971797838099));
#205031=CARTESIAN_POINT('Ctrl Pts',(-6.76699761639396,-0.00567976394980745,
87.6971797838099));
#205032=CARTESIAN_POINT('Ctrl Pts',(-6.76677386767964,-0.272258979179347,
87.7097537505765));
#205033=CARTESIAN_POINT('Ctrl Pts',(-6.75079460165027,-0.538161101664258,
87.7223277173431));
#205034=CARTESIAN_POINT('Ctrl Pts',(-6.71931721421665,-0.801913445910326,
87.7349016841098));
#205035=CARTESIAN_POINT('Ctrl Pts',(-6.68967829484414,-1.05026107266005,
87.7467412558651));
#205036=CARTESIAN_POINT('Ctrl Pts',(-6.64629915915566,-1.29670433671583,
87.7585808276203));
#205037=CARTESIAN_POINT('Ctrl Pts',(-6.58942873953572,-1.54003827438822,
87.7704203993756));
#205038=CARTESIAN_POINT('Ctrl Pts',(-6.55066589085075,-1.70589456081885,
87.7784902453784));
#205039=CARTESIAN_POINT('Ctrl Pts',(-6.50556537859396,-1.87059265702531,
87.7865600913812));
#205040=CARTESIAN_POINT('Ctrl Pts',(-6.45420528747431,-2.03359856096002,
87.7946299373839));
#205041=CARTESIAN_POINT('Ctrl Pts',(-6.40290981388201,-2.19639938273411,
87.802689630494));
#205042=CARTESIAN_POINT('Ctrl Pts',(-6.345370541888,-2.35751189703273,87.810749323604));
#205043=CARTESIAN_POINT('Ctrl Pts',(-6.28171678335449,-2.51641078795225,
87.8188090167141));
#205044=CARTESIAN_POINT('Ctrl Pts',(-6.2181291393595,-2.67514463713527,
87.8268603385527));
#205045=CARTESIAN_POINT('Ctrl Pts',(-6.1484397846706,-2.83166909497776,
87.8349116603913));
#205046=CARTESIAN_POINT('Ctrl Pts',(-6.07282817571208,-2.98547265073346,
87.8429629822299));
#205047=CARTESIAN_POINT('Ctrl Pts',(-5.9972785323391,-3.13915016066734,
87.8510077058109));
#205048=CARTESIAN_POINT('Ctrl Pts',(-5.91581645835378,-3.29011087351234,
87.859052429392));
#205049=CARTESIAN_POINT('Ctrl Pts',(-5.82866995165558,-3.43786206742903,
87.867097152973));
#205050=CARTESIAN_POINT('Ctrl Pts',(-5.74157578726874,-3.58552451838527,
87.8751370446974));
#205051=CARTESIAN_POINT('Ctrl Pts',(-5.64880417587126,-3.72998096734556,
87.8831769364218));
#205052=CARTESIAN_POINT('Ctrl Pts',(-5.55062954996713,-3.87076227622309,
87.8912168281462));
#205053=CARTESIAN_POINT('Ctrl Pts',(-5.45034095540003,-4.01457499237677,
87.8994298407661));
#205054=CARTESIAN_POINT('Ctrl Pts',(-5.34441419912616,-4.15455214362565,
87.9076428533861));
#205055=CARTESIAN_POINT('Ctrl Pts',(-5.23318945006422,-4.29022344170284,
87.9158558660061));
#205056=CARTESIAN_POINT('Ctrl Pts',(-5.1243471804551,-4.42298860528448,
87.9238929525486));
#205057=CARTESIAN_POINT('Ctrl Pts',(-5.01043184572974,-4.55163022099534,
87.9319300390912));
#205058=CARTESIAN_POINT('Ctrl Pts',(-4.89180360283301,-4.67574020998921,
87.9399671256338));
#205059=CARTESIAN_POINT('Ctrl Pts',(-4.77316400666122,-4.79986207688677,
87.9480049813629));
#205060=CARTESIAN_POINT('Ctrl Pts',(-4.6498108622847,-4.91945118331582,
87.9560428370921));
#205061=CARTESIAN_POINT('Ctrl Pts',(-4.52214165802727,-5.03413585680148,
87.9640806928213));
#205062=CARTESIAN_POINT('Ctrl Pts',(-4.3944349397009,-5.14885422900698,
87.9721209103782));
#205063=CARTESIAN_POINT('Ctrl Pts',(-4.26240991493434,-5.25866505025289,
87.9801611279351));
#205064=CARTESIAN_POINT('Ctrl Pts',(-4.12649752469757,-5.36323663273073,
87.9882013454921));
#205065=CARTESIAN_POINT('Ctrl Pts',(-3.98545027727593,-5.47175899659563,
87.9965453276199));
#205066=CARTESIAN_POINT('Ctrl Pts',(-3.84021654539729,-5.57463823408338,
88.0048893097476));
#205067=CARTESIAN_POINT('Ctrl Pts',(-3.69131042004525,-5.67155326016298,
88.0132332918754));
#205068=CARTESIAN_POINT('Ctrl Pts',(-3.54757546166741,-5.7651026504705,
88.0212875067105));
#205069=CARTESIAN_POINT('Ctrl Pts',(-3.4004192511565,-5.85309499968583,
88.0293417215455));
#205070=CARTESIAN_POINT('Ctrl Pts',(-3.25032824980126,-5.93528897936267,
88.0373959363806));
#205071=CARTESIAN_POINT('Ctrl Pts',(-3.10012493015034,-6.01754446764181,
88.0454561784636));
#205072=CARTESIAN_POINT('Ctrl Pts',(-2.94698277869687,-6.09399278091668,
88.0535164205466));
#205073=CARTESIAN_POINT('Ctrl Pts',(-2.79140779562201,-6.16444089261473,
88.0615766626296));
#205074=CARTESIAN_POINT('Ctrl Pts',(-2.63561530804912,-6.23498749560533,
88.069648173484));
#205075=CARTESIAN_POINT('Ctrl Pts',(-2.47738354540936,-6.29951702038352,
88.0777196843383));
#205076=CARTESIAN_POINT('Ctrl Pts',(-2.31723373688198,-6.35788619028809,
88.0857911951927));
#205077=CARTESIAN_POINT('Ctrl Pts',(-2.30044836484954,-6.36400388871734,
88.0866371738036));
#205078=CARTESIAN_POINT('Ctrl Pts',(-2.28364193153735,-6.3700539605859,
88.0874831524145));
#205079=CARTESIAN_POINT('Ctrl Pts',(-2.2668150428355,-6.37603627354603,
88.0883291310254));
#205080=CARTESIAN_POINT('Ctrl Pts',(-2.10313162623069,-6.43422917193996,
88.0965583807613));
#205081=CARTESIAN_POINT('Ctrl Pts',(-1.93696538622776,-6.48620049473463,
88.1047876304973));
#205082=CARTESIAN_POINT('Ctrl Pts',(-1.76882973990278,-6.53173256886988,
88.1130168802333));
#205083=CARTESIAN_POINT('Ctrl Pts',(-1.600894202349,-6.57721045242981,88.1212363358233));
#205084=CARTESIAN_POINT('Ctrl Pts',(-1.43099426845363,-6.61626425463261,
88.1294557914134));
#205085=CARTESIAN_POINT('Ctrl Pts',(-1.25966241056945,-6.64872466051937,
88.1376752470035));
#205086=CARTESIAN_POINT('Ctrl Pts',(-1.08850005781628,-6.68115295209054,
88.1458865707731));
#205087=CARTESIAN_POINT('Ctrl Pts',(-0.915908952253664,-6.70700077162168,
88.1540978945428));
#205088=CARTESIAN_POINT('Ctrl Pts',(-0.742435866460153,-6.72614882263198,
88.1623092183124));
#205089=CARTESIAN_POINT('Ctrl Pts',(-0.569099579126017,-6.74528177375594,
88.1705140667465));
#205090=CARTESIAN_POINT('Ctrl Pts',(-0.394883051739474,-6.75772544035168,
88.1787189151806));
#205091=CARTESIAN_POINT('Ctrl Pts',(-0.220342460866645,-6.76341172781454,
88.1869237636147));
#205092=CARTESIAN_POINT('Ctrl Pts',(-0.0459044799351441,-6.76909467238954,
88.1951237885347));
#205093=CARTESIAN_POINT('Ctrl Pts',(0.128856827466691,-6.76802813993521,
88.2033238134546));
#205094=CARTESIAN_POINT('Ctrl Pts',(0.303380870132504,-6.76019593263669,
88.2115238383745));
#205095=CARTESIAN_POINT('Ctrl Pts',(0.477854401586501,-6.75236599215641,
88.2197214900214));
#205096=CARTESIAN_POINT('Ctrl Pts',(0.652090447071619,-6.73777428929547,
88.2279191416683));
#205097=CARTESIAN_POINT('Ctrl Pts',(0.825528870059933,-6.71645673586137,
88.2361167933152));
#205098=CARTESIAN_POINT('Ctrl Pts',(0.998944068579247,-6.69514203697848,
88.2443133472463));
#205099=CARTESIAN_POINT('Ctrl Pts',(1.17156150126438,-6.66710332416293,
88.2525099011774));
#205100=CARTESIAN_POINT('Ctrl Pts',(1.34282659419896,-6.63242834397116,
88.2607064551085));
#205101=CARTESIAN_POINT('Ctrl Pts',(1.51409989413084,-6.5977517021596,88.2689034018172));
#205102=CARTESIAN_POINT('Ctrl Pts',(1.6840203735552,-6.5564382305585,88.2771003485259));
#205103=CARTESIAN_POINT('Ctrl Pts',(1.85204403267246,-6.50862672927572,
88.2852972952346));
#205104=CARTESIAN_POINT('Ctrl Pts',(2.02010629445776,-6.46080424351895,
88.2934961251543));
#205105=CARTESIAN_POINT('Ctrl Pts',(2.18627052300146,-6.40648085285346,
88.3016949550741));
#205106=CARTESIAN_POINT('Ctrl Pts',(2.35000820109461,-6.34584513321812,
88.3098937849938));
#205107=CARTESIAN_POINT('Ctrl Pts',(2.513900959701,-6.28515198380467,88.3181003802536));
#205108=CARTESIAN_POINT('Ctrl Pts',(2.67536223929557,-6.21813468550847,
88.3263069755135));
#205109=CARTESIAN_POINT('Ctrl Pts',(2.83388295057802,-6.145030221441,88.3345135707733));
#205110=CARTESIAN_POINT('Ctrl Pts',(2.99248038679347,-6.07189037439384,
88.3427241380723));
#205111=CARTESIAN_POINT('Ctrl Pts',(3.14813409755171,-5.99265765015605,
88.3509347053712));
#205112=CARTESIAN_POINT('Ctrl Pts',(3.30035999983158,-5.90761482084874,
88.3591452726702));
#205113=CARTESIAN_POINT('Ctrl Pts',(3.45279584342336,-5.82245470530509,
88.3673671635169));
#205114=CARTESIAN_POINT('Ctrl Pts',(3.60179412446357,-5.73146865773804,
88.3755890543636));
#205115=CARTESIAN_POINT('Ctrl Pts',(3.74689910053372,-5.63498324136103,
88.3838109452103));
#205116=CARTESIAN_POINT('Ctrl Pts',(3.87883376871325,-5.54725522721139,
88.3912865843652));
#205117=CARTESIAN_POINT('Ctrl Pts',(4.00755002574031,-5.45498147662335,
88.39876222352));
#205118=CARTESIAN_POINT('Ctrl Pts',(4.13272995211434,-5.35843560592987,
88.4062378626748));
#205119=CARTESIAN_POINT('Ctrl Pts',(4.28236274204428,-5.24303029769447,
88.4151738061255));
#205120=CARTESIAN_POINT('Ctrl Pts',(4.42725421261317,-5.12128037415425,
88.4241097495762));
#205121=CARTESIAN_POINT('Ctrl Pts',(4.56688427115261,-4.99358158578579,
88.433045693027));
#205122=CARTESIAN_POINT('Ctrl Pts',(4.7063044286795,-4.86607476256624,88.4419682033846));
#205123=CARTESIAN_POINT('Ctrl Pts',(4.84047876584189,-4.73263709217481,
88.4508907137422));
#205124=CARTESIAN_POINT('Ctrl Pts',(4.96892031122625,-4.59370438107234,
88.4598132240998));
#205125=CARTESIAN_POINT('Ctrl Pts',(5.09704713496527,-4.45511209822695,
88.4687138715382));
#205126=CARTESIAN_POINT('Ctrl Pts',(5.21946902751944,-4.31105183678416,
88.4776145189764));
#205127=CARTESIAN_POINT('Ctrl Pts',(5.33573633219791,-4.161995530183,88.4865151664148));
#205128=CARTESIAN_POINT('Ctrl Pts',(5.45182396010673,-4.01316957170713,
88.495402059001));
#205129=CARTESIAN_POINT('Ctrl Pts',(5.56177581438848,-3.85936317156363,
88.5042889515872));
#205130=CARTESIAN_POINT('Ctrl Pts',(5.6651809466036,-3.70108279321601,88.5131758441734));
#205131=CARTESIAN_POINT('Ctrl Pts',(5.76832028902891,-3.54320925452507,
88.5220398941283));
#205132=CARTESIAN_POINT('Ctrl Pts',(5.86494634674065,-3.38088490018784,
88.5309039440832));
#205133=CARTESIAN_POINT('Ctrl Pts',(5.95469054103665,-3.21464610190433,
88.5397679940381));
#205134=CARTESIAN_POINT('Ctrl Pts',(6.04049321020595,-3.05570843775663,
88.5482427388586));
#205135=CARTESIAN_POINT('Ctrl Pts',(6.12000535808697,-2.89319298766221,
88.5567174836791));
#205136=CARTESIAN_POINT('Ctrl Pts',(6.19294068818319,-2.7275950272438,88.5651922284996));
#205137=CARTESIAN_POINT('Ctrl Pts',(6.26358822935403,-2.56719143805004,
88.5734011429287));
#205138=CARTESIAN_POINT('Ctrl Pts',(6.32799608660961,-2.40404991503855,
88.5816100573578));
#205139=CARTESIAN_POINT('Ctrl Pts',(6.38596282342662,-2.23869779510616,
88.5898189717869));
#205140=CARTESIAN_POINT('Ctrl Pts',(6.44394334154081,-2.07330636354732,
88.5980298378437));
#205141=CARTESIAN_POINT('Ctrl Pts',(6.49547957054619,-1.90570362404628,
88.6062407039005));
#205142=CARTESIAN_POINT('Ctrl Pts',(6.54041966642451,-1.73643300678358,
88.6144515699573));
#205143=CARTESIAN_POINT('Ctrl Pts',(6.58537845734285,-1.56709197309426,
88.6226658517271));
#205144=CARTESIAN_POINT('Ctrl Pts',(6.62373555724049,-1.39608202325226,
88.6308801334969));
#205145=CARTESIAN_POINT('Ctrl Pts',(6.65539001618576,-1.22395781481834,
88.6390944152667));
#205146=CARTESIAN_POINT('Ctrl Pts',(6.68708010472354,-1.05163986699947,
88.6473179428591));
#205147=CARTESIAN_POINT('Ctrl Pts',(6.71205241932193,-0.878205505909337,
88.6555414704515));
#205148=CARTESIAN_POINT('Ctrl Pts',(6.73025765205767,-0.704216541213815,
88.6637649980439));
#205149=CARTESIAN_POINT('Ctrl Pts',(6.74847455363942,-0.530116056360071,
88.6719937965976));
#205150=CARTESIAN_POINT('Ctrl Pts',(6.7599157037378,-0.355460613673461,
88.6802225951513));
#205151=CARTESIAN_POINT('Ctrl Pts',(6.76458392267415,-0.180813033541366,
88.688451393705));
#205152=CARTESIAN_POINT('Ctrl Pts',(6.7692585670403,-0.00592506499107798,
88.6966915185414));
#205153=CARTESIAN_POINT('Ctrl Pts',(6.76714166390616,0.168954664377458,
88.7049316433779));
#205154=CARTESIAN_POINT('Ctrl Pts',(6.75828803461468,0.343266428862604,
88.7131717682143));
#205155=CARTESIAN_POINT('Ctrl Pts',(6.75435738858502,0.420653658713603,
88.7168300435843));
#205156=CARTESIAN_POINT('Ctrl Pts',(6.74909961933731,0.497929046713516,
88.7204883189543));
#205157=CARTESIAN_POINT('Ctrl Pts',(6.74252275698131,0.575044234463026,
88.7241465943243));
#205158=CARTESIAN_POINT('Ctrl Pts',(6.72733486726004,0.753125651402736,
88.7325946170868));
#205159=CARTESIAN_POINT('Ctrl Pts',(6.70507433255718,0.93075961668229,88.7410426398493));
#205160=CARTESIAN_POINT('Ctrl Pts',(6.67578011767778,1.10736119690823,88.7494906626119));
#205161=CARTESIAN_POINT('Ctrl Pts',(6.64651272838582,1.28380105779292,88.7579309492676));
#205162=CARTESIAN_POINT('Ctrl Pts',(6.61022455195311,1.45921009062143,88.7663712359234));
#205163=CARTESIAN_POINT('Ctrl Pts',(6.56700632778351,1.63300853973619,88.7748115225792));
#205164=CARTESIAN_POINT('Ctrl Pts',(6.52382102662986,1.80667459171475,88.7832453795471));
#205165=CARTESIAN_POINT('Ctrl Pts',(6.4737162820617,1.97873218332865,88.791679236515));
#205166=CARTESIAN_POINT('Ctrl Pts',(6.41683395237216,2.14861141849424,88.8001130934829));
#205167=CARTESIAN_POINT('Ctrl Pts',(6.35998621009213,2.31838735826556,88.808541822228));
#205168=CARTESIAN_POINT('Ctrl Pts',(6.29636920474078,2.48598726692218,88.816970550973));
#205169=CARTESIAN_POINT('Ctrl Pts',(6.22617482945705,2.65085570958427,88.825399279718));
#205170=CARTESIAN_POINT('Ctrl Pts',(6.1560123567467,2.81564922134812,88.8338241776983));
#205171=CARTESIAN_POINT('Ctrl Pts',(6.07927860530176,2.97771343617818,88.8422490756786));
#205172=CARTESIAN_POINT('Ctrl Pts',(5.99621400014499,3.13651186263742,88.8506739736589));
#205173=CARTESIAN_POINT('Ctrl Pts',(5.91316778562696,3.29527513086665,88.8590970063531));
#205174=CARTESIAN_POINT('Ctrl Pts',(5.82379366413594,3.45077375588089,88.8675200390473));
#205175=CARTESIAN_POINT('Ctrl Pts',(5.72837875409058,3.60249439273453,88.8759430717414));
#205176=CARTESIAN_POINT('Ctrl Pts',(5.63297464013393,3.7541978625704,88.884365151379));
#205177=CARTESIAN_POINT('Ctrl Pts',(5.53153127772242,3.90212391420367,88.8927872310166));
#205178=CARTESIAN_POINT('Ctrl Pts',(5.42438015879135,4.04578656047384,88.9012093106542));
#205179=CARTESIAN_POINT('Ctrl Pts',(5.31722620639194,4.18945300571098,88.9096316130024));
#205180=CARTESIAN_POINT('Ctrl Pts',(5.20436439622973,4.32885555373081,88.9180539153507));
#205181=CARTESIAN_POINT('Ctrl Pts',(5.08616791855498,4.46353950405528,88.926476217699));
#205182=CARTESIAN_POINT('Ctrl Pts',(4.96795181502739,4.59824581788366,88.9348999185226));
#205183=CARTESIAN_POINT('Ctrl Pts',(4.84439949836761,4.72823172174645,88.9433236193463));
#205184=CARTESIAN_POINT('Ctrl Pts',(4.71592282819866,4.85307746470987,88.9517473201699));
#205185=CARTESIAN_POINT('Ctrl Pts',(4.58735921669263,4.97800769192873,88.9601767213889));
#205186=CARTESIAN_POINT('Ctrl Pts',(4.45386483222662,5.09779057494462,88.9686061226079));
#205187=CARTESIAN_POINT('Ctrl Pts',(4.31588735153932,5.21204426005986,88.9770355238269));
#205188=CARTESIAN_POINT('Ctrl Pts',(4.17786064067857,5.32633871073124,88.9854679326445));
#205189=CARTESIAN_POINT('Ctrl Pts',(4.03534790489707,5.43509982189,88.9939003414622));
#205190=CARTESIAN_POINT('Ctrl Pts',(3.88882839713545,5.53798724245849,89.0023327502798));
#205191=CARTESIAN_POINT('Ctrl Pts',(3.74217332526218,5.64096985746205,89.0107729610074));
#205192=CARTESIAN_POINT('Ctrl Pts',(3.59150435104617,5.73806773708686,89.0192131717351));
#205193=CARTESIAN_POINT('Ctrl Pts',(3.43732901724787,5.82898432209127,89.0276533824627));
#205194=CARTESIAN_POINT('Ctrl Pts',(3.34963671825044,5.88069612422988,89.0324540302998));
#205195=CARTESIAN_POINT('Ctrl Pts',(3.26081053119302,5.93040902174888,89.0372546781368));
#205196=CARTESIAN_POINT('Ctrl Pts',(3.17094717973204,5.97807519050651,89.0420553259739));
#205197=CARTESIAN_POINT('Ctrl Pts',(3.14708018295447,5.99073494865754,89.0433303401437));
#205198=CARTESIAN_POINT('Ctrl Pts',(3.1231325977284,6.0032543053834,89.0446053543134));
#205199=CARTESIAN_POINT('Ctrl Pts',(3.09910619832144,6.01563211736935,89.0458803684832));
#205200=CARTESIAN_POINT('Ctrl Pts',(3.09910619832123,6.01563211736946,87.0457552630241));
#205201=CARTESIAN_POINT('Ctrl Pts',(2.93375330764813,6.1008178731466,87.0545047109265));
#205202=CARTESIAN_POINT('Ctrl Pts',(2.76488627843054,6.17918207037046,87.0632541588287));
#205203=CARTESIAN_POINT('Ctrl Pts',(2.59307866646683,6.25045854554005,87.072003606731));
#205204=CARTESIAN_POINT('Ctrl Pts',(2.42127244185361,6.32173444515043,87.0807529839813));
#205205=CARTESIAN_POINT('Ctrl Pts',(2.24652594672453,6.38592262741842,87.0895023612317));
#205206=CARTESIAN_POINT('Ctrl Pts',(2.06943269687114,6.44280508110564,87.098251738482));
#205207=CARTESIAN_POINT('Ctrl Pts',(1.89234081822068,6.49968709436169,87.1070010479873));
#205208=CARTESIAN_POINT('Ctrl Pts',(1.71290249405577,6.54926340459548,87.1157503574927));
#205209=CARTESIAN_POINT('Ctrl Pts',(1.53172716625045,6.59136563150387,87.124499666998));
#205210=CARTESIAN_POINT('Ctrl Pts',(1.35055318107335,6.63346754640709,87.1332489116653));
#205211=CARTESIAN_POINT('Ctrl Pts',(1.16764249714435,6.66809542395773,87.1419981563325));
#205212=CARTESIAN_POINT('Ctrl Pts',(0.983616340614653,6.69513165624664,
87.1507474009997));
#205213=CARTESIAN_POINT('Ctrl Pts',(0.799591486714114,6.72216769715958,
87.1594965837354));
#205214=CARTESIAN_POINT('Ctrl Pts',(0.614451459526959,6.74161215869369,
87.1682457664711));
#205215=CARTESIAN_POINT('Ctrl Pts',(0.428825047910503,6.75339900185711,
87.1769949492068));
#205216=CARTESIAN_POINT('Ctrl Pts',(0.243199888597404,6.76518576550219,
87.1857440729174));
#205217=CARTESIAN_POINT('Ctrl Pts',(0.0570886373924126,6.76931499599833,
87.1944931966279));
#205218=CARTESIAN_POINT('Ctrl Pts',(-0.128876626810517,6.76577266947848,
87.2032423203384));
#205219=CARTESIAN_POINT('Ctrl Pts',(-0.314840698187495,6.76223036567996,
87.2119913879299));
#205220=CARTESIAN_POINT('Ctrl Pts',(-0.500658497950559,6.75101660879228,
87.2207404555215));
#205221=CARTESIAN_POINT('Ctrl Pts',(-0.685698951925494,6.73216948296226,
87.229489523113));
#205222=CARTESIAN_POINT('Ctrl Pts',(-0.870738280459194,6.71332247176302,
87.2382385374916));
#205223=CARTESIAN_POINT('Ctrl Pts',(-1.05499998761191,6.68684221356196,
87.2469875518701));
#205224=CARTESIAN_POINT('Ctrl Pts',(-1.23785829161367,6.65281863948532,
87.2557365662486));
#205225=CARTESIAN_POINT('Ctrl Pts',(-1.4300741291735,6.61705395368873,87.2649332999478));
#205226=CARTESIAN_POINT('Ctrl Pts',(-1.62073882535738,6.57295372727803,
87.274130033647));
#205227=CARTESIAN_POINT('Ctrl Pts',(-1.80913696091459,6.52068343478295,
87.2833267673462));
#205228=CARTESIAN_POINT('Ctrl Pts',(-1.98838356186048,6.47095219815218,
87.2920767650598));
#205229=CARTESIAN_POINT('Ctrl Pts',(-2.1655782757246,6.41382586850915,87.3008267627735));
#205230=CARTESIAN_POINT('Ctrl Pts',(-2.34011918621618,6.34949849943308,
87.3095767604872));
#205231=CARTESIAN_POINT('Ctrl Pts',(-2.51465655691013,6.28517243495584,
87.3183265807455));
#205232=CARTESIAN_POINT('Ctrl Pts',(-2.6865399629524,6.21364572242412,87.3270764010038));
#205233=CARTESIAN_POINT('Ctrl Pts',(-2.85518555379898,6.13516132252263,
87.3358262212621));
#205234=CARTESIAN_POINT('Ctrl Pts',(-3.02382794858592,6.05667841000555,
87.3445758756996));
#205235=CARTESIAN_POINT('Ctrl Pts',(-3.18923239109178,5.97123819492136,
87.3533255301371));
#205236=CARTESIAN_POINT('Ctrl Pts',(-3.35083705967589,5.87913088810775,
87.3620751845746));
#205237=CARTESIAN_POINT('Ctrl Pts',(-3.51243888042279,5.78702520443176,
87.3708246848236));
#205238=CARTESIAN_POINT('Ctrl Pts',(-3.67024081223559,5.68825280605868,
87.3795741850725));
#205239=CARTESIAN_POINT('Ctrl Pts',(-3.8237068754426,5.58314917682601,87.3883236853214));
#205240=CARTESIAN_POINT('Ctrl Pts',(-3.97717043817686,5.47804726008115,
87.3970730430119));
#205241=CARTESIAN_POINT('Ctrl Pts',(-4.12629803722343,5.36661448084326,
87.4058224007024));
#205242=CARTESIAN_POINT('Ctrl Pts',(-4.27058317206802,5.24922931204663,
87.4145717583928));
#205243=CARTESIAN_POINT('Ctrl Pts',(-4.41486614774747,5.13184589986867,
87.4233209851529));
#205244=CARTESIAN_POINT('Ctrl Pts',(-4.55430658194343,5.00851045723099,
87.432070211913));
#205245=CARTESIAN_POINT('Ctrl Pts',(-4.68843089001791,4.87964187103171,
87.4408194386731));
#205246=CARTESIAN_POINT('Ctrl Pts',(-4.82255336917802,4.75077504207996,
87.449568546129));
#205247=CARTESIAN_POINT('Ctrl Pts',(-4.95135966065118,4.61637541908112,
87.458317653585));
#205248=CARTESIAN_POINT('Ctrl Pts',(-5.07441230869245,4.47689945401844,
87.4670667610409));
#205249=CARTESIAN_POINT('Ctrl Pts',(-5.19746344226383,4.33742520555554,
87.4758157608173));
#205250=CARTESIAN_POINT('Ctrl Pts',(-5.31476088454702,4.19287495491417,
87.4845647605936));
#205251=CARTESIAN_POINT('Ctrl Pts',(-5.42590627628761,4.04373961586831,
87.4933137603699));
#205252=CARTESIAN_POINT('Ctrl Pts',(-5.53706380672581,3.89458798906857,
87.5020637156646));
#205253=CARTESIAN_POINT('Ctrl Pts',(-5.64206777071784,3.74085050155405,
87.5108136709593));
#205254=CARTESIAN_POINT('Ctrl Pts',(-5.74056148163933,3.5830493822328,87.519563626254));
#205255=CARTESIAN_POINT('Ctrl Pts',(-5.83905138951811,3.42525435593406,
87.5283132436951));
#205256=CARTESIAN_POINT('Ctrl Pts',(-5.93103139557581,3.26339625497312,
87.5370628611362));
#205257=CARTESIAN_POINT('Ctrl Pts',(-6.01618907820777,3.09802485065139,
87.5458124785773));
#205258=CARTESIAN_POINT('Ctrl Pts',(-6.1013439254492,2.93265895249773,87.5545618046932));
#205259=CARTESIAN_POINT('Ctrl Pts',(-6.17967677261773,2.76378023986166,
87.5633111308091));
#205260=CARTESIAN_POINT('Ctrl Pts',(-6.2509215700917,2.59196229227245,87.572060456925));
#205261=CARTESIAN_POINT('Ctrl Pts',(-6.32216437407696,2.42014915229239,
87.5808095382274));
#205262=CARTESIAN_POINT('Ctrl Pts',(-6.38631941548862,2.24539720663018,
87.5895586195299));
#205263=CARTESIAN_POINT('Ctrl Pts',(-6.44316881037478,2.06829994947872,
87.5983077008323));
#205264=CARTESIAN_POINT('Ctrl Pts',(-6.50002334524512,1.89118668024652,
87.6070575731746));
#205265=CARTESIAN_POINT('Ctrl Pts',(-6.54957082411038,1.71172794807922,
87.615807445517));
#205266=CARTESIAN_POINT('Ctrl Pts',(-6.59164294296029,1.53053334250576,
87.6245573178593));
#205267=CARTESIAN_POINT('Ctrl Pts',(-6.63371214082084,1.34935131693846,
87.6333065827142));
#205268=CARTESIAN_POINT('Ctrl Pts',(-6.66830695239645,1.1664339383002,87.6420558475691));
#205269=CARTESIAN_POINT('Ctrl Pts',(-6.69530988153949,0.982402458343655,
87.650805112424));
#205270=CARTESIAN_POINT('Ctrl Pts',(-6.72231419690451,0.798361530949721,
87.6595548264311));
#205271=CARTESIAN_POINT('Ctrl Pts',(-6.74172580829254,0.613206671365132,
87.6683045404381));
#205272=CARTESIAN_POINT('Ctrl Pts',(-6.75347878028163,0.427566795116044,
87.6770542544451));
#205273=CARTESIAN_POINT('Ctrl Pts',(-6.76248992368205,0.285234494207813,
87.6837627642334));
#205274=CARTESIAN_POINT('Ctrl Pts',(-6.76699999999992,0.142617266094565,
87.6904712740216));
#205275=CARTESIAN_POINT('Ctrl Pts',(-6.767,3.76450867784256E-12,87.6971797838099));
#205276=CARTESIAN_POINT('',(-6.767,3.91310898614772E-12,87.3028202161898));
#205277=CARTESIAN_POINT('Ctrl Pts',(3.09910619832139,6.01563211736938,86.6514537215909));
#205278=CARTESIAN_POINT('Ctrl Pts',(2.94383374465635,6.09562467911404,86.6596510417769));
#205279=CARTESIAN_POINT('Ctrl Pts',(2.78541012641986,6.16962848848196,86.6678483619629));
#205280=CARTESIAN_POINT('Ctrl Pts',(2.62433993952006,6.23739760491824,86.6760456821488));
#205281=CARTESIAN_POINT('Ctrl Pts',(2.46328560259829,6.30516005259089,86.6842421956843));
#205282=CARTESIAN_POINT('Ctrl Pts',(2.29958554603934,6.36668888949535,86.6924387092198));
#205283=CARTESIAN_POINT('Ctrl Pts',(2.13376513616885,6.42178599329426,86.7006352227552));
#205284=CARTESIAN_POINT('Ctrl Pts',(1.96793089327903,6.47688769338684,86.7088324200578));
#205285=CARTESIAN_POINT('Ctrl Pts',(1.79997628520236,6.5255564784604,86.7170296173603));
#205286=CARTESIAN_POINT('Ctrl Pts',(1.63044270444559,6.56764383835788,86.7252268146628));
#205287=CARTESIAN_POINT('Ctrl Pts',(1.46086415536567,6.60974236181358,86.7334261862497));
#205288=CARTESIAN_POINT('Ctrl Pts',(1.28970614750773,6.64525589676282,86.7416255578366));
#205289=CARTESIAN_POINT('Ctrl Pts',(1.11752120001407,6.67408685645603,86.7498249294235));
#205290=CARTESIAN_POINT('Ctrl Pts',(0.945170491246863,6.70294557151733,
86.7580321944895));
#205291=CARTESIAN_POINT('Ctrl Pts',(0.771791222117369,6.72510880078116,
86.7662394595554));
#205292=CARTESIAN_POINT('Ctrl Pts',(0.597942898001018,6.74053063866118,
86.7744467246214));
#205293=CARTESIAN_POINT('Ctrl Pts',(0.424004893424784,6.75596043196741,
86.7826582234429));
#205294=CARTESIAN_POINT('Ctrl Pts',(0.249597709372894,6.76464188321101,
86.7908697222644));
#205295=CARTESIAN_POINT('Ctrl Pts',(0.0752817218204754,6.76658123887978,
86.7990812210859));
#205296=CARTESIAN_POINT('Ctrl Pts',(-0.0992660794267649,6.76852317359599,
86.8073036399493));
#205297=CARTESIAN_POINT('Ctrl Pts',(-0.27372208355303,6.76370510835888,
86.8155260588126));
#205298=CARTESIAN_POINT('Ctrl Pts',(-0.447529064371234,6.7521853304351,
86.823748477676));
#205299=CARTESIAN_POINT('Ctrl Pts',(-0.57165930965902,6.74395808402298,
86.8296208014777));
#205300=CARTESIAN_POINT('Ctrl Pts',(-0.695458615619168,6.73231365799035,
86.8354931252795));
#205301=CARTESIAN_POINT('Ctrl Pts',(-0.818727194630302,6.71728924349494,
86.8413654490812));
#205302=CARTESIAN_POINT('Ctrl Pts',(-1.00630558582367,6.69442651949601,
86.850301392532));
#205303=CARTESIAN_POINT('Ctrl Pts',(-1.19304528443073,6.66368782905504,
86.8592373359827));
#205304=CARTESIAN_POINT('Ctrl Pts',(-1.37829705002254,6.62514801660304,
86.8681732794335));
#205305=CARTESIAN_POINT('Ctrl Pts',(-1.56327033307593,6.58666613971115,
86.8770957897911));
#205306=CARTESIAN_POINT('Ctrl Pts',(-1.7467598940025,6.54040659298026,86.8860183001487));
#205307=CARTESIAN_POINT('Ctrl Pts',(-1.92812452835058,6.48649557181479,
86.8949408105064));
#205308=CARTESIAN_POINT('Ctrl Pts',(-2.10904476306238,6.43271664938115,
86.9038414579448));
#205309=CARTESIAN_POINT('Ctrl Pts',(-2.28785021585018,6.37132374460046,
86.9127421053832));
#205310=CARTESIAN_POINT('Ctrl Pts',(-2.46391332976258,6.30249316567803,
86.9216427528216));
#205311=CARTESIAN_POINT('Ctrl Pts',(-2.63970435986028,6.23376895592098,
86.9305296454077));
#205312=CARTESIAN_POINT('Ctrl Pts',(-2.81276126539432,6.15763009309876,
86.9394165379939));
#205313=CARTESIAN_POINT('Ctrl Pts',(-2.98247215036693,6.07430233625934,
86.9483034305801));
#205314=CARTESIAN_POINT('Ctrl Pts',(-3.15174681501544,5.9911887628596,86.9571674805351));
#205315=CARTESIAN_POINT('Ctrl Pts',(-3.31769238976927,5.90092328075294,
86.96603153049));
#205316=CARTESIAN_POINT('Ctrl Pts',(-3.47971814726007,5.80377899438193,
86.974895580445));
#205317=CARTESIAN_POINT('Ctrl Pts',(-3.63462780549006,5.71090124189506,
86.9833703252653));
#205318=CARTESIAN_POINT('Ctrl Pts',(-3.78595431431762,5.61173602165759,
86.9918450700856));
#205319=CARTESIAN_POINT('Ctrl Pts',(-3.93319867912149,5.50656309784579,
87.0003198149059));
#205320=CARTESIAN_POINT('Ctrl Pts',(-4.07582437658705,5.40468917123996,
87.008528729335));
#205321=CARTESIAN_POINT('Ctrl Pts',(-4.21448195710526,5.29727593196517,
87.0167376437641));
#205322=CARTESIAN_POINT('Ctrl Pts',(-4.34872903395071,5.18467402922056,
87.0249465581932));
#205323=CARTESIAN_POINT('Ctrl Pts',(-4.48300802735684,5.07204535594547,
87.03315742425));
#205324=CARTESIAN_POINT('Ctrl Pts',(-4.6128741552097,4.95422579040202,87.0413682903068));
#205325=CARTESIAN_POINT('Ctrl Pts',(-4.7379194619536,4.83160513411861,87.0495791563636));
#205326=CARTESIAN_POINT('Ctrl Pts',(-4.8630167874318,4.70893346775331,87.0577934381333));
#205327=CARTESIAN_POINT('Ctrl Pts',(-4.98328904247643,4.58145698081226,
87.0660077199029));
#205328=CARTESIAN_POINT('Ctrl Pts',(-5.09836630564968,4.44960110722479,
87.0742220016726));
#205329=CARTESIAN_POINT('Ctrl Pts',(-5.21357309736919,4.31759681944019,
87.082445529265));
#205330=CARTESIAN_POINT('Ctrl Pts',(-5.32357298385505,4.18120356786216,
87.0906690568573));
#205331=CARTESIAN_POINT('Ctrl Pts',(-5.42803680107344,4.04087929616716,
87.0988925844497));
#205332=CARTESIAN_POINT('Ctrl Pts',(-5.53256757553528,3.90046508207229,
87.1071213830034));
#205333=CARTESIAN_POINT('Ctrl Pts',(-5.63155500635019,3.75611511803967,
87.1153501815571));
#205334=CARTESIAN_POINT('Ctrl Pts',(-5.72471423974431,3.60831482457791,
87.1235789801108));
#205335=CARTESIAN_POINT('Ctrl Pts',(-5.81800169936844,3.46031109583945,
87.1318191049472));
#205336=CARTESIAN_POINT('Ctrl Pts',(-5.905444760755,3.30884785924964,87.1400592297836));
#205337=CARTESIAN_POINT('Ctrl Pts',(-5.98680486650131,3.15443441688621,
87.14829935462));
#205338=CARTESIAN_POINT('Ctrl Pts',(-6.0229253958474,3.08588122087992,87.1519576299902));
#205339=CARTESIAN_POINT('Ctrl Pts',(-6.05784761721732,3.01674679976217,
87.1556159053605));
#205340=CARTESIAN_POINT('Ctrl Pts',(-6.0915537524103,2.94707683671396,87.1592741807307));
#205341=CARTESIAN_POINT('Ctrl Pts',(-6.1759339152134,2.77266458829585,87.1684323315999));
#205342=CARTESIAN_POINT('Ctrl Pts',(-6.25285077445145,2.59456200883916,
87.1775904824692));
#205343=CARTESIAN_POINT('Ctrl Pts',(-6.32201145009694,2.41339185066229,
87.1867486333385));
#205344=CARTESIAN_POINT('Ctrl Pts',(-6.39107338526958,2.2324803485341,87.1958937091454));
#205345=CARTESIAN_POINT('Ctrl Pts',(-6.45240116500455,2.04851021229947,
87.2050387849522));
#205346=CARTESIAN_POINT('Ctrl Pts',(-6.50574998604927,1.86212408797588,
87.2141838607591));
#205347=CARTESIAN_POINT('Ctrl Pts',(-6.55895794440002,1.67623009920609,
87.2233047898278));
#205348=CARTESIAN_POINT('Ctrl Pts',(-6.60422893723639,1.48793306383961,
87.2324257188965));
#205349=CARTESIAN_POINT('Ctrl Pts',(-6.64136810965814,1.29789006931091,
87.2415466479652));
#205350=CARTESIAN_POINT('Ctrl Pts',(-6.67843688274809,1.10820731166839,
87.2506502878142));
#205351=CARTESIAN_POINT('Ctrl Pts',(-6.70740454900505,0.916785410033402,
87.2597539276632));
#205352=CARTESIAN_POINT('Ctrl Pts',(-6.72812655419379,0.724294187987466,
87.2688575675122));
#205353=CARTESIAN_POINT('Ctrl Pts',(-6.74878566459043,0.532387209371671,
87.2779335762738));
#205354=CARTESIAN_POINT('Ctrl Pts',(-6.76124902294262,0.339417601311186,
87.2870095850354));
#205355=CARTESIAN_POINT('Ctrl Pts',(-6.76542347337597,0.146062404106671,
87.2960855937971));
#205356=CARTESIAN_POINT('Ctrl Pts',(-6.76645598844231,0.0982376287365919,
87.298330467928));
#205357=CARTESIAN_POINT('Ctrl Pts',(-6.76698164913032,0.0503893190892879,
87.3005753420589));
#205358=CARTESIAN_POINT('Ctrl Pts',(-6.76699952786402,0.00252782281982319,
87.3028202161898));
#205359=CARTESIAN_POINT('Ctrl Pts',(-6.767,3.91310882501737E-12,87.3028202161898));
#205360=CARTESIAN_POINT('Ctrl Pts',(-6.76700000000011,-0.186007249523053,
87.311569728001));
#205361=CARTESIAN_POINT('Ctrl Pts',(-6.75932637294541,-0.372014355746198,
87.3203192398122));
#205362=CARTESIAN_POINT('Ctrl Pts',(-6.7440051826421,-0.557389537483875,
87.3290687516234));
#205363=CARTESIAN_POINT('Ctrl Pts',(-6.72868405705124,-0.742763936248352,
87.337818226479));
#205364=CARTESIAN_POINT('Ctrl Pts',(-6.7057154564577,-0.927506130239004,
87.3465677013347));
#205365=CARTESIAN_POINT('Ctrl Pts',(-6.67517739404852,-1.11098863989852,
87.3553171761904));
#205366=CARTESIAN_POINT('Ctrl Pts',(-6.6446394580873,-1.29447038981804,
87.3640666148174));
#205367=CARTESIAN_POINT('Ctrl Pts',(-6.60653217008382,-1.47669218313562,
87.3728160534445));
#205368=CARTESIAN_POINT('Ctrl Pts',(-6.56098496092703,-1.65703510599185,
87.3815654920715));
#205369=CARTESIAN_POINT('Ctrl Pts',(-6.51543793658326,-1.83737729708595,
87.3903148951966));
#205370=CARTESIAN_POINT('Ctrl Pts',(-6.46245112167454,-2.01584035510818,
87.3990642983218));
#205371=CARTESIAN_POINT('Ctrl Pts',(-6.40220448374292,-2.1918181376068,
87.407813701447));
#205372=CARTESIAN_POINT('Ctrl Pts',(-6.34195808526543,-2.36779522067039,
87.4165630697971));
#205373=CARTESIAN_POINT('Ctrl Pts',(-6.27445201433143,-2.54128677684068,
87.4253124381472));
#205374=CARTESIAN_POINT('Ctrl Pts',(-6.19991555071942,-2.71170355384721,
87.4340618064973));
#205375=CARTESIAN_POINT('Ctrl Pts',(-6.12537937716736,-2.88211966767384,
87.442811140799));
#205376=CARTESIAN_POINT('Ctrl Pts',(-6.04381298052568,-3.0494607637169,
87.4515604751008));
#205377=CARTESIAN_POINT('Ctrl Pts',(-5.95549339335884,-3.2131584837445,
87.4603098094026));
#205378=CARTESIAN_POINT('Ctrl Pts',(-5.86717414255468,-3.37685558033391,
87.4690591103828));
#205379=CARTESIAN_POINT('Ctrl Pts',(-5.77210188876663,-3.5369090764665,
87.477808411363));
#205380=CARTESIAN_POINT('Ctrl Pts',(-5.67059953347068,-3.69277536969176,
87.4865577123431));
#205381=CARTESIAN_POINT('Ctrl Pts',(-5.56909755631467,-3.84864108224802,
87.4953069807284));
#205382=CARTESIAN_POINT('Ctrl Pts',(-5.46116568196946,-4.00031938297385,
87.5040562491137));
#205383=CARTESIAN_POINT('Ctrl Pts',(-5.34717048533713,-4.14729511859712,
87.512805517499));
#205384=CARTESIAN_POINT('Ctrl Pts',(-5.23317570391972,-4.29427031887749,
87.521554754016));
#205385=CARTESIAN_POINT('Ctrl Pts',(-5.11311782003678,-4.43654276189357,
87.530303990533));
#205386=CARTESIAN_POINT('Ctrl Pts',(-4.98740458984947,-4.57362924351641,
87.5390532270501));
#205387=CARTESIAN_POINT('Ctrl Pts',(-4.86169180711949,-4.71071523720054,
87.5478024324255));
#205388=CARTESIAN_POINT('Ctrl Pts',(-4.73032391204389,-4.84261509523025,
87.5565516378009));
#205389=CARTESIAN_POINT('Ctrl Pts',(-4.59374707013829,-4.96888084538117,
87.5653008431764));
#205390=CARTESIAN_POINT('Ctrl Pts',(-4.45717070301705,-5.09514615659235,
87.5740500181368));
#205391=CARTESIAN_POINT('Ctrl Pts',(-4.31538563571333,-5.21577720459284,
87.5827991930972));
#205392=CARTESIAN_POINT('Ctrl Pts',(-4.16887341029835,-5.33036429232631,
87.5915483680576));
#205393=CARTESIAN_POINT('Ctrl Pts',(-4.02236168204043,-5.44495099123367,
87.6002975133297));
#205394=CARTESIAN_POINT('Ctrl Pts',(-3.87112305348512,-5.5534935943836,
87.6090466586017));
#205395=CARTESIAN_POINT('Ctrl Pts',(-3.71567117018118,-5.65562346298659,
87.6177958038737));
#205396=CARTESIAN_POINT('Ctrl Pts',(-3.56021980146173,-5.75775299351426,
87.6265449201839));
#205397=CARTESIAN_POINT('Ctrl Pts',(-3.40055544538699,-5.8534696746367,
87.635294036494));
#205398=CARTESIAN_POINT('Ctrl Pts',(-3.23722035987199,-5.94244842986713,
87.6440431528042));
#205399=CARTESIAN_POINT('Ctrl Pts',(-3.07388580147527,-6.03142689794352,
87.6527922408791));
#205400=CARTESIAN_POINT('Ctrl Pts',(-2.90688078896926,-6.11366734656616,
87.6615413289539));
#205401=CARTESIAN_POINT('Ctrl Pts',(-2.73677250721718,-6.188890469522,87.6702904170288));
#205402=CARTESIAN_POINT('Ctrl Pts',(-2.56666476031827,-6.26411335596186,
87.6790394775948));
#205403=CARTESIAN_POINT('Ctrl Pts',(-2.39345402575506,-6.33231884500427,
87.6877885381608));
#205404=CARTESIAN_POINT('Ctrl Pts',(-2.21772856065927,-6.39327529762611,
87.6965375987268));
#205405=CARTESIAN_POINT('Ctrl Pts',(-2.04200363348862,-6.45423156365,87.7052866325105));
#205406=CARTESIAN_POINT('Ctrl Pts',(-1.8637642618964,-6.50793874375554,
87.7140356662942));
#205407=CARTESIAN_POINT('Ctrl Pts',(-1.68361577753529,-6.55421443909446,
87.7227847000779));
#205408=CARTESIAN_POINT('Ctrl Pts',(-1.50346782968192,-6.60048999661778,
87.7315337078057));
#205409=CARTESIAN_POINT('Ctrl Pts',(-1.32141105795398,-6.6393340423763,
87.7402827155336));
#205410=CARTESIAN_POINT('Ctrl Pts',(-1.13806375487451,-6.67061465607488,
87.7490317232614));
#205411=CARTESIAN_POINT('Ctrl Pts',(-0.954716982608237,-6.70189517921219,
87.7577807056598));
#205412=CARTESIAN_POINT('Ctrl Pts',(-0.770079968908298,-6.72561226592155,
87.7665296880581));
#205413=CARTESIAN_POINT('Ctrl Pts',(-0.584779765565347,-6.74168536983041,
87.7752786704565));
#205414=CARTESIAN_POINT('Ctrl Pts',(-0.391489830658313,-6.75845151013813,
87.7844048894664));
#205415=CARTESIAN_POINT('Ctrl Pts',(-0.197478578245256,-6.76689983031605,
87.7935311084762));
#205416=CARTESIAN_POINT('Ctrl Pts',(-0.00346287645816003,-6.76699911397117,
87.8026573274861));
#205417=CARTESIAN_POINT('Ctrl Pts',(0.184489834648061,-6.76709529501207,
87.8114983521519));
#205418=CARTESIAN_POINT('Ctrl Pts',(0.372446404243646,-6.759356397382,87.8203393768177));
#205419=CARTESIAN_POINT('Ctrl Pts',(0.559755019482719,-6.74380925873233,
87.8291804014835));
#205420=CARTESIAN_POINT('Ctrl Pts',(0.745134705516256,-6.72842222659867,
87.8379303800933));
#205421=CARTESIAN_POINT('Ctrl Pts',(0.929879431223152,-6.70538706057599,
87.846680358703));
#205422=CARTESIAN_POINT('Ctrl Pts',(1.11336163626295,-6.67478200894216,
87.8554303373128));
#205423=CARTESIAN_POINT('Ctrl Pts',(1.29684196300207,-6.64417727061113,
87.8641802263493));
#205424=CARTESIAN_POINT('Ctrl Pts',(1.47905951217019,-6.60600284890701,
87.8729301153858));
#205425=CARTESIAN_POINT('Ctrl Pts',(1.65939532066612,-6.5603884160735,87.8816800044224));
#205426=CARTESIAN_POINT('Ctrl Pts',(1.83972934300345,-6.51477443503386,
87.8904298067945));
#205427=CARTESIAN_POINT('Ctrl Pts',(2.01818138405824,-6.46172066062279,
87.8991796091667));
#205428=CARTESIAN_POINT('Ctrl Pts',(2.19414528353774,-6.40140730423624,
87.9079294115389));
#205429=CARTESIAN_POINT('Ctrl Pts',(2.37010749863578,-6.341094525188,87.9166791301552));
#205430=CARTESIAN_POINT('Ctrl Pts',(2.54358134866041,-6.27352239616673,
87.9254288487715));
#205431=CARTESIAN_POINT('Ctrl Pts',(2.71397759435142,-6.19892043967,87.9341785673878));
#205432=CARTESIAN_POINT('Ctrl Pts',(2.88437226557709,-6.1243191724971,87.9429282051565));
#205433=CARTESIAN_POINT('Ctrl Pts',(3.05168912680541,-6.04268832279008,
87.9516778429252));
#205434=CARTESIAN_POINT('Ctrl Pts',(3.2153598627344,-5.95430516123558,87.9604274806939));
#205435=CARTESIAN_POINT('Ctrl Pts',(3.3790291407245,-5.86592278697667,87.969177040523));
#205436=CARTESIAN_POINT('Ctrl Pts',(3.53905210621203,-5.77078835742169,
87.9779266003521));
#205437=CARTESIAN_POINT('Ctrl Pts',(3.6948852283135,-5.66922500431856,87.9866761601812));
#205438=CARTESIAN_POINT('Ctrl Pts',(3.85071701406603,-5.56766252217326,
87.9954256449783));
#205439=CARTESIAN_POINT('Ctrl Pts',(4.00235878822078,-5.45967138329609,
88.0041751297754));
#205440=CARTESIAN_POINT('Ctrl Pts',(4.14929549611011,-5.34561838199851,
88.0129246145725));
#205441=CARTESIAN_POINT('Ctrl Pts',(4.29623099275787,-5.23156632087264,
88.0216740272451));
#205442=CARTESIAN_POINT('Ctrl Pts',(4.43846127435738,-5.11145267305216,
88.0304234399177));
#205443=CARTESIAN_POINT('Ctrl Pts',(4.57550326054164,-4.9856854005014,88.0391728525903));
#205444=CARTESIAN_POINT('Ctrl Pts',(4.71254416257516,-4.85991912290617,
88.0479221960455));
#205445=CARTESIAN_POINT('Ctrl Pts',(4.8443966401851,-4.72849950385677,88.0566715395008));
#205446=CARTESIAN_POINT('Ctrl Pts',(4.97061286794506,-4.59187289861326,
88.065420882956));
#205447=CARTESIAN_POINT('Ctrl Pts',(5.09682813912455,-4.45524732884947,
88.0741701601009));
#205448=CARTESIAN_POINT('Ctrl Pts',(5.21740705147619,-4.31341506236053,
88.0829194372457));
#205449=CARTESIAN_POINT('Ctrl Pts',(5.33194007545486,-4.16685781275992,
88.0916687143905));
#205450=CARTESIAN_POINT('Ctrl Pts',(5.44647226944278,-4.02030162522122,
88.1004179281316));
#205451=CARTESIAN_POINT('Ctrl Pts',(5.55495848627908,-3.86902074888228,
88.1091671418728));
#205452=CARTESIAN_POINT('Ctrl Pts',(5.65703027291587,-3.71352898080969,
88.1179163556139));
#205453=CARTESIAN_POINT('Ctrl Pts',(5.75910135376803,-3.55803828789902,
88.1266655088578));
#205454=CARTESIAN_POINT('Ctrl Pts',(5.85475793592566,-3.39833700107034,
88.1354146621017));
#205455=CARTESIAN_POINT('Ctrl Pts',(5.9436751442722,-3.23496750823882,88.1441638153455));
#205456=CARTESIAN_POINT('Ctrl Pts',(6.03259176732475,-3.0715990907805,88.1529129109985));
#205457=CARTESIAN_POINT('Ctrl Pts',(6.11476896835772,-2.90456276731755,
88.1616620066514));
#205458=CARTESIAN_POINT('Ctrl Pts',(6.18992765547747,-2.73442583003366,
88.1704111023043));
#205459=CARTESIAN_POINT('Ctrl Pts',(6.26508587282926,-2.56428995616483,
88.1791601432724));
#205460=CARTESIAN_POINT('Ctrl Pts',(6.33322554827043,-2.39105376935511,
88.1879091842404));
#205461=CARTESIAN_POINT('Ctrl Pts',(6.39411526732925,-2.21530561054385,
88.1966582252084));
#205462=CARTESIAN_POINT('Ctrl Pts',(6.45500462602747,-2.03955849185415,
88.2054072143975));
#205463=CARTESIAN_POINT('Ctrl Pts',(6.50864402040646,-1.86129970164872,
88.2141562035865));
#205464=CARTESIAN_POINT('Ctrl Pts',(6.55485128368514,-1.68113463136397,
88.2229051927755));
#205465=CARTESIAN_POINT('Ctrl Pts',(6.60199809554247,-1.49730620117218,
88.231832078247));
#205466=CARTESIAN_POINT('Ctrl Pts',(6.64140720707802,-1.31149343246059,
88.2407589637184));
#205467=CARTESIAN_POINT('Ctrl Pts',(6.67293928722821,-1.12435326697897,
88.2496858491898));
#205468=CARTESIAN_POINT('Ctrl Pts',(6.70384625876204,-0.940923067010339,
88.2584357633673));
#205469=CARTESIAN_POINT('Ctrl Pts',(6.72718554579753,-0.75621789952545,
88.2671856775447));
#205470=CARTESIAN_POINT('Ctrl Pts',(6.74287786815295,-0.570865181258313,
88.2759355917222));
#205471=CARTESIAN_POINT('Ctrl Pts',(6.75856988190823,-0.38551610807784,
88.2846853338267));
#205472=CARTESIAN_POINT('Ctrl Pts',(6.76661520773391,-0.199519795230314,
88.2934350759312));
#205473=CARTESIAN_POINT('Ctrl Pts',(6.76698651789578,-0.0135080204596825,
88.3021848180356));
#205474=CARTESIAN_POINT('Ctrl Pts',(6.76735782124913,0.172500343508857,
88.3109343997006));
#205475=CARTESIAN_POINT('Ctrl Pts',(6.76005538995206,0.358523882206753,
88.3196839813656));
#205476=CARTESIAN_POINT('Ctrl Pts',(6.74510402742395,0.543930748560149,
88.3284335630305));
#205477=CARTESIAN_POINT('Ctrl Pts',(6.73015291918077,0.729334461610889,
88.3371829958872));
#205478=CARTESIAN_POINT('Ctrl Pts',(6.70755316306655,0.914121237630222,
88.3459324287439));
#205479=CARTESIAN_POINT('Ctrl Pts',(6.67738151874649,1.09766345165665,88.3546818616006));
#205480=CARTESIAN_POINT('Ctrl Pts',(6.64721034747657,1.2812027879921,88.3634311572781));
#205481=CARTESIAN_POINT('Ctrl Pts',(6.60946757205242,1.46349731859877,88.3721804529556));
#205482=CARTESIAN_POINT('Ctrl Pts',(6.56428138111635,1.64392790277714,88.3809297486332));
#205483=CARTESIAN_POINT('Ctrl Pts',(6.51909583859976,1.82435589778607,88.3896789187587));
#205484=CARTESIAN_POINT('Ctrl Pts',(6.46646716393014,2.00291972191816,88.3984280888844));
#205485=CARTESIAN_POINT('Ctrl Pts',(6.40657409873036,2.17901292274215,88.40717725901));
#205486=CARTESIAN_POINT('Ctrl Pts',(6.34668181342242,2.35510383058531,88.4159263152091));
#205487=CARTESIAN_POINT('Ctrl Pts',(6.27952541914228,2.52872390822137,88.4246753714082));
#205488=CARTESIAN_POINT('Ctrl Pts',(6.20533299175708,2.69928350889846,88.4334244276073));
#205489=CARTESIAN_POINT('Ctrl Pts',(6.12831602991743,2.8763363796521,88.4425065637655));
#205490=CARTESIAN_POINT('Ctrl Pts',(6.04371690605466,3.05009086601076,88.4515886999237));
#205491=CARTESIAN_POINT('Ctrl Pts',(5.95184520316826,3.21991112882374,88.4606708360819));
#205492=CARTESIAN_POINT('Ctrl Pts',(5.86333549509478,3.38351691182665,88.4694206164255));
#205493=CARTESIAN_POINT('Ctrl Pts',(5.7680761809958,3.54347103711661,88.478170396769));
#205494=CARTESIAN_POINT('Ctrl Pts',(5.66639083309234,3.69923018027361,88.4869201771126));
#205495=CARTESIAN_POINT('Ctrl Pts',(5.56470914082432,3.85498372381716,88.4956696428975));
#205496=CARTESIAN_POINT('Ctrl Pts',(5.45660203372311,4.00654234701665,88.5044191086824));
#205497=CARTESIAN_POINT('Ctrl Pts',(5.34243669839474,4.15339127986338,88.5131685744673));
#205498=CARTESIAN_POINT('Ctrl Pts',(5.2282748605086,4.30023571400953,88.5219177722133));
#205499=CARTESIAN_POINT('Ctrl Pts',(5.10805534167391,4.44237052028148,88.5306669699593));
#205500=CARTESIAN_POINT('Ctrl Pts',(4.98218644340242,4.57931296628404,88.5394161677053));
#205501=CARTESIAN_POINT('Ctrl Pts',(4.85632073219883,4.71625194483055,88.548165143917));
#205502=CARTESIAN_POINT('Ctrl Pts',(4.72480612170621,4.84799861524214,88.5569141201286));
#205503=CARTESIAN_POINT('Ctrl Pts',(4.58808925235619,4.97410554898201,88.5656630963402));
#205504=CARTESIAN_POINT('Ctrl Pts',(4.45136349474367,5.10022068120928,88.574412641342));
#205505=CARTESIAN_POINT('Ctrl Pts',(4.30943501210409,5.22069514871562,88.5831621863436));
#205506=CARTESIAN_POINT('Ctrl Pts',(4.16278587432121,5.33511975165992,88.5919117313453));
#205507=CARTESIAN_POINT('Ctrl Pts',(4.01614535740789,5.44953762807591,88.6006607619991));
#205508=CARTESIAN_POINT('Ctrl Pts',(3.86478496658266,5.55790617532546,88.6094097926528));
#205509=CARTESIAN_POINT('Ctrl Pts',(3.70921874747539,5.65985735539131,88.6181588233065));
#205510=CARTESIAN_POINT('Ctrl Pts',(3.55365041606255,5.76180991976828,88.6269079727562));
#205511=CARTESIAN_POINT('Ctrl Pts',(3.39387638174887,5.85734478552602,88.6356571222058));
#205512=CARTESIAN_POINT('Ctrl Pts',(3.23043927904913,5.94613749121029,88.6444062716554));
#205513=CARTESIAN_POINT('Ctrl Pts',(3.18691767070677,5.96978206944017,88.6467360795716));
#205514=CARTESIAN_POINT('Ctrl Pts',(3.14313645919747,5.99294880633365,88.6490658874879));
#205515=CARTESIAN_POINT('Ctrl Pts',(3.09910619832125,6.01563211736945,88.6513956954041));
#205516=CARTESIAN_POINT('Origin',(0.,0.,4.30282021618968));
#205517=CARTESIAN_POINT('',(3.09910619832119,6.01563211736948,91.0458502363996));
#205518=CARTESIAN_POINT('',(3.09910619832126,6.01563211736944,90.6515218032501));
#205519=CARTESIAN_POINT('',(3.09910619832133,6.0156321173694,4.30282021618968));
#205520=CARTESIAN_POINT('',(-6.76699986371212,0.00135813113412233,89.6971797838355));
#205521=CARTESIAN_POINT('Ctrl Pts',(-6.76699986371212,0.00135813113412683,
89.6971797838355));
#205522=CARTESIAN_POINT('Ctrl Pts',(-6.76703500186648,-0.173720607425384,
89.7054399898427));
#205523=CARTESIAN_POINT('Ctrl Pts',(-6.7602712822433,-0.348979168962801,
89.71370019585));
#205524=CARTESIAN_POINT('Ctrl Pts',(-6.74669303449373,-0.523853126662233,
89.7219604018572));
#205525=CARTESIAN_POINT('Ctrl Pts',(-6.7331260173862,-0.698582445166926,
89.7302137758035));
#205526=CARTESIAN_POINT('Ctrl Pts',(-6.71275572688528,-0.872927442307335,
89.7384671497498));
#205527=CARTESIAN_POINT('Ctrl Pts',(-6.68561853810828,-1.04632392828553,
89.746720523696));
#205528=CARTESIAN_POINT('Ctrl Pts',(-6.65849853992186,-1.21961057281989,
89.7549686693788));
#205529=CARTESIAN_POINT('Ctrl Pts',(-6.62462023809079,-1.39194955459326,
89.7632168150617));
#205530=CARTESIAN_POINT('Ctrl Pts',(-6.58407182212003,-1.56278189174469,
89.7714649607445));
#205531=CARTESIAN_POINT('Ctrl Pts',(-6.54354124270484,-1.73353908266899,
89.7797094782089));
#205532=CARTESIAN_POINT('Ctrl Pts',(-6.49634647718534,-1.90279060574003,
89.7879539956732));
#205533=CARTESIAN_POINT('Ctrl Pts',(-6.44262681568658,-2.06998761199101,
89.7961985131377));
#205534=CARTESIAN_POINT('Ctrl Pts',(-6.3884416573607,-2.23863342997576,
89.8045144717954));
#205535=CARTESIAN_POINT('Ctrl Pts',(-6.32761805760378,-2.40518859796871,
89.812830430453));
#205536=CARTESIAN_POINT('Ctrl Pts',(-6.26035054698763,-2.5691049081016,
89.8211463891107));
#205537=CARTESIAN_POINT('Ctrl Pts',(-6.19366655536911,-2.73159930920131,
89.8293902101226));
#205538=CARTESIAN_POINT('Ctrl Pts',(-6.12065017010656,-2.89150013206863,
89.8376340311344));
#205539=CARTESIAN_POINT('Ctrl Pts',(-6.0415394290993,-3.04829301850045,
89.8458778521462));
#205540=CARTESIAN_POINT('Ctrl Pts',(-5.9624154888514,-3.20511206505934,
89.8541230485993));
#205541=CARTESIAN_POINT('Ctrl Pts',(-5.87719532613465,-3.35882182562928,
89.8623682450523));
#205542=CARTESIAN_POINT('Ctrl Pts',(-5.78616317349773,-3.50893213523127,
89.8706134415054));
#205543=CARTESIAN_POINT('Ctrl Pts',(-5.69509985964289,-3.65909382909624,
89.8788614603719));
#205544=CARTESIAN_POINT('Ctrl Pts',(-5.59822077542912,-3.80565331434493,
89.8871094792383));
#205545=CARTESIAN_POINT('Ctrl Pts',(-5.49585379998729,-3.94814893452176,
89.8953574981047));
#205546=CARTESIAN_POINT('Ctrl Pts',(-5.39198942920089,-4.09272894057942,
89.9037261666729));
#205547=CARTESIAN_POINT('Ctrl Pts',(-5.28247558541717,-4.23312495718327,
89.912094835241));
#205548=CARTESIAN_POINT('Ctrl Pts',(-5.16769692743683,-4.36888972922869,
89.9204635038092));
#205549=CARTESIAN_POINT('Ctrl Pts',(-5.05437929604085,-4.50292634078969,
89.9287256469355));
#205550=CARTESIAN_POINT('Ctrl Pts',(-4.93593037606399,-4.63244869562128,
89.9369877900618));
#205551=CARTESIAN_POINT('Ctrl Pts',(-4.81275718074231,-4.75706393894525,
89.9452499331881));
#205552=CARTESIAN_POINT('Ctrl Pts',(-4.68720184094805,-4.88408921565603,
89.9536718644772));
#205553=CARTESIAN_POINT('Ctrl Pts',(-4.5567379217822,-5.00601537902839,
89.9620937957663));
#205554=CARTESIAN_POINT('Ctrl Pts',(-4.42183123249962,-5.12246986826579,
89.9705157270554));
#205555=CARTESIAN_POINT('Ctrl Pts',(-4.28692454321713,-5.2389243575031,
89.9789376583444));
#205556=CARTESIAN_POINT('Ctrl Pts',(-4.14757542056657,-5.34990697991828,
89.9873595896335));
#205557=CARTESIAN_POINT('Ctrl Pts',(-4.00427986530766,-5.45509227788969,
89.9957815209225));
#205558=CARTESIAN_POINT('Ctrl Pts',(-3.8669748904592,-5.55588022393795,
90.0038513669253));
#205559=CARTESIAN_POINT('Ctrl Pts',(-3.72560857413471,-5.65166688119633,
90.0119212129281));
#205560=CARTESIAN_POINT('Ctrl Pts',(-3.58058750187815,-5.74209736432551,
90.0199910589308));
#205561=CARTESIAN_POINT('Ctrl Pts',(-3.43574888457639,-5.83241407440466,
90.0280507520409));
#205562=CARTESIAN_POINT('Ctrl Pts',(-3.28726497294158,-5.91738782370924,
90.0361104451509));
#205563=CARTESIAN_POINT('Ctrl Pts',(-3.13557561949261,-5.99670363903733,
90.044170138261));
#205564=CARTESIAN_POINT('Ctrl Pts',(-2.98404381953061,-6.07593707229316,
90.0522214600996));
#205565=CARTESIAN_POINT('Ctrl Pts',(-2.82931353102591,-6.14952409478376,
90.0602727819382));
#205566=CARTESIAN_POINT('Ctrl Pts',(-2.67185372211453,-6.21719283017849,
90.0683241037768));
#205567=CARTESIAN_POINT('Ctrl Pts',(-2.5145229554147,-6.28480610936931,
90.0763688273578));
#205568=CARTESIAN_POINT('Ctrl Pts',(-2.3544674615105,-6.34651060832816,
90.0844135509388));
#205569=CARTESIAN_POINT('Ctrl Pts',(-2.19218086535646,-6.40208029109016,
90.0924582745199));
#205570=CARTESIAN_POINT('Ctrl Pts',(-2.02999174247932,-6.45761659734908,
90.1004981662442));
#205571=CARTESIAN_POINT('Ctrl Pts',(-1.86557453707419,-6.50702530198869,
90.1085380579686));
#205572=CARTESIAN_POINT('Ctrl Pts',(-1.69944281225294,-6.5501284817843,
90.116577949693));
#205573=CARTESIAN_POINT('Ctrl Pts',(-1.52973381624805,-6.59415979112994,
90.1247909623129));
#205574=CARTESIAN_POINT('Ctrl Pts',(-1.35823599277948,-6.63161078727063,
90.1330039749329));
#205575=CARTESIAN_POINT('Ctrl Pts',(-1.18551359082838,-6.66234542229395,
90.1412169875528));
#205576=CARTESIAN_POINT('Ctrl Pts',(-1.01649097311715,-6.69242170890971,
90.1492540740954));
#205577=CARTESIAN_POINT('Ctrl Pts',(-0.84629609241444,-6.71606639881895,
90.157291160638));
#205578=CARTESIAN_POINT('Ctrl Pts',(-0.675467926551339,-6.73320370107726,
90.1653282471806));
#205579=CARTESIAN_POINT('Ctrl Pts',(-0.50462341163754,-6.75034264345517,
90.1733661029097));
#205580=CARTESIAN_POINT('Ctrl Pts',(-0.333145862640353,-6.76097292068633,
90.1814039586389));
#205581=CARTESIAN_POINT('Ctrl Pts',(-0.161578941431658,-6.7650706755869,
90.189441814368));
#205582=CARTESIAN_POINT('Ctrl Pts',(0.01003839266516,-6.76916963456375,
90.197482031925));
#205583=CARTESIAN_POINT('Ctrl Pts',(0.181744777936125,-6.76673224159009,
90.2055222494819));
#205584=CARTESIAN_POINT('Ctrl Pts',(0.352997142022572,-6.75778676918145,
90.2135624670388));
#205585=CARTESIAN_POINT('Ctrl Pts',(0.530719530148687,-6.7485033310937,
90.2219064491666));
#205586=CARTESIAN_POINT('Ctrl Pts',(0.707952476140451,-6.73221047264373,
90.2302504312944));
#205587=CARTESIAN_POINT('Ctrl Pts',(0.884096636273593,-6.70899859425606,
90.2385944134221));
#205588=CARTESIAN_POINT('Ctrl Pts',(1.05412371518278,-6.68659281097452,
90.2466486282572));
#205589=CARTESIAN_POINT('Ctrl Pts',(1.22313601107666,-6.65774064209402,
90.2547028430922));
#205590=CARTESIAN_POINT('Ctrl Pts',(1.39060703617396,-6.62257510874309,
90.2627570579273));
#205591=CARTESIAN_POINT('Ctrl Pts',(1.55820338564052,-6.58738325980541,
90.2708173000103));
#205592=CARTESIAN_POINT('Ctrl Pts',(1.72425580781475,-6.54586872928396,
90.2788775420933));
#205593=CARTESIAN_POINT('Ctrl Pts',(1.88825438303719,-6.49821393807105,
90.2869377841763));
#205594=CARTESIAN_POINT('Ctrl Pts',(2.05248223951706,-6.4504925221912,90.2950092950307));
#205595=CARTESIAN_POINT('Ctrl Pts',(2.21465016887878,-6.39661383472942,
90.303080805885));
#205596=CARTESIAN_POINT('Ctrl Pts',(2.37426903535021,-6.33680799360192,
90.3111523167393));
#205597=CARTESIAN_POINT('Ctrl Pts',(2.39099875911102,-6.33053971702871,
90.3119982953502));
#205598=CARTESIAN_POINT('Ctrl Pts',(2.40770050421689,-6.32420637030809,
90.312844273961));
#205599=CARTESIAN_POINT('Ctrl Pts',(2.42437372432497,-6.31780824691623,
90.3136902525719));
#205600=CARTESIAN_POINT('Ctrl Pts',(2.58656233099902,-6.25557055608454,
90.3219195023079));
#205601=CARTESIAN_POINT('Ctrl Pts',(2.74659110609951,-6.1869919234823,90.3301487520439));
#205602=CARTESIAN_POINT('Ctrl Pts',(2.9039284677193,-6.11224087012034,90.3383780017798));
#205603=CARTESIAN_POINT('Ctrl Pts',(3.0610785722831,-6.03757878267239,90.3465974573699));
#205604=CARTESIAN_POINT('Ctrl Pts',(3.21554332089398,-5.95675905463117,
90.3548169129599));
#205605=CARTESIAN_POINT('Ctrl Pts',(3.3668081037196,-5.86999933498532,90.36303636855));
#205606=CARTESIAN_POINT('Ctrl Pts',(3.51792323453601,-5.78332545003357,
90.3712476923197));
#205607=CARTESIAN_POINT('Ctrl Pts',(3.66584439531142,-5.69072345389549,
90.3794590160893));
#205608=CARTESIAN_POINT('Ctrl Pts',(3.81007864031179,-5.59245829261514,
90.387670339859));
#205609=CARTESIAN_POINT('Ctrl Pts',(3.95419914419499,-5.49427062187266,
90.3958751882931));
#205610=CARTESIAN_POINT('Ctrl Pts',(4.09463822819254,-5.3904288820048,90.4040800367272));
#205611=CARTESIAN_POINT('Ctrl Pts',(4.23092909976346,-5.28124303102734,
90.4122848851613));
#205612=CARTESIAN_POINT('Ctrl Pts',(4.36713984786098,-5.17212136886549,
90.4204849100811));
#205613=CARTESIAN_POINT('Ctrl Pts',(4.49920696246336,-5.0576620778637,90.428684935001));
#205614=CARTESIAN_POINT('Ctrl Pts',(4.62669404638303,-4.93821741128961,
90.4368849599209));
#205615=CARTESIAN_POINT('Ctrl Pts',(4.75414423265293,-4.81880731470754,
90.4450826115679));
#205616=CARTESIAN_POINT('Ctrl Pts',(4.87701676449178,-4.69441495859912,
90.4532802632148));
#205617=CARTESIAN_POINT('Ctrl Pts',(4.99490947754159,-4.56543188659793,
90.4614779148617));
#205618=CARTESIAN_POINT('Ctrl Pts',(5.11278640403386,-4.43646608622139,
90.4696744687928));
#205619=CARTESIAN_POINT('Ctrl Pts',(5.2256845972344,-4.30291105840411,90.4778710227239));
#205620=CARTESIAN_POINT('Ctrl Pts',(5.33323982719857,-4.16519410659131,
90.486067576655));
#205621=CARTESIAN_POINT('Ctrl Pts',(5.44080021119289,-4.02747055540326,
90.4942645233637));
#205622=CARTESIAN_POINT('Ctrl Pts',(5.54301690099167,-3.88558496561313,
90.5024614700724));
#205623=CARTESIAN_POINT('Ctrl Pts',(5.63956690012634,-3.73999654799299,
90.5106584167811));
#205624=CARTESIAN_POINT('Ctrl Pts',(5.73613908118205,-3.59437468209926,
90.5188572467008));
#205625=CARTESIAN_POINT('Ctrl Pts',(5.82704178035555,-3.4450485929394,90.5270560766206));
#205626=CARTESIAN_POINT('Ctrl Pts',(5.91199613255347,-3.29250523593705,
90.5352549065403));
#205627=CARTESIAN_POINT('Ctrl Pts',(5.99703094738359,-3.13981740087427,
90.5434615018002));
#205628=CARTESIAN_POINT('Ctrl Pts',(6.07610598455327,-2.98390652384556,
90.55166809706));
#205629=CARTESIAN_POINT('Ctrl Pts',(6.14898861742622,-2.82528369951812,
90.5598746923198));
#205630=CARTESIAN_POINT('Ctrl Pts',(6.22190652591139,-2.66658410083417,
90.5680852596188));
#205631=CARTESIAN_POINT('Ctrl Pts',(6.28862591752067,-2.5051702691891,90.5762958269178));
#205632=CARTESIAN_POINT('Ctrl Pts',(6.34896293916979,-2.34157182188556,
90.5845063942168));
#205633=CARTESIAN_POINT('Ctrl Pts',(6.40938317420954,-2.17774774890267,
90.5927282850635));
#205634=CARTESIAN_POINT('Ctrl Pts',(6.46340333699398,-2.01173338019453,
90.6009501759102));
#205635=CARTESIAN_POINT('Ctrl Pts',(6.5108895817058,-1.84407316959898,90.6091720667569));
#205636=CARTESIAN_POINT('Ctrl Pts',(6.55406578495451,-1.69163047017469,
90.6166477059118));
#205637=CARTESIAN_POINT('Ctrl Pts',(6.59184092278741,-1.53782748310096,
90.6241233450666));
#205638=CARTESIAN_POINT('Ctrl Pts',(6.62415141723914,-1.38307881246466,
90.6315989842215));
#205639=CARTESIAN_POINT('Ctrl Pts',(6.66277349961948,-1.19810126857434,
90.6405349276722));
#205640=CARTESIAN_POINT('Ctrl Pts',(6.69366778144579,-1.01138724800797,
90.649470871123));
#205641=CARTESIAN_POINT('Ctrl Pts',(6.71669652522179,-0.823575611631092,
90.6584068145737));
#205642=CARTESIAN_POINT('Ctrl Pts',(6.73969065068789,-0.636046305957762,
90.6673293249313));
#205643=CARTESIAN_POINT('Ctrl Pts',(6.75484279967089,-0.447422932502711,
90.6762518352889));
#205644=CARTESIAN_POINT('Ctrl Pts',(6.76206644467396,-0.258353242314716,
90.6851743456465));
#205645=CARTESIAN_POINT('Ctrl Pts',(6.76927238950509,-0.0697468315408935,
90.6940749930848));
#205646=CARTESIAN_POINT('Ctrl Pts',(6.76858859394774,0.119303455756674,
90.7029756405231));
#205647=CARTESIAN_POINT('Ctrl Pts',(6.75998037107751,0.308146690144195,
90.7118762879614));
#205648=CARTESIAN_POINT('Ctrl Pts',(6.75138545115332,0.496698090619526,
90.7207631805476));
#205649=CARTESIAN_POINT('Ctrl Pts',(6.73489054362257,0.685042819801436,
90.7296500731339));
#205650=CARTESIAN_POINT('Ctrl Pts',(6.7105128222379,0.872528889252838,90.7385369657201));
#205651=CARTESIAN_POINT('Ctrl Pts',(6.68619776069702,1.05953304952001,90.747401015675));
#205652=CARTESIAN_POINT('Ctrl Pts',(6.65404034946211,1.24568269884231,90.7562650656299));
#205653=CARTESIAN_POINT('Ctrl Pts',(6.61410939888276,1.43033068190916,90.7651291155848));
#205654=CARTESIAN_POINT('Ctrl Pts',(6.5759321979058,1.60686900762538,90.7736038604053));
#205655=CARTESIAN_POINT('Ctrl Pts',(6.53064961384517,1.78203447442935,90.7820786052257));
#205656=CARTESIAN_POINT('Ctrl Pts',(6.47836623906234,1.95526465537975,90.7905533500462));
#205657=CARTESIAN_POINT('Ctrl Pts',(6.42772285583972,2.12306106247923,90.7987622644753));
#205658=CARTESIAN_POINT('Ctrl Pts',(6.37055887359042,2.28887966137623,90.8069711789044));
#205659=CARTESIAN_POINT('Ctrl Pts',(6.3070641999167,2.45218885449901,90.8151800933335));
#205660=CARTESIAN_POINT('Ctrl Pts',(6.24355443070684,2.6155368735529,90.8233909593904));
#205661=CARTESIAN_POINT('Ctrl Pts',(6.17371110054856,2.77637396635425,90.8316018254472));
#205662=CARTESIAN_POINT('Ctrl Pts',(6.09777225654522,2.93418856028501,90.839812691504));
#205663=CARTESIAN_POINT('Ctrl Pts',(6.02180182205004,3.09206880494707,90.8480269732738));
#205664=CARTESIAN_POINT('Ctrl Pts',(5.93973097627568,3.24692372521614,90.8562412550436));
#205665=CARTESIAN_POINT('Ctrl Pts',(5.85184373025022,3.39826631633414,90.8644555368135));
#205666=CARTESIAN_POINT('Ctrl Pts',(5.76385756019135,3.54977925548576,90.8726790644059));
#205667=CARTESIAN_POINT('Ctrl Pts',(5.67004209261495,3.69777166119129,90.8809025919983));
#205668=CARTESIAN_POINT('Ctrl Pts',(5.5707252204531,3.84178467879289,90.8891261195907));
#205669=CARTESIAN_POINT('Ctrl Pts',(5.4713446900399,3.98589000313626,90.8973549181444));
#205670=CARTESIAN_POINT('Ctrl Pts',(5.36645593864416,4.1260105705275,90.905583716698));
#205671=CARTESIAN_POINT('Ctrl Pts',(5.25642711667533,4.26172065803007,90.9138125152517));
#205672=CARTESIAN_POINT('Ctrl Pts',(5.14624684883752,4.39761753960863,90.9220526400881));
#205673=CARTESIAN_POINT('Ctrl Pts',(5.03091261310206,4.52909154878991,90.9302927649246));
#205674=CARTESIAN_POINT('Ctrl Pts',(4.91083005091975,4.65575313037359,90.938532889761));
#205675=CARTESIAN_POINT('Ctrl Pts',(4.85751834893465,4.71198564546683,90.942191165131));
#205676=CARTESIAN_POINT('Ctrl Pts',(4.80327120491539,4.76727015589958,90.945849440501));
#205677=CARTESIAN_POINT('Ctrl Pts',(4.74812616705041,4.82157514737365,90.949507715871));
#205678=CARTESIAN_POINT('Ctrl Pts',(4.6207926986536,4.94696889417971,90.957954910927));
#205679=CARTESIAN_POINT('Ctrl Pts',(4.48837834219849,5.0674242804353,90.9664021059829));
#205680=CARTESIAN_POINT('Ctrl Pts',(4.35129296385923,5.18252241120762,90.9748493010389));
#205681=CARTESIAN_POINT('Ctrl Pts',(4.21431818108728,5.29752768493548,90.9832896812008));
#205682=CARTESIAN_POINT('Ctrl Pts',(4.07268013894871,5.40718410131449,90.9917300613627));
#205683=CARTESIAN_POINT('Ctrl Pts',(3.9268248019547,5.51111023068433,91.0001704415246));
#205684=CARTESIAN_POINT('Ctrl Pts',(3.78109282050226,5.6149484656772,91.0086036833281));
#205685=CARTESIAN_POINT('Ctrl Pts',(3.63115092728356,5.71306588493759,91.0170369251317));
#205686=CARTESIAN_POINT('Ctrl Pts',(3.47747738834778,5.80512187757759,91.0254701669352));
#205687=CARTESIAN_POINT('Ctrl Pts',(3.3536864243144,5.87927713002294,91.0322635234234));
#205688=CARTESIAN_POINT('Ctrl Pts',(3.22747467812902,5.94949982342603,91.0390568799115));
#205689=CARTESIAN_POINT('Ctrl Pts',(3.09910619832119,6.01563211736948,91.0458502363996));
#205690=CARTESIAN_POINT('Ctrl Pts',(3.09910619832144,6.01563211736935,89.0458803684832));
#205691=CARTESIAN_POINT('Ctrl Pts',(2.94574414940646,6.09464048541888,89.0540188657321));
#205692=CARTESIAN_POINT('Ctrl Pts',(2.7891686254625,6.16787827641324,89.062157362981));
#205693=CARTESIAN_POINT('Ctrl Pts',(2.62985788981656,6.23507309334619,89.0702958602299));
#205694=CARTESIAN_POINT('Ctrl Pts',(2.47068172296856,6.30221115123082,89.0784274829403));
#205695=CARTESIAN_POINT('Ctrl Pts',(2.30877527871085,6.36331625436805,89.0865591056507));
#205696=CARTESIAN_POINT('Ctrl Pts',(2.14464122207223,6.41816196652816,89.094690728361));
#205697=CARTESIAN_POINT('Ctrl Pts',(1.98061446992856,6.47297182268394,89.1028170349311));
#205698=CARTESIAN_POINT('Ctrl Pts',(1.8143633510293,6.52153031983798,89.1109433415012));
#205699=CARTESIAN_POINT('Ctrl Pts',(1.64641026628949,6.56365921076472,89.1190696480713));
#205700=CARTESIAN_POINT('Ctrl Pts',(1.47853167663572,6.60576941554849,89.1271923502426));
#205701=CARTESIAN_POINT('Ctrl Pts',(1.30895297895508,6.64145560418459,89.1353150524138));
#205702=CARTESIAN_POINT('Ctrl Pts',(1.13821147157311,6.67058945266304,89.143437754585));
#205703=CARTESIAN_POINT('Ctrl Pts',(0.967513373666449,6.6997158941255,89.1515583916331));
#205704=CARTESIAN_POINT('Ctrl Pts',(0.795653415853312,6.72229325329825,
89.1596790286812));
#205705=CARTESIAN_POINT('Ctrl Pts',(0.623178770462661,6.73824437224153,
89.1677996657292));
#205706=CARTESIAN_POINT('Ctrl Pts',(0.450693819226889,6.75419644430903,
89.1759207880082));
#205707=CARTESIAN_POINT('Ctrl Pts',(0.277594471498387,6.76352144946732,
89.1840419102872));
#205708=CARTESIAN_POINT('Ctrl Pts',(0.104432856585541,6.76619411327117,
89.1921630325662));
#205709=CARTESIAN_POINT('Ctrl Pts',(0.0415555946075978,6.76716459268289,
89.195111918977));
#205710=CARTESIAN_POINT('Ctrl Pts',(-0.0213298580456094,6.76725845031424,
89.1980608053878));
#205711=CARTESIAN_POINT('Ctrl Pts',(-0.0841970533259905,6.76647617717015,
89.2010096917986));
#205712=CARTESIAN_POINT('Ctrl Pts',(-0.27573595059093,6.76409280799471,
89.2099941303244));
#205713=CARTESIAN_POINT('Ctrl Pts',(-0.467010343119068,6.75357432232411,
89.2189785688502));
#205714=CARTESIAN_POINT('Ctrl Pts',(-0.657353833176219,6.7349962834443,
89.227963007376));
#205715=CARTESIAN_POINT('Ctrl Pts',(-0.848025844737191,6.71638617997815,
89.2369629525065));
#205716=CARTESIAN_POINT('Ctrl Pts',(-1.03776350463907,6.68968874356541,
89.245962897637));
#205717=CARTESIAN_POINT('Ctrl Pts',(-1.22590818518116,6.65503103835781,
89.2549628427675));
#205718=CARTESIAN_POINT('Ctrl Pts',(-1.41449623349204,6.62029166137833,
89.2639839964997));
#205719=CARTESIAN_POINT('Ctrl Pts',(-1.6014835555457,6.57755452620292,89.2730051502319));
#205720=CARTESIAN_POINT('Ctrl Pts',(-1.78622161222539,6.5269978820296,89.2820263039641));
#205721=CARTESIAN_POINT('Ctrl Pts',(-1.97114764133391,6.47638979607234,
89.2910566367913));
#205722=CARTESIAN_POINT('Ctrl Pts',(-2.15381960422244,6.41794637496796,
89.3000869696185));
#205723=CARTESIAN_POINT('Ctrl Pts',(-2.33360513622278,6.35189547050286,
89.3091173024458));
#205724=CARTESIAN_POINT('Ctrl Pts',(-2.5136455474358,6.28575092667567,89.3181604374384));
#205725=CARTESIAN_POINT('Ctrl Pts',(-2.69079112119019,6.21197741704217,
89.327203572431));
#205726=CARTESIAN_POINT('Ctrl Pts',(-2.86442828932985,6.13085145597958,
89.3362467074237));
#205727=CARTESIAN_POINT('Ctrl Pts',(-3.01622717794516,6.05992867568379,
89.3441524908236));
#205728=CARTESIAN_POINT('Ctrl Pts',(-3.16534490603844,5.98338734153934,
89.3520582742235));
#205729=CARTESIAN_POINT('Ctrl Pts',(-3.31138686120792,5.90144101516058,
89.3599640576234));
#205730=CARTESIAN_POINT('Ctrl Pts',(-3.47123917081076,5.81174549225478,
89.3686174458516));
#205731=CARTESIAN_POINT('Ctrl Pts',(-3.6275470699987,5.71549403260485,89.3772708340798));
#205732=CARTESIAN_POINT('Ctrl Pts',(-3.77977306256917,5.61298535500285,
89.3859242223081));
#205733=CARTESIAN_POINT('Ctrl Pts',(-3.93185846363741,5.51057135143603,
89.3945696185184));
#205734=CARTESIAN_POINT('Ctrl Pts',(-4.07986922599621,5.40191182545246,
89.4032150147288));
#205735=CARTESIAN_POINT('Ctrl Pts',(-4.22329472397144,5.28735006165423,
89.4118604109392));
#205736=CARTESIAN_POINT('Ctrl Pts',(-4.37130074920802,5.16912958103372,
89.4207819119816));
#205737=CARTESIAN_POINT('Ctrl Pts',(-4.51442349841515,5.04462377878463,
89.4297034130241));
#205738=CARTESIAN_POINT('Ctrl Pts',(-4.65213466616417,4.91425803635438,
89.4386249140665));
#205739=CARTESIAN_POINT('Ctrl Pts',(-4.78532974938659,4.78816749340004,
89.4472538444085));
#205740=CARTESIAN_POINT('Ctrl Pts',(-4.91346229956792,4.65659547223805,
89.4558827747504));
#205741=CARTESIAN_POINT('Ctrl Pts',(-5.03608783609214,4.51996773297828,
89.4645117050923));
#205742=CARTESIAN_POINT('Ctrl Pts',(-5.16494994615941,4.37639128655632,
89.473579491485));
#205743=CARTESIAN_POINT('Ctrl Pts',(-5.28773002020762,4.22723167850583,
89.4826472778776));
#205744=CARTESIAN_POINT('Ctrl Pts',(-5.40395577284719,4.07302725317564,
89.4917150642702));
#205745=CARTESIAN_POINT('Ctrl Pts',(-5.52018152548685,3.91882282784535,
89.5007828506629));
#205746=CARTESIAN_POINT('Ctrl Pts',(-5.62985269355601,3.75957387589938,
89.5098506370555));
#205747=CARTESIAN_POINT('Ctrl Pts',(-5.7325456686147,3.59586000245377,89.5189184234482));
#205748=CARTESIAN_POINT('Ctrl Pts',(-5.82795857013114,3.44375207418494,
89.5273433795813));
#205749=CARTESIAN_POINT('Ctrl Pts',(-5.91730593764035,3.28785670772003,
89.5357683357145));
#205750=CARTESIAN_POINT('Ctrl Pts',(-6.00029950281174,3.12868900285043,
89.5441932918476));
#205751=CARTESIAN_POINT('Ctrl Pts',(-6.08331233158658,2.96948435362806,
89.552620203494));
#205752=CARTESIAN_POINT('Ctrl Pts',(-6.1599682642167,2.80700614562378,89.5610471151404));
#205753=CARTESIAN_POINT('Ctrl Pts',(-6.23002569731353,2.64179272669396,
89.5694740267868));
#205754=CARTESIAN_POINT('Ctrl Pts',(-6.3001088932571,2.47651855235525,89.5779040373368));
#205755=CARTESIAN_POINT('Ctrl Pts',(-6.36358862201089,2.30850746667938,
89.5863340478868));
#205756=CARTESIAN_POINT('Ctrl Pts',(-6.42027184426169,2.13831673186659,
89.5947640584368));
#205757=CARTESIAN_POINT('Ctrl Pts',(-6.47700728191154,1.96796922090771,
89.6032018345362));
#205758=CARTESIAN_POINT('Ctrl Pts',(-6.52693359967498,1.79543836414719,
89.6116396106356));
#205759=CARTESIAN_POINT('Ctrl Pts',(-6.569907643377,1.62129656679353,89.6200773867351));
#205760=CARTESIAN_POINT('Ctrl Pts',(-6.61290424528407,1.4470633578334,89.628519592045));
#205761=CARTESIAN_POINT('Ctrl Pts',(-6.64894122299971,1.27121784521705,
89.6369617973549));
#205762=CARTESIAN_POINT('Ctrl Pts',(-6.67792665757091,1.09434206539997,
89.6454040026647));
#205763=CARTESIAN_POINT('Ctrl Pts',(-6.70694267018077,0.917279691367016,
89.6538551140367));
#205764=CARTESIAN_POINT('Ctrl Pts',(-6.72889223375355,0.739185207131805,
89.6623062254088));
#205765=CARTESIAN_POINT('Ctrl Pts',(-6.7437352225717,0.56064627693926,89.6707573367808));
#205766=CARTESIAN_POINT('Ctrl Pts',(-6.74790093037528,0.510539049624142,
89.6731291542781));
#205767=CARTESIAN_POINT('Ctrl Pts',(-6.75150720210199,0.460396821494576,
89.6755009717754));
#205768=CARTESIAN_POINT('Ctrl Pts',(-6.7545538882394,0.410232581434043,
89.6778727892727));
#205769=CARTESIAN_POINT('Ctrl Pts',(-6.76282073461048,0.274117455950735,
89.6843084541184));
#205770=CARTESIAN_POINT('Ctrl Pts',(-6.76697248697646,0.137764909183088,
89.6907441189641));
#205771=CARTESIAN_POINT('Ctrl Pts',(-6.76699986371201,0.00135813167870539,
89.6971797838098));
#205772=CARTESIAN_POINT('',(-6.76699948056331,-0.00136021873801901,89.3028202161898));
#205773=CARTESIAN_POINT('Ctrl Pts',(3.09910619832125,6.01563211736945,88.6513956954041));
#205774=CARTESIAN_POINT('Ctrl Pts',(2.93375330764816,6.10081787314658,88.6601451433064));
#205775=CARTESIAN_POINT('Ctrl Pts',(2.7648862784306,6.17918207037044,88.6688945912087));
#205776=CARTESIAN_POINT('Ctrl Pts',(2.59307866646691,6.25045854554002,88.677644039111));
#205777=CARTESIAN_POINT('Ctrl Pts',(2.4212724418536,6.32173444515044,88.6863934163613));
#205778=CARTESIAN_POINT('Ctrl Pts',(2.24652594672442,6.38592262741846,88.6951427936116));
#205779=CARTESIAN_POINT('Ctrl Pts',(2.06943269687093,6.44280508110571,88.7038921708619));
#205780=CARTESIAN_POINT('Ctrl Pts',(1.89234081822049,6.49968709436174,88.7126414803672));
#205781=CARTESIAN_POINT('Ctrl Pts',(1.7129024940556,6.54926340459552,88.7213907898726));
#205782=CARTESIAN_POINT('Ctrl Pts',(1.5317271662503,6.5913656315039,88.730140099378));
#205783=CARTESIAN_POINT('Ctrl Pts',(1.3505531810731,6.63346754640715,88.7388893440452));
#205784=CARTESIAN_POINT('Ctrl Pts',(1.167642497144,6.66809542395779,88.7476385887124));
#205785=CARTESIAN_POINT('Ctrl Pts',(0.983616340614198,6.6951316562467,88.7563878333797));
#205786=CARTESIAN_POINT('Ctrl Pts',(0.799591486713808,6.72216769715961,
88.7651370161154));
#205787=CARTESIAN_POINT('Ctrl Pts',(0.614451459526804,6.7416121586937,88.773886198851));
#205788=CARTESIAN_POINT('Ctrl Pts',(0.4288250479105,6.75339900185711,88.7826353815867));
#205789=CARTESIAN_POINT('Ctrl Pts',(0.243199888597169,6.76518576550221,
88.7913845052973));
#205790=CARTESIAN_POINT('Ctrl Pts',(0.0570886373919456,6.76931499599834,
88.8001336290078));
#205791=CARTESIAN_POINT('Ctrl Pts',(-0.128876626811216,6.76577266947847,
88.8088827527183));
#205792=CARTESIAN_POINT('Ctrl Pts',(-0.314840698188169,6.76223036567993,
88.8176318203099));
#205793=CARTESIAN_POINT('Ctrl Pts',(-0.500658497951208,6.75101660879223,
88.8263808879014));
#205794=CARTESIAN_POINT('Ctrl Pts',(-0.685698951926118,6.73216948296219,
88.835129955493));
#205795=CARTESIAN_POINT('Ctrl Pts',(-0.870738280460047,6.71332247176291,
88.8438789698715));
#205796=CARTESIAN_POINT('Ctrl Pts',(-1.05499998761299,6.6868422135618,88.85262798425));
#205797=CARTESIAN_POINT('Ctrl Pts',(-1.23785829161497,6.65281863948508,
88.8613769986286));
#205798=CARTESIAN_POINT('Ctrl Pts',(-1.43007412917477,6.61705395368845,
88.8705737323278));
#205799=CARTESIAN_POINT('Ctrl Pts',(-1.62073882535861,6.57295372727773,
88.879770466027));
#205800=CARTESIAN_POINT('Ctrl Pts',(-1.80913696091579,6.52068343478261,
88.8889671997262));
#205801=CARTESIAN_POINT('Ctrl Pts',(-1.98838356186177,6.47095219815179,
88.8977171974399));
#205802=CARTESIAN_POINT('Ctrl Pts',(-2.16557827572598,6.41382586850869,
88.9064671951535));
#205803=CARTESIAN_POINT('Ctrl Pts',(-2.34011918621764,6.34949849943254,
88.9152171928672));
#205804=CARTESIAN_POINT('Ctrl Pts',(-2.51465655691168,6.28517243495523,
88.9239670131255));
#205805=CARTESIAN_POINT('Ctrl Pts',(-2.68653996295402,6.21364572242343,
88.9327168333838));
#205806=CARTESIAN_POINT('Ctrl Pts',(-2.85518555380067,6.13516132252184,
88.9414666536421));
#205807=CARTESIAN_POINT('Ctrl Pts',(-3.02382794858768,6.05667841000467,
88.9502163080796));
#205808=CARTESIAN_POINT('Ctrl Pts',(-3.18923239109361,5.97123819492038,
88.9589659625171));
#205809=CARTESIAN_POINT('Ctrl Pts',(-3.35083705967778,5.87913088810667,
88.9677156169546));
#205810=CARTESIAN_POINT('Ctrl Pts',(-3.51243888042463,5.78702520443064,
88.9764651172036));
#205811=CARTESIAN_POINT('Ctrl Pts',(-3.67024081223738,5.68825280605752,
88.9852146174525));
#205812=CARTESIAN_POINT('Ctrl Pts',(-3.82370687544434,5.58314917682482,
88.9939641177014));
#205813=CARTESIAN_POINT('Ctrl Pts',(-3.97717043817854,5.47804726007993,
89.0027134753919));
#205814=CARTESIAN_POINT('Ctrl Pts',(-4.12629803722506,5.36661448084201,
89.0114628330824));
#205815=CARTESIAN_POINT('Ctrl Pts',(-4.27058317206959,5.24922931204535,
89.0202121907728));
#205816=CARTESIAN_POINT('Ctrl Pts',(-4.41486614774869,5.13184589986761,
89.0289614175329));
#205817=CARTESIAN_POINT('Ctrl Pts',(-4.55430658194432,5.00851045723017,
89.037710644293));
#205818=CARTESIAN_POINT('Ctrl Pts',(-4.68843089001849,4.87964187103116,
89.046459871053));
#205819=CARTESIAN_POINT('Ctrl Pts',(-4.82255336917847,4.7507750420795,89.055208978509));
#205820=CARTESIAN_POINT('Ctrl Pts',(-4.95135966065152,4.61637541908075,
89.0639580859649));
#205821=CARTESIAN_POINT('Ctrl Pts',(-5.07441230869268,4.47689945401818,
89.0727071934208));
#205822=CARTESIAN_POINT('Ctrl Pts',(-5.19746344226446,4.33742520555481,
89.0814561931972));
#205823=CARTESIAN_POINT('Ctrl Pts',(-5.31476088454801,4.19287495491294,
89.0902051929736));
#205824=CARTESIAN_POINT('Ctrl Pts',(-5.42590627628892,4.04373961586655,
89.0989541927499));
#205825=CARTESIAN_POINT('Ctrl Pts',(-5.53706380672706,3.8945879890668,89.1077041480446));
#205826=CARTESIAN_POINT('Ctrl Pts',(-5.64206777071902,3.74085050155226,
89.1164541033393));
#205827=CARTESIAN_POINT('Ctrl Pts',(-5.74056148164046,3.583049382231,89.125204058634));
#205828=CARTESIAN_POINT('Ctrl Pts',(-5.83905138951924,3.42525435593214,
89.1339536760752));
#205829=CARTESIAN_POINT('Ctrl Pts',(-5.93103139557694,3.26339625497108,
89.1427032935163));
#205830=CARTESIAN_POINT('Ctrl Pts',(-6.01618907820889,3.09802485064922,
89.1514529109574));
#205831=CARTESIAN_POINT('Ctrl Pts',(-6.10134392545018,2.93265895249567,
89.1602022370732));
#205832=CARTESIAN_POINT('Ctrl Pts',(-6.1796767726186,2.76378023985972,89.1689515631891));
#205833=CARTESIAN_POINT('Ctrl Pts',(-6.25092157009246,2.59196229227063,
89.177700889305));
#205834=CARTESIAN_POINT('Ctrl Pts',(-6.32216437407776,2.42014915229033,
89.1864499706074));
#205835=CARTESIAN_POINT('Ctrl Pts',(-6.38631941548944,2.24539720662787,
89.1951990519099));
#205836=CARTESIAN_POINT('Ctrl Pts',(-6.4431688103756,2.06829994947617,89.2039481332123));
#205837=CARTESIAN_POINT('Ctrl Pts',(-6.5000233452459,1.89118668024385,89.2126980055547));
#205838=CARTESIAN_POINT('Ctrl Pts',(-6.54957082411112,1.71172794807643,
89.221447877897));
#205839=CARTESIAN_POINT('Ctrl Pts',(-6.59164294296096,1.53053334250286,
89.2301977502394));
#205840=CARTESIAN_POINT('Ctrl Pts',(-6.63371214082145,1.34935131693543,
89.2389470150943));
#205841=CARTESIAN_POINT('Ctrl Pts',(-6.668306952397,1.16643393829706,89.2476962799492));
#205842=CARTESIAN_POINT('Ctrl Pts',(-6.69530988153997,0.982402458340396,
89.2564455448041));
#205843=CARTESIAN_POINT('Ctrl Pts',(-6.7223141969049,0.798361530946474,
89.2651952588111));
#205844=CARTESIAN_POINT('Ctrl Pts',(-6.74172580829283,0.613206671361901,
89.2739449728181));
#205845=CARTESIAN_POINT('Ctrl Pts',(-6.75347878028183,0.427566795112832,
89.2826946868252));
#205846=CARTESIAN_POINT('Ctrl Pts',(-6.76248992368212,0.285234494205639,
89.2894031966134));
#205847=CARTESIAN_POINT('Ctrl Pts',(-6.76699999999992,0.142617266093434,
89.2961117064016));
#205848=CARTESIAN_POINT('Ctrl Pts',(-6.767,3.67735927903396E-12,89.3028202161898));
#205849=CARTESIAN_POINT('Ctrl Pts',(-6.76699802633313,-0.00516832696203806,
89.3028202161898));
#205850=CARTESIAN_POINT('Ctrl Pts',(-6.76684902442674,-0.20025962320532,
89.311976675311));
#205851=CARTESIAN_POINT('Ctrl Pts',(-6.75825935055282,-0.395062537055501,
89.3211331344321));
#205852=CARTESIAN_POINT('Ctrl Pts',(-6.74132778610909,-0.588887663509377,
89.3302895935532));
#205853=CARTESIAN_POINT('Ctrl Pts',(-6.72431072437874,-0.78369152541593,
89.3394922889458));
#205854=CARTESIAN_POINT('Ctrl Pts',(-6.69886739001077,-0.977507505031502,
89.3486949843384));
#205855=CARTESIAN_POINT('Ctrl Pts',(-6.66514850928785,-1.16965137931693,
89.357897679731));
#205856=CARTESIAN_POINT('Ctrl Pts',(-6.6324927612709,-1.35573709174684,
89.3668102205798));
#205857=CARTESIAN_POINT('Ctrl Pts',(-6.59207542885528,-1.54025441184314,
89.3757227614285));
#205858=CARTESIAN_POINT('Ctrl Pts',(-6.54407704261772,-1.72259822950209,
89.3846353022773));
#205859=CARTESIAN_POINT('Ctrl Pts',(-6.49858031319104,-1.89543835986806,
89.3930833250398));
#205860=CARTESIAN_POINT('Ctrl Pts',(-6.44619239626076,-2.06662499248261,
89.4015313478023));
#205861=CARTESIAN_POINT('Ctrl Pts',(-6.38705197200869,-2.23558853702105,
89.4099793705649));
#205862=CARTESIAN_POINT('Ctrl Pts',(-6.32796570440939,-2.40439735659551,
89.4184196572206));
#205863=CARTESIAN_POINT('Ctrl Pts',(-6.26213936463124,-2.57098683266773,
89.4268599438764));
#205864=CARTESIAN_POINT('Ctrl Pts',(-6.1897617529613,-2.73480135322066,
89.4353002305322));
#205865=CARTESIAN_POINT('Ctrl Pts',(-6.1174392775055,-2.89849108224927,
89.4437340875001));
#205866=CARTESIAN_POINT('Ctrl Pts',(-6.0385756133742,-3.0594097658754,89.452167944468));
#205867=CARTESIAN_POINT('Ctrl Pts',(-5.9534082322147,-3.21702027046742,
89.4606018014359));
#205868=CARTESIAN_POINT('Ctrl Pts',(-5.86829263724442,-3.37453493969028,
89.4690305301809));
#205869=CARTESIAN_POINT('Ctrl Pts',(-5.77688112535556,-3.5287451476719,
89.4774592589259));
#205870=CARTESIAN_POINT('Ctrl Pts',(-5.67945798257234,-3.67913658678165,
89.485887987671));
#205871=CARTESIAN_POINT('Ctrl Pts',(-5.58207911753852,-3.82945967463254,
89.4943128856513));
#205872=CARTESIAN_POINT('Ctrl Pts',(-5.47869425069848,-3.97596717494488,
89.5027377836316));
#205873=CARTESIAN_POINT('Ctrl Pts',(-5.369632233226,-4.11817176425417,89.5111626816119));
#205874=CARTESIAN_POINT('Ctrl Pts',(-5.26059436226174,-4.26034486923589,
89.519585714306));
#205875=CARTESIAN_POINT('Ctrl Pts',(-5.14588204741826,-4.3982166966584,
89.5280087470002));
#205876=CARTESIAN_POINT('Ctrl Pts',(-5.02586617310408,-4.53133073280336,
89.5364317796943));
#205877=CARTESIAN_POINT('Ctrl Pts',(-4.90586387844969,-4.66442970724639,
89.5448538593319));
#205878=CARTESIAN_POINT('Ctrl Pts',(-4.78055944389228,-4.79277171599418,
89.5532759389695));
#205879=CARTESIAN_POINT('Ctrl Pts',(-4.65036277948422,-4.91593480623857,
89.5616980186071));
#205880=CARTESIAN_POINT('Ctrl Pts',(-4.5201626721991,-5.03910115336652,
89.5701203209553));
#205881=CARTESIAN_POINT('Ctrl Pts',(-4.38507031965246,-5.15708808006154,
89.5785426233036));
#205882=CARTESIAN_POINT('Ctrl Pts',(-4.24553134830853,-5.26951160645174,
89.5869649256518));
#205883=CARTESIAN_POINT('Ctrl Pts',(-4.10596920731208,-5.38195380012905,
89.5953886264755));
#205884=CARTESIAN_POINT('Ctrl Pts',(-3.9619592355185,-5.48883054305774,
89.6038123272991));
#205885=CARTESIAN_POINT('Ctrl Pts',(-3.81397916368428,-5.58979891758033,
89.6122360281228));
#205886=CARTESIAN_POINT('Ctrl Pts',(-3.6658989523829,-5.69083561832481,
89.6206654293418));
#205887=CARTESIAN_POINT('Ctrl Pts',(-3.51384354830047,-5.78595577306,89.6290948305607));
#205888=CARTESIAN_POINT('Ctrl Pts',(-3.35831947105741,-5.87485994133619,
89.6375242317797));
#205889=CARTESIAN_POINT('Ctrl Pts',(-3.20273990303963,-5.96379583049613,
89.6459566405973));
#205890=CARTESIAN_POINT('Ctrl Pts',(-3.04368948665119,-6.04651115076413,
89.654389049415));
#205891=CARTESIAN_POINT('Ctrl Pts',(-2.88169873408829,-6.12275276374557,
89.6628214582326));
#205892=CARTESIAN_POINT('Ctrl Pts',(-2.7195581029678,-6.19906491768568,
89.6712616689602));
#205893=CARTESIAN_POINT('Ctrl Pts',(-2.55447200463676,-6.26889126054263,
89.6797018796879));
#205894=CARTESIAN_POINT('Ctrl Pts',(-2.38699131364464,-6.33202664781072,
89.6881420904155));
#205895=CARTESIAN_POINT('Ctrl Pts',(-2.29173115451881,-6.36793697873903,
89.6929427382526));
#205896=CARTESIAN_POINT('Ctrl Pts',(-2.19569663012468,-6.40168359059077,
89.6977433860897));
#205897=CARTESIAN_POINT('Ctrl Pts',(-2.09899123165856,-6.43323595163589,
89.7025440339268));
#205898=CARTESIAN_POINT('Ctrl Pts',(-1.93502286481216,-6.48673440356076,
89.7106837489597));
#205899=CARTESIAN_POINT('Ctrl Pts',(-1.76879808507651,-6.534028424973,89.7188234639926));
#205900=CARTESIAN_POINT('Ctrl Pts',(-1.60083180762972,-6.57492406980347,
89.7269631790255));
#205901=CARTESIAN_POINT('Ctrl Pts',(-1.43301243248145,-6.61578394754832,
89.7350957751124));
#205902=CARTESIAN_POINT('Ctrl Pts',(-1.26345494472767,-6.65025650143955,
89.7432283711994));
#205903=CARTESIAN_POINT('Ctrl Pts',(-1.09269118493701,-6.67819698529184,
89.7513609672863));
#205904=CARTESIAN_POINT('Ctrl Pts',(-0.922044168413402,-6.70611836753046,
89.7594880034943));
#205905=CARTESIAN_POINT('Ctrl Pts',(-0.75019288165403,-6.72751651176724,
89.7676150397023));
#205906=CARTESIAN_POINT('Ctrl Pts',(-0.577681135053577,-6.74229734632071,
89.7757420759102));
#205907=CARTESIAN_POINT('Ctrl Pts',(-0.40525185219047,-6.75707111536772,
89.7838652272478));
#205908=CARTESIAN_POINT('Ctrl Pts',(-0.232163102268462,-6.76523384249223,
89.7919883785854));
#205909=CARTESIAN_POINT('Ctrl Pts',(-0.0589656085607672,-6.76674309080868,
89.8001115299229));
#205910=CARTESIAN_POINT('Ctrl Pts',(0.11418321536401,-6.76825191501514,
89.8082323985946));
#205911=CARTESIAN_POINT('Ctrl Pts',(0.287440356326177,-6.76311098204415,
89.8163532672663));
#205912=CARTESIAN_POINT('Ctrl Pts',(0.460253321125572,-6.75132993419762,
89.8244741359379));
#205913=CARTESIAN_POINT('Ctrl Pts',(0.633075625399209,-6.73954824965817,
89.8325954434925));
#205914=CARTESIAN_POINT('Ctrl Pts',(0.805453339905235,-6.72112575425677,
89.840716751047));
#205915=CARTESIAN_POINT('Ctrl Pts',(0.976837135832493,-6.69612411847769,
89.8488380586015));
#205916=CARTESIAN_POINT('Ctrl Pts',(1.06589411380776,-6.68313239942469,
89.8530581723182));
#205917=CARTESIAN_POINT('Ctrl Pts',(1.1546828009662,-6.66836503221109,89.8572782860349));
#205918=CARTESIAN_POINT('Ctrl Pts',(1.24312696509458,-6.65183616369606,
89.8614983997516));
#205919=CARTESIAN_POINT('Ctrl Pts',(1.43142074315825,-6.61664692164167,
89.8704828382773));
#205920=CARTESIAN_POINT('Ctrl Pts',(1.6180590903051,-6.57348838654307,89.8794672768031));
#205921=CARTESIAN_POINT('Ctrl Pts',(1.80239843341973,-6.52254926291907,
89.8884517153289));
#205922=CARTESIAN_POINT('Ctrl Pts',(1.98705593523852,-6.47152222140794,
89.8974516604593));
#205923=CARTESIAN_POINT('Ctrl Pts',(2.16940627181495,-6.41268781441574,
89.9064516055897));
#205924=CARTESIAN_POINT('Ctrl Pts',(2.3488223553158,-6.34628415241303,89.9154515507202));
#205925=CARTESIAN_POINT('Ctrl Pts',(2.52866123742258,-6.27972400847639,
89.9244727044523));
#205926=CARTESIAN_POINT('Ctrl Pts',(2.70555180636407,-6.20555900358184,
89.9334938581845));
#205927=CARTESIAN_POINT('Ctrl Pts',(2.8788856896544,-6.12407594547154,89.9425150119166));
#205928=CARTESIAN_POINT('Ctrl Pts',(3.05239594153723,-6.04250997770734,
89.9515453447438));
#205929=CARTESIAN_POINT('Ctrl Pts',(3.22234206447384,-5.9536111880958,89.960575677571));
#205930=CARTESIAN_POINT('Ctrl Pts',(3.38814012573824,-5.85771247914768,
89.9696060103982));
#205931=CARTESIAN_POINT('Ctrl Pts',(3.55417323639093,-5.76167781605931,
89.9786491453908));
#205932=CARTESIAN_POINT('Ctrl Pts',(3.71604631992265,-5.65862351070531,
89.9876922803834));
#205933=CARTESIAN_POINT('Ctrl Pts',(3.87320230542965,-5.54892718471007,
89.996735415376));
#205934=CARTESIAN_POINT('Ctrl Pts',(4.01059284338607,-5.45302732323355,
90.004641198776));
#205935=CARTESIAN_POINT('Ctrl Pts',(4.14437857112505,-5.352051822645,90.0125469821761));
#205936=CARTESIAN_POINT('Ctrl Pts',(4.27420733716696,-5.24627874201402,
90.0204527655762));
#205937=CARTESIAN_POINT('Ctrl Pts',(4.41631326885093,-5.13050330465603,
90.0291061538045));
#205938=CARTESIAN_POINT('Ctrl Pts',(4.55380320092629,-5.0088767392532,90.0377595420328));
#205939=CARTESIAN_POINT('Ctrl Pts',(4.68619881506422,-4.88178549976243,
90.0464129302611));
#205940=CARTESIAN_POINT('Ctrl Pts',(4.8184721524608,-4.75481163804676,90.0550583264716));
#205941=CARTESIAN_POINT('Ctrl Pts',(4.94566033750963,-4.6223833784292,90.063703722682));
#205942=CARTESIAN_POINT('Ctrl Pts',(5.06731916572162,-4.48492647350103,
90.0723491188924));
#205943=CARTESIAN_POINT('Ctrl Pts',(5.19286336708493,-4.34307965806887,
90.0812706199348));
#205944=CARTESIAN_POINT('Ctrl Pts',(5.31251892980312,-4.19587788347152,
90.0901921209772));
#205945=CARTESIAN_POINT('Ctrl Pts',(5.42583830773499,-4.04383081474924,
90.0991136220195));
#205946=CARTESIAN_POINT('Ctrl Pts',(5.53544150274975,-3.89676996047409,
90.1077425523615));
#205947=CARTESIAN_POINT('Ctrl Pts',(5.63911728330392,-3.74517682179181,
90.1163714827035));
#205948=CARTESIAN_POINT('Ctrl Pts',(5.73650075164642,-3.58954706423527,
90.1250004130455));
#205949=CARTESIAN_POINT('Ctrl Pts',(5.8388370151344,-3.42600218185482,90.1340681994381));
#205950=CARTESIAN_POINT('Ctrl Pts',(5.93422402424429,-3.25799964095291,
90.1431359858307));
#205951=CARTESIAN_POINT('Ctrl Pts',(6.0222887918476,-3.08615079145313,90.1522037722233));
#205952=CARTESIAN_POINT('Ctrl Pts',(6.11035355945096,-2.91430194195324,
90.1612715586158));
#205953=CARTESIAN_POINT('Ctrl Pts',(6.19109587612012,-2.7386071153367,90.1703393450084));
#205954=CARTESIAN_POINT('Ctrl Pts',(6.26419778537867,-2.55970996514391,
90.179407131401));
#205955=CARTESIAN_POINT('Ctrl Pts',(6.33211738031526,-2.3934951275337,90.1878320875342));
#205956=CARTESIAN_POINT('Ctrl Pts',(6.39341187239156,-2.22458893283593,
90.1962570436673));
#205957=CARTESIAN_POINT('Ctrl Pts',(6.44788558095911,-2.05354827916454,
90.2046819998005));
#205958=CARTESIAN_POINT('Ctrl Pts',(6.5023719333974,-1.88246792531532,90.2131089114469));
#205959=CARTESIAN_POINT('Ctrl Pts',(6.55003424509045,-1.70925244065029,
90.2215358230933));
#205960=CARTESIAN_POINT('Ctrl Pts',(6.59072679538052,-1.534473625923,90.2299627347397));
#205961=CARTESIAN_POINT('Ctrl Pts',(6.6314343099064,-1.35963053821748,90.2383927452897));
#205962=CARTESIAN_POINT('Ctrl Pts',(6.66516687738618,-1.18322329697116,
90.2468227558397));
#205963=CARTESIAN_POINT('Ctrl Pts',(6.69182986510452,-1.00583401040893,
90.2552527663898));
#205964=CARTESIAN_POINT('Ctrl Pts',(6.7185174142095,-0.828281316545892,
90.2636905424892));
#205965=CARTESIAN_POINT('Ctrl Pts',(6.73812232313079,-0.6497450981302,90.2721283185887));
#205966=CARTESIAN_POINT('Ctrl Pts',(6.75060170196344,-0.470813828862723,
90.2805660946882));
#205967=CARTESIAN_POINT('Ctrl Pts',(6.76308763155006,-0.291788633868696,
90.2890082999981));
#205968=CARTESIAN_POINT('Ctrl Pts',(6.7684405560547,-0.112368305394942,
90.297450505308));
#205969=CARTESIAN_POINT('Ctrl Pts',(6.76666971342945,0.0668579790049228,
90.3058927106179));
#205970=CARTESIAN_POINT('Ctrl Pts',(6.76489700266267,0.246273337273407,
90.31434382199));
#205971=CARTESIAN_POINT('Ctrl Pts',(6.75598552361211,0.425493911419589,
90.322794933362));
#205972=CARTESIAN_POINT('Ctrl Pts',(6.73999650540597,0.60393385988483,90.331246044734));
#205973=CARTESIAN_POINT('Ctrl Pts',(6.73550916267943,0.65401330782504,90.3336178622313));
#205974=CARTESIAN_POINT('Ctrl Pts',(6.73046466724945,0.704031317616007,
90.3359896797286));
#205975=CARTESIAN_POINT('Ctrl Pts',(6.72486509888547,0.75397506708915,90.3383614972259));
#205976=CARTESIAN_POINT('Ctrl Pts',(6.70523127933225,0.929093308572983,
90.3466778233656));
#205977=CARTESIAN_POINT('Ctrl Pts',(6.6787339000174,1.10361393938351,90.3549941495051));
#205978=CARTESIAN_POINT('Ctrl Pts',(6.64542263473519,1.27696789534791,90.3633104756447));
#205979=CARTESIAN_POINT('Ctrl Pts',(6.61213959741287,1.45017495120281,90.3716197545311));
#205980=CARTESIAN_POINT('Ctrl Pts',(6.57205424364966,1.62221696198514,90.3799290334175));
#205981=CARTESIAN_POINT('Ctrl Pts',(6.52526791707303,1.79253106260878,90.3882383123039));
#205982=CARTESIAN_POINT('Ctrl Pts',(6.47851265905959,1.96273206577888,90.3965420733953));
#205983=CARTESIAN_POINT('Ctrl Pts',(6.42506538689996,2.1312071107869,90.4048458344868));
#205984=CARTESIAN_POINT('Ctrl Pts',(6.36507833186934,2.29740436779586,90.4131495955782));
#205985=CARTESIAN_POINT('Ctrl Pts',(6.30512011780479,2.46352171940775,90.4214493643334));
#205986=CARTESIAN_POINT('Ctrl Pts',(6.23862850497366,2.62736313892462,90.4297491330887));
#205987=CARTESIAN_POINT('Ctrl Pts',(6.16580537077836,2.78839257094132,90.4380489018439));
#205988=CARTESIAN_POINT('Ctrl Pts',(6.0930039075049,2.94937408334741,90.4463462007296));
#205989=CARTESIAN_POINT('Ctrl Pts',(6.01387482180807,3.10754495961661,90.4546434996153));
#205990=CARTESIAN_POINT('Ctrl Pts',(5.92866794794776,3.26238951735946,90.4629407985011));
#205991=CARTESIAN_POINT('Ctrl Pts',(5.84345361350842,3.41724763304674,90.4712388238851));
#205992=CARTESIAN_POINT('Ctrl Pts',(5.75216058895213,3.56877853995535,90.4795368492692));
#205993=CARTESIAN_POINT('Ctrl Pts',(5.65508472775332,3.71649104962345,90.4878348746533));
#205994=CARTESIAN_POINT('Ctrl Pts',(5.55799936493663,3.86421801713724,90.4961337122338));
#205995=CARTESIAN_POINT('Ctrl Pts',(5.45513022814476,4.00812555134536,90.5044325498142));
#205996=CARTESIAN_POINT('Ctrl Pts',(5.34681653722777,4.14775142905498,90.5127313873947));
#205997=CARTESIAN_POINT('Ctrl Pts',(5.23847424448607,4.28741417703322,90.5210324164054));
#205998=CARTESIAN_POINT('Ctrl Pts',(5.12468474555575,4.42279274016383,90.5293334454162));
#205999=CARTESIAN_POINT('Ctrl Pts',(5.00582768909733,4.55345782313469,90.5376344744269));
#206000=CARTESIAN_POINT('Ctrl Pts',(4.88691949199242,4.68417912739366,90.5459390751228));
#206001=CARTESIAN_POINT('Ctrl Pts',(4.76293962589371,4.81018265238984,90.5542436758187));
#206002=CARTESIAN_POINT('Ctrl Pts',(4.63430486078077,4.93107568967906,90.5625482765147));
#206003=CARTESIAN_POINT('Ctrl Pts',(4.50552329878613,5.05210668905711,90.5708623543491));
#206004=CARTESIAN_POINT('Ctrl Pts',(4.37207647916042,5.16801531114477,90.5791764321836));
#206005=CARTESIAN_POINT('Ctrl Pts',(4.23441539124735,5.2784481899861,90.587490510018));
#206006=CARTESIAN_POINT('Ctrl Pts',(4.09666738435227,5.38895079596351,90.5958098373474));
#206007=CARTESIAN_POINT('Ctrl Pts',(3.95470008203291,5.493970557266,90.6041291646767));
#206008=CARTESIAN_POINT('Ctrl Pts',(3.80899387004078,5.59319718032467,90.6124484920061));
#206009=CARTESIAN_POINT('Ctrl Pts',(3.66308419770517,5.6925623608445,90.6207794362265));
#206010=CARTESIAN_POINT('Ctrl Pts',(3.51342547851905,5.78611805558909,90.629110380447));
#206011=CARTESIAN_POINT('Ctrl Pts',(3.36052415939679,5.87359909885843,90.6374413246674));
#206012=CARTESIAN_POINT('Ctrl Pts',(3.27438251317608,5.92288422683237,90.6421348175283));
#206013=CARTESIAN_POINT('Ctrl Pts',(3.18721208119283,5.97024212636128,90.6468283103892));
#206014=CARTESIAN_POINT('Ctrl Pts',(3.09910619832126,6.01563211736944,90.6515218032501));
#206015=CARTESIAN_POINT('Origin',(0.,0.,4.30282021618968));
#206016=CARTESIAN_POINT('',(3.09910619832149,6.01563211736932,93.0457552630241));
#206017=CARTESIAN_POINT('',(3.09910619832136,6.01563211736939,92.6514522942042));
#206018=CARTESIAN_POINT('',(3.09910619832133,6.0156321173694,4.30282021618968));
#206019=CARTESIAN_POINT('',(-6.76729221817928,0.000612721246602595,91.6966736401472));
#206020=CARTESIAN_POINT('Ctrl Pts',(-6.767,3.66969153868988E-12,91.6971797838099));
#206021=CARTESIAN_POINT('Ctrl Pts',(-6.7670000000001,-0.186007249523421,
91.7059292956211));
#206022=CARTESIAN_POINT('Ctrl Pts',(-6.75932637294539,-0.372014355746692,
91.7146788074323));
#206023=CARTESIAN_POINT('Ctrl Pts',(-6.74400518264205,-0.557389537484492,
91.7234283192435));
#206024=CARTESIAN_POINT('Ctrl Pts',(-6.72868405705117,-0.742763936248965,
91.7321777940992));
#206025=CARTESIAN_POINT('Ctrl Pts',(-6.70571545645762,-0.927506130239609,
91.7409272689548));
#206026=CARTESIAN_POINT('Ctrl Pts',(-6.67517739404842,-1.11098863989912,
91.7496767438105));
#206027=CARTESIAN_POINT('Ctrl Pts',(-6.64463945808718,-1.29447038981863,
91.7584261824375));
#206028=CARTESIAN_POINT('Ctrl Pts',(-6.60653217008369,-1.47669218313621,
91.7671756210645));
#206029=CARTESIAN_POINT('Ctrl Pts',(-6.56098496092688,-1.65703510599243,
91.7759250596916));
#206030=CARTESIAN_POINT('Ctrl Pts',(-6.51543793658307,-1.83737729708665,
91.7846744628167));
#206031=CARTESIAN_POINT('Ctrl Pts',(-6.46245112167429,-2.01584035510899,
91.7934238659419));
#206032=CARTESIAN_POINT('Ctrl Pts',(-6.4022044837426,-2.19181813760771,
91.8021732690671));
#206033=CARTESIAN_POINT('Ctrl Pts',(-6.34195808526513,-2.36779522067117,
91.8109226374172));
#206034=CARTESIAN_POINT('Ctrl Pts',(-6.27445201433117,-2.54128677684134,
91.8196720057673));
#206035=CARTESIAN_POINT('Ctrl Pts',(-6.19991555071918,-2.71170355384774,
91.8284213741174));
#206036=CARTESIAN_POINT('Ctrl Pts',(-6.12537937716706,-2.88211966767448,
91.8371707084192));
#206037=CARTESIAN_POINT('Ctrl Pts',(-6.04381298052531,-3.04946076371764,
91.8459200427209));
#206038=CARTESIAN_POINT('Ctrl Pts',(-5.95549339335839,-3.21315848374533,
91.8546693770227));
#206039=CARTESIAN_POINT('Ctrl Pts',(-5.86717414255426,-3.37685558033461,
91.8634186780029));
#206040=CARTESIAN_POINT('Ctrl Pts',(-5.77210188876627,-3.53690907646709,
91.8721679789831));
#206041=CARTESIAN_POINT('Ctrl Pts',(-5.67059953347037,-3.69277536969223,
91.8809172799633));
#206042=CARTESIAN_POINT('Ctrl Pts',(-5.56909755631429,-3.84864108224858,
91.8896665483485));
#206043=CARTESIAN_POINT('Ctrl Pts',(-5.46116568196899,-4.0003193829745,
91.8984158167338));
#206044=CARTESIAN_POINT('Ctrl Pts',(-5.34717048533656,-4.14729511859786,
91.9071650851191));
#206045=CARTESIAN_POINT('Ctrl Pts',(-5.23317570391898,-4.29427031887841,
91.9159143216361));
#206046=CARTESIAN_POINT('Ctrl Pts',(-5.11311782003584,-4.43654276189466,
91.9246635581532));
#206047=CARTESIAN_POINT('Ctrl Pts',(-4.98740458984832,-4.57362924351766,
91.9334127946702));
#206048=CARTESIAN_POINT('Ctrl Pts',(-4.86169180711831,-4.71071523720176,
91.9421620000456));
#206049=CARTESIAN_POINT('Ctrl Pts',(-4.73032391204268,-4.84261509523143,
91.9509112054211));
#206050=CARTESIAN_POINT('Ctrl Pts',(-4.59374707013705,-4.96888084538231,
91.9596604107965));
#206051=CARTESIAN_POINT('Ctrl Pts',(-4.45717070301551,-5.09514615659371,
91.968409585757));
#206052=CARTESIAN_POINT('Ctrl Pts',(-4.31538563571146,-5.21577720459441,
91.9771587607174));
#206053=CARTESIAN_POINT('Ctrl Pts',(-4.16887341029613,-5.33036429232806,
91.9859079356779));
#206054=CARTESIAN_POINT('Ctrl Pts',(-4.02236168203806,-5.44495099123543,
91.9946570809499));
#206055=CARTESIAN_POINT('Ctrl Pts',(-3.87112305348261,-5.55349359438535,
92.0034062262219));
#206056=CARTESIAN_POINT('Ctrl Pts',(-3.71567117017851,-5.65562346298834,
92.0121553714939));
#206057=CARTESIAN_POINT('Ctrl Pts',(-3.56021980145912,-5.75775299351586,
92.0209044878041));
#206058=CARTESIAN_POINT('Ctrl Pts',(-3.40055544538445,-5.85346967463817,
92.0296536041143));
#206059=CARTESIAN_POINT('Ctrl Pts',(-3.23722035986952,-5.94244842986847,
92.0384027204244));
#206060=CARTESIAN_POINT('Ctrl Pts',(-3.07388580147277,-6.03142689794479,
92.0471518084993));
#206061=CARTESIAN_POINT('Ctrl Pts',(-2.90688078896673,-6.11366734656736,
92.0559008965741));
#206062=CARTESIAN_POINT('Ctrl Pts',(-2.73677250721463,-6.18889046952313,
92.064649984649));
#206063=CARTESIAN_POINT('Ctrl Pts',(-2.56666476031568,-6.26411335596292,
92.073399045215));
#206064=CARTESIAN_POINT('Ctrl Pts',(-2.39345402575245,-6.33231884500526,
92.082148105781));
#206065=CARTESIAN_POINT('Ctrl Pts',(-2.21772856065664,-6.39327529762702,
92.0908971663471));
#206066=CARTESIAN_POINT('Ctrl Pts',(-2.0420036334856,-6.45423156365097,
92.0996462001308));
#206067=CARTESIAN_POINT('Ctrl Pts',(-1.86376426189299,-6.50793874375653,
92.1083952339145));
#206068=CARTESIAN_POINT('Ctrl Pts',(-1.68361577753148,-6.55421443909543,
92.1171442676982));
#206069=CARTESIAN_POINT('Ctrl Pts',(-1.50346782967784,-6.60048999661872,
92.125893275426));
#206070=CARTESIAN_POINT('Ctrl Pts',(-1.32141105794962,-6.63933404237718,
92.1346422831539));
#206071=CARTESIAN_POINT('Ctrl Pts',(-1.13806375486988,-6.67061465607567,
92.1433912908817));
#206072=CARTESIAN_POINT('Ctrl Pts',(-0.954716982602583,-6.70189517921303,
92.1521402732801));
#206073=CARTESIAN_POINT('Ctrl Pts',(-0.770079968901612,-6.72561226592234,
92.1608892556785));
#206074=CARTESIAN_POINT('Ctrl Pts',(-0.584779765557624,-6.74168536983108,
92.1696382380769));
#206075=CARTESIAN_POINT('Ctrl Pts',(-0.391489830650703,-6.75845151013856,
92.1787644570868));
#206076=CARTESIAN_POINT('Ctrl Pts',(-0.197478578237765,-6.76689983031627,
92.1878906760966));
#206077=CARTESIAN_POINT('Ctrl Pts',(-0.00346287645080042,-6.76699911397118,
92.1970168951065));
#206078=CARTESIAN_POINT('Ctrl Pts',(0.184489834655289,-6.76709529501187,
92.2058579197723));
#206079=CARTESIAN_POINT('Ctrl Pts',(0.372446404250735,-6.75935639738161,
92.2146989444381));
#206080=CARTESIAN_POINT('Ctrl Pts',(0.559755019489661,-6.74380925873175,
92.2235399691039));
#206081=CARTESIAN_POINT('Ctrl Pts',(0.745134705523179,-6.7284222265979,
92.2322899477137));
#206082=CARTESIAN_POINT('Ctrl Pts',(0.929879431230048,-6.70538706057503,
92.2410399263234));
#206083=CARTESIAN_POINT('Ctrl Pts',(1.11336163626981,-6.67478200894101,
92.2497899049332));
#206084=CARTESIAN_POINT('Ctrl Pts',(1.2968419630089,-6.6441772706098,92.2585397939697));
#206085=CARTESIAN_POINT('Ctrl Pts',(1.47905951217697,-6.60600284890549,
92.2672896830062));
#206086=CARTESIAN_POINT('Ctrl Pts',(1.65939532067285,-6.5603884160718,92.2760395720428));
#206087=CARTESIAN_POINT('Ctrl Pts',(1.83972934301001,-6.514774435032,92.2847893744149));
#206088=CARTESIAN_POINT('Ctrl Pts',(2.01818138406461,-6.4617206606208,92.2935391767871));
#206089=CARTESIAN_POINT('Ctrl Pts',(2.19414528354394,-6.40140730423412,
92.3022889791592));
#206090=CARTESIAN_POINT('Ctrl Pts',(2.37010749864179,-6.34109452518575,
92.3110386977756));
#206091=CARTESIAN_POINT('Ctrl Pts',(2.54358134866624,-6.27352239616437,
92.3197884163919));
#206092=CARTESIAN_POINT('Ctrl Pts',(2.71397759435706,-6.19892043966753,
92.3285381350082));
#206093=CARTESIAN_POINT('Ctrl Pts',(2.88437226558266,-6.12431917249448,
92.3372877727769));
#206094=CARTESIAN_POINT('Ctrl Pts',(3.0516891268109,-6.04268832278731,92.3460374105456));
#206095=CARTESIAN_POINT('Ctrl Pts',(3.21535986273981,-5.95430516123266,
92.3547870483143));
#206096=CARTESIAN_POINT('Ctrl Pts',(3.37902914072971,-5.86592278697366,
92.3635366081434));
#206097=CARTESIAN_POINT('Ctrl Pts',(3.53905210621704,-5.77078835741861,
92.3722861679724));
#206098=CARTESIAN_POINT('Ctrl Pts',(3.69488522831831,-5.66922500431542,
92.3810357278015));
#206099=CARTESIAN_POINT('Ctrl Pts',(3.85071701407076,-5.56766252216999,
92.3897852125986));
#206100=CARTESIAN_POINT('Ctrl Pts',(4.00235878822542,-5.45967138329269,
92.3985346973957));
#206101=CARTESIAN_POINT('Ctrl Pts',(4.14929549611464,-5.34561838199499,
92.4072841821929));
#206102=CARTESIAN_POINT('Ctrl Pts',(4.29623099276231,-5.231566320869,92.4160335948655));
#206103=CARTESIAN_POINT('Ctrl Pts',(4.43846127436171,-5.1114526730484,92.424783007538));
#206104=CARTESIAN_POINT('Ctrl Pts',(4.57550326054586,-4.98568540049753,
92.4335324202106));
#206105=CARTESIAN_POINT('Ctrl Pts',(4.71254416257918,-4.85991912290227,
92.4422817636659));
#206106=CARTESIAN_POINT('Ctrl Pts',(4.84439664018891,-4.72849950385285,
92.4510311071211));
#206107=CARTESIAN_POINT('Ctrl Pts',(4.97061286794868,-4.59187289860934,
92.4597804505764));
#206108=CARTESIAN_POINT('Ctrl Pts',(5.09682813912806,-4.45524732884546,
92.4685297277212));
#206109=CARTESIAN_POINT('Ctrl Pts',(5.21740705147959,-4.31341506235642,
92.477279004866));
#206110=CARTESIAN_POINT('Ctrl Pts',(5.33194007545814,-4.16685781275573,
92.4860282820109));
#206111=CARTESIAN_POINT('Ctrl Pts',(5.44647226944594,-4.02030162521694,
92.494777495752));
#206112=CARTESIAN_POINT('Ctrl Pts',(5.55495848628212,-3.86902074887791,
92.5035267094931));
#206113=CARTESIAN_POINT('Ctrl Pts',(5.65703027291878,-3.71352898080525,
92.5122759232342));
#206114=CARTESIAN_POINT('Ctrl Pts',(5.75910135377082,-3.5580382878945,92.5210250764781));
#206115=CARTESIAN_POINT('Ctrl Pts',(5.85475793592832,-3.39833700106574,
92.529774229722));
#206116=CARTESIAN_POINT('Ctrl Pts',(5.94367514427473,-3.23496750823416,
92.5385233829659));
#206117=CARTESIAN_POINT('Ctrl Pts',(6.03259176732709,-3.07159909077588,
92.5472724786188));
#206118=CARTESIAN_POINT('Ctrl Pts',(6.11476896835988,-2.90456276731299,
92.5560215742717));
#206119=CARTESIAN_POINT('Ctrl Pts',(6.18992765547945,-2.73442583002917,
92.5647706699247));
#206120=CARTESIAN_POINT('Ctrl Pts',(6.26508587283112,-2.56428995616029,
92.5735197108927));
#206121=CARTESIAN_POINT('Ctrl Pts',(6.33322554827217,-2.39105376935052,
92.5822687518607));
#206122=CARTESIAN_POINT('Ctrl Pts',(6.39411526733085,-2.21530561053922,
92.5910177928288));
#206123=CARTESIAN_POINT('Ctrl Pts',(6.45500462602899,-2.03955849184935,
92.5997667820178));
#206124=CARTESIAN_POINT('Ctrl Pts',(6.50864402040788,-1.86129970164377,
92.6085157712068));
#206125=CARTESIAN_POINT('Ctrl Pts',(6.55485128368645,-1.68113463135886,
92.6172647603958));
#206126=CARTESIAN_POINT('Ctrl Pts',(6.60199809554361,-1.49730620116717,
92.6261916458673));
#206127=CARTESIAN_POINT('Ctrl Pts',(6.64140720707899,-1.31149343245567,
92.6351185313387));
#206128=CARTESIAN_POINT('Ctrl Pts',(6.67293928722902,-1.12435326697415,
92.6440454168101));
#206129=CARTESIAN_POINT('Ctrl Pts',(6.70384625876272,-0.940923067005509,
92.6527953309876));
#206130=CARTESIAN_POINT('Ctrl Pts',(6.72718554579808,-0.756217899520606,
92.661545245165));
#206131=CARTESIAN_POINT('Ctrl Pts',(6.74287786815337,-0.570865181253461,
92.6702951593425));
#206132=CARTESIAN_POINT('Ctrl Pts',(6.75856988190851,-0.38551610807298,
92.679044901447));
#206133=CARTESIAN_POINT('Ctrl Pts',(6.76661520773405,-0.199519795225453,
92.6877946435514));
#206134=CARTESIAN_POINT('Ctrl Pts',(6.76698651789579,-0.0135080204548247,
92.6965443856559));
#206135=CARTESIAN_POINT('Ctrl Pts',(6.76735782124901,0.172500343513712,
92.7052939673209));
#206136=CARTESIAN_POINT('Ctrl Pts',(6.7600553899518,0.358523882211601,92.7140435489859));
#206137=CARTESIAN_POINT('Ctrl Pts',(6.74510402742356,0.543930748564983,
92.7227931306508));
#206138=CARTESIAN_POINT('Ctrl Pts',(6.73015291918024,0.729334461615836,
92.7315425635075));
#206139=CARTESIAN_POINT('Ctrl Pts',(6.70755316306587,0.914121237635275,
92.7402919963642));
#206140=CARTESIAN_POINT('Ctrl Pts',(6.67738151874565,1.09766345166181,92.7490414292209));
#206141=CARTESIAN_POINT('Ctrl Pts',(6.64721034747558,1.28120278799723,92.7577907248984));
#206142=CARTESIAN_POINT('Ctrl Pts',(6.60946757205129,1.46349731860387,92.766540020576));
#206143=CARTESIAN_POINT('Ctrl Pts',(6.56428138111508,1.64392790278219,92.7752893162535));
#206144=CARTESIAN_POINT('Ctrl Pts',(6.51909583859835,1.82435589779109,92.7840384863791));
#206145=CARTESIAN_POINT('Ctrl Pts',(6.4664671639286,2.00291972192314,92.7927876565047));
#206146=CARTESIAN_POINT('Ctrl Pts',(6.40657409872868,2.17901292274708,92.8015368266303));
#206147=CARTESIAN_POINT('Ctrl Pts',(6.34668181342061,2.35510383059019,92.8102858828294));
#206148=CARTESIAN_POINT('Ctrl Pts',(6.27952541914034,2.52872390822619,92.8190349390285));
#206149=CARTESIAN_POINT('Ctrl Pts',(6.20533299175501,2.69928350890322,92.8277839952276));
#206150=CARTESIAN_POINT('Ctrl Pts',(6.12831602991533,2.87633637965657,92.8368661313858));
#206151=CARTESIAN_POINT('Ctrl Pts',(6.04371690605255,3.05009086601493,92.845948267544));
#206152=CARTESIAN_POINT('Ctrl Pts',(5.95184520316616,3.21991112882762,92.8550304037022));
#206153=CARTESIAN_POINT('Ctrl Pts',(5.86333549509257,3.38351691183047,92.8637801840457));
#206154=CARTESIAN_POINT('Ctrl Pts',(5.76807618099349,3.54347103712036,92.8725299643893));
#206155=CARTESIAN_POINT('Ctrl Pts',(5.66639083308994,3.69923018027729,92.8812797447329));
#206156=CARTESIAN_POINT('Ctrl Pts',(5.56470914082181,3.85498372382078,92.8900292105178));
#206157=CARTESIAN_POINT('Ctrl Pts',(5.45660203372051,4.00654234702019,92.8987786763027));
#206158=CARTESIAN_POINT('Ctrl Pts',(5.34243669839204,4.15339127986684,92.9075281420876));
#206159=CARTESIAN_POINT('Ctrl Pts',(5.22827486050581,4.30023571401292,92.9162773398336));
#206160=CARTESIAN_POINT('Ctrl Pts',(5.10805534167103,4.44237052028479,92.9250265375796));
#206161=CARTESIAN_POINT('Ctrl Pts',(4.98218644339946,4.57931296628727,92.9337757353256));
#206162=CARTESIAN_POINT('Ctrl Pts',(4.85632073219587,4.7162519448336,92.9425247115373));
#206163=CARTESIAN_POINT('Ctrl Pts',(4.72480612170326,4.84799861524501,92.9512736877489));
#206164=CARTESIAN_POINT('Ctrl Pts',(4.58808925235326,4.97410554898472,92.9600226639605));
#206165=CARTESIAN_POINT('Ctrl Pts',(4.45136349474066,5.10022068121191,92.9687722089622));
#206166=CARTESIAN_POINT('Ctrl Pts',(4.30943501210102,5.22069514871816,92.9775217539639));
#206167=CARTESIAN_POINT('Ctrl Pts',(4.16278587431808,5.33511975166237,92.9862712989656));
#206168=CARTESIAN_POINT('Ctrl Pts',(4.01614535740469,5.44953762807827,92.9950203296194));
#206169=CARTESIAN_POINT('Ctrl Pts',(3.8647849665794,5.55790617532772,93.0037693602731));
#206170=CARTESIAN_POINT('Ctrl Pts',(3.70921874747207,5.65985735539349,93.0125183909268));
#206171=CARTESIAN_POINT('Ctrl Pts',(3.55365041605906,5.76180991977043,93.0212675403765));
#206172=CARTESIAN_POINT('Ctrl Pts',(3.39387638174522,5.85734478552814,93.0300166898261));
#206173=CARTESIAN_POINT('Ctrl Pts',(3.23043927904532,5.94613749121236,93.0387658392757));
#206174=CARTESIAN_POINT('Ctrl Pts',(3.18691767070429,5.96978206944148,93.0410956471919));
#206175=CARTESIAN_POINT('Ctrl Pts',(3.14313645919635,5.99294880633423,93.043425455108));
#206176=CARTESIAN_POINT('Ctrl Pts',(3.09910619832149,6.01563211736932,93.0457552630241));
#206177=CARTESIAN_POINT('Ctrl Pts',(3.09910619832119,6.01563211736948,91.0458502363996));
#206178=CARTESIAN_POINT('Ctrl Pts',(2.9398956747614,6.09765347618519,91.0542757770372));
#206179=CARTESIAN_POINT('Ctrl Pts',(2.77736701447553,6.17338133629389,91.0627013176748));
#206180=CARTESIAN_POINT('Ctrl Pts',(2.61204730635548,6.24255539577833,91.0711268583124));
#206181=CARTESIAN_POINT('Ctrl Pts',(2.44677049905691,6.31171150444485,91.079550212504));
#206182=CARTESIAN_POINT('Ctrl Pts',(2.27870439445777,6.374317072692,91.0879735666956));
#206183=CARTESIAN_POINT('Ctrl Pts',(2.10839732830607,6.43015938418262,91.0963969208872));
#206184=CARTESIAN_POINT('Ctrl Pts',(1.93811414965261,6.4859938631555,91.1048190936078));
#206185=CARTESIAN_POINT('Ctrl Pts',(1.76559095281422,6.5350668725321,91.1132412663284));
#206186=CARTESIAN_POINT('Ctrl Pts',(1.59139286804078,6.5772150443443,91.121663439049));
#206187=CARTESIAN_POINT('Ctrl Pts',(1.4171948994209,6.61936318805251,91.1300856061537));
#206188=CARTESIAN_POINT('Ctrl Pts',(1.24132236927861,6.65458642527241,91.1385077732585));
#206189=CARTESIAN_POINT('Ctrl Pts',(1.06435263838302,6.6827720641338,91.1469299403633));
#206190=CARTESIAN_POINT('Ctrl Pts',(0.887358321108872,6.71096161882183,
91.1553532775585));
#206191=CARTESIAN_POINT('Ctrl Pts',(0.709266828560109,6.73211157397049,
91.1637766147537));
#206192=CARTESIAN_POINT('Ctrl Pts',(0.530663084433825,6.74616081121842,
91.1721999519489));
#206193=CARTESIAN_POINT('Ctrl Pts',(0.351940488742354,6.76021939750797,
91.1806288944399));
#206194=CARTESIAN_POINT('Ctrl Pts',(0.172705293067564,6.76716779651611,
91.1890578369308));
#206195=CARTESIAN_POINT('Ctrl Pts',(-0.00645406409859743,6.76699692219943,
91.1974867794218));
#206196=CARTESIAN_POINT('Ctrl Pts',(-0.185672892685407,6.76682599116153,
91.2059185198754));
#206197=CARTESIAN_POINT('Ctrl Pts',(-0.364815499032925,6.75953108099326,
91.2143502603289));
#206198=CARTESIAN_POINT('Ctrl Pts',(-0.543295520171679,6.74515522265881,
91.2227820007825));
#206199=CARTESIAN_POINT('Ctrl Pts',(-0.721947152431176,6.73076554172873,
91.2312218484764));
#206200=CARTESIAN_POINT('Ctrl Pts',(-0.89993459407557,6.7092813395262,91.2396616961704));
#206201=CARTESIAN_POINT('Ctrl Pts',(-1.07667744414064,6.68079745848344,
91.2481015438643));
#206202=CARTESIAN_POINT('Ctrl Pts',(-1.21150496096729,6.65906865333423,
91.254539845083));
#206203=CARTESIAN_POINT('Ctrl Pts',(-1.34560832735392,6.63326756376359,
91.2609781463017));
#206204=CARTESIAN_POINT('Ctrl Pts',(-1.47873466302166,6.6034561251195,91.2674164475204));
#206205=CARTESIAN_POINT('Ctrl Pts',(-1.64704155002527,6.56576658450292,
91.2755561625533));
#206206=CARTESIAN_POINT('Ctrl Pts',(-1.81412186111606,6.52158998995999,
91.2836958775862));
#206207=CARTESIAN_POINT('Ctrl Pts',(-1.97943381462411,6.47102239012682,
91.2918355926191));
#206208=CARTESIAN_POINT('Ctrl Pts',(-2.14460118729004,6.4204990164129,91.2999681887061));
#206209=CARTESIAN_POINT('Ctrl Pts',(-2.30800293306743,6.36359586973028,
91.3081007847931));
#206210=CARTESIAN_POINT('Ctrl Pts',(-2.4691078287673,6.30045994590237,91.31623338088));
#206211=CARTESIAN_POINT('Ctrl Pts',(-2.63010258451681,6.23736718517938,
91.324360417088));
#206212=CARTESIAN_POINT('Ctrl Pts',(-2.78880327691345,6.16805026393771,
91.332487453296));
#206213=CARTESIAN_POINT('Ctrl Pts',(-2.94469425532868,6.0927058637878,91.3406144895039));
#206214=CARTESIAN_POINT('Ctrl Pts',(-3.10051071503471,6.01739747962485,
91.3487376408415));
#206215=CARTESIAN_POINT('Ctrl Pts',(-3.25351980628306,5.93606751307471,
91.3568607921791));
#206216=CARTESIAN_POINT('Ctrl Pts',(-3.4032262897393,5.84896057610472,91.3649839435167));
#206217=CARTESIAN_POINT('Ctrl Pts',(-3.55289070456197,5.76187811683088,
91.3731048121884));
#206218=CARTESIAN_POINT('Ctrl Pts',(-3.69925404424552,5.66902210526866,
91.3812256808601));
#206219=CARTESIAN_POINT('Ctrl Pts',(-3.84184613011026,5.57068284077965,
91.3893465495319));
#206220=CARTESIAN_POINT('Ctrl Pts',(-3.98444592219597,5.47233826166117,
91.3974678570864));
#206221=CARTESIAN_POINT('Ctrl Pts',(-4.12327374954491,5.36851004223815,
91.4055891646408));
#206222=CARTESIAN_POINT('Ctrl Pts',(-4.25788871121837,5.25953160679534,
91.4137104721953));
#206223=CARTESIAN_POINT('Ctrl Pts',(-4.32783932476428,5.20290262345106,
91.417930585912));
#206224=CARTESIAN_POINT('Ctrl Pts',(-4.39665288973983,5.14488366640152,
91.4221506996287));
#206225=CARTESIAN_POINT('Ctrl Pts',(-4.46427107342832,5.08552581184593,
91.4263708133454));
#206226=CARTESIAN_POINT('Ctrl Pts',(-4.60822724507752,4.95915552159235,
91.4353552518713));
#206227=CARTESIAN_POINT('Ctrl Pts',(-4.74669213064618,4.82677724828876,
91.4443396903972));
#206228=CARTESIAN_POINT('Ctrl Pts',(-4.87920862823121,4.68888176031281,
91.4533241289231));
#206229=CARTESIAN_POINT('Ctrl Pts',(-5.01195384138075,4.55074827295602,
91.4623240740535));
#206230=CARTESIAN_POINT('Ctrl Pts',(-5.13872998085703,4.40707871057319,
91.471324019184));
#206231=CARTESIAN_POINT('Ctrl Pts',(-5.25911933895199,4.25839791220375,
91.4803239643144));
#206232=CARTESIAN_POINT('Ctrl Pts',(-5.37979239766028,4.10936674371559,
91.4893451180467));
#206233=CARTESIAN_POINT('Ctrl Pts',(-5.49404841016782,3.95530089760421,
91.4983662717789));
#206234=CARTESIAN_POINT('Ctrl Pts',(-5.60151061891099,3.7967575358755,91.5073874255112));
#206235=CARTESIAN_POINT('Ctrl Pts',(-5.70908217129881,3.63805285502625,
91.5164177583384));
#206236=CARTESIAN_POINT('Ctrl Pts',(-5.80984598096192,3.47486175796944,
91.5254480911657));
#206237=CARTESIAN_POINT('Ctrl Pts',(-5.90346983463317,3.30776856983317,
91.534478423993));
#206238=CARTESIAN_POINT('Ctrl Pts',(-5.99722641741692,3.14043849622708,
91.5435215589857));
#206239=CARTESIAN_POINT('Ctrl Pts',(-6.08382268774475,2.96919547887985,
91.5525646939784));
#206240=CARTESIAN_POINT('Ctrl Pts',(-6.16297235725555,2.79464858680014,
91.5616078289711));
#206241=CARTESIAN_POINT('Ctrl Pts',(-6.23216740342193,2.64205438987798,
91.5695136123708));
#206242=CARTESIAN_POINT('Ctrl Pts',(-6.29567185242913,2.48693553989782,
91.5774193957705));
#206243=CARTESIAN_POINT('Ctrl Pts',(-6.35332481091421,2.3297108934419,91.5853251791702));
#206244=CARTESIAN_POINT('Ctrl Pts',(-6.42129982523422,2.14433710040292,
91.5946463962235));
#206245=CARTESIAN_POINT('Ctrl Pts',(-6.48119410585874,1.9558845786944,91.6039676132768));
#206246=CARTESIAN_POINT('Ctrl Pts',(-6.53275243902799,1.76505936737944,
91.61328883033));
#206247=CARTESIAN_POINT('Ctrl Pts',(-6.58166644677203,1.58402120554867,
91.6221319805078));
#206248=CARTESIAN_POINT('Ctrl Pts',(-6.62307798233069,1.40084792773441,
91.6309751306855));
#206249=CARTESIAN_POINT('Ctrl Pts',(-6.65681923776214,1.21616061264945,
91.6398182808632));
#206250=CARTESIAN_POINT('Ctrl Pts',(-6.69052569194362,1.03166378690272,
91.6486523100798));
#206251=CARTESIAN_POINT('Ctrl Pts',(-6.71657759937819,0.845656305320527,
91.6574863392965));
#206252=CARTESIAN_POINT('Ctrl Pts',(-6.73485780107018,0.658771128210807,
91.6663203685131));
#206253=CARTESIAN_POINT('Ctrl Pts',(-6.75311200586027,0.472151726922313,
91.6751418345537));
#206254=CARTESIAN_POINT('Ctrl Pts',(-6.7636165360224,0.284657390739837,
91.6839633005943));
#206255=CARTESIAN_POINT('Ctrl Pts',(-6.76630578097467,0.0969282123470912,
91.6927847666349));
#206256=CARTESIAN_POINT('Ctrl Pts',(-6.76675239146241,0.0657514986545169,
91.6942497723599));
#206257=CARTESIAN_POINT('Ctrl Pts',(-6.76698357027965,0.0345683247144677,
91.6957147780849));
#206258=CARTESIAN_POINT('Ctrl Pts',(-6.76699915505439,0.00338164061046775,
91.6971797838099));
#206259=CARTESIAN_POINT('',(-6.7669999994732,-8.44378501004791E-5,91.3028202161459));
#206260=CARTESIAN_POINT('Ctrl Pts',(3.09910619832126,6.01563211736944,90.6515218032501));
#206261=CARTESIAN_POINT('Ctrl Pts',(3.06939383950441,6.03093919625649,90.6531046117919));
#206262=CARTESIAN_POINT('Ctrl Pts',(3.03957510944118,6.04602251175088,90.6546874203336));
#206263=CARTESIAN_POINT('Ctrl Pts',(3.00965363156952,6.06088063056685,90.6562702288754));
#206264=CARTESIAN_POINT('Ctrl Pts',(2.85710093032343,6.13663377920923,90.6643400748781));
#206265=CARTESIAN_POINT('Ctrl Pts',(2.70140454992178,6.20676334665172,90.6724099208809));
#206266=CARTESIAN_POINT('Ctrl Pts',(2.54302590332117,6.27098941595643,90.6804797668836));
#206267=CARTESIAN_POINT('Ctrl Pts',(2.38484651720289,6.33513468069675,90.6885394599937));
#206268=CARTESIAN_POINT('Ctrl Pts',(2.22399192081392,6.39339108726076,90.6965991531037));
#206269=CARTESIAN_POINT('Ctrl Pts',(2.06094945812464,6.44552374373532,90.7046588462138));
#206270=CARTESIAN_POINT('Ctrl Pts',(1.89807634092915,6.49760225216582,90.7127101680524));
#206271=CARTESIAN_POINT('Ctrl Pts',(1.73302023197066,6.54356955527737,90.720761489891));
#206272=CARTESIAN_POINT('Ctrl Pts',(1.56628977029931,6.58323821196345,90.7288128117296));
#206273=CARTESIAN_POINT('Ctrl Pts',(1.39969594836909,6.6228743592033,90.7368575353107));
#206274=CARTESIAN_POINT('Ctrl Pts',(1.23143086590423,6.6562220479362,90.7449022588917));
#206275=CARTESIAN_POINT('Ctrl Pts',(1.0620195938675,6.68314322622533,90.7529469824727));
#206276=CARTESIAN_POINT('Ctrl Pts',(0.892710074361159,6.71004823500001,
90.7609868741971));
#206277=CARTESIAN_POINT('Ctrl Pts',(0.7222561032782,6.73053435882903,90.7690267659215));
#206278=CARTESIAN_POINT('Ctrl Pts',(0.551194145090353,6.74451436460907,
90.7770666576459));
#206279=CARTESIAN_POINT('Ctrl Pts',(0.376448754287485,6.75879539821432,
90.7852796702659));
#206280=CARTESIAN_POINT('Ctrl Pts',(0.201069283828813,6.76628685388274,
90.7934926828858));
#206281=CARTESIAN_POINT('Ctrl Pts',(0.0256349535357023,6.76695144427365,
90.8017056955058));
#206282=CARTESIAN_POINT('Ctrl Pts',(-0.146041501907251,6.76760179886755,
90.8097427820483));
#206283=CARTESIAN_POINT('Ctrl Pts',(-0.317770101994881,6.7617148055548,
90.8177798685909));
#206284=CARTESIAN_POINT('Ctrl Pts',(-0.489006855450561,6.74930820864793,
90.8258169551335));
#206285=CARTESIAN_POINT('Ctrl Pts',(-0.660259997060672,6.73690042437198,
90.8338548108626));
#206286=CARTESIAN_POINT('Ctrl Pts',(-0.831020825641169,6.71797182097387,
90.8418926665918));
#206287=CARTESIAN_POINT('Ctrl Pts',(-1.0007496397776,6.69259211057159,90.849930522321));
#206288=CARTESIAN_POINT('Ctrl Pts',(-1.1705283266965,6.66720494264488,90.8579707398779));
#206289=CARTESIAN_POINT('Ctrl Pts',(-1.33927402626337,6.63536294985121,
90.8660109574349));
#206290=CARTESIAN_POINT('Ctrl Pts',(-1.5064565559803,6.59718710095022,90.8740511749918));
#206291=CARTESIAN_POINT('Ctrl Pts',(-1.67995534878654,6.55756894401786,
90.8823951571196));
#206292=CARTESIAN_POINT('Ctrl Pts',(-1.85177011566018,6.51112908758498,
90.8907391392473));
#206293=CARTESIAN_POINT('Ctrl Pts',(-2.02132588847267,6.45805935653972,
90.8990831213751));
#206294=CARTESIAN_POINT('Ctrl Pts',(-2.18499337958725,6.40683261509513,
90.9071373362101));
#206295=CARTESIAN_POINT('Ctrl Pts',(-2.34655582124598,6.34942894572099,
90.9151915510452));
#206296=CARTESIAN_POINT('Ctrl Pts',(-2.50551733007726,6.28606967100131,
90.9232457658803));
#206297=CARTESIAN_POINT('Ctrl Pts',(-2.66459779531212,6.22266298234156,
90.9313060079633));
#206298=CARTESIAN_POINT('Ctrl Pts',(-2.82107311305556,6.15329196468001,
90.9393662500463));
#206299=CARTESIAN_POINT('Ctrl Pts',(-2.97447219276308,6.07822376804928,
90.9474264921293));
#206300=CARTESIAN_POINT('Ctrl Pts',(-3.12808573490635,6.00305062093041,
90.9554980029836));
#206301=CARTESIAN_POINT('Ctrl Pts',(-3.27861413220835,5.92216457836578,
90.963569513838));
#206302=CARTESIAN_POINT('Ctrl Pts',(-3.4256149483357,5.83587621747917,90.9716410246923));
#206303=CARTESIAN_POINT('Ctrl Pts',(-3.44102216867744,5.82683229633553,
90.9724870033032));
#206304=CARTESIAN_POINT('Ctrl Pts',(-3.45639066779913,5.81772906586434,
90.973332981914));
#206305=CARTESIAN_POINT('Ctrl Pts',(-3.47171995776792,5.80856690887141,
90.9741789605249));
#206306=CARTESIAN_POINT('Ctrl Pts',(-3.62083549545187,5.71944210471361,
90.9824082102609));
#206307=CARTESIAN_POINT('Ctrl Pts',(-3.76673597130493,5.62444058443306,
90.9906374599968));
#206308=CARTESIAN_POINT('Ctrl Pts',(-3.90892657006052,5.5238195182206,90.9988667097328));
#206309=CARTESIAN_POINT('Ctrl Pts',(-4.05094793887191,5.42331820744605,
91.0070861653229));
#206310=CARTESIAN_POINT('Ctrl Pts',(-4.18926793260898,5.3172108734082,91.0153056209129));
#206311=CARTESIAN_POINT('Ctrl Pts',(-4.32341688020288,5.20580017672373,
91.0235250765029));
#206312=CARTESIAN_POINT('Ctrl Pts',(-4.45743310913498,5.09449970288364,
91.0317364002726));
#206313=CARTESIAN_POINT('Ctrl Pts',(-4.58728623588905,4.97790654285264,
91.0399477240422));
#206314=CARTESIAN_POINT('Ctrl Pts',(-4.71253604220504,4.85636623937266,
91.0481590478119));
#206315=CARTESIAN_POINT('Ctrl Pts',(-4.8376870782683,4.73492178088313,91.056363896246));
#206316=CARTESIAN_POINT('Ctrl Pts',(-4.95824176799382,4.60853819793749,
91.0645687446801));
#206317=CARTESIAN_POINT('Ctrl Pts',(-5.07379337674746,4.47760089446052,
91.0727735931142));
#206318=CARTESIAN_POINT('Ctrl Pts',(-5.18927705434655,4.34674056717016,
91.0809736180341));
#206319=CARTESIAN_POINT('Ctrl Pts',(-5.29976327354346,4.21133212052189,
91.089173642954));
#206320=CARTESIAN_POINT('Ctrl Pts',(-5.40488249686137,4.07179741577618,
91.0973736678739));
#206321=CARTESIAN_POINT('Ctrl Pts',(-5.5099712962948,3.9323030955349,91.1055713195208));
#206322=CARTESIAN_POINT('Ctrl Pts',(-5.60969597518714,3.78868517966619,
91.1137689711678));
#206323=CARTESIAN_POINT('Ctrl Pts',(-5.70372745865022,3.64139836840733,
91.1219666228147));
#206324=CARTESIAN_POINT('Ctrl Pts',(-5.79774635072071,3.49413127975619,
91.1301631767458));
#206325=CARTESIAN_POINT('Ctrl Pts',(-5.88607337199358,3.34319657600585,
91.1383597306769));
#206326=CARTESIAN_POINT('Ctrl Pts',(-5.96842295158974,3.18907768342773,
91.1465562846079));
#206327=CARTESIAN_POINT('Ctrl Pts',(-6.05077647736528,3.03495140549564,
91.1547532313166));
#206328=CARTESIAN_POINT('Ctrl Pts',(-6.12715182167917,2.87764095115629,
91.1629501780253));
#206329=CARTESIAN_POINT('Ctrl Pts',(-6.19730950732372,2.7176541116255,91.171147124734));
#206330=CARTESIAN_POINT('Ctrl Pts',(-6.26748331137602,2.55763051584927,
91.1793459546538));
#206331=CARTESIAN_POINT('Ctrl Pts',(-6.33143646761472,2.39492963869119,
91.1875447845735));
#206332=CARTESIAN_POINT('Ctrl Pts',(-6.38897773375776,2.23007903840818,
91.1957436144933));
#206333=CARTESIAN_POINT('Ctrl Pts',(-6.44657349883587,2.06507230353235,
91.2039502097531));
#206334=CARTESIAN_POINT('Ctrl Pts',(-6.49774512238016,1.89791211681596,
91.2121568050129));
#206335=CARTESIAN_POINT('Ctrl Pts',(-6.54235105473117,1.72914189026173,
91.2203634002727));
#206336=CARTESIAN_POINT('Ctrl Pts',(-6.58697857660921,1.56028997795012,
91.2285739675717));
#206337=CARTESIAN_POINT('Ctrl Pts',(-6.62503399333639,1.38982682204616,
91.2367845348707));
#206338=CARTESIAN_POINT('Ctrl Pts',(-6.65642698240801,1.21830572019939,
91.2449951021697));
#206339=CARTESIAN_POINT('Ctrl Pts',(-6.68786326690575,1.04654806619846,
91.2532169930164));
#206340=CARTESIAN_POINT('Ctrl Pts',(-6.7126187097016,0.873729905530169,
91.2614388838631));
#206341=CARTESIAN_POINT('Ctrl Pts',(-6.73065479887372,0.700410578445401,
91.2696607747098));
#206342=CARTESIAN_POINT('Ctrl Pts',(-6.74705386046797,0.542822406574355,
91.2771364138647));
#206343=CARTESIAN_POINT('Ctrl Pts',(-6.75789860586077,0.384820155424103,
91.2846120530196));
#206344=CARTESIAN_POINT('Ctrl Pts',(-6.76319748642094,0.226823190325659,
91.2920876921745));
#206345=CARTESIAN_POINT('Ctrl Pts',(-6.76573329468454,0.151212878832433,
91.295665200165));
#206346=CARTESIAN_POINT('Ctrl Pts',(-6.76700094344126,0.0755668471369315,
91.2992427081555));
#206347=CARTESIAN_POINT('Ctrl Pts',(-6.7669999994732,-8.44378502934827E-5,
91.302820216146));
#206348=CARTESIAN_POINT('Ctrl Pts',(-6.76699999947319,-8.44387777600782E-5,
91.3028202161898));
#206349=CARTESIAN_POINT('Ctrl Pts',(-6.76699768248362,-0.185770078054274,
91.3116011887582));
#206350=CARTESIAN_POINT('Ctrl Pts',(-6.75934825938162,-0.371614094343413,
91.3203821613265));
#206351=CARTESIAN_POINT('Ctrl Pts',(-6.74403856800726,-0.556985451542986,
91.3291631338949));
#206352=CARTESIAN_POINT('Ctrl Pts',(-6.72875226280503,-0.742073646504984,
91.3379306931729));
#206353=CARTESIAN_POINT('Ctrl Pts',(-6.70582905174118,-0.926690340762121,
91.3466982524509));
#206354=CARTESIAN_POINT('Ctrl Pts',(-6.67530773716562,-1.11020521262372,
91.3554658117289));
#206355=CARTESIAN_POINT('Ctrl Pts',(-6.64485355501386,-1.2933164387602,
91.3642140865326));
#206356=CARTESIAN_POINT('Ctrl Pts',(-6.60683466384861,-1.47533039936832,
91.3729623613364));
#206357=CARTESIAN_POINT('Ctrl Pts',(-6.56134143433908,-1.65562301929674,
91.3817106361401));
#206358=CARTESIAN_POINT('Ctrl Pts',(-6.51590982674312,-1.83567142758392,
91.390447061149));
#206359=CARTESIAN_POINT('Ctrl Pts',(-6.4630241384197,-2.01400287093144,
91.399183486158));
#206360=CARTESIAN_POINT('Ctrl Pts',(-6.40282590211974,-2.19000216144748,
91.4079199111669));
#206361=CARTESIAN_POINT('Ctrl Pts',(-6.3427454549406,-2.36565707639755,
91.4166392417246));
#206362=CARTESIAN_POINT('Ctrl Pts',(-6.27538109980184,-2.53898867583702,
91.4253585722821));
#206363=CARTESIAN_POINT('Ctrl Pts',(-6.20092433901847,-2.70939593669297,
91.4340779028398));
#206364=CARTESIAN_POINT('Ctrl Pts',(-6.15263714409944,-2.81990958963724,
91.4397326212262));
#206365=CARTESIAN_POINT('Ctrl Pts',(-6.10136800821583,-2.92919352916704,
91.4453873396127));
#206366=CARTESIAN_POINT('Ctrl Pts',(-6.04718044105795,-3.03708704407466,
91.4510420579992));
#206367=CARTESIAN_POINT('Ctrl Pts',(-5.96851673554355,-3.19371529163704,
91.4592509724283));
#206368=CARTESIAN_POINT('Ctrl Pts',(-5.88376810752466,-3.34727700123832,
91.4674598868574));
#206369=CARTESIAN_POINT('Ctrl Pts',(-5.79321279975888,-3.49728100911406,
91.4756688012865));
#206370=CARTESIAN_POINT('Ctrl Pts',(-5.70263596292875,-3.64732067968058,
91.4838796673433));
#206371=CARTESIAN_POINT('Ctrl Pts',(-5.60624988002251,-3.79380065855253,
91.4920905334001));
#206372=CARTESIAN_POINT('Ctrl Pts',(-5.50437678694001,-3.93625776434878,
91.5003013994569));
#206373=CARTESIAN_POINT('Ctrl Pts',(-5.4024613147416,-4.07877413217403,
91.5085156812267));
#206374=CARTESIAN_POINT('Ctrl Pts',(-5.29505449192088,-4.2172640035322,
91.5167299629964));
#206375=CARTESIAN_POINT('Ctrl Pts',(-5.18251962523664,-4.35129628203333,
91.5249442447662));
#206376=CARTESIAN_POINT('Ctrl Pts',(-5.06985809167539,-4.48547942444569,
91.5331677723586));
#206377=CARTESIAN_POINT('Ctrl Pts',(-4.95205721468211,-4.61519467984284,
91.541391299951));
#206378=CARTESIAN_POINT('Ctrl Pts',(-4.82951870647705,-4.74004620903513,
91.5496148275435));
#206379=CARTESIAN_POINT('Ctrl Pts',(-4.70690165585513,-4.86497776320074,
91.5578436260971));
#206380=CARTESIAN_POINT('Ctrl Pts',(-4.57954117910739,-4.98503913308348,
91.5660724246508));
#206381=CARTESIAN_POINT('Ctrl Pts',(-4.44787296901597,-5.09987402310067,
91.5743012232045));
#206382=CARTESIAN_POINT('Ctrl Pts',(-4.31602352816969,-5.21486697415469,
91.5825413480409));
#206383=CARTESIAN_POINT('Ctrl Pts',(-4.17985478727197,-5.32461885352455,
91.5907814728773));
#206384=CARTESIAN_POINT('Ctrl Pts',(-4.03983317364497,-5.42881542595782,
91.5990215977137));
#206385=CARTESIAN_POINT('Ctrl Pts',(-3.97766935567199,-5.47507440408533,
91.6026798730838));
#206386=CARTESIAN_POINT('Ctrl Pts',(-3.91474649289734,-5.52023902595243,
91.6063381484538));
#206387=CARTESIAN_POINT('Ctrl Pts',(-3.85110698089105,-5.5642846819454,
91.6099964238239));
#206388=CARTESIAN_POINT('Ctrl Pts',(-3.70414482204787,-5.66599892343348,
91.6184444465864));
#206389=CARTESIAN_POINT('Ctrl Pts',(-3.553022930525,-5.76197564419767,91.6268924693489));
#206390=CARTESIAN_POINT('Ctrl Pts',(-3.39821706777274,-5.85187232945986,
91.6353404921115));
#206391=CARTESIAN_POINT('Ctrl Pts',(-3.24355296537231,-5.94168669364259,
91.6437807787672));
#206392=CARTESIAN_POINT('Ctrl Pts',(-3.08521190319609,-6.02543195366043,
91.652221065423));
#206393=CARTESIAN_POINT('Ctrl Pts',(-2.92369862713102,-6.10280880723886,
91.6606613520788));
#206394=CARTESIAN_POINT('Ctrl Pts',(-2.7623083895356,-6.18012671625321,
91.6690952090467));
#206395=CARTESIAN_POINT('Ctrl Pts',(-2.59775105516567,-6.25108574644093,
91.6775290660146));
#206396=CARTESIAN_POINT('Ctrl Pts',(-2.43055632733157,-6.31543228446545,
91.6859629229825));
#206397=CARTESIAN_POINT('Ctrl Pts',(-2.26346326257204,-6.37973969645425,
91.6943916517275));
#206398=CARTESIAN_POINT('Ctrl Pts',(-2.09373631212831,-6.43744251306235,
91.7028203804725));
#206399=CARTESIAN_POINT('Ctrl Pts',(-1.92192589874289,-6.48833490502312,
91.7112491092175));
#206400=CARTESIAN_POINT('Ctrl Pts',(-1.75019357130512,-6.53920416695017,
91.7196740071978));
#206401=CARTESIAN_POINT('Ctrl Pts',(-1.57637998831376,-6.58326908164322,
91.728098905178));
#206402=CARTESIAN_POINT('Ctrl Pts',(-1.40105187917827,-6.62037330003762,
91.7365238031583));
#206403=CARTESIAN_POINT('Ctrl Pts',(-1.22576258797132,-6.65746930349772,
91.7449468358525));
#206404=CARTESIAN_POINT('Ctrl Pts',(-1.04895976461049,-6.6876076117648,
91.7533698685466));
#206405=CARTESIAN_POINT('Ctrl Pts',(-0.871222033941675,-6.71068261561926,
91.7617929012408));
#206406=CARTESIAN_POINT('Ctrl Pts',(-0.693504414095105,-6.73375500856325,
91.7702149808784));
#206407=CARTESIAN_POINT('Ctrl Pts',(-0.514852428456964,-6.74976564742314,
91.778637060516));
#206408=CARTESIAN_POINT('Ctrl Pts',(-0.33585187311627,-6.75866055659879,
91.7870591401536));
#206409=CARTESIAN_POINT('Ctrl Pts',(-0.156846584344886,-6.76755570098844,
91.7954814425018));
#206410=CARTESIAN_POINT('Ctrl Pts',(0.0225069594262393,-6.76933472437189,
91.80390374485));
#206411=CARTESIAN_POINT('Ctrl Pts',(0.201620523660513,-6.76399572475019,
91.8123260471983));
#206412=CARTESIAN_POINT('Ctrl Pts',(0.380763828683505,-6.75865583861797,
91.8207497480219));
#206413=CARTESIAN_POINT('Ctrl Pts',(0.559666741463216,-6.74619558364666,
91.8291734488456));
#206414=CARTESIAN_POINT('Ctrl Pts',(0.73774334201908,-6.72666512926774,
91.8375971496692));
#206415=CARTESIAN_POINT('Ctrl Pts',(0.91594044863803,-6.70712145845184,
91.8460265508882));
#206416=CARTESIAN_POINT('Ctrl Pts',(1.09330979384886,-6.68049806409771,
91.8544559521072));
#206417=CARTESIAN_POINT('Ctrl Pts',(1.26927186134911,-6.64689686560483,
91.8628853533262));
#206418=CARTESIAN_POINT('Ctrl Pts',(1.44529671187075,-6.61328367825098,
91.8713177621438));
#206419=CARTESIAN_POINT('Ctrl Pts',(1.61991295711736,-6.57268779106609,
91.8797501709614));
#206420=CARTESIAN_POINT('Ctrl Pts',(1.79255296508185,-6.52526190029,91.8881825797791));
#206421=CARTESIAN_POINT('Ctrl Pts',(1.96535270460476,-6.47779212969989,
91.8966227905067));
#206422=CARTESIAN_POINT('Ctrl Pts',(2.13617223350927,-6.42347982387776,
91.9050630012343));
#206423=CARTESIAN_POINT('Ctrl Pts',(2.30445966206695,-6.36252738036594,
91.9135032119619));
#206424=CARTESIAN_POINT('Ctrl Pts',(2.4001786797552,-6.32785867059568,91.9183038597991));
#206425=CARTESIAN_POINT('Ctrl Pts',(2.49507886966456,-6.29104267349489,
91.9231045076362));
#206426=CARTESIAN_POINT('Ctrl Pts',(2.58906175767578,-6.25212349645629,
91.9279051554734));
#206427=CARTESIAN_POINT('Ctrl Pts',(2.74841398519276,-6.18613427559421,
91.9360448705063));
#206428=CARTESIAN_POINT('Ctrl Pts',(2.90544553379042,-6.11396437463473,
91.9441845855391));
#206429=CARTESIAN_POINT('Ctrl Pts',(3.05963911340726,-6.03580131347184,
91.952324300572));
#206430=CARTESIAN_POINT('Ctrl Pts',(3.21369783624446,-5.9577066132533,91.960456896659));
#206431=CARTESIAN_POINT('Ctrl Pts',(3.36492320624515,-5.87362935061182,
91.9685894927459));
#206432=CARTESIAN_POINT('Ctrl Pts',(3.51281707085037,-5.78380542780808,
91.9767220888329));
#206433=CARTESIAN_POINT('Ctrl Pts',(3.66060982727565,-5.69404291345678,
91.9848491250408));
#206434=CARTESIAN_POINT('Ctrl Pts',(3.80507530116462,-5.5985417501571,91.9929761612488));
#206435=CARTESIAN_POINT('Ctrl Pts',(3.94573920100857,-5.49758412010442,
92.0011031974568));
#206436=CARTESIAN_POINT('Ctrl Pts',(4.08633586096258,-5.39667474962609,
92.0092263487944));
#206437=CARTESIAN_POINT('Ctrl Pts',(4.2231342686755,-5.29031431943281,92.0173495001319));
#206438=CARTESIAN_POINT('Ctrl Pts',(4.35568845978136,-5.17882873257337,
92.0254726514695));
#206439=CARTESIAN_POINT('Ctrl Pts',(4.48820540217429,-5.06737447399248,
92.0335935201412));
#206440=CARTESIAN_POINT('Ctrl Pts',(4.61648022398761,-4.95079816347045,
92.0417143888128));
#206441=CARTESIAN_POINT('Ctrl Pts',(4.74009948392975,-4.82946641798542,
92.0498352574845));
#206442=CARTESIAN_POINT('Ctrl Pts',(4.86372542472989,-4.70812811526843,
92.0579565650389));
#206443=CARTESIAN_POINT('Ctrl Pts',(4.98269503684909,-4.58203411784084,
92.0660778725935));
#206444=CARTESIAN_POINT('Ctrl Pts',(5.09663111734629,-4.45158850902658,
92.074199180148));
#206445=CARTESIAN_POINT('Ctrl Pts',(5.15583626539749,-4.38380443616069,
92.0784192938647));
#206446=CARTESIAN_POINT('Ctrl Pts',(5.21368287901529,-4.31484593128487,
92.0826394075814));
#206447=CARTESIAN_POINT('Ctrl Pts',(5.27012224682327,-4.24477331591906,
92.0868595212981));
#206448=CARTESIAN_POINT('Ctrl Pts',(5.39027920574609,-4.0955917659986,92.0958439598239));
#206449=CARTESIAN_POINT('Ctrl Pts',(5.50399607223322,-3.94143273754319,
92.1048283983497));
#206450=CARTESIAN_POINT('Ctrl Pts',(5.6109066604396,-3.78285810569662,92.1138128368755));
#206451=CARTESIAN_POINT('Ctrl Pts',(5.7180017699404,-3.62400978349979,92.122812782006));
#206452=CARTESIAN_POINT('Ctrl Pts',(5.81826698801442,-3.46073082361633,
92.1318127271365));
#206453=CARTESIAN_POINT('Ctrl Pts',(5.91138078136888,-3.29360991279518,
92.140812672267));
#206454=CARTESIAN_POINT('Ctrl Pts',(6.00471399976738,-3.12609517725809,
92.1498338259992));
#206455=CARTESIAN_POINT('Ctrl Pts',(6.0908619575219,-2.95472058548155,92.1588549797314));
#206456=CARTESIAN_POINT('Ctrl Pts',(6.16954900714058,-2.78009964722323,
92.1678761334636));
#206457=CARTESIAN_POINT('Ctrl Pts',(6.24831612145253,-2.60530103078371,
92.1769064662908));
#206458=CARTESIAN_POINT('Ctrl Pts',(6.31960706899713,-2.42724968904704,
92.1859367991181));
#206459=CARTESIAN_POINT('Ctrl Pts',(6.38319474430584,-2.24657825509514,
92.1949671319453));
#206460=CARTESIAN_POINT('Ctrl Pts',(6.44687256689409,-2.06565068600097,
92.204010266938));
#206461=CARTESIAN_POINT('Ctrl Pts',(6.50282520144573,-1.88209582305477,
92.2130534019306));
#206462=CARTESIAN_POINT('Ctrl Pts',(6.55087502987781,-1.69656280252853,
92.2220965369233));
#206463=CARTESIAN_POINT('Ctrl Pts',(6.59288164995984,-1.53436419828303,
92.2300023203232));
#206464=CARTESIAN_POINT('Ctrl Pts',(6.62884906818787,-1.37065403521884,
92.2379081037231));
#206465=CARTESIAN_POINT('Ctrl Pts',(6.6586905907916,-1.20587255383952,92.245813887123));
#206466=CARTESIAN_POINT('Ctrl Pts',(6.69135405592223,-1.02550862795411,
92.2544672753513));
#206467=CARTESIAN_POINT('Ctrl Pts',(6.71670584184189,-0.843701615481007,
92.2631206635796));
#206468=CARTESIAN_POINT('Ctrl Pts',(6.73463390008914,-0.661056148727285,
92.2717740518079));
#206469=CARTESIAN_POINT('Ctrl Pts',(6.75254540050286,-0.478579368018239,
92.2804194480183));
#206470=CARTESIAN_POINT('Ctrl Pts',(6.76304681876529,-0.295265979047824,
92.2890648442287));
#206471=CARTESIAN_POINT('Ctrl Pts',(6.7660775779376,-0.111728283483179,
92.2977102404392));
#206472=CARTESIAN_POINT('Ctrl Pts',(6.76920512934841,0.0776709878100624,
92.3066317414816));
#206473=CARTESIAN_POINT('Ctrl Pts',(6.76437688126879,0.267308811449076,
92.315553242524));
#206474=CARTESIAN_POINT('Ctrl Pts',(6.75158428734202,0.456506966996586,
92.3244747435664));
#206475=CARTESIAN_POINT('Ctrl Pts',(6.73921121229972,0.639500579539438,
92.3331036739083));
#206476=CARTESIAN_POINT('Ctrl Pts',(6.71938787487004,0.822082567868297,
92.3417326042503));
#206477=CARTESIAN_POINT('Ctrl Pts',(6.69215941006571,1.00363909363324,92.3503615345923));
#206478=CARTESIAN_POINT('Ctrl Pts',(6.66354614134544,1.19442934556127,92.3594293209849));
#206479=CARTESIAN_POINT('Ctrl Pts',(6.62675488043951,1.38408676929546,92.3684971073775));
#206480=CARTESIAN_POINT('Ctrl Pts',(6.58189984786576,1.57190438407198,92.3775648937701));
#206481=CARTESIAN_POINT('Ctrl Pts',(6.53704481529201,1.7597219988485,92.3866326801627));
#206482=CARTESIAN_POINT('Ctrl Pts',(6.48412606752052,1.94569941665851,92.3957004665552));
#206483=CARTESIAN_POINT('Ctrl Pts',(6.42332063750698,2.12914090369261,92.4047682529478));
#206484=CARTESIAN_POINT('Ctrl Pts',(6.36682580422096,2.29957792264669,92.413193209081));
#206485=CARTESIAN_POINT('Ctrl Pts',(6.30354787053495,2.46775110860223,92.4216181652141));
#206486=CARTESIAN_POINT('Ctrl Pts',(6.23370034057328,2.63311015036146,92.4300431213473));
#206487=CARTESIAN_POINT('Ctrl Pts',(6.16383659832928,2.79850757354195,92.4384700329937));
#206488=CARTESIAN_POINT('Ctrl Pts',(6.08740034848315,2.96108924468914,92.44689694464));
#206489=CARTESIAN_POINT('Ctrl Pts',(6.00465273953959,3.12032602103366,92.4553238562864));
#206490=CARTESIAN_POINT('Ctrl Pts',(5.92187470107723,3.27962135494305,92.4637538668364));
#206491=CARTESIAN_POINT('Ctrl Pts',(5.83278082863023,3.43556904734347,92.4721838773864));
#206492=CARTESIAN_POINT('Ctrl Pts',(5.73767778366786,3.58766534821801,92.4806138879364));
#206493=CARTESIAN_POINT('Ctrl Pts',(5.64248713176929,3.73990175702425,92.4890516640358));
#206494=CARTESIAN_POINT('Ctrl Pts',(5.54127642379871,3.8882794047072,92.4974894401353));
#206495=CARTESIAN_POINT('Ctrl Pts',(5.4343957681525,4.03232335448018,92.5059272162347));
#206496=CARTESIAN_POINT('Ctrl Pts',(5.32745900804079,4.17644291670857,92.5143694215446));
#206497=CARTESIAN_POINT('Ctrl Pts',(5.21484656800135,4.31622398273164,92.5228116268544));
#206498=CARTESIAN_POINT('Ctrl Pts',(5.09694861405359,4.45122498035061,92.5312538321643));
#206499=CARTESIAN_POINT('Ctrl Pts',(4.97892628425141,4.58636839659401,92.5397049435363));
#206500=CARTESIAN_POINT('Ctrl Pts',(4.85560752589527,4.71672142683671,92.5481560549083));
#206501=CARTESIAN_POINT('Ctrl Pts',(4.72741983164075,4.84187884352859,92.5566071662803));
#206502=CARTESIAN_POINT('Ctrl Pts',(4.69144375668446,4.877004466393,92.5589789837777));
#206503=CARTESIAN_POINT('Ctrl Pts',(4.65508438413134,4.9117210944733,92.5613508012751));
#206504=CARTESIAN_POINT('Ctrl Pts',(4.61835163230548,4.94602033966514,92.5637226187725));
#206505=CARTESIAN_POINT('Ctrl Pts',(4.48956147683812,5.06627828117774,92.572038542003));
#206506=CARTESIAN_POINT('Ctrl Pts',(4.35594639022535,5.18161926967145,92.5803544652335));
#206507=CARTESIAN_POINT('Ctrl Pts',(4.21791411620621,5.29164336556314,92.588670388464));
#206508=CARTESIAN_POINT('Ctrl Pts',(4.07998670130477,5.40158387933824,92.5969799943286));
#206509=CARTESIAN_POINT('Ctrl Pts',(3.93764905253301,5.50621532877486,92.6052896001932));
#206510=CARTESIAN_POINT('Ctrl Pts',(3.79134424574178,5.60517598388139,92.6135992060579));
#206511=CARTESIAN_POINT('Ctrl Pts',(3.64514512056804,5.70406515588133,92.621902809573));
#206512=CARTESIAN_POINT('Ctrl Pts',(3.49498483646513,5.79729150392402,92.6302064130881));
#206513=CARTESIAN_POINT('Ctrl Pts',(3.34133787182237,5.88453483516969,92.6385100166033));
#206514=CARTESIAN_POINT('Ctrl Pts',(3.26151141794891,5.9298616385572,92.6428241091369));
#206515=CARTESIAN_POINT('Ctrl Pts',(3.18074432323989,5.97357415670657,92.6471382016706));
#206516=CARTESIAN_POINT('Ctrl Pts',(3.09910619832136,6.01563211736939,92.6514522942042));
#206517=CARTESIAN_POINT('Origin',(0.,0.,4.30282021618968));
#206518=CARTESIAN_POINT('',(3.09910619832144,6.01563211736935,95.0455663730808));
#206519=CARTESIAN_POINT('',(3.09910619832124,6.01563211736945,94.6514100603466));
#206520=CARTESIAN_POINT('',(3.09910619832133,6.0156321173694,4.30282021618968));
#206521=CARTESIAN_POINT('',(-6.76699933137488,-0.00202679626836213,93.6971797838099));
#206522=CARTESIAN_POINT('Ctrl Pts',(-6.7669985271066,-0.00446476618441742,
93.6971797838099));
#206523=CARTESIAN_POINT('Ctrl Pts',(-6.76686577009316,-0.205677209860647,
93.7066386602188));
#206524=CARTESIAN_POINT('Ctrl Pts',(-6.75775404271323,-0.406695906542261,
93.7160975366277));
#206525=CARTESIAN_POINT('Ctrl Pts',(-6.73974217978172,-0.606765481937798,
93.7255564130366));
#206526=CARTESIAN_POINT('Ctrl Pts',(-6.7220965388771,-0.802767189078906,
93.734822969034));
#206527=CARTESIAN_POINT('Ctrl Pts',(-6.69590926045183,-0.99785783025461,
93.7440895250314));
#206528=CARTESIAN_POINT('Ctrl Pts',(-6.66130632404342,-1.19133834709506,
93.7533560810288));
#206529=CARTESIAN_POINT('Ctrl Pts',(-6.62562615069218,-1.39084217819991,
93.7629111176435));
#206530=CARTESIAN_POINT('Ctrl Pts',(-6.58099798383396,-1.58863380155292,
93.7724661542581));
#206531=CARTESIAN_POINT('Ctrl Pts',(-6.5276158027552,-1.78396214411084,
93.7820211908727));
#206532=CARTESIAN_POINT('Ctrl Pts',(-6.47423362167641,-1.97929048666888,
93.7915762274874));
#206533=CARTESIAN_POINT('Ctrl Pts',(-6.41209751328803,-2.17215534877263,
93.801131264102));
#206534=CARTESIAN_POINT('Ctrl Pts',(-6.34145688008581,-2.3618242182712,
93.8106863007167));
#206535=CARTESIAN_POINT('Ctrl Pts',(-6.27748215676012,-2.5335952358799,
93.819339688945));
#206536=CARTESIAN_POINT('Ctrl Pts',(-6.20648337750343,-2.70287511116803,
93.8279930771732));
#206537=CARTESIAN_POINT('Ctrl Pts',(-6.12867281049903,-2.8690867156379,
93.8366464654015));
#206538=CARTESIAN_POINT('Ctrl Pts',(-6.05093410707278,-3.03514481190078,
93.8452918616119));
#206539=CARTESIAN_POINT('Ctrl Pts',(-5.96639629222485,-3.19814001496491,
93.8539372578223));
#206540=CARTESIAN_POINT('Ctrl Pts',(-5.87531981022229,-3.35751487377338,
93.8625826540327));
#206541=CARTESIAN_POINT('Ctrl Pts',(-5.78133465218575,-3.52197962870041,
93.8715041550751));
#206542=CARTESIAN_POINT('Ctrl Pts',(-5.68038637326566,-3.68258866056744,
93.8804256561175));
#206543=CARTESIAN_POINT('Ctrl Pts',(-5.57281380666296,-3.8387543912403,
93.8893471571598));
#206544=CARTESIAN_POINT('Ctrl Pts',(-5.46876896269455,-3.98979884052895,
93.8979760875018));
#206545=CARTESIAN_POINT('Ctrl Pts',(-5.35852758771888,-4.13668650649272,
93.9066050178438));
#206546=CARTESIAN_POINT('Ctrl Pts',(-5.24244181427066,-4.27891257494081,
93.9152339481857));
#206547=CARTESIAN_POINT('Ctrl Pts',(-5.12045207103073,-4.42837207421136,
93.9243017345784));
#206548=CARTESIAN_POINT('Ctrl Pts',(-4.99200812919201,-4.57268315854584,
93.933369520971));
#206549=CARTESIAN_POINT('Ctrl Pts',(-4.85756907180305,-4.71129618180204,
93.9424373073636));
#206550=CARTESIAN_POINT('Ctrl Pts',(-4.72313001441418,-4.84990920505814,
93.9515050937562));
#206551=CARTESIAN_POINT('Ctrl Pts',(-4.58269608808526,-4.982823862403,93.9605728801488));
#206552=CARTESIAN_POINT('Ctrl Pts',(-4.43677464882927,-5.10953224038228,
93.9696406665414));
#206553=CARTESIAN_POINT('Ctrl Pts',(-4.30119781988855,-5.22725805349268,
93.9780656226746));
#206554=CARTESIAN_POINT('Ctrl Pts',(-4.16094358476472,-5.33957486833351,
93.9864905788078));
#206555=CARTESIAN_POINT('Ctrl Pts',(-4.01647643407986,-5.44611843926307,
93.994915534941));
#206556=CARTESIAN_POINT('Ctrl Pts',(-3.87197575118233,-5.55268673997833,
94.0033424465874));
#206557=CARTESIAN_POINT('Ctrl Pts',(-3.72326046989799,-5.65347892814872,
94.0117693582337));
#206558=CARTESIAN_POINT('Ctrl Pts',(-3.57082524629212,-5.74817328030765,
94.0201962698801));
#206559=CARTESIAN_POINT('Ctrl Pts',(-3.4183339663168,-5.84290245526845,
94.0286262804302));
#206560=CARTESIAN_POINT('Ctrl Pts',(-3.26212029796605,-5.9315291481623,
94.0370562909802));
#206561=CARTESIAN_POINT('Ctrl Pts',(-3.10270507368833,-6.01377670234843,
94.0454863015303));
#206562=CARTESIAN_POINT('Ctrl Pts',(-2.9431429994403,-6.09610002126119,
94.0539240776297));
#206563=CARTESIAN_POINT('Ctrl Pts',(-2.78037377191445,-6.17203230892936,
94.0623618537292));
#206564=CARTESIAN_POINT('Ctrl Pts',(-2.61494087740784,-6.24134386231535,
94.0707996298286));
#206565=CARTESIAN_POINT('Ctrl Pts',(-2.44942114282594,-6.31069179915781,
94.0792418351385));
#206566=CARTESIAN_POINT('Ctrl Pts',(-2.28123526116274,-6.37341194966489,
94.0876840404485));
#206567=CARTESIAN_POINT('Ctrl Pts',(-2.11094413489262,-6.42932374821508,
94.0961262457584));
#206568=CARTESIAN_POINT('Ctrl Pts',(-1.94047336085457,-6.4852945306362,
94.1045773571304));
#206569=CARTESIAN_POINT('Ctrl Pts',(-1.76789322286463,-6.53444251764913,
94.1130284685024));
#206570=CARTESIAN_POINT('Ctrl Pts',(-1.59377817003713,-6.57663744969366,
94.1214795798744));
#206571=CARTESIAN_POINT('Ctrl Pts',(-1.54491251075818,-6.58847952273159,
94.1238513973717));
#206572=CARTESIAN_POINT('Ctrl Pts',(-1.49592600811817,-6.59977424701124,
94.1262232148689));
#206573=CARTESIAN_POINT('Ctrl Pts',(-1.44683147260946,-6.61051947201328,
94.1285950323662));
#206574=CARTESIAN_POINT('Ctrl Pts',(-1.27469195035897,-6.64819531269818,
94.1369113047703));
#206575=CARTESIAN_POINT('Ctrl Pts',(-1.10091298009481,-6.67917962337993,
94.1452275771744));
#206576=CARTESIAN_POINT('Ctrl Pts',(-0.926049399486271,-6.70333659528679,
94.1535438495785));
#206577=CARTESIAN_POINT('Ctrl Pts',(-0.751333666241069,-6.72747314244546,
94.1618530905645));
#206578=CARTESIAN_POINT('Ctrl Pts',(-0.575535492661531,-6.74479380444557,
94.1701623315505));
#206579=CARTESIAN_POINT('Ctrl Pts',(-0.399220451517156,-6.75521369248157,
94.1784715725366));
#206580=CARTESIAN_POINT('Ctrl Pts',(-0.223022158218122,-6.76562668093901,
94.186775311519));
#206581=CARTESIAN_POINT('Ctrl Pts',(-0.0463080254900932,-6.76914797997407,
94.1950790505015));
#206582=CARTESIAN_POINT('Ctrl Pts',(0.130350469610198,-6.76574443465554,
94.203382789484));
#206583=CARTESIAN_POINT('Ctrl Pts',(0.306924364736936,-6.76234251926057,
94.2116825518895));
#206584=CARTESIAN_POINT('Ctrl Pts',(0.48344232817631,-6.75202237510446,
94.219982314295));
#206585=CARTESIAN_POINT('Ctrl Pts',(0.659331865264326,-6.73480292892428,
94.2282820767005));
#206586=CARTESIAN_POINT('Ctrl Pts',(0.835169394121983,-6.71758857430861,
94.2365793849751));
#206587=CARTESIAN_POINT('Ctrl Pts',(1.01037852113831,-6.69347901789371,
94.2448766932496));
#206588=CARTESIAN_POINT('Ctrl Pts',(1.18439063156209,-6.66254514670392,
94.2531740015242));
#206589=CARTESIAN_POINT('Ctrl Pts',(1.35842032338573,-6.63160815009512,
94.2614721481214));
#206590=CARTESIAN_POINT('Ctrl Pts',(1.53125241308379,-6.59384551445604,
94.2697702947187));
#206591=CARTESIAN_POINT('Ctrl Pts',(1.70232667151901,-6.54937958156611,
94.2780684413159));
#206592=CARTESIAN_POINT('Ctrl Pts',(1.87341813254701,-6.50490917734692,
94.286367422344));
#206593=CARTESIAN_POINT('Ctrl Pts',(2.04275107291088,-6.45373421938314,
94.294666403372));
#206594=CARTESIAN_POINT('Ctrl Pts',(2.20977875475255,-6.39602742763384,
94.3029653844001));
#206595=CARTESIAN_POINT('Ctrl Pts',(2.37685099038889,-6.33830524288786,
94.3112665791396));
#206596=CARTESIAN_POINT('Ctrl Pts',(2.54161641293948,-6.2740478653736,94.3195677738792));
#206597=CARTESIAN_POINT('Ctrl Pts',(2.70354647290647,-6.20347688549212,
94.3278689686187));
#206598=CARTESIAN_POINT('Ctrl Pts',(2.86554664101356,-6.132875351678,94.3361737573872));
#206599=CARTESIAN_POINT('Ctrl Pts',(3.02470868112125,-6.05595490657058,
94.3444785461557));
#206600=CARTESIAN_POINT('Ctrl Pts',(3.18052676064206,-5.97298405529763,
94.3527833349242));
#206601=CARTESIAN_POINT('Ctrl Pts',(3.33652956109664,-5.88991484282572,
94.3610979689452));
#206602=CARTESIAN_POINT('Ctrl Pts',(3.48918017297209,-5.80078105698932,
94.3694126029662));
#206603=CARTESIAN_POINT('Ctrl Pts',(3.63799896426392,-5.70589629558886,
94.3777272369872));
#206604=CARTESIAN_POINT('Ctrl Pts',(3.78691185499685,-5.61095153771256,
94.386047128425));
#206605=CARTESIAN_POINT('Ctrl Pts',(3.93198780781265,-5.51024875057221,
94.3943670198628));
#206606=CARTESIAN_POINT('Ctrl Pts',(4.07277854115722,-5.40414322114887,
94.4026869113006));
#206607=CARTESIAN_POINT('Ctrl Pts',(4.21377980229941,-5.29787902955442,
94.4110192436738));
#206608=CARTESIAN_POINT('Ctrl Pts',(4.35048276869771,-5.18619617025387,
94.419351576047));
#206609=CARTESIAN_POINT('Ctrl Pts',(4.48247340901378,-5.06948923832415,
94.4276839084202));
#206610=CARTESIAN_POINT('Ctrl Pts',(4.58184713693827,-4.98162237994152,
94.4339571936187));
#206611=CARTESIAN_POINT('Ctrl Pts',(4.67855047776066,-4.89090850201358,
94.4402304788172));
#206612=CARTESIAN_POINT('Ctrl Pts',(4.77242149879349,-4.79752874278558,
94.4465037640157));
#206613=CARTESIAN_POINT('Ctrl Pts',(4.89317556303413,-4.67740662926717,
94.4545736100184));
#206614=CARTESIAN_POINT('Ctrl Pts',(5.00961438061434,-4.55250058113334,
94.4626434560212));
#206615=CARTESIAN_POINT('Ctrl Pts',(5.12132461771142,-4.42315760063137,
94.4707133020239));
#206616=CARTESIAN_POINT('Ctrl Pts',(5.2328943091212,-4.29397735005069,94.478772995134));
#206617=CARTESIAN_POINT('Ctrl Pts',(5.33974701646822,-4.16037155295409,
94.486832688244));
#206618=CARTESIAN_POINT('Ctrl Pts',(5.4415037112129,-4.022726234888,94.494892381354));
#206619=CARTESIAN_POINT('Ctrl Pts',(5.54315471546799,-3.88522388334705,
94.5029437031927));
#206620=CARTESIAN_POINT('Ctrl Pts',(5.63972002037714,-3.74369065775069,
94.5109950250313));
#206621=CARTESIAN_POINT('Ctrl Pts',(5.73085868944113,-3.59854799629755,
94.5190463468699));
#206622=CARTESIAN_POINT('Ctrl Pts',(5.82192266810941,-3.45352428284892,
94.527091070451));
#206623=CARTESIAN_POINT('Ctrl Pts',(5.9075686650232,-3.30489733531461,94.535135794032));
#206624=CARTESIAN_POINT('Ctrl Pts',(5.98749723392353,-3.15312002209845,
94.543180517613));
#206625=CARTESIAN_POINT('Ctrl Pts',(6.06737779578135,-3.00143387002813,
94.5512204093374));
#206626=CARTESIAN_POINT('Ctrl Pts',(6.1415475923023,-2.84660144832157,94.5592603010618));
#206627=CARTESIAN_POINT('Ctrl Pts',(6.20975164025075,-2.68910274374244,
94.5673001927862));
#206628=CARTESIAN_POINT('Ctrl Pts',(6.27942430820883,-2.5282126605576,94.5755132054062));
#206629=CARTESIAN_POINT('Ctrl Pts',(6.34287118327832,-2.36454050467807,
94.5837262180261));
#206630=CARTESIAN_POINT('Ctrl Pts',(6.39987084133188,-2.19862279945196,
94.5919392306461));
#206631=CARTESIAN_POINT('Ctrl Pts',(6.45564954348077,-2.0362591190885,94.5999763171886));
#206632=CARTESIAN_POINT('Ctrl Pts',(6.50525432077201,-1.87174548789571,
94.6080134037312));
#206633=CARTESIAN_POINT('Ctrl Pts',(6.54852718205247,-1.70560275149872,
94.6160504902738));
#206634=CARTESIAN_POINT('Ctrl Pts',(6.59180418474718,-1.53944411446844,
94.624088346003));
#206635=CARTESIAN_POINT('Ctrl Pts',(6.62874797049889,-1.37165642332735,
94.6321262017322));
#206636=CARTESIAN_POINT('Ctrl Pts',(6.65925113857969,-1.20277315954635,
94.6401640574613));
#206637=CARTESIAN_POINT('Ctrl Pts',(6.68976326965166,-1.03384027143787,
94.6482042750183));
#206638=CARTESIAN_POINT('Ctrl Pts',(6.7138309497305,-0.863811537386868,
94.6562444925752));
#206639=CARTESIAN_POINT('Ctrl Pts',(6.73139837525425,-0.693227894436233,
94.6642847101322));
#206640=CARTESIAN_POINT('Ctrl Pts',(6.74962950937001,-0.516199492159291,
94.6726286922599));
#206641=CARTESIAN_POINT('Ctrl Pts',(6.76085958200391,-0.338573875059958,
94.6809726743877));
#206642=CARTESIAN_POINT('Ctrl Pts',(6.76508549784856,-0.160957158272201,
94.6893166565154));
#206643=CARTESIAN_POINT('Ctrl Pts',(6.76916465736336,0.0104913387888412,
94.6973708713505));
#206644=CARTESIAN_POINT('Ctrl Pts',(6.76671805279467,0.181931176453537,
94.7054250861855));
#206645=CARTESIAN_POINT('Ctrl Pts',(6.75779593370413,0.352821652413778,
94.7134793010206));
#206646=CARTESIAN_POINT('Ctrl Pts',(6.74886713788282,0.523840011636674,
94.7215395431036));
#206647=CARTESIAN_POINT('Ctrl Pts',(6.73345321223899,0.694307821062776,
94.7295997851866));
#206648=CARTESIAN_POINT('Ctrl Pts',(6.71165577000229,0.863693131265336,
94.7376600272696));
#206649=CARTESIAN_POINT('Ctrl Pts',(6.68982785344615,1.03331525375057,94.745731538124));
#206650=CARTESIAN_POINT('Ctrl Pts',(6.66159867532509,1.20185149252047,94.7538030489783));
#206651=CARTESIAN_POINT('Ctrl Pts',(6.62712018020191,1.36878307892839,94.7618745598326));
#206652=CARTESIAN_POINT('Ctrl Pts',(6.62350647392875,1.38627925208894,94.7627205384435));
#206653=CARTESIAN_POINT('Ctrl Pts',(6.61982416158567,1.40375781456,94.7635665170543));
#206654=CARTESIAN_POINT('Ctrl Pts',(6.61607344889682,1.42121818128059,94.7644124956652));
#206655=CARTESIAN_POINT('Ctrl Pts',(6.57958530667037,1.5910782577725,94.7726424483258));
#206656=CARTESIAN_POINT('Ctrl Pts',(6.53649789669645,1.75978186392105,94.7808724009865));
#206657=CARTESIAN_POINT('Ctrl Pts',(6.48689578226858,1.92677764933739,94.7891023536471));
#206658=CARTESIAN_POINT('Ctrl Pts',(6.43735351517776,2.0935719463057,94.797322376474));
#206659=CARTESIAN_POINT('Ctrl Pts',(6.38131229709004,2.25866218522143,94.8055423993008));
#206660=CARTESIAN_POINT('Ctrl Pts',(6.31890785907017,2.42150623963295,94.8137624221277));
#206661=CARTESIAN_POINT('Ctrl Pts',(6.25656618174205,2.58418652034779,94.8219741780054));
#206662=CARTESIAN_POINT('Ctrl Pts',(6.18787415730906,2.74462478290262,94.8301859338831));
#206663=CARTESIAN_POINT('Ctrl Pts',(6.11301759282562,2.90229304340627,94.8383976897607));
#206664=CARTESIAN_POINT('Ctrl Pts',(6.03432991560557,3.0680306681019,94.8470297182324));
#206665=CARTESIAN_POINT('Ctrl Pts',(5.94883021529023,3.23070692169701,94.8556617467041));
#206666=CARTESIAN_POINT('Ctrl Pts',(5.85679275852635,3.38972972133078,94.8642937751757));
#206667=CARTESIAN_POINT('Ctrl Pts',(5.76936430980571,3.54078905273825,94.8724935330257));
#206668=CARTESIAN_POINT('Ctrl Pts',(5.67603708184902,3.68855153338375,94.8806932908757));
#206669=CARTESIAN_POINT('Ctrl Pts',(5.57709418534632,3.83253303283563,94.8888930487256));
#206670=CARTESIAN_POINT('Ctrl Pts',(5.47818390360759,3.97646707135008,94.8970901036714));
#206671=CARTESIAN_POINT('Ctrl Pts',(5.37366184258913,4.11662231548417,94.9052871586173));
#206672=CARTESIAN_POINT('Ctrl Pts',(5.26385501927317,4.25254269068197,94.9134842135631));
#206673=CARTESIAN_POINT('Ctrl Pts',(5.1540644262943,4.3884429757484,94.9216800569178));
#206674=CARTESIAN_POINT('Ctrl Pts',(5.03899085257448,4.52010936008753,94.9298759002725));
#206675=CARTESIAN_POINT('Ctrl Pts',(4.91900229758501,4.6471179666922,94.9380717436273));
#206676=CARTESIAN_POINT('Ctrl Pts',(4.79900966164792,4.77413089300445,94.946267865732));
#206677=CARTESIAN_POINT('Ctrl Pts',(4.67410195871594,4.89648546630697,94.9544639878367));
#206678=CARTESIAN_POINT('Ctrl Pts',(4.54468484794874,5.01379383629055,94.9626601099415));
#206679=CARTESIAN_POINT('Ctrl Pts',(4.41519628569744,5.13116697249464,94.9708607571441));
#206680=CARTESIAN_POINT('Ctrl Pts',(4.28119360827926,5.24348809903702,94.9790614043466));
#206681=CARTESIAN_POINT('Ctrl Pts',(4.14311689527926,5.35040852571573,94.9872620515492));
#206682=CARTESIAN_POINT('Ctrl Pts',(4.00499597758547,5.45736318253085,94.9954653241553));
#206683=CARTESIAN_POINT('Ctrl Pts',(3.86279871414833,5.55891348177531,95.0036685967615));
#206684=CARTESIAN_POINT('Ctrl Pts',(3.71699506866281,5.65475345700733,95.0118718693676));
#206685=CARTESIAN_POINT('Ctrl Pts',(3.57106337376203,5.75067760196464,95.0200823463496));
#206686=CARTESIAN_POINT('Ctrl Pts',(3.42151927671942,5.84088121963626,95.0282928233316));
#206687=CARTESIAN_POINT('Ctrl Pts',(3.26885886520031,5.92510343533354,95.0365033003136));
#206688=CARTESIAN_POINT('Ctrl Pts',(3.21268785259049,5.95609278675008,95.0395243245694));
#206689=CARTESIAN_POINT('Ctrl Pts',(3.15609515520393,5.98627280382349,95.0425453488251));
#206690=CARTESIAN_POINT('Ctrl Pts',(3.09910619832144,6.01563211736935,95.0455663730808));
#206691=CARTESIAN_POINT('Ctrl Pts',(3.09910619832149,6.01563211736932,93.0457552630241));
#206692=CARTESIAN_POINT('Ctrl Pts',(2.93375330764842,6.10081787314646,93.0545047109265));
#206693=CARTESIAN_POINT('Ctrl Pts',(2.76488627843086,6.17918207037032,93.0632541588287));
#206694=CARTESIAN_POINT('Ctrl Pts',(2.59307866646717,6.25045854553991,93.072003606731));
#206695=CARTESIAN_POINT('Ctrl Pts',(2.42127244185387,6.32173444515033,93.0807529839814));
#206696=CARTESIAN_POINT('Ctrl Pts',(2.2465259467247,6.38592262741836,93.0895023612317));
#206697=CARTESIAN_POINT('Ctrl Pts',(2.06943269687121,6.44280508110562,93.098251738482));
#206698=CARTESIAN_POINT('Ctrl Pts',(1.89234081822077,6.49968709436166,93.1070010479873));
#206699=CARTESIAN_POINT('Ctrl Pts',(1.7129024940559,6.54926340459544,93.1157503574927));
#206700=CARTESIAN_POINT('Ctrl Pts',(1.5317271662506,6.59136563150383,93.124499666998));
#206701=CARTESIAN_POINT('Ctrl Pts',(1.3505531810734,6.63346754640709,93.1332489116653));
#206702=CARTESIAN_POINT('Ctrl Pts',(1.1676424971443,6.66809542395774,93.1419981563325));
#206703=CARTESIAN_POINT('Ctrl Pts',(0.983616340614511,6.69513165624666,
93.1507474009997));
#206704=CARTESIAN_POINT('Ctrl Pts',(0.799591486713998,6.72216769715959,
93.1594965837354));
#206705=CARTESIAN_POINT('Ctrl Pts',(0.614451459526872,6.7416121586937,93.1682457664711));
#206706=CARTESIAN_POINT('Ctrl Pts',(0.428825047910443,6.75339900185711,
93.1769949492068));
#206707=CARTESIAN_POINT('Ctrl Pts',(0.243199888597115,6.76518576550221,
93.1857440729174));
#206708=CARTESIAN_POINT('Ctrl Pts',(0.0570886373918941,6.76931499599834,
93.1944931966279));
#206709=CARTESIAN_POINT('Ctrl Pts',(-0.128876626811264,6.76577266947847,
93.2032423203385));
#206710=CARTESIAN_POINT('Ctrl Pts',(-0.314840698188214,6.76223036567993,
93.21199138793));
#206711=CARTESIAN_POINT('Ctrl Pts',(-0.500658497951248,6.75101660879223,
93.2207404555215));
#206712=CARTESIAN_POINT('Ctrl Pts',(-0.685698951926153,6.73216948296219,
93.2294895231131));
#206713=CARTESIAN_POINT('Ctrl Pts',(-0.870738280459569,6.71332247176296,
93.2382385374916));
#206714=CARTESIAN_POINT('Ctrl Pts',(-1.05499998761201,6.68684221356194,
93.2469875518701));
#206715=CARTESIAN_POINT('Ctrl Pts',(-1.23785829161348,6.65281863948535,
93.2557365662486));
#206716=CARTESIAN_POINT('Ctrl Pts',(-1.43007412917329,6.61705395368877,
93.2649332999478));
#206717=CARTESIAN_POINT('Ctrl Pts',(-1.62073882535714,6.57295372727809,
93.274130033647));
#206718=CARTESIAN_POINT('Ctrl Pts',(-1.80913696091433,6.52068343478302,
93.2833267673462));
#206719=CARTESIAN_POINT('Ctrl Pts',(-1.98838356186031,6.47095219815223,
93.2920767650599));
#206720=CARTESIAN_POINT('Ctrl Pts',(-2.16557827572453,6.41382586850918,
93.3008267627735));
#206721=CARTESIAN_POINT('Ctrl Pts',(-2.3401191862162,6.34949849943307,93.3095767604872));
#206722=CARTESIAN_POINT('Ctrl Pts',(-2.51465655691025,6.2851724349558,93.3183265807455));
#206723=CARTESIAN_POINT('Ctrl Pts',(-2.68653996295261,6.21364572242404,
93.3270764010038));
#206724=CARTESIAN_POINT('Ctrl Pts',(-2.85518555379927,6.13516132252249,
93.3358262212621));
#206725=CARTESIAN_POINT('Ctrl Pts',(-3.0238279485863,6.05667841000536,93.3445758756996));
#206726=CARTESIAN_POINT('Ctrl Pts',(-3.18923239109224,5.97123819492111,
93.3533255301371));
#206727=CARTESIAN_POINT('Ctrl Pts',(-3.35083705967644,5.87913088810744,
93.3620751845746));
#206728=CARTESIAN_POINT('Ctrl Pts',(-3.5124388804233,5.78702520443145,93.3708246848236));
#206729=CARTESIAN_POINT('Ctrl Pts',(-3.67024081223607,5.68825280605837,
93.3795741850725));
#206730=CARTESIAN_POINT('Ctrl Pts',(-3.82370687544305,5.58314917682571,
93.3883236853214));
#206731=CARTESIAN_POINT('Ctrl Pts',(-3.97717043817728,5.47804726008085,
93.3970730430119));
#206732=CARTESIAN_POINT('Ctrl Pts',(-4.12629803722381,5.36661448084297,
93.4058224007024));
#206733=CARTESIAN_POINT('Ctrl Pts',(-4.27058317206837,5.24922931204634,
93.4145717583928));
#206734=CARTESIAN_POINT('Ctrl Pts',(-4.4148661477477,5.13184589986847,93.4233209851529));
#206735=CARTESIAN_POINT('Ctrl Pts',(-4.55430658194353,5.00851045723089,
93.432070211913));
#206736=CARTESIAN_POINT('Ctrl Pts',(-4.6884308900179,4.87964187103172,93.4408194386731));
#206737=CARTESIAN_POINT('Ctrl Pts',(-4.82255336917762,4.75077504208035,
93.449568546129));
#206738=CARTESIAN_POINT('Ctrl Pts',(-4.95135966065043,4.6163754190819,93.4583176535849));
#206739=CARTESIAN_POINT('Ctrl Pts',(-5.07441230869137,4.47689945401966,
93.4670667610408));
#206740=CARTESIAN_POINT('Ctrl Pts',(-5.19746344226328,4.33742520555623,
93.4758157608172));
#206741=CARTESIAN_POINT('Ctrl Pts',(-5.31476088454695,4.19287495491429,
93.4845647605936));
#206742=CARTESIAN_POINT('Ctrl Pts',(-5.42590627628796,4.04373961586783,
93.4933137603699));
#206743=CARTESIAN_POINT('Ctrl Pts',(-5.53706380672614,3.89458798906811,
93.5020637156646));
#206744=CARTESIAN_POINT('Ctrl Pts',(-5.64206777071813,3.7408505015536,93.5108136709593));
#206745=CARTESIAN_POINT('Ctrl Pts',(-5.7405614816396,3.58304938223237,93.519563626254));
#206746=CARTESIAN_POINT('Ctrl Pts',(-5.83905138951835,3.42525435593364,
93.5283132436952));
#206747=CARTESIAN_POINT('Ctrl Pts',(-5.93103139557603,3.26339625497273,
93.5370628611363));
#206748=CARTESIAN_POINT('Ctrl Pts',(-6.01618907820797,3.09802485065101,
93.5458124785774));
#206749=CARTESIAN_POINT('Ctrl Pts',(-6.10134392544937,2.93265895249737,
93.5545618046932));
#206750=CARTESIAN_POINT('Ctrl Pts',(-6.17967677261788,2.76378023986132,
93.5633111308091));
#206751=CARTESIAN_POINT('Ctrl Pts',(-6.25092157009184,2.59196229227214,
93.572060456925));
#206752=CARTESIAN_POINT('Ctrl Pts',(-6.32216437407717,2.42014915229186,
93.5808095382274));
#206753=CARTESIAN_POINT('Ctrl Pts',(-6.38631941548889,2.24539720662942,
93.5895586195299));
#206754=CARTESIAN_POINT('Ctrl Pts',(-6.4431688103751,2.06829994947774,93.5983077008324));
#206755=CARTESIAN_POINT('Ctrl Pts',(-6.50002334524544,1.89118668024543,
93.6070575731747));
#206756=CARTESIAN_POINT('Ctrl Pts',(-6.5495708241107,1.71172794807803,93.615807445517));
#206757=CARTESIAN_POINT('Ctrl Pts',(-6.59164294296059,1.53053334250447,
93.6245573178594));
#206758=CARTESIAN_POINT('Ctrl Pts',(-6.6337121408211,1.34935131693718,93.6333065827143));
#206759=CARTESIAN_POINT('Ctrl Pts',(-6.66830695239667,1.16643393829894,
93.6420558475692));
#206760=CARTESIAN_POINT('Ctrl Pts',(-6.69530988153967,0.982402458342421,
93.6508051124241));
#206761=CARTESIAN_POINT('Ctrl Pts',(-6.72231419690466,0.79836153094851,
93.6595548264311));
#206762=CARTESIAN_POINT('Ctrl Pts',(-6.74172580829264,0.613206671363948,
93.6683045404381));
#206763=CARTESIAN_POINT('Ctrl Pts',(-6.7534787802817,0.427566795114886,
93.6770542544452));
#206764=CARTESIAN_POINT('Ctrl Pts',(-6.76248992368207,0.285234494207059,
93.6837627642334));
#206765=CARTESIAN_POINT('Ctrl Pts',(-6.76699999999992,0.142617266094214,
93.6904712740216));
#206766=CARTESIAN_POINT('Ctrl Pts',(-6.767,3.81860140813756E-12,93.6971797838099));
#206767=CARTESIAN_POINT('',(-6.76699756073415,0.00574569560949348,93.3028202161555));
#206768=CARTESIAN_POINT('Ctrl Pts',(3.09910619832136,6.01563211736939,92.6514522942042));
#206769=CARTESIAN_POINT('Ctrl Pts',(2.94207261405183,6.09653197042874,92.6597505912818));
#206770=CARTESIAN_POINT('Ctrl Pts',(2.78181483905431,6.17130714984468,92.6680488883594));
#206771=CARTESIAN_POINT('Ctrl Pts',(2.61884743168782,6.23970569254209,92.6763471854369));
#206772=CARTESIAN_POINT('Ctrl Pts',(2.4508680467396,6.3102077967317,92.6849006923113));
#206773=CARTESIAN_POINT('Ctrl Pts',(2.28001003531816,6.37393458933078,92.6934541991857));
#206774=CARTESIAN_POINT('Ctrl Pts',(2.10686043388856,6.43066311604915,92.7020077060601));
#206775=CARTESIAN_POINT('Ctrl Pts',(1.93887427303521,6.48569995896189,92.7103061414581));
#206776=CARTESIAN_POINT('Ctrl Pts',(1.76873158870496,6.53414984324859,92.7186045768561));
#206777=CARTESIAN_POINT('Ctrl Pts',(1.59698493863653,6.57585949559205,92.7269030122542));
#206778=CARTESIAN_POINT('Ctrl Pts',(1.42520530402759,6.61757715841907,92.7352030413955));
#206779=CARTESIAN_POINT('Ctrl Pts',(1.25182142793851,6.65255192688433,92.7435030705369));
#206780=CARTESIAN_POINT('Ctrl Pts',(1.07739734666933,6.68068139918301,92.7518030996783));
#206781=CARTESIAN_POINT('Ctrl Pts',(0.902910777742995,6.70882094890225,
92.760106102316));
#206782=CARTESIAN_POINT('Ctrl Pts',(0.727383604427435,6.73011025950068,
92.7684091049538));
#206783=CARTESIAN_POINT('Ctrl Pts',(0.551386481042489,6.74449864322943,
92.7767121075915));
#206784=CARTESIAN_POINT('Ctrl Pts',(0.366057091468037,6.75964997253599,
92.7854553778274));
#206785=CARTESIAN_POINT('Ctrl Pts',(0.180207001970892,6.76714860824585,
92.7941986480633));
#206786=CARTESIAN_POINT('Ctrl Pts',(-0.00549659759097798,6.76699776765258,
92.8029419182992));
#206787=CARTESIAN_POINT('Ctrl Pts',(-0.182160250272311,6.76685426989462,
92.8112595710528));
#206788=CARTESIAN_POINT('Ctrl Pts',(-0.358690993949632,6.75978841471152,
92.8195772238063));
#206789=CARTESIAN_POINT('Ctrl Pts',(-0.534519146364061,6.7458563787091,
92.82789487656));
#206790=CARTESIAN_POINT('Ctrl Pts',(-0.710474373024073,6.73191427376755,
92.8362185406345));
#206791=CARTESIAN_POINT('Ctrl Pts',(-0.885725651466783,6.71109613397475,
92.844542204709));
#206792=CARTESIAN_POINT('Ctrl Pts',(-1.05971193905513,6.68350952765267,
92.8528658687835));
#206793=CARTESIAN_POINT('Ctrl Pts',(-1.23392922408229,6.65588629525221,
92.861200583988));
#206794=CARTESIAN_POINT('Ctrl Pts',(-1.40687782424718,6.62147671746085,
92.8695352991925));
#206795=CARTESIAN_POINT('Ctrl Pts',(-1.57800942395164,6.58043883475257,
92.877870014397));
#206796=CARTESIAN_POINT('Ctrl Pts',(-1.60375249315826,6.57426556776695,
92.879123793072));
#206797=CARTESIAN_POINT('Ctrl Pts',(-1.62945447887022,6.56794240090994,
92.880377571747));
#206798=CARTESIAN_POINT('Ctrl Pts',(-1.65511355105345,6.56146996740206,
92.881631350422));
#206799=CARTESIAN_POINT('Ctrl Pts',(-1.82026611364065,6.51981066762819,
92.8897011964247));
#206800=CARTESIAN_POINT('Ctrl Pts',(-1.98414975799722,6.47183494238821,
92.8977710424275));
#206801=CARTESIAN_POINT('Ctrl Pts',(-2.14623193028149,6.41763020915355,
92.9058408884303));
#206802=CARTESIAN_POINT('Ctrl Pts',(-2.30811018257692,6.36349367236789,
92.9139005815403));
#206803=CARTESIAN_POINT('Ctrl Pts',(-2.46819112315017,6.30314383765067,
92.9219602746503));
#206804=CARTESIAN_POINT('Ctrl Pts',(-2.62595177941827,6.23671918977999,
92.9300199677604));
#206805=CARTESIAN_POINT('Ctrl Pts',(-2.78354857618758,6.17036353445642,
92.938071289599));
#206806=CARTESIAN_POINT('Ctrl Pts',(-2.93882954361198,6.09794576581048,
92.9461226114376));
#206807=CARTESIAN_POINT('Ctrl Pts',(-3.09128638965204,6.01965426392182,
92.9541739332763));
#206808=CARTESIAN_POINT('Ctrl Pts',(-3.24361829353213,5.94142692385735,
92.9622186568573));
#206809=CARTESIAN_POINT('Ctrl Pts',(-3.39313035230538,5.85733560086816,
92.9702633804384));
#206810=CARTESIAN_POINT('Ctrl Pts',(-3.53933390940917,5.76761688028135,
92.9783081040194));
#206811=CARTESIAN_POINT('Ctrl Pts',(-3.68544965310094,5.67795204694007,
92.9863479957438));
#206812=CARTESIAN_POINT('Ctrl Pts',(-3.8282605337627,5.58266673908945,92.9943878874682));
#206813=CARTESIAN_POINT('Ctrl Pts',(-3.96730228755121,5.48204355684912,
93.0024277791926));
#206814=CARTESIAN_POINT('Ctrl Pts',(-4.10933799122855,5.37925368181994,
93.0106407918125));
#206815=CARTESIAN_POINT('Ctrl Pts',(-4.24744005283929,5.27089362854747,
93.0188538044325));
#206816=CARTESIAN_POINT('Ctrl Pts',(-4.38114420888447,5.1573117436275,93.0270668170525));
#206817=CARTESIAN_POINT('Ctrl Pts',(-4.51198436741841,5.04616282897079,
93.035103903595));
#206818=CARTESIAN_POINT('Ctrl Pts',(-4.63861283387288,4.93001378566132,
93.0431409901376));
#206819=CARTESIAN_POINT('Ctrl Pts',(-4.76062789442236,4.80923185663238,
93.0511780766801));
#206820=CARTESIAN_POINT('Ctrl Pts',(-4.88265463238121,4.6884383682105,93.0592159324093));
#206821=CARTESIAN_POINT('Ctrl Pts',(-5.00006681965695,4.56301137397376,
93.0672537881385));
#206822=CARTESIAN_POINT('Ctrl Pts',(-5.1124997964976,4.43335480542805,93.0752916438677));
#206823=CARTESIAN_POINT('Ctrl Pts',(-5.22496581042372,4.30366013885046,
93.0833318614246));
#206824=CARTESIAN_POINT('Ctrl Pts',(-5.33244945706255,4.16973370631207,
93.0913720789815));
#206825=CARTESIAN_POINT('Ctrl Pts',(-5.43462664060732,4.03201218713451,
93.0994122965384));
#206826=CARTESIAN_POINT('Ctrl Pts',(-5.54066414361326,3.88908746072163,
93.1077562786662));
#206827=CARTESIAN_POINT('Ctrl Pts',(-5.64098612335692,3.74207564227954,
93.116100260794));
#206828=CARTESIAN_POINT('Ctrl Pts',(-5.73528054026139,3.59149636286869,
93.1244442429217));
#206829=CARTESIAN_POINT('Ctrl Pts',(-5.82630032911838,3.44614635522084,
93.1324984577568));
#206830=CARTESIAN_POINT('Ctrl Pts',(-5.91170405792819,3.29747286424898,
93.1405526725918));
#206831=CARTESIAN_POINT('Ctrl Pts',(-5.99125894798247,3.14596649985659,
93.1486068874269));
#206832=CARTESIAN_POINT('Ctrl Pts',(-6.07087337171676,2.99434675800357,
93.1566671295099));
#206833=CARTESIAN_POINT('Ctrl Pts',(-6.14463008186374,2.83989025648101,
93.1647273715929));
#206834=CARTESIAN_POINT('Ctrl Pts',(-6.21234493611154,2.68310629583871,
93.1727876136759));
#206835=CARTESIAN_POINT('Ctrl Pts',(-6.2801544603705,2.52610314046481,93.1808591245303));
#206836=CARTESIAN_POINT('Ctrl Pts',(-6.34190514192247,2.36676637884349,
93.1889306353846));
#206837=CARTESIAN_POINT('Ctrl Pts',(-6.39746284724739,2.20561966759669,
93.1970021462389));
#206838=CARTESIAN_POINT('Ctrl Pts',(-6.40328587483431,2.1887298097517,93.1978481248498));
#206839=CARTESIAN_POINT('Ctrl Pts',(-6.40904091765605,2.17182007727671,
93.1986941034606));
#206840=CARTESIAN_POINT('Ctrl Pts',(-6.41472785398784,2.15489107828506,
93.1995400820715));
#206841=CARTESIAN_POINT('Ctrl Pts',(-6.48413205695589,1.94828709794964,
93.2098645288014));
#206842=CARTESIAN_POINT('Ctrl Pts',(-6.54357511398344,1.73825647702735,
93.2201889755314));
#206843=CARTESIAN_POINT('Ctrl Pts',(-6.592774769044,1.52565062994672,93.2305134222613));
#206844=CARTESIAN_POINT('Ctrl Pts',(-6.64160012784474,1.31466222455912,
93.2407593236887));
#206845=CARTESIAN_POINT('Ctrl Pts',(-6.68033733735106,1.10113750658047,
93.251005225116));
#206846=CARTESIAN_POINT('Ctrl Pts',(-6.70875668730291,0.885930420839292,
93.2612511265434));
#206847=CARTESIAN_POINT('Ctrl Pts',(-6.7367317048082,0.674088066912383,
93.2713368347764));
#206848=CARTESIAN_POINT('Ctrl Pts',(-6.75470895760259,0.460615460068659,
93.2814225430094));
#206849=CARTESIAN_POINT('Ctrl Pts',(-6.76251438321489,0.246349785491624,
93.2915082512425));
#206850=CARTESIAN_POINT('Ctrl Pts',(-6.76543252899164,0.166244163527138,
93.2952789062135));
#206851=CARTESIAN_POINT('Ctrl Pts',(-6.76692939501214,0.0860279287729566,
93.2990495611845));
#206852=CARTESIAN_POINT('Ctrl Pts',(-6.76699756073415,0.00574569560929515,
93.3028202161555));
#206853=CARTESIAN_POINT('Ctrl Pts',(-6.76699756073477,0.00574569487926894,
93.3028202161898));
#206854=CARTESIAN_POINT('Ctrl Pts',(-6.7671436277408,-0.166284859165535,
93.3109000594902));
#206855=CARTESIAN_POINT('Ctrl Pts',(-6.76072543132084,-0.338454857998046,
93.3189799027906));
#206856=CARTESIAN_POINT('Ctrl Pts',(-6.74773793184909,-0.51021740766559,
93.327059746091));
#206857=CARTESIAN_POINT('Ctrl Pts',(-6.73475543507659,-0.68191379553035,
93.335136477089));
#206858=CARTESIAN_POINT('Ctrl Pts',(-6.71520869785343,-0.853202677750636,
93.3432132080871));
#206859=CARTESIAN_POINT('Ctrl Pts',(-6.68914476403856,-1.02353862933231,
93.3512899390851));
#206860=CARTESIAN_POINT('Ctrl Pts',(-6.66308569624209,-1.19384277996337,
93.359365162194));
#206861=CARTESIAN_POINT('Ctrl Pts',(-6.6305119087998,-1.36319398784643,
93.3674403853029));
#206862=CARTESIAN_POINT('Ctrl Pts',(-6.59152214198045,-1.53105351042396,
93.3755156084118));
#206863=CARTESIAN_POINT('Ctrl Pts',(-6.55253204053807,-1.6989144736272,
93.383590900825));
#206864=CARTESIAN_POINT('Ctrl Pts',(-6.50712593385131,-1.86528336504561,
93.3916661932381));
#206865=CARTESIAN_POINT('Ctrl Pts',(-6.45545333513781,-2.02963327669265,
93.3997414856512));
#206866=CARTESIAN_POINT('Ctrl Pts',(-6.40377020156673,-2.19401669551671,
93.4078184244312));
#206867=CARTESIAN_POINT('Ctrl Pts',(-6.34581814429612,-2.35637996189023,
93.4158953632113));
#206868=CARTESIAN_POINT('Ctrl Pts',(-6.28179599943399,-2.51621303181888,
93.4239723019913));
#206869=CARTESIAN_POINT('Ctrl Pts',(-6.21771389257149,-2.67619579855353,
93.4320568054883));
#206870=CARTESIAN_POINT('Ctrl Pts',(-6.14755048035773,-2.83364329106876,
93.4401413089853));
#206871=CARTESIAN_POINT('Ctrl Pts',(-6.07155237022323,-2.98806640080783,
93.4482258124823));
#206872=CARTESIAN_POINT('Ctrl Pts',(-5.99551744981171,-3.14256430658379,
93.4563142317716));
#206873=CARTESIAN_POINT('Ctrl Pts',(-5.91364237693362,-3.29403458549646,
93.4644026510609));
#206874=CARTESIAN_POINT('Ctrl Pts',(-5.82621866723013,-3.44201467771698,
93.4724910703501));
#206875=CARTESIAN_POINT('Ctrl Pts',(-5.73867350453855,-3.59020035060252,
93.4805907264389));
#206876=CARTESIAN_POINT('Ctrl Pts',(-5.64556450551341,-3.73488583879291,
93.4886903825276));
#206877=CARTESIAN_POINT('Ctrl Pts',(-5.54722586563247,-3.87563855327843,
93.4967900386163));
#206878=CARTESIAN_POINT('Ctrl Pts',(-5.46361919463534,-3.99530530793551,
93.5036762969846));
#206879=CARTESIAN_POINT('Ctrl Pts',(-5.37623319098954,-4.11212980405513,
93.5105625553527));
#206880=CARTESIAN_POINT('Ctrl Pts',(-5.28529476372309,-4.2258665691857,
93.5174488137209));
#206881=CARTESIAN_POINT('Ctrl Pts',(-5.16728864195111,-4.37345692190449,
93.5263847571717));
#206882=CARTESIAN_POINT('Ctrl Pts',(-5.04302184668053,-4.51619565427602,
93.5353207006224));
#206883=CARTESIAN_POINT('Ctrl Pts',(-4.91289916910149,-4.65356967867054,
93.5442566440732));
#206884=CARTESIAN_POINT('Ctrl Pts',(-4.78297210041976,-4.79073719347021,
93.5531791544308));
#206885=CARTESIAN_POINT('Ctrl Pts',(-4.64720689148205,-4.92255590486862,
93.5621016647885));
#206886=CARTESIAN_POINT('Ctrl Pts',(-4.50604780372686,-5.04854654237517,
93.5710241751461));
#206887=CARTESIAN_POINT('Ctrl Pts',(-4.36523459954218,-5.17422846372152,
93.5799248225845));
#206888=CARTESIAN_POINT('Ctrl Pts',(-4.21905408696584,-5.29411064107391,
93.5888254700228));
#206889=CARTESIAN_POINT('Ctrl Pts',(-4.06798599589699,-5.40775174515121,
93.5977261174611));
#206890=CARTESIAN_POINT('Ctrl Pts',(-3.91715136191804,-5.52121723092777,
93.6066130100474));
#206891=CARTESIAN_POINT('Ctrl Pts',(-3.76144442130983,-5.62846072784876,
93.6154999026337));
#206892=CARTESIAN_POINT('Ctrl Pts',(-3.60137875133706,-5.72908021321206,
93.6243867952199));
#206893=CARTESIAN_POINT('Ctrl Pts',(-3.44172450988688,-5.82944106893782,
93.6332508451749));
#206894=CARTESIAN_POINT('Ctrl Pts',(-3.27773411294933,-5.92321175066983,
93.6421148951298));
#206895=CARTESIAN_POINT('Ctrl Pts',(-3.10995030000059,-6.01003312233188,
93.6509789450847));
#206896=CARTESIAN_POINT('Ctrl Pts',(-2.94953547754915,-6.09304133793616,
93.6594536899051));
#206897=CARTESIAN_POINT('Ctrl Pts',(-2.78565349739834,-6.16969738636362,
93.6679284347254));
#206898=CARTESIAN_POINT('Ctrl Pts',(-2.6188045693501,-6.23972368198713,
93.6764031795457));
#206899=CARTESIAN_POINT('Ctrl Pts',(-2.4571892520777,-6.30755343742514,
93.6846120939748));
#206900=CARTESIAN_POINT('Ctrl Pts',(-2.29294561100739,-6.36909655218897,
93.6928210084039));
#206901=CARTESIAN_POINT('Ctrl Pts',(-2.12660442730655,-6.42416084868368,
93.701029922833));
#206902=CARTESIAN_POINT('Ctrl Pts',(-1.96022369683498,-6.47923823643493,
93.7092407888898));
#206903=CARTESIAN_POINT('Ctrl Pts',(-1.79174476827033,-6.52783362528962,
93.7174516549466));
#206904=CARTESIAN_POINT('Ctrl Pts',(-1.62171364575998,-6.56980470418687,
93.7256625210034));
#206905=CARTESIAN_POINT('Ctrl Pts',(-1.45161179045112,-6.61179324301629,
93.7338768027733));
#206906=CARTESIAN_POINT('Ctrl Pts',(-1.27995680022436,-6.64715189667427,
93.7420910845432));
#206907=CARTESIAN_POINT('Ctrl Pts',(-1.10730501427173,-6.67578943686578,
93.7503053663131));
#206908=CARTESIAN_POINT('Ctrl Pts',(-0.934458895105898,-6.70445921086925,
93.7585288939055));
#206909=CARTESIAN_POINT('Ctrl Pts',(-0.760614090683128,-6.72639270303103,
93.766752421498));
#206910=CARTESIAN_POINT('Ctrl Pts',(-0.586333187500856,-6.74155044431436,
93.7749759490904));
#206911=CARTESIAN_POINT('Ctrl Pts',(-0.411940577039404,-6.75671790112019,
93.7832047476441));
#206912=CARTESIAN_POINT('Ctrl Pts',(-0.237111665358444,-6.76510093255562,
93.7914335461977));
#206913=CARTESIAN_POINT('Ctrl Pts',(-0.0624091373087647,-6.76671220753332,
93.7996623447514));
#206914=CARTESIAN_POINT('Ctrl Pts',(0.112533854790776,-6.76832570030208,
93.8079024695878));
#206915=CARTESIAN_POINT('Ctrl Pts',(0.287349760914585,-6.76314882971623,
93.8161425944243));
#206916=CARTESIAN_POINT('Ctrl Pts',(0.461479900410779,-6.75124620359211,
93.8243827192607));
#206917=CARTESIAN_POINT('Ctrl Pts',(0.538786496261446,-6.74596192879625,
93.8280409946307));
#206918=CARTESIAN_POINT('Ctrl Pts',(0.615958043517288,-6.739352691166,93.8316992700007));
#206919=CARTESIAN_POINT('Ctrl Pts',(0.6929463317061,-6.73142736582481,93.8353575453706));
#206920=CARTESIAN_POINT('Ctrl Pts',(0.870734700620672,-6.71312548252962,
93.8438055681332));
#206921=CARTESIAN_POINT('Ctrl Pts',(1.04795191929681,-6.68775986739998,
93.8522535908957));
#206922=CARTESIAN_POINT('Ctrl Pts',(1.22401382577075,-6.65537971526209,
93.8607016136583));
#206923=CARTESIAN_POINT('Ctrl Pts',(1.39991450709895,-6.62302921459652,
93.869141900314));
#206924=CARTESIAN_POINT('Ctrl Pts',(1.57466165860447,-6.58367704073766,
93.8775821869698));
#206925=CARTESIAN_POINT('Ctrl Pts',(1.74767720129136,-6.53742406457516,
93.8860224736256));
#206926=CARTESIAN_POINT('Ctrl Pts',(1.92056094324894,-6.4912063232586,93.8944563305936));
#206927=CARTESIAN_POINT('Ctrl Pts',(2.09171538498122,-6.4380983451796,93.9028901875615));
#206928=CARTESIAN_POINT('Ctrl Pts',(2.26057320010668,-6.37825193975273,
93.9113240445294));
#206929=CARTESIAN_POINT('Ctrl Pts',(2.42932834091417,-6.31844192404733,
93.9197527732745));
#206930=CARTESIAN_POINT('Ctrl Pts',(2.59578932572333,-6.25190176107784,
93.9281815020195));
#206931=CARTESIAN_POINT('Ctrl Pts',(2.75940416272226,-6.17883303438045,
93.9366102307645));
#206932=CARTESIAN_POINT('Ctrl Pts',(2.92294463857237,-6.10579751661789,
93.9450351287448));
#206933=CARTESIAN_POINT('Ctrl Pts',(3.08364124193321,-6.02623948743528,
93.9534600267251));
#206934=CARTESIAN_POINT('Ctrl Pts',(3.24096177081412,-5.94040872332211,
93.9618849247053));
#206935=CARTESIAN_POINT('Ctrl Pts',(3.39824746867427,-5.8545969622796,93.9703079573995));
#206936=CARTESIAN_POINT('Ctrl Pts',(3.55215828860114,-5.76251539255458,
93.9787309900937));
#206937=CARTESIAN_POINT('Ctrl Pts',(3.70218598865787,-5.66446007183256,
93.9871540227878));
#206938=CARTESIAN_POINT('Ctrl Pts',(3.85219671325051,-5.56641584595887,
93.9955761024254));
#206939=CARTESIAN_POINT('Ctrl Pts',(3.99832491479458,-5.46239939897792,
94.003998182063));
#206940=CARTESIAN_POINT('Ctrl Pts',(4.14009048145941,-5.35275067655212,
94.0124202617006));
#206941=CARTESIAN_POINT('Ctrl Pts',(4.28185979692558,-5.2430990546121,94.0208425640488));
#206942=CARTESIAN_POINT('Ctrl Pts',(4.41926598396192,-5.12781506460663,
94.0292648663971));
#206943=CARTESIAN_POINT('Ctrl Pts',(4.55186094232517,-5.00727979662957,
94.0376871687453));
#206944=CARTESIAN_POINT('Ctrl Pts',(4.6844779173268,-4.88672451445709,94.0461108695689));
#206945=CARTESIAN_POINT('Ctrl Pts',(4.81228182461522,-4.76091644064371,
94.0545345703925));
#206946=CARTESIAN_POINT('Ctrl Pts',(4.93486018483085,-4.63027471713842,
94.0629582712162));
#206947=CARTESIAN_POINT('Ctrl Pts',(5.05752149494364,-4.49954458718429,
94.0713876724352));
#206948=CARTESIAN_POINT('Ctrl Pts',(5.17494996344339,-4.36397451477395,
94.0798170736541));
#206949=CARTESIAN_POINT('Ctrl Pts',(5.28677162918184,-4.22401879030835,
94.0882464748731));
#206950=CARTESIAN_POINT('Ctrl Pts',(5.39863319273521,-4.08401312983478,
94.0966788836907));
#206951=CARTESIAN_POINT('Ctrl Pts',(5.50488376129901,-3.93961896153071,
94.1051112925084));
#206952=CARTESIAN_POINT('Ctrl Pts',(5.60519142255469,-3.79132142089264,
94.113543701326));
#206953=CARTESIAN_POINT('Ctrl Pts',(5.70559189137714,-3.64288667105506,
94.1219839120536));
#206954=CARTESIAN_POINT('Ctrl Pts',(5.80003828501711,-3.49054161288996,
94.1304241227813));
#206955=CARTESIAN_POINT('Ctrl Pts',(5.88824297134146,-3.33479890105054,
94.1388643335089));
#206956=CARTESIAN_POINT('Ctrl Pts',(5.93841229178721,-3.24621510416893,
94.143664981346));
#206957=CARTESIAN_POINT('Ctrl Pts',(5.98656317132938,-3.15653257250145,
94.148465629183));
#206958=CARTESIAN_POINT('Ctrl Pts',(6.03264948575596,-3.06584885178777,
94.1532662770201));
#206959=CARTESIAN_POINT('Ctrl Pts',(6.11079091147118,-2.9120905112935,94.161405992053));
#206960=CARTESIAN_POINT('Ctrl Pts',(6.18315003011602,-2.75514606313375,
94.1695457070858));
#206961=CARTESIAN_POINT('Ctrl Pts',(6.24945581875254,-2.59549435935816,
94.1776854221186));
#206962=CARTESIAN_POINT('Ctrl Pts',(6.31570361674432,-2.43598228600438,
94.1858180182056));
#206963=CARTESIAN_POINT('Ctrl Pts',(6.37590848331387,-2.27376800591042,
94.1939506142925));
#206964=CARTESIAN_POINT('Ctrl Pts',(6.42984539723636,-2.1093546803794,94.2020832103794));
#206965=CARTESIAN_POINT('Ctrl Pts',(6.48374543699039,-1.94505375661961,
94.2102102465873));
#206966=CARTESIAN_POINT('Ctrl Pts',(6.53138594184629,-1.77855712712222,
94.2183372827952));
#206967=CARTESIAN_POINT('Ctrl Pts',(6.5725901133903,-1.61038759352028,94.2264643190031));
#206968=CARTESIAN_POINT('Ctrl Pts',(6.61377458859492,-1.44229844799767,
94.2345874703406));
#206969=CARTESIAN_POINT('Ctrl Pts',(6.64852877021056,-1.27253834572459,
94.2427106216782));
#206970=CARTESIAN_POINT('Ctrl Pts',(6.67672581118828,-1.10164488026417,
94.2508337730157));
#206971=CARTESIAN_POINT('Ctrl Pts',(6.70491492858801,-0.930799437137095,
94.2589546416874));
#206972=CARTESIAN_POINT('Ctrl Pts',(6.72655051667087,-0.75882162631679,
94.2670755103591));
#206973=CARTESIAN_POINT('Ctrl Pts',(6.74155691183685,-0.586258820372734,
94.2751963790307));
#206974=CARTESIAN_POINT('Ctrl Pts',(6.7565641180058,-0.413686688474876,
94.2833176865852));
#206975=CARTESIAN_POINT('Ctrl Pts',(6.76494137982004,-0.240529862795474,
94.2914389941397));
#206976=CARTESIAN_POINT('Ctrl Pts',(6.76666492757033,-0.0673406117405915,
94.2995603016942));
#206977=CARTESIAN_POINT('Ctrl Pts',(6.76756054289508,0.0226545434845253,
94.3037804154111));
#206978=CARTESIAN_POINT('Ctrl Pts',(6.76666037691786,0.112658408977732,
94.308000529128));
#206979=CARTESIAN_POINT('Ctrl Pts',(6.76396665283788,0.202593482859393,
94.3122206428449));
#206980=CARTESIAN_POINT('Ctrl Pts',(6.7582318314502,0.394061342924849,94.3212050813707));
#206981=CARTESIAN_POINT('Ctrl Pts',(6.74436776794409,0.585122379039508,
94.3301895198965));
#206982=CARTESIAN_POINT('Ctrl Pts',(6.72246167560015,0.775111617824945,
94.3391739584224));
#206983=CARTESIAN_POINT('Ctrl Pts',(6.70051777464833,0.965428766696629,
94.3481739035528));
#206984=CARTESIAN_POINT('Ctrl Pts',(6.67050412973394,1.1546701834502,94.3571738486833));
#206985=CARTESIAN_POINT('Ctrl Pts',(6.63255931114618,1.34217956478561,94.3661737938138));
#206986=CARTESIAN_POINT('Ctrl Pts',(6.59452507461947,1.53013081679105,94.375194947546));
#206987=CARTESIAN_POINT('Ctrl Pts',(6.54852231632505,1.71634163162484,94.3842161012782));
#206988=CARTESIAN_POINT('Ctrl Pts',(6.49474060721642,1.90016668873393,94.3932372550104));
#206989=CARTESIAN_POINT('Ctrl Pts',(6.44090417479457,2.08417878928858,94.4022675878376));
#206990=CARTESIAN_POINT('Ctrl Pts',(6.37927305184458,2.26580005505941,94.4112979206649));
#206991=CARTESIAN_POINT('Ctrl Pts',(6.31008612126959,2.44440220548111,94.4203282534922));
#206992=CARTESIAN_POINT('Ctrl Pts',(6.24080110543641,2.62325755745248,94.4293713884848));
#206993=CARTESIAN_POINT('Ctrl Pts',(6.16393894993225,2.79908501286153,94.4384145234775));
#206994=CARTESIAN_POINT('Ctrl Pts',(6.07978686387173,2.9712759363433,94.4474576584701));
#206995=CARTESIAN_POINT('Ctrl Pts',(6.00621855314991,3.1218104739313,94.4553634418699));
#206996=CARTESIAN_POINT('Ctrl Pts',(5.92707946764804,3.26956594019165,94.4632692252698));
#206997=CARTESIAN_POINT('Ctrl Pts',(5.84259004176172,3.4141515203498,94.4711750086696));
#206998=CARTESIAN_POINT('Ctrl Pts',(5.75011093293703,3.57240973386773,94.4798283968978));
#206999=CARTESIAN_POINT('Ctrl Pts',(5.6511389163362,3.72700935470634,94.4884817851261));
#207000=CARTESIAN_POINT('Ctrl Pts',(5.5459820708745,3.87741819636967,94.4971351733544));
#207001=CARTESIAN_POINT('Ctrl Pts',(5.44092234521913,4.02768812479813,94.5057805695647));
#207002=CARTESIAN_POINT('Ctrl Pts',(5.32968935726328,4.17377474551138,94.5144259657751));
#207003=CARTESIAN_POINT('Ctrl Pts',(5.21263527468974,4.31517351830263,94.5230713619855));
#207004=CARTESIAN_POINT('Ctrl Pts',(5.09184287902795,4.46108809157999,94.5319928630279));
#207005=CARTESIAN_POINT('Ctrl Pts',(4.96485157862196,4.60201014718321,94.5409143640703));
#207006=CARTESIAN_POINT('Ctrl Pts',(4.8320959348139,4.73741890450433,94.5498358651127));
#207007=CARTESIAN_POINT('Ctrl Pts',(4.70369386463786,4.86838708228767,94.5584647954546));
#207008=CARTESIAN_POINT('Ctrl Pts',(4.56989974694032,4.99419757961759,94.5670937257966));
#207009=CARTESIAN_POINT('Ctrl Pts',(4.43114705478339,5.11441343448929,94.5757226561386));
#207010=CARTESIAN_POINT('Ctrl Pts',(4.28533758315489,5.24074330966307,94.5847904425312));
#207011=CARTESIAN_POINT('Ctrl Pts',(4.1340522368523,5.36089437811868,94.5938582289238));
#207012=CARTESIAN_POINT('Ctrl Pts',(3.97783754250411,5.47440384749288,94.6029260153164));
#207013=CARTESIAN_POINT('Ctrl Pts',(3.82162284815593,5.58791331686708,94.611993801709));
#207014=CARTESIAN_POINT('Ctrl Pts',(3.66047910098683,5.6947809291248,94.6210615881017));
#207015=CARTESIAN_POINT('Ctrl Pts',(3.49499323025666,5.7945932834376,94.6301293744943));
#207016=CARTESIAN_POINT('Ctrl Pts',(3.36553668759303,5.87267464619951,94.6372229364451));
#207017=CARTESIAN_POINT('Ctrl Pts',(3.23347124895921,5.94641053713559,94.6443164983958));
#207018=CARTESIAN_POINT('Ctrl Pts',(3.09910619832125,6.01563211736945,94.6514100603466));
#207019=CARTESIAN_POINT('Origin',(0.,0.,4.30282021618968));
#207020=CARTESIAN_POINT('',(3.09910619832136,6.01563211736939,97.0457552630242));
#207021=CARTESIAN_POINT('',(3.09910619832137,6.01563211736939,96.6512761190133));
#207022=CARTESIAN_POINT('',(3.09910619832133,6.0156321173694,4.30282021618968));
#207023=CARTESIAN_POINT('',(-6.767,3.9611911840931E-12,95.6971797838099));
#207024=CARTESIAN_POINT('Ctrl Pts',(-6.767,4.34585066737734E-12,95.6971797838099));
#207025=CARTESIAN_POINT('Ctrl Pts',(-6.76700000000012,-0.186007249522647,
95.7059292956211));
#207026=CARTESIAN_POINT('Ctrl Pts',(-6.75932637294543,-0.37201435574582,
95.7146788074323));
#207027=CARTESIAN_POINT('Ctrl Pts',(-6.74400518264213,-0.557389537483525,
95.7234283192435));
#207028=CARTESIAN_POINT('Ctrl Pts',(-6.72868405705128,-0.742763936248029,
95.7321777940992));
#207029=CARTESIAN_POINT('Ctrl Pts',(-6.70571545645775,-0.927506130238709,
95.7409272689549));
#207030=CARTESIAN_POINT('Ctrl Pts',(-6.67517739404857,-1.11098863989826,
95.7496767438105));
#207031=CARTESIAN_POINT('Ctrl Pts',(-6.64463945808734,-1.2944703898178,
95.7584261824376));
#207032=CARTESIAN_POINT('Ctrl Pts',(-6.60653217008387,-1.47669218313541,
95.7671756210646));
#207033=CARTESIAN_POINT('Ctrl Pts',(-6.56098496092707,-1.65703510599166,
95.7759250596916));
#207034=CARTESIAN_POINT('Ctrl Pts',(-6.51543793658327,-1.83737729708592,
95.7846744628168));
#207035=CARTESIAN_POINT('Ctrl Pts',(-6.46245112167451,-2.0158403551083,
95.7934238659419));
#207036=CARTESIAN_POINT('Ctrl Pts',(-6.40220448374283,-2.19181813760706,
95.8021732690671));
#207037=CARTESIAN_POINT('Ctrl Pts',(-6.34195808526528,-2.36779522067079,
95.8109226374172));
#207038=CARTESIAN_POINT('Ctrl Pts',(-6.27445201433122,-2.54128677684122,
95.8196720057673));
#207039=CARTESIAN_POINT('Ctrl Pts',(-6.19991555071912,-2.71170355384789,
95.8284213741174));
#207040=CARTESIAN_POINT('Ctrl Pts',(-6.12537937716708,-2.88211966767442,
95.8371707084192));
#207041=CARTESIAN_POINT('Ctrl Pts',(-6.04381298052543,-3.04946076371738,
95.845920042721));
#207042=CARTESIAN_POINT('Ctrl Pts',(-5.95549339335863,-3.21315848374488,
95.8546693770228));
#207043=CARTESIAN_POINT('Ctrl Pts',(-5.86717414255438,-3.37685558033442,
95.8634186780029));
#207044=CARTESIAN_POINT('Ctrl Pts',(-5.77210188876624,-3.53690907646714,
95.8721679789831));
#207045=CARTESIAN_POINT('Ctrl Pts',(-5.67059953347018,-3.69277536969252,
95.8809172799633));
#207046=CARTESIAN_POINT('Ctrl Pts',(-5.569097556314,-3.848641082249,95.8896665483486));
#207047=CARTESIAN_POINT('Ctrl Pts',(-5.4611656819686,-4.00031938297504,
95.8984158167339));
#207048=CARTESIAN_POINT('Ctrl Pts',(-5.34717048533606,-4.14729511859851,
95.9071650851192));
#207049=CARTESIAN_POINT('Ctrl Pts',(-5.23317570391852,-4.29427031887897,
95.9159143216362));
#207050=CARTESIAN_POINT('Ctrl Pts',(-5.11311782003543,-4.43654276189513,
95.9246635581532));
#207051=CARTESIAN_POINT('Ctrl Pts',(-4.98740458984797,-4.57362924351804,
95.9334127946703));
#207052=CARTESIAN_POINT('Ctrl Pts',(-4.86169180711801,-4.71071523720206,
95.9421620000457));
#207053=CARTESIAN_POINT('Ctrl Pts',(-4.73032391204244,-4.84261509523166,
95.9509112054211));
#207054=CARTESIAN_POINT('Ctrl Pts',(-4.59374707013688,-4.96888084538247,
95.9596604107966));
#207055=CARTESIAN_POINT('Ctrl Pts',(-4.45717070301531,-5.09514615659389,
95.968409585757));
#207056=CARTESIAN_POINT('Ctrl Pts',(-4.31538563571123,-5.2157772045946,
95.9771587607175));
#207057=CARTESIAN_POINT('Ctrl Pts',(-4.16887341029587,-5.33036429232826,
95.9859079356779));
#207058=CARTESIAN_POINT('Ctrl Pts',(-4.02236168203777,-5.44495099123564,
95.99465708095));
#207059=CARTESIAN_POINT('Ctrl Pts',(-3.87112305348229,-5.55349359438558,
96.003406226222));
#207060=CARTESIAN_POINT('Ctrl Pts',(-3.71567117017816,-5.65562346298857,
96.012155371494));
#207061=CARTESIAN_POINT('Ctrl Pts',(-3.56021980145874,-5.7577529935161,
96.0209044878042));
#207062=CARTESIAN_POINT('Ctrl Pts',(-3.40055544538404,-5.85346967463841,
96.0296536041143));
#207063=CARTESIAN_POINT('Ctrl Pts',(-3.23722035986908,-5.94244842986871,
96.0384027204245));
#207064=CARTESIAN_POINT('Ctrl Pts',(-3.0738858014723,-6.03142689794504,
96.0471518084994));
#207065=CARTESIAN_POINT('Ctrl Pts',(-2.90688078896622,-6.11366734656761,
96.0559008965742));
#207066=CARTESIAN_POINT('Ctrl Pts',(-2.73677250721408,-6.18889046952337,
96.064649984649));
#207067=CARTESIAN_POINT('Ctrl Pts',(-2.56666476031511,-6.26411335596316,
96.0733990452151));
#207068=CARTESIAN_POINT('Ctrl Pts',(-2.39345402575184,-6.33231884500549,
96.0821481057811));
#207069=CARTESIAN_POINT('Ctrl Pts',(-2.21772856065599,-6.39327529762724,
96.0908971663472));
#207070=CARTESIAN_POINT('Ctrl Pts',(-2.04200363348504,-6.45423156365115,
96.0996462001309));
#207071=CARTESIAN_POINT('Ctrl Pts',(-1.86376426189252,-6.50793874375666,
96.1083952339145));
#207072=CARTESIAN_POINT('Ctrl Pts',(-1.6836157775311,-6.55421443909553,
96.1171442676983));
#207073=CARTESIAN_POINT('Ctrl Pts',(-1.50346782967756,-6.60048999661878,
96.1258932754261));
#207074=CARTESIAN_POINT('Ctrl Pts',(-1.32141105794943,-6.63933404237721,
96.1346422831539));
#207075=CARTESIAN_POINT('Ctrl Pts',(-1.13806375486979,-6.67061465607568,
96.1433912908817));
#207076=CARTESIAN_POINT('Ctrl Pts',(-0.954716982602963,-6.70189517921296,
96.1521402732801));
#207077=CARTESIAN_POINT('Ctrl Pts',(-0.770079968902468,-6.72561226592223,
96.1608892556785));
#207078=CARTESIAN_POINT('Ctrl Pts',(-0.584779765558964,-6.74168536983096,
96.1696382380769));
#207079=CARTESIAN_POINT('Ctrl Pts',(-0.391489830652015,-6.75845151013849,
96.1787644570868));
#207080=CARTESIAN_POINT('Ctrl Pts',(-0.197478578239049,-6.76689983031623,
96.1878906760966));
#207081=CARTESIAN_POINT('Ctrl Pts',(-0.00346287645205357,-6.76699911397118,
96.1970168951065));
#207082=CARTESIAN_POINT('Ctrl Pts',(0.184489834654066,-6.76709529501191,
96.2058579197723));
#207083=CARTESIAN_POINT('Ctrl Pts',(0.372446404249543,-6.75935639738167,
96.2146989444381));
#207084=CARTESIAN_POINT('Ctrl Pts',(0.559755019488502,-6.74380925873185,
96.2235399691039));
#207085=CARTESIAN_POINT('Ctrl Pts',(0.745134705521925,-6.72842222659804,
96.2322899477137));
#207086=CARTESIAN_POINT('Ctrl Pts',(0.929879431228705,-6.70538706057522,
96.2410399263234));
#207087=CARTESIAN_POINT('Ctrl Pts',(1.11336163626838,-6.67478200894125,
96.2497899049332));
#207088=CARTESIAN_POINT('Ctrl Pts',(1.2968419630075,-6.64417727061007,96.2585397939697));
#207089=CARTESIAN_POINT('Ctrl Pts',(1.4790595121756,-6.6060028489058,96.2672896830062));
#207090=CARTESIAN_POINT('Ctrl Pts',(1.65939532067153,-6.56038841607213,
96.2760395720427));
#207091=CARTESIAN_POINT('Ctrl Pts',(1.8397293430086,-6.5147744350324,96.2847893744149));
#207092=CARTESIAN_POINT('Ctrl Pts',(2.01818138406312,-6.46172066062126,
96.2935391767871));
#207093=CARTESIAN_POINT('Ctrl Pts',(2.19414528354237,-6.40140730423466,
96.3022889791592));
#207094=CARTESIAN_POINT('Ctrl Pts',(2.37010749864039,-6.34109452518628,
96.3110386977755));
#207095=CARTESIAN_POINT('Ctrl Pts',(2.543581348665,-6.27352239616488,96.3197884163918));
#207096=CARTESIAN_POINT('Ctrl Pts',(2.71397759435597,-6.19892043966801,
96.3285381350082));
#207097=CARTESIAN_POINT('Ctrl Pts',(2.88437226558162,-6.12431917249497,
96.3372877727769));
#207098=CARTESIAN_POINT('Ctrl Pts',(3.05168912680989,-6.04268832278782,
96.3460374105456));
#207099=CARTESIAN_POINT('Ctrl Pts',(3.21535986273884,-5.95430516123318,
96.3547870483143));
#207100=CARTESIAN_POINT('Ctrl Pts',(3.37902914072867,-5.86592278697426,
96.3635366081434));
#207101=CARTESIAN_POINT('Ctrl Pts',(3.53905210621594,-5.77078835741928,
96.3722861679724));
#207102=CARTESIAN_POINT('Ctrl Pts',(3.69488522831715,-5.66922500431617,
96.3810357278015));
#207103=CARTESIAN_POINT('Ctrl Pts',(3.85071701406964,-5.56766252217076,
96.3897852125986));
#207104=CARTESIAN_POINT('Ctrl Pts',(4.00235878822435,-5.45967138329347,
96.3985346973957));
#207105=CARTESIAN_POINT('Ctrl Pts',(4.14929549611362,-5.34561838199579,
96.4072841821929));
#207106=CARTESIAN_POINT('Ctrl Pts',(4.29623099276123,-5.23156632086988,
96.4160335948654));
#207107=CARTESIAN_POINT('Ctrl Pts',(4.43846127436058,-5.11145267304938,
96.424783007538));
#207108=CARTESIAN_POINT('Ctrl Pts',(4.57550326054469,-4.9856854004986,96.4335324202106));
#207109=CARTESIAN_POINT('Ctrl Pts',(4.71254416257796,-4.85991912290345,
96.4422817636658));
#207110=CARTESIAN_POINT('Ctrl Pts',(4.84439664018766,-4.72849950385413,
96.4510311071211));
#207111=CARTESIAN_POINT('Ctrl Pts',(4.97061286794741,-4.59187289861073,
96.4597804505763));
#207112=CARTESIAN_POINT('Ctrl Pts',(5.09682813912685,-4.45524732884685,
96.4685297277212));
#207113=CARTESIAN_POINT('Ctrl Pts',(5.21740705147843,-4.31341506235783,
96.477279004866));
#207114=CARTESIAN_POINT('Ctrl Pts',(5.33194007545704,-4.16685781275714,
96.4860282820108));
#207115=CARTESIAN_POINT('Ctrl Pts',(5.44647226944489,-4.02030162521836,
96.4947774957519));
#207116=CARTESIAN_POINT('Ctrl Pts',(5.55495848628114,-3.86902074887933,
96.5035267094931));
#207117=CARTESIAN_POINT('Ctrl Pts',(5.65703027291785,-3.71352898080667,
96.5122759232342));
#207118=CARTESIAN_POINT('Ctrl Pts',(5.75910135376988,-3.55803828789603,
96.5210250764781));
#207119=CARTESIAN_POINT('Ctrl Pts',(5.85475793592737,-3.39833700106738,
96.5297742297219));
#207120=CARTESIAN_POINT('Ctrl Pts',(5.94367514427378,-3.23496750823592,
96.5385233829658));
#207121=CARTESIAN_POINT('Ctrl Pts',(6.0325917673262,-3.07159909077764,96.5472724786187));
#207122=CARTESIAN_POINT('Ctrl Pts',(6.11476896835905,-2.90456276731474,
96.5560215742717));
#207123=CARTESIAN_POINT('Ctrl Pts',(6.18992765547868,-2.73442583003091,
96.5647706699246));
#207124=CARTESIAN_POINT('Ctrl Pts',(6.26508587283041,-2.56428995616202,
96.5735197108926));
#207125=CARTESIAN_POINT('Ctrl Pts',(6.33322554827152,-2.39105376935225,
96.5822687518607));
#207126=CARTESIAN_POINT('Ctrl Pts',(6.39411526733026,-2.21530561054093,
96.5910177928287));
#207127=CARTESIAN_POINT('Ctrl Pts',(6.45500462602837,-2.0395584918513,96.5997667820177));
#207128=CARTESIAN_POINT('Ctrl Pts',(6.50864402040725,-1.86129970164594,
96.6085157712068));
#207129=CARTESIAN_POINT('Ctrl Pts',(6.55485128368583,-1.68113463136127,
96.6172647603958));
#207130=CARTESIAN_POINT('Ctrl Pts',(6.6019980955431,-1.49730620116944,96.6261916458672));
#207131=CARTESIAN_POINT('Ctrl Pts',(6.64140720707857,-1.3114934324578,96.6351185313386));
#207132=CARTESIAN_POINT('Ctrl Pts',(6.67293928722869,-1.12435326697614,
96.6440454168101));
#207133=CARTESIAN_POINT('Ctrl Pts',(6.70384625876244,-0.940923067007474,
96.6527953309875));
#207134=CARTESIAN_POINT('Ctrl Pts',(6.72718554579786,-0.756217899522548,
96.661545245165));
#207135=CARTESIAN_POINT('Ctrl Pts',(6.7428778681532,-0.570865181255377,
96.6702951593425));
#207136=CARTESIAN_POINT('Ctrl Pts',(6.7585698819084,-0.38551610807487,96.6790449014469));
#207137=CARTESIAN_POINT('Ctrl Pts',(6.766615207734,-0.199519795227315,96.6877946435514));
#207138=CARTESIAN_POINT('Ctrl Pts',(6.76698651789579,-0.0135080204566571,
96.6965443856559));
#207139=CARTESIAN_POINT('Ctrl Pts',(6.76735782124905,0.17250034351191,96.7052939673209));
#207140=CARTESIAN_POINT('Ctrl Pts',(6.76005538995189,0.35852388220983,96.7140435489858));
#207141=CARTESIAN_POINT('Ctrl Pts',(6.7451040274237,0.543930748563247,96.7227931306508));
#207142=CARTESIAN_POINT('Ctrl Pts',(6.73015291918043,0.729334461614134,
96.7315425635075));
#207143=CARTESIAN_POINT('Ctrl Pts',(6.70755316306609,0.914121237633609,
96.7402919963642));
#207144=CARTESIAN_POINT('Ctrl Pts',(6.67738151874591,1.09766345166018,96.7490414292209));
#207145=CARTESIAN_POINT('Ctrl Pts',(6.64721034747589,1.28120278799564,96.7577907248984));
#207146=CARTESIAN_POINT('Ctrl Pts',(6.60946757205163,1.46349731860232,96.7665400205759));
#207147=CARTESIAN_POINT('Ctrl Pts',(6.56428138111546,1.64392790278068,96.7752893162534));
#207148=CARTESIAN_POINT('Ctrl Pts',(6.51909583859876,1.82435589778962,96.784038486379));
#207149=CARTESIAN_POINT('Ctrl Pts',(6.46646716392905,2.00291972192171,96.7927876565046));
#207150=CARTESIAN_POINT('Ctrl Pts',(6.40657409872916,2.17901292274569,96.8015368266302));
#207151=CARTESIAN_POINT('Ctrl Pts',(6.34668181342111,2.35510383058884,96.8102858828293));
#207152=CARTESIAN_POINT('Ctrl Pts',(6.27952541914087,2.52872390822489,96.8190349390285));
#207153=CARTESIAN_POINT('Ctrl Pts',(6.20533299175556,2.69928350890195,96.8277839952276));
#207154=CARTESIAN_POINT('Ctrl Pts',(6.12831602991585,2.87633637965547,96.8368661313858));
#207155=CARTESIAN_POINT('Ctrl Pts',(6.04371690605303,3.05009086601398,96.845948267544));
#207156=CARTESIAN_POINT('Ctrl Pts',(5.95184520316659,3.21991112882683,96.8550304037022));
#207157=CARTESIAN_POINT('Ctrl Pts',(5.86333549509301,3.38351691182972,96.8637801840457));
#207158=CARTESIAN_POINT('Ctrl Pts',(5.76807618099393,3.54347103711965,96.8725299643893));
#207159=CARTESIAN_POINT('Ctrl Pts',(5.66639083309038,3.69923018027662,96.8812797447329));
#207160=CARTESIAN_POINT('Ctrl Pts',(5.56470914082218,3.85498372382024,96.8900292105178));
#207161=CARTESIAN_POINT('Ctrl Pts',(5.4566020337208,4.0065423470198,96.8987786763027));
#207162=CARTESIAN_POINT('Ctrl Pts',(5.34243669839225,4.15339127986658,96.9075281420876));
#207163=CARTESIAN_POINT('Ctrl Pts',(5.22827486050601,4.30023571401268,96.9162773398336));
#207164=CARTESIAN_POINT('Ctrl Pts',(5.10805534167121,4.44237052028458,96.9250265375796));
#207165=CARTESIAN_POINT('Ctrl Pts',(4.98218644339962,4.57931296628709,96.9337757353256));
#207166=CARTESIAN_POINT('Ctrl Pts',(4.85632073219602,4.71625194483345,96.9425247115373));
#207167=CARTESIAN_POINT('Ctrl Pts',(4.72480612170339,4.84799861524488,96.9512736877489));
#207168=CARTESIAN_POINT('Ctrl Pts',(4.58808925235337,4.97410554898461,96.9600226639605));
#207169=CARTESIAN_POINT('Ctrl Pts',(4.45136349474075,5.10022068121183,96.9687722089622));
#207170=CARTESIAN_POINT('Ctrl Pts',(4.30943501210109,5.2206951487181,96.977521753964));
#207171=CARTESIAN_POINT('Ctrl Pts',(4.16278587431812,5.33511975166233,96.9862712989657));
#207172=CARTESIAN_POINT('Ctrl Pts',(4.01614535740482,5.44953762807817,96.9950203296194));
#207173=CARTESIAN_POINT('Ctrl Pts',(3.86478496657961,5.55790617532758,97.0037693602731));
#207174=CARTESIAN_POINT('Ctrl Pts',(3.70921874747237,5.65985735539329,97.0125183909268));
#207175=CARTESIAN_POINT('Ctrl Pts',(3.55365041605945,5.76180991977019,97.0212675403764));
#207176=CARTESIAN_POINT('Ctrl Pts',(3.39387638174569,5.85734478552786,97.0300166898261));
#207177=CARTESIAN_POINT('Ctrl Pts',(3.23043927904589,5.94613749121205,97.0387658392757));
#207178=CARTESIAN_POINT('Ctrl Pts',(3.18691767070463,5.9697820694413,97.0410956471919));
#207179=CARTESIAN_POINT('Ctrl Pts',(3.14313645919646,5.99294880633418,97.043425455108));
#207180=CARTESIAN_POINT('Ctrl Pts',(3.09910619832136,6.01563211736939,97.0457552630242));
#207181=CARTESIAN_POINT('Ctrl Pts',(3.09910619832144,6.01563211736935,95.0455663730808));
#207182=CARTESIAN_POINT('Ctrl Pts',(2.94398460122206,6.09554696150953,95.0537894768725));
#207183=CARTESIAN_POINT('Ctrl Pts',(2.78592596187934,6.1693775730439,95.0620125806642));
#207184=CARTESIAN_POINT('Ctrl Pts',(2.62545481752041,6.23692841077712,95.0702356844558));
#207185=CARTESIAN_POINT('Ctrl Pts',(2.54683969676187,6.27002169547297,95.0742641987422));
#207186=CARTESIAN_POINT('Ctrl Pts',(2.46764580997816,6.30160856605184,95.0782927130285));
#207187=CARTESIAN_POINT('Ctrl Pts',(2.38793604010017,6.331670432705,95.0823212273148));
#207188=CARTESIAN_POINT('Ctrl Pts',(2.21112594449757,6.39835286730585,95.0912571707656));
#207189=CARTESIAN_POINT('Ctrl Pts',(2.03140856638816,6.45766767263564,95.1001931142163));
#207190=CARTESIAN_POINT('Ctrl Pts',(1.84939388817998,6.50938025055862,95.109129057667));
#207191=CARTESIAN_POINT('Ctrl Pts',(1.66765282630942,6.56101509076109,95.1180515680247));
#207192=CARTESIAN_POINT('Ctrl Pts',(1.48362160296594,6.60507043626395,95.1269740783823));
#207193=CARTESIAN_POINT('Ctrl Pts',(1.2979268806446,6.64136091569342,95.13589658874));
#207194=CARTESIAN_POINT('Ctrl Pts',(1.11268716801945,6.6775624721863,95.1447972361783));
#207195=CARTESIAN_POINT('Ctrl Pts',(0.925792344517236,6.7060370863505,95.1536978836166));
#207196=CARTESIAN_POINT('Ctrl Pts',(0.737880206460599,6.72665011732539,
95.162598531055));
#207197=CARTESIAN_POINT('Ctrl Pts',(0.550258463421176,6.74723129340497,
95.1714854236412));
#207198=CARTESIAN_POINT('Ctrl Pts',(0.361622797206337,6.75997509256352,
95.1803723162275));
#207199=CARTESIAN_POINT('Ctrl Pts',(0.172620047030761,6.76479795111156,
95.1892592088138));
#207200=CARTESIAN_POINT('Ctrl Pts',(-0.0158968955242036,6.7696084131128,
95.1981232587687));
#207201=CARTESIAN_POINT('Ctrl Pts',(-0.204778781918719,6.76653855445609,
95.2069873087236));
#207202=CARTESIAN_POINT('Ctrl Pts',(-0.393375586261886,6.75555657574808,
95.2158513586785));
#207203=CARTESIAN_POINT('Ctrl Pts',(-0.573689302776424,6.7450569206642,
95.2243261034989));
#207204=CARTESIAN_POINT('Ctrl Pts',(-0.753742179121024,6.7273251723314,
95.2328008483192));
#207205=CARTESIAN_POINT('Ctrl Pts',(-0.9329623871501,6.70237794996397,95.2412755931395));
#207206=CARTESIAN_POINT('Ctrl Pts',(-1.10656092998103,6.67821325615911,
95.2494845075686));
#207207=CARTESIAN_POINT('Ctrl Pts',(-1.27921074848217,6.64730098063199,
95.2576934219978));
#207208=CARTESIAN_POINT('Ctrl Pts',(-1.45035732016783,6.6097467912043,95.2659023364269));
#207209=CARTESIAN_POINT('Ctrl Pts',(-1.62154458108142,6.57218367345887,
95.2741132024837));
#207210=CARTESIAN_POINT('Ctrl Pts',(-1.79122753534553,6.52797557215911,
95.2823240685405));
#207211=CARTESIAN_POINT('Ctrl Pts',(-1.95886402317029,6.47727880662313,
95.2905349345973));
#207212=CARTESIAN_POINT('Ctrl Pts',(-2.12657024762539,6.42656095127762,
95.2987492163671));
#207213=CARTESIAN_POINT('Ctrl Pts',(-2.29222796905997,6.36934915715565,
95.3069634981369));
#207214=CARTESIAN_POINT('Ctrl Pts',(-2.45531221441518,6.30584894599796,
95.3151777799067));
#207215=CARTESIAN_POINT('Ctrl Pts',(-2.618580023963,6.24227726033969,95.3234013074991));
#207216=CARTESIAN_POINT('Ctrl Pts',(-2.77926823992194,6.17240314957602,
95.3316248350915));
#207217=CARTESIAN_POINT('Ctrl Pts',(-2.9368729363965,6.09647983310548,95.3398483626839));
#207218=CARTESIAN_POINT('Ctrl Pts',(-3.09457865135069,6.02050785274249,
95.3480771612376));
#207219=CARTESIAN_POINT('Ctrl Pts',(-3.24919659322046,5.9384791039557,95.3563059597913));
#207220=CARTESIAN_POINT('Ctrl Pts',(-3.40024936417954,5.85069169085132,
95.364534758345));
#207221=CARTESIAN_POINT('Ctrl Pts',(-3.55151004719001,5.76278344539789,
95.3727748831814));
#207222=CARTESIAN_POINT('Ctrl Pts',(-3.69919545785659,5.66910089366582,
95.3810150080178));
#207223=CARTESIAN_POINT('Ctrl Pts',(-3.84285815269377,5.5699847592498,95.3892551328542));
#207224=CARTESIAN_POINT('Ctrl Pts',(-3.90663846046189,5.52598128594028,
95.3929134082243));
#207225=CARTESIAN_POINT('Ctrl Pts',(-3.96962633961643,5.48090738209684,
95.3965716835943));
#207226=CARTESIAN_POINT('Ctrl Pts',(-4.03178486307862,5.43479528757525,
95.4002299589643));
#207227=CARTESIAN_POINT('Ctrl Pts',(-4.17399707305187,5.32929563116208,
95.4085997109481));
#207228=CARTESIAN_POINT('Ctrl Pts',(-4.31220732511742,5.21810561209049,
95.416969462932));
#207229=CARTESIAN_POINT('Ctrl Pts',(-4.44594362259907,5.10155606699276,
95.4253392149158));
#207230=CARTESIAN_POINT('Ctrl Pts',(-4.57955297740067,4.98511715088576,
95.4337010223194));
#207231=CARTESIAN_POINT('Ctrl Pts',(-4.70869658297601,4.86332907027042,
95.442062829723));
#207232=CARTESIAN_POINT('Ctrl Pts',(-4.83293364915331,4.73656429734482,
95.4504246371266));
#207233=CARTESIAN_POINT('Ctrl Pts',(-4.95707439156866,4.60989780796848,
95.4587799614349));
#207234=CARTESIAN_POINT('Ctrl Pts',(-5.07631593703795,4.47826256013943,
95.4671352857431));
#207235=CARTESIAN_POINT('Ctrl Pts',(-5.19025245315042,4.34206960706137,
95.4754906100514));
#207236=CARTESIAN_POINT('Ctrl Pts',(-5.30412042747101,4.20595858477569,
95.4838409079737));
#207237=CARTESIAN_POINT('Ctrl Pts',(-5.41268951421426,4.06529558465423,
95.4921912058961));
#207238=CARTESIAN_POINT('Ctrl Pts',(-5.51559228467209,3.92052684588,95.5005415038184));
#207239=CARTESIAN_POINT('Ctrl Pts',(-5.61845546337996,3.77581380675001,
95.508888588971));
#207240=CARTESIAN_POINT('Ctrl Pts',(-5.71565647205855,3.62699845604368,
95.5172356741236));
#207241=CARTESIAN_POINT('Ctrl Pts',(-5.80686935428632,3.47455857660371,
95.5255827592762));
#207242=CARTESIAN_POINT('Ctrl Pts',(-5.8980635146385,3.32214998617016,95.5339281311501));
#207243=CARTESIAN_POINT('Ctrl Pts',(-5.9832718217372,3.16611864344385,95.542273503024));
#207244=CARTESIAN_POINT('Ctrl Pts',(-6.0622125463111,3.00696991061571,95.5506188748979));
#207245=CARTESIAN_POINT('Ctrl Pts',(-6.14114950608394,2.84782876782837,
95.5589638487685));
#207246=CARTESIAN_POINT('Ctrl Pts',(-6.21381932690151,2.68557083841541,
95.5673088226391));
#207247=CARTESIAN_POINT('Ctrl Pts',(-6.27998689226227,2.52072482294559,
95.5756537965098));
#207248=CARTESIAN_POINT('Ctrl Pts',(-6.34616172701123,2.35586069694572,
95.5839996871869));
#207249=CARTESIAN_POINT('Ctrl Pts',(-6.40583275540286,2.18840823654171,
95.592345577864));
#207250=CARTESIAN_POINT('Ctrl Pts',(-6.45881344340899,2.01891503120842,
95.6006914685412));
#207251=CARTESIAN_POINT('Ctrl Pts',(-6.5118302066246,1.84930641584334,95.6090430420391));
#207252=CARTESIAN_POINT('Ctrl Pts',(-6.55814742301891,1.67765460618518,
95.617394615537));
#207253=CARTESIAN_POINT('Ctrl Pts',(-6.59762851793987,1.50452216310249,
95.6257461890349));
#207254=CARTESIAN_POINT('Ctrl Pts',(-6.63712300236069,1.33133100440341,
95.6341005948603));
#207255=CARTESIAN_POINT('Ctrl Pts',(-6.669776674115,1.15665854709362,95.6424550006858));
#207256=CARTESIAN_POINT('Ctrl Pts',(-6.69550426880555,0.981076748479276,
95.6508094065112));
#207257=CARTESIAN_POINT('Ctrl Pts',(-6.72125887753533,0.805310588534168,
95.6591725844838));
#207258=CARTESIAN_POINT('Ctrl Pts',(-6.74007283333838,0.628633519789852,
95.6675357624564));
#207259=CARTESIAN_POINT('Ctrl Pts',(-6.75191274003437,0.451623018635648,
95.6758989404291));
#207260=CARTESIAN_POINT('Ctrl Pts',(-6.76195530203917,0.301483412050447,
95.6829925548893));
#207261=CARTESIAN_POINT('Ctrl Pts',(-6.76698136676099,0.151104096454122,
95.6900861693496));
#207262=CARTESIAN_POINT('Ctrl Pts',(-6.7669999482633,0.000836782275842868,
95.6971797838099));
#207263=CARTESIAN_POINT('',(-6.76699802674232,-0.00516779117013347,95.3028202162247));
#207264=CARTESIAN_POINT('Ctrl Pts',(3.09910619832125,6.01563211736945,94.6514100603466));
#207265=CARTESIAN_POINT('Ctrl Pts',(2.93949235646195,6.09786125588604,94.6598365869624));
#207266=CARTESIAN_POINT('Ctrl Pts',(2.77663313941226,6.17371884275999,94.6682631135781));
#207267=CARTESIAN_POINT('Ctrl Pts',(2.61106778260609,6.24296516365713,94.6766896401939));
#207268=CARTESIAN_POINT('Ctrl Pts',(2.44544509023424,6.3122354646734,94.6851190849302));
#207269=CARTESIAN_POINT('Ctrl Pts',(2.27711469535598,6.37488980680728,94.6935485296666));
#207270=CARTESIAN_POINT('Ctrl Pts',(2.10663459586528,6.4307371023471,94.7019779744029));
#207271=CARTESIAN_POINT('Ctrl Pts',(1.93599819608286,6.48663560004254,94.7104151474587));
#207272=CARTESIAN_POINT('Ctrl Pts',(1.76320846910119,6.53571447812687,94.7188523205145));
#207273=CARTESIAN_POINT('Ctrl Pts',(1.58883842969782,6.57783257952917,94.7272894935703));
#207274=CARTESIAN_POINT('Ctrl Pts',(1.41438029856451,6.61997195899293,94.7357309290852));
#207275=CARTESIAN_POINT('Ctrl Pts',(1.23834058661119,6.65514347807464,94.7441723646001));
#207276=CARTESIAN_POINT('Ctrl Pts',(1.06130178350248,6.68325725408909,94.7526138001151));
#207277=CARTESIAN_POINT('Ctrl Pts',(0.884070075688366,6.71140166338611,
94.761064433572));
#207278=CARTESIAN_POINT('Ctrl Pts',(0.705837430278023,6.7324729208087,94.7695150670289));
#207279=CARTESIAN_POINT('Ctrl Pts',(0.527191902262931,6.74643296106827,
94.7779657004857));
#207280=CARTESIAN_POINT('Ctrl Pts',(0.44884716015256,6.7525551168599,94.7816717137636));
#207281=CARTESIAN_POINT('Ctrl Pts',(0.370423027894518,6.75731028461828,
94.7853777270414));
#207282=CARTESIAN_POINT('Ctrl Pts',(0.291969074682313,6.76069841506254,
94.7890837403192));
#207283=CARTESIAN_POINT('Ctrl Pts',(0.115918856514544,6.76830136022299,
94.7974000127233));
#207284=CARTESIAN_POINT('Ctrl Pts',(-0.0605992048154732,6.76903077016871,
94.8057162851275));
#207285=CARTESIAN_POINT('Ctrl Pts',(-0.237015202430699,6.76284797949923,
94.8140325575316));
#207286=CARTESIAN_POINT('Ctrl Pts',(-0.413282040112049,6.75667041638654,
94.8223417985176));
#207287=CARTESIAN_POINT('Ctrl Pts',(-0.589446640035441,6.74359230872918,
94.8306510395036));
#207288=CARTESIAN_POINT('Ctrl Pts',(-0.764937249910979,6.72362699766269,
94.8389602804896));
#207289=CARTESIAN_POINT('Ctrl Pts',(-0.940311657841507,6.70367490672223,
94.8472640194721));
#207290=CARTESIAN_POINT('Ctrl Pts',(-1.11501262044503,6.67684473866661,
94.8555677584545));
#207291=CARTESIAN_POINT('Ctrl Pts',(-1.28847143884538,6.6432018147336,94.8638714974369));
#207292=CARTESIAN_POINT('Ctrl Pts',(-1.46184718956637,6.60957500205768,
94.8721712598425));
#207293=CARTESIAN_POINT('Ctrl Pts',(-1.63398164068556,6.56914200154682,
94.880471022248));
#207294=CARTESIAN_POINT('Ctrl Pts',(-1.80431402068705,6.52201961931671,
94.8887707846536));
#207295=CARTESIAN_POINT('Ctrl Pts',(-1.97459603563731,6.47491117055713,
94.8970680929282));
#207296=CARTESIAN_POINT('Ctrl Pts',(-2.14307670663951,6.42111737538106,
94.9053654012028));
#207297=CARTESIAN_POINT('Ctrl Pts',(-2.30920799371961,6.36080556547215,
94.9136627094774));
#207298=CARTESIAN_POINT('Ctrl Pts',(-2.47535606595535,6.3004876619301,94.9219608560746));
#207299=CARTESIAN_POINT('Ctrl Pts',(-2.63915395035085,6.23365053940582,
94.9302590026719));
#207300=CARTESIAN_POINT('Ctrl Pts',(-2.80007069077254,6.16051078455972,
94.9385571492691));
#207301=CARTESIAN_POINT('Ctrl Pts',(-2.96100361238503,6.08736367505105,
94.9468561302972));
#207302=CARTESIAN_POINT('Ctrl Pts',(-3.11905449539384,6.00791281353841,
94.9551551113253));
#207303=CARTESIAN_POINT('Ctrl Pts',(-3.27371431297307,5.92242210561146,
94.9634540923533));
#207304=CARTESIAN_POINT('Ctrl Pts',(-3.42841538528168,5.83690859346765,
94.9717552870929));
#207305=CARTESIAN_POINT('Ctrl Pts',(-3.57972328468885,5.74535219221408,
94.9800564818325));
#207306=CARTESIAN_POINT('Ctrl Pts',(-3.72715528268313,5.64806183560053,
94.988357676572));
#207307=CARTESIAN_POINT('Ctrl Pts',(-3.87465111183475,5.55072935681443,
94.9966624653405));
#207308=CARTESIAN_POINT('Ctrl Pts',(-4.01826740484435,5.44765816651817,
95.004967254109));
#207309=CARTESIAN_POINT('Ctrl Pts',(-4.15755185767649,5.33919952340524,
95.0132720428776));
#207310=CARTESIAN_POINT('Ctrl Pts',(-4.29700143097627,5.23061230354519,
95.0215866768986));
#207311=CARTESIAN_POINT('Ctrl Pts',(-4.43210862885219,5.11662508423684,
95.0299013109196));
#207312=CARTESIAN_POINT('Ctrl Pts',(-4.5624546914198,4.99762905673695,95.0382159449406));
#207313=CARTESIAN_POINT('Ctrl Pts',(-4.69288317295837,4.8785577869939,95.0465358363784));
#207314=CARTESIAN_POINT('Ctrl Pts',(-4.81854426821285,4.75447163723195,
95.0548557278162));
#207315=CARTESIAN_POINT('Ctrl Pts',(-4.93905725149254,4.62579749518707,
95.063175619254));
#207316=CARTESIAN_POINT('Ctrl Pts',(-5.05975044075847,4.49693094357734,
95.0715079516272));
#207317=CARTESIAN_POINT('Ctrl Pts',(-5.17527990584107,4.36346295197853,
95.0798402840004));
#207318=CARTESIAN_POINT('Ctrl Pts',(-5.285305403807,4.22585326158973,95.0881726163736));
#207319=CARTESIAN_POINT('Ctrl Pts',(-5.36814191307135,4.12224903708273,
95.094445901572));
#207320=CARTESIAN_POINT('Ctrl Pts',(-5.44785943194402,4.01629781736874,
95.1007191867703));
#207321=CARTESIAN_POINT('Ctrl Pts',(-5.52432948364893,3.9082058231479,95.1069924719686));
#207322=CARTESIAN_POINT('Ctrl Pts',(-5.62379197454233,3.76761354223343,
95.1151519613111));
#207323=CARTESIAN_POINT('Ctrl Pts',(-5.71806758277806,3.62296217473682,
95.1233114506537));
#207324=CARTESIAN_POINT('Ctrl Pts',(-5.80680017721763,3.47467418643322,
95.1314709399962));
#207325=CARTESIAN_POINT('Ctrl Pts',(-5.89508512257271,3.32713429957558,
95.1395892653454));
#207326=CARTESIAN_POINT('Ctrl Pts',(-5.97788261509272,3.17599468398584,
95.1477075906945));
#207327=CARTESIAN_POINT('Ctrl Pts',(-6.05488091884273,3.02170581934017,
95.1558259160436));
#207328=CARTESIAN_POINT('Ctrl Pts',(-6.13179484964074,2.86758602084709,
95.1639353455205));
#207329=CARTESIAN_POINT('Ctrl Pts',(-6.20292207562393,2.71032416579163,
95.1720447749973));
#207330=CARTESIAN_POINT('Ctrl Pts',(-6.26799429392437,2.55039928860787,
95.1801542044741));
#207331=CARTESIAN_POINT('Ctrl Pts',(-6.33300770738426,2.3906189332669,95.1882563055746));
#207332=CARTESIAN_POINT('Ctrl Pts',(-6.39197686717571,2.22818068358095,
95.1963584066751));
#207333=CARTESIAN_POINT('Ctrl Pts',(-6.44467957671181,2.06358768980473,
95.2044605077756));
#207334=CARTESIAN_POINT('Ctrl Pts',(-6.49799726017764,1.89707410406887,
95.2126571501435));
#207335=CARTESIAN_POINT('Ctrl Pts',(-6.54490113992903,1.72835550117301,
95.2208537925113));
#207336=CARTESIAN_POINT('Ctrl Pts',(-6.5852111044506,1.55797423272034,95.2290504348791));
#207337=CARTESIAN_POINT('Ctrl Pts',(-6.6250059872246,1.38977010043113,95.2371423403432));
#207338=CARTESIAN_POINT('Ctrl Pts',(-6.65837438342804,1.21994591049759,
95.2452342458073));
#207339=CARTESIAN_POINT('Ctrl Pts',(-6.68519307302459,1.04903888220792,
95.2533261512713));
#207340=CARTESIAN_POINT('Ctrl Pts',(-6.71253245083062,0.874813672609407,
95.261575162091));
#207341=CARTESIAN_POINT('Ctrl Pts',(-6.73306507342869,0.699463520814487,
95.2698241729108));
#207342=CARTESIAN_POINT('Ctrl Pts',(-6.74671515434204,0.523568167645297,
95.2780731837305));
#207343=CARTESIAN_POINT('Ctrl Pts',(-6.7603652352554,0.347672814475979,
95.2863221945502));
#207344=CARTESIAN_POINT('Ctrl Pts',(-6.7671327394428,0.171232663151217,
95.29457120537));
#207345=CARTESIAN_POINT('Ctrl Pts',(-6.76699802674289,-0.0051677904223947,
95.3028202161897));
#207346=CARTESIAN_POINT('Ctrl Pts',(-6.76699802674232,-0.0051677911699413,
95.3028202162247));
#207347=CARTESIAN_POINT('Ctrl Pts',(-6.76685125828067,-0.197354715467158,
95.3118074494536));
#207348=CARTESIAN_POINT('Ctrl Pts',(-6.75851323921425,-0.389205863367142,
95.3207946826824));
#207349=CARTESIAN_POINT('Ctrl Pts',(-6.74209344069607,-0.5800560636034,
95.3297819159113));
#207350=CARTESIAN_POINT('Ctrl Pts',(-6.72557542582627,-0.772047849733753,
95.338822907002));
#207351=CARTESIAN_POINT('Ctrl Pts',(-6.7008787490104,-0.963026460833392,
95.3478638980926));
#207352=CARTESIAN_POINT('Ctrl Pts',(-6.66816458479939,-1.15233244770216,
95.3569048891833));
#207353=CARTESIAN_POINT('Ctrl Pts',(-6.63534812016205,-1.34223041311084,
95.3659741523471));
#207354=CARTESIAN_POINT('Ctrl Pts',(-6.59446406922571,-1.53044507688767,
95.3750434155108));
#207355=CARTESIAN_POINT('Ctrl Pts',(-6.54572337338254,-1.71633170429073,
95.3841126786746));
#207356=CARTESIAN_POINT('Ctrl Pts',(-6.49676834367769,-1.90303575536812,
95.3932218233001));
#207357=CARTESIAN_POINT('Ctrl Pts',(-6.43988753964119,-2.08739105330672,
95.4023309679256));
#207358=CARTESIAN_POINT('Ctrl Pts',(-6.37534147991665,-2.26876839154069,
95.4114401125511));
#207359=CARTESIAN_POINT('Ctrl Pts',(-6.34354704243316,-2.35811219449339,
95.4159271429068));
#207360=CARTESIAN_POINT('Ctrl Pts',(-6.30989340892669,-2.44673381102486,
95.4204141732625));
#207361=CARTESIAN_POINT('Ctrl Pts',(-6.27441572084779,-2.53456038830763,
95.4249012036182));
#207362=CARTESIAN_POINT('Ctrl Pts',(-6.209349355766,-2.69563503693346,95.4331304533541));
#207363=CARTESIAN_POINT('Ctrl Pts',(-6.13798081565125,-2.85443922199044,
95.4413597030901));
#207364=CARTESIAN_POINT('Ctrl Pts',(-6.06048789807765,-3.0104443919884,
95.4495889528261));
#207365=CARTESIAN_POINT('Ctrl Pts',(-5.98308720968262,-3.1662638904549,
95.4578084084161));
#207366=CARTESIAN_POINT('Ctrl Pts',(-5.89957681572885,-3.31929068910676,
95.4660278640061));
#207367=CARTESIAN_POINT('Ctrl Pts',(-5.81018333724418,-3.46901406564027,
95.4742473195961));
#207368=CARTESIAN_POINT('Ctrl Pts',(-5.7208782991314,-3.61858931513673,
95.4824586433658));
#207369=CARTESIAN_POINT('Ctrl Pts',(-5.62570195016482,-3.76486734524126,
95.4906699671355));
#207370=CARTESIAN_POINT('Ctrl Pts',(-5.52492782207648,-3.90735992210153,
95.4988812909052));
#207371=CARTESIAN_POINT('Ctrl Pts',(-5.424233163062,-4.04974013130028,95.5070861393393));
#207372=CARTESIAN_POINT('Ctrl Pts',(-5.31794972337494,-4.18834054147748,
95.5152909877734));
#207373=CARTESIAN_POINT('Ctrl Pts',(-5.20639558216113,-4.32269985565192,
95.5234958362075));
#207374=CARTESIAN_POINT('Ctrl Pts',(-5.09490702204723,-4.45698018188821,
95.5316958611274));
#207375=CARTESIAN_POINT('Ctrl Pts',(-4.97815416155505,-4.58702410378795,
95.5398958860473));
#207376=CARTESIAN_POINT('Ctrl Pts',(-4.85649683670507,-4.71240145521088,
95.5480959109672));
#207377=CARTESIAN_POINT('Ctrl Pts',(-4.7348747222409,-4.83774251958805,
95.5562935626141));
#207378=CARTESIAN_POINT('Ctrl Pts',(-4.60835121740478,-4.95841944390518,
95.5644912142611));
#207379=CARTESIAN_POINT('Ctrl Pts',(-4.47732484351252,-5.07403697716774,
95.572688865908));
#207380=CARTESIAN_POINT('Ctrl Pts',(-4.34631601485576,-5.18963902853313,
95.5808854198391));
#207381=CARTESIAN_POINT('Ctrl Pts',(-4.21080578637142,-5.30018280022209,
95.5890819737701));
#207382=CARTESIAN_POINT('Ctrl Pts',(-4.07122776988145,-5.40531159562019,
95.5972785277012));
#207383=CARTESIAN_POINT('Ctrl Pts',(-3.93164306483399,-5.51044542877431,
95.6054754744099));
#207384=CARTESIAN_POINT('Ctrl Pts',(-3.7879904699832,-5.61016355278476,
95.6136724211186));
#207385=CARTESIAN_POINT('Ctrl Pts',(-3.64073477803065,-5.70415105655856,
95.6218693678273));
#207386=CARTESIAN_POINT('Ctrl Pts',(-3.49344525475554,-5.79816015353201,
95.6300681977471));
#207387=CARTESIAN_POINT('Ctrl Pts',(-3.34255128800087,-5.88643581505879,
95.6382670276668));
#207388=CARTESIAN_POINT('Ctrl Pts',(-3.1885446385984,-5.96870774017839,
95.6464658575866));
#207389=CARTESIAN_POINT('Ctrl Pts',(-3.03439212521109,-6.05105758732853,
95.6546724528464));
#207390=CARTESIAN_POINT('Ctrl Pts',(-2.87712135596695,-6.12739216809328,
95.6628790481062));
#207391=CARTESIAN_POINT('Ctrl Pts',(-2.71724741809939,-6.19748783531135,
95.671085643366));
#207392=CARTESIAN_POINT('Ctrl Pts',(-2.55729610032918,-6.26761742923429,
95.679296210665));
#207393=CARTESIAN_POINT('Ctrl Pts',(-2.39473943558964,-6.33150195796964,
95.6875067779639));
#207394=CARTESIAN_POINT('Ctrl Pts',(-2.23011017740507,-6.38896686457477,
95.6957173452629));
#207395=CARTESIAN_POINT('Ctrl Pts',(-2.06525387190525,-6.44651102351274,
95.7039392361096));
#207396=CARTESIAN_POINT('Ctrl Pts',(-1.89831960354303,-6.49761776133823,
95.7121611269563));
#207397=CARTESIAN_POINT('Ctrl Pts',(-1.72985408500851,-6.54216278034867,
95.720383017803));
#207398=CARTESIAN_POINT('Ctrl Pts',(-1.57667917061277,-6.58266471530269,
95.727858656958));
#207399=CARTESIAN_POINT('Ctrl Pts',(-1.42223869230681,-6.61774260765869,
95.7353342961129));
#207400=CARTESIAN_POINT('Ctrl Pts',(-1.26694830326736,-6.64734014451254,
95.7428099352679));
#207401=CARTESIAN_POINT('Ctrl Pts',(-1.08132322076399,-6.68271931546043,
95.7517458787186));
#207402=CARTESIAN_POINT('Ctrl Pts',(-0.894097159413995,-6.71034148187159,
95.7606818221693));
#207403=CARTESIAN_POINT('Ctrl Pts',(-0.705911292581039,-6.73008010702745,
95.7696177656201));
#207404=CARTESIAN_POINT('Ctrl Pts',(-0.518008319019261,-6.74978905979434,
95.7785402759777));
#207405=CARTESIAN_POINT('Ctrl Pts',(-0.329148675146541,-6.76163809135364,
95.7874627863354));
#207406=CARTESIAN_POINT('Ctrl Pts',(-0.13998152700382,-6.76555202271756,
95.796385296693));
#207407=CARTESIAN_POINT('Ctrl Pts',(0.0487221029221133,-6.76945636373504,
95.8052859441313));
#207408=CARTESIAN_POINT('Ctrl Pts',(0.237731475622388,-6.76546440491512,
95.8141865915697));
#207409=CARTESIAN_POINT('Ctrl Pts',(0.426395154337038,-6.75355285552411,
95.823087239008));
#207410=CARTESIAN_POINT('Ctrl Pts',(0.614767276621399,-6.74165971396255,
95.8319741315943));
#207411=CARTESIAN_POINT('Ctrl Pts',(0.802794514158681,-6.72187141111576,
95.8408610241805));
#207412=CARTESIAN_POINT('Ctrl Pts',(0.98982527887892,-6.69421652751779,
95.8497479167668));
#207413=CARTESIAN_POINT('Ctrl Pts',(1.17637530471704,-6.66663272729396,
95.8586119667217));
#207414=CARTESIAN_POINT('Ctrl Pts',(1.36193371398728,-6.63122273168152,
95.8674760166766));
#207415=CARTESIAN_POINT('Ctrl Pts',(1.54585465461591,-6.58806666532772,
95.8763400666316));
#207416=CARTESIAN_POINT('Ctrl Pts',(1.72169786927129,-6.54680599422853,
95.8848148114519));
#207417=CARTESIAN_POINT('Ctrl Pts',(1.89604409524305,-6.49846505228454,
95.8932895562722));
#207418=CARTESIAN_POINT('Ctrl Pts',(2.06833282201662,-6.44315825797945,
95.9017643010925));
#207419=CARTESIAN_POINT('Ctrl Pts',(2.23521730587638,-6.38958629192926,
95.9099732155216));
#207420=CARTESIAN_POINT('Ctrl Pts',(2.4000101777703,-6.32952933579917,95.9181821299508));
#207421=CARTESIAN_POINT('Ctrl Pts',(2.56218324479872,-6.26318657075396,
95.9263910443798));
#207422=CARTESIAN_POINT('Ctrl Pts',(2.72439486764991,-6.19682803305341,
95.9346019104366));
#207423=CARTESIAN_POINT('Ctrl Pts',(2.88398511517514,-6.12418084396062,
95.9428127764934));
#207424=CARTESIAN_POINT('Ctrl Pts',(3.04044665877479,-6.04549196634527,
95.9510236425502));
#207425=CARTESIAN_POINT('Ctrl Pts',(3.19697329023779,-5.96677035422664,
95.95923792432));
#207426=CARTESIAN_POINT('Ctrl Pts',(3.35036830698329,-5.88200220634624,
95.9674522060898));
#207427=CARTESIAN_POINT('Ctrl Pts',(3.50014974885115,-5.79148001253714,
95.9756664878596));
#207428=CARTESIAN_POINT('Ctrl Pts',(3.65009978155624,-5.7008559288527,95.983890015452));
#207429=CARTESIAN_POINT('Ctrl Pts',(3.79642781065042,-5.60446504751834,
95.9921135430443));
#207430=CARTESIAN_POINT('Ctrl Pts',(3.93868078967053,-5.5026432409416,96.0003370706367));
#207431=CARTESIAN_POINT('Ctrl Pts',(4.08102494731668,-5.40075617054764,
96.0085658691904));
#207432=CARTESIAN_POINT('Ctrl Pts',(4.21928856757974,-5.29343145350961,
96.0167946677441));
#207433=CARTESIAN_POINT('Ctrl Pts',(4.35305243512652,-5.18104463376249,
96.0250234662978));
#207434=CARTESIAN_POINT('Ctrl Pts',(4.48700041793267,-5.06850312255162,
96.0332635911342));
#207435=CARTESIAN_POINT('Ctrl Pts',(4.61643601421664,-4.95088583029674,
96.0415037159706));
#207436=CARTESIAN_POINT('Ctrl Pts',(4.74097682691424,-4.82860515331936,
96.049743840807));
#207437=CARTESIAN_POINT('Ctrl Pts',(4.79626780814425,-4.77431757907679,
96.0534021161771));
#207438=CARTESIAN_POINT('Ctrl Pts',(4.85059456019711,-4.71911129556049,
96.0570603915472));
#207439=CARTESIAN_POINT('Ctrl Pts',(4.90392623067133,-4.66302439669081,
96.0607186669173));
#207440=CARTESIAN_POINT('Ctrl Pts',(5.02708458277735,-4.53350342016588,
96.0691666896798));
#207441=CARTESIAN_POINT('Ctrl Pts',(5.14521543230861,-4.39898777269238,
96.0776147124423));
#207442=CARTESIAN_POINT('Ctrl Pts',(5.25790700161998,-4.25989471258571,
96.0860627352049));
#207443=CARTESIAN_POINT('Ctrl Pts',(5.3704953758957,-4.1209290241483,96.0945030218607));
#207444=CARTESIAN_POINT('Ctrl Pts',(5.47765418944091,-3.97739453621532,
96.1029433085164));
#207445=CARTESIAN_POINT('Ctrl Pts',(5.57900989112737,-3.8297438079724,96.1113835951722));
#207446=CARTESIAN_POINT('Ctrl Pts',(5.68028838151141,-3.68220555791119,
96.1198174521401));
#207447=CARTESIAN_POINT('Ctrl Pts',(5.7757723846831,-3.53055759254873,96.128251309108));
#207448=CARTESIAN_POINT('Ctrl Pts',(5.86512964378643,-3.37528417493664,
96.1366851660759));
#207449=CARTESIAN_POINT('Ctrl Pts',(5.95443256903717,-3.22010517162359,
96.145113894821));
#207450=CARTESIAN_POINT('Ctrl Pts',(6.0376160116873,-3.06130539951905,96.153542623566));
#207451=CARTESIAN_POINT('Ctrl Pts',(6.11439173269742,-2.89939696128721,
96.161971352311));
#207452=CARTESIAN_POINT('Ctrl Pts',(6.19113255998483,-2.73756210866385,
96.1703962502913));
#207453=CARTESIAN_POINT('Ctrl Pts',(6.26147133000044,-2.57262170799719,
96.1788211482716));
#207454=CARTESIAN_POINT('Ctrl Pts',(6.32516617778657,-2.40511160310386,
96.1872460462519));
#207455=CARTESIAN_POINT('Ctrl Pts',(6.38884692342967,-2.23763858522056,
96.1956690789461));
#207456=CARTESIAN_POINT('Ctrl Pts',(6.44588655879162,-2.06759730796299,
96.2040921116403));
#207457=CARTESIAN_POINT('Ctrl Pts',(6.49609151775605,-1.89554319205286,
96.2125151443344));
#207458=CARTESIAN_POINT('Ctrl Pts',(6.54629079608638,-1.72350854387056,
96.220937223972));
#207459=CARTESIAN_POINT('Ctrl Pts',(6.58965684630891,-1.5494618311258,96.2293593036096));
#207460=CARTESIAN_POINT('Ctrl Pts',(6.62604601267164,-1.37397352156373,
96.2377813832472));
#207461=CARTESIAN_POINT('Ctrl Pts',(6.66243614129735,-1.19848057144738,
96.2462036855955));
#207462=CARTESIAN_POINT('Ctrl Pts',(6.69184895089623,-1.0215462751138,96.2546259879437));
#207463=CARTESIAN_POINT('Ctrl Pts',(6.71419186056453,-0.843751538978782,
96.263048290292));
#207464=CARTESIAN_POINT('Ctrl Pts',(6.73653848014587,-0.665927281039336,
96.2714719911156));
#207465=CARTESIAN_POINT('Ctrl Pts',(6.75181281838071,-0.48724262935804,
96.2798956919392));
#207466=CARTESIAN_POINT('Ctrl Pts',(6.75997409994863,-0.308284232525387,
96.2883193927629));
#207467=CARTESIAN_POINT('Ctrl Pts',(6.76814090433038,-0.129204732909792,
96.2967487939819));
#207468=CARTESIAN_POINT('Ctrl Pts',(6.76918501836201,0.0501485485583775,
96.3051781952008));
#207469=CARTESIAN_POINT('Ctrl Pts',(6.76311778520249,0.229187310900414,
96.3136075964198));
#207470=CARTESIAN_POINT('Ctrl Pts',(6.75704838726261,0.408289954024154,
96.3220400052374));
#207471=CARTESIAN_POINT('Ctrl Pts',(6.74386260028697,0.587077521215506,
96.3304724140551));
#207472=CARTESIAN_POINT('Ctrl Pts',(6.72362376949708,0.764965624230176,
96.3389048228727));
#207473=CARTESIAN_POINT('Ctrl Pts',(6.70336621315207,0.943018314493633,
96.3473450336003));
#207474=CARTESIAN_POINT('Ctrl Pts',(6.67604261856037,1.12016954705363,96.355785244328));
#207475=CARTESIAN_POINT('Ctrl Pts',(6.64176786520474,1.29584282408544,96.3642254550556));
#207476=CARTESIAN_POINT('Ctrl Pts',(6.6222729703647,1.3957627863505,96.3690261028927));
#207477=CARTESIAN_POINT('Ctrl Pts',(6.60053021063109,1.4952048100933,96.3738267507297));
#207478=CARTESIAN_POINT('Ctrl Pts',(6.57656798188469,1.59406479782006,96.3786273985668));
#207479=CARTESIAN_POINT('Ctrl Pts',(6.53593894177013,1.76168636798307,96.3867671135996));
#207480=CARTESIAN_POINT('Ctrl Pts',(6.48884530541958,1.9279680304558,96.3949068286325));
#207481=CARTESIAN_POINT('Ctrl Pts',(6.43539258761967,2.09236976732359,96.4030465436654));
#207482=CARTESIAN_POINT('Ctrl Pts',(6.38198661924602,2.25662771941878,96.4111791397523));
#207483=CARTESIAN_POINT('Ctrl Pts',(6.32223275223909,2.41900867274407,96.4193117358393));
#207484=CARTESIAN_POINT('Ctrl Pts',(6.25628725600429,2.57898405779454,96.4274443319262));
#207485=CARTESIAN_POINT('Ctrl Pts',(6.19038684364855,2.73885007508943,96.4355713681342));
#207486=CARTESIAN_POINT('Ctrl Pts',(6.11830336860602,2.89631346119327,96.4436984043421));
#207487=CARTESIAN_POINT('Ctrl Pts',(6.04024250595037,3.05086208624881,96.4518254405501));
#207488=CARTESIAN_POINT('Ctrl Pts',(5.96221895779985,3.20533683426447,96.4599485918876));
#207489=CARTESIAN_POINT('Ctrl Pts',(5.87822387660907,3.356899269582,96.4680717432252));
#207490=CARTESIAN_POINT('Ctrl Pts',(5.78851050328361,3.50505850926563,96.4761948945628));
#207491=CARTESIAN_POINT('Ctrl Pts',(5.69882234008279,3.6531761151018,96.4843157632344));
#207492=CARTESIAN_POINT('Ctrl Pts',(5.60341927553491,3.79789211753768,96.4924366319061));
#207493=CARTESIAN_POINT('Ctrl Pts',(5.50259979239729,3.93874148995708,96.5005575005777));
#207494=CARTESIAN_POINT('Ctrl Pts',(5.40177486058888,4.0795984744157,96.5086788081322));
#207495=CARTESIAN_POINT('Ctrl Pts',(5.29553313531284,4.2165881112698,96.5168001156867));
#207496=CARTESIAN_POINT('Ctrl Pts',(5.18421570530295,4.34927540182157,96.5249214232412));
#207497=CARTESIAN_POINT('Ctrl Pts',(5.12637129907314,4.41822433044424,96.529141536958));
#207498=CARTESIAN_POINT('Ctrl Pts',(5.06715702965564,4.48601206089266,96.5333616506747));
#207499=CARTESIAN_POINT('Ctrl Pts',(5.0066249862165,4.55258116318563,96.5375817643915));
#207500=CARTESIAN_POINT('Ctrl Pts',(4.87781571041155,4.69423700974505,96.5465619633206));
#207501=CARTESIAN_POINT('Ctrl Pts',(4.74310104553792,4.83030255785421,96.5555421622498));
#207502=CARTESIAN_POINT('Ctrl Pts',(4.60297897068858,4.9603299885591,96.5645223611789));
#207503=CARTESIAN_POINT('Ctrl Pts',(4.46249551332879,5.09069276713395,96.5735257205332));
#207504=CARTESIAN_POINT('Ctrl Pts',(4.31657691694639,5.21498610547453,96.5825290798875));
#207505=CARTESIAN_POINT('Ctrl Pts',(4.16575584732585,5.33280106702571,96.5915324392419));
#207506=CARTESIAN_POINT('Ctrl Pts',(4.01474440479513,5.4507647397427,96.6005471630278));
#207507=CARTESIAN_POINT('Ctrl Pts',(3.85881831625122,5.5622335545351,96.6095618868136));
#207508=CARTESIAN_POINT('Ctrl Pts',(3.69854003538396,5.66684132534713,96.6185766105995));
#207509=CARTESIAN_POINT('Ctrl Pts',(3.53801115510602,5.77161265322739,96.6276054291489));
#207510=CARTESIAN_POINT('Ctrl Pts',(3.37311667741377,5.86950135883824,96.6366342476984));
#207511=CARTESIAN_POINT('Ctrl Pts',(3.20444633434113,5.96018562549253,96.6456630662478));
#207512=CARTESIAN_POINT('Ctrl Pts',(3.16949323645566,5.9789778802025,96.6475340838363));
#207513=CARTESIAN_POINT('Ctrl Pts',(3.13437806885556,5.99746091433267,96.6494051014248));
#207514=CARTESIAN_POINT('Ctrl Pts',(3.09910619832137,6.01563211736939,96.6512761190133));
#207515=CARTESIAN_POINT('Origin',(0.,0.,4.30282021618968));
#207516=CARTESIAN_POINT('',(3.09910619832142,6.01563211736936,99.0457552630242));
#207517=CARTESIAN_POINT('',(3.09910619832134,6.0156321173694,98.651562053011));
#207518=CARTESIAN_POINT('',(3.09910619832133,6.0156321173694,4.30282021618968));
#207519=CARTESIAN_POINT('',(-6.767,8.45744073366125E-10,97.6971797837703));
#207520=CARTESIAN_POINT('Ctrl Pts',(-6.767,4.49310309984705E-12,97.6971797838099));
#207521=CARTESIAN_POINT('Ctrl Pts',(-6.76700000000012,-0.186007249522473,
97.7059292956211));
#207522=CARTESIAN_POINT('Ctrl Pts',(-6.75932637294544,-0.372014355745619,
97.7146788074323));
#207523=CARTESIAN_POINT('Ctrl Pts',(-6.74400518264215,-0.557389537483297,
97.7234283192435));
#207524=CARTESIAN_POINT('Ctrl Pts',(-6.7286840570513,-0.742763936247776,
97.7321777940991));
#207525=CARTESIAN_POINT('Ctrl Pts',(-6.70571545645778,-0.927506130238429,
97.7409272689548));
#207526=CARTESIAN_POINT('Ctrl Pts',(-6.67517739404862,-1.11098863989795,
97.7496767438105));
#207527=CARTESIAN_POINT('Ctrl Pts',(-6.64463945808741,-1.29447038981747,
97.7584261824375));
#207528=CARTESIAN_POINT('Ctrl Pts',(-6.60653217008395,-1.47669218313505,
97.7671756210645));
#207529=CARTESIAN_POINT('Ctrl Pts',(-6.56098496092717,-1.65703510599129,
97.7759250596916));
#207530=CARTESIAN_POINT('Ctrl Pts',(-6.51543793658342,-1.83737729708539,
97.7846744628167));
#207531=CARTESIAN_POINT('Ctrl Pts',(-6.46245112167471,-2.01584035510763,
97.7934238659419));
#207532=CARTESIAN_POINT('Ctrl Pts',(-6.4022044837431,-2.19181813760625,
97.8021732690671));
#207533=CARTESIAN_POINT('Ctrl Pts',(-6.34195808526559,-2.36779522066997,
97.8109226374172));
#207534=CARTESIAN_POINT('Ctrl Pts',(-6.27445201433156,-2.54128677684038,
97.8196720057673));
#207535=CARTESIAN_POINT('Ctrl Pts',(-6.19991555071949,-2.71170355384703,
97.8284213741174));
#207536=CARTESIAN_POINT('Ctrl Pts',(-6.12537937716739,-2.88211966767378,
97.8371707084192));
#207537=CARTESIAN_POINT('Ctrl Pts',(-6.04381298052565,-3.04946076371696,
97.8459200427209));
#207538=CARTESIAN_POINT('Ctrl Pts',(-5.95549339335875,-3.21315848374467,
97.8546693770227));
#207539=CARTESIAN_POINT('Ctrl Pts',(-5.86717414255452,-3.37685558033418,
97.8634186780029));
#207540=CARTESIAN_POINT('Ctrl Pts',(-5.7721018887664,-3.53690907646688,
97.8721679789831));
#207541=CARTESIAN_POINT('Ctrl Pts',(-5.67059953347036,-3.69277536969225,
97.8809172799633));
#207542=CARTESIAN_POINT('Ctrl Pts',(-5.56909755631428,-3.8486410822486,
97.8896665483486));
#207543=CARTESIAN_POINT('Ctrl Pts',(-5.46116568196897,-4.00031938297452,
97.8984158167339));
#207544=CARTESIAN_POINT('Ctrl Pts',(-5.34717048533654,-4.14729511859788,
97.9071650851191));
#207545=CARTESIAN_POINT('Ctrl Pts',(-5.23317570391888,-4.29427031887854,
97.9159143216362));
#207546=CARTESIAN_POINT('Ctrl Pts',(-5.11311782003565,-4.43654276189488,
97.9246635581532));
#207547=CARTESIAN_POINT('Ctrl Pts',(-4.98740458984804,-4.57362924351797,
97.9334127946703));
#207548=CARTESIAN_POINT('Ctrl Pts',(-4.86169180711819,-4.71071523720187,
97.9421620000457));
#207549=CARTESIAN_POINT('Ctrl Pts',(-4.73032391204274,-4.84261509523136,
97.9509112054211));
#207550=CARTESIAN_POINT('Ctrl Pts',(-4.5937470701373,-4.96888084538208,
97.9596604107965));
#207551=CARTESIAN_POINT('Ctrl Pts',(-4.45717070301595,-5.09514615659332,
97.968409585757));
#207552=CARTESIAN_POINT('Ctrl Pts',(-4.3153856357121,-5.21577720459387,
97.9771587607174));
#207553=CARTESIAN_POINT('Ctrl Pts',(-4.16887341029699,-5.33036429232738,
97.9859079356779));
#207554=CARTESIAN_POINT('Ctrl Pts',(-4.02236168203894,-5.44495099123477,
97.9946570809499));
#207555=CARTESIAN_POINT('Ctrl Pts',(-3.8711230534835,-5.55349359438473,
98.0034062262219));
#207556=CARTESIAN_POINT('Ctrl Pts',(-3.71567117017942,-5.65562346298775,
98.0121553714939));
#207557=CARTESIAN_POINT('Ctrl Pts',(-3.56021980145993,-5.75775299351537,
98.0209044878041));
#207558=CARTESIAN_POINT('Ctrl Pts',(-3.40055544538517,-5.85346967463776,
98.0296536041143));
#207559=CARTESIAN_POINT('Ctrl Pts',(-3.23722035987013,-5.94244842986814,
98.0384027204244));
#207560=CARTESIAN_POINT('Ctrl Pts',(-3.07388580147316,-6.03142689794461,
98.0471518084993));
#207561=CARTESIAN_POINT('Ctrl Pts',(-2.90688078896689,-6.1136673465673,
98.0559008965742));
#207562=CARTESIAN_POINT('Ctrl Pts',(-2.73677250721455,-6.18889046952316,
98.064649984649));
#207563=CARTESIAN_POINT('Ctrl Pts',(-2.56666476031572,-6.2641133559629,
98.0733990452151));
#207564=CARTESIAN_POINT('Ctrl Pts',(-2.3934540257526,-6.3323188450052,98.0821481057811));
#207565=CARTESIAN_POINT('Ctrl Pts',(-2.21772856065691,-6.39327529762692,
98.0908971663471));
#207566=CARTESIAN_POINT('Ctrl Pts',(-2.042003633486,-6.45423156365084,98.0996462001308));
#207567=CARTESIAN_POINT('Ctrl Pts',(-1.86376426189351,-6.50793874375638,
98.1083952339145));
#207568=CARTESIAN_POINT('Ctrl Pts',(-1.68361577753213,-6.55421443909527,
98.1171442676982));
#207569=CARTESIAN_POINT('Ctrl Pts',(-1.50346782967874,-6.60048999661851,
98.125893275426));
#207570=CARTESIAN_POINT('Ctrl Pts',(-1.32141105795077,-6.63933404237694,
98.1346422831538));
#207571=CARTESIAN_POINT('Ctrl Pts',(-1.13806375487129,-6.67061465607543,
98.1433912908817));
#207572=CARTESIAN_POINT('Ctrl Pts',(-0.954716982604495,-6.70189517921274,
98.15214027328));
#207573=CARTESIAN_POINT('Ctrl Pts',(-0.770079968904035,-6.72561226592205,
98.1608892556784));
#207574=CARTESIAN_POINT('Ctrl Pts',(-0.584779765560561,-6.74168536983082,
98.1696382380768));
#207575=CARTESIAN_POINT('Ctrl Pts',(-0.391489830653644,-6.75845151013839,
98.1787644570867));
#207576=CARTESIAN_POINT('Ctrl Pts',(-0.197478578240707,-6.76689983031618,
98.1878906760965));
#207577=CARTESIAN_POINT('Ctrl Pts',(-0.00346287645373946,-6.76699911397118,
98.1970168951064));
#207578=CARTESIAN_POINT('Ctrl Pts',(0.184489834652353,-6.76709529501195,
98.2058579197722));
#207579=CARTESIAN_POINT('Ctrl Pts',(0.372446404247802,-6.75935639738177,
98.214698944438));
#207580=CARTESIAN_POINT('Ctrl Pts',(0.559755019486738,-6.743809258732,98.2235399691039));
#207581=CARTESIAN_POINT('Ctrl Pts',(0.745134705520139,-6.72842222659824,
98.2322899477136));
#207582=CARTESIAN_POINT('Ctrl Pts',(0.929879431226895,-6.70538706057547,
98.2410399263233));
#207583=CARTESIAN_POINT('Ctrl Pts',(1.11336163626655,-6.67478200894156,
98.2497899049331));
#207584=CARTESIAN_POINT('Ctrl Pts',(1.29684196300553,-6.64417727061045,
98.2585397939696));
#207585=CARTESIAN_POINT('Ctrl Pts',(1.4790595121735,-6.60600284890626,98.2672896830061));
#207586=CARTESIAN_POINT('Ctrl Pts',(1.65939532066929,-6.5603884160727,98.2760395720426));
#207587=CARTESIAN_POINT('Ctrl Pts',(1.83972934300659,-6.51477443503297,
98.2847893744148));
#207588=CARTESIAN_POINT('Ctrl Pts',(2.01818138406136,-6.46172066062182,
98.293539176787));
#207589=CARTESIAN_POINT('Ctrl Pts',(2.19414528354083,-6.40140730423518,
98.3022889791591));
#207590=CARTESIAN_POINT('Ctrl Pts',(2.37010749863872,-6.3410945251869,98.3110386977754));
#207591=CARTESIAN_POINT('Ctrl Pts',(2.54358134866321,-6.2735223961656,98.3197884163918));
#207592=CARTESIAN_POINT('Ctrl Pts',(2.71397759435406,-6.19892043966884,
98.3285381350081));
#207593=CARTESIAN_POINT('Ctrl Pts',(2.8843722655797,-6.12431917249587,98.3372877727768));
#207594=CARTESIAN_POINT('Ctrl Pts',(3.05168912680798,-6.04268832278878,
98.3460374105455));
#207595=CARTESIAN_POINT('Ctrl Pts',(3.21535986273693,-5.95430516123421,
98.3547870483142));
#207596=CARTESIAN_POINT('Ctrl Pts',(3.37902914072688,-5.86592278697529,
98.3635366081433));
#207597=CARTESIAN_POINT('Ctrl Pts',(3.53905210621426,-5.77078835742031,
98.3722861679723));
#207598=CARTESIAN_POINT('Ctrl Pts',(3.69488522831559,-5.66922500431719,
98.3810357278014));
#207599=CARTESIAN_POINT('Ctrl Pts',(3.8507170140682,-5.56766252217177,98.3897852125985));
#207600=CARTESIAN_POINT('Ctrl Pts',(4.00235878822301,-5.45967138329446,
98.3985346973956));
#207601=CARTESIAN_POINT('Ctrl Pts',(4.14929549611238,-5.34561838199675,
98.4072841821928));
#207602=CARTESIAN_POINT('Ctrl Pts',(4.29623099276,-5.23156632087089,98.4160335948654));
#207603=CARTESIAN_POINT('Ctrl Pts',(4.43846127435936,-5.11145267305044,
98.4247830075379));
#207604=CARTESIAN_POINT('Ctrl Pts',(4.57550326054348,-4.98568540049972,
98.4335324202105));
#207605=CARTESIAN_POINT('Ctrl Pts',(4.71254416257686,-4.85991912290452,
98.4422817636658));
#207606=CARTESIAN_POINT('Ctrl Pts',(4.84439664018666,-4.72849950385516,
98.451031107121));
#207607=CARTESIAN_POINT('Ctrl Pts',(4.9706128679465,-4.59187289861171,98.4597804505763));
#207608=CARTESIAN_POINT('Ctrl Pts',(5.09682813912586,-4.45524732884798,
98.4685297277211));
#207609=CARTESIAN_POINT('Ctrl Pts',(5.21740705147737,-4.3134150623591,98.4772790048659));
#207610=CARTESIAN_POINT('Ctrl Pts',(5.33194007545592,-4.16685781275856,
98.4860282820107));
#207611=CARTESIAN_POINT('Ctrl Pts',(5.44647226944372,-4.02030162521994,
98.4947774957519));
#207612=CARTESIAN_POINT('Ctrl Pts',(5.55495848627992,-3.86902074888107,
98.5035267094929));
#207613=CARTESIAN_POINT('Ctrl Pts',(5.6570302729166,-3.71352898080857,98.5122759232341));
#207614=CARTESIAN_POINT('Ctrl Pts',(5.75910135376881,-3.55803828789777,
98.5210250764779));
#207615=CARTESIAN_POINT('Ctrl Pts',(5.85475793592646,-3.39833700106895,
98.5297742297219));
#207616=CARTESIAN_POINT('Ctrl Pts',(5.94367514427302,-3.2349675082373,98.5385233829657));
#207617=CARTESIAN_POINT('Ctrl Pts',(6.03259176732553,-3.07159909077896,
98.5472724786187));
#207618=CARTESIAN_POINT('Ctrl Pts',(6.11476896835846,-2.90456276731599,
98.5560215742716));
#207619=CARTESIAN_POINT('Ctrl Pts',(6.18992765547817,-2.73442583003208,
98.5647706699245));
#207620=CARTESIAN_POINT('Ctrl Pts',(6.26508587282987,-2.56428995616335,
98.5735197108925));
#207621=CARTESIAN_POINT('Ctrl Pts',(6.33322554827095,-2.39105376935373,
98.5822687518606));
#207622=CARTESIAN_POINT('Ctrl Pts',(6.39411526732969,-2.21530561054258,
98.5910177928286));
#207623=CARTESIAN_POINT('Ctrl Pts',(6.45500462602788,-2.03955849185287,
98.5997667820176));
#207624=CARTESIAN_POINT('Ctrl Pts',(6.50864402040683,-1.86129970164743,
98.6085157712066));
#207625=CARTESIAN_POINT('Ctrl Pts',(6.55485128368548,-1.68113463136267,
98.6172647603957));
#207626=CARTESIAN_POINT('Ctrl Pts',(6.60199809554277,-1.49730620117087,
98.6261916458671));
#207627=CARTESIAN_POINT('Ctrl Pts',(6.64140720707828,-1.31149343245927,
98.6351185313385));
#207628=CARTESIAN_POINT('Ctrl Pts',(6.67293928722843,-1.12435326697764,
98.64404541681));
#207629=CARTESIAN_POINT('Ctrl Pts',(6.70384625876223,-0.940923067009009,
98.6527953309874));
#207630=CARTESIAN_POINT('Ctrl Pts',(6.72718554579768,-0.756217899524115,
98.6615452451649));
#207631=CARTESIAN_POINT('Ctrl Pts',(6.74287786815307,-0.570865181256975,
98.6702951593424));
#207632=CARTESIAN_POINT('Ctrl Pts',(6.75856988190831,-0.385516108076499,
98.6790449014469));
#207633=CARTESIAN_POINT('Ctrl Pts',(6.76661520773395,-0.199519795228973,
98.6877946435513));
#207634=CARTESIAN_POINT('Ctrl Pts',(6.76698651789578,-0.0135080204583415,
98.6965443856558));
#207635=CARTESIAN_POINT('Ctrl Pts',(6.7673578212491,0.172500343510199,98.7052939673208));
#207636=CARTESIAN_POINT('Ctrl Pts',(6.76005538995198,0.358523882208095,
98.7140435489857));
#207637=CARTESIAN_POINT('Ctrl Pts',(6.74510402742384,0.543930748561488,
98.7227931306507));
#207638=CARTESIAN_POINT('Ctrl Pts',(6.73015291918062,0.729334461612352,
98.7315425635074));
#207639=CARTESIAN_POINT('Ctrl Pts',(6.70755316306634,0.914121237631807,
98.7402919963641));
#207640=CARTESIAN_POINT('Ctrl Pts',(6.67738151874621,1.09766345165836,98.7490414292208));
#207641=CARTESIAN_POINT('Ctrl Pts',(6.64721034747624,1.2812027879938,98.7577907248983));
#207642=CARTESIAN_POINT('Ctrl Pts',(6.60946757205204,1.46349731860046,98.7665400205758));
#207643=CARTESIAN_POINT('Ctrl Pts',(6.56428138111593,1.64392790277881,98.7752893162533));
#207644=CARTESIAN_POINT('Ctrl Pts',(6.51909583859929,1.82435589778774,98.7840384863789));
#207645=CARTESIAN_POINT('Ctrl Pts',(6.46646716392963,2.00291972191981,98.7927876565045));
#207646=CARTESIAN_POINT('Ctrl Pts',(6.4065740987298,2.17901292274379,98.8015368266301));
#207647=CARTESIAN_POINT('Ctrl Pts',(6.34668181342182,2.35510383058693,98.8102858828292));
#207648=CARTESIAN_POINT('Ctrl Pts',(6.27952541914164,2.52872390822297,98.8190349390284));
#207649=CARTESIAN_POINT('Ctrl Pts',(6.20533299175639,2.69928350890004,98.8277839952275));
#207650=CARTESIAN_POINT('Ctrl Pts',(6.12831602991675,2.87633637965355,98.8368661313857));
#207651=CARTESIAN_POINT('Ctrl Pts',(6.04371690605399,3.05009086601207,98.8459482675438));
#207652=CARTESIAN_POINT('Ctrl Pts',(5.95184520316762,3.21991112882492,98.855030403702));
#207653=CARTESIAN_POINT('Ctrl Pts',(5.86333549509411,3.38351691182781,98.8637801840456));
#207654=CARTESIAN_POINT('Ctrl Pts',(5.76807618099509,3.54347103711775,98.8725299643892));
#207655=CARTESIAN_POINT('Ctrl Pts',(5.66639083309161,3.69923018027473,98.8812797447328));
#207656=CARTESIAN_POINT('Ctrl Pts',(5.56470914082355,3.85498372381826,98.8900292105177));
#207657=CARTESIAN_POINT('Ctrl Pts',(5.45660203372232,4.00654234701773,98.8987786763026));
#207658=CARTESIAN_POINT('Ctrl Pts',(5.34243669839392,4.15339127986444,98.9075281420875));
#207659=CARTESIAN_POINT('Ctrl Pts',(5.22827486050767,4.30023571401066,98.9162773398335));
#207660=CARTESIAN_POINT('Ctrl Pts',(5.10805534167286,4.44237052028269,98.9250265375795));
#207661=CARTESIAN_POINT('Ctrl Pts',(4.98218644340125,4.57931296628531,98.9337757353255));
#207662=CARTESIAN_POINT('Ctrl Pts',(4.85632073219772,4.71625194483169,98.9425247115372));
#207663=CARTESIAN_POINT('Ctrl Pts',(4.72480612170516,4.84799861524316,98.9512736877488));
#207664=CARTESIAN_POINT('Ctrl Pts',(4.5880892523552,4.97410554898292,98.9600226639604));
#207665=CARTESIAN_POINT('Ctrl Pts',(4.45136349474265,5.10022068121017,98.9687722089621));
#207666=CARTESIAN_POINT('Ctrl Pts',(4.30943501210306,5.22069514871648,98.9775217539638));
#207667=CARTESIAN_POINT('Ctrl Pts',(4.16278587432015,5.33511975166074,98.9862712989655));
#207668=CARTESIAN_POINT('Ctrl Pts',(4.01614535740691,5.44953762807663,98.9950203296193));
#207669=CARTESIAN_POINT('Ctrl Pts',(3.86478496658177,5.55790617532607,99.003769360273));
#207670=CARTESIAN_POINT('Ctrl Pts',(3.70921874747459,5.65985735539183,99.0125183909267));
#207671=CARTESIAN_POINT('Ctrl Pts',(3.55365041606173,5.76180991976878,99.0212675403763));
#207672=CARTESIAN_POINT('Ctrl Pts',(3.39387638174804,5.8573447855265,99.0300166898259));
#207673=CARTESIAN_POINT('Ctrl Pts',(3.23043927904829,5.94613749121074,99.0387658392756));
#207674=CARTESIAN_POINT('Ctrl Pts',(3.18691767070626,5.96978206944044,99.0410956471918));
#207675=CARTESIAN_POINT('Ctrl Pts',(3.14313645919731,5.99294880633374,99.043425455108));
#207676=CARTESIAN_POINT('Ctrl Pts',(3.09910619832142,6.01563211736936,99.0457552630242));
#207677=CARTESIAN_POINT('Ctrl Pts',(3.09910619832136,6.01563211736939,97.0457552630242));
#207678=CARTESIAN_POINT('Ctrl Pts',(2.93375330764826,6.10081787314653,97.0545047109265));
#207679=CARTESIAN_POINT('Ctrl Pts',(2.76488627843067,6.17918207037041,97.0632541588288));
#207680=CARTESIAN_POINT('Ctrl Pts',(2.59307866646696,6.25045854554,97.0720036067311));
#207681=CARTESIAN_POINT('Ctrl Pts',(2.42127244185374,6.32173444515038,97.0807529839814));
#207682=CARTESIAN_POINT('Ctrl Pts',(2.24652594672466,6.38592262741837,97.0895023612317));
#207683=CARTESIAN_POINT('Ctrl Pts',(2.06943269687126,6.4428050811056,97.098251738482));
#207684=CARTESIAN_POINT('Ctrl Pts',(1.89234081822068,6.49968709436169,97.1070010479874));
#207685=CARTESIAN_POINT('Ctrl Pts',(1.71290249405564,6.54926340459551,97.1157503574927));
#207686=CARTESIAN_POINT('Ctrl Pts',(1.53172716625019,6.59136563150393,97.1244996669981));
#207687=CARTESIAN_POINT('Ctrl Pts',(1.35055318107296,6.63346754640718,97.1332489116653));
#207688=CARTESIAN_POINT('Ctrl Pts',(1.16764249714383,6.66809542395782,97.1419981563326));
#207689=CARTESIAN_POINT('Ctrl Pts',(0.983616340614008,6.69513165624673,
97.1507474009998));
#207690=CARTESIAN_POINT('Ctrl Pts',(0.79959148671359,6.72216769715964,97.1594965837355));
#207691=CARTESIAN_POINT('Ctrl Pts',(0.614451459526558,6.74161215869372,
97.1682457664712));
#207692=CARTESIAN_POINT('Ctrl Pts',(0.428825047910227,6.75339900185713,
97.1769949492069));
#207693=CARTESIAN_POINT('Ctrl Pts',(0.243199888596869,6.76518576550222,
97.1857440729174));
#207694=CARTESIAN_POINT('Ctrl Pts',(0.0570886373916178,6.76931499599835,
97.1944931966279));
#207695=CARTESIAN_POINT('Ctrl Pts',(-0.12887662681157,6.76577266947846,
97.2032423203385));
#207696=CARTESIAN_POINT('Ctrl Pts',(-0.314840698188679,6.76223036567991,
97.21199138793));
#207697=CARTESIAN_POINT('Ctrl Pts',(-0.500658497951871,6.75101660879219,
97.2207404555216));
#207698=CARTESIAN_POINT('Ctrl Pts',(-0.685698951926932,6.73216948296211,
97.2294895231131));
#207699=CARTESIAN_POINT('Ctrl Pts',(-0.870738280460631,6.71332247176283,
97.2382385374917));
#207700=CARTESIAN_POINT('Ctrl Pts',(-1.05499998761335,6.68684221356173,
97.2469875518702));
#207701=CARTESIAN_POINT('Ctrl Pts',(-1.2378582916151,6.65281863948505,97.2557365662487));
#207702=CARTESIAN_POINT('Ctrl Pts',(-1.43007412915765,6.61705395369163,
97.2649332999471));
#207703=CARTESIAN_POINT('Ctrl Pts',(-1.62073882532453,6.57295372728561,
97.2741300336454));
#207704=CARTESIAN_POINT('Ctrl Pts',(-1.80913696086522,6.52068343479665,
97.2833267673438));
#207705=CARTESIAN_POINT('Ctrl Pts',(-1.98838356181161,6.4709521981672,97.2920767650575));
#207706=CARTESIAN_POINT('Ctrl Pts',(-2.16557827567628,6.41382586852547,
97.3008267627712));
#207707=CARTESIAN_POINT('Ctrl Pts',(-2.34011918616847,6.34949849945066,
97.3095767604848));
#207708=CARTESIAN_POINT('Ctrl Pts',(-2.51465655686291,6.28517243497474,
97.3183265807431));
#207709=CARTESIAN_POINT('Ctrl Pts',(-2.68653996290572,6.21364572244431,
97.3270764010015));
#207710=CARTESIAN_POINT('Ctrl Pts',(-2.85518555375289,6.13516132254408,
97.3358262212598));
#207711=CARTESIAN_POINT('Ctrl Pts',(-3.02382794854042,6.05667841002826,
97.3445758756973));
#207712=CARTESIAN_POINT('Ctrl Pts',(-3.18923239104692,5.97123819494532,
97.3533255301348));
#207713=CARTESIAN_POINT('Ctrl Pts',(-3.35083705963173,5.87913088813292,
97.3620751845723));
#207714=CARTESIAN_POINT('Ctrl Pts',(-3.51243888037944,5.78702520445808,
97.3708246848212));
#207715=CARTESIAN_POINT('Ctrl Pts',(-3.67024081219308,5.68825280608611,
97.3795741850702));
#207716=CARTESIAN_POINT('Ctrl Pts',(-3.82370687540098,5.58314917685451,
97.3883236853191));
#207717=CARTESIAN_POINT('Ctrl Pts',(-3.97717043813603,5.4780472601108,97.3970730430096));
#207718=CARTESIAN_POINT('Ctrl Pts',(-4.12629803718343,5.36661448087402,
97.4058224007));
#207719=CARTESIAN_POINT('Ctrl Pts',(-4.27058317202889,5.24922931207846,
97.4145717583905));
#207720=CARTESIAN_POINT('Ctrl Pts',(-4.41486614770903,5.13184589990173,
97.4233209851506));
#207721=CARTESIAN_POINT('Ctrl Pts',(-4.55430658190572,5.00851045726527,
97.4320702119107));
#207722=CARTESIAN_POINT('Ctrl Pts',(-4.68843088998099,4.87964187106718,
97.4408194386707));
#207723=CARTESIAN_POINT('Ctrl Pts',(-4.82255336914208,4.75077504211645,
97.4495685461267));
#207724=CARTESIAN_POINT('Ctrl Pts',(-4.95135966061626,4.61637541911857,
97.4583176535826));
#207725=CARTESIAN_POINT('Ctrl Pts',(-5.07441230865859,4.47689945405682,
97.4670667610386));
#207726=CARTESIAN_POINT('Ctrl Pts',(-5.1974634422312,4.33742520559466,97.4758157608149));
#207727=CARTESIAN_POINT('Ctrl Pts',(-5.31476088451563,4.19287495495397,
97.4845647605912));
#207728=CARTESIAN_POINT('Ctrl Pts',(-5.42590627625749,4.04373961590873,
97.4933137603676));
#207729=CARTESIAN_POINT('Ctrl Pts',(-5.5370638066968,3.89458798910982,97.5020637156623));
#207730=CARTESIAN_POINT('Ctrl Pts',(-5.64206777068997,3.74085050159608,
97.510813670957));
#207731=CARTESIAN_POINT('Ctrl Pts',(-5.74056148161265,3.58304938227556,
97.5195636262517));
#207732=CARTESIAN_POINT('Ctrl Pts',(-5.83905138949253,3.42525435597766,
97.5283132436928));
#207733=CARTESIAN_POINT('Ctrl Pts',(-5.93103139555138,3.26339625501752,
97.5370628611339));
#207734=CARTESIAN_POINT('Ctrl Pts',(-6.01618907818452,3.09802485069653,
97.545812478575));
#207735=CARTESIAN_POINT('Ctrl Pts',(-6.10134392542713,2.93265895254363,
97.5545618046908));
#207736=CARTESIAN_POINT('Ctrl Pts',(-6.17967677259689,2.76378023990826,
97.5633111308067));
#207737=CARTESIAN_POINT('Ctrl Pts',(-6.25092157007211,2.59196229231971,
97.5720604569226));
#207738=CARTESIAN_POINT('Ctrl Pts',(-6.32216437405876,2.42014915233994,
97.5808095382251));
#207739=CARTESIAN_POINT('Ctrl Pts',(-6.38631941547183,2.24539720667797,
97.5895586195275));
#207740=CARTESIAN_POINT('Ctrl Pts',(-6.44316881035938,2.06829994952669,
97.59830770083));
#207741=CARTESIAN_POINT('Ctrl Pts',(-6.50002334523104,1.89118668029491,
97.6070575731723));
#207742=CARTESIAN_POINT('Ctrl Pts',(-6.54957082409764,1.71172794812797,
97.6158074455146));
#207743=CARTESIAN_POINT('Ctrl Pts',(-6.59164294294889,1.53053334255483,
97.624557317857));
#207744=CARTESIAN_POINT('Ctrl Pts',(-6.63371214081082,1.34935131698771,
97.6333065827119));
#207745=CARTESIAN_POINT('Ctrl Pts',(-6.66830695238781,1.16643393834958,
97.6420558475668));
#207746=CARTESIAN_POINT('Ctrl Pts',(-6.69530988153224,0.982402458393107,
97.6508051124217));
#207747=CARTESIAN_POINT('Ctrl Pts',(-6.7223141968986,0.798361530999497,
97.6595548264287));
#207748=CARTESIAN_POINT('Ctrl Pts',(-6.74172580828798,0.613206671415178,
97.6683045404357));
#207749=CARTESIAN_POINT('Ctrl Pts',(-6.75347878027844,0.427566795166304,
97.6770542544428));
#207750=CARTESIAN_POINT('Ctrl Pts',(-6.76248992366325,0.285234494521487,
97.6837627642186));
#207751=CARTESIAN_POINT('Ctrl Pts',(-6.76699999998218,0.142617266672671,
97.6904712739945));
#207752=CARTESIAN_POINT('Ctrl Pts',(-6.767,8.45744902084614E-10,97.6971797837703));
#207753=CARTESIAN_POINT('',(-6.76699990772313,-0.00111753082879368,97.302820216166));
#207754=CARTESIAN_POINT('Ctrl Pts',(3.09910619832137,6.01563211736939,96.6512761190133));
#207755=CARTESIAN_POINT('Ctrl Pts',(2.92861376027321,6.10346564196215,96.6603199929407));
#207756=CARTESIAN_POINT('Ctrl Pts',(2.75445852336425,6.18400957271852,96.6693638668681));
#207757=CARTESIAN_POINT('Ctrl Pts',(2.57725861818762,6.25699824316562,96.6784077407955));
#207758=CARTESIAN_POINT('Ctrl Pts',(2.45885991308518,6.30576668951141,96.6844505372691));
#207759=CARTESIAN_POINT('Ctrl Pts',(2.33910235745289,6.3511631275774,96.6904933337427));
#207760=CARTESIAN_POINT('Ctrl Pts',(2.21817473501266,6.39312050918419,96.6965361302162));
#207761=CARTESIAN_POINT('Ctrl Pts',(2.04500430488565,6.45320419952089,96.7051895184445));
#207762=CARTESIAN_POINT('Ctrl Pts',(1.86928063661445,6.50628616672954,96.7138429066727));
#207763=CARTESIAN_POINT('Ctrl Pts',(1.69158385446612,6.55216247229184,96.722496294901));
#207764=CARTESIAN_POINT('Ctrl Pts',(1.51405118790107,6.59799640783171,96.7311416911114));
#207765=CARTESIAN_POINT('Ctrl Pts',(1.33454933544504,6.63663787941284,96.7397870873218));
#207766=CARTESIAN_POINT('Ctrl Pts',(1.15367393555411,6.66793262191687,96.7484324835322));
#207767=CARTESIAN_POINT('Ctrl Pts',(0.967021984688984,6.70022681307675,
96.7573539845746));
#207768=CARTESIAN_POINT('Ctrl Pts',(0.778907605749406,6.72469713327135,
96.766275485617));
#207769=CARTESIAN_POINT('Ctrl Pts',(0.589999590374173,6.74123056150421,
96.7751969866594));
#207770=CARTESIAN_POINT('Ctrl Pts',(0.407286603180601,6.75722179435357,
96.7838259170014));
#207771=CARTESIAN_POINT('Ctrl Pts',(0.223831539131578,6.76578839481647,
96.7924548473433));
#207772=CARTESIAN_POINT('Ctrl Pts',(0.0402478550319398,6.76688030854435,
96.8010837776853));
#207773=CARTESIAN_POINT('Ctrl Pts',(-0.152672653839921,6.76802775556864,
96.8101515640779));
#207774=CARTESIAN_POINT('Ctrl Pts',(-0.345734871493498,6.76092033890367,
96.8192193504706));
#207775=CARTESIAN_POINT('Ctrl Pts',(-0.538222660122076,6.74556190158619,
96.8282871368632));
#207776=CARTESIAN_POINT('Ctrl Pts',(-0.730710448750655,6.73020346426871,
96.8373549232558));
#207777=CARTESIAN_POINT('Ctrl Pts',(-0.922623416278408,6.7065940022652,
96.8464227096485));
#207778=CARTESIAN_POINT('Ctrl Pts',(-1.11324685210927,6.67480115406211,
96.8554904960411));
#207779=CARTESIAN_POINT('Ctrl Pts',(-1.29035667972246,6.64526215304662,
96.8639154521743));
#207780=CARTESIAN_POINT('Ctrl Pts',(-1.46627565472855,6.60867210523293,
96.8723404083075));
#207781=CARTESIAN_POINT('Ctrl Pts',(-1.64042712639814,6.56515710725777,
96.8807653644406));
#207782=CARTESIAN_POINT('Ctrl Pts',(-1.81461902029628,6.5216320090338,96.889192276087));
#207783=CARTESIAN_POINT('Ctrl Pts',(-1.98704227115564,6.47117883622198,
96.8976191877334));
#207784=CARTESIAN_POINT('Ctrl Pts',(-2.15713379708643,6.41397402407178,
96.9060460993798));
#207785=CARTESIAN_POINT('Ctrl Pts',(-2.32728787229691,6.35674817548384,
96.9144761099298));
#207786=CARTESIAN_POINT('Ctrl Pts',(-2.49510819871737,6.29276584266367,
96.9229061204799));
#207787=CARTESIAN_POINT('Ctrl Pts',(-2.66004976575128,6.22225234490908,
96.9313361310299));
#207788=CARTESIAN_POINT('Ctrl Pts',(-2.8251432735071,6.15167389159511,96.9397739071294));
#207789=CARTESIAN_POINT('Ctrl Pts',(-2.98735241858218,6.07455238360894,
96.9482116832288));
#207790=CARTESIAN_POINT('Ctrl Pts',(-3.14615395981322,5.99116051038124,
96.9566494593283));
#207791=CARTESIAN_POINT('Ctrl Pts',(-3.30503886014756,5.90772486256723,
96.9650916646382));
#207792=CARTESIAN_POINT('Ctrl Pts',(-3.46051229959971,5.81801244594944,
96.9735338699481));
#207793=CARTESIAN_POINT('Ctrl Pts',(-3.61207782597344,5.72234067310843,
96.9819760752581));
#207794=CARTESIAN_POINT('Ctrl Pts',(-3.76380324563791,5.62656797181121,
96.9904271866301));
#207795=CARTESIAN_POINT('Ctrl Pts',(-3.91161224098012,5.5248235392749,96.9988782980021));
#207796=CARTESIAN_POINT('Ctrl Pts',(-4.0550385142914,5.41746727240815,97.0073294093741));
#207797=CARTESIAN_POINT('Ctrl Pts',(-4.0952913200611,5.38733756981895,97.0097012268713));
#207798=CARTESIAN_POINT('Ctrl Pts',(-4.13519912412756,5.35676608945096,
97.0120730443685));
#207799=CARTESIAN_POINT('Ctrl Pts',(-4.17475210936568,5.32576133762552,
97.0144448618657));
#207800=CARTESIAN_POINT('Ctrl Pts',(-4.31130984734547,5.21871660382311,
97.0226336251251));
#207801=CARTESIAN_POINT('Ctrl Pts',(-4.44390991622575,5.10628919919418,
97.0308223883844));
#207802=CARTESIAN_POINT('Ctrl Pts',(-4.57210181061662,4.98880487024259,
97.0390111516438));
#207803=CARTESIAN_POINT('Ctrl Pts',(-4.70017891787413,4.87142574052688,
97.047192582422));
#207804=CARTESIAN_POINT('Ctrl Pts',(-4.82385544599577,4.74899894623214,
97.0553740132001));
#207805=CARTESIAN_POINT('Ctrl Pts',(-4.9427126636262,4.6218914445094,97.0635554439783));
#207806=CARTESIAN_POINT('Ctrl Pts',(-5.06148777639424,4.49487174682705,
97.0717312231413));
#207807=CARTESIAN_POINT('Ctrl Pts',(-5.17544996309289,4.36317804441761,
97.0799070023043));
#207808=CARTESIAN_POINT('Ctrl Pts',(-5.28421614999827,4.22721523938603,
97.0880827814673));
#207809=CARTESIAN_POINT('Ctrl Pts',(-5.39292945624847,4.09131853763907,
97.0962545856766));
#207810=CARTESIAN_POINT('Ctrl Pts',(-5.49645156964861,3.95115714951615,
97.104426389886));
#207811=CARTESIAN_POINT('Ctrl Pts',(-5.59443861436529,3.8071702864593,97.1125981940953));
#207812=CARTESIAN_POINT('Ctrl Pts',(-5.69241281932611,3.66320229075552,
97.1207689275103));
#207813=CARTESIAN_POINT('Ctrl Pts',(-5.78485319070877,3.51541011286518,
97.1289396609253));
#207814=CARTESIAN_POINT('Ctrl Pts',(-5.87145807933155,3.36426351861033,
97.1371103943403));
#207815=CARTESIAN_POINT('Ctrl Pts',(-5.95806023035527,3.21312170213164,
97.1452808694767));
#207816=CARTESIAN_POINT('Ctrl Pts',(-6.03882708539064,3.05862599373177,
97.1534513446129));
#207817=CARTESIAN_POINT('Ctrl Pts',(-6.11350210031256,2.90127231908244,
97.1616218197493));
#207818=CARTESIAN_POINT('Ctrl Pts',(-6.1881885961294,2.74389445212452,97.1697935510537));
#207819=CARTESIAN_POINT('Ctrl Pts',(-6.25678123120196,2.58365807037784,
97.1779652823581));
#207820=CARTESIAN_POINT('Ctrl Pts',(-6.31907090956425,2.4210807173448,97.1861370136625));
#207821=CARTESIAN_POINT('Ctrl Pts',(-6.38138171056235,2.25844823379402,
97.194311516028));
#207822=CARTESIAN_POINT('Ctrl Pts',(-6.4373851687022,2.0934735353858,97.2024860183935));
#207823=CARTESIAN_POINT('Ctrl Pts',(-6.48692151016709,1.92669102892277,
97.210660520759));
#207824=CARTESIAN_POINT('Ctrl Pts',(-6.53651203079824,1.75972610815784,
97.2188439637872));
#207825=CARTESIAN_POINT('Ctrl Pts',(-6.57962120273745,1.59094977665672,
97.2270274068155));
#207826=CARTESIAN_POINT('Ctrl Pts',(-6.61613978835074,1.42090932187888,
97.2352108498437));
#207827=CARTESIAN_POINT('Ctrl Pts',(-6.65267973177354,1.25076941933814,
97.2433990789395));
#207828=CARTESIAN_POINT('Ctrl Pts',(-6.68262134463256,1.07936427551682,
97.2515873080353));
#207829=CARTESIAN_POINT('Ctrl Pts',(-6.70590711640198,0.907247896767613,
97.259775537131));
#207830=CARTESIAN_POINT('Ctrl Pts',(-6.72922704277555,0.734879064853413,
97.2679757763816));
#207831=CARTESIAN_POINT('Ctrl Pts',(-6.74587158896306,0.561797273121107,
97.2761760156322));
#207832=CARTESIAN_POINT('Ctrl Pts',(-6.75583530513779,0.388559300305317,
97.2843762548827));
#207833=CARTESIAN_POINT('Ctrl Pts',(-6.76330542845771,0.258677136067334,
97.2905242419772));
#207834=CARTESIAN_POINT('Ctrl Pts',(-6.76702134752883,0.128707221600665,
97.2966722290716));
#207835=CARTESIAN_POINT('Ctrl Pts',(-6.76699990772313,-0.00111753082898668,
97.302820216166));
#207836=CARTESIAN_POINT('Ctrl Pts',(-6.76699990772305,-0.00111753133218596,
97.3028202161898));
#207837=CARTESIAN_POINT('Ctrl Pts',(-6.76696557723693,-0.208999305795223,
97.3126646752983));
#207838=CARTESIAN_POINT('Ctrl Pts',(-6.75735392725586,-0.416689416762483,
97.3225091344068));
#207839=CARTESIAN_POINT('Ctrl Pts',(-6.73820661880235,-0.623586852273372,
97.3323535935154));
#207840=CARTESIAN_POINT('Ctrl Pts',(-6.72251090318371,-0.79318788616753,
97.3404234395182));
#207841=CARTESIAN_POINT('Ctrl Pts',(-6.70037864351555,-0.962509125773961,
97.3484932855209));
#207842=CARTESIAN_POINT('Ctrl Pts',(-6.67181409574403,-1.13101090703462,
97.3565631315237));
#207843=CARTESIAN_POINT('Ctrl Pts',(-6.64328548580689,-1.29930069162182,
97.3646228246337));
#207844=CARTESIAN_POINT('Ctrl Pts',(-6.60834075144577,-1.46677270607685,
97.3726825177438));
#207845=CARTESIAN_POINT('Ctrl Pts',(-6.56703608254974,-1.6328888787942,
97.3807422108538));
#207846=CARTESIAN_POINT('Ctrl Pts',(-6.52577431511291,-1.79883251348143,
97.3887935326924));
#207847=CARTESIAN_POINT('Ctrl Pts',(-6.47816584801549,-1.9634227498881,
97.396844854531));
#207848=CARTESIAN_POINT('Ctrl Pts',(-6.42431843337466,-2.12612832787736,
97.4048961763696));
#207849=CARTESIAN_POINT('Ctrl Pts',(-6.37051514802313,-2.28870056461767,
97.4129408999507));
#207850=CARTESIAN_POINT('Ctrl Pts',(-6.31048320821169,-2.44939086464614,
97.4209856235317));
#207851=CARTESIAN_POINT('Ctrl Pts',(-6.24438102245941,-2.60767993556509,
97.4290303471128));
#207852=CARTESIAN_POINT('Ctrl Pts',(-6.17831853928764,-2.76587393421814,
97.4370702388372));
#207853=CARTESIAN_POINT('Ctrl Pts',(-6.10619321152113,-2.92166923139394,
97.4451101305615));
#207854=CARTESIAN_POINT('Ctrl Pts',(-6.02821267335559,-3.07456354053628,
97.4531500222859));
#207855=CARTESIAN_POINT('Ctrl Pts',(-5.9485530005616,-3.23075008303602,
97.4613630349059));
#207856=CARTESIAN_POINT('Ctrl Pts',(-5.8627832246035,-3.38390890941726,
97.4695760475258));
#207857=CARTESIAN_POINT('Ctrl Pts',(-5.7711759399275,-3.53352759581725,
97.4777890601458));
#207858=CARTESIAN_POINT('Ctrl Pts',(-5.68153092062217,-3.6799413889801,
97.4858261466883));
#207859=CARTESIAN_POINT('Ctrl Pts',(-5.58629615700854,-3.82296484362236,
97.4938632332309));
#207860=CARTESIAN_POINT('Ctrl Pts',(-5.48577255860638,-3.96214442382421,
97.5019003197735));
#207861=CARTESIAN_POINT('Ctrl Pts',(-5.38523933962797,-4.10133732415967,
97.5099381755026));
#207862=CARTESIAN_POINT('Ctrl Pts',(-5.27941649666478,-4.23668531458168,
97.5179760312318));
#207863=CARTESIAN_POINT('Ctrl Pts',(-5.16864690252021,-4.3677658129836,
97.5260138869609));
#207864=CARTESIAN_POINT('Ctrl Pts',(-5.05784476005486,-4.49888482782266,
97.5340541045179));
#207865=CARTESIAN_POINT('Ctrl Pts',(-4.94209321420227,-4.62573356948039,
97.5420943220748));
#207866=CARTESIAN_POINT('Ctrl Pts',(-4.82177374861879,-4.74792448519674,
97.5501345396318));
#207867=CARTESIAN_POINT('Ctrl Pts',(-4.69690853653508,-4.8747318519984,
97.5584785217595));
#207868=CARTESIAN_POINT('Ctrl Pts',(-4.56712381728006,-4.99652224993349,
97.5668225038873));
#207869=CARTESIAN_POINT('Ctrl Pts',(-4.43288489319439,-5.11290724771034,
97.575166486015));
#207870=CARTESIAN_POINT('Ctrl Pts',(-4.30330777794423,-5.22525046241532,
97.58322070085));
#207871=CARTESIAN_POINT('Ctrl Pts',(-4.16958096857007,-5.33255723884154,
97.5912749156851));
#207872=CARTESIAN_POINT('Ctrl Pts',(-4.03215331479852,-5.43452193352454,
97.5993291305202));
#207873=CARTESIAN_POINT('Ctrl Pts',(-3.89462281915308,-5.5365629319207,
97.6073893726032));
#207874=CARTESIAN_POINT('Ctrl Pts',(-3.75338627090088,-5.63325367911062,
97.6154496146862));
#207875=CARTESIAN_POINT('Ctrl Pts',(-3.60891848628086,-5.72433370440441,
97.6235098567692));
#207876=CARTESIAN_POINT('Ctrl Pts',(-3.46424872578826,-5.81554106582114,
97.6315813676236));
#207877=CARTESIAN_POINT('Ctrl Pts',(-3.31633903606825,-5.90112186952757,
97.6396528784779));
#207878=CARTESIAN_POINT('Ctrl Pts',(-3.16568612874992,-5.98086284195185,
97.6477243893322));
#207879=CARTESIAN_POINT('Ctrl Pts',(-3.14989613112094,-5.98922052842418,
97.6485703679431));
#207880=CARTESIAN_POINT('Ctrl Pts',(-3.13407601377241,-5.9975141077073,
97.6494163465539));
#207881=CARTESIAN_POINT('Ctrl Pts',(-3.11822635877598,-6.00574336576536,
97.6502623251648));
#207882=CARTESIAN_POINT('Ctrl Pts',(-2.96404897471086,-6.08579340347751,
97.6584915749007));
#207883=CARTESIAN_POINT('Ctrl Pts',(-2.80656053152289,-6.16002027173922,
97.6667208246367));
#207884=CARTESIAN_POINT('Ctrl Pts',(-2.64623981894299,-6.22813807013305,
97.6749500743726));
#207885=CARTESIAN_POINT('Ctrl Pts',(-2.48610991409193,-6.29617479726543,
97.6831695299627));
#207886=CARTESIAN_POINT('Ctrl Pts',(-2.32315477876337,-6.35811679331115,
97.6913889855527));
#207887=CARTESIAN_POINT('Ctrl Pts',(-2.15787869783316,-6.41372345252256,
97.6996084411428));
#207888=CARTESIAN_POINT('Ctrl Pts',(-1.99276613082334,-6.46927509794857,
97.7078197649124));
#207889=CARTESIAN_POINT('Ctrl Pts',(-1.82533752860868,-6.51850377510092,
97.7160310886821));
#207890=CARTESIAN_POINT('Ctrl Pts',(-1.65611818818594,-6.5612164685186,
97.7242424124517));
#207891=CARTESIAN_POINT('Ctrl Pts',(-1.4870322917781,-6.60389547930118,
97.7324472608858));
#207892=CARTESIAN_POINT('Ctrl Pts',(-1.31615881600288,-6.64006865346927,
97.7406521093199));
#207893=CARTESIAN_POINT('Ctrl Pts',(-1.1440393818071,-6.66959240830161,
97.748856957754));
#207894=CARTESIAN_POINT('Ctrl Pts',(-0.972021134188419,-6.69909880653672,
97.7570569826739));
#207895=CARTESIAN_POINT('Ctrl Pts',(-0.798758739862287,-6.72196351228072,
97.7652570075939));
#207896=CARTESIAN_POINT('Ctrl Pts',(-0.624805296458579,-6.73809374686323,
97.7734570325138));
#207897=CARTESIAN_POINT('Ctrl Pts',(-0.450902199122845,-6.75421931299037,
97.7816546841607));
#207898=CARTESIAN_POINT('Ctrl Pts',(-0.276308807395237,-6.76361425331227,
97.7898523358076));
#207899=CARTESIAN_POINT('Ctrl Pts',(-0.101584901233675,-6.76623747054752,
97.7980499874546));
#207900=CARTESIAN_POINT('Ctrl Pts',(0.0731156083249307,-6.7688603365179,
97.8062465413856));
#207901=CARTESIAN_POINT('Ctrl Pts',(0.247946238931239,-6.76471327913527,
97.8144430953167));
#207902=CARTESIAN_POINT('Ctrl Pts',(0.422345625779649,-6.75380730939111,
97.8226396492478));
#207903=CARTESIAN_POINT('Ctrl Pts',(0.596753369820246,-6.74290081703454,
97.8308365959565));
#207904=CARTESIAN_POINT('Ctrl Pts',(0.770729470853724,-6.72523478939104,
97.8390335426652));
#207905=CARTESIAN_POINT('Ctrl Pts',(0.943716050492217,-6.70087225785147,
97.8472304893739));
#207906=CARTESIAN_POINT('Ctrl Pts',(1.1167423730068,-6.67650412913161,97.8554293192936));
#207907=CARTESIAN_POINT('Ctrl Pts',(1.28877836616733,-6.64543648232545,
97.8636281492134));
#207908=CARTESIAN_POINT('Ctrl Pts',(1.45927467517108,-6.60778377539734,
97.8718269791331));
#207909=CARTESIAN_POINT('Ctrl Pts',(1.62993246597567,-6.57009540654226,
97.880033574393));
#207910=CARTESIAN_POINT('Ctrl Pts',(1.79904730835214,-6.52580959428659,
97.8882401696528));
#207911=CARTESIAN_POINT('Ctrl Pts',(1.96608246660753,-6.47509140742418,
97.8964467649126));
#207912=CARTESIAN_POINT('Ctrl Pts',(2.13319847083731,-6.42434867266851,
97.9046573322116));
#207913=CARTESIAN_POINT('Ctrl Pts',(2.29823244529167,-6.36716747349638,
97.9128678995105));
#207914=CARTESIAN_POINT('Ctrl Pts',(2.46066615762505,-6.30376165957429,
97.9210784668095));
#207915=CARTESIAN_POINT('Ctrl Pts',(2.62332388930164,-6.24026839995767,
97.9293003576562));
#207916=CARTESIAN_POINT('Ctrl Pts',(2.78337386297379,-6.17053351247428,
97.9375222485029));
#207917=CARTESIAN_POINT('Ctrl Pts',(2.94031992605678,-6.09481810495059,
97.9457441393496));
#207918=CARTESIAN_POINT('Ctrl Pts',(3.08302093684233,-6.02597493059229,
97.9532197785045));
#207919=CARTESIAN_POINT('Ctrl Pts',(3.22315604607831,-5.95218827169844,
97.9606954176594));
#207920=CARTESIAN_POINT('Ctrl Pts',(3.36037287420268,-5.87368565266501,
97.9681710568143));
#207921=CARTESIAN_POINT('Ctrl Pts',(3.52439387510971,-5.77984819611038,
97.9771070002651));
#207922=CARTESIAN_POINT('Ctrl Pts',(3.68458662949134,-5.67907685311374,
97.9860429437158));
#207923=CARTESIAN_POINT('Ctrl Pts',(3.8403817698925,-5.571692459341,97.9949788871666));
#207924=CARTESIAN_POINT('Ctrl Pts',(3.99594270887565,-5.46446949279397,
98.0039013975242));
#207925=CARTESIAN_POINT('Ctrl Pts',(4.14711901254683,-5.35065345771596,
98.0128239078818));
#207926=CARTESIAN_POINT('Ctrl Pts',(4.29336864012611,-5.23060940235281,
98.0217464182394));
#207927=CARTESIAN_POINT('Ctrl Pts',(4.4392599107323,-5.11085949217849,98.0306470656777));
#207928=CARTESIAN_POINT('Ctrl Pts',(4.58024839936626,-4.98491218265454,
98.039547713116));
#207929=CARTESIAN_POINT('Ctrl Pts',(4.71582408372049,-4.85317341658032,
98.0484483605543));
#207930=CARTESIAN_POINT('Ctrl Pts',(4.85119025258741,-4.72163823650974,
98.0573352531406));
#207931=CARTESIAN_POINT('Ctrl Pts',(4.98116011854419,-4.58432963179605,
98.0662221457268));
#207932=CARTESIAN_POINT('Ctrl Pts',(5.10525727675793,-4.44169304861448,
98.075109038313));
#207933=CARTESIAN_POINT('Ctrl Pts',(5.22903545895087,-4.29942309469646,
98.0839730882679));
#207934=CARTESIAN_POINT('Ctrl Pts',(5.34697088555874,-4.15185268373672,
98.0928371382229));
#207935=CARTESIAN_POINT('Ctrl Pts',(5.4586250288735,-3.99946268818148,98.1017011881778));
#207936=CARTESIAN_POINT('Ctrl Pts',(5.56537537183755,-3.85376559350265,
98.1101759329982));
#207937=CARTESIAN_POINT('Ctrl Pts',(5.66638412626853,-3.7036633459917,98.1186506778186));
#207938=CARTESIAN_POINT('Ctrl Pts',(5.76129989740328,-3.54960737155266,
98.1271254226391));
#207939=CARTESIAN_POINT('Ctrl Pts',(5.85323841115532,-3.40038372668082,
98.1353343370682));
#207940=CARTESIAN_POINT('Ctrl Pts',(5.93937073690846,-3.24759383477967,
98.1435432514973));
#207941=CARTESIAN_POINT('Ctrl Pts',(6.01942515262468,-3.09173249682915,
98.1517521659264));
#207942=CARTESIAN_POINT('Ctrl Pts',(6.09949860087152,-2.93583410363737,
98.1599630319832));
#207943=CARTESIAN_POINT('Ctrl Pts',(6.17349109755966,-2.77686312634199,
98.16817389804));
#207944=CARTESIAN_POINT('Ctrl Pts',(6.24117784354158,-2.61533709591818,
98.1763847640968));
#207945=CARTESIAN_POINT('Ctrl Pts',(6.30889274714978,-2.45374387080901,
98.1845990458666));
#207946=CARTESIAN_POINT('Ctrl Pts',(6.37029653660469,-2.2895938031936,98.1928133276365));
#207947=CARTESIAN_POINT('Ctrl Pts',(6.42521329102133,-2.1234225120976,98.2010276094063));
#207948=CARTESIAN_POINT('Ctrl Pts',(6.48019185858039,-1.95706418209532,
98.2092511369987));
#207949=CARTESIAN_POINT('Ctrl Pts',(6.52866869548075,-1.78868042282136,
98.2174746645911));
#207950=CARTESIAN_POINT('Ctrl Pts',(6.57051805780283,-1.61882100680926,
98.2256981921835));
#207951=CARTESIAN_POINT('Ctrl Pts',(6.61239424393825,-1.44885271751887,
98.2339269907372));
#207952=CARTESIAN_POINT('Ctrl Pts',(6.64763441596179,-1.27740723390562,
98.2421557892909));
#207953=CARTESIAN_POINT('Ctrl Pts',(6.67616432920691,-1.10504246498732,
98.2503845878446));
#207954=CARTESIAN_POINT('Ctrl Pts',(6.70473351159456,-0.932440449757783,
98.2586247126811));
#207955=CARTESIAN_POINT('Ctrl Pts',(6.72657394253494,-0.758916974114773,
98.2668648375175));
#207956=CARTESIAN_POINT('Ctrl Pts',(6.74166331253418,-0.585033999380091,
98.2751049623539));
#207957=CARTESIAN_POINT('Ctrl Pts',(6.74836237009857,-0.507837134482928,
98.2787632377239));
#207958=CARTESIAN_POINT('Ctrl Pts',(6.75373148684604,-0.430569403098271,
98.2824215130939));
#207959=CARTESIAN_POINT('Ctrl Pts',(6.7577719980426,-0.353279807619042,
98.2860797884639));
#207960=CARTESIAN_POINT('Ctrl Pts',(6.76710271459848,-0.174795632460588,
98.2945278112264));
#207961=CARTESIAN_POINT('Ctrl Pts',(6.76936610890676,0.00421340103325585,
98.3029758339889));
#207962=CARTESIAN_POINT('Ctrl Pts',(6.76452071377118,0.18316253154156,98.3114238567515));
#207963=CARTESIAN_POINT('Ctrl Pts',(6.75967975570863,0.361947792986718,
98.3198641434073));
#207964=CARTESIAN_POINT('Ctrl Pts',(6.74774299300604,0.540672928999616,
98.3283044300631));
#207965=CARTESIAN_POINT('Ctrl Pts',(6.72872095447458,0.718751220391842,
98.3367447167189));
#207966=CARTESIAN_POINT('Ctrl Pts',(6.70971340665599,0.896693854326269,
98.3451785736868));
#207967=CARTESIAN_POINT('Ctrl Pts',(6.6836313781627,1.07399029549173,98.3536124306547));
#207968=CARTESIAN_POINT('Ctrl Pts',(6.65053738512199,1.25005659435674,98.3620462876226));
#207969=CARTESIAN_POINT('Ctrl Pts',(6.61746351494715,1.42601583577142,98.3704750163676));
#207970=CARTESIAN_POINT('Ctrl Pts',(6.57738624223562,1.6007460992165,98.3789037451127));
#207971=CARTESIAN_POINT('Ctrl Pts',(6.53041962645837,1.77367091151864,98.3873324738577));
#207972=CARTESIAN_POINT('Ctrl Pts',(6.48347435649263,1.94651713139105,98.395757371838));
#207973=CARTESIAN_POINT('Ctrl Pts',(6.42964607422645,2.11755921500679,98.4041822698183));
#207974=CARTESIAN_POINT('Ctrl Pts',(6.36909950718439,2.28623281132599,98.4126071677985));
#207975=CARTESIAN_POINT('Ctrl Pts',(6.30856634525084,2.45486906303636,98.4210302004927));
#207976=CARTESIAN_POINT('Ctrl Pts',(6.24131797429288,2.62113755848007,98.4294532331868));
#207977=CARTESIAN_POINT('Ctrl Pts',(6.16756854401525,2.78449048388994,98.437876265881));
#207978=CARTESIAN_POINT('Ctrl Pts',(6.0938274584019,2.94782492610181,98.4462983455186));
#207979=CARTESIAN_POINT('Ctrl Pts',(6.01358691708799,3.10824415206556,98.4547204251562));
#207980=CARTESIAN_POINT('Ctrl Pts',(5.92710877035332,3.26522137448609,98.4631425047938));
#207981=CARTESIAN_POINT('Ctrl Pts',(5.84062833681939,3.4222027479599,98.471564807142));
#207982=CARTESIAN_POINT('Ctrl Pts',(5.74791013024976,3.57574164452383,98.4799871094903));
#207983=CARTESIAN_POINT('Ctrl Pts',(5.64926158926187,3.72533656145193,98.4884094118385));
#207984=CARTESIAN_POINT('Ctrl Pts',(5.5505966682449,3.87495631776503,98.4968331126622));
#207985=CARTESIAN_POINT('Ctrl Pts',(5.4459996336756,4.02063051079294,98.5052568134858));
#207986=CARTESIAN_POINT('Ctrl Pts',(5.33582101344589,4.1618869653643,98.5136805143095));
#207987=CARTESIAN_POINT('Ctrl Pts',(5.22556783433685,4.30323900946955,98.5221099155284));
#207988=CARTESIAN_POINT('Ctrl Pts',(5.10972572729284,4.44016707811551,98.5305393167474));
#207989=CARTESIAN_POINT('Ctrl Pts',(4.98868588754732,4.57223163404768,98.5389687179664));
#207990=CARTESIAN_POINT('Ctrl Pts',(4.86760286095511,4.70434331042994,98.547401126784));
#207991=CARTESIAN_POINT('Ctrl Pts',(4.7413186336268,4.83158777234661,98.5558335356016));
#207992=CARTESIAN_POINT('Ctrl Pts',(4.6102613606425,4.95356227240223,98.5642659444193));
#207993=CARTESIAN_POINT('Ctrl Pts',(4.47908282965597,5.07564962681431,98.5727061551469));
#207994=CARTESIAN_POINT('Ctrl Pts',(4.34312267796113,5.19245705453213,98.5811463658745));
#207995=CARTESIAN_POINT('Ctrl Pts',(4.20284307838113,5.3036213155262,98.5895865766021));
#207996=CARTESIAN_POINT('Ctrl Pts',(4.12305443588864,5.36684965025879,98.5943872244392));
#207997=CARTESIAN_POINT('Ctrl Pts',(4.04186896918814,5.42825310035317,98.5991878722763));
#207998=CARTESIAN_POINT('Ctrl Pts',(3.95937594541419,5.48777105233769,98.6039885201133));
#207999=CARTESIAN_POINT('Ctrl Pts',(3.81951609252751,5.5886786397657,98.612127607148));
#208000=CARTESIAN_POINT('Ctrl Pts',(3.67561726787852,5.68436515395346,98.6202666941827));
#208001=CARTESIAN_POINT('Ctrl Pts',(3.52811070582312,5.77448905509884,98.6284057812174));
#208002=CARTESIAN_POINT('Ctrl Pts',(3.38822187768102,5.85995865552304,98.636124538482));
#208003=CARTESIAN_POINT('Ctrl Pts',(3.24508879753987,5.94042546090201,98.6438432957465));
#208004=CARTESIAN_POINT('Ctrl Pts',(3.09910619832135,6.0156321173694,98.651562053011));
#208005=CARTESIAN_POINT('Origin',(0.,0.,4.30282021618968));
#208006=CARTESIAN_POINT('',(3.09910619832146,6.01563211736934,101.0456200824));
#208007=CARTESIAN_POINT('',(3.09910619832147,6.01563211736933,100.651473518761));
#208008=CARTESIAN_POINT('',(3.09910619832133,6.0156321173694,4.30282021618968));
#208009=CARTESIAN_POINT('',(-6.767,4.25434840622355E-12,99.6971797838099));
#208010=CARTESIAN_POINT('Ctrl Pts',(-6.76699999999964,2.20710901944525E-6,
99.6972269161604));
#208011=CARTESIAN_POINT('Ctrl Pts',(-6.76700005739661,-0.175976986951552,
99.7054676366832));
#208012=CARTESIAN_POINT('Ctrl Pts',(-6.76013113518234,-0.351928063196356,
99.7137083572059));
#208013=CARTESIAN_POINT('Ctrl Pts',(-6.74642581124832,-0.52728338995501,
99.7219490777287));
#208014=CARTESIAN_POINT('Ctrl Pts',(-6.73271589701395,-0.70269744816884,
99.7301925583017));
#208015=CARTESIAN_POINT('Ctrl Pts',(-6.71216504593372,-0.877515008085112,
99.7384360388747));
#208016=CARTESIAN_POINT('Ctrl Pts',(-6.6848576569018,-1.05117415634203,
99.7466795194477));
#208017=CARTESIAN_POINT('Ctrl Pts',(-6.65753639969662,-1.22492149813339,
99.7549271865072));
#208018=CARTESIAN_POINT('Ctrl Pts',(-6.62345182177918,-1.3975089083452,
99.7631748535667));
#208019=CARTESIAN_POINT('Ctrl Pts',(-6.58273933361654,-1.56838511394929,
99.7714225206262));
#208020=CARTESIAN_POINT('Ctrl Pts',(-6.54197807578351,-1.73946601291898,
99.7796800676028));
#208021=CARTESIAN_POINT('Ctrl Pts',(-6.49457313230035,-1.90883127057889,
99.7879376145793));
#208022=CARTESIAN_POINT('Ctrl Pts',(-6.4407099366649,-2.07594424581827,
99.7961951615558));
#208023=CARTESIAN_POINT('Ctrl Pts',(-6.38680837714483,-2.24317624672676,
99.8044585899431));
#208024=CARTESIAN_POINT('Ctrl Pts',(-6.32643951565873,-2.40815243731166,
99.8127220183304));
#208025=CARTESIAN_POINT('Ctrl Pts',(-6.25983675034266,-2.57035656263085,
99.8209854467177));
#208026=CARTESIAN_POINT('Ctrl Pts',(-6.19314394731612,-2.73277996545306,
99.8292600461153));
#208027=CARTESIAN_POINT('Ctrl Pts',(-6.12020055689815,-2.89242350031711,
99.8375346455128));
#208028=CARTESIAN_POINT('Ctrl Pts',(-6.04128608876983,-3.04879507242388,
99.8458092449103));
#208029=CARTESIAN_POINT('Ctrl Pts',(-6.02493670803759,-3.08119189937728,
99.8475235639593));
#208030=CARTESIAN_POINT('Ctrl Pts',(-6.00833117996067,-3.11344838274264,
99.8492378830084));
#208031=CARTESIAN_POINT('Ctrl Pts',(-5.99147222024645,-3.14556030525805,
99.8509522020574));
#208032=CARTESIAN_POINT('Ctrl Pts',(-5.90839265842365,-3.30380520868575,
99.85940022482));
#208033=CARTESIAN_POINT('Ctrl Pts',(-5.81896785728657,-3.45889409277439,
99.8678482475825));
#208034=CARTESIAN_POINT('Ctrl Pts',(-5.72346063661553,-3.6103029431216,
99.8762962703451));
#208035=CARTESIAN_POINT('Ctrl Pts',(-5.62804087475901,-3.76157314386239,
99.8847365570008));
#208036=CARTESIAN_POINT('Ctrl Pts',(-5.52654997281395,-3.90916974737669,
99.8931768436566));
#208037=CARTESIAN_POINT('Ctrl Pts',(-5.41929646235672,-4.0525935958455,
99.9016171303124));
#208038=CARTESIAN_POINT('Ctrl Pts',(-5.31212465606703,-4.19590818610826,
99.9100509872803));
#208039=CARTESIAN_POINT('Ctrl Pts',(-5.19919919151935,-4.33505609201034,
99.9184848442482));
#208040=CARTESIAN_POINT('Ctrl Pts',(-5.08087189155359,-4.46956707317618,
99.9269187012161));
#208041=CARTESIAN_POINT('Ctrl Pts',(-4.9626165407296,-4.60399626468184,
99.9353474299611));
#208042=CARTESIAN_POINT('Ctrl Pts',(-4.83896612283186,-4.73379390296965,
99.9437761587062));
#208043=CARTESIAN_POINT('Ctrl Pts',(-4.71031296775279,-4.85852248588189,
99.9522048874512));
#208044=CARTESIAN_POINT('Ctrl Pts',(-4.58171828412037,-4.98319438102243,
99.9606297854315));
#208045=CARTESIAN_POINT('Ctrl Pts',(-4.44812563610895,-5.10280158288232,
99.9690546834118));
#208046=CARTESIAN_POINT('Ctrl Pts',(-4.30996473665161,-5.21694287574817,
99.9774795813921));
#208047=CARTESIAN_POINT('Ctrl Pts',(-4.17183442624283,-5.33105889754556,
99.9859026140863));
#208048=CARTESIAN_POINT('Ctrl Pts',(-4.02913813615296,-5.43971120892498,
99.9943256467804));
#208049=CARTESIAN_POINT('Ctrl Pts',(-3.88233963739472,-5.54253804135919,
100.002748679475));
#208050=CARTESIAN_POINT('Ctrl Pts',(-3.7355577487197,-5.64535323905425,
100.011170759112));
#208051=CARTESIAN_POINT('Ctrl Pts',(-3.58467484977971,-5.74234408056313,
100.01959283875));
#208052=CARTESIAN_POINT('Ctrl Pts',(-3.43018499781208,-5.83319122614585,
100.028014918387));
#208053=CARTESIAN_POINT('Ctrl Pts',(-3.27569106056693,-5.92404077405985,
100.036437220736));
#208054=CARTESIAN_POINT('Ctrl Pts',(-3.11759026777796,-6.00874613343463,
100.044859523084));
#208055=CARTESIAN_POINT('Ctrl Pts',(-2.95640297310033,-6.08703297679942,
100.053281825432));
#208056=CARTESIAN_POINT('Ctrl Pts',(-2.79518891418851,-6.1653328192496,
100.061705526256));
#208057=CARTESIAN_POINT('Ctrl Pts',(-2.63088763181189,-6.23721187575772,
100.070129227079));
#208058=CARTESIAN_POINT('Ctrl Pts',(-2.46404156339597,-6.30244303217864,
100.078552927903));
#208059=CARTESIAN_POINT('Ctrl Pts',(-2.29708258872094,-6.3677183311192,
100.086982329122));
#208060=CARTESIAN_POINT('Ctrl Pts',(-2.1275756977702,-6.42633661894526,
100.095411730341));
#208061=CARTESIAN_POINT('Ctrl Pts',(-1.95608163936907,-6.47811960526534,
100.10384113156));
#208062=CARTESIAN_POINT('Ctrl Pts',(-1.78452639212626,-6.52992106768298,
100.112273540378));
#208063=CARTESIAN_POINT('Ctrl Pts',(-1.61098288467417,-6.57488227520103,
100.120705949195));
#208064=CARTESIAN_POINT('Ctrl Pts',(-1.43602486982045,-6.61287543911551,
100.129138358013));
#208065=CARTESIAN_POINT('Ctrl Pts',(-1.26090497872051,-6.65090375541076,
100.13757856874));
#208066=CARTESIAN_POINT('Ctrl Pts',(-1.08436829267871,-6.68195108219252,
100.146018779468));
#208067=CARTESIAN_POINT('Ctrl Pts',(-0.906997651418675,-6.70594096755415,
100.154458990196));
#208068=CARTESIAN_POINT('Ctrl Pts',(-0.806112257341587,-6.71958600498187,
100.159259638033));
#208069=CARTESIAN_POINT('Ctrl Pts',(-0.704957176500564,-6.73094880866589,
100.16406028587));
#208070=CARTESIAN_POINT('Ctrl Pts',(-0.603640110343725,-6.74002282022726,
100.168860933707));
#208071=CARTESIAN_POINT('Ctrl Pts',(-0.431852452833622,-6.75540821628614,
100.17700064874));
#208072=CARTESIAN_POINT('Ctrl Pts',(-0.25925645436591,-6.76424128893959,
100.185140363773));
#208073=CARTESIAN_POINT('Ctrl Pts',(-0.086397400190767,-6.76644843985678,
100.193280078806));
#208074=CARTESIAN_POINT('Ctrl Pts',(0.0863104724931837,-6.76865366041303,
100.201412674893));
#208075=CARTESIAN_POINT('Ctrl Pts',(0.259280579266327,-6.76424448948375,
100.20954527098));
#208076=CARTESIAN_POINT('Ctrl Pts',(0.431962167790192,-6.75319907048489,
100.217677867067));
#208077=CARTESIAN_POINT('Ctrl Pts',(0.604525701916003,-6.74216120272703,
100.225804903275));
#208078=CARTESIAN_POINT('Ctrl Pts',(0.776800746537316,-6.7244961429065,
100.233931939483));
#208079=CARTESIAN_POINT('Ctrl Pts',(0.948236242228564,-6.70023410254629,
100.242058975691));
#208080=CARTESIAN_POINT('Ctrl Pts',(1.11958978865013,-6.67598365988048,
100.250182127028));
#208081=CARTESIAN_POINT('Ctrl Pts',(1.29010422347559,-6.645142567487,100.258305278366));
#208082=CARTESIAN_POINT('Ctrl Pts',(1.45923332371553,-6.60779290739034,
100.266428429704));
#208083=CARTESIAN_POINT('Ctrl Pts',(1.6283148974206,-6.57045374282592,100.274549298375));
#208084=CARTESIAN_POINT('Ctrl Pts',(1.79601155481641,-6.52660973315067,
100.282670167047));
#208085=CARTESIAN_POINT('Ctrl Pts',(1.96178702105474,-6.47639411123359,
100.290791035719));
#208086=CARTESIAN_POINT('Ctrl Pts',(2.12757144643456,-6.42617577547188,
100.298912343273));
#208087=CARTESIAN_POINT('Ctrl Pts',(2.29143412157694,-6.36958524189536,
100.307033650828));
#208088=CARTESIAN_POINT('Ctrl Pts',(2.45285351711438,-6.30680573853196,
100.315154958382));
#208089=CARTESIAN_POINT('Ctrl Pts',(2.53673264626406,-6.27418332625592,
100.319375072099));
#208090=CARTESIAN_POINT('Ctrl Pts',(2.61995231673305,-6.23989057850436,
100.323595185816));
#208091=CARTESIAN_POINT('Ctrl Pts',(2.70244140676876,-6.20395836889495,
100.327815299532));
#208092=CARTESIAN_POINT('Ctrl Pts',(2.8780570911426,-6.12746025770365,100.336799738058));
#208093=CARTESIAN_POINT('Ctrl Pts',(3.05027322548326,-6.04356666527602,
100.345784176584));
#208094=CARTESIAN_POINT('Ctrl Pts',(3.21850490740853,-5.95260574546872,
100.354768615109));
#208095=CARTESIAN_POINT('Ctrl Pts',(3.38702694717759,-5.86148783254192,
100.36376856024));
#208096=CARTESIAN_POINT('Ctrl Pts',(3.55155057917703,-5.76327832582239,
100.372768505371));
#208097=CARTESIAN_POINT('Ctrl Pts',(3.71151804072702,-5.65834983306598,
100.381768450501));
#208098=CARTESIAN_POINT('Ctrl Pts',(3.8718624697043,-5.55317407362434,100.390789604233));
#208099=CARTESIAN_POINT('Ctrl Pts',(4.02762904515278,-5.44124777955361,
100.399810757965));
#208100=CARTESIAN_POINT('Ctrl Pts',(4.1782891585767,-5.32298682201266,100.408831911698));
#208101=CARTESIAN_POINT('Ctrl Pts',(4.32910256985377,-5.20460553301509,
100.417862244525));
#208102=CARTESIAN_POINT('Ctrl Pts',(4.47479895494853,-5.07987685601615,
100.426892577352));
#208103=CARTESIAN_POINT('Ctrl Pts',(4.61488385498987,-4.94925610621979,
100.435922910179));
#208104=CARTESIAN_POINT('Ctrl Pts',(4.75516735126224,-4.81845017737417,
100.444966045172));
#208105=CARTESIAN_POINT('Ctrl Pts',(4.88982328077036,-4.68173563655124,
100.454009180164));
#208106=CARTESIAN_POINT('Ctrl Pts',(5.0183933863659,-4.53960535946452,100.463052315157));
#208107=CARTESIAN_POINT('Ctrl Pts',(5.13079327947637,-4.41535075238996,
100.470958098557));
#208108=CARTESIAN_POINT('Ctrl Pts',(5.23854242541837,-4.28695762868836,
100.478863881957));
#208109=CARTESIAN_POINT('Ctrl Pts',(5.34135995672388,-4.15477590402981,
100.486769665357));
#208110=CARTESIAN_POINT('Ctrl Pts',(5.45390035532087,-4.01009450785711,
100.495423053585));
#208111=CARTESIAN_POINT('Ctrl Pts',(5.56063072693521,-3.86074548506657,
100.504076441813));
#208112=CARTESIAN_POINT('Ctrl Pts',(5.66117154296611,-3.70721266737029,
100.512729830042));
#208113=CARTESIAN_POINT('Ctrl Pts',(5.76161950242172,-3.55382164812173,
100.521375226252));
#208114=CARTESIAN_POINT('Ctrl Pts',(5.8558891419884,-3.39625479431927,100.530020622462));
#208115=CARTESIAN_POINT('Ctrl Pts',(5.9436429873451,-3.23502659015091,100.538666018673));
#208116=CARTESIAN_POINT('Ctrl Pts',(6.03419939491393,-3.06864930025651,
100.547587519715));
#208117=CARTESIAN_POINT('Ctrl Pts',(6.11781672766863,-2.89837317803971,
100.556509020757));
#208118=CARTESIAN_POINT('Ctrl Pts',(6.19417306280503,-2.72479523414524,
100.5654305218));
#208119=CARTESIAN_POINT('Ctrl Pts',(6.26802537688636,-2.55690958579417,
100.574059452142));
#208120=CARTESIAN_POINT('Ctrl Pts',(6.33508522134007,-2.38593553972064,
100.582688382484));
#208121=CARTESIAN_POINT('Ctrl Pts',(6.39510808107167,-2.21243793843169,
100.591317312826));
#208122=CARTESIAN_POINT('Ctrl Pts',(6.45818362452259,-2.03011647728058,
100.600385099218));
#208123=CARTESIAN_POINT('Ctrl Pts',(6.51348758383214,-1.84500838091116,
100.609452885611));
#208124=CARTESIAN_POINT('Ctrl Pts',(6.56079348986117,-1.65779304600884,
100.618520672003));
#208125=CARTESIAN_POINT('Ctrl Pts',(6.60809939589018,-1.47057771110666,
100.627588458396));
#208126=CARTESIAN_POINT('Ctrl Pts',(6.6474071188378,-1.28125550766004,100.636656244789));
#208127=CARTESIAN_POINT('Ctrl Pts',(6.67855106060494,-1.09052497949047,
100.645724031181));
#208128=CARTESIAN_POINT('Ctrl Pts',(6.70748715722669,-0.913315651490259,
100.654148987314));
#208129=CARTESIAN_POINT('Ctrl Pts',(6.7293634728444,-0.734968394205431,
100.662573943447));
#208130=CARTESIAN_POINT('Ctrl Pts',(6.74411412874157,-0.556069796435935,
100.670998899581));
#208131=CARTESIAN_POINT('Ctrl Pts',(6.75886820840767,-0.377129674583572,
100.679425811227));
#208132=CARTESIAN_POINT('Ctrl Pts',(6.76649330340398,-0.197638287575471,
100.687852722873));
#208133=CARTESIAN_POINT('Ctrl Pts',(6.76697556414859,-0.0181855496434833,
100.69627963452));
#208134=CARTESIAN_POINT('Ctrl Pts',(6.76745800223927,0.161333180051648,
100.70470964507));
#208135=CARTESIAN_POINT('Ctrl Pts',(6.76079236779913,0.340812900886664,
100.71313965562));
#208136=CARTESIAN_POINT('Ctrl Pts',(6.7470169096723,0.519665104270093,100.72156966617));
#208137=CARTESIAN_POINT('Ctrl Pts',(6.73322876188165,0.698682062561421,
100.73000744227));
#208138=CARTESIAN_POINT('Ctrl Pts',(6.71231773072315,0.87707001763686,100.738445218369));
#208139=CARTESIAN_POINT('Ctrl Pts',(6.68437391811377,1.05424585502643,100.746882994469));
#208140=CARTESIAN_POINT('Ctrl Pts',(6.65641543706287,1.23151469666869,100.755325199778));
#208141=CARTESIAN_POINT('Ctrl Pts',(6.62141687123447,1.40756982570475,100.763767405088));
#208142=CARTESIAN_POINT('Ctrl Pts',(6.57951928187132,1.58183912566465,100.772209610398));
#208143=CARTESIAN_POINT('Ctrl Pts',(6.53757749285652,1.75629227014807,100.78066072177));
#208144=CARTESIAN_POINT('Ctrl Pts',(6.48872222670304,1.92895550197544,100.789111833142));
#208145=CARTESIAN_POINT('Ctrl Pts',(6.4331444652841,2.09927160910269,100.797562944514));
#208146=CARTESIAN_POINT('Ctrl Pts',(6.41754648045252,2.14707108838575,100.799934762011));
#208147=CARTESIAN_POINT('Ctrl Pts',(6.40141928934946,2.19468581241639,100.802306579509));
#208148=CARTESIAN_POINT('Ctrl Pts',(6.38476779279114,2.2421037514212,100.804678397006));
#208149=CARTESIAN_POINT('Ctrl Pts',(6.32637599193586,2.40838423207581,100.812995649121));
#208150=CARTESIAN_POINT('Ctrl Pts',(6.26142774917761,2.57254343537232,100.821312901235));
#208151=CARTESIAN_POINT('Ctrl Pts',(6.19009908614766,2.73403772901435,100.82963015335));
#208152=CARTESIAN_POINT('Ctrl Pts',(6.11883292640286,2.89539050978544,100.837940117293));
#208153=CARTESIAN_POINT('Ctrl Pts',(6.04119762702078,3.054082717188,100.846250081235));
#208154=CARTESIAN_POINT('Ctrl Pts',(5.95741817684249,3.20958839514145,100.854560045178));
#208155=CARTESIAN_POINT('Ctrl Pts',(5.87370418750134,3.36497256917197,100.862863516153));
#208156=CARTESIAN_POINT('Ctrl Pts',(5.78385578310677,3.51717487231519,100.871166987129));
#208157=CARTESIAN_POINT('Ctrl Pts',(5.68814498861566,3.66569169304875,100.879470458105));
#208158=CARTESIAN_POINT('Ctrl Pts',(5.59247644153815,3.81414295741967,100.88777026387));
#208159=CARTESIAN_POINT('Ctrl Pts',(5.49095084781472,3.95891168854038,100.896070069636));
#208160=CARTESIAN_POINT('Ctrl Pts',(5.3838851113239,4.09952071687226,100.904369875401));
#208161=CARTESIAN_POINT('Ctrl Pts',(5.27684883973796,4.24009104905559,100.912667397028));
#208162=CARTESIAN_POINT('Ctrl Pts',(5.16427567419766,4.376503683142,100.920964918655));
#208163=CARTESIAN_POINT('Ctrl Pts',(5.04652471368958,4.5083120249291,100.929262440282));
#208164=CARTESIAN_POINT('Ctrl Pts',(4.92878659129806,4.64010599595567,100.937559057249));
#208165=CARTESIAN_POINT('Ctrl Pts',(4.80587203134584,4.76729641639244,100.945855674216));
#208166=CARTESIAN_POINT('Ctrl Pts',(4.6781792560858,4.88947112149448,100.954152291183));
#208167=CARTESIAN_POINT('Ctrl Pts',(4.55044301688451,5.01168741230249,100.962451732145));
#208168=CARTESIAN_POINT('Ctrl Pts',(4.41792556204721,5.12888433361145,100.970751173106));
#208169=CARTESIAN_POINT('Ctrl Pts',(4.28106118001807,5.24068737599776,100.979050614068));
#208170=CARTESIAN_POINT('Ctrl Pts',(4.14417377997452,5.35250922155261,100.987351450839));
#208171=CARTESIAN_POINT('Ctrl Pts',(4.00293826883781,5.4589351645489,100.99565228761));
#208172=CARTESIAN_POINT('Ctrl Pts',(3.85782082818095,5.5596319534348,101.003953124382));
#208173=CARTESIAN_POINT('Ctrl Pts',(3.71259759803485,5.66040214949917,101.012260012399));
#208174=CARTESIAN_POINT('Ctrl Pts',(3.56348707363411,5.75543465319206,101.020566900416));
#208175=CARTESIAN_POINT('Ctrl Pts',(3.41098385638364,5.84443993308941,101.028873788433));
#208176=CARTESIAN_POINT('Ctrl Pts',(3.30850409493752,5.90425008015238,101.034455886422));
#208177=CARTESIAN_POINT('Ctrl Pts',(3.20449288244415,5.96133948118201,101.040037984411));
#208178=CARTESIAN_POINT('Ctrl Pts',(3.09910619832146,6.01563211736934,101.0456200824));
#208179=CARTESIAN_POINT('Ctrl Pts',(3.09910619832142,6.01563211736936,99.0457552630242));
#208180=CARTESIAN_POINT('Ctrl Pts',(2.93375330764834,6.10081787314649,99.0545047109265));
#208181=CARTESIAN_POINT('Ctrl Pts',(2.76488627843078,6.17918207037036,99.0632541588288));
#208182=CARTESIAN_POINT('Ctrl Pts',(2.59307866646709,6.25045854553994,99.0720036067311));
#208183=CARTESIAN_POINT('Ctrl Pts',(2.42127244185378,6.32173444515037,99.0807529839814));
#208184=CARTESIAN_POINT('Ctrl Pts',(2.24652594672461,6.3859226274184,99.0895023612317));
#208185=CARTESIAN_POINT('Ctrl Pts',(2.06943269687111,6.44280508110565,99.098251738482));
#208186=CARTESIAN_POINT('Ctrl Pts',(1.89234081822067,6.49968709436169,99.1070010479874));
#208187=CARTESIAN_POINT('Ctrl Pts',(1.71290249405579,6.54926340459547,99.1157503574927));
#208188=CARTESIAN_POINT('Ctrl Pts',(1.53172716625049,6.59136563150386,99.1244996669981));
#208189=CARTESIAN_POINT('Ctrl Pts',(1.35055318107329,6.63346754640711,99.1332489116653));
#208190=CARTESIAN_POINT('Ctrl Pts',(1.16764249714419,6.66809542395776,99.1419981563325));
#208191=CARTESIAN_POINT('Ctrl Pts',(0.983616340614392,6.69513165624668,
99.1507474009998));
#208192=CARTESIAN_POINT('Ctrl Pts',(0.799591486713875,6.7221676971596,99.1594965837355));
#208193=CARTESIAN_POINT('Ctrl Pts',(0.614451459526745,6.74161215869371,
99.1682457664712));
#208194=CARTESIAN_POINT('Ctrl Pts',(0.428825047910313,6.75339900185712,
99.1769949492069));
#208195=CARTESIAN_POINT('Ctrl Pts',(0.243199888597109,6.7651857655022,99.1857440729174));
#208196=CARTESIAN_POINT('Ctrl Pts',(0.0570886373920129,6.76931499599834,
99.1944931966279));
#208197=CARTESIAN_POINT('Ctrl Pts',(-0.12887662681102,6.76577266947847,
99.2032423203385));
#208198=CARTESIAN_POINT('Ctrl Pts',(-0.314840698187974,6.76223036567994,
99.21199138793));
#208199=CARTESIAN_POINT('Ctrl Pts',(-0.500658497951012,6.75101660879225,
99.2207404555215));
#208200=CARTESIAN_POINT('Ctrl Pts',(-0.685698951925922,6.73216948296221,
99.2294895231131));
#208201=CARTESIAN_POINT('Ctrl Pts',(-0.870738280459596,6.71332247176297,
99.2382385374916));
#208202=CARTESIAN_POINT('Ctrl Pts',(-1.05499998761229,6.6868422135619,99.2469875518701));
#208203=CARTESIAN_POINT('Ctrl Pts',(-1.23785829161402,6.65281863948525,
99.2557365662487));
#208204=CARTESIAN_POINT('Ctrl Pts',(-1.43007412917382,6.61705395368866,
99.2649332999479));
#208205=CARTESIAN_POINT('Ctrl Pts',(-1.62073882535767,6.57295372727796,
99.274130033647));
#208206=CARTESIAN_POINT('Ctrl Pts',(-1.80913696091486,6.52068343478287,
99.2833267673462));
#208207=CARTESIAN_POINT('Ctrl Pts',(-1.98838356186085,6.47095219815207,
99.2920767650599));
#208208=CARTESIAN_POINT('Ctrl Pts',(-2.16557827572506,6.413825868509,99.3008267627736));
#208209=CARTESIAN_POINT('Ctrl Pts',(-2.34011918621674,6.34949849943288,
99.3095767604873));
#208210=CARTESIAN_POINT('Ctrl Pts',(-2.51465655691078,6.28517243495559,
99.3183265807456));
#208211=CARTESIAN_POINT('Ctrl Pts',(-2.68653996295314,6.21364572242381,
99.3270764010039));
#208212=CARTESIAN_POINT('Ctrl Pts',(-2.8551855537998,6.13516132252225,99.3358262212622));
#208213=CARTESIAN_POINT('Ctrl Pts',(-3.02382794858682,6.0566784100051,99.3445758756997));
#208214=CARTESIAN_POINT('Ctrl Pts',(-3.18923239109276,5.97123819492084,
99.3533255301372));
#208215=CARTESIAN_POINT('Ctrl Pts',(-3.35083705967695,5.87913088810715,
99.3620751845747));
#208216=CARTESIAN_POINT('Ctrl Pts',(-3.51243888042392,5.78702520443108,
99.3708246848236));
#208217=CARTESIAN_POINT('Ctrl Pts',(-3.67024081223679,5.68825280605791,
99.3795741850726));
#208218=CARTESIAN_POINT('Ctrl Pts',(-3.82370687544386,5.58314917682515,
99.3883236853216));
#208219=CARTESIAN_POINT('Ctrl Pts',(-3.97717043817807,5.47804726008027,
99.397073043012));
#208220=CARTESIAN_POINT('Ctrl Pts',(-4.1262980372246,5.36661448084237,99.4058224007025));
#208221=CARTESIAN_POINT('Ctrl Pts',(-4.27058317206914,5.24922931204571,
99.414571758393));
#208222=CARTESIAN_POINT('Ctrl Pts',(-4.41486614774825,5.13184589986798,
99.423320985153));
#208223=CARTESIAN_POINT('Ctrl Pts',(-4.55430658194389,5.00851045723056,
99.4320702119131));
#208224=CARTESIAN_POINT('Ctrl Pts',(-4.68843089001807,4.87964187103156,
99.4408194386731));
#208225=CARTESIAN_POINT('Ctrl Pts',(-4.82255336917816,4.75077504207982,
99.4495685461291));
#208226=CARTESIAN_POINT('Ctrl Pts',(-4.9513596606513,4.61637541908099,99.458317653585));
#208227=CARTESIAN_POINT('Ctrl Pts',(-5.07441230869255,4.47689945401832,
99.4670667610409));
#208228=CARTESIAN_POINT('Ctrl Pts',(-5.197463442264,4.33742520555534,99.4758157608173));
#208229=CARTESIAN_POINT('Ctrl Pts',(-5.31476088454725,4.19287495491389,
99.4845647605936));
#208230=CARTESIAN_POINT('Ctrl Pts',(-5.42590627628788,4.04373961586794,
99.49331376037));
#208231=CARTESIAN_POINT('Ctrl Pts',(-5.53706380672606,3.89458798906821,
99.5020637156647));
#208232=CARTESIAN_POINT('Ctrl Pts',(-5.64206777071807,3.74085050155371,
99.5108136709594));
#208233=CARTESIAN_POINT('Ctrl Pts',(-5.74056148163954,3.58304938223247,
99.5195636262541));
#208234=CARTESIAN_POINT('Ctrl Pts',(-5.83905138951829,3.42525435593374,
99.5283132436952));
#208235=CARTESIAN_POINT('Ctrl Pts',(-5.93103139557598,3.26339625497282,
99.5370628611363));
#208236=CARTESIAN_POINT('Ctrl Pts',(-6.01618907820792,3.0980248506511,99.5458124785774));
#208237=CARTESIAN_POINT('Ctrl Pts',(-6.10134392544938,2.93265895249735,
99.5545618046933));
#208238=CARTESIAN_POINT('Ctrl Pts',(-6.17967677261795,2.76378023986118,
99.5633111308091));
#208239=CARTESIAN_POINT('Ctrl Pts',(-6.25092157009195,2.59196229227187,
99.572060456925));
#208240=CARTESIAN_POINT('Ctrl Pts',(-6.32216437407727,2.42014915229159,
99.5808095382275));
#208241=CARTESIAN_POINT('Ctrl Pts',(-6.38631941548899,2.24539720662914,
99.5895586195299));
#208242=CARTESIAN_POINT('Ctrl Pts',(-6.44316881037518,2.06829994947745,
99.5983077008324));
#208243=CARTESIAN_POINT('Ctrl Pts',(-6.50002334524556,1.89118668024503,
99.6070575731747));
#208244=CARTESIAN_POINT('Ctrl Pts',(-6.54957082411084,1.71172794807748,
99.6158074455171));
#208245=CARTESIAN_POINT('Ctrl Pts',(-6.59164294296075,1.53053334250379,
99.6245573178594));
#208246=CARTESIAN_POINT('Ctrl Pts',(-6.63371214082135,1.349351316936,99.6333065827144));
#208247=CARTESIAN_POINT('Ctrl Pts',(-6.66830695239698,1.16643393829725,
99.6420558475693));
#208248=CARTESIAN_POINT('Ctrl Pts',(-6.69530988154,0.982402458340209,99.6508051124242));
#208249=CARTESIAN_POINT('Ctrl Pts',(-6.7223141969049,0.798361530946412,
99.6595548264312));
#208250=CARTESIAN_POINT('Ctrl Pts',(-6.74172580829282,0.613206671361964,
99.6683045404382));
#208251=CARTESIAN_POINT('Ctrl Pts',(-6.75347878028182,0.427566795113024,
99.6770542544453));
#208252=CARTESIAN_POINT('Ctrl Pts',(-6.7624899236821,0.285234494205959,
99.6837627642335));
#208253=CARTESIAN_POINT('Ctrl Pts',(-6.76699999999991,0.142617266093883,
99.6904712740217));
#208254=CARTESIAN_POINT('Ctrl Pts',(-6.767,4.25434840218059E-12,99.6971797838099));
#208255=CARTESIAN_POINT('',(-6.76699937651497,0.00290486591272912,99.3028202161581));
#208256=CARTESIAN_POINT('Ctrl Pts',(3.09910619832135,6.0156321173694,98.651562053011));
#208257=CARTESIAN_POINT('Ctrl Pts',(2.94539729005725,6.0948191788526,98.6596893350202));
#208258=CARTESIAN_POINT('Ctrl Pts',(2.78852930422189,6.16817400846309,98.6678166170294));
#208259=CARTESIAN_POINT('Ctrl Pts',(2.62899026849084,6.23543897157052,98.6759438990386));
#208260=CARTESIAN_POINT('Ctrl Pts',(2.4695293027883,6.30267101873633,98.6840672039827));
#208261=CARTESIAN_POINT('Ctrl Pts',(2.3074002266862,6.36381899169876,98.6921905089268));
#208262=CARTESIAN_POINT('Ctrl Pts',(2.14311362026115,6.41867221554826,98.7003138138708));
#208263=CARTESIAN_POINT('Ctrl Pts',(1.97887461140244,6.47350954717125,98.7084347653087));
#208264=CARTESIAN_POINT('Ctrl Pts',(1.81247966450007,6.52205564690004,98.7165557167466));
#208265=CARTESIAN_POINT('Ctrl Pts',(1.64445716343334,6.56414881287991,98.7246766681845));
#208266=CARTESIAN_POINT('Ctrl Pts',(1.47642585951481,6.60624418415908,98.7327980450864));
#208267=CARTESIAN_POINT('Ctrl Pts',(1.30676718520606,6.64188585278288,98.7409194219883));
#208268=CARTESIAN_POINT('Ctrl Pts',(1.13602263220171,6.67096256766035,98.7490407988902));
#208269=CARTESIAN_POINT('Ctrl Pts',(1.03859639247689,6.68755363861527,98.7536748279062));
#208270=CARTESIAN_POINT('Ctrl Pts',(0.940816821740404,6.70200822244948,
98.7583088569221));
#208271=CARTESIAN_POINT('Ctrl Pts',(0.842785732967011,6.71431315983305,
98.7629428859381));
#208272=CARTESIAN_POINT('Ctrl Pts',(0.652723416207684,6.73816992747649,
98.7719273244639));
#208273=CARTESIAN_POINT('Ctrl Pts',(0.461809585811702,6.75393194326004,
98.7809117629898));
#208274=CARTESIAN_POINT('Ctrl Pts',(0.270714710250231,6.76158284321461,
98.7898962015156));
#208275=CARTESIAN_POINT('Ctrl Pts',(0.0792900163384037,6.76924694816587,
98.7988961466462));
#208276=CARTESIAN_POINT('Ctrl Pts',(-0.112316108485565,6.7687719468986,
98.8078960917767));
#208277=CARTESIAN_POINT('Ctrl Pts',(-0.303433843249637,6.76019355512627,
98.8168960369072));
#208278=CARTESIAN_POINT('Ctrl Pts',(-0.495001951861071,6.75159494815355,
98.8259171906394));
#208279=CARTESIAN_POINT('Ctrl Pts',(-0.686079127952757,6.73485475374515,
98.8349383443717));
#208280=CARTESIAN_POINT('Ctrl Pts',(-0.87599853800856,6.71006077181175,
98.8439594981039));
#208281=CARTESIAN_POINT('Ctrl Pts',(-1.06611119256134,6.68524156180626,
98.8529898309312));
#208282=CARTESIAN_POINT('Ctrl Pts',(-1.25506349169075,6.65235222995014,
98.8620201637584));
#208283=CARTESIAN_POINT('Ctrl Pts',(-1.44219783452507,6.61153192581653,
98.8710504965857));
#208284=CARTESIAN_POINT('Ctrl Pts',(-1.62959747486912,6.57065375135901,
98.8800936315784));
#208285=CARTESIAN_POINT('Ctrl Pts',(-1.81517377197393,6.52182217369165,
98.889136766571));
#208286=CARTESIAN_POINT('Ctrl Pts',(-1.99828108366242,6.46522711980615,
98.8981799015637));
#208287=CARTESIAN_POINT('Ctrl Pts',(-2.15835905952878,6.41575000397448,
98.9060856849634));
#208288=CARTESIAN_POINT('Ctrl Pts',(-2.31655017419342,6.36034022230886,
98.9139914683632));
#208289=CARTESIAN_POINT('Ctrl Pts',(-2.47243429729272,6.29915531206928,
98.9218972517629));
#208290=CARTESIAN_POINT('Ctrl Pts',(-2.64305949249448,6.23218449396756,
98.9305506399911));
#208291=CARTESIAN_POINT('Ctrl Pts',(-2.81107101001989,6.15823428901692,
98.9392040282194));
#208292=CARTESIAN_POINT('Ctrl Pts',(-2.9758955243122,6.0775270323034,98.9478574164476));
#208293=CARTESIAN_POINT('Ctrl Pts',(-3.14056781147405,5.99689431446628,
98.956502812658));
#208294=CARTESIAN_POINT('Ctrl Pts',(-3.30205869402704,5.90951712514607,
98.9651482088684));
#208295=CARTESIAN_POINT('Ctrl Pts',(-3.45981536389501,5.81566562379201,
98.9737936050788));
#208296=CARTESIAN_POINT('Ctrl Pts',(-3.62261025037805,5.71881682163369,
98.9827151061212));
#208297=CARTESIAN_POINT('Ctrl Pts',(-3.78142815372573,5.6150734376972,98.9916366071637));
#208298=CARTESIAN_POINT('Ctrl Pts',(-3.93568751515778,5.50478453556823,
99.0005581082061));
#208299=CARTESIAN_POINT('Ctrl Pts',(-4.08488811246321,5.39811243527532,
99.009187038548));
#208300=CARTESIAN_POINT('Ctrl Pts',(-4.22982412733714,5.28531749407164,
99.0178159688899));
#208301=CARTESIAN_POINT('Ctrl Pts',(-4.36999698499979,5.16676062452024,
99.0264448992319));
#208302=CARTESIAN_POINT('Ctrl Pts',(-4.51729884988509,5.04217410847792,
99.0355126856245));
#208303=CARTESIAN_POINT('Ctrl Pts',(-4.65934014354247,4.91122447635432,
99.0445804720172));
#208304=CARTESIAN_POINT('Ctrl Pts',(-4.79557933767625,4.774380359382,99.0536482584098));
#208305=CARTESIAN_POINT('Ctrl Pts',(-4.93181853181004,4.63753624240968,
99.0627160448025));
#208306=CARTESIAN_POINT('Ctrl Pts',(-5.06225532594945,4.49479789249544,
99.0717838311951));
#208307=CARTESIAN_POINT('Ctrl Pts',(-5.1863907628446,4.34668147614708,99.0808516175878));
#208308=CARTESIAN_POINT('Ctrl Pts',(-5.30172603488717,4.20906527564233,
99.089276573721));
#208309=CARTESIAN_POINT('Ctrl Pts',(-5.41157128508455,4.06686703945213,
99.0977015298542));
#208310=CARTESIAN_POINT('Ctrl Pts',(-5.51557045188123,3.92055756115564,
99.1061264859874));
#208311=CARTESIAN_POINT('Ctrl Pts',(-5.61959375788314,3.77421412302436,
99.1145533976339));
#208312=CARTESIAN_POINT('Ctrl Pts',(-5.71776808284151,3.62375781041807,
99.1229803092803));
#208313=CARTESIAN_POINT('Ctrl Pts',(-5.80978040874206,3.46968883362715,
99.1314072209268));
#208314=CARTESIAN_POINT('Ctrl Pts',(-5.90182657115849,3.31556319967287,
99.1398372314768));
#208315=CARTESIAN_POINT('Ctrl Pts',(-5.98770604636861,3.15782253715786,
99.1482672420269));
#208316=CARTESIAN_POINT('Ctrl Pts',(-6.06715133435416,2.99699244010466,
99.156697252577));
#208317=CARTESIAN_POINT('Ctrl Pts',(-6.14666980567764,2.83601418972937,
99.1651350286765));
#208318=CARTESIAN_POINT('Ctrl Pts',(-6.21974210111039,2.67194111643444,
99.173572804776));
#208319=CARTESIAN_POINT('Ctrl Pts',(-6.28614806347648,2.50532064296189,
99.1820105808754));
#208320=CARTESIAN_POINT('Ctrl Pts',(-6.35258888407773,2.3386127060231,99.1904527861854));
#208321=CARTESIAN_POINT('Ctrl Pts',(-6.41235627723871,2.16935501259267,
99.1988949914954));
#208322=CARTESIAN_POINT('Ctrl Pts',(-6.46527952044811,1.99811153904739,
99.2073371968053));
#208323=CARTESIAN_POINT('Ctrl Pts',(-6.51825859476721,1.82668741305946,
99.2157883081774));
#208324=CARTESIAN_POINT('Ctrl Pts',(-6.56437900580895,1.65327364099432,
99.2242394195495));
#208325=CARTESIAN_POINT('Ctrl Pts',(-6.60352056647827,1.47844686346807,
99.2326905309215));
#208326=CARTESIAN_POINT('Ctrl Pts',(-6.61450570610864,1.42938145755646,
99.2350623484185));
#208327=CARTESIAN_POINT('Ctrl Pts',(-6.6249414661072,1.38020480506695,99.2374341659155));
#208328=CARTESIAN_POINT('Ctrl Pts',(-6.63482592045994,1.3309297521631,99.2398059834124));
#208329=CARTESIAN_POINT('Ctrl Pts',(-6.68056170661874,1.10293200922748,
99.2507804827604));
#208330=CARTESIAN_POINT('Ctrl Pts',(-6.71454523216173,0.872555263279585,
99.2617549821083));
#208331=CARTESIAN_POINT('Ctrl Pts',(-6.73658836297482,0.640832449109899,
99.2727294814563));
#208332=CARTESIAN_POINT('Ctrl Pts',(-6.75673488569275,0.42904724584105,
99.2827597263568));
#208333=CARTESIAN_POINT('Ctrl Pts',(-6.76690784226229,0.216137507080814,
99.2927899712574));
#208334=CARTESIAN_POINT('Ctrl Pts',(-6.76699937651497,0.00290486591292295,
99.302820216158));
#208335=CARTESIAN_POINT('Ctrl Pts',(-6.76699937651526,0.0029048652382334,
99.3028202161898));
#208336=CARTESIAN_POINT('Ctrl Pts',(-6.76707461989407,-0.172377585301011,
99.311065323018));
#208337=CARTESIAN_POINT('Ctrl Pts',(-6.7603351851076,-0.3477811383096,99.3193104298461));
#208338=CARTESIAN_POINT('Ctrl Pts',(-6.74677933403267,-0.522740488071986,
99.3275555366743));
#208339=CARTESIAN_POINT('Ctrl Pts',(-6.73323011857456,-0.697614194874938,
99.3357966075058));
#208340=CARTESIAN_POINT('Ctrl Pts',(-6.71287116233085,-0.872043779040175,
99.3440376783373));
#208341=CARTESIAN_POINT('Ctrl Pts',(-6.68575278601598,-1.04546577384418,
99.3522787491688));
#208342=CARTESIAN_POINT('Ctrl Pts',(-6.65758548255101,-1.22559565693259,
99.360838581081));
#208343=CARTESIAN_POINT('Ctrl Pts',(-6.62212542119759,-1.4046380490682,
99.3693984129932));
#208344=CARTESIAN_POINT('Ctrl Pts',(-6.57948809993647,-1.58196881852786,
99.3779582449054));
#208345=CARTESIAN_POINT('Ctrl Pts',(-6.53844634137191,-1.75266356226325,
99.3861977530242));
#208346=CARTESIAN_POINT('Ctrl Pts',(-6.49075486168368,-1.92177210105994,
99.394437261143));
#208347=CARTESIAN_POINT('Ctrl Pts',(-6.43656847215185,-2.08874969857588,
99.4026767692618));
#208348=CARTESIAN_POINT('Ctrl Pts',(-6.38237508461469,-2.25574886073428,
99.4109173414876));
#208349=CARTESIAN_POINT('Ctrl Pts',(-6.3216852249945,-2.42061619582955,
99.4191579137135));
#208350=CARTESIAN_POINT('Ctrl Pts',(-6.25470312132414,-2.58282362233624,
99.4273984859394));
#208351=CARTESIAN_POINT('Ctrl Pts',(-6.18770057383033,-2.74508055669367,
99.4356415732969));
#208352=CARTESIAN_POINT('Ctrl Pts',(-6.11440209114554,-2.90467563728018,
99.4438846606543));
#208353=CARTESIAN_POINT('Ctrl Pts',(-6.03505947804925,-3.06110210486484,
99.4521277480118));
#208354=CARTESIAN_POINT('Ctrl Pts',(-5.95567867843879,-3.21760385836821,
99.4603748026544));
#208355=CARTESIAN_POINT('Ctrl Pts',(-5.8702481127369,-3.3709336445959,99.468621857297));
#208356=CARTESIAN_POINT('Ctrl Pts',(-5.77906487104334,-3.5206104891443,
99.4768689119396));
#208357=CARTESIAN_POINT('Ctrl Pts',(-5.68777422208742,-3.67046364218768,
99.485125681016));
#208358=CARTESIAN_POINT('Ctrl Pts',(-5.59071754823313,-3.81665495715636,
99.4933824500924));
#208359=CARTESIAN_POINT('Ctrl Pts',(-5.48823504557674,-3.95873276245105,
99.5016392191688));
#208360=CARTESIAN_POINT('Ctrl Pts',(-5.38568136729878,-4.1009092428936,
99.509901722694));
#208361=CARTESIAN_POINT('Ctrl Pts',(-5.27769456590132,-4.23896624024573,
99.5181642262193));
#208362=CARTESIAN_POINT('Ctrl Pts',(-5.164654200136,-4.37248624846524,99.5264267297445));
#208363=CARTESIAN_POINT('Ctrl Pts',(-5.05146025447411,-4.50618766081338,
99.5347004589451));
#208364=CARTESIAN_POINT('Ctrl Pts',(-4.93319927158584,-4.63533951395193,
99.5429741881455));
#208365=CARTESIAN_POINT('Ctrl Pts',(-4.8102872529871,-4.75956148649745,
99.551247917346));
#208366=CARTESIAN_POINT('Ctrl Pts',(-4.77826432266308,-4.79192570617986,
99.5534035165847));
#208367=CARTESIAN_POINT('Ctrl Pts',(-4.74592585773266,-4.82395550698373,
99.5555591158233));
#208368=CARTESIAN_POINT('Ctrl Pts',(-4.7132795673047,-4.85564462460218,
99.5577147150619));
#208369=CARTESIAN_POINT('Ctrl Pts',(-4.59106272309898,-4.97427813242865,
99.5657845610646));
#208370=CARTESIAN_POINT('Ctrl Pts',(-4.464138191083,-5.08851333835254,99.5738544070674));
#208371=CARTESIAN_POINT('Ctrl Pts',(-4.33286015346576,-5.19794304417706,
99.5819242530702));
#208372=CARTESIAN_POINT('Ctrl Pts',(-4.20174728031799,-5.30723507351254,
99.5899839461802));
#208373=CARTESIAN_POINT('Ctrl Pts',(-4.06629208274724,-5.41173339663901,
99.5980436392903));
#208374=CARTESIAN_POINT('Ctrl Pts',(-3.92688715996402,-5.51106579827439,
99.6061033324003));
#208375=CARTESIAN_POINT('Ctrl Pts',(-3.78762703133491,-5.61029502743362,
99.6141546542389));
#208376=CARTESIAN_POINT('Ctrl Pts',(-3.64442564260747,-5.70436879809481,
99.6222059760775));
#208377=CARTESIAN_POINT('Ctrl Pts',(-3.49771033363369,-5.79295360088376,
99.6302572979162));
#208378=CARTESIAN_POINT('Ctrl Pts',(-3.35111526148789,-5.88146580623371,
99.6383020214972));
#208379=CARTESIAN_POINT('Ctrl Pts',(-3.20101231847573,-5.96449780500423,
99.6463467450782));
#208380=CARTESIAN_POINT('Ctrl Pts',(-3.04785954378699,-6.04175812171809,
99.6543914686593));
#208381=CARTESIAN_POINT('Ctrl Pts',(-2.89479875637982,-6.11897203400657,
99.6624313603837));
#208382=CARTESIAN_POINT('Ctrl Pts',(-2.73869211612158,-6.19042099757312,
99.6704712521081));
#208383=CARTESIAN_POINT('Ctrl Pts',(-2.5800239983328,-6.25585846771063,
99.6785111438325));
#208384=CARTESIAN_POINT('Ctrl Pts',(-2.41793932126784,-6.32270498585807,
99.6867241564524));
#208385=CARTESIAN_POINT('Ctrl Pts',(-2.2531819452021,-6.38327797982675,
99.6949371690724));
#208386=CARTESIAN_POINT('Ctrl Pts',(-2.08629218611878,-6.43736544823577,
99.7031501816923));
#208387=CARTESIAN_POINT('Ctrl Pts',(-1.92297727368812,-6.49029434102904,
99.7111872682349));
#208388=CARTESIAN_POINT('Ctrl Pts',(-1.75762077966772,-6.5370126314901,
99.7192243547775));
#208389=CARTESIAN_POINT('Ctrl Pts',(-1.59074623467904,-6.57737146714814,
99.7272614413201));
#208390=CARTESIAN_POINT('Ctrl Pts',(-1.42385571901983,-6.61773416533457,
99.7352992970492));
#208391=CARTESIAN_POINT('Ctrl Pts',(-1.25544722624345,-6.65173610887908,
99.7433371527784));
#208392=CARTESIAN_POINT('Ctrl Pts',(-1.08605603557982,-6.67927924910919,
99.7513750085075));
#208393=CARTESIAN_POINT('Ctrl Pts',(-0.916615071340223,-6.70683048256173,
99.7594152260645));
#208394=CARTESIAN_POINT('Ctrl Pts',(-0.746191203033471,-6.72791907518196,
99.7674554436214));
#208395=CARTESIAN_POINT('Ctrl Pts',(-0.575326261399993,-6.74249869803054,
99.7754956611784));
#208396=CARTESIAN_POINT('Ctrl Pts',(-0.398005932795349,-6.75762914837177,
99.7838396433062));
#208397=CARTESIAN_POINT('Ctrl Pts',(-0.220210995243738,-6.76574915837271,
99.7921836254339));
#208398=CARTESIAN_POINT('Ctrl Pts',(-0.0425475252329801,-6.76686623985553,
99.8005276075617));
#208399=CARTESIAN_POINT('Ctrl Pts',(0.128946101418613,-6.76794452766981,
99.8085818223968));
#208400=CARTESIAN_POINT('Ctrl Pts',(0.300316872996476,-6.76249820220135,
99.8166360372318));
#208401=CARTESIAN_POINT('Ctrl Pts',(0.471025049325828,-6.75058696728719,
99.8246902520669));
#208402=CARTESIAN_POINT('Ctrl Pts',(0.641860972496963,-6.73866681878332,
99.8327504941499));
#208403=CARTESIAN_POINT('Ctrl Pts',(0.812032944247111,-6.72027216779632,
99.8408107362329));
#208404=CARTESIAN_POINT('Ctrl Pts',(0.98101087477628,-6.69551392079583,
99.8488709783159));
#208405=CARTESIAN_POINT('Ctrl Pts',(1.15022504804352,-6.67072106006771,
99.8569424891702));
#208406=CARTESIAN_POINT('Ctrl Pts',(1.31824148558976,-6.63954692029786,
99.8650140000246));
#208407=CARTESIAN_POINT('Ctrl Pts',(1.48454415714527,-6.60215250092618,
99.8730855108789));
#208408=CARTESIAN_POINT('Ctrl Pts',(1.50197441346389,-6.59823317534688,
99.8739314894898));
#208409=CARTESIAN_POINT('Ctrl Pts',(1.51938586122411,-6.59424556237967,
99.8747774681007));
#208410=CARTESIAN_POINT('Ctrl Pts',(1.53677791905461,-6.59018987795543,
99.8756234467116));
#208411=CARTESIAN_POINT('Ctrl Pts',(1.70595901354953,-6.55073824224293,
99.8838526964476));
#208412=CARTESIAN_POINT('Ctrl Pts',(1.87386854883584,-6.50470971120342,
99.8920819461835));
#208413=CARTESIAN_POINT('Ctrl Pts',(2.0399568793622,-6.45219845714179,99.9003111959195));
#208414=CARTESIAN_POINT('Ctrl Pts',(2.20584753775609,-6.39974970001499,
99.9085306515096));
#208415=CARTESIAN_POINT('Ctrl Pts',(2.36992096880443,-6.34083369006769,
99.9167501070996));
#208416=CARTESIAN_POINT('Ctrl Pts',(2.53163761468347,-6.27559558830234,
99.9249695626897));
#208417=CARTESIAN_POINT('Ctrl Pts',(2.69319426812721,-6.21042202907508,
99.9331808864594));
#208418=CARTESIAN_POINT('Ctrl Pts',(2.85239844952946,-6.13893896731954,
99.941392210229));
#208419=CARTESIAN_POINT('Ctrl Pts',(3.00872558727029,-6.06134138128723,
99.9496035339987));
#208420=CARTESIAN_POINT('Ctrl Pts',(3.16492944760644,-5.98380498763109,
99.9578083824328));
#208421=CARTESIAN_POINT('Ctrl Pts',(3.31826046338572,-5.90016383237433,
99.9660132308668));
#208422=CARTESIAN_POINT('Ctrl Pts',(3.46821380881486,-5.8106610619056,99.9742180793009));
#208423=CARTESIAN_POINT('Ctrl Pts',(3.61807899879668,-5.7212109088476,99.9824181042208));
#208424=CARTESIAN_POINT('Ctrl Pts',(3.76457016697336,-5.62590618859519,
99.9906181291407));
#208425=CARTESIAN_POINT('Ctrl Pts',(3.90720680747295,-5.52503610518855,
99.9988181540606));
#208426=CARTESIAN_POINT('Ctrl Pts',(4.04980216569743,-5.4241952158692,100.007015805707));
#208427=CARTESIAN_POINT('Ctrl Pts',(4.18854492360851,-5.31779237537217,
100.015213457354));
#208428=CARTESIAN_POINT('Ctrl Pts',(4.32298310791889,-5.20616039405702,
100.023411109001));
#208429=CARTESIAN_POINT('Ctrl Pts',(4.45740329013162,-5.09454336094902,
100.031607662932));
#208430=CARTESIAN_POINT('Ctrl Pts',(4.58751977028578,-4.97769881004729,
100.039804216864));
#208431=CARTESIAN_POINT('Ctrl Pts',(4.71291325768196,-4.85600016737702,
100.048000770795));
#208432=CARTESIAN_POINT('Ctrl Pts',(4.83831275391542,-4.73429569292587,
100.056197717503));
#208433=CARTESIAN_POINT('Ctrl Pts',(4.95898854899892,-4.60773691312512,
100.064394664212));
#208434=CARTESIAN_POINT('Ctrl Pts',(5.07455783015735,-4.47673450501464,
100.072591610921));
#208435=CARTESIAN_POINT('Ctrl Pts',(5.19015366282928,-4.34570199970038,
100.08079044084));
#208436=CARTESIAN_POINT('Ctrl Pts',(5.30064040763602,-4.21022410171465,
100.08898927076));
#208437=CARTESIAN_POINT('Ctrl Pts',(5.40567517013402,-4.07074501227926,
100.09718810068));
#208438=CARTESIAN_POINT('Ctrl Pts',(5.51080941398005,-3.93113381831479,
100.10539469594));
#208439=CARTESIAN_POINT('Ctrl Pts',(5.61048114277883,-3.78751414850098,
100.1136012912));
#208440=CARTESIAN_POINT('Ctrl Pts',(5.70438996117341,-3.64036044518452,
100.121807886459));
#208441=CARTESIAN_POINT('Ctrl Pts',(5.79834423197477,-3.49313551863154,
100.130018453758));
#208442=CARTESIAN_POINT('Ctrl Pts',(5.88652985018573,-3.34237345774138,
100.138229021057));
#208443=CARTESIAN_POINT('Ctrl Pts',(5.96869219956712,-3.18857372924426,
100.146439588356));
#208444=CARTESIAN_POINT('Ctrl Pts',(6.05096786259049,-3.0345618889039,100.154661479203));
#208445=CARTESIAN_POINT('Ctrl Pts',(6.12720349859119,-2.87750433127488,
100.16288337005));
#208446=CARTESIAN_POINT('Ctrl Pts',(6.1971919971014,-2.71792206493535,100.171105260896));
#208447=CARTESIAN_POINT('Ctrl Pts',(6.26082805960978,-2.57282412324239,
100.178580900051));
#208448=CARTESIAN_POINT('Ctrl Pts',(6.31930008812324,-2.42563940340715,
100.186056539206));
#208449=CARTESIAN_POINT('Ctrl Pts',(6.37248835238525,-2.27676990464875,
100.193532178361));
#208450=CARTESIAN_POINT('Ctrl Pts',(6.43606650427784,-2.09881998025171,
100.202468121812));
#208451=CARTESIAN_POINT('Ctrl Pts',(6.49222727935702,-1.91809214767458,
100.211404065263));
#208452=CARTESIAN_POINT('Ctrl Pts',(6.54074678974077,-1.73520040124931,
100.220340008713));
#208453=CARTESIAN_POINT('Ctrl Pts',(6.58919336243151,-1.55258358962758,
100.229262519071));
#208454=CARTESIAN_POINT('Ctrl Pts',(6.63002152457474,-1.36780960388155,
100.238185029429));
#208455=CARTESIAN_POINT('Ctrl Pts',(6.66305689940416,-1.18150825443693,
100.247107539786));
#208456=CARTESIAN_POINT('Ctrl Pts',(6.69601132731341,-0.995663401113205,
100.256008187225));
#208457=CARTESIAN_POINT('Ctrl Pts',(6.7212110326332,-0.808298907264183,
100.264908834663));
#208458=CARTESIAN_POINT('Ctrl Pts',(6.7385325561776,-0.620054827684308,
100.273809482101));
#208459=CARTESIAN_POINT('Ctrl Pts',(6.75582731144526,-0.432101656095412,
100.282696374687));
#208460=CARTESIAN_POINT('Ctrl Pts',(6.76526814684622,-0.243271866040026,
100.291583267274));
#208461=CARTESIAN_POINT('Ctrl Pts',(6.76678283078964,-0.05421365999973,
100.30047015986));
#208462=CARTESIAN_POINT('Ctrl Pts',(6.76829362142991,0.134358595876913,
100.309334209815));
#208463=CARTESIAN_POINT('Ctrl Pts',(6.76191891179613,0.323157838770076,
100.31819825977));
#208464=CARTESIAN_POINT('Ctrl Pts',(6.74763828243208,0.511533585854418,
100.327062309725));
#208465=CARTESIAN_POINT('Ctrl Pts',(6.73398485196275,0.691635953849492,
100.335537054545));
#208466=CARTESIAN_POINT('Ctrl Pts',(6.71310500021671,0.871350964271029,
100.344011799366));
#208467=CARTESIAN_POINT('Ctrl Pts',(6.68502535051704,1.05010716736179,100.352486544186));
#208468=CARTESIAN_POINT('Ctrl Pts',(6.65782648536332,1.22325625986319,100.360695458615));
#208469=CARTESIAN_POINT('Ctrl Pts',(6.62389767383333,1.39533869462894,100.368904373044));
#208470=CARTESIAN_POINT('Ctrl Pts',(6.58335427138304,1.56580188320958,100.377113287473));
#208471=CARTESIAN_POINT('Ctrl Pts',(6.54280122994474,1.73630559854754,100.38532415353));
#208472=CARTESIAN_POINT('Ctrl Pts',(6.49563054694887,1.90518895431156,100.393535019587));
#208473=CARTESIAN_POINT('Ctrl Pts',(6.44200800525192,2.07191260922613,100.401745885644));
#208474=CARTESIAN_POINT('Ctrl Pts',(6.3883631566255,2.23870562103226,100.409960167414));
#208475=CARTESIAN_POINT('Ctrl Pts',(6.32826121120446,2.40333680341831,100.418174449183));
#208476=CARTESIAN_POINT('Ctrl Pts',(6.2619168459761,2.56528486022132,100.426388730953));
#208477=CARTESIAN_POINT('Ctrl Pts',(6.19549780492688,2.72741520234786,100.434612258545));
#208478=CARTESIAN_POINT('Ctrl Pts',(6.12282244519839,2.88685605718566,100.442835786138));
#208479=CARTESIAN_POINT('Ctrl Pts',(6.04415276581908,3.04310800719291,100.45105931373));
#208480=CARTESIAN_POINT('Ctrl Pts',(5.96543266223536,3.19946010862227,100.459288112284));
#208481=CARTESIAN_POINT('Ctrl Pts',(5.88071075187738,3.3526189199293,100.467516910838));
#208482=CARTESIAN_POINT('Ctrl Pts',(5.79029344738274,3.50211233303509,100.475745709391));
#208483=CARTESIAN_POINT('Ctrl Pts',(5.69975169070402,3.65181151186097,100.483985834228));
#208484=CARTESIAN_POINT('Ctrl Pts',(5.60349907709188,3.79783491887417,100.492225959064));
#208485=CARTESIAN_POINT('Ctrl Pts',(5.50188410796304,3.93974114156549,100.500466083901));
#208486=CARTESIAN_POINT('Ctrl Pts',(5.45677125516429,4.00274164818753,100.504124359271));
#208487=CARTESIAN_POINT('Ctrl Pts',(5.41060200277377,4.06493111563783,100.507782634641));
#208488=CARTESIAN_POINT('Ctrl Pts',(5.36340923191248,4.12627318667051,100.511440910011));
#208489=CARTESIAN_POINT('Ctrl Pts',(5.25442051244402,4.26793881997365,100.5198894656));
#208490=CARTESIAN_POINT('Ctrl Pts',(5.13972092806317,4.4054066894299,100.52833802119));
#208491=CARTESIAN_POINT('Ctrl Pts',(5.01965932110736,4.53820551540144,100.536786576779));
#208492=CARTESIAN_POINT('Ctrl Pts',(4.89970465433643,4.67088605600797,100.545227607148));
#208493=CARTESIAN_POINT('Ctrl Pts',(4.77439770683847,4.79890559577125,100.553668637516));
#208494=CARTESIAN_POINT('Ctrl Pts',(4.6441281338455,4.92182515703521,100.562109667885));
#208495=CARTESIAN_POINT('Ctrl Pts',(4.51397820040631,5.04463182899492,100.570542946013));
#208496=CARTESIAN_POINT('Ctrl Pts',(4.37887497366288,5.16234763637225,100.578976224141));
#208497=CARTESIAN_POINT('Ctrl Pts',(4.23924560992898,5.27456971313281,100.587409502268));
#208498=CARTESIAN_POINT('Ctrl Pts',(4.09969275739106,5.38673029677273,100.595838159304));
#208499=CARTESIAN_POINT('Ctrl Pts',(3.95561897013448,5.49340294114936,100.604266816339));
#208500=CARTESIAN_POINT('Ctrl Pts',(3.80748577284527,5.5942239041337,100.612695473375));
#208501=CARTESIAN_POINT('Ctrl Pts',(3.65942011893495,5.69499889640635,100.621120287247));
#208502=CARTESIAN_POINT('Ctrl Pts',(3.50729902106169,5.78992734033334,100.62954510112));
#208503=CARTESIAN_POINT('Ctrl Pts',(3.35161460815422,5.87868765273401,100.637969914993));
#208504=CARTESIAN_POINT('Ctrl Pts',(3.2684356934009,5.92611042499985,100.642471116249));
#208505=CARTESIAN_POINT('Ctrl Pts',(3.18424012333501,5.97177320619438,100.646972317505));
#208506=CARTESIAN_POINT('Ctrl Pts',(3.09910619832147,6.01563211736933,100.651473518761));
#208507=CARTESIAN_POINT('Origin',(0.,0.,4.30282021618968));
#208508=CARTESIAN_POINT('',(3.09910619832139,6.01563211736937,103.045799558392));
#208509=CARTESIAN_POINT('',(3.09910619832148,6.01563211736933,102.651395695404));
#208510=CARTESIAN_POINT('',(3.09910619832133,6.0156321173694,4.30282021618968));
#208511=CARTESIAN_POINT('',(-6.76699760869595,-0.00568892813878999,101.69717978384));
#208512=CARTESIAN_POINT('Ctrl Pts',(-6.76699760869595,-0.00568892813878413,
101.69717978384));
#208513=CARTESIAN_POINT('Ctrl Pts',(-6.76680510301031,-0.234675036349317,
101.707957090383));
#208514=CARTESIAN_POINT('Ctrl Pts',(-6.75498606488932,-0.463202034117518,
101.718734396925));
#208515=CARTESIAN_POINT('Ctrl Pts',(-6.73170191760452,-0.690274070583281,
101.729511703468));
#208516=CARTESIAN_POINT('Ctrl Pts',(-6.71089442214133,-0.893193263233427,
101.739142666297));
#208517=CARTESIAN_POINT('Ctrl Pts',(-6.68093182727304,-1.09495111148143,
101.748773629126));
#208518=CARTESIAN_POINT('Ctrl Pts',(-6.64196113402566,-1.29485184252585,
101.758404591954));
#208519=CARTESIAN_POINT('Ctrl Pts',(-6.6058027646821,-1.48032671769085,
101.767340535405));
#208520=CARTESIAN_POINT('Ctrl Pts',(-6.56184811814019,-1.6644043403748,
101.776276478856));
#208521=CARTESIAN_POINT('Ctrl Pts',(-6.51021806817828,-1.84644244555986,
101.785212422307));
#208522=CARTESIAN_POINT('Ctrl Pts',(-6.45866563187552,-2.02820689919009,
101.794134932664));
#208523=CARTESIAN_POINT('Ctrl Pts',(-6.39946088504986,-2.20793770507951,
101.803057443022));
#208524=CARTESIAN_POINT('Ctrl Pts',(-6.33277535008608,-2.38500426945995,
101.811979953379));
#208525=CARTESIAN_POINT('Ctrl Pts',(-6.26625321537738,-2.56163696580885,
101.820880600818));
#208526=CARTESIAN_POINT('Ctrl Pts',(-6.19228696729786,-2.73561820861534,
101.829781248256));
#208527=CARTESIAN_POINT('Ctrl Pts',(-6.11109714232497,-2.90633458450117,
101.838681895694));
#208528=CARTESIAN_POINT('Ctrl Pts',(-6.03003278620595,-3.07678713929827,
101.847568788281));
#208529=CARTESIAN_POINT('Ctrl Pts',(-5.94176723108616,-3.2439846595089,
101.856455680867));
#208530=CARTESIAN_POINT('Ctrl Pts',(-5.84656922391986,-3.40733287336491,
101.865342573453));
#208531=CARTESIAN_POINT('Ctrl Pts',(-5.7516159111686,-3.57026122133477,
101.874206623408));
#208532=CARTESIAN_POINT('Ctrl Pts',(-5.64976583255248,-3.72935978363406,
101.883070673363));
#208533=CARTESIAN_POINT('Ctrl Pts',(-5.5413334533065,-3.88405877392017,
101.891934723318));
#208534=CARTESIAN_POINT('Ctrl Pts',(-5.43766337596293,-4.03196345331075,
101.900409468139));
#208535=CARTESIAN_POINT('Ctrl Pts',(-5.32797686686972,-4.17584647143222,
101.908884212959));
#208536=CARTESIAN_POINT('Ctrl Pts',(-5.21258850367004,-4.31523001604862,
101.91735895778));
#208537=CARTESIAN_POINT('Ctrl Pts',(-5.10081956906823,-4.45024146651733,
101.925567872209));
#208538=CARTESIAN_POINT('Ctrl Pts',(-4.98380786530573,-4.58090052586389,
101.933776786638));
#208539=CARTESIAN_POINT('Ctrl Pts',(-4.86193464529849,-4.70679089240708,
101.941985701067));
#208540=CARTESIAN_POINT('Ctrl Pts',(-4.74003245055219,-4.83271118874552,
101.950196567124));
#208541=CARTESIAN_POINT('Ctrl Pts',(-4.61326668455911,-4.95386027772515,
101.958407433181));
#208542=CARTESIAN_POINT('Ctrl Pts',(-4.48205520208169,-5.06985898871877,
101.966618299238));
#208543=CARTESIAN_POINT('Ctrl Pts',(-4.35078913574405,-5.18590595507318,
101.974832581007));
#208544=CARTESIAN_POINT('Ctrl Pts',(-4.21507393505767,-5.29679803937224,
101.983046862777));
#208545=CARTESIAN_POINT('Ctrl Pts',(-4.075360289141,-5.4021965452668,101.991261144547));
#208546=CARTESIAN_POINT('Ctrl Pts',(-3.93548938448625,-5.50771368550037,
101.999484672139));
#208547=CARTESIAN_POINT('Ctrl Pts',(-3.79161132986243,-5.6077246823996,
102.007708199732));
#208548=CARTESIAN_POINT('Ctrl Pts',(-3.64420634014303,-5.70193380796913,
102.015931727324));
#208549=CARTESIAN_POINT('Ctrl Pts',(-3.49670686955903,-5.79620331792358,
102.024160525878));
#208550=CARTESIAN_POINT('Ctrl Pts',(-3.34567626392025,-5.88466336391086,
102.032389324431));
#208551=CARTESIAN_POINT('Ctrl Pts',(-3.19161899078301,-5.96706437183924,
102.040618122985));
#208552=CARTESIAN_POINT('Ctrl Pts',(-3.03734967013756,-6.04957879816098,
102.048858247822));
#208553=CARTESIAN_POINT('Ctrl Pts',(-2.8800456801906,-6.12601737330258,
102.057098372658));
#208554=CARTESIAN_POINT('Ctrl Pts',(-2.72023201364944,-6.19617840220218,
102.065338497494));
#208555=CARTESIAN_POINT('Ctrl Pts',(-2.64928134097196,-6.22732700359471,
102.068996772864));
#208556=CARTESIAN_POINT('Ctrl Pts',(-2.57783622507843,-6.25723896011439,
102.072655048234));
#208557=CARTESIAN_POINT('Ctrl Pts',(-2.50594349886725,-6.28589979084021,
102.076313323604));
#208558=CARTESIAN_POINT('Ctrl Pts',(-2.33992226588979,-6.35208599222701,
102.084761346367));
#208559=CARTESIAN_POINT('Ctrl Pts',(-2.17113314524973,-6.4117482900346,
102.093209369129));
#208560=CARTESIAN_POINT('Ctrl Pts',(-2.00011656487015,-6.4646595213462,
102.101657391892));
#208561=CARTESIAN_POINT('Ctrl Pts',(-1.82925658948067,-6.51752230026307,
102.110097678548));
#208562=CARTESIAN_POINT('Ctrl Pts',(-1.65617353726104,-6.56364623744236,
102.118537965203));
#208563=CARTESIAN_POINT('Ctrl Pts',(-1.48142639746172,-6.60285277958729,
102.126978251859));
#208564=CARTESIAN_POINT('Ctrl Pts',(-1.30681237749751,-6.64202945475739,
102.135412108827));
#208565=CARTESIAN_POINT('Ctrl Pts',(-1.13053712135248,-6.67429916704483,
102.143845965795));
#208566=CARTESIAN_POINT('Ctrl Pts',(-0.953173699982523,-6.69953348358389,
102.152279822763));
#208567=CARTESIAN_POINT('Ctrl Pts',(-0.775918124780594,-6.72475245634845,
102.160708551508));
#208568=CARTESIAN_POINT('Ctrl Pts',(-0.59757603289914,-6.74294451546294,
102.169137280253));
#208569=CARTESIAN_POINT('Ctrl Pts',(-0.41872997723262,-6.75403244041415,
102.177566008998));
#208570=CARTESIAN_POINT('Ctrl Pts',(-0.239965205135707,-6.76511532602516,
102.185990906978));
#208571=CARTESIAN_POINT('Ctrl Pts',(-0.0606972582868748,-6.76910049502238,
102.194415804958));
#208572=CARTESIAN_POINT('Ctrl Pts',(0.118486509143059,-6.76596260314459,
102.202840702939));
#208573=CARTESIAN_POINT('Ctrl Pts',(0.297630604995052,-6.76282540600117,
102.211263735633));
#208574=CARTESIAN_POINT('Ctrl Pts',(0.476690225396251,-6.75256829552415,
102.219686768327));
#208575=CARTESIAN_POINT('Ctrl Pts',(0.655077796231265,-6.73521804256438,
102.228109801021));
#208576=CARTESIAN_POINT('Ctrl Pts',(0.833445182715354,-6.71786975276603,
102.236531880659));
#208577=CARTESIAN_POINT('Ctrl Pts',(1.01114033938551,-6.69342995274387,
102.244953960296));
#208578=CARTESIAN_POINT('Ctrl Pts',(1.18758027650778,-6.66197734061365,
102.253376039934));
#208579=CARTESIAN_POINT('Ctrl Pts',(1.36402487934886,-6.63052389676105,
102.261798342282));
#208580=CARTESIAN_POINT('Ctrl Pts',(1.53921386823527,-6.59205732997234,
102.270220644631));
#208581=CARTESIAN_POINT('Ctrl Pts',(1.71257354881077,-6.5467076336059,102.278642946979));
#208582=CARTESIAN_POINT('Ctrl Pts',(1.88596201477482,-6.50135040718041,
102.287066647803));
#208583=CARTESIAN_POINT('Ctrl Pts',(2.05752024442653,-6.4491078575326,102.295490348626));
#208584=CARTESIAN_POINT('Ctrl Pts',(2.22668847037332,-6.39016020580913,
102.30391404945));
#208585=CARTESIAN_POINT('Ctrl Pts',(2.39597117400493,-6.33117266367091,
102.312343450669));
#208586=CARTESIAN_POINT('Ctrl Pts',(2.5628603268792,-6.26547106246991,102.320772851888));
#208587=CARTESIAN_POINT('Ctrl Pts',(2.72681400159689,-6.19328462132132,
102.329202253107));
#208588=CARTESIAN_POINT('Ctrl Pts',(2.8908261747581,-6.12107242415075,102.337634661924));
#208589=CARTESIAN_POINT('Ctrl Pts',(3.05190047865451,-6.04237091346222,
102.346067070742));
#208590=CARTESIAN_POINT('Ctrl Pts',(3.20951794893678,-5.95745612954495,
102.35449947956));
#208591=CARTESIAN_POINT('Ctrl Pts',(3.36728125148852,-5.87246277999895,
102.362939690287));
#208592=CARTESIAN_POINT('Ctrl Pts',(3.52158103934015,-5.78124483501094,
102.371379901015));
#208593=CARTESIAN_POINT('Ctrl Pts',(3.67192482994536,-5.68412324314232,
102.379820111743));
#208594=CARTESIAN_POINT('Ctrl Pts',(3.75743781255772,-5.62888213898156,
102.38462075958));
#208595=CARTESIAN_POINT('Ctrl Pts',(3.84167150762846,-5.57173191324348,
102.389421407417));
#208596=CARTESIAN_POINT('Ctrl Pts',(3.92453983275924,-5.51273762309491,
102.394222055254));
#208597=CARTESIAN_POINT('Ctrl Pts',(4.06504681737886,-5.41271014208249,
102.402361770287));
#208598=CARTESIAN_POINT('Ctrl Pts',(4.20190682985241,-5.30717939374251,
102.41050148532));
#208599=CARTESIAN_POINT('Ctrl Pts',(4.33465777230064,-5.19644407234733,
102.418641200352));
#208600=CARTESIAN_POINT('Ctrl Pts',(4.46729261157105,-5.08580559939988,
102.426773796439));
#208601=CARTESIAN_POINT('Ctrl Pts',(4.59582525489943,-4.96997184687442,
102.434906392526));
#208602=CARTESIAN_POINT('Ctrl Pts',(4.71982309942207,-4.84928437093164,
102.443038988613));
#208603=CARTESIAN_POINT('Ctrl Pts',(4.84373617236596,-4.72867940342205,
102.451166024821));
#208604=CARTESIAN_POINT('Ctrl Pts',(4.96312035755527,-4.60322757336693,
102.459293061029));
#208605=CARTESIAN_POINT('Ctrl Pts',(5.07757667926858,-4.47331019113899,
102.467420097237));
#208606=CARTESIAN_POINT('Ctrl Pts',(5.19197828878869,-4.34345491177097,
102.475543248574));
#208607=CARTESIAN_POINT('Ctrl Pts',(5.30145648405404,-4.20913860514696,
102.483666399912));
#208608=CARTESIAN_POINT('Ctrl Pts',(5.40564969535407,-4.07077884085079,
102.49178955125));
#208609=CARTESIAN_POINT('Ctrl Pts',(5.5098136275873,-3.93245795667675,102.499910419921));
#208610=CARTESIAN_POINT('Ctrl Pts',(5.60869531444674,-3.79009617075798,
102.508031288593));
#208611=CARTESIAN_POINT('Ctrl Pts',(5.70197400743463,-3.64414344099405,
102.516152157265));
#208612=CARTESIAN_POINT('Ctrl Pts',(5.79525774156021,-3.49818282338581,
102.524273464819));
#208613=CARTESIAN_POINT('Ctrl Pts',(5.88293767629461,-3.34863118066643,
102.532394772373));
#208614=CARTESIAN_POINT('Ctrl Pts',(5.96473677718711,-3.19596686135377,
102.540516079928));
#208615=CARTESIAN_POINT('Ctrl Pts',(6.00724243349643,-3.11663717414944,
102.544736193645));
#208616=CARTESIAN_POINT('Ctrl Pts',(6.04816088332226,-3.0364674381777,102.548956307361));
#208617=CARTESIAN_POINT('Ctrl Pts',(6.08745817512855,-2.95552735836781,
102.553176421078));
#208618=CARTESIAN_POINT('Ctrl Pts',(6.17112039993154,-2.78320944938805,
102.562160859604));
#208619=CARTESIAN_POINT('Ctrl Pts',(6.24739073536623,-2.60748418737219,
102.57114529813));
#208620=CARTESIAN_POINT('Ctrl Pts',(6.3160382512479,-2.42898122857576,102.580129736656));
#208621=CARTESIAN_POINT('Ctrl Pts',(6.3848042486448,-2.25017018432628,102.589129681786));
#208622=CARTESIAN_POINT('Ctrl Pts',(6.44592104434475,-2.06857208417301,
102.598129626917));
#208623=CARTESIAN_POINT('Ctrl Pts',(6.49920723417377,-1.8848327053782,102.607129572047));
#208624=CARTESIAN_POINT('Ctrl Pts',(6.55261899427689,-1.700660340021,102.616150725779));
#208625=CARTESIAN_POINT('Ctrl Pts',(6.59816316017791,-1.51433683027483,
102.625171879511));
#208626=CARTESIAN_POINT('Ctrl Pts',(6.63570860986035,-1.32652185998771,
102.634193033244));
#208627=CARTESIAN_POINT('Ctrl Pts',(6.6732922623338,-1.13851578648779,102.643223366071));
#208628=CARTESIAN_POINT('Ctrl Pts',(6.70286089843514,-0.949015455999851,
102.652253698898));
#208629=CARTESIAN_POINT('Ctrl Pts',(6.72433498941725,-0.758688308924628,
102.661284031725));
#208630=CARTESIAN_POINT('Ctrl Pts',(6.74583952389134,-0.568091337949582,
102.670327166718));
#208631=CARTESIAN_POINT('Ctrl Pts',(6.759226540875,-0.376665444192629,102.679370301711));
#208632=CARTESIAN_POINT('Ctrl Pts',(6.76446843892268,-0.185083059243751,
102.688413436703));
#208633=CARTESIAN_POINT('Ctrl Pts',(6.76905106547896,-0.0175959168006838,
102.696319220103));
#208634=CARTESIAN_POINT('Ctrl Pts',(6.76740934505064,0.150010698279156,
102.704225003503));
#208635=CARTESIAN_POINT('Ctrl Pts',(6.75955746518642,0.317288315010941,
102.712130786903));
#208636=CARTESIAN_POINT('Ctrl Pts',(6.75096307784368,0.500384421526346,
102.720784175131));
#208637=CARTESIAN_POINT('Ctrl Pts',(6.73491958926912,0.683248057353243,
102.72943756336));
#208638=CARTESIAN_POINT('Ctrl Pts',(6.71145332422156,0.865264859332294,
102.738090951588));
#208639=CARTESIAN_POINT('Ctrl Pts',(6.68800873193436,1.04711355588331,102.746736347798));
#208640=CARTESIAN_POINT('Ctrl Pts',(6.65715507527826,1.22811667804449,102.755381744009));
#208641=CARTESIAN_POINT('Ctrl Pts',(6.6189705599523,1.40766392526224,102.764027140219));
#208642=CARTESIAN_POINT('Ctrl Pts',(6.57956655983556,1.59294530673156,102.772948641262));
#208643=CARTESIAN_POINT('Ctrl Pts',(6.53235571106689,1.77667595712159,102.781870142304));
#208644=CARTESIAN_POINT('Ctrl Pts',(6.47748170115115,1.95819299642606,102.790791643346));
#208645=CARTESIAN_POINT('Ctrl Pts',(6.42440722333664,2.13375738638614,102.799420573688));
#208646=CARTESIAN_POINT('Ctrl Pts',(6.36416430221327,2.30725072234848,102.80804950403));
#208647=CARTESIAN_POINT('Ctrl Pts',(6.29693451022695,2.47808490046504,102.816678434372));
#208648=CARTESIAN_POINT('Ctrl Pts',(6.22628549942339,2.65760748024384,102.825746220765));
#208649=CARTESIAN_POINT('Ctrl Pts',(6.14792048194812,2.83419303824045,102.834814007157));
#208650=CARTESIAN_POINT('Ctrl Pts',(6.06210923495723,3.0071781828562,102.84388179355));
#208651=CARTESIAN_POINT('Ctrl Pts',(5.97629798796633,3.18016332747195,102.852949579943));
#208652=CARTESIAN_POINT('Ctrl Pts',(5.88304065346145,3.34954769322734,102.862017366335));
#208653=CARTESIAN_POINT('Ctrl Pts',(5.78266570200121,3.51469292810893,102.871085152728));
#208654=CARTESIAN_POINT('Ctrl Pts',(5.68940649558566,3.66813074625289,102.879510108861));
#208655=CARTESIAN_POINT('Ctrl Pts',(5.59004418751204,3.81784196527256,102.887935064994));
#208656=CARTESIAN_POINT('Ctrl Pts',(5.48491019652612,3.96333813042034,102.896360021127));
#208657=CARTESIAN_POINT('Ctrl Pts',(5.37975180293139,4.10886806662512,102.904786932774));
#208658=CARTESIAN_POINT('Ctrl Pts',(5.26881924955178,4.25018072948424,102.91321384442));
#208659=CARTESIAN_POINT('Ctrl Pts',(5.15248564259967,4.38681897310617,102.921640756067));
#208660=CARTESIAN_POINT('Ctrl Pts',(5.03610925524897,4.52350746393248,102.930070766617));
#208661=CARTESIAN_POINT('Ctrl Pts',(4.91432806894055,4.65551785569813,102.938500777167));
#208662=CARTESIAN_POINT('Ctrl Pts',(4.78755385332686,4.78242795047611,102.946930787717));
#208663=CARTESIAN_POINT('Ctrl Pts',(4.66066285595716,4.90945495217916,102.955368563816));
#208664=CARTESIAN_POINT('Ctrl Pts',(4.52876987445921,5.03137203536056,102.963806339916));
#208665=CARTESIAN_POINT('Ctrl Pts',(4.39232256178812,5.14779482042623,102.972244116015));
#208666=CARTESIAN_POINT('Ctrl Pts',(4.2558036243361,5.26427871887193,102.980686321325));
#208667=CARTESIAN_POINT('Ctrl Pts',(4.11472584479548,5.37526235816219,102.989128526635));
#208668=CARTESIAN_POINT('Ctrl Pts',(3.96956843621229,5.48040285291393,102.997570731945));
#208669=CARTESIAN_POINT('Ctrl Pts',(3.82425789454982,5.58565426510264,103.006021843317));
#208670=CARTESIAN_POINT('Ctrl Pts',(3.6748593994887,5.6850500312575,103.014472954689));
#208671=CARTESIAN_POINT('Ctrl Pts',(3.52188039471258,5.77829105232154,103.022924066061));
#208672=CARTESIAN_POINT('Ctrl Pts',(3.47894660005773,5.80445928931347,103.025295883558));
#208673=CARTESIAN_POINT('Ctrl Pts',(3.43573093221849,5.83014302523311,103.027667701055));
#208674=CARTESIAN_POINT('Ctrl Pts',(3.39224493727712,5.8553363084897,103.030039518553));
#208675=CARTESIAN_POINT('Ctrl Pts',(3.2959276597028,5.91113699695742,103.035292865166));
#208676=CARTESIAN_POINT('Ctrl Pts',(3.19817427377089,5.96459467347469,103.040546211779));
#208677=CARTESIAN_POINT('Ctrl Pts',(3.09910619832139,6.01563211736937,103.045799558392));
#208678=CARTESIAN_POINT('Ctrl Pts',(3.09910619832146,6.01563211736934,101.0456200824));
#208679=CARTESIAN_POINT('Ctrl Pts',(2.94206679343137,6.09653496906972,101.053938109991));
#208680=CARTESIAN_POINT('Ctrl Pts',(2.78197250407096,6.1712253801484,101.062256137582));
#208681=CARTESIAN_POINT('Ctrl Pts',(2.61935543177763,6.23949245708472,101.070574165172));
#208682=CARTESIAN_POINT('Ctrl Pts',(2.44988024168382,6.31063859000771,101.07924299242));
#208683=CARTESIAN_POINT('Ctrl Pts',(2.27766527045293,6.37480769062343,101.087911819667));
#208684=CARTESIAN_POINT('Ctrl Pts',(2.10332965315264,6.43181882286564,101.096580646914));
#208685=CARTESIAN_POINT('Ctrl Pts',(1.92899403585247,6.48882995510782,101.105249474161));
#208686=CARTESIAN_POINT('Ctrl Pts',(1.75253819497853,6.53868306401959,101.113918301409));
#208687=CARTESIAN_POINT('Ctrl Pts',(1.57459222930509,6.58125735034059,101.122587128656));
#208688=CARTESIAN_POINT('Ctrl Pts',(1.40894161719297,6.62088992398518,101.130656974659));
#208689=CARTESIAN_POINT('Ctrl Pts',(1.24148778099825,6.65433737297032,101.138726820661));
#208690=CARTESIAN_POINT('Ctrl Pts',(1.07274313453212,6.68143032346475,101.146796666664));
#208691=CARTESIAN_POINT('Ctrl Pts',(0.904210790295027,6.70848918758131,
101.154856359774));
#208692=CARTESIAN_POINT('Ctrl Pts',(0.734391230787464,6.72920940219974,
101.162916052884));
#208693=CARTESIAN_POINT('Ctrl Pts',(0.5638120491549,6.74347128511924,101.170975745994));
#208694=CARTESIAN_POINT('Ctrl Pts',(0.393410041095697,6.75771835480811,
101.179027067833));
#208695=CARTESIAN_POINT('Ctrl Pts',(0.222250349639107,6.76552041097045,
101.187078389672));
#208696=CARTESIAN_POINT('Ctrl Pts',(0.050870685568204,6.76680878799969,
101.19512971151));
#208697=CARTESIAN_POINT('Ctrl Pts',(-0.120368528625231,6.76809610917206,
101.203174435091));
#208698=CARTESIAN_POINT('Ctrl Pts',(-0.291826985450638,6.7628803729991,
101.211219158672));
#208699=CARTESIAN_POINT('Ctrl Pts',(-0.462962030385573,6.75114472948264,
101.219263882253));
#208700=CARTESIAN_POINT('Ctrl Pts',(-0.633994287449413,6.73941613467917,
101.227303773978));
#208701=CARTESIAN_POINT('Ctrl Pts',(-0.80470314802758,6.72117545356874,
101.235343665702));
#208702=CARTESIAN_POINT('Ctrl Pts',(-0.974546244514403,6.69645791574194,
101.243383557426));
#208703=CARTESIAN_POINT('Ctrl Pts',(-1.14804652818518,6.67120814160746,
101.251596570046));
#208704=CARTESIAN_POINT('Ctrl Pts',(-1.32064294170514,6.63919941457178,
101.259809582666));
#208705=CARTESIAN_POINT('Ctrl Pts',(-1.49176264479612,6.60052522240396,
101.268022595286));
#208706=CARTESIAN_POINT('Ctrl Pts',(-1.65921689410972,6.56267944719345,
101.276059681829));
#208707=CARTESIAN_POINT('Ctrl Pts',(-1.8252566793481,6.5184509665929,101.284096768371));
#208708=CARTESIAN_POINT('Ctrl Pts',(-1.98935582725716,6.46797900371963,
101.292133854914));
#208709=CARTESIAN_POINT('Ctrl Pts',(-2.1534706802192,6.41750221044437,101.300171710643));
#208710=CARTESIAN_POINT('Ctrl Pts',(-2.31564416887222,6.36078085483351,
101.308209566372));
#208711=CARTESIAN_POINT('Ctrl Pts',(-2.47536594874771,6.29800384405888,
101.316247422102));
#208712=CARTESIAN_POINT('Ctrl Pts',(-2.63513466095759,6.23520838701058,
101.324287639659));
#208713=CARTESIAN_POINT('Ctrl Pts',(-2.79244988291351,6.16635386959734,
101.332327857215));
#208714=CARTESIAN_POINT('Ctrl Pts',(-2.9468220355432,6.09167701793497,101.340368074772));
#208715=CARTESIAN_POINT('Ctrl Pts',(-3.1070264670085,6.01417882696987,101.3487120569));
#208716=CARTESIAN_POINT('Ctrl Pts',(-3.26406070273427,5.93040995929566,
101.357056039028));
#208717=CARTESIAN_POINT('Ctrl Pts',(-3.41740739920343,5.84068623261596,
101.365400021156));
#208718=CARTESIAN_POINT('Ctrl Pts',(-3.5654287178849,5.75407840443353,101.373454235991));
#208719=CARTESIAN_POINT('Ctrl Pts',(-3.71001404861886,5.66192263440905,
101.381508450826));
#208720=CARTESIAN_POINT('Ctrl Pts',(-3.85072973210325,5.56454576136238,
101.389562665661));
#208721=CARTESIAN_POINT('Ctrl Pts',(-3.99155071800775,5.46709601782864,
101.397622907744));
#208722=CARTESIAN_POINT('Ctrl Pts',(-4.12849599391133,5.36441761424839,
101.405683149827));
#208723=CARTESIAN_POINT('Ctrl Pts',(-4.26116633430348,5.25687649383154,
101.41374339191));
#208724=CARTESIAN_POINT('Ctrl Pts',(-4.39402215693354,5.14918502355035,
101.421814902764));
#208725=CARTESIAN_POINT('Ctrl Pts',(-4.52259084117014,5.03661751620381,
101.429886413618));
#208726=CARTESIAN_POINT('Ctrl Pts',(-4.64651082041657,4.91957581461571,
101.437957924473));
#208727=CARTESIAN_POINT('Ctrl Pts',(-4.65949892806982,4.90730862227602,
101.438803903084));
#208728=CARTESIAN_POINT('Ctrl Pts',(-4.67243600608959,4.89499230859961,
101.439649881695));
#208729=CARTESIAN_POINT('Ctrl Pts',(-4.68532166475965,4.88262735601786,
101.440495860305));
#208730=CARTESIAN_POINT('Ctrl Pts',(-4.80979550241226,4.76318347350842,
101.448667906994));
#208731=CARTESIAN_POINT('Ctrl Pts',(-4.9298945580079,4.63878884005489,101.456839953683));
#208732=CARTESIAN_POINT('Ctrl Pts',(-5.04519683654342,4.50979798666551,
101.465012000372));
#208733=CARTESIAN_POINT('Ctrl Pts',(-5.16035907248924,4.38096380158648,
101.473174121545));
#208734=CARTESIAN_POINT('Ctrl Pts',(-5.27073588981002,4.24754477950296,
101.481336242717));
#208735=CARTESIAN_POINT('Ctrl Pts',(-5.37593976111861,4.10993438935757,
101.48949836389));
#208736=CARTESIAN_POINT('Ctrl Pts',(-5.4810378177215,3.97246240859534,101.497652275551));
#208737=CARTESIAN_POINT('Ctrl Pts',(-5.58097306863981,3.83080774162944,
101.505806187212));
#208738=CARTESIAN_POINT('Ctrl Pts',(-5.67539614195182,3.68539925000243,
101.513960098873));
#208739=CARTESIAN_POINT('Ctrl Pts',(-5.76973307192783,3.54012341633825,
101.52210657162));
#208740=CARTESIAN_POINT('Ctrl Pts',(-5.85856764704998,3.39110088621093,
101.530253044366));
#208741=CARTESIAN_POINT('Ctrl Pts',(-5.94159206921411,3.23879185546895,
101.538399517113));
#208742=CARTESIAN_POINT('Ctrl Pts',(-6.02457418649144,3.08656043341291,
101.546541838845));
#208743=CARTESIAN_POINT('Ctrl Pts',(-6.10175187064456,2.93104616362484,
101.554684160576));
#208744=CARTESIAN_POINT('Ctrl Pts',(-6.17286161926892,2.7727366318056,101.562826482308));
#208745=CARTESIAN_POINT('Ctrl Pts',(-6.24394856591401,2.61447786335895,
101.570966193131));
#208746=CARTESIAN_POINT('Ctrl Pts',(-6.30897130248828,2.45342594979255,
101.579105903954));
#208747=CARTESIAN_POINT('Ctrl Pts',(-6.36771313026394,2.29009137168458,
101.587245614778));
#208748=CARTESIAN_POINT('Ctrl Pts',(-6.4264472172201,2.12677831731084,101.595384252974));
#208749=CARTESIAN_POINT('Ctrl Pts',(-6.47890192160153,1.96118354067021,
101.603522891171));
#208750=CARTESIAN_POINT('Ctrl Pts',(-6.52490938756892,1.79383569036157,
101.611661529368));
#208751=CARTESIAN_POINT('Ctrl Pts',(-6.5709326468189,1.62643039346608,101.619802961368));
#208752=CARTESIAN_POINT('Ctrl Pts',(-6.61050414693564,1.45727117161119,
101.627944393368));
#208753=CARTESIAN_POINT('Ctrl Pts',(-6.6435063304656,1.2869003990455,101.636085825369));
#208754=CARTESIAN_POINT('Ctrl Pts',(-6.67651474699476,1.11649744918802,
101.644228795011));
#208755=CARTESIAN_POINT('Ctrl Pts',(-6.7029513136287,0.944882852027836,
101.652371764653));
#208756=CARTESIAN_POINT('Ctrl Pts',(-6.72274997655316,0.772607114097821,
101.660514734295));
#208757=CARTESIAN_POINT('Ctrl Pts',(-6.74256349027035,0.600202153740679,
101.668663811903));
#208758=CARTESIAN_POINT('Ctrl Pts',(-6.75572912332282,0.427135425137091,
101.67681288951));
#208759=CARTESIAN_POINT('Ctrl Pts',(-6.76223282506295,0.253961059300643,
101.684961967118));
#208760=CARTESIAN_POINT('Ctrl Pts',(-6.76548313303249,0.167414959265863,
101.689034572682));
#208761=CARTESIAN_POINT('Ctrl Pts',(-6.76707035411167,0.0808419783983983,
101.693107178246));
#208762=CARTESIAN_POINT('Ctrl Pts',(-6.76699760869648,-0.00568892750522595,
101.69717978381));
#208763=CARTESIAN_POINT('',(-6.76727197366057,0.000320845660479878,101.303291156375));
#208764=CARTESIAN_POINT('Ctrl Pts',(3.09910619832147,6.01563211736933,100.651473518761));
#208765=CARTESIAN_POINT('Ctrl Pts',(2.93980871858144,6.09769827387746,100.659895895807));
#208766=CARTESIAN_POINT('Ctrl Pts',(2.77722459638561,6.17344596557304,100.668318272853));
#208767=CARTESIAN_POINT('Ctrl Pts',(2.61188535517925,6.24262315788805,100.6767406499));
#208768=CARTESIAN_POINT('Ctrl Pts',(2.44655248697758,6.31179768376666,100.685162702305));
#208769=CARTESIAN_POINT('Ctrl Pts',(2.27846501917269,6.37440208664836,100.693584754711));
#208770=CARTESIAN_POINT('Ctrl Pts',(2.1081747221875,6.43023237066357,100.702006807116));
#208771=CARTESIAN_POINT('Ctrl Pts',(1.93786721771301,6.48606829621581,100.710429710553));
#208772=CARTESIAN_POINT('Ctrl Pts',(1.76535675730985,6.535128634809,100.71885261399));
#208773=CARTESIAN_POINT('Ctrl Pts',(1.59121089754127,6.57725907042941,100.727275517427));
#208774=CARTESIAN_POINT('Ctrl Pts',(1.41534333340634,6.61980603134109,100.735781694447));
#208775=CARTESIAN_POINT('Ctrl Pts',(1.23780819329335,6.65528523302602,100.744287871466));
#208776=CARTESIAN_POINT('Ctrl Pts',(1.05920117056735,6.68359049316075,100.752794048485));
#208777=CARTESIAN_POINT('Ctrl Pts',(0.882174701826115,6.71164527047004,
100.761224951466));
#208778=CARTESIAN_POINT('Ctrl Pts',(0.704095583496147,6.73265256018185,
100.769655854446));
#208779=CARTESIAN_POINT('Ctrl Pts',(0.525549680055566,6.74656108945836,
100.778086757427));
#208780=CARTESIAN_POINT('Ctrl Pts',(0.3446125965744,6.76065588902703,100.786630571466));
#208781=CARTESIAN_POINT('Ctrl Pts',(0.163196488995154,6.76746039834387,
100.795174385505));
#208782=CARTESIAN_POINT('Ctrl Pts',(-0.0180881004267439,6.76697582533165,
100.803718199544));
#208783=CARTESIAN_POINT('Ctrl Pts',(-0.199372689848642,6.76649125231943,
100.812262013583));
#208784=CARTESIAN_POINT('Ctrl Pts',(-0.380525408145483,6.75871763816219,
100.820805827621));
#208785=CARTESIAN_POINT('Ctrl Pts',(-0.560940188314447,6.74371078154556,
100.82934964166));
#208786=CARTESIAN_POINT('Ctrl Pts',(-0.732821843464126,6.72941370814921,
100.837489356693));
#208787=CARTESIAN_POINT('Ctrl Pts',(-0.904376410743714,6.70852274586707,
100.845629071726));
#208788=CARTESIAN_POINT('Ctrl Pts',(-1.07505406080753,6.68105888062224,
100.853768786759));
#208789=CARTESIAN_POINT('Ctrl Pts',(-1.24558243722208,6.65361903510926,
100.861901382846));
#208790=CARTESIAN_POINT('Ctrl Pts',(-1.41523506394114,6.61961778700909,
100.870033978933));
#208791=CARTESIAN_POINT('Ctrl Pts',(-1.58346559710706,6.57912803514101,
100.87816657502));
#208792=CARTESIAN_POINT('Ctrl Pts',(-1.75158111885478,6.53866596423962,
100.886293611228));
#208793=CARTESIAN_POINT('Ctrl Pts',(-1.91827612810709,6.49172430653978,
100.894420647436));
#208794=CARTESIAN_POINT('Ctrl Pts',(-2.0830129060397,6.43842731055279,100.902547683644));
#208795=CARTESIAN_POINT('Ctrl Pts',(-2.24767093681206,6.38515579149413,
100.910670834981));
#208796=CARTESIAN_POINT('Ctrl Pts',(-2.41037225260023,6.32553509622326,
100.918793986319));
#208797=CARTESIAN_POINT('Ctrl Pts',(-2.5705927930854,6.25973974635826,100.926917137656));
#208798=CARTESIAN_POINT('Ctrl Pts',(-2.73076831040713,6.19396288547591,
100.935038006328));
#208799=CARTESIAN_POINT('Ctrl Pts',(-2.88846410278187,6.1220149657471,100.943158875));
#208800=CARTESIAN_POINT('Ctrl Pts',(-3.04317468101102,6.04411919644653,
100.951279743671));
#208801=CARTESIAN_POINT('Ctrl Pts',(-3.19789362039328,5.96621921735979,
100.959401051226));
#208802=CARTESIAN_POINT('Ctrl Pts',(-3.34962669442722,5.88237090765951,
100.96752235878));
#208803=CARTESIAN_POINT('Ctrl Pts',(-3.49789151317762,5.79284420315616,
100.975643666335));
#208804=CARTESIAN_POINT('Ctrl Pts',(-3.57493506695422,5.74632301538568,
100.979863780052));
#208805=CARTESIAN_POINT('Ctrl Pts',(-3.65104253294218,5.69826929833173,
100.984083893768));
#208806=CARTESIAN_POINT('Ctrl Pts',(-3.72614913619489,5.64872566291142,
100.988304007485));
#208807=CARTESIAN_POINT('Ctrl Pts',(-3.88604782734473,5.54324941827475,
100.997288446011));
#208808=CARTESIAN_POINT('Ctrl Pts',(-4.04132928615683,5.43107009608483,
101.006272884537));
#208809=CARTESIAN_POINT('Ctrl Pts',(-4.19147353707513,5.31261127770505,
101.015257323062));
#208810=CARTESIAN_POINT('Ctrl Pts',(-4.34187692800926,5.19394800647488,
101.024257268193));
#208811=CARTESIAN_POINT('Ctrl Pts',(-4.48712520165042,5.06898372477758,
101.033257213323));
#208812=CARTESIAN_POINT('Ctrl Pts',(-4.62673274228182,4.93818115620492,
101.042257158454));
#208813=CARTESIAN_POINT('Ctrl Pts',(-4.76666927166609,4.80707034802204,
101.051278312186));
#208814=CARTESIAN_POINT('Ctrl Pts',(-4.90093829675574,4.67009388933978,
101.060299465918));
#208815=CARTESIAN_POINT('Ctrl Pts',(-5.02909034220098,4.52775212770982,
101.06932061965));
#208816=CARTESIAN_POINT('Ctrl Pts',(-5.15737278336259,4.38526553221544,
101.078350952477));
#208817=CARTESIAN_POINT('Ctrl Pts',(-5.2795256554229,4.23740290900318,101.087381285305));
#208818=CARTESIAN_POINT('Ctrl Pts',(-5.39513988999777,4.08469761027116,
101.096411618132));
#208819=CARTESIAN_POINT('Ctrl Pts',(-5.51091802911308,3.93177582356165,
101.105454753124));
#208820=CARTESIAN_POINT('Ctrl Pts',(-5.62013885138369,3.77399782444096,
101.114497888117));
#208821=CARTESIAN_POINT('Ctrl Pts',(-5.72243539414993,3.61192776225939,
101.12354102311));
#208822=CARTESIAN_POINT('Ctrl Pts',(-5.81186614027298,3.47024118915372,
101.13144680651));
#208823=CARTESIAN_POINT('Ctrl Pts',(-5.89600542329012,3.32527480091662,
101.13935258991));
#208824=CARTESIAN_POINT('Ctrl Pts',(-5.97463653142679,3.17742148877678,
101.14725837331));
#208825=CARTESIAN_POINT('Ctrl Pts',(-6.06076738254096,3.01546610093565,
101.155918201069));
#208826=CARTESIAN_POINT('Ctrl Pts',(-6.14036378958474,2.84990385863868,
101.164578028828));
#208827=CARTESIAN_POINT('Ctrl Pts',(-6.21313452694192,2.68127737284343,
101.173237856587));
#208828=CARTESIAN_POINT('Ctrl Pts',(-6.28583775382177,2.51280732430525,
101.181889650497));
#208829=CARTESIAN_POINT('Ctrl Pts',(-6.35172782142323,2.34127897961005,
101.190541444407));
#208830=CARTESIAN_POINT('Ctrl Pts',(-6.41056020199429,2.16725792110838,
101.199193238317));
#208831=CARTESIAN_POINT('Ctrl Pts',(-6.46932382959776,1.99344022789768,
101.207834921528));
#208832=CARTESIAN_POINT('Ctrl Pts',(-6.52104613445438,1.81713592098677,
101.216476604739));
#208833=CARTESIAN_POINT('Ctrl Pts',(-6.56553126704991,1.63892897386985,
101.22511828795));
#208834=CARTESIAN_POINT('Ctrl Pts',(-6.6099838820073,1.46085229205017,101.233753654284));
#208835=CARTESIAN_POINT('Ctrl Pts',(-6.64720980163098,1.28087603669714,
101.242389020617));
#208836=CARTESIAN_POINT('Ctrl Pts',(-6.67706304938711,1.099599033516,101.251024386951));
#208837=CARTESIAN_POINT('Ctrl Pts',(-6.70690686575957,0.918379300250059,
101.259657025157));
#208838=CARTESIAN_POINT('Ctrl Pts',(-6.72938259100124,0.735859934554445,
101.268289663364));
#208839=CARTESIAN_POINT('Ctrl Pts',(-6.7443951469935,0.552650975942862,
101.27692230157));
#208840=CARTESIAN_POINT('Ctrl Pts',(-6.75940770298576,0.369442017331279,
101.285554939777));
#208841=CARTESIAN_POINT('Ctrl Pts',(-6.76695703681141,0.185543765753519,
101.294187577983));
#208842=CARTESIAN_POINT('Ctrl Pts',(-6.76699981703943,0.00157359091162204,
101.30282021619));
#208843=CARTESIAN_POINT('Ctrl Pts',(-6.767,4.55020098182511E-12,101.30282021619));
#208844=CARTESIAN_POINT('Ctrl Pts',(-6.76700000000013,-0.186007249522411,
101.311569728001));
#208845=CARTESIAN_POINT('Ctrl Pts',(-6.75932637294545,-0.372014355745552,
101.320319239812));
#208846=CARTESIAN_POINT('Ctrl Pts',(-6.74400518264216,-0.557389537483226,
101.329068751624));
#208847=CARTESIAN_POINT('Ctrl Pts',(-6.7286840570513,-0.742763936247827,
101.337818226479));
#208848=CARTESIAN_POINT('Ctrl Pts',(-6.70571545645776,-0.927506130238602,
101.346567701335));
#208849=CARTESIAN_POINT('Ctrl Pts',(-6.67517739404857,-1.11098863989824,
101.355317176191));
#208850=CARTESIAN_POINT('Ctrl Pts',(-6.64463945808735,-1.29447038981776,
101.364066614818));
#208851=CARTESIAN_POINT('Ctrl Pts',(-6.60653217008389,-1.47669218313533,
101.372816053445));
#208852=CARTESIAN_POINT('Ctrl Pts',(-6.5609849609271,-1.65703510599156,
101.381565492072));
#208853=CARTESIAN_POINT('Ctrl Pts',(-6.51543793658328,-1.83737729708591,
101.390314895197));
#208854=CARTESIAN_POINT('Ctrl Pts',(-6.46245112167449,-2.01584035510838,
101.399064298322));
#208855=CARTESIAN_POINT('Ctrl Pts',(-6.40220448374277,-2.19181813760723,
101.407813701447));
#208856=CARTESIAN_POINT('Ctrl Pts',(-6.34195808526531,-2.36779522067069,
101.416563069797));
#208857=CARTESIAN_POINT('Ctrl Pts',(-6.27445201433136,-2.54128677684086,
101.425312438147));
#208858=CARTESIAN_POINT('Ctrl Pts',(-6.19991555071939,-2.71170355384726,
101.434061806498));
#208859=CARTESIAN_POINT('Ctrl Pts',(-6.12537937716729,-2.88211966767401,
101.442811140799));
#208860=CARTESIAN_POINT('Ctrl Pts',(-6.04381298052555,-3.04946076371717,
101.451560475101));
#208861=CARTESIAN_POINT('Ctrl Pts',(-5.95549339335864,-3.21315848374487,
101.460309809403));
#208862=CARTESIAN_POINT('Ctrl Pts',(-5.86717414255447,-3.37685558033427,
101.469059110383));
#208863=CARTESIAN_POINT('Ctrl Pts',(-5.77210188876641,-3.53690907646685,
101.477808411363));
#208864=CARTESIAN_POINT('Ctrl Pts',(-5.67059953347045,-3.69277536969211,
101.486557712343));
#208865=CARTESIAN_POINT('Ctrl Pts',(-5.5690975563143,-3.84864108224857,
101.495306980729));
#208866=CARTESIAN_POINT('Ctrl Pts',(-5.46116568196893,-4.00031938297459,
101.504056249114));
#208867=CARTESIAN_POINT('Ctrl Pts',(-5.34717048533642,-4.14729511859804,
101.512805517499));
#208868=CARTESIAN_POINT('Ctrl Pts',(-5.23317570391899,-4.29427031887839,
101.521554754016));
#208869=CARTESIAN_POINT('Ctrl Pts',(-5.11311782003602,-4.43654276189444,
101.530303990533));
#208870=CARTESIAN_POINT('Ctrl Pts',(-4.98740458984869,-4.57362924351726,
101.53905322705));
#208871=CARTESIAN_POINT('Ctrl Pts',(-4.86169180711877,-4.71071523720127,
101.547802432426));
#208872=CARTESIAN_POINT('Ctrl Pts',(-4.73032391204326,-4.84261509523086,
101.556551637801));
#208873=CARTESIAN_POINT('Ctrl Pts',(-4.59374707013774,-4.96888084538168,
101.565300843177));
#208874=CARTESIAN_POINT('Ctrl Pts',(-4.45717070301659,-5.09514615659275,
101.574050018137));
#208875=CARTESIAN_POINT('Ctrl Pts',(-4.31538563571296,-5.21577720459315,
101.582799193097));
#208876=CARTESIAN_POINT('Ctrl Pts',(-4.16887341029808,-5.33036429232653,
101.591548368058));
#208877=CARTESIAN_POINT('Ctrl Pts',(-4.02236168204015,-5.44495099123387,
101.60029751333));
#208878=CARTESIAN_POINT('Ctrl Pts',(-3.87112305348485,-5.55349359438379,
101.609046658602));
#208879=CARTESIAN_POINT('Ctrl Pts',(-3.7156711701809,-5.65562346298677,
101.617795803874));
#208880=CARTESIAN_POINT('Ctrl Pts',(-3.56021980146167,-5.75775299351429,
101.626544920184));
#208881=CARTESIAN_POINT('Ctrl Pts',(-3.40055544538715,-5.8534696746366,
101.635294036494));
#208882=CARTESIAN_POINT('Ctrl Pts',(-3.23722035987238,-5.94244842986691,
101.644043152804));
#208883=CARTESIAN_POINT('Ctrl Pts',(-3.07388580147568,-6.03142689794332,
101.652792240879));
#208884=CARTESIAN_POINT('Ctrl Pts',(-2.90688078896968,-6.11366734656596,
101.661541328954));
#208885=CARTESIAN_POINT('Ctrl Pts',(-2.73677250721761,-6.18889046952181,
101.670290417029));
#208886=CARTESIAN_POINT('Ctrl Pts',(-2.5666647603187,-6.26411335596168,
101.679039477595));
#208887=CARTESIAN_POINT('Ctrl Pts',(-2.39345402575551,-6.33231884500411,
101.687788538161));
#208888=CARTESIAN_POINT('Ctrl Pts',(-2.21772856065972,-6.39327529762595,
101.696537598727));
#208889=CARTESIAN_POINT('Ctrl Pts',(-2.04200363348908,-6.45423156364986,
101.705286632511));
#208890=CARTESIAN_POINT('Ctrl Pts',(-1.86376426189688,-6.50793874375541,
101.714035666294));
#208891=CARTESIAN_POINT('Ctrl Pts',(-1.68361577753577,-6.55421443909433,
101.722784700078));
#208892=CARTESIAN_POINT('Ctrl Pts',(-1.50346782968266,-6.60048999661761,
101.731533707806));
#208893=CARTESIAN_POINT('Ctrl Pts',(-1.32141105795497,-6.6393340423761,
101.740282715534));
#208894=CARTESIAN_POINT('Ctrl Pts',(-1.13806375487577,-6.67061465607466,
101.749031723262));
#208895=CARTESIAN_POINT('Ctrl Pts',(-0.954716982608748,-6.70189517921214,
101.75778070566));
#208896=CARTESIAN_POINT('Ctrl Pts',(-0.770079968908055,-6.7256122659216,
101.766529688058));
#208897=CARTESIAN_POINT('Ctrl Pts',(-0.58477976556434,-6.74168536983049,
101.775278670457));
#208898=CARTESIAN_POINT('Ctrl Pts',(-0.391489830657309,-6.75845151013819,
101.784404889467));
#208899=CARTESIAN_POINT('Ctrl Pts',(-0.197478578244254,-6.76689983031608,
101.793531108477));
#208900=CARTESIAN_POINT('Ctrl Pts',(-0.00346287645716383,-6.76699911397117,
101.802657327486));
#208901=CARTESIAN_POINT('Ctrl Pts',(0.184489834649052,-6.76709529501204,
101.811498352152));
#208902=CARTESIAN_POINT('Ctrl Pts',(0.37244640424463,-6.75935639738194,
101.820339376818));
#208903=CARTESIAN_POINT('Ctrl Pts',(0.559755019483695,-6.74380925873225,
101.829180401484));
#208904=CARTESIAN_POINT('Ctrl Pts',(0.745134705517098,-6.72842222659857,
101.837930380094));
#208905=CARTESIAN_POINT('Ctrl Pts',(0.92987943122386,-6.70538706057589,
101.846680358703));
#208906=CARTESIAN_POINT('Ctrl Pts',(1.11336163626352,-6.67478200894206,
101.855430337313));
#208907=CARTESIAN_POINT('Ctrl Pts',(1.29684196300264,-6.64417727061102,
101.86418022635));
#208908=CARTESIAN_POINT('Ctrl Pts',(1.47905951217074,-6.60600284890688,
101.872930115386));
#208909=CARTESIAN_POINT('Ctrl Pts',(1.65939532066667,-6.56038841607336,
101.881680004423));
#208910=CARTESIAN_POINT('Ctrl Pts',(1.83972934300399,-6.51477443503371,
101.890429806795));
#208911=CARTESIAN_POINT('Ctrl Pts',(2.01818138405877,-6.46172066062263,
101.899179609167));
#208912=CARTESIAN_POINT('Ctrl Pts',(2.19414528353827,-6.40140730423606,
101.907929411539));
#208913=CARTESIAN_POINT('Ctrl Pts',(2.37010749863629,-6.34109452518781,
101.916679130155));
#208914=CARTESIAN_POINT('Ctrl Pts',(2.54358134866092,-6.27352239616653,
101.925428848772));
#208915=CARTESIAN_POINT('Ctrl Pts',(2.71397759435191,-6.19892043966979,
101.934178567388));
#208916=CARTESIAN_POINT('Ctrl Pts',(2.88437226557757,-6.12431917249688,
101.942928205157));
#208917=CARTESIAN_POINT('Ctrl Pts',(3.05168912680587,-6.04268832278984,
101.951677842925));
#208918=CARTESIAN_POINT('Ctrl Pts',(3.21535986273485,-5.95430516123533,
101.960427480694));
#208919=CARTESIAN_POINT('Ctrl Pts',(3.37902914072483,-5.86592278697647,
101.969177040523));
#208920=CARTESIAN_POINT('Ctrl Pts',(3.53905210621224,-5.77078835742155,
101.977926600352));
#208921=CARTESIAN_POINT('Ctrl Pts',(3.6948852283136,-5.66922500431849,101.986676160181));
#208922=CARTESIAN_POINT('Ctrl Pts',(3.85071701406623,-5.56766252217313,
101.995425644979));
#208923=CARTESIAN_POINT('Ctrl Pts',(4.00235878822108,-5.45967138329587,
102.004175129776));
#208924=CARTESIAN_POINT('Ctrl Pts',(4.14929549611049,-5.34561838199821,
102.012924614573));
#208925=CARTESIAN_POINT('Ctrl Pts',(4.29623099275825,-5.23156632087233,
102.021674027245));
#208926=CARTESIAN_POINT('Ctrl Pts',(4.43846127435774,-5.11145267305185,
102.030423439918));
#208927=CARTESIAN_POINT('Ctrl Pts',(4.57550326054199,-4.98568540050108,
102.039172852591));
#208928=CARTESIAN_POINT('Ctrl Pts',(4.7125441625754,-4.85991912290594,102.047922196046));
#208929=CARTESIAN_POINT('Ctrl Pts',(4.84439664018524,-4.72849950385662,
102.056671539501));
#208930=CARTESIAN_POINT('Ctrl Pts',(4.97061286794511,-4.59187289861321,
102.065420882956));
#208931=CARTESIAN_POINT('Ctrl Pts',(5.09682813912451,-4.45524732884951,
102.074170160101));
#208932=CARTESIAN_POINT('Ctrl Pts',(5.21740705147607,-4.31341506236068,
102.082919437246));
#208933=CARTESIAN_POINT('Ctrl Pts',(5.33194007545466,-4.16685781276018,
102.091668714391));
#208934=CARTESIAN_POINT('Ctrl Pts',(5.44647226944258,-4.02030162522149,
102.100417928132));
#208935=CARTESIAN_POINT('Ctrl Pts',(5.55495848627889,-3.86902074888255,
102.109167141873));
#208936=CARTESIAN_POINT('Ctrl Pts',(5.65703027291568,-3.71352898080998,
102.117916355614));
#208937=CARTESIAN_POINT('Ctrl Pts',(5.75910135376778,-3.55803828789943,
102.126665508858));
#208938=CARTESIAN_POINT('Ctrl Pts',(5.85475793592535,-3.39833700107086,
102.135414662102));
#208939=CARTESIAN_POINT('Ctrl Pts',(5.94367514427184,-3.23496750823947,
102.144163815346));
#208940=CARTESIAN_POINT('Ctrl Pts',(6.03259176732435,-3.07159909078128,
102.152912910999));
#208941=CARTESIAN_POINT('Ctrl Pts',(6.11476896835729,-2.90456276731846,
102.161662006652));
#208942=CARTESIAN_POINT('Ctrl Pts',(6.18992765547701,-2.7344258300347,102.170411102305));
#208943=CARTESIAN_POINT('Ctrl Pts',(6.26508587282888,-2.56428995616577,
102.179160143273));
#208944=CARTESIAN_POINT('Ctrl Pts',(6.33322554827012,-2.39105376935595,
102.187909184241));
#208945=CARTESIAN_POINT('Ctrl Pts',(6.39411526732899,-2.21530561054458,
102.196658225209));
#208946=CARTESIAN_POINT('Ctrl Pts',(6.45500462602724,-2.03955849185489,
102.205407214398));
#208947=CARTESIAN_POINT('Ctrl Pts',(6.50864402040625,-1.86129970164947,
102.214156203587));
#208948=CARTESIAN_POINT('Ctrl Pts',(6.55485128368495,-1.68113463136473,
102.222905192776));
#208949=CARTESIAN_POINT('Ctrl Pts',(6.6019980955423,-1.49730620117296,102.231832078247));
#208950=CARTESIAN_POINT('Ctrl Pts',(6.64140720707787,-1.31149343246137,
102.240758963719));
#208951=CARTESIAN_POINT('Ctrl Pts',(6.67293928722808,-1.12435326697976,
102.24968584919));
#208952=CARTESIAN_POINT('Ctrl Pts',(6.70384625876193,-0.940923067011138,
102.258435763367));
#208953=CARTESIAN_POINT('Ctrl Pts',(6.72718554579744,-0.756217899526259,
102.267185677545));
#208954=CARTESIAN_POINT('Ctrl Pts',(6.74287786815289,-0.570865181259129,
102.275935591722));
#208955=CARTESIAN_POINT('Ctrl Pts',(6.75856988190819,-0.385516108078663,
102.284685333827));
#208956=CARTESIAN_POINT('Ctrl Pts',(6.76661520773389,-0.199519795231143,
102.293435075931));
#208957=CARTESIAN_POINT('Ctrl Pts',(6.76698651789578,-0.0135080204605165,
102.302184818036));
#208958=CARTESIAN_POINT('Ctrl Pts',(6.76735782124915,0.172500343508018,
102.310934399701));
#208959=CARTESIAN_POINT('Ctrl Pts',(6.7600553899521,0.358523882205911,102.319683981366));
#208960=CARTESIAN_POINT('Ctrl Pts',(6.74510402742402,0.543930748559304,
102.328433563031));
#208961=CARTESIAN_POINT('Ctrl Pts',(6.73015291918085,0.729334461610168,
102.337182995887));
#208962=CARTESIAN_POINT('Ctrl Pts',(6.70755316306664,0.914121237629624,
102.345932428744));
#208963=CARTESIAN_POINT('Ctrl Pts',(6.67738151874657,1.09766345165618,102.354681861601));
#208964=CARTESIAN_POINT('Ctrl Pts',(6.64721034747666,1.28120278799162,102.363431157278));
#208965=CARTESIAN_POINT('Ctrl Pts',(6.60946757205252,1.4634973185983,102.372180452956));
#208966=CARTESIAN_POINT('Ctrl Pts',(6.56428138111647,1.64392790277666,102.380929748633));
#208967=CARTESIAN_POINT('Ctrl Pts',(6.51909583859992,1.82435589778547,102.389678918759));
#208968=CARTESIAN_POINT('Ctrl Pts',(6.46646716393037,2.00291972191743,102.398428088885));
#208969=CARTESIAN_POINT('Ctrl Pts',(6.40657409873065,2.17901292274131,102.40717725901));
#208970=CARTESIAN_POINT('Ctrl Pts',(6.34668181342273,2.35510383058447,102.415926315209));
#208971=CARTESIAN_POINT('Ctrl Pts',(6.27952541914262,2.52872390822053,102.424675371408));
#208972=CARTESIAN_POINT('Ctrl Pts',(6.20533299175744,2.69928350889762,102.433424427607));
#208973=CARTESIAN_POINT('Ctrl Pts',(6.12831602991782,2.87633637965127,102.442506563766));
#208974=CARTESIAN_POINT('Ctrl Pts',(6.04371690605507,3.05009086600993,102.451588699924));
#208975=CARTESIAN_POINT('Ctrl Pts',(5.9518452031687,3.21991112882293,102.460670836082));
#208976=CARTESIAN_POINT('Ctrl Pts',(5.86333549509518,3.38351691182596,102.469420616426));
#208977=CARTESIAN_POINT('Ctrl Pts',(5.76807618099615,3.54347103711603,102.478170396769));
#208978=CARTESIAN_POINT('Ctrl Pts',(5.66639083309265,3.69923018027314,102.486920177113));
#208979=CARTESIAN_POINT('Ctrl Pts',(5.56470914082457,3.8549837238168,102.495669642898));
#208980=CARTESIAN_POINT('Ctrl Pts',(5.4566020337233,4.0065423470164,102.504419108683));
#208981=CARTESIAN_POINT('Ctrl Pts',(5.34243669839485,4.15339127986323,102.513168574468));
#208982=CARTESIAN_POINT('Ctrl Pts',(5.22827486050865,4.30023571400948,102.521917772214));
#208983=CARTESIAN_POINT('Ctrl Pts',(5.10805534167387,4.44237052028152,102.53066696996));
#208984=CARTESIAN_POINT('Ctrl Pts',(4.9821864434023,4.57931296628418,102.539416167706));
#208985=CARTESIAN_POINT('Ctrl Pts',(4.85632073219889,4.71625194483049,102.548165143917));
#208986=CARTESIAN_POINT('Ctrl Pts',(4.72480612170645,4.84799861524189,102.556914120129));
#208987=CARTESIAN_POINT('Ctrl Pts',(4.58808925235663,4.9741055489816,102.56566309634));
#208988=CARTESIAN_POINT('Ctrl Pts',(4.45136349474412,5.10022068120889,102.574412641342));
#208989=CARTESIAN_POINT('Ctrl Pts',(4.30943501210456,5.22069514871523,102.583162186344));
#208990=CARTESIAN_POINT('Ctrl Pts',(4.1627858743217,5.33511975165954,102.591911731346));
#208991=CARTESIAN_POINT('Ctrl Pts',(4.01614535740839,5.44953762807554,102.600660761999));
#208992=CARTESIAN_POINT('Ctrl Pts',(3.86478496658317,5.5579061753251,102.609409792653));
#208993=CARTESIAN_POINT('Ctrl Pts',(3.70921874747592,5.65985735539096,102.618158823307));
#208994=CARTESIAN_POINT('Ctrl Pts',(3.55365041606298,5.76180991976801,102.626907972756));
#208995=CARTESIAN_POINT('Ctrl Pts',(3.3938763817492,5.85734478552583,102.635657122206));
#208996=CARTESIAN_POINT('Ctrl Pts',(3.23043927904936,5.94613749121016,102.644406271656));
#208997=CARTESIAN_POINT('Ctrl Pts',(3.186917670707,5.96978206944005,102.646736079572));
#208998=CARTESIAN_POINT('Ctrl Pts',(3.14313645919771,5.99294880633353,102.649065887488));
#208999=CARTESIAN_POINT('Ctrl Pts',(3.09910619832148,6.01563211736933,102.651395695404));
#209000=CARTESIAN_POINT('Origin',(0.,0.,4.30282021618968));
#209001=CARTESIAN_POINT('',(3.09910619832126,6.01563211736944,105.045908754666));
#209002=CARTESIAN_POINT('',(3.09910619832133,6.0156321173694,104.651395695404));
#209003=CARTESIAN_POINT('',(3.09910619832133,6.0156321173694,4.30282021618968));
#209004=CARTESIAN_POINT('',(-6.76699971567252,0.00196165442175408,103.697179783839));
#209005=CARTESIAN_POINT('Ctrl Pts',(-6.76699971567252,0.0019616544219389,
103.697179783839));
#209006=CARTESIAN_POINT('Ctrl Pts',(-6.76704929032538,-0.169053004476753,
103.705273455863));
#209007=CARTESIAN_POINT('Ctrl Pts',(-6.76061186475369,-0.340348538486266,
103.713367127887));
#209008=CARTESIAN_POINT('Ctrl Pts',(-6.74764967260861,-0.511383315864874,
103.72146079991));
#209009=CARTESIAN_POINT('Ctrl Pts',(-6.734702167456,-0.682224299905047,
103.729545301286));
#209010=CARTESIAN_POINT('Ctrl Pts',(-6.71524463675656,-0.852804748767579,
103.737629802663));
#209011=CARTESIAN_POINT('Ctrl Pts',(-6.68929126238576,-1.02258075816513,
103.745714304039));
#209012=CARTESIAN_POINT('Ctrl Pts',(-6.6633616594919,-1.19220126460439,
103.753791400576));
#209013=CARTESIAN_POINT('Ctrl Pts',(-6.63094811150644,-1.36101843350394,
103.761868497114));
#209014=CARTESIAN_POINT('Ctrl Pts',(-6.59211675840777,-1.52849129651413,
103.769945593652));
#209015=CARTESIAN_POINT('Ctrl Pts',(-6.55331254905335,-1.69584709328275,
103.778017044169));
#209016=CARTESIAN_POINT('Ctrl Pts',(-6.50809954936712,-1.86186009455973,
103.786088494685));
#209017=CARTESIAN_POINT('Ctrl Pts',(-6.45659533533666,-2.02599745204897,
103.794159945202));
#209018=CARTESIAN_POINT('Ctrl Pts',(-6.40511251921879,-2.19006661712142,
103.802228042358));
#209019=CARTESIAN_POINT('Ctrl Pts',(-6.347343800751,-2.35226133528762,103.810296139515));
#209020=CARTESIAN_POINT('Ctrl Pts',(-6.28345717847996,-2.51206187945453,
103.818364236671));
#209021=CARTESIAN_POINT('Ctrl Pts',(-6.21958362568529,-2.67182973274875,
103.826430683312));
#209022=CARTESIAN_POINT('Ctrl Pts',(-6.1495947971142,-2.82920404177331,
103.834497129954));
#209023=CARTESIAN_POINT('Ctrl Pts',(-6.07370756813553,-2.98368318974605,
103.842563576596));
#209024=CARTESIAN_POINT('Ctrl Pts',(-5.99782097043651,-3.13816105266013,
103.850629956135));
#209025=CARTESIAN_POINT('Ctrl Pts',(-5.91603623378747,-3.28974346894448,
103.858696335675));
#209026=CARTESIAN_POINT('Ctrl Pts',(-5.82861704916746,-3.43795175855543,
103.866762715214));
#209027=CARTESIAN_POINT('Ctrl Pts',(-5.74118143383553,-3.58618790438264,
103.874830610856));
#209028=CARTESIAN_POINT('Ctrl Pts',(-5.64810945175457,-3.73104834150695,
103.882898506497));
#209029=CARTESIAN_POINT('Ctrl Pts',(-5.54970906004895,-3.87208191401094,
103.890966402138));
#209030=CARTESIAN_POINT('Ctrl Pts',(-5.45121910266651,-4.01324385762359,
103.899041641312));
#209031=CARTESIAN_POINT('Ctrl Pts',(-5.34739126114274,-4.15057167410523,
103.907116880486));
#209032=CARTESIAN_POINT('Ctrl Pts',(-5.23857531030885,-4.28364537727186,
103.915192119661));
#209033=CARTESIAN_POINT('Ctrl Pts',(-5.12970795282688,-4.41678194689304,
103.923271173726));
#209034=CARTESIAN_POINT('Ctrl Pts',(-5.01584803700327,-4.5456601212334,
103.931350227791));
#209035=CARTESIAN_POINT('Ctrl Pts',(-4.89738310684792,-4.66989589870702,
103.939429281856));
#209036=CARTESIAN_POINT('Ctrl Pts',(-4.77875699930115,-4.794300705095,103.947519327873));
#209037=CARTESIAN_POINT('Ctrl Pts',(-4.65551362731212,-4.91405023814169,
103.955609373891));
#209038=CARTESIAN_POINT('Ctrl Pts',(-4.52807532787225,-5.02879934229978,
103.963699419908));
#209039=CARTESIAN_POINT('Ctrl Pts',(-4.42271068898769,-5.12367268865706,
103.970388184439));
#209040=CARTESIAN_POINT('Ctrl Pts',(-4.31447916453073,-5.21512852071409,
103.97707694897));
#209041=CARTESIAN_POINT('Ctrl Pts',(-4.20363434417333,-5.30299418258086,
103.983765713501));
#209042=CARTESIAN_POINT('Ctrl Pts',(-4.05554974021816,-5.4203794757939,
103.992701656952));
#209043=CARTESIAN_POINT('Ctrl Pts',(-3.9024511963491,-5.53163332063073,
104.001637600403));
#209044=CARTESIAN_POINT('Ctrl Pts',(-3.74484820815153,-5.63634641393734,
104.010573543853));
#209045=CARTESIAN_POINT('Ctrl Pts',(-3.58748213904692,-5.74090209569122,
104.019496054211));
#209046=CARTESIAN_POINT('Ctrl Pts',(-3.42562535140029,-5.83893650253526,
104.028418564569));
#209047=CARTESIAN_POINT('Ctrl Pts',(-3.25981822702301,-5.93008213490914,
104.037341074926));
#209048=CARTESIAN_POINT('Ctrl Pts',(-3.09441738155513,-6.02100443219862,
104.046241722365));
#209049=CARTESIAN_POINT('Ctrl Pts',(-2.92508574388218,-6.10507151961483,
104.055142369803));
#209050=CARTESIAN_POINT('Ctrl Pts',(-2.75238975770195,-6.18196082337129,
104.064043017241));
#209051=CARTESIAN_POINT('Ctrl Pts',(-2.57996065185501,-6.25873130419812,
104.072929909828));
#209052=CARTESIAN_POINT('Ctrl Pts',(-2.40417780321668,-6.32834602325587,
104.081816802414));
#209053=CARTESIAN_POINT('Ctrl Pts',(-2.22563183148763,-6.39052829980973,
104.090703695));
#209054=CARTESIAN_POINT('Ctrl Pts',(-2.04754478955433,-6.45255074470118,
104.099567744955));
#209055=CARTESIAN_POINT('Ctrl Pts',(-1.86670903970273,-6.50717878343272,
104.10843179491));
#209056=CARTESIAN_POINT('Ctrl Pts',(-1.68373400925483,-6.55418406714968,
104.117295844865));
#209057=CARTESIAN_POINT('Ctrl Pts',(-1.50879516082221,-6.59912489969697,
104.125770589685));
#209058=CARTESIAN_POINT('Ctrl Pts',(-1.33190114540597,-6.63709805455192,
104.134245334506));
#209059=CARTESIAN_POINT('Ctrl Pts',(-1.15360166401145,-6.66794512580825,
104.142720079326));
#209060=CARTESIAN_POINT('Ctrl Pts',(-0.980894967051109,-6.69782460580401,
104.150928993755));
#209061=CARTESIAN_POINT('Ctrl Pts',(-0.807035907377264,-6.72098828375315,
104.159137908184));
#209062=CARTESIAN_POINT('Ctrl Pts',(-0.632584836163848,-6.7373678410085,
104.167346822613));
#209063=CARTESIAN_POINT('Ctrl Pts',(-0.45809229009454,-6.75375129242037,
104.17555768867));
#209064=CARTESIAN_POINT('Ctrl Pts',(-0.283007806606332,-6.76334737652044,
104.183768554727));
#209065=CARTESIAN_POINT('Ctrl Pts',(-0.107895395442345,-6.76613978451837,
104.191979420784));
#209066=CARTESIAN_POINT('Ctrl Pts',(0.067289862329342,-6.76893335415555,
104.200193702554));
#209067=CARTESIAN_POINT('Ctrl Pts',(0.242502715178607,-6.76491760341774,
104.208407984323));
#209068=CARTESIAN_POINT('Ctrl Pts',(0.41718053097064,-6.75412832307612,
104.216622266093));
#209069=CARTESIAN_POINT('Ctrl Pts',(0.592054960434044,-6.74332689854774,
104.224845793686));
#209070=CARTESIAN_POINT('Ctrl Pts',(0.766392794454234,-6.72573673845055,
104.233069321278));
#209071=CARTESIAN_POINT('Ctrl Pts',(0.939636913868471,-6.70144547617122,
104.24129284887));
#209072=CARTESIAN_POINT('Ctrl Pts',(1.11299207602382,-6.67713864413774,
104.249521647424));
#209073=CARTESIAN_POINT('Ctrl Pts',(1.28525177658029,-6.64612221075652,
104.257750445978));
#209074=CARTESIAN_POINT('Ctrl Pts',(1.45587048673085,-6.60853464285889,
104.265979244531));
#209075=CARTESIAN_POINT('Ctrl Pts',(1.62672403988286,-6.57089533868185,
104.274219369368));
#209076=CARTESIAN_POINT('Ctrl Pts',(1.79593174760206,-6.52666692393174,
104.282459494204));
#209077=CARTESIAN_POINT('Ctrl Pts',(1.96296362499377,-6.4760375853566,104.290699619041));
#209078=CARTESIAN_POINT('Ctrl Pts',(2.03711888540524,-6.45356024842471,
104.294357894411));
#209079=CARTESIAN_POINT('Ctrl Pts',(2.11084555593323,-6.42982192959471,
104.298016169781));
#209080=CARTESIAN_POINT('Ctrl Pts',(2.18409864199947,-6.40484208408108,
104.301674445151));
#209081=CARTESIAN_POINT('Ctrl Pts',(2.3532613418849,-6.34715634909395,104.310122467913));
